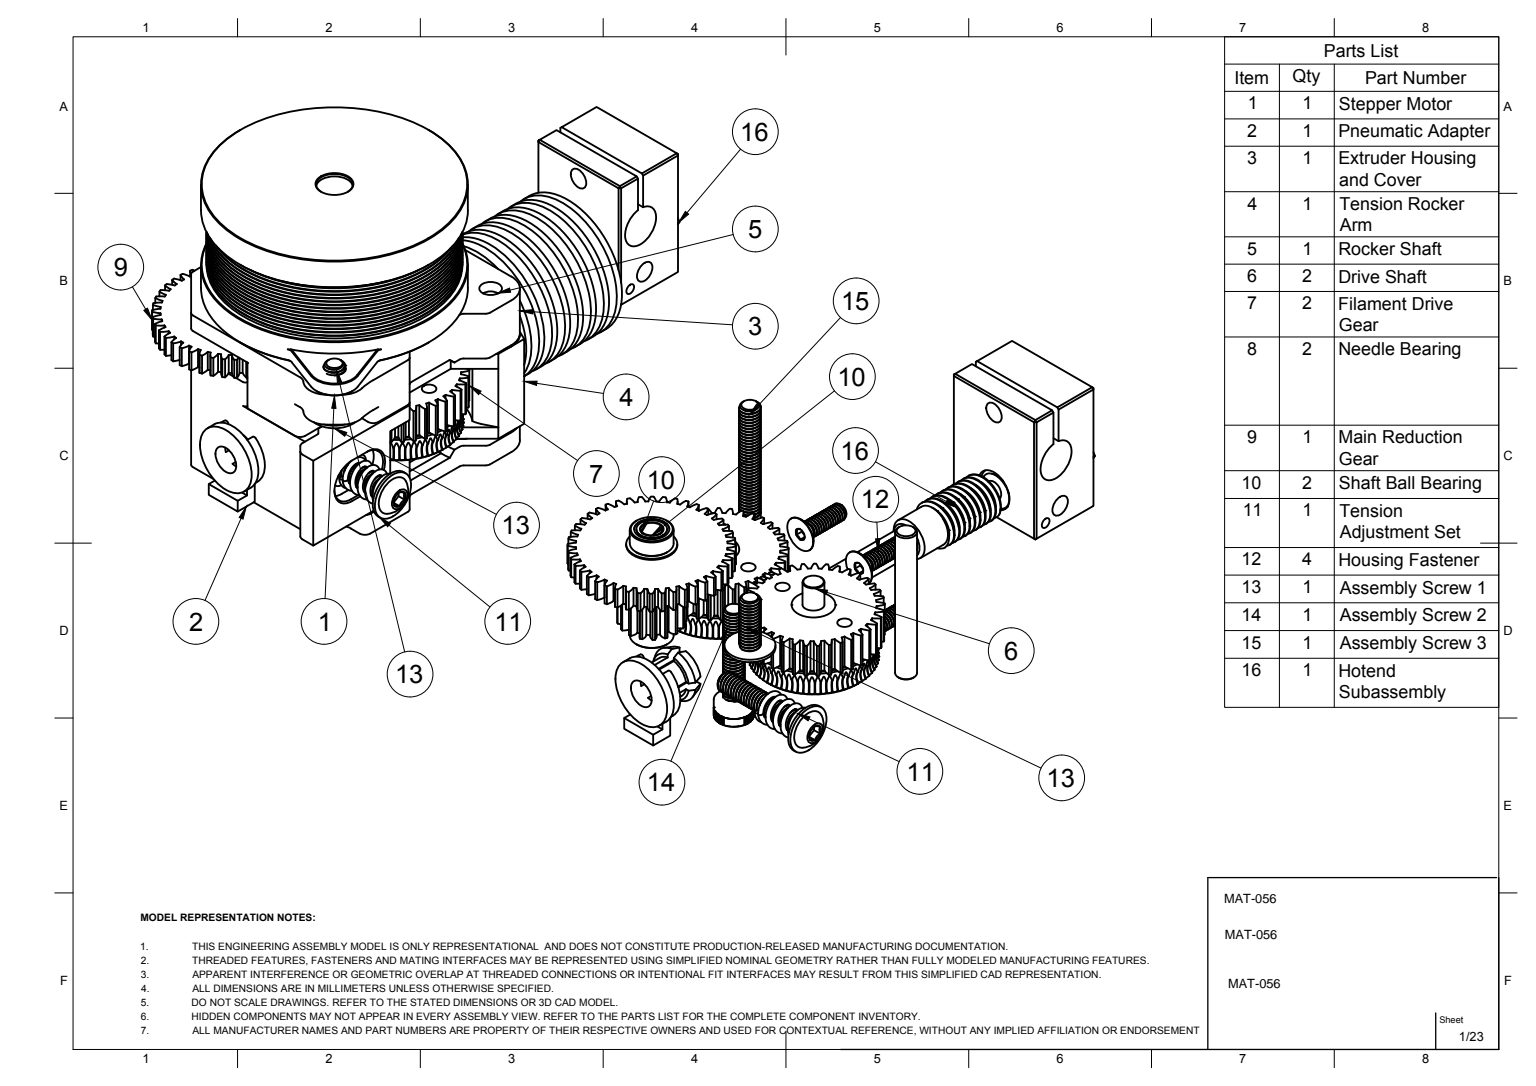
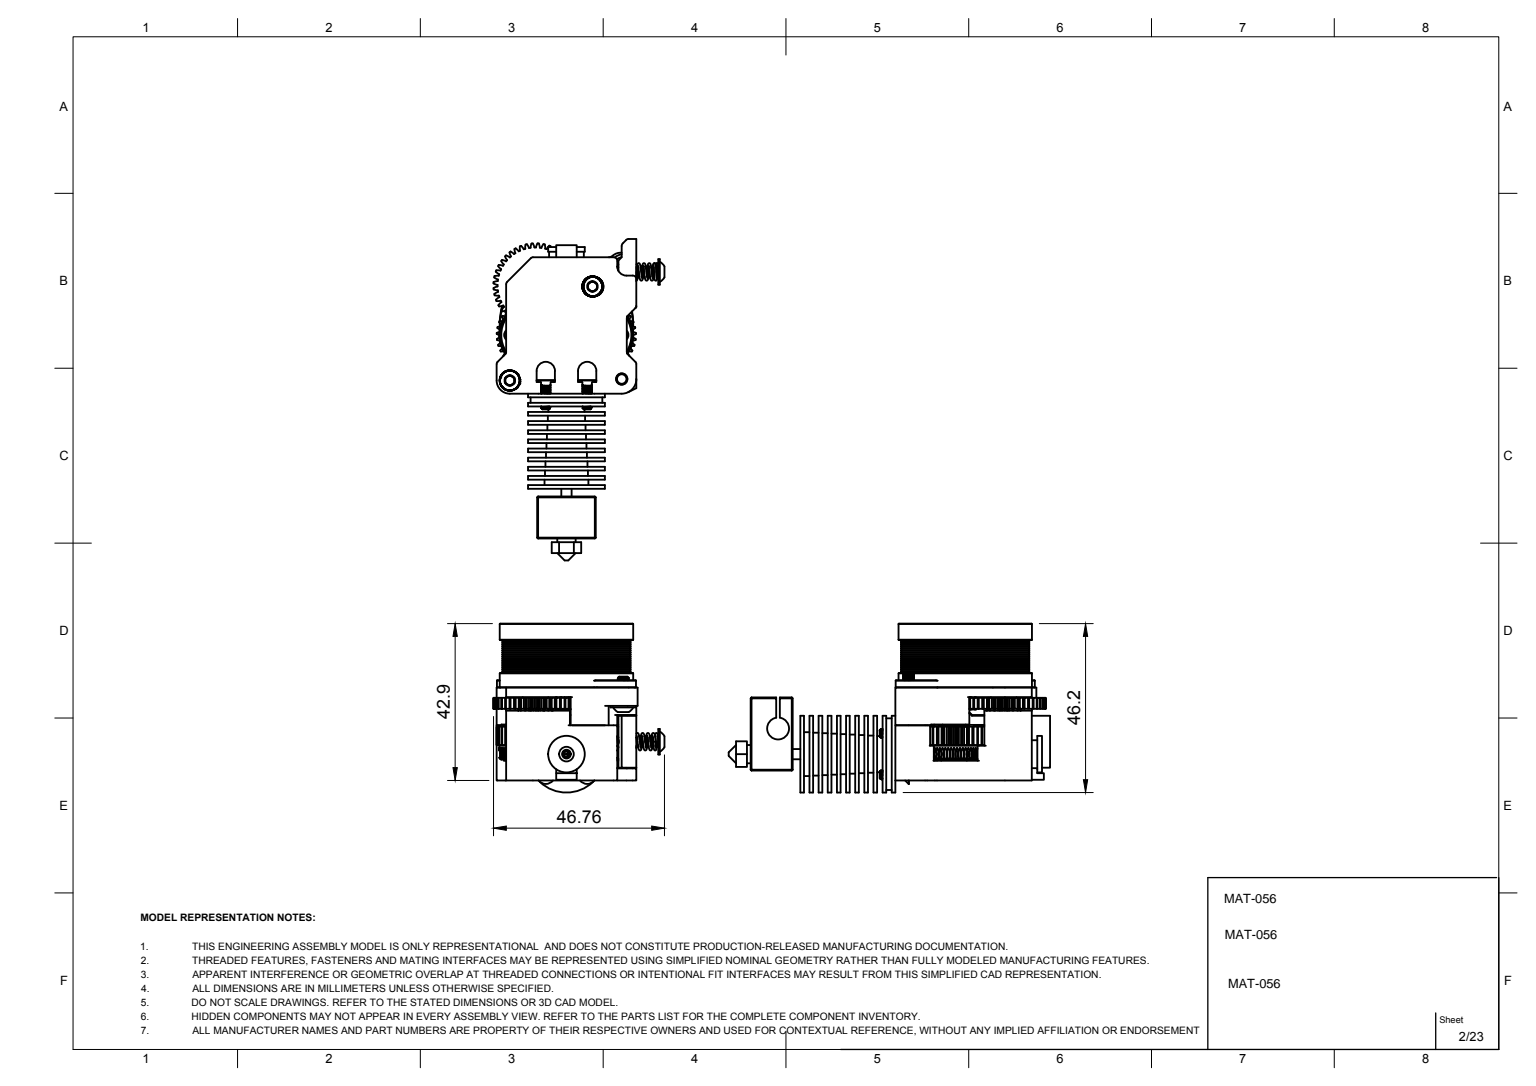
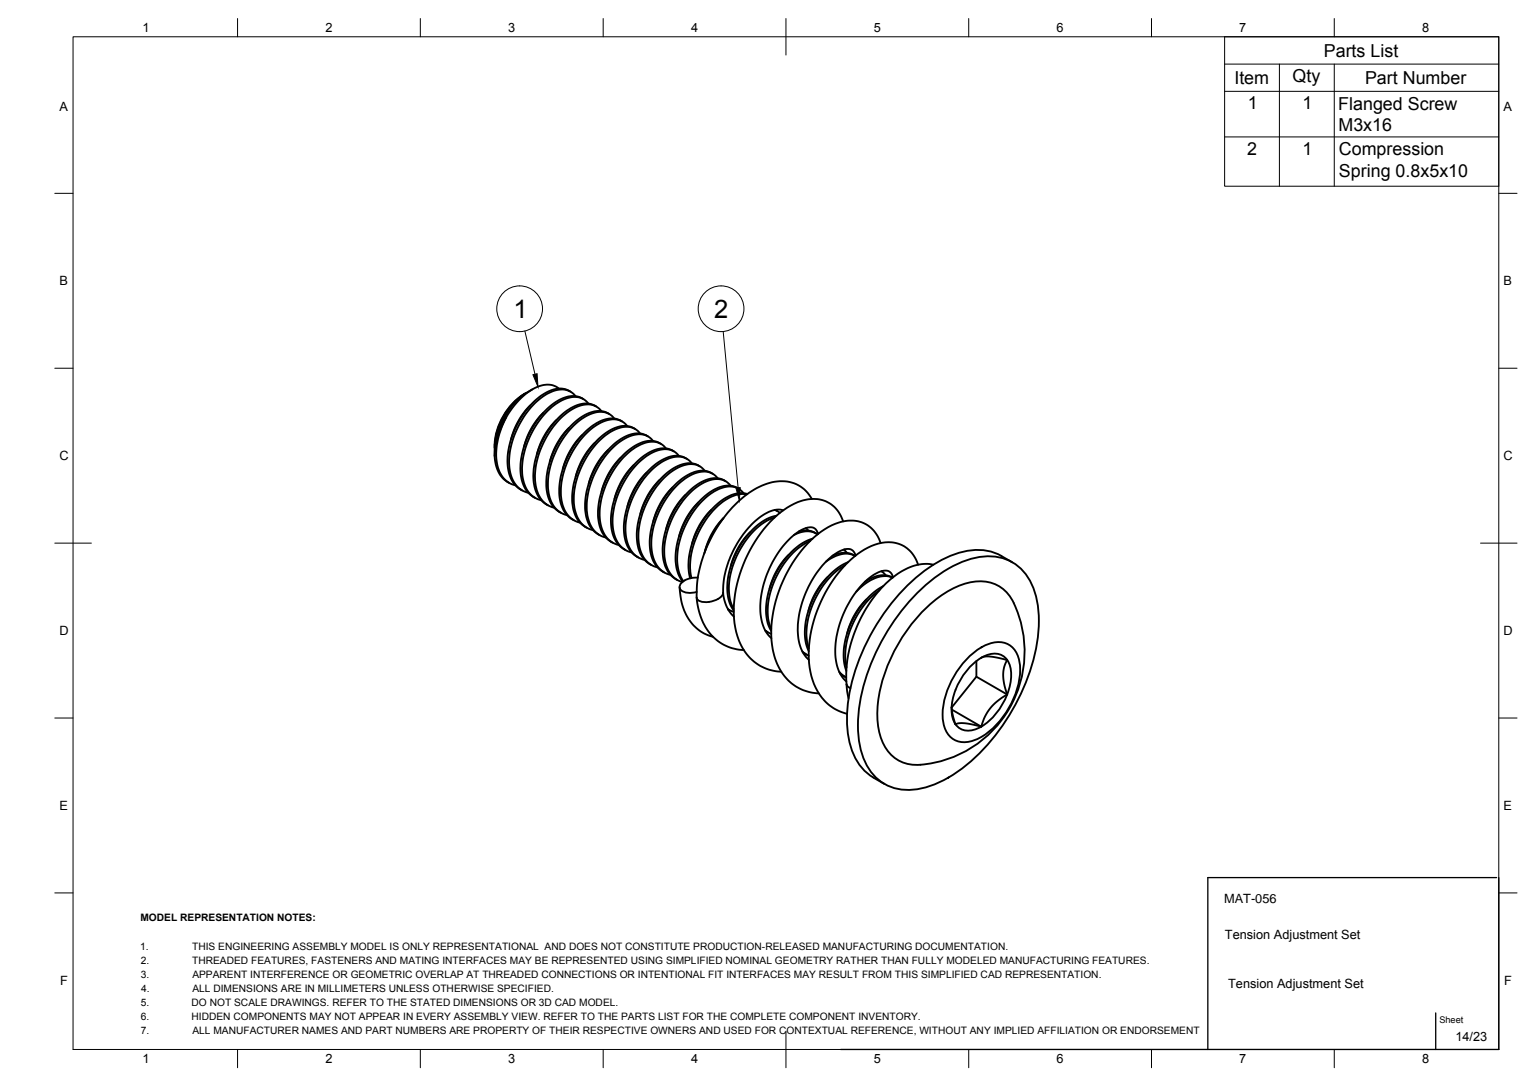
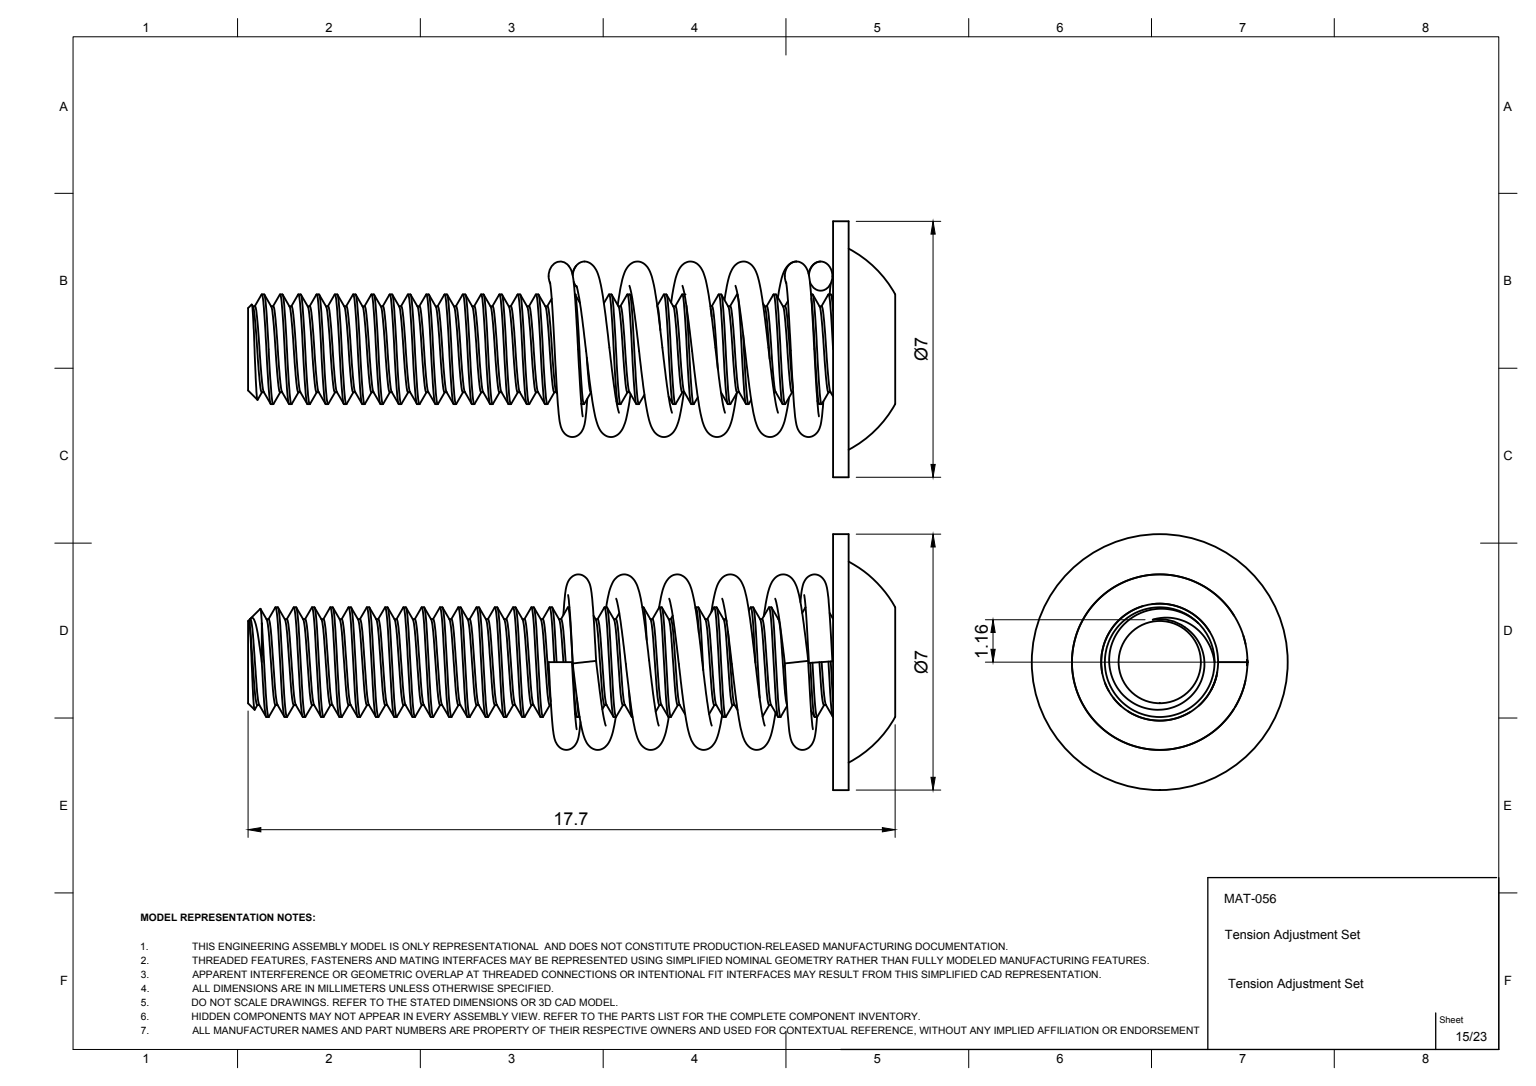
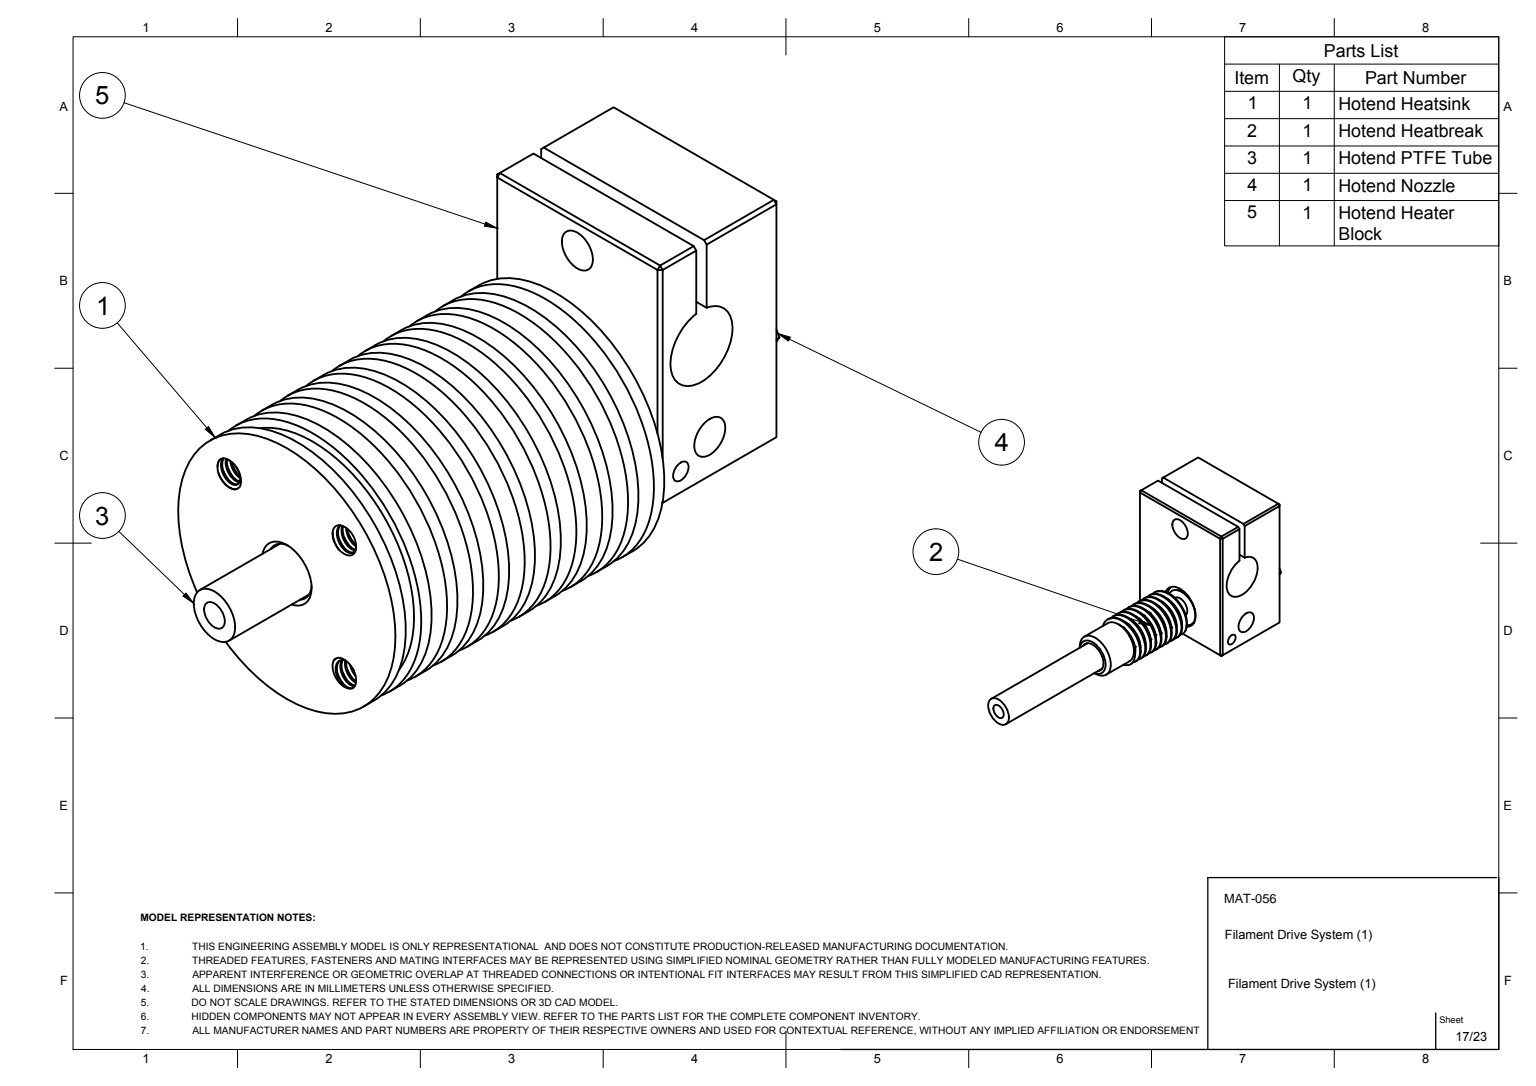
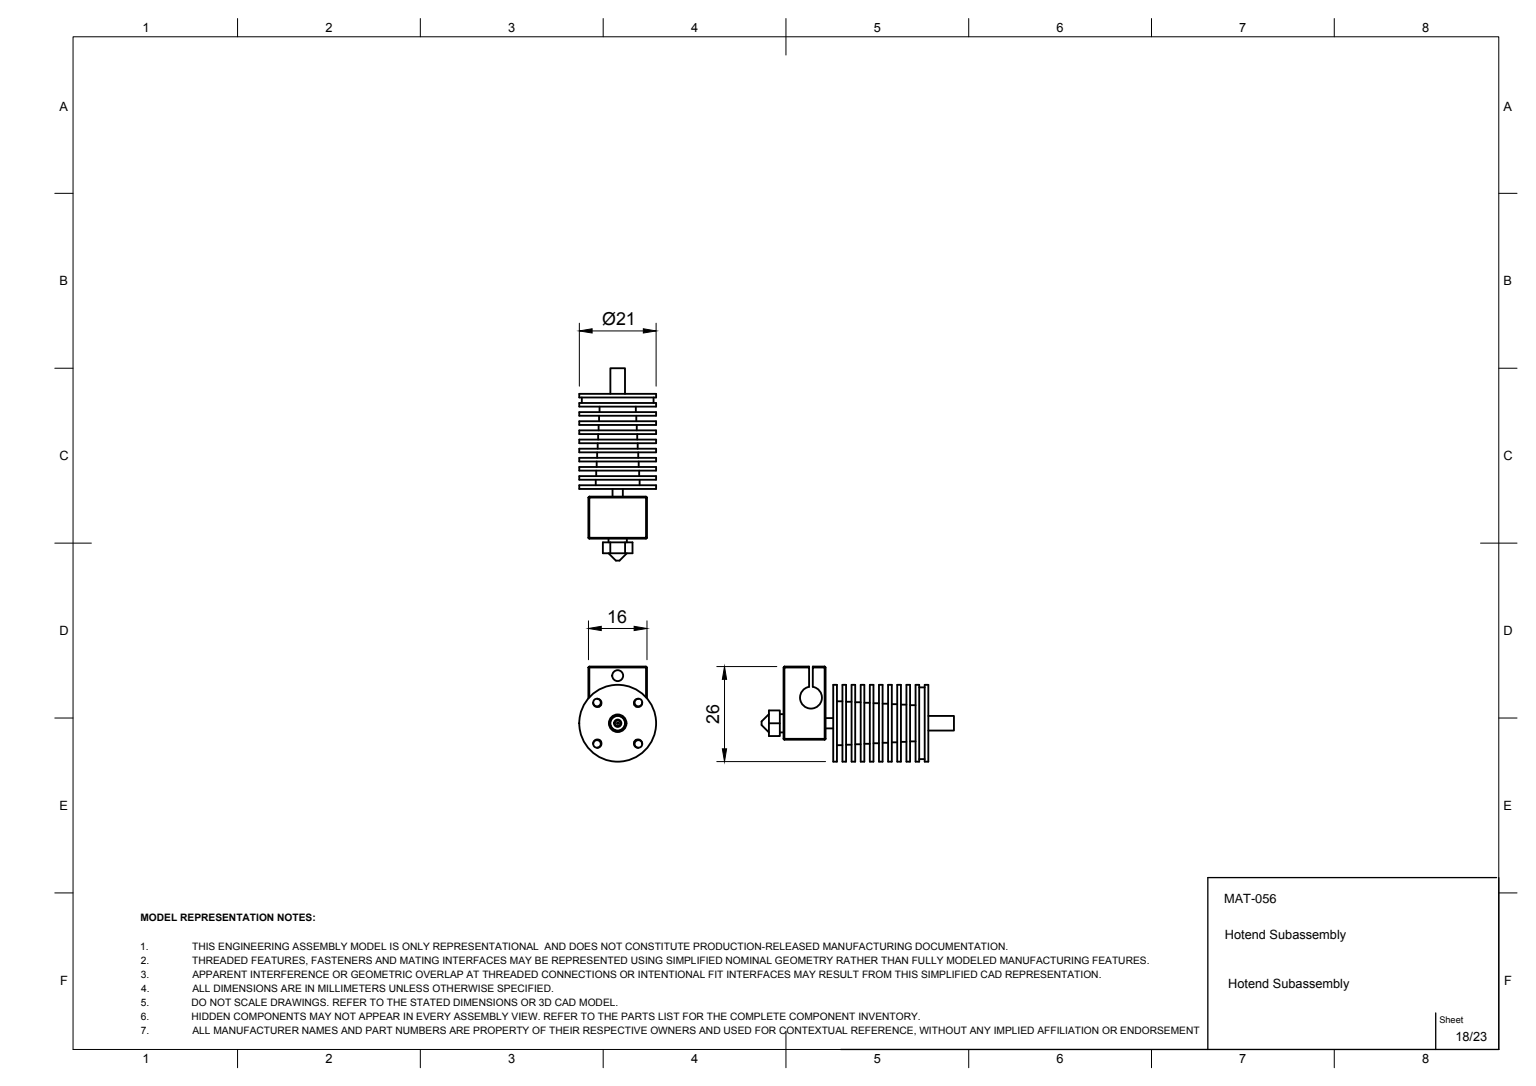
ISO-10303-21;
HEADER;
/* Generated by software containing ST-Developer
 * from STEP Tools, Inc. (www.steptools.com) 
 */

FILE_DESCRIPTION(
/* description */ (''),
/* implementation_level */ '2;1');

FILE_NAME(
/* name */ 'MAT-056',
/* time_stamp */ '2026-10-28T16:47:13+01:00',
/* author */ (''),
/* organization */ (''),
/* preprocessor_version */ 'ST-DEVELOPER v20.2',
/* originating_system */ 'Autodesk Translation Framework v15.17.0.0',
/* authorisation */ '');

FILE_SCHEMA (('AUTOMOTIVE_DESIGN { 1 0 10303 214 3 1 1 }'));
ENDSEC;

DATA;
#10=MECHANICAL_DESIGN_GEOMETRIC_PRESENTATION_REPRESENTATION('',(#4494,#4495,
#4496,#4497,#4498,#4499,#4500,#4501,#4502,#4503,#4504,#4505,#4506,#4507,
#4508,#4509,#4510,#4511,#4512,#4513,#4514,#4515,#4516,#4517,#4518,#4519,
#4520,#4521,#4522,#4523,#4524,#4525,#4526,#4527,#4528,#4529,#4530,#4531,
#4532,#4533,#4534,#4535,#4536,#4537,#4538,#4539,#4540,#4541,#4542,#4543,
#4544,#4545,#4546,#4547,#4548,#4549,#4550,#4551,#4552,#4553,#4554,#4555,
#4556,#4557,#4558,#4559,#4560,#4561,#4562,#4563,#4564,#4565,#4566,#4567,
#4568,#4569,#4570,#4571,#4572,#4573,#4574,#4575,#4576,#4577,#4578,#4579,
#4580,#4581,#4582,#4583,#4584,#4585,#4586,#4587,#4588,#4589,#4590,#4591,
#4592,#4593,#4594,#4595,#4596,#4597,#4598,#4599,#4600,#4601,#4602,#4603,
#4604,#4605,#4606,#4607,#4608,#4609,#4610,#4611,#4612,#4613),#459242);
#11=ITEM_DEFINED_TRANSFORMATION($,$,#99052,#99169);
#12=ITEM_DEFINED_TRANSFORMATION($,$,#99154,#99170);
#13=ITEM_DEFINED_TRANSFORMATION($,$,#105175,#105546);
#14=ITEM_DEFINED_TRANSFORMATION($,$,#105363,#105547);
#15=ITEM_DEFINED_TRANSFORMATION($,$,#105431,#105548);
#16=ITEM_DEFINED_TRANSFORMATION($,$,#105440,#105549);
#17=ITEM_DEFINED_TRANSFORMATION($,$,#105494,#105550);
#18=ITEM_DEFINED_TRANSFORMATION($,$,#94906,#105551);
#19=ITEM_DEFINED_TRANSFORMATION($,$,#95243,#105552);
#20=ITEM_DEFINED_TRANSFORMATION($,$,#95341,#105553);
#21=ITEM_DEFINED_TRANSFORMATION($,$,#97093,#105554);
#22=ITEM_DEFINED_TRANSFORMATION($,$,#97223,#105555);
#23=ITEM_DEFINED_TRANSFORMATION($,$,#97233,#105556);
#24=ITEM_DEFINED_TRANSFORMATION($,$,#97243,#105557);
#25=ITEM_DEFINED_TRANSFORMATION($,$,#97233,#105558);
#26=ITEM_DEFINED_TRANSFORMATION($,$,#98856,#105559);
#27=ITEM_DEFINED_TRANSFORMATION($,$,#97243,#105560);
#28=ITEM_DEFINED_TRANSFORMATION($,$,#98432,#105561);
#29=ITEM_DEFINED_TRANSFORMATION($,$,#99171,#105562);
#30=ITEM_DEFINED_TRANSFORMATION($,$,#98856,#105563);
#31=ITEM_DEFINED_TRANSFORMATION($,$,#99051,#105564);
#32=ITEM_DEFINED_TRANSFORMATION($,$,#99171,#105565);
#33=ITEM_DEFINED_TRANSFORMATION($,$,#99318,#105566);
#34=ITEM_DEFINED_TRANSFORMATION($,$,#99248,#105567);
#35=ITEM_DEFINED_TRANSFORMATION($,$,#99318,#105568);
#36=ITEM_DEFINED_TRANSFORMATION($,$,#99318,#105569);
#37=ITEM_DEFINED_TRANSFORMATION($,$,#99318,#105570);
#38=ITEM_DEFINED_TRANSFORMATION($,$,#99385,#105571);
#39=ITEM_DEFINED_TRANSFORMATION($,$,#102648,#105572);
#40=ITEM_DEFINED_TRANSFORMATION($,$,#105174,#105573);
#41=ITEM_DEFINED_TRANSFORMATION($,$,#94905,#105574);
#42=(
REPRESENTATION_RELATIONSHIP($,$,#459340,#459339)
REPRESENTATION_RELATIONSHIP_WITH_TRANSFORMATION(#11)
SHAPE_REPRESENTATION_RELATIONSHIP()
);
#43=(
REPRESENTATION_RELATIONSHIP($,$,#459341,#459339)
REPRESENTATION_RELATIONSHIP_WITH_TRANSFORMATION(#12)
SHAPE_REPRESENTATION_RELATIONSHIP()
);
#44=(
REPRESENTATION_RELATIONSHIP($,$,#459348,#459347)
REPRESENTATION_RELATIONSHIP_WITH_TRANSFORMATION(#13)
SHAPE_REPRESENTATION_RELATIONSHIP()
);
#45=(
REPRESENTATION_RELATIONSHIP($,$,#459349,#459347)
REPRESENTATION_RELATIONSHIP_WITH_TRANSFORMATION(#14)
SHAPE_REPRESENTATION_RELATIONSHIP()
);
#46=(
REPRESENTATION_RELATIONSHIP($,$,#459350,#459347)
REPRESENTATION_RELATIONSHIP_WITH_TRANSFORMATION(#15)
SHAPE_REPRESENTATION_RELATIONSHIP()
);
#47=(
REPRESENTATION_RELATIONSHIP($,$,#459351,#459347)
REPRESENTATION_RELATIONSHIP_WITH_TRANSFORMATION(#16)
SHAPE_REPRESENTATION_RELATIONSHIP()
);
#48=(
REPRESENTATION_RELATIONSHIP($,$,#459352,#459347)
REPRESENTATION_RELATIONSHIP_WITH_TRANSFORMATION(#17)
SHAPE_REPRESENTATION_RELATIONSHIP()
);
#49=(
REPRESENTATION_RELATIONSHIP($,$,#459330,#459329)
REPRESENTATION_RELATIONSHIP_WITH_TRANSFORMATION(#18)
SHAPE_REPRESENTATION_RELATIONSHIP()
);
#50=(
REPRESENTATION_RELATIONSHIP($,$,#459331,#459329)
REPRESENTATION_RELATIONSHIP_WITH_TRANSFORMATION(#19)
SHAPE_REPRESENTATION_RELATIONSHIP()
);
#51=(
REPRESENTATION_RELATIONSHIP($,$,#459332,#459329)
REPRESENTATION_RELATIONSHIP_WITH_TRANSFORMATION(#20)
SHAPE_REPRESENTATION_RELATIONSHIP()
);
#52=(
REPRESENTATION_RELATIONSHIP($,$,#459333,#459329)
REPRESENTATION_RELATIONSHIP_WITH_TRANSFORMATION(#21)
SHAPE_REPRESENTATION_RELATIONSHIP()
);
#53=(
REPRESENTATION_RELATIONSHIP($,$,#459334,#459329)
REPRESENTATION_RELATIONSHIP_WITH_TRANSFORMATION(#22)
SHAPE_REPRESENTATION_RELATIONSHIP()
);
#54=(
REPRESENTATION_RELATIONSHIP($,$,#459335,#459329)
REPRESENTATION_RELATIONSHIP_WITH_TRANSFORMATION(#23)
SHAPE_REPRESENTATION_RELATIONSHIP()
);
#55=(
REPRESENTATION_RELATIONSHIP($,$,#459336,#459329)
REPRESENTATION_RELATIONSHIP_WITH_TRANSFORMATION(#24)
SHAPE_REPRESENTATION_RELATIONSHIP()
);
#56=(
REPRESENTATION_RELATIONSHIP($,$,#459335,#459329)
REPRESENTATION_RELATIONSHIP_WITH_TRANSFORMATION(#25)
SHAPE_REPRESENTATION_RELATIONSHIP()
);
#57=(
REPRESENTATION_RELATIONSHIP($,$,#459338,#459329)
REPRESENTATION_RELATIONSHIP_WITH_TRANSFORMATION(#26)
SHAPE_REPRESENTATION_RELATIONSHIP()
);
#58=(
REPRESENTATION_RELATIONSHIP($,$,#459336,#459329)
REPRESENTATION_RELATIONSHIP_WITH_TRANSFORMATION(#27)
SHAPE_REPRESENTATION_RELATIONSHIP()
);
#59=(
REPRESENTATION_RELATIONSHIP($,$,#459337,#459329)
REPRESENTATION_RELATIONSHIP_WITH_TRANSFORMATION(#28)
SHAPE_REPRESENTATION_RELATIONSHIP()
);
#60=(
REPRESENTATION_RELATIONSHIP($,$,#459342,#459329)
REPRESENTATION_RELATIONSHIP_WITH_TRANSFORMATION(#29)
SHAPE_REPRESENTATION_RELATIONSHIP()
);
#61=(
REPRESENTATION_RELATIONSHIP($,$,#459338,#459329)
REPRESENTATION_RELATIONSHIP_WITH_TRANSFORMATION(#30)
SHAPE_REPRESENTATION_RELATIONSHIP()
);
#62=(
REPRESENTATION_RELATIONSHIP($,$,#459339,#459329)
REPRESENTATION_RELATIONSHIP_WITH_TRANSFORMATION(#31)
SHAPE_REPRESENTATION_RELATIONSHIP()
);
#63=(
REPRESENTATION_RELATIONSHIP($,$,#459342,#459329)
REPRESENTATION_RELATIONSHIP_WITH_TRANSFORMATION(#32)
SHAPE_REPRESENTATION_RELATIONSHIP()
);
#64=(
REPRESENTATION_RELATIONSHIP($,$,#459344,#459329)
REPRESENTATION_RELATIONSHIP_WITH_TRANSFORMATION(#33)
SHAPE_REPRESENTATION_RELATIONSHIP()
);
#65=(
REPRESENTATION_RELATIONSHIP($,$,#459343,#459329)
REPRESENTATION_RELATIONSHIP_WITH_TRANSFORMATION(#34)
SHAPE_REPRESENTATION_RELATIONSHIP()
);
#66=(
REPRESENTATION_RELATIONSHIP($,$,#459344,#459329)
REPRESENTATION_RELATIONSHIP_WITH_TRANSFORMATION(#35)
SHAPE_REPRESENTATION_RELATIONSHIP()
);
#67=(
REPRESENTATION_RELATIONSHIP($,$,#459344,#459329)
REPRESENTATION_RELATIONSHIP_WITH_TRANSFORMATION(#36)
SHAPE_REPRESENTATION_RELATIONSHIP()
);
#68=(
REPRESENTATION_RELATIONSHIP($,$,#459344,#459329)
REPRESENTATION_RELATIONSHIP_WITH_TRANSFORMATION(#37)
SHAPE_REPRESENTATION_RELATIONSHIP()
);
#69=(
REPRESENTATION_RELATIONSHIP($,$,#459345,#459329)
REPRESENTATION_RELATIONSHIP_WITH_TRANSFORMATION(#38)
SHAPE_REPRESENTATION_RELATIONSHIP()
);
#70=(
REPRESENTATION_RELATIONSHIP($,$,#459346,#459329)
REPRESENTATION_RELATIONSHIP_WITH_TRANSFORMATION(#39)
SHAPE_REPRESENTATION_RELATIONSHIP()
);
#71=(
REPRESENTATION_RELATIONSHIP($,$,#459347,#459329)
REPRESENTATION_RELATIONSHIP_WITH_TRANSFORMATION(#40)
SHAPE_REPRESENTATION_RELATIONSHIP()
);
#72=(
REPRESENTATION_RELATIONSHIP($,$,#459329,#459328)
REPRESENTATION_RELATIONSHIP_WITH_TRANSFORMATION(#41)
SHAPE_REPRESENTATION_RELATIONSHIP()
);
#73=CONTEXT_DEPENDENT_SHAPE_REPRESENTATION(#42,#459286);
#74=CONTEXT_DEPENDENT_SHAPE_REPRESENTATION(#43,#459287);
#75=CONTEXT_DEPENDENT_SHAPE_REPRESENTATION(#44,#459299);
#76=CONTEXT_DEPENDENT_SHAPE_REPRESENTATION(#45,#459300);
#77=CONTEXT_DEPENDENT_SHAPE_REPRESENTATION(#46,#459301);
#78=CONTEXT_DEPENDENT_SHAPE_REPRESENTATION(#47,#459302);
#79=CONTEXT_DEPENDENT_SHAPE_REPRESENTATION(#48,#459303);
#80=CONTEXT_DEPENDENT_SHAPE_REPRESENTATION(#49,#459304);
#81=CONTEXT_DEPENDENT_SHAPE_REPRESENTATION(#50,#459305);
#82=CONTEXT_DEPENDENT_SHAPE_REPRESENTATION(#51,#459306);
#83=CONTEXT_DEPENDENT_SHAPE_REPRESENTATION(#52,#459307);
#84=CONTEXT_DEPENDENT_SHAPE_REPRESENTATION(#53,#459308);
#85=CONTEXT_DEPENDENT_SHAPE_REPRESENTATION(#54,#459309);
#86=CONTEXT_DEPENDENT_SHAPE_REPRESENTATION(#55,#459310);
#87=CONTEXT_DEPENDENT_SHAPE_REPRESENTATION(#56,#459311);
#88=CONTEXT_DEPENDENT_SHAPE_REPRESENTATION(#57,#459312);
#89=CONTEXT_DEPENDENT_SHAPE_REPRESENTATION(#58,#459313);
#90=CONTEXT_DEPENDENT_SHAPE_REPRESENTATION(#59,#459314);
#91=CONTEXT_DEPENDENT_SHAPE_REPRESENTATION(#60,#459315);
#92=CONTEXT_DEPENDENT_SHAPE_REPRESENTATION(#61,#459316);
#93=CONTEXT_DEPENDENT_SHAPE_REPRESENTATION(#62,#459317);
#94=CONTEXT_DEPENDENT_SHAPE_REPRESENTATION(#63,#459318);
#95=CONTEXT_DEPENDENT_SHAPE_REPRESENTATION(#64,#459319);
#96=CONTEXT_DEPENDENT_SHAPE_REPRESENTATION(#65,#459320);
#97=CONTEXT_DEPENDENT_SHAPE_REPRESENTATION(#66,#459321);
#98=CONTEXT_DEPENDENT_SHAPE_REPRESENTATION(#67,#459322);
#99=CONTEXT_DEPENDENT_SHAPE_REPRESENTATION(#68,#459323);
#100=CONTEXT_DEPENDENT_SHAPE_REPRESENTATION(#69,#459324);
#101=CONTEXT_DEPENDENT_SHAPE_REPRESENTATION(#70,#459325);
#102=CONTEXT_DEPENDENT_SHAPE_REPRESENTATION(#71,#459326);
#103=CONTEXT_DEPENDENT_SHAPE_REPRESENTATION(#72,#459327);
#104=NEXT_ASSEMBLY_USAGE_OCCURRENCE('Flanged Screw M3x16:1',
'Flanged Screw M3x16:1','Flanged Screw M3x16:1',#459365,#459366,
'Flanged Screw M3x16:1');
#105=NEXT_ASSEMBLY_USAGE_OCCURRENCE('Compression Spring 0.8x5x10:1',
'Compression Spring 0.8x5x10:1','Compression Spring 0.8x5x10:1',#459365,
#459367,'Compression Spring 0.8x5x10:1');
#106=NEXT_ASSEMBLY_USAGE_OCCURRENCE('Hotend Heatsink:1',
'Hotend Heatsink:1','Hotend Heatsink:1',#459373,#459374,
'Hotend Heatsink:1');
#107=NEXT_ASSEMBLY_USAGE_OCCURRENCE('Hotend Heatbreak:1',
'Hotend Heatbreak:1','Hotend Heatbreak:1',#459373,#459375,
'Hotend Heatbreak:1');
#108=NEXT_ASSEMBLY_USAGE_OCCURRENCE('Hotend PTFE Tube:1',
'Hotend PTFE Tube:1','Hotend PTFE Tube:1',#459373,#459376,
'Hotend PTFE Tube:1');
#109=NEXT_ASSEMBLY_USAGE_OCCURRENCE('Hotend Nozzle:1','Hotend Nozzle:1',
'Hotend Nozzle:1',#459373,#459377,'Hotend Nozzle:1');
#110=NEXT_ASSEMBLY_USAGE_OCCURRENCE('Hotend Heater Block:1',
'Hotend Heater Block:1','Hotend Heater Block:1',#459373,#459378,
'Hotend Heater Block:1');
#111=NEXT_ASSEMBLY_USAGE_OCCURRENCE('Stepper Motor:1','Stepper Motor:1',
'Stepper Motor:1',#459355,#459356,'Stepper Motor:1');
#112=NEXT_ASSEMBLY_USAGE_OCCURRENCE('Pneumatic Adapter:1',
'Pneumatic Adapter:1','Pneumatic Adapter:1',#459355,#459357,
'Pneumatic Adapter:1');
#113=NEXT_ASSEMBLY_USAGE_OCCURRENCE('Extruder Housing and Cover:1',
'Extruder Housing and Cover:1','Extruder Housing and Cover:1',#459355,#459358,
'Extruder Housing and Cover:1');
#114=NEXT_ASSEMBLY_USAGE_OCCURRENCE('Tension Rocker Arm:1',
'Tension Rocker Arm:1','Tension Rocker Arm:1',#459355,#459359,
'Tension Rocker Arm:1');
#115=NEXT_ASSEMBLY_USAGE_OCCURRENCE('Rocker Shaft:1','Rocker Shaft:1',
'Rocker Shaft:1',#459355,#459360,'Rocker Shaft:1');
#116=NEXT_ASSEMBLY_USAGE_OCCURRENCE('Drive Shaft:1','Drive Shaft:1',
'Drive Shaft:1',#459355,#459361,'Drive Shaft:1');
#117=NEXT_ASSEMBLY_USAGE_OCCURRENCE('Filament Drive Gear:1',
'Filament Drive Gear:1','Filament Drive Gear:1',#459355,#459362,
'Filament Drive Gear:1');
#118=NEXT_ASSEMBLY_USAGE_OCCURRENCE('Drive Shaft:2','Drive Shaft:2',
'Drive Shaft:2',#459355,#459361,'Drive Shaft:2');
#119=NEXT_ASSEMBLY_USAGE_OCCURRENCE('Needle Bearing:1',
'Needle Bearing:1','Needle Bearing:1',#459355,#459364,
'Needle Bearing:1');
#120=NEXT_ASSEMBLY_USAGE_OCCURRENCE('Filament Drive Gear:2',
'Filament Drive Gear:2','Filament Drive Gear:2',#459355,#459362,
'Filament Drive Gear:2');
#121=NEXT_ASSEMBLY_USAGE_OCCURRENCE('Main Reduction Gear:1',
'Main Reduction Gear:1','Main Reduction Gear:1',#459355,#459363,
'Main Reduction Gear:1');
#122=NEXT_ASSEMBLY_USAGE_OCCURRENCE('Shaft Ball Bearing:1',
'Shaft Ball Bearing:1','Shaft Ball Bearing:1',#459355,#459368,
'Shaft Ball Bearing:1');
#123=NEXT_ASSEMBLY_USAGE_OCCURRENCE('Needle Bearing:2',
'Needle Bearing:2','Needle Bearing:2',#459355,#459364,
'Needle Bearing:2');
#124=NEXT_ASSEMBLY_USAGE_OCCURRENCE('Tension Adjustment Set:1',
'Tension Adjustment Set:1','Tension Adjustment Set:1',#459355,#459365,
'Tension Adjustment Set:1');
#125=NEXT_ASSEMBLY_USAGE_OCCURRENCE('Shaft Ball Bearing:2',
'Shaft Ball Bearing:2','Shaft Ball Bearing:2',#459355,#459368,
'Shaft Ball Bearing:2');
#126=NEXT_ASSEMBLY_USAGE_OCCURRENCE('Housing Fastener:1',
'Housing Fastener:1','Housing Fastener:1',#459355,#459370,
'Housing Fastener:1');
#127=NEXT_ASSEMBLY_USAGE_OCCURRENCE('Assembly Screw 1:1',
'Assembly Screw 1:1','Assembly Screw 1:1',#459355,#459369,
'Assembly Screw 1:1');
#128=NEXT_ASSEMBLY_USAGE_OCCURRENCE('Housing Fastener:2',
'Housing Fastener:2','Housing Fastener:2',#459355,#459370,
'Housing Fastener:2');
#129=NEXT_ASSEMBLY_USAGE_OCCURRENCE('Housing Fastener:3',
'Housing Fastener:3','Housing Fastener:3',#459355,#459370,
'Housing Fastener:3');
#130=NEXT_ASSEMBLY_USAGE_OCCURRENCE('Housing Fastener:4',
'Housing Fastener:4','Housing Fastener:4',#459355,#459370,
'Housing Fastener:4');
#131=NEXT_ASSEMBLY_USAGE_OCCURRENCE('Assembly Screw 2:1',
'Assembly Screw 2:1','Assembly Screw 2:1',#459355,#459371,
'Assembly Screw 2:1');
#132=NEXT_ASSEMBLY_USAGE_OCCURRENCE('Assembly Screw 3:1',
'Assembly Screw 3:1','Assembly Screw 3:1',#459355,#459372,
'Assembly Screw 3:1');
#133=NEXT_ASSEMBLY_USAGE_OCCURRENCE('Hotend Subassembly:1',
'Hotend Subassembly:1','Hotend Subassembly:1',#459355,#459373,
'Hotend Subassembly:1');
#134=NEXT_ASSEMBLY_USAGE_OCCURRENCE('Filament Drive System:1',
'Filament Drive System:1','Filament Drive System:1',#459354,#459355,
'Filament Drive System:1');
#135=SPHERICAL_SURFACE('',#96252,3.7);
#136=SPHERICAL_SURFACE('',#96289,0.4);
#137=SPHERICAL_SURFACE('',#96515,3.7);
#138=SPHERICAL_SURFACE('',#96673,2.5);
#139=SPHERICAL_SURFACE('',#96678,2.5);
#140=SPHERICAL_SURFACE('',#96891,0.4);
#141=SPHERICAL_SURFACE('',#96896,0.4);
#142=SPHERICAL_SURFACE('',#99121,3.10691712599126);
#143=SPHERICAL_SURFACE('',#99208,0.576463888168111);
#144=SPHERICAL_SURFACE('',#99210,0.576463888168111);
#145=SPHERICAL_SURFACE('',#99212,0.576463888168111);
#146=SPHERICAL_SURFACE('',#99214,0.576463888168111);
#147=SPHERICAL_SURFACE('',#99216,0.576463888168111);
#148=SPHERICAL_SURFACE('',#99218,0.576463888168111);
#149=SPHERICAL_SURFACE('',#99220,0.576463888168111);
#150=SPHERICAL_SURFACE('',#99222,0.576463888168111);
#151=SPHERICAL_SURFACE('',#99224,0.576463888168111);
#152=SPHERICAL_SURFACE('',#99226,0.576463888168111);
#153=SPHERICAL_SURFACE('',#99228,0.576463888168111);
#154=SPHERICAL_SURFACE('',#99230,0.576463888168111);
#155=SPHERICAL_SURFACE('',#99285,3.10691712599126);
#156=ELLIPSE('',#96160,1.23559647500717,0.4);
#157=ELLIPSE('',#96173,0.405496303869506,0.4);
#158=ELLIPSE('',#96175,0.680073525436772,0.4);
#159=ELLIPSE('',#96193,0.565685424949236,0.4);
#160=ELLIPSE('',#96250,11.2311262166053,9.2);
#161=ELLIPSE('',#96391,11.2311262166054,9.2);
#162=ELLIPSE('',#96412,0.565685424948761,0.4);
#163=ELLIPSE('',#96519,10.6232449530892,9.2);
#164=ELLIPSE('',#96520,11.2311262166053,9.2);
#165=ELLIPSE('',#96521,11.2311262166053,9.2);
#166=ELLIPSE('',#96562,11.2311262166054,9.2);
#167=ELLIPSE('',#96563,10.6232449530892,9.2);
#168=ELLIPSE('',#96876,12.4909175466738,7.94395207421036);
#169=ELLIPSE('',#97006,2.10877579943506,1.);
#170=ELLIPSE('',#97007,2.46373699895096,1.);
#171=ELLIPSE('',#97009,2.59999999999994,1.3);
#172=ELLIPSE('',#97010,0.230940107675852,0.2);
#173=ELLIPSE('',#97011,0.230940107675852,0.2);
#174=ELLIPSE('',#97015,2.26648083430746,1.3);
#175=ELLIPSE('',#97016,0.24415491775229,0.2);
#176=ELLIPSE('',#97017,0.24415491775229,0.2);
#177=ELLIPSE('',#97027,0.24415491775229,0.2);
#178=ELLIPSE('',#97030,0.24415491775229,0.2);
#179=ELLIPSE('',#97033,0.230940107675851,0.2);
#180=ELLIPSE('',#97035,0.230940107675851,0.2);
#181=ELLIPSE('',#97037,2.59999999999997,1.3);
#182=ELLIPSE('',#97038,2.46373699895092,1.);
#183=ELLIPSE('',#97040,2.10877579943508,1.);
#184=ELLIPSE('',#97042,2.26648083430744,1.3);
#185=ELLIPSE('',#97153,2.40416305603427,1.7);
#186=ELLIPSE('',#99155,0.40000000018352,0.321902553589955);
#187=ELLIPSE('',#99156,0.400000000332434,0.321319291807333);
#188=ELLIPSE('',#99157,0.40000000018352,0.321902553589955);
#189=ELLIPSE('',#99158,0.400000000010015,0.321902553729585);
#190=ELLIPSE('',#99159,0.400000000010015,0.321902553729585);
#191=ELLIPSE('',#99160,0.4,0.32);
#192=ELLIPSE('',#99161,0.4,0.32);
#193=ELLIPSE('',#99162,0.400000000010016,0.321902553729585);
#194=ELLIPSE('',#99163,0.400000000010016,0.321902553729585);
#195=ELLIPSE('',#99165,0.400000000183514,0.321902553589955);
#196=ELLIPSE('',#99166,0.400000000183514,0.321902553589955);
#197=ELLIPSE('',#99168,0.40000000033243,0.321319291807334);
#198=ELLIPSE('',#99479,0.027499979201819,0.0194466400235264);
#199=ELLIPSE('',#99481,0.0274999792018223,0.0194466400235272);
#200=ELLIPSE('',#99483,0.0274999792017924,0.0194466400235207);
#201=ELLIPSE('',#99485,0.0274999792018212,0.0194466400235271);
#202=ELLIPSE('',#99487,0.0274999792018093,0.0194466400235266);
#203=ELLIPSE('',#99489,0.0274999792018116,0.0194466400235246);
#204=ELLIPSE('',#99491,0.0274999792018137,0.0194466400235258);
#205=ELLIPSE('',#99493,0.0274999792018285,0.019446640023529);
#206=ELLIPSE('',#99495,0.0274999792018225,0.0194466400235274);
#207=ELLIPSE('',#99497,0.0274999792018218,0.0194466400235291);
#208=ELLIPSE('',#99499,0.0274999792018109,0.019446640023525);
#209=ELLIPSE('',#99501,0.0274999792018031,0.0194466400235235);
#210=ELLIPSE('',#99503,0.0274999792018403,0.0194466400235318);
#211=ELLIPSE('',#99505,0.0274999792018273,0.0194466400235287);
#212=ELLIPSE('',#99507,0.0274999792018071,0.0194466400235239);
#213=ELLIPSE('',#99509,0.0274999792018003,0.0194466400235229);
#214=ELLIPSE('',#99511,0.0274999792018132,0.0194466400235249);
#215=ELLIPSE('',#99513,0.0274999792018307,0.0194466400235292);
#216=ELLIPSE('',#99515,0.0274999792018211,0.0194466400235281);
#217=ELLIPSE('',#99517,0.027499979201803,0.0194466400235226);
#218=ELLIPSE('',#99519,0.027499979201819,0.019446640023527);
#219=ELLIPSE('',#99521,0.0274999792018149,0.0194466400235247);
#220=ELLIPSE('',#99523,0.0274999792018479,0.019446640023533);
#221=ELLIPSE('',#99525,0.0274999792018327,0.0194466400235312);
#222=ELLIPSE('',#99527,0.0274999792018231,0.0194466400235292);
#223=ELLIPSE('',#99529,0.0274999792018213,0.0194466400235274);
#224=ELLIPSE('',#99531,0.0274999792018071,0.0194466400235238);
#225=ELLIPSE('',#99533,0.0274999792018454,0.0194466400235312);
#226=ELLIPSE('',#99535,0.0274999792018473,0.0194466400235348);
#227=ELLIPSE('',#99537,0.0274999792017789,0.0194466400235172);
#228=ELLIPSE('',#99539,0.0274999792017695,0.0194466400235156);
#229=ELLIPSE('',#99541,0.0274999792018213,0.0194466400235258);
#230=ELLIPSE('',#99543,0.0274999792018424,0.0194466400235306);
#231=ELLIPSE('',#99545,0.0274999792018183,0.0194466400235275);
#232=ELLIPSE('',#99547,0.0274999792018239,0.0194466400235288);
#233=ELLIPSE('',#99549,0.02749997920184,0.0194466400235311);
#234=ELLIPSE('',#99551,0.0274999792018135,0.0194466400235251);
#235=ELLIPSE('',#99553,0.0274999792017894,0.019446640023519);
#236=ELLIPSE('',#99555,0.0274999792018526,0.0194466400235354);
#237=ELLIPSE('',#99557,0.0274999792017924,0.0194466400235216);
#238=ELLIPSE('',#99559,0.0274999792018348,0.0194466400235303);
#239=ELLIPSE('',#99561,0.0274999792018408,0.0194466400235337);
#240=ELLIPSE('',#99563,0.0274999792018198,0.0194466400235256);
#241=ELLIPSE('',#99565,0.0274999792018384,0.0194466400235318);
#242=ELLIPSE('',#99567,0.027499979201788,0.0194466400235206);
#243=ELLIPSE('',#99569,0.0274999792018338,0.0194466400235292);
#244=ELLIPSE('',#99571,0.027499979201835,0.0194466400235291);
#245=ELLIPSE('',#99573,0.0274999792018021,0.0194466400235238);
#246=ELLIPSE('',#99575,0.0274999792018534,0.0194466400235355);
#247=ELLIPSE('',#99580,0.0274999792018521,0.0194466400235337);
#248=ELLIPSE('',#99582,0.027499979201854,0.0194466400235346);
#249=ELLIPSE('',#99584,0.0274999792018411,0.0194466400235325);
#250=ELLIPSE('',#99586,0.0274999792017827,0.0194466400235186);
#251=ELLIPSE('',#99588,0.0274999792018246,0.0194466400235274);
#252=ELLIPSE('',#99590,0.0274999792018228,0.0194466400235272);
#253=ELLIPSE('',#99592,0.0274999792018508,0.0194466400235342);
#254=ELLIPSE('',#99594,0.027499979201825,0.019446640023528);
#255=ELLIPSE('',#99596,0.0274999792018088,0.0194466400235245);
#256=ELLIPSE('',#99598,0.0274999792018039,0.0194466400235234);
#257=ELLIPSE('',#99600,0.0274999792018231,0.0194466400235278);
#258=ELLIPSE('',#99602,0.0274999792018028,0.0194466400235229);
#259=ELLIPSE('',#99604,0.0274999792018038,0.019446640023523);
#260=ELLIPSE('',#99606,0.0274999792018027,0.0194466400235246);
#261=ELLIPSE('',#99608,0.0274999792018087,0.0194466400235226);
#262=ELLIPSE('',#99610,0.027499979201824,0.0194466400235279);
#263=ELLIPSE('',#99612,0.0274999792018275,0.0194466400235301);
#264=ELLIPSE('',#99614,0.0274999792018072,0.019446640023524);
#265=ELLIPSE('',#99616,0.0274999792018082,0.0194466400235244);
#266=ELLIPSE('',#99618,0.0274999792018318,0.0194466400235293);
#267=ELLIPSE('',#99620,0.0274999792017886,0.0194466400235195);
#268=ELLIPSE('',#99622,0.0274999792018619,0.0194466400235365);
#269=ELLIPSE('',#99624,0.0274999792018085,0.0194466400235243);
#270=ELLIPSE('',#99626,0.0274999792018058,0.0194466400235241);
#271=ELLIPSE('',#99628,0.0274999792018022,0.0194466400235246);
#272=ELLIPSE('',#99630,0.02749997920182,0.0194466400235268);
#273=ELLIPSE('',#99632,0.0274999792017819,0.0194466400235169);
#274=ELLIPSE('',#99634,0.0274999792018284,0.0194466400235286);
#275=ELLIPSE('',#99636,0.0274999792018055,0.0194466400235254);
#276=ELLIPSE('',#99638,0.0274999792018053,0.0194466400235236);
#277=ELLIPSE('',#99640,0.0274999792018291,0.0194466400235292);
#278=ELLIPSE('',#99642,0.0274999792018261,0.0194466400235284);
#279=ELLIPSE('',#99644,0.0274999792018197,0.0194466400235282);
#280=ELLIPSE('',#99646,0.0274999792018074,0.0194466400235247);
#281=ELLIPSE('',#99648,0.0274999792018118,0.0194466400235253);
#282=ELLIPSE('',#99650,0.0274999792018347,0.0194466400235298);
#283=ELLIPSE('',#99652,0.0274999792017871,0.0194466400235192);
#284=ELLIPSE('',#99654,0.0274999792018461,0.0194466400235328);
#285=ELLIPSE('',#99656,0.0274999792018429,0.0194466400235337);
#286=ELLIPSE('',#99658,0.0274999792018179,0.0194466400235262);
#287=ELLIPSE('',#99660,0.0274999792018226,0.0194466400235276);
#288=ELLIPSE('',#99662,0.0274999792018338,0.0194466400235298);
#289=ELLIPSE('',#99664,0.027499979201791,0.0194466400235187);
#290=ELLIPSE('',#99666,0.0274999792018158,0.0194466400235259);
#291=ELLIPSE('',#99668,0.0274999792018309,0.0194466400235295);
#292=ELLIPSE('',#99670,0.0274999792018025,0.0194466400235224);
#293=ELLIPSE('',#99672,0.0274999792018289,0.0194466400235288);
#294=ELLIPSE('',#99674,0.0274999792018066,0.0194466400235238);
#295=ELLIPSE('',#99676,0.027499979201837,0.0194466400235302);
#296=ELLIPSE('',#99682,0.0377939546271109,0.0250703601820978);
#297=ELLIPSE('',#99684,0.0378695219465235,0.0250983059764406);
#298=ELLIPSE('',#99686,0.0377939546270395,0.0250703601820702);
#299=ELLIPSE('',#99688,0.037869521946444,0.0250983059764107);
#300=ELLIPSE('',#99690,0.0377939546272685,0.0250703601821445);
#301=ELLIPSE('',#99692,0.0378695219466119,0.0250983059764672);
#302=ELLIPSE('',#99694,0.0377939546269576,0.0250703601820378);
#303=ELLIPSE('',#99696,0.0378695219464082,0.0250983059763933);
#304=ELLIPSE('',#99698,0.0377939546267997,0.0250703601819834);
#305=ELLIPSE('',#99700,0.0378695219464645,0.0250983059764194);
#306=ELLIPSE('',#99702,0.0377939546267974,0.0250703601819848);
#307=ELLIPSE('',#99704,0.0378695219466849,0.0250983059764935);
#308=ELLIPSE('',#99706,0.0377939546269491,0.0250703601820439);
#309=ELLIPSE('',#99708,0.0378695219464801,0.0250983059764239);
#310=ELLIPSE('',#99710,0.0377939546268274,0.0250703601820047);
#311=ELLIPSE('',#99712,0.0378695219465395,0.0250983059764457);
#312=ELLIPSE('',#99714,0.0377939546270607,0.0250703601820776);
#313=ELLIPSE('',#99716,0.0378695219463676,0.02509830597638);
#314=ELLIPSE('',#99718,0.0377939546270672,0.0250703601820751);
#315=ELLIPSE('',#99720,0.0378695219465767,0.0250983059764549);
#316=ELLIPSE('',#99722,0.0377939546270847,0.0250703601820898);
#317=ELLIPSE('',#99724,0.0378695219463306,0.0250983059763689);
#318=ELLIPSE('',#99726,0.0377939546271058,0.0250703601820951);
#319=ELLIPSE('',#99728,0.0378695219463806,0.0250983059763838);
#320=ELLIPSE('',#99730,0.0377939546273992,0.0250703601821958);
#321=ELLIPSE('',#99732,0.0378695219463341,0.0250983059763734);
#322=ELLIPSE('',#99734,0.0377939546267671,0.0250703601819788);
#323=ELLIPSE('',#99736,0.0378695219467491,0.0250983059765119);
#324=ELLIPSE('',#99738,0.037793954627011,0.0250703601820574);
#325=ELLIPSE('',#99740,0.0378695219464796,0.0250983059764208);
#326=ELLIPSE('',#99742,0.0377939546271938,0.0250703601821272);
#327=ELLIPSE('',#99744,0.0378695219464403,0.0250983059764047);
#328=ELLIPSE('',#99746,0.0377939546272078,0.0250703601821293);
#329=ELLIPSE('',#99748,0.0378695219462217,0.0250983059763317);
#330=ELLIPSE('',#99750,0.0377939546274431,0.0250703601822155);
#331=ELLIPSE('',#99752,0.0378695219465727,0.025098305976455);
#332=ELLIPSE('',#99754,0.0377939546272413,0.0250703601821465);
#333=ELLIPSE('',#99756,0.0378695219465893,0.0250983059764576);
#334=ELLIPSE('',#99758,0.0377939546268262,0.0250703601819944);
#335=ELLIPSE('',#99760,0.037869521946427,0.0250983059763988);
#336=ELLIPSE('',#99762,0.0377939546267704,0.0250703601819765);
#337=ELLIPSE('',#99764,0.0378695219464597,0.0250983059764122);
#338=ELLIPSE('',#99766,0.0377939546267808,0.0250703601819798);
#339=ELLIPSE('',#99768,0.0378695219460054,0.025098305976261);
#340=ELLIPSE('',#99770,0.0377939546271222,0.0250703601820998);
#341=ELLIPSE('',#99772,0.0378695219467645,0.0250983059765208);
#342=ELLIPSE('',#99774,0.0377939546272981,0.025070360182163);
#343=ELLIPSE('',#99776,0.0378695219464416,0.0250983059764082);
#344=ELLIPSE('',#99778,0.0377939546270981,0.0250703601820953);
#345=ELLIPSE('',#99780,0.0378695219463879,0.0250983059763866);
#346=ELLIPSE('',#99782,0.0377939546269133,0.0250703601820331);
#347=ELLIPSE('',#99784,0.03786952194643,0.0250983059764058);
#348=ELLIPSE('',#99786,0.037793954627311,0.0250703601821679);
#349=ELLIPSE('',#99788,0.0378695219464575,0.0250983059764103);
#350=ELLIPSE('',#99790,0.037793954626787,0.0250703601819827);
#351=ELLIPSE('',#99792,0.0378695219465744,0.0250983059764543);
#352=ELLIPSE('',#99794,0.037793954627,0.0250703601820628);
#353=ELLIPSE('',#99796,0.0378695219464972,0.0250983059764296);
#354=ELLIPSE('',#99798,0.0377939546271824,0.0250703601821208);
#355=ELLIPSE('',#99800,0.0378695219463181,0.0250983059763621);
#356=ELLIPSE('',#99802,0.0377939546270806,0.02507036018209);
#357=ELLIPSE('',#99804,0.0378695219464793,0.025098305976419);
#358=ELLIPSE('',#99806,0.0377939546271536,0.0250703601821112);
#359=ELLIPSE('',#99808,0.0378695219464171,0.0250983059764114);
#360=ELLIPSE('',#99810,0.0377939546268865,0.0250703601820144);
#361=ELLIPSE('',#99812,0.0378695219466686,0.0250983059764919);
#362=ELLIPSE('',#99814,0.0377939546269507,0.0250703601820383);
#363=ELLIPSE('',#99816,0.0378695219467058,0.0250983059764957);
#364=ELLIPSE('',#99818,0.0377939546272764,0.0250703601821624);
#365=ELLIPSE('',#99820,0.0378695219461522,0.0250983059763082);
#366=ELLIPSE('',#99822,0.0377939546272405,0.0250703601821427);
#367=ELLIPSE('',#99824,0.0378695219465727,0.0250983059764577);
#368=ELLIPSE('',#99826,0.0377939546272697,0.0250703601821556);
#369=ELLIPSE('',#99828,0.0378695219465898,0.0250983059764639);
#370=ELLIPSE('',#99830,0.0377939546271452,0.0250703601821021);
#371=ELLIPSE('',#99832,0.0378695219464919,0.0250983059764311);
#372=ELLIPSE('',#99834,0.0377939546270735,0.0250703601820848);
#373=ELLIPSE('',#99836,0.0378695219467591,0.0250983059765092);
#374=ELLIPSE('',#99838,0.0377939546272653,0.0250703601821518);
#375=ELLIPSE('',#99840,0.0378695219467233,0.0250983059764915);
#376=ELLIPSE('',#99842,0.0377939546271496,0.0250703601821116);
#377=ELLIPSE('',#99844,0.037869521946483,0.0250983059764293);
#378=ELLIPSE('',#99846,0.0377939546268239,0.0250703601819968);
#379=ELLIPSE('',#99848,0.0378695219468845,0.0250983059765543);
#380=ELLIPSE('',#99850,0.0377939546266337,0.0250703601819282);
#381=ELLIPSE('',#99852,0.0378695219461948,0.0250983059763309);
#382=ELLIPSE('',#99854,0.0377939546269812,0.025070360182053);
#383=ELLIPSE('',#99856,0.0378695219463886,0.0250983059763826);
#384=ELLIPSE('',#99858,0.037793954627197,0.025070360182132);
#385=ELLIPSE('',#99860,0.0378695219465481,0.0250983059764459);
#386=ELLIPSE('',#99862,0.0377939546267804,0.0250703601819784);
#387=ELLIPSE('',#99864,0.0378695219459524,0.0250983059762446);
#388=ELLIPSE('',#99866,0.0377939546270476,0.0250703601820695);
#389=ELLIPSE('',#99868,0.0378695219469002,0.0250983059765617);
#390=ELLIPSE('',#99870,0.0377939546271249,0.0250703601820983);
#391=ELLIPSE('',#99872,0.037869521946226,0.0250983059763336);
#392=ELLIPSE('',#99874,0.0377939546270712,0.0250703601820862);
#393=ELLIPSE('',#99876,0.0378695219466723,0.0250983059764892);
#394=ELLIPSE('',#99879,0.0377939546273518,0.0250703601821778);
#395=ELLIPSE('',#99881,0.037869521947147,0.0250983059766503);
#396=ELLIPSE('',#99883,0.0377939546273672,0.0250703601821858);
#397=ELLIPSE('',#99885,0.0378695219471249,0.0250983059766443);
#398=ELLIPSE('',#99887,0.0377939546272684,0.0250703601821527);
#399=ELLIPSE('',#99889,0.0378695219465376,0.0250983059764453);
#400=ELLIPSE('',#99891,0.0377939546267177,0.0250703601819543);
#401=ELLIPSE('',#99893,0.0378695219465633,0.0250983059764556);
#402=ELLIPSE('',#99895,0.0377939546267279,0.0250703601819634);
#403=ELLIPSE('',#99897,0.0378695219465408,0.0250983059764424);
#404=ELLIPSE('',#99899,0.0377939546271458,0.0250703601821111);
#405=ELLIPSE('',#99901,0.037869521946556,0.0250983059764535);
#406=ELLIPSE('',#99903,0.0377939546272391,0.0250703601821381);
#407=ELLIPSE('',#99905,0.0378695219461841,0.0250983059763208);
#408=ELLIPSE('',#99907,0.0377939546271602,0.0250703601821172);
#409=ELLIPSE('',#99909,0.0378695219469737,0.0250983059765869);
#410=ELLIPSE('',#99911,0.0377939546268286,0.025070360181992);
#411=ELLIPSE('',#99913,0.0378695219464023,0.0250983059763922);
#412=ELLIPSE('',#99915,0.0377939546271851,0.0250703601821223);
#413=ELLIPSE('',#99917,0.0378695219460789,0.0250983059762906);
#414=ELLIPSE('',#99919,0.037793954627282,0.0250703601821508);
#415=ELLIPSE('',#99921,0.0378695219465084,0.0250983059764242);
#416=ELLIPSE('',#99923,0.0377939546267815,0.0250703601819804);
#417=ELLIPSE('',#99925,0.0378695219463702,0.0250983059763883);
#418=ELLIPSE('',#99927,0.0377939546265622,0.025070360181903);
#419=ELLIPSE('',#99929,0.0378695219464024,0.0250983059764034);
#420=ELLIPSE('',#99931,0.0377939546270649,0.0250703601820832);
#421=ELLIPSE('',#99933,0.037869521946096,0.0250983059762913);
#422=ELLIPSE('',#99935,0.0377939546270451,0.0250703601820666);
#423=ELLIPSE('',#99937,0.0378695219465469,0.0250983059764424);
#424=ELLIPSE('',#99939,0.0377939546274933,0.025070360182228);
#425=ELLIPSE('',#99941,0.0378695219459719,0.0250983059762507);
#426=ELLIPSE('',#99943,0.037793954626721,0.0250703601819633);
#427=ELLIPSE('',#99945,0.0378695219467833,0.0250983059765231);
#428=ELLIPSE('',#99947,0.0377939546272019,0.0250703601821268);
#429=ELLIPSE('',#99949,0.0378695219465463,0.0250983059764481);
#430=ELLIPSE('',#99951,0.0377939546273632,0.0250703601821844);
#431=ELLIPSE('',#99953,0.0378695219468885,0.0250983059765562);
#432=ELLIPSE('',#99955,0.0377939546272644,0.0250703601821503);
#433=ELLIPSE('',#99957,0.0378695219465198,0.0250983059764359);
#434=ELLIPSE('',#99959,0.0377939546270628,0.025070360182078);
#435=ELLIPSE('',#99961,0.0378695219461977,0.02509830597633);
#436=ELLIPSE('',#99963,0.0377939546271482,0.0250703601821143);
#437=ELLIPSE('',#99965,0.0378695219465306,0.0250983059764382);
#438=ELLIPSE('',#99967,0.0377939546267965,0.0250703601819846);
#439=ELLIPSE('',#99969,0.0378695219466369,0.0250983059764776);
#440=ELLIPSE('',#99971,0.0377939546272131,0.0250703601821351);
#441=ELLIPSE('',#99973,0.0378695219464218,0.0250983059764017);
#442=ELLIPSE('',#99975,0.0377939546270981,0.0250703601820953);
#443=ELLIPSE('',#99977,0.0378695219460318,0.0250983059762701);
#444=ELLIPSE('',#99979,0.0377939546271911,0.0250703601821247);
#445=ELLIPSE('',#99981,0.0378695219466486,0.0250983059764816);
#446=ELLIPSE('',#99983,0.0377939546272545,0.0250703601821443);
#447=ELLIPSE('',#99985,0.0378695219464022,0.0250983059763928);
#448=ELLIPSE('',#99987,0.0377939546270471,0.0250703601820705);
#449=ELLIPSE('',#99989,0.0378695219464218,0.025098305976405);
#450=ELLIPSE('',#99991,0.037793954627098,0.0250703601820907);
#451=ELLIPSE('',#99993,0.03786952194662,0.0250983059764673);
#452=ELLIPSE('',#99995,0.0377939546268382,0.0250703601819987);
#453=ELLIPSE('',#99997,0.0378695219465927,0.0250983059764667);
#454=ELLIPSE('',#99999,0.0377939546271273,0.0250703601821041);
#455=ELLIPSE('',#100001,0.0378695219461789,0.0250983059763172);
#456=ELLIPSE('',#100003,0.0377939546268529,0.0250703601820112);
#457=ELLIPSE('',#100005,0.0378695219465492,0.0250983059764485);
#458=ELLIPSE('',#100007,0.0377939546268233,0.0250703601819974);
#459=ELLIPSE('',#100009,0.0378695219464527,0.0250983059764105);
#460=ELLIPSE('',#100011,0.0377939546267064,0.0250703601819536);
#461=ELLIPSE('',#100013,0.0378695219465347,0.0250983059764463);
#462=ELLIPSE('',#100015,0.0377939546271184,0.0250703601820973);
#463=ELLIPSE('',#100017,0.0378695219464462,0.0250983059764076);
#464=ELLIPSE('',#100019,0.0377939546269241,0.0250703601820279);
#465=ELLIPSE('',#100021,0.037869521946493,0.0250983059764276);
#466=ELLIPSE('',#100023,0.0377939546272981,0.025070360182169);
#467=ELLIPSE('',#100025,0.037869521946465,0.0250983059764108);
#468=ELLIPSE('',#100027,0.037793954627171,0.0250703601821197);
#469=ELLIPSE('',#100029,0.0378695219462166,0.0250983059763296);
#470=ELLIPSE('',#100031,0.0377939546272262,0.0250703601821393);
#471=ELLIPSE('',#100033,0.0378695219463891,0.0250983059763892);
#472=ELLIPSE('',#100035,0.0377939546270739,0.0250703601820887);
#473=ELLIPSE('',#100037,0.0378695219466546,0.0250983059764808);
#474=ELLIPSE('',#100039,0.0377939546270089,0.0250703601820585);
#475=ELLIPSE('',#100041,0.0378695219463441,0.0250983059763761);
#476=ELLIPSE('',#100043,0.0377939546270472,0.0250703601820732);
#477=ELLIPSE('',#100045,0.0378695219463518,0.0250983059763784);
#478=ELLIPSE('',#100047,0.0377939546271573,0.0250703601821169);
#479=ELLIPSE('',#100049,0.0378695219466952,0.0250983059764971);
#480=ELLIPSE('',#100051,0.0377939546271577,0.0250703601821112);
#481=ELLIPSE('',#100053,0.0378695219462776,0.0250983059763517);
#482=ELLIPSE('',#100055,0.0377939546271348,0.0250703601821107);
#483=ELLIPSE('',#100057,0.0378695219464613,0.0250983059764109);
#484=ELLIPSE('',#100059,0.0377939546271653,0.0250703601821089);
#485=ELLIPSE('',#100061,0.0378695219465757,0.0250983059764537);
#486=ELLIPSE('',#100063,0.0377939546272274,0.0250703601821409);
#487=ELLIPSE('',#100065,0.0378695219463364,0.0250983059763705);
#488=ELLIPSE('',#100067,0.0377939546269824,0.0250703601820482);
#489=ELLIPSE('',#100069,0.0378695219463565,0.0250983059763739);
#490=ELLIPSE('',#100071,0.0377939546272586,0.0250703601821497);
#491=ELLIPSE('',#100073,0.037869521946479,0.0250983059764217);
#492=ELLIPSE('',#100075,0.0594717522093815,0.0552292627679723);
#493=ELLIPSE('',#100076,0.0523574408941029,0.0489195958911169);
#494=ELLIPSE('',#100078,0.0523574408930336,0.048919595889694);
#495=ELLIPSE('',#100079,0.0594717522063949,0.0552292627663424);
#496=ELLIPSE('',#100081,0.059471752210527,0.0552292627685546);
#497=ELLIPSE('',#100082,0.0523574408933772,0.0489195958901572);
#498=ELLIPSE('',#100084,0.0594717522080122,0.0552292627672104);
#499=ELLIPSE('',#100085,0.0523574408945968,0.0489195958918944);
#500=ELLIPSE('',#100087,0.0594717522099653,0.0552292627682868);
#501=ELLIPSE('',#100088,0.0523574408935738,0.0489195958903706);
#502=ELLIPSE('',#100090,0.0594717522071289,0.0552292627667538);
#503=ELLIPSE('',#100091,0.0523574408941314,0.0489195958911761);
#504=ELLIPSE('',#100093,0.0594717522078325,0.0552292627671278);
#505=ELLIPSE('',#100094,0.0523574408930899,0.0489195958898256);
#506=ELLIPSE('',#100096,0.0594717522074437,0.0552292627669329);
#507=ELLIPSE('',#100097,0.0523574408948173,0.0489195958920454);
#508=ELLIPSE('',#100099,0.0594717522075256,0.0552292627669854);
#509=ELLIPSE('',#100100,0.0523574408932733,0.0489195958900324);
#510=ELLIPSE('',#100102,0.0594717522088852,0.0552292627677376);
#511=ELLIPSE('',#100103,0.0523574408934708,0.0489195958902787);
#512=ELLIPSE('',#100105,0.0594717522104183,0.0552292627685669);
#513=ELLIPSE('',#100106,0.0523574408933491,0.0489195958901329);
#514=ELLIPSE('',#100108,0.059471752206937,0.0552292627666515);
#515=ELLIPSE('',#100109,0.0523574408941294,0.0489195958912471);
#516=ELLIPSE('',#100111,0.0594717522082379,0.055229262767351);
#517=ELLIPSE('',#100112,0.052357440893126,0.0489195958898559);
#518=ELLIPSE('',#100114,0.0594717522082644,0.0552292627674078);
#519=ELLIPSE('',#100115,0.0523574408934445,0.0489195958902684);
#520=ELLIPSE('',#100117,0.0594717522068689,0.0552292627666162);
#521=ELLIPSE('',#100118,0.0523574408922878,0.0489195958887345);
#522=ELLIPSE('',#100120,0.0594717522080172,0.055229262767222);
#523=ELLIPSE('',#100121,0.0523574408943491,0.0489195958914509);
#524=ELLIPSE('',#100123,0.0594717522070147,0.055229262766697);
#525=ELLIPSE('',#100124,0.0523574408928524,0.0489195958894166);
#526=ELLIPSE('',#100126,0.059471752206359,0.0552292627663632);
#527=ELLIPSE('',#100127,0.0523574408936573,0.0489195958905023);
#528=ELLIPSE('',#100129,0.0594717522080242,0.0552292627672641);
#529=ELLIPSE('',#100130,0.0523574408925724,0.0489195958890778);
#530=ELLIPSE('',#100132,0.0594717522087728,0.0552292627676604);
#531=ELLIPSE('',#100133,0.0523574408942549,0.0489195958913365);
#532=ELLIPSE('',#100135,0.0594717522117556,0.0552292627692794);
#533=ELLIPSE('',#100136,0.0523574408925802,0.0489195958890979);
#534=ELLIPSE('',#100138,0.0594717522092905,0.055229262767912);
#535=ELLIPSE('',#100139,0.0523574408935547,0.0489195958904525);
#536=ELLIPSE('',#100141,0.0594717522079891,0.0552292627672496);
#537=ELLIPSE('',#100142,0.0523574408925326,0.0489195958890156);
#538=ELLIPSE('',#100144,0.059471752209349,0.05522926276795);
#539=ELLIPSE('',#100145,0.0523574408931156,0.048919595889817);
#540=ELLIPSE('',#100147,0.0594717522060788,0.0552292627661841);
#541=ELLIPSE('',#100148,0.0523574408937248,0.0489195958905856);
#542=ELLIPSE('',#100150,0.0594717522076025,0.0552292627670435);
#543=ELLIPSE('',#100151,0.0523574408931184,0.0489195958898577);
#544=ELLIPSE('',#100153,0.0594717522085552,0.0552292627675089);
#545=ELLIPSE('',#100154,0.0523574408942864,0.0489195958914513);
#546=ELLIPSE('',#100156,0.0594717522095339,0.0552292627680599);
#547=ELLIPSE('',#100157,0.0523574408933161,0.0489195958900139);
#548=ELLIPSE('',#100159,0.0594717522094596,0.0552292627679749);
#549=ELLIPSE('',#100160,0.0523574408929958,0.0489195958896259);
#550=ELLIPSE('',#100162,0.0594717522107856,0.0552292627686926);
#551=ELLIPSE('',#100163,0.052357440893669,0.0489195958905554);
#552=ELLIPSE('',#100165,0.059471752207577,0.0552292627670372);
#553=ELLIPSE('',#100166,0.0523574408935437,0.0489195958903441);
#554=ELLIPSE('',#100168,0.0594717522095802,0.0552292627680481);
#555=ELLIPSE('',#100169,0.0523574408924447,0.0489195958888946);
#556=ELLIPSE('',#100171,0.0594717522083012,0.0552292627673983);
#557=ELLIPSE('',#100172,0.052357440892708,0.0489195958892621);
#558=ELLIPSE('',#100174,0.0594717522076934,0.0552292627670944);
#559=ELLIPSE('',#100175,0.0523574408938724,0.0489195958907808);
#560=ELLIPSE('',#100177,0.0594717522081998,0.0552292627673637);
#561=ELLIPSE('',#100178,0.0523574408925381,0.0489195958889725);
#562=ELLIPSE('',#100180,0.0594717522060484,0.0552292627661945);
#563=ELLIPSE('',#100181,0.0523574408917811,0.0489195958880099);
#564=ELLIPSE('',#100183,0.0594717522096474,0.0552292627681111);
#565=ELLIPSE('',#100184,0.0523574408933097,0.0489195958901172);
#566=ELLIPSE('',#100186,0.0594717522073831,0.0552292627668932);
#567=ELLIPSE('',#100187,0.0523574408935224,0.0489195958904008);
#568=ELLIPSE('',#100189,0.0594717522078441,0.0552292627671437);
#569=ELLIPSE('',#100190,0.0523574408939627,0.0489195958908927);
#570=ELLIPSE('',#100192,0.0594717522112087,0.0552292627689124);
#571=ELLIPSE('',#100193,0.0523574408926999,0.0489195958892166);
#572=ELLIPSE('',#100195,0.0594717522077727,0.0552292627671321);
#573=ELLIPSE('',#100196,0.0523574408945673,0.0489195958917693);
#574=ELLIPSE('',#100198,0.0594717522067864,0.0552292627665967);
#575=ELLIPSE('',#100199,0.052357440893046,0.048919595889673);
#576=ELLIPSE('',#100201,0.0594717522070521,0.0552292627667294);
#577=ELLIPSE('',#100202,0.052357440893711,0.0489195958906244);
#578=ELLIPSE('',#100204,0.0594717522074139,0.055229262766935);
#579=ELLIPSE('',#100205,0.0523574408936527,0.0489195958906036);
#580=ELLIPSE('',#100207,0.0594717522106702,0.0552292627686464);
#581=ELLIPSE('',#100208,0.0523574408925687,0.0489195958890896);
#582=ELLIPSE('',#100210,0.0594717522061032,0.0552292627662244);
#583=ELLIPSE('',#100211,0.0523574408933305,0.0489195958901204);
#584=ELLIPSE('',#100213,0.0594717522078377,0.0552292627671592);
#585=ELLIPSE('',#100214,0.0523574408934019,0.0489195958902017);
#586=ELLIPSE('',#100216,0.0594717522095676,0.0552292627680807);
#587=ELLIPSE('',#100217,0.0523574408935074,0.048919595890387);
#588=ELLIPSE('',#100219,0.0594717522063091,0.0552292627662996);
#589=ELLIPSE('',#100220,0.0523574408934654,0.0489195958902804);
#590=ELLIPSE('',#100222,0.0594717522078024,0.055229262767126);
#591=ELLIPSE('',#100223,0.0523574408931717,0.048919595889865);
#592=ELLIPSE('',#100225,0.0594717522062108,0.0552292627662818);
#593=ELLIPSE('',#100226,0.0523574408944596,0.048919595891611);
#594=ELLIPSE('',#100228,0.0594717522059097,0.055229262766132);
#595=ELLIPSE('',#100229,0.0523574408929005,0.0489195958895422);
#596=ELLIPSE('',#100231,0.0594717522087653,0.0552292627676661);
#597=ELLIPSE('',#100232,0.052357440892832,0.0489195958893877);
#598=ELLIPSE('',#100234,0.0594717522108721,0.0552292627687884);
#599=ELLIPSE('',#100235,0.0523574408940629,0.0489195958911095);
#600=ELLIPSE('',#100237,0.0594717522082771,0.0552292627674181);
#601=ELLIPSE('',#100238,0.0523574408928738,0.0489195958895351);
#602=ELLIPSE('',#100240,0.0594717522078313,0.0552292627671469);
#603=ELLIPSE('',#100241,0.0523574408941011,0.0489195958911154);
#604=ELLIPSE('',#100243,0.0594717522081063,0.0552292627673198);
#605=ELLIPSE('',#100244,0.0523574408937338,0.0489195958906628);
#606=ELLIPSE('',#100246,0.0594717522056887,0.0552292627659561);
#607=ELLIPSE('',#100247,0.0523574408928622,0.0489195958894712);
#608=ELLIPSE('',#100249,0.0594717522088224,0.0552292627677157);
#609=ELLIPSE('',#100250,0.0523574408944811,0.0489195958916444);
#610=ELLIPSE('',#100252,0.0594717522089922,0.0552292627677814);
#611=ELLIPSE('',#100253,0.0523574408947637,0.0489195958920602);
#612=ELLIPSE('',#100255,0.0594717522120167,0.0552292627693562);
#613=ELLIPSE('',#100256,0.0523574408934261,0.0489195958901972);
#614=ELLIPSE('',#100258,0.0594717522125058,0.0552292627696656);
#615=ELLIPSE('',#100259,0.052357440893374,0.048919595890127);
#616=ELLIPSE('',#100261,0.0594717522094242,0.0552292627680217);
#617=ELLIPSE('',#100262,0.0523574408935378,0.0489195958903875);
#618=ELLIPSE('',#100264,0.0594717522087569,0.0552292627676444);
#619=ELLIPSE('',#100265,0.052357440892614,0.0489195958891282);
#620=ELLIPSE('',#100267,0.0594717522092211,0.0552292627678974);
#621=ELLIPSE('',#100268,0.0523574408936857,0.0489195958905767);
#622=ELLIPSE('',#100270,0.0523574408929943,0.0489195958897697);
#623=ELLIPSE('',#100271,0.0594717522085673,0.0552292627675639);
#624=ELLIPSE('',#100273,0.0523574408939794,0.0489195958909905);
#625=ELLIPSE('',#100274,0.0594717522101173,0.0552292627683671);
#626=ELLIPSE('',#100276,0.052357440892821,0.0489195958893363);
#627=ELLIPSE('',#100277,0.0594717522076746,0.0552292627670676);
#628=ELLIPSE('',#100279,0.0523574408943176,0.048919595891439);
#629=ELLIPSE('',#100280,0.0594717522097422,0.0552292627682068);
#630=ELLIPSE('',#100282,0.0523574408948324,0.0489195958921146);
#631=ELLIPSE('',#100283,0.0594717522092244,0.0552292627678736);
#632=ELLIPSE('',#100285,0.0523574408928958,0.0489195958894956);
#633=ELLIPSE('',#100286,0.059471752209436,0.0552292627679566);
#634=ELLIPSE('',#100288,0.0523574408927136,0.0489195958892958);
#635=ELLIPSE('',#100289,0.0594717522101865,0.0552292627683888);
#636=ELLIPSE('',#100291,0.0523574408933246,0.0489195958900545);
#637=ELLIPSE('',#100292,0.0594717522084889,0.0552292627675033);
#638=ELLIPSE('',#100294,0.0523574408929252,0.0489195958895466);
#639=ELLIPSE('',#100295,0.0594717522067242,0.0552292627665378);
#640=ELLIPSE('',#100297,0.0523574408935323,0.0489195958904197);
#641=ELLIPSE('',#100298,0.0594717522084362,0.0552292627674681);
#642=ELLIPSE('',#100300,0.0523574408934523,0.048919595890263);
#643=ELLIPSE('',#100301,0.0594717522090756,0.0552292627677804);
#644=ELLIPSE('',#100303,0.052357440893078,0.0489195958897325);
#645=ELLIPSE('',#100304,0.0594717522116622,0.055229262769157);
#646=ELLIPSE('',#100306,0.0523574408933239,0.0489195958901453);
#647=ELLIPSE('',#100307,0.0594717522098756,0.0552292627682184);
#648=ELLIPSE('',#100309,0.0523574408931826,0.0489195958898953);
#649=ELLIPSE('',#100310,0.05947175220972,0.0552292627681239);
#650=ELLIPSE('',#100312,0.0523574408929838,0.0489195958896346);
#651=ELLIPSE('',#100313,0.0594717522045155,0.0552292627653588);
#652=ELLIPSE('',#100315,0.0523574408926991,0.0489195958892291);
#653=ELLIPSE('',#100316,0.0594717522098512,0.0552292627682459);
#654=ELLIPSE('',#100318,0.0523574408937797,0.0489195958907056);
#655=ELLIPSE('',#100319,0.0594717522087746,0.0552292627676573);
#656=ELLIPSE('',#100321,0.0523574408945519,0.0489195958917232);
#657=ELLIPSE('',#100322,0.0594717522092935,0.0552292627679665);
#658=ELLIPSE('',#100324,0.0523574408931019,0.0489195958897895);
#659=ELLIPSE('',#100325,0.059471752208446,0.0552292627674902);
#660=ELLIPSE('',#100327,0.0523574408941714,0.0489195958912245);
#661=ELLIPSE('',#100328,0.0594717522091084,0.0552292627678568);
#662=ELLIPSE('',#100330,0.0523574408940044,0.0489195958909118);
#663=ELLIPSE('',#100331,0.0594717522068734,0.0552292627666293);
#664=ELLIPSE('',#100333,0.0523574408937834,0.0489195958907224);
#665=ELLIPSE('',#100334,0.0594717522098918,0.0552292627682498);
#666=ELLIPSE('',#100336,0.0523574408935842,0.0489195958904222);
#667=ELLIPSE('',#100337,0.0594717522076412,0.0552292627670567);
#668=ELLIPSE('',#100339,0.0523574408937256,0.0489195958906133);
#669=ELLIPSE('',#100340,0.0594717522070184,0.0552292627667054);
#670=ELLIPSE('',#100342,0.0523574408927693,0.0489195958892124);
#671=ELLIPSE('',#100343,0.0594717522081041,0.0552292627672715);
#672=ELLIPSE('',#100345,0.0523574408933158,0.0489195958900367);
#673=ELLIPSE('',#100346,0.0594717522063655,0.0552292627663595);
#674=ELLIPSE('',#100348,0.0523574408935146,0.0489195958902675);
#675=ELLIPSE('',#100349,0.0594717522087871,0.0552292627676304);
#676=ELLIPSE('',#100351,0.0523574408942678,0.0489195958913386);
#677=ELLIPSE('',#100352,0.0594717522065507,0.0552292627664879);
#678=ELLIPSE('',#100354,0.0523574408935429,0.0489195958904555);
#679=ELLIPSE('',#100355,0.0594717522103784,0.0552292627684482);
#680=ELLIPSE('',#100357,0.0523574408931172,0.0489195958897559);
#681=ELLIPSE('',#100358,0.0594717522069347,0.0552292627666673);
#682=ELLIPSE('',#100360,0.0523574408936834,0.0489195958906288);
#683=ELLIPSE('',#100361,0.0594717522080242,0.0552292627672641);
#684=ELLIPSE('',#100363,0.059471752207151,0.0552292627668208);
#685=ELLIPSE('',#100364,0.0523574408926382,0.0489195958891156);
#686=ELLIPSE('',#100368,0.0496327928416145,0.0434076000955403);
#687=ELLIPSE('',#100370,0.0425526869750752,0.039014288226265);
#688=ELLIPSE('',#100383,0.0594717522070795,0.0552292627667962);
#689=ELLIPSE('',#100384,0.0523574408936573,0.0489195958905023);
#690=ELLIPSE('',#100402,0.0192307675635318,0.0124961950671783);
#691=ELLIPSE('',#100406,0.0192307675634953,0.0124961950670989);
#692=ELLIPSE('',#100418,0.0425526869738727,0.0390142882252431);
#693=ELLIPSE('',#100420,0.0496327928421636,0.0434076000958099);
#694=ELLIPSE('',#100423,0.0192307675634341,0.0124961950670948);
#695=ELLIPSE('',#100424,0.0192307675633307,0.0124961950669426);
#696=ELLIPSE('',#100441,0.0425526869750512,0.0390142882262157);
#697=ELLIPSE('',#100443,0.0496327928428896,0.0434076000962082);
#698=ELLIPSE('',#100446,0.0192307675634649,0.0124961950671064);
#699=ELLIPSE('',#100447,0.0192307675632899,0.0124961950669237);
#700=ELLIPSE('',#100464,0.0425526869732722,0.0390142882247097);
#701=ELLIPSE('',#100466,0.0496327928411177,0.0434076000953248);
#702=ELLIPSE('',#100469,0.0192307675635973,0.0124961950671957);
#703=ELLIPSE('',#100470,0.0192307675633788,0.0124961950669941);
#704=ELLIPSE('',#100487,0.042552686974379,0.0390142882257283);
#705=ELLIPSE('',#100489,0.0496327928396385,0.0434076000945822);
#706=ELLIPSE('',#100492,0.0192307675633234,0.0124961950669785);
#707=ELLIPSE('',#100493,0.0192307675635267,0.0124961950671152);
#708=ELLIPSE('',#100510,0.0425526869749281,0.0390142882261518);
#709=ELLIPSE('',#100512,0.0496327928406238,0.0434076000950604);
#710=ELLIPSE('',#100515,0.0192307675632406,0.0124961950669363);
#711=ELLIPSE('',#100516,0.0192307675635317,0.0124961950671101);
#712=ELLIPSE('',#100533,0.0425526869741915,0.0390142882254985);
#713=ELLIPSE('',#100535,0.0496327928403701,0.0434076000948868);
#714=ELLIPSE('',#100538,0.0192307675638857,0.0124961950674675);
#715=ELLIPSE('',#100539,0.0192307675637902,0.0124961950673144);
#716=ELLIPSE('',#100556,0.0425526869735336,0.0390142882250337);
#717=ELLIPSE('',#100558,0.0496327928395447,0.0434076000945563);
#718=ELLIPSE('',#100561,0.0192307675636895,0.0124961950672939);
#719=ELLIPSE('',#100562,0.0192307675635296,0.0124961950671171);
#720=ELLIPSE('',#100579,0.0425526869736662,0.0390142882251435);
#721=ELLIPSE('',#100581,0.0496327928443886,0.0434076000968867);
#722=ELLIPSE('',#100584,0.0192307675636211,0.0124961950672701);
#723=ELLIPSE('',#100585,0.0192307675635263,0.0124961950670976);
#724=ELLIPSE('',#100602,0.042552686973854,0.0390142882252422);
#725=ELLIPSE('',#100604,0.049632792838296,0.0434076000939053);
#726=ELLIPSE('',#100607,0.0192307675635304,0.0124961950671889);
#727=ELLIPSE('',#100608,0.0192307675630496,0.0124961950667192);
#728=ELLIPSE('',#100625,0.0425526869739649,0.0390142882253226);
#729=ELLIPSE('',#100627,0.0496327928427627,0.0434076000960995);
#730=ELLIPSE('',#100630,0.0192307675628893,0.0124961950666526);
#731=ELLIPSE('',#100631,0.0192307675635299,0.0124961950671293);
#732=ELLIPSE('',#100648,0.0425526869747805,0.0390142882260044);
#733=ELLIPSE('',#100650,0.049632792841599,0.0434076000955309);
#734=ELLIPSE('',#100653,0.0192307675637578,0.0124961950673562);
#735=ELLIPSE('',#100654,0.0192307675639124,0.012496195067421);
#736=ELLIPSE('',#100671,0.0425526869743715,0.0390142882256719);
#737=ELLIPSE('',#100673,0.0496327928404835,0.043407600094977);
#738=ELLIPSE('',#100676,0.0192307675632384,0.012496195066941);
#739=ELLIPSE('',#100677,0.0192307675635312,0.0124961950671388);
#740=ELLIPSE('',#100694,0.0425526869740824,0.0390142882254308);
#741=ELLIPSE('',#100696,0.0496327928393061,0.0434076000944058);
#742=ELLIPSE('',#100699,0.019230767563583,0.0124961950672037);
#743=ELLIPSE('',#100700,0.0192307675632949,0.0124961950669026);
#744=ELLIPSE('',#100717,0.0425526869744841,0.0390142882257579);
#745=ELLIPSE('',#100719,0.0496327928399138,0.0434076000947192);
#746=ELLIPSE('',#100722,0.0192307675631686,0.0124961950668521);
#747=ELLIPSE('',#100723,0.0192307675635192,0.0124961950671158);
#748=ELLIPSE('',#100740,0.0425526869733499,0.0390142882248535);
#749=ELLIPSE('',#100742,0.0496327928401791,0.0434076000948666);
#750=ELLIPSE('',#100745,0.0192307675633233,0.0124961950669949);
#751=ELLIPSE('',#100746,0.0192307675638509,0.012496195067394);
#752=ELLIPSE('',#100763,0.0425526869753439,0.0390142882264477);
#753=ELLIPSE('',#100765,0.0496327928419698,0.0434076000956947);
#754=ELLIPSE('',#100768,0.0192307675639329,0.0124961950675036);
#755=ELLIPSE('',#100769,0.0192307675637545,0.0124961950673123);
#756=ELLIPSE('',#100786,0.0425526869744145,0.0390142882257717);
#757=ELLIPSE('',#100788,0.0496327928401159,0.0434076000948093);
#758=ELLIPSE('',#100791,0.0192307675636705,0.0124961950673185);
#759=ELLIPSE('',#100792,0.0192307675636708,0.0124961950672442);
#760=ELLIPSE('',#100809,0.0425526869732906,0.0390142882248623);
#761=ELLIPSE('',#100811,0.04963279284165,0.0434076000955818);
#762=ELLIPSE('',#100814,0.0192307675631284,0.012496195066834);
#763=ELLIPSE('',#100815,0.0192307675635161,0.012496195067104);
#764=ELLIPSE('',#100832,0.0425526869746155,0.0390142882259526);
#765=ELLIPSE('',#100834,0.0496327928399284,0.0434076000947457);
#766=ELLIPSE('',#100837,0.019230767563741,0.0124961950673528);
#767=ELLIPSE('',#100838,0.0192307675636219,0.0124961950671777);
#768=ELLIPSE('',#100855,0.0425526869749252,0.0390142882261626);
#769=ELLIPSE('',#100857,0.0496327928407413,0.0434076000951222);
#770=ELLIPSE('',#100860,0.0192307675635523,0.012496195067215);
#771=ELLIPSE('',#100861,0.0192307675633197,0.0124961950669376);
#772=ELLIPSE('',#100878,0.0425526869747909,0.0390142882260437);
#773=ELLIPSE('',#100880,0.0496327928410715,0.043407600095254);
#774=ELLIPSE('',#100883,0.0192307675635571,0.0124961950671645);
#775=ELLIPSE('',#100884,0.0192307675637541,0.0124961950673131);
#776=ELLIPSE('',#100901,0.0425526869737034,0.0390142882252059);
#777=ELLIPSE('',#100903,0.0496327928401919,0.0434076000948428);
#778=ELLIPSE('',#100906,0.0192307675631893,0.0124961950668821);
#779=ELLIPSE('',#100907,0.0192307675632753,0.0124961950669121);
#780=ELLIPSE('',#100924,0.0425526869745075,0.0390142882257448);
#781=ELLIPSE('',#100926,0.0496327928397759,0.0434076000946169);
#782=ELLIPSE('',#100929,0.0192307675634038,0.0124961950670969);
#783=ELLIPSE('',#100930,0.0192307675637935,0.0124961950673019);
#784=ELLIPSE('',#100947,0.0425526869742738,0.0390142882255607);
#785=ELLIPSE('',#100949,0.0496327928432332,0.0434076000963396);
#786=ELLIPSE('',#100952,0.0192307675634102,0.0124961950670913);
#787=ELLIPSE('',#100953,0.019230767563503,0.012496195067078);
#788=ELLIPSE('',#100970,0.0425526869742644,0.0390142882255844);
#789=ELLIPSE('',#100972,0.0496327928394013,0.043407600094468);
#790=ELLIPSE('',#100975,0.0192307675630013,0.0124961950667316);
#791=ELLIPSE('',#100976,0.0192307675636216,0.0124961950672165);
#792=ELLIPSE('',#100993,0.0425526869761727,0.0390142882271604);
#793=ELLIPSE('',#100995,0.0496327928412727,0.0434076000953756);
#794=ELLIPSE('',#100998,0.0192307675631514,0.0124961950668792);
#795=ELLIPSE('',#100999,0.019230767563722,0.0124961950672546);
#796=ELLIPSE('',#101016,0.0425526869747384,0.0390142882259681);
#797=ELLIPSE('',#101018,0.0496327928446237,0.0434076000970921);
#798=ELLIPSE('',#101021,0.0192307675632903,0.0124961950669737);
#799=ELLIPSE('',#101022,0.019230767563666,0.0124961950672293);
#800=ELLIPSE('',#101039,0.0425526869737097,0.0390142882251084);
#801=ELLIPSE('',#101041,0.0496327928425481,0.0434076000960501);
#802=ELLIPSE('',#101044,0.0192307675631588,0.0124961950668712);
#803=ELLIPSE('',#101045,0.0192307675640625,0.0124961950675836);
#804=ELLIPSE('',#101062,0.0425526869745639,0.0390142882258298);
#805=ELLIPSE('',#101064,0.0496327928409908,0.043407600095271);
#806=ELLIPSE('',#101067,0.0192307675634594,0.0124961950671047);
#807=ELLIPSE('',#101068,0.0192307675634831,0.0124961950671005);
#808=ELLIPSE('',#101085,0.0425526869762421,0.0390142882271955);
#809=ELLIPSE('',#101087,0.0496327928398201,0.0434076000947202);
#810=ELLIPSE('',#101090,0.0192307675634189,0.0124961950670756);
#811=ELLIPSE('',#101091,0.0192307675636712,0.0124961950672523);
#812=ELLIPSE('',#101108,0.0425526869751123,0.0390142882263016);
#813=ELLIPSE('',#101110,0.0496327928428975,0.0434076000961352);
#814=ELLIPSE('',#101113,0.0192307675638601,0.0124961950674287);
#815=ELLIPSE('',#101114,0.0192307675633655,0.0124961950669765);
#816=ELLIPSE('',#101131,0.042552686974957,0.039014288226131);
#817=ELLIPSE('',#101133,0.0496327928377014,0.0434076000936218);
#818=ELLIPSE('',#101136,0.0192307675633611,0.0124961950670825);
#819=ELLIPSE('',#101137,0.0192307675636668,0.0124961950672304);
#820=ELLIPSE('',#101154,0.0425526869741348,0.0390142882255173);
#821=ELLIPSE('',#101156,0.0496327928422112,0.0434076000958298);
#822=ELLIPSE('',#101159,0.0192307675636596,0.0124961950672704);
#823=ELLIPSE('',#101160,0.0192307675634132,0.0124961950670193);
#824=ELLIPSE('',#101177,0.0425526869757438,0.0390142882268549);
#825=ELLIPSE('',#101179,0.049632792839498,0.0434076000944692);
#826=ELLIPSE('',#101182,0.0192307675636907,0.0124961950673134);
#827=ELLIPSE('',#101183,0.0192307675632347,0.0124961950668581);
#828=ELLIPSE('',#101200,0.0425526869756515,0.0390142882267198);
#829=ELLIPSE('',#101202,0.0496327928408119,0.0434076000951749);
#830=ELLIPSE('',#101205,0.019230767563772,0.0124961950673667);
#831=ELLIPSE('',#101206,0.0192307675640002,0.0124961950674824);
#832=ELLIPSE('',#101223,0.0425526869742298,0.0390142882257123);
#833=ELLIPSE('',#101225,0.0496327928392884,0.0434076000944368);
#834=ELLIPSE('',#101228,0.0192307675638603,0.0124961950674543);
#835=ELLIPSE('',#101229,0.0192307675640063,0.0124961950675154);
#836=ELLIPSE('',#101246,0.0425526869754304,0.039014288226562);
#837=ELLIPSE('',#101248,0.0496327928399952,0.0434076000947494);
#838=ELLIPSE('',#101251,0.0192307675631104,0.0124961950668259);
#839=ELLIPSE('',#101252,0.0192307675637105,0.0124961950672723);
#840=ELLIPSE('',#101269,0.0425526869751533,0.0390142882263134);
#841=ELLIPSE('',#101271,0.0496327928434795,0.0434076000964837);
#842=ELLIPSE('',#101274,0.0192307675635219,0.012496195067161);
#843=ELLIPSE('',#101275,0.0192307675636582,0.0124961950672209);
#844=ELLIPSE('',#101292,0.0425526869738089,0.0390142882252893);
#845=ELLIPSE('',#101294,0.0496327928415335,0.0434076000954915);
#846=ELLIPSE('',#101297,0.0192307675636047,0.0124961950672229);
#847=ELLIPSE('',#101298,0.0192307675637509,0.0124961950672977);
#848=ELLIPSE('',#101315,0.0425526869748406,0.0390142882260696);
#849=ELLIPSE('',#101317,0.0496327928416895,0.0434076000955919);
#850=ELLIPSE('',#101320,0.0192307675636503,0.0124961950672501);
#851=ELLIPSE('',#101321,0.0192307675637744,0.0124961950673005);
#852=ELLIPSE('',#101338,0.0425526869748277,0.0390142882260173);
#853=ELLIPSE('',#101340,0.0496327928393208,0.0434076000944356);
#854=ELLIPSE('',#101343,0.019230767563307,0.0124961950669749);
#855=ELLIPSE('',#101344,0.0192307675635884,0.0124961950671878);
#856=ELLIPSE('',#101361,0.0425526869745431,0.0390142882258003);
#857=ELLIPSE('',#101363,0.049632792839495,0.0434076000945007);
#858=ELLIPSE('',#101366,0.0192307675636009,0.0124961950672421);
#859=ELLIPSE('',#101367,0.0192307675639625,0.0124961950674852);
#860=ELLIPSE('',#101384,0.0425526869740447,0.0390142882253699);
#861=ELLIPSE('',#101386,0.0496327928390667,0.043407600094334);
#862=ELLIPSE('',#101389,0.0192307675635503,0.012496195067186);
#863=ELLIPSE('',#101390,0.0192307675639065,0.0124961950674353);
#864=ELLIPSE('',#101407,0.042552686974613,0.0390142882258343);
#865=ELLIPSE('',#101409,0.0496327928417377,0.0434076000955981);
#866=ELLIPSE('',#101412,0.0192307675632349,0.0124961950669307);
#867=ELLIPSE('',#101413,0.0192307675636638,0.012496195067226);
#868=ELLIPSE('',#101430,0.0425526869746227,0.0390142882258163);
#869=ELLIPSE('',#101432,0.0496327928412397,0.043407600095381);
#870=ELLIPSE('',#101435,0.0192307675631595,0.0124961950668576);
#871=ELLIPSE('',#101436,0.019230767563481,0.012496195067064);
#872=ELLIPSE('',#101453,0.0425526869750388,0.0390142882262424);
#873=ELLIPSE('',#101455,0.0496327928405082,0.0434076000950075);
#874=ELLIPSE('',#101458,0.0192307675638917,0.0124961950674706);
#875=ELLIPSE('',#101459,0.0192307675638487,0.01249619506737);
#876=ELLIPSE('',#101476,0.0425526869741601,0.0390142882255349);
#877=ELLIPSE('',#101478,0.0496327928403301,0.0434076000948956);
#878=ELLIPSE('',#101481,0.0192307675637445,0.0124961950673484);
#879=ELLIPSE('',#101482,0.0192307675638341,0.0124961950673598);
#880=ELLIPSE('',#101499,0.0425526869743731,0.0390142882256932);
#881=ELLIPSE('',#101501,0.049632792839551,0.0434076000945117);
#882=ELLIPSE('',#101504,0.0192307675633938,0.0124961950670532);
#883=ELLIPSE('',#101505,0.0192307675634615,0.0124961950670706);
#884=ELLIPSE('',#101522,0.0425526869753327,0.0390142882265068);
#885=ELLIPSE('',#101524,0.0496327928392813,0.0434076000943744);
#886=ELLIPSE('',#101527,0.0192307675634685,0.0124961950671455);
#887=ELLIPSE('',#101528,0.0192307675636214,0.01249619506719);
#888=ELLIPSE('',#101545,0.0425526869753598,0.039014288226546);
#889=ELLIPSE('',#101547,0.0496327928418455,0.0434076000956737);
#890=ELLIPSE('',#101550,0.0192307675632718,0.0124961950669572);
#891=ELLIPSE('',#101551,0.0192307675635591,0.0124961950671161);
#892=ELLIPSE('',#101568,0.0425526869738626,0.0390142882253316);
#893=ELLIPSE('',#101570,0.0496327928412948,0.0434076000954059);
#894=ELLIPSE('',#101573,0.0192307675634556,0.0124961950670978);
#895=ELLIPSE('',#101574,0.0192307675636301,0.0124961950672015);
#896=ELLIPSE('',#101591,0.0425526869756818,0.0390142882267155);
#897=ELLIPSE('',#101593,0.0496327928431759,0.0434076000963139);
#898=ELLIPSE('',#101596,0.0192307675635293,0.0124961950671862);
#899=ELLIPSE('',#101597,0.0192307675636501,0.0124961950672362);
#900=ELLIPSE('',#101614,0.0425526869746175,0.0390142882259505);
#901=ELLIPSE('',#101616,0.049632792837045,0.0434076000933051);
#902=ELLIPSE('',#101619,0.0192307675633792,0.0124961950670546);
#903=ELLIPSE('',#101620,0.0192307675635501,0.0124961950671421);
#904=ELLIPSE('',#101637,0.0425526869752923,0.0390142882263946);
#905=ELLIPSE('',#101639,0.0496327928408134,0.0434076000951231);
#906=ELLIPSE('',#101642,0.0192307675636319,0.0124961950672612);
#907=ELLIPSE('',#101643,0.0192307675636181,0.0124961950671656);
#908=ELLIPSE('',#101660,0.0425526869742864,0.0390142882256438);
#909=ELLIPSE('',#101662,0.0496327928417663,0.0434076000956443);
#910=ELLIPSE('',#101665,0.0192307675637982,0.012496195067383);
#911=ELLIPSE('',#101666,0.0192307675638904,0.012496195067438);
#912=ELLIPSE('',#101683,0.0425526869752358,0.0390142882264552);
#913=ELLIPSE('',#101685,0.0496327928396165,0.0434076000945633);
#914=ELLIPSE('',#101688,0.019230767563197,0.0124961950669256);
#915=ELLIPSE('',#101689,0.0192307675639446,0.0124961950674674);
#916=ELLIPSE('',#101706,0.0425526869754807,0.0390142882265653);
#917=ELLIPSE('',#101708,0.0496327928408132,0.0434076000951034);
#918=ELLIPSE('',#101711,0.0192307675635509,0.0124961950671871);
#919=ELLIPSE('',#101712,0.0192307675641415,0.0124961950676206);
#920=ELLIPSE('',#101729,0.0425526869749276,0.0390142882262301);
#921=ELLIPSE('',#101731,0.0496327928440629,0.0434076000967274);
#922=ELLIPSE('',#101734,0.019230767563645,0.0124961950672504);
#923=ELLIPSE('',#101735,0.0192307675638628,0.0124961950674008);
#924=ELLIPSE('',#101752,0.0425526869745453,0.0390142882258204);
#925=ELLIPSE('',#101754,0.0496327928416776,0.0434076000955951);
#926=ELLIPSE('',#101757,0.0192307675636142,0.0124961950672563);
#927=ELLIPSE('',#101758,0.0192307675632203,0.0124961950668388);
#928=ELLIPSE('',#101775,0.0425526869749915,0.0390142882261663);
#929=ELLIPSE('',#101777,0.0496327928438602,0.0434076000966784);
#930=ELLIPSE('',#101780,0.0192307675633165,0.0124961950669919);
#931=ELLIPSE('',#101781,0.01923076756384,0.0124961950673881);
#932=ELLIPSE('',#101798,0.0425526869744079,0.0390142882256586);
#933=ELLIPSE('',#101800,0.0496327928408126,0.0434076000951567);
#934=ELLIPSE('',#101803,0.0192307675637739,0.0124961950674063);
#935=ELLIPSE('',#101804,0.0192307675637082,0.0124961950672627);
#936=ELLIPSE('',#101821,0.0425526869734033,0.0390142882248949);
#937=ELLIPSE('',#101823,0.0496327928401318,0.0434076000948125);
#938=ELLIPSE('',#101826,0.0192307675635592,0.0124961950672023);
#939=ELLIPSE('',#101827,0.0192307675639849,0.0124961950674855);
#940=ELLIPSE('',#101844,0.042552686975287,0.0390142882264506);
#941=ELLIPSE('',#101846,0.0496327928407087,0.043407600095097);
#942=ELLIPSE('',#101849,0.0192307675633303,0.0124961950670066);
#943=ELLIPSE('',#101850,0.0192307675633735,0.0124961950670145);
#944=ELLIPSE('',#101867,0.0425526869737294,0.0390142882251553);
#945=ELLIPSE('',#101869,0.0496327928412784,0.0434076000953894);
#946=ELLIPSE('',#101872,0.0192307675636036,0.0124961950672486);
#947=ELLIPSE('',#101873,0.0192307675637504,0.0124961950672888);
#948=ELLIPSE('',#101890,0.0425526869748891,0.039014288226071);
#949=ELLIPSE('',#101892,0.0496327928397892,0.0434076000946233);
#950=ELLIPSE('',#101895,0.0192307675635607,0.0124961950671772);
#951=ELLIPSE('',#101896,0.0192307675637951,0.0124961950673368);
#952=ELLIPSE('',#101913,0.0425526869755134,0.0390142882265691);
#953=ELLIPSE('',#101915,0.0496327928419113,0.0434076000957154);
#954=ELLIPSE('',#101918,0.0192307675634443,0.0124961950671131);
#955=ELLIPSE('',#101919,0.0192307675636348,0.0124961950672014);
#956=ELLIPSE('',#101936,0.042552686974117,0.0390142882255079);
#957=ELLIPSE('',#101938,0.0496327928414422,0.0434076000954564);
#958=ELLIPSE('',#101941,0.0192307675635264,0.0124961950671719);
#959=ELLIPSE('',#101942,0.0192307675631223,0.0124961950667821);
#960=ELLIPSE('',#101959,0.0425526869740302,0.0390142882253675);
#961=ELLIPSE('',#101961,0.049632792844195,0.0434076000968254);
#962=ELLIPSE('',#101964,0.0192307675632831,0.0124961950669592);
#963=ELLIPSE('',#101965,0.0192307675637101,0.0124961950672638);
#964=ELLIPSE('',#101982,0.0425526869744749,0.0390142882257445);
#965=ELLIPSE('',#101984,0.0496327928427934,0.0434076000960854);
#966=ELLIPSE('',#101987,0.0192307675634205,0.0124961950670957);
#967=ELLIPSE('',#101988,0.0192307675635492,0.012496195067125);
#968=ELLIPSE('',#102005,0.042552686973661,0.0390142882250711);
#969=ELLIPSE('',#102007,0.0496327928417467,0.0434076000956492);
#970=ELLIPSE('',#102010,0.0192307675638008,0.0124961950674073);
#971=ELLIPSE('',#102011,0.0192307675632246,0.0124961950668404);
#972=ELLIPSE('',#102028,0.0425526869754936,0.0390142882266065);
#973=ELLIPSE('',#102030,0.0496327928427154,0.0434076000961266);
#974=ELLIPSE('',#102033,0.0192307675637723,0.0124961950673811);
#975=ELLIPSE('',#102034,0.0192307675634061,0.0124961950670075);
#976=ELLIPSE('',#102051,0.0425526869745814,0.0390142882258619);
#977=ELLIPSE('',#102053,0.0496327928401041,0.0434076000948024);
#978=ELLIPSE('',#102056,0.0192307675635512,0.0124961950671918);
#979=ELLIPSE('',#102057,0.0192307675634758,0.0124961950670549);
#980=ELLIPSE('',#102074,0.0425526869738501,0.0390142882253079);
#981=ELLIPSE('',#102076,0.0496327928405524,0.0434076000950126);
#982=ELLIPSE('',#102079,0.0192307675632594,0.0124961950669426);
#983=ELLIPSE('',#102080,0.019230767563644,0.0124961950672196);
#984=ELLIPSE('',#102097,0.0425526869746686,0.0390142882259405);
#985=ELLIPSE('',#102099,0.0496327928412873,0.0434076000953856);
#986=ELLIPSE('',#102102,0.0192307675633519,0.0124961950670217);
#987=ELLIPSE('',#102103,0.0192307675635051,0.012496195067098);
#988=ELLIPSE('',#102120,0.0425526869738852,0.0390142882252857);
#989=ELLIPSE('',#102122,0.0496327928420414,0.0434076000957133);
#990=ELLIPSE('',#102125,0.0192307675637008,0.0124961950673219);
#991=ELLIPSE('',#102126,0.019230767563814,0.0124961950673542);
#992=ELLIPSE('',#102143,0.0425526869754299,0.0390142882265886);
#993=ELLIPSE('',#102145,0.0496327928386749,0.0434076000941317);
#994=ELLIPSE('',#102148,0.0192307675633133,0.0124961950669842);
#995=ELLIPSE('',#102149,0.0192307675636375,0.0124961950671983);
#996=ELLIPSE('',#102166,0.0425526869745743,0.0390142882257796);
#997=ELLIPSE('',#102168,0.0496327928421313,0.043407600095765);
#998=ELLIPSE('',#102171,0.0192307675631128,0.0124961950668294);
#999=ELLIPSE('',#102172,0.0192307675634278,0.0124961950670298);
#1000=ELLIPSE('',#102189,0.0425526869737158,0.0390142882251488);
#1001=ELLIPSE('',#102191,0.0496327928430415,0.0434076000962617);
#1002=ELLIPSE('',#102194,0.0192307675635778,0.0124961950672225);
#1003=ELLIPSE('',#102195,0.019230767563536,0.0124961950671344);
#1004=ELLIPSE('',#102212,0.0425526869745159,0.0390142882257335);
#1005=ELLIPSE('',#102214,0.0496327928416729,0.0434076000956114);
#1006=ELLIPSE('',#102217,0.0192307675629175,0.0124961950666397);
#1007=ELLIPSE('',#102218,0.0192307675639304,0.0124961950674491);
#1008=ELLIPSE('',#102235,0.0425526869749957,0.0390142882261683);
#1009=ELLIPSE('',#102237,0.0496327928395604,0.0434076000945359);
#1010=ELLIPSE('',#102240,0.0192307675634575,0.0124961950671176);
#1011=ELLIPSE('',#102241,0.0192307675637056,0.0124961950672668);
#1012=ELLIPSE('',#102258,0.0425526869750752,0.039014288226265);
#1013=ELLIPSE('',#102260,0.0496327928416145,0.0434076000955403);
#1014=ELLIPSE('',#102263,0.0192307675635318,0.0124961950671783);
#1015=ELLIPSE('',#102264,0.019230767563965,0.012496195067492);
#1016=ELLIPSE('',#102281,0.0425526869753011,0.0390142882264729);
#1017=ELLIPSE('',#102283,0.0496327928402229,0.0434076000948783);
#1018=ELLIPSE('',#102286,0.0192307675628003,0.0124961950665828);
#1019=ELLIPSE('',#102287,0.0192307675639499,0.0124961950674749);
#1020=ELLIPSE('',#102304,0.0425526869746192,0.0390142882259507);
#1021=ELLIPSE('',#102306,0.0496327928388132,0.0434076000941526);
#1022=ELLIPSE('',#102309,0.0192307675632284,0.0124961950669226);
#1023=ELLIPSE('',#102310,0.0192307675632992,0.0124961950669107);
#1024=ELLIPSE('',#102327,0.0425526869730377,0.0390142882245624);
#1025=ELLIPSE('',#102329,0.0496327928419789,0.0434076000957078);
#1026=ELLIPSE('',#102332,0.0192307675636472,0.012496195067296);
#1027=ELLIPSE('',#102333,0.0192307675638403,0.0124961950673552);
#1028=ELLIPSE('',#102350,0.0425526869748947,0.0390142882261328);
#1029=ELLIPSE('',#102352,0.0496327928390325,0.0434076000943003);
#1030=ELLIPSE('',#102355,0.0192307675634255,0.0124961950670811);
#1031=ELLIPSE('',#102356,0.0192307675635047,0.0124961950670899);
#1032=ELLIPSE('',#102373,0.0425526869747593,0.0390142882260281);
#1033=ELLIPSE('',#102375,0.0496327928439498,0.0434076000966843);
#1034=ELLIPSE('',#102378,0.0192307675631962,0.0124961950669167);
#1035=ELLIPSE('',#102379,0.0192307675637204,0.0124961950672605);
#1036=ELLIPSE('',#102396,0.0425526869755656,0.0390142882266576);
#1037=ELLIPSE('',#102398,0.0496327928402873,0.0434076000948886);
#1038=ELLIPSE('',#102401,0.0192307675633131,0.0124961950669589);
#1039=ELLIPSE('',#102402,0.0192307675637082,0.0124961950672744);
#1040=ELLIPSE('',#102419,0.0425526869745731,0.0390142882258727);
#1041=ELLIPSE('',#102421,0.0496327928400867,0.0434076000948188);
#1042=ELLIPSE('',#102424,0.0192307675635455,0.0124961950671794);
#1043=ELLIPSE('',#102425,0.0192307675635274,0.0124961950671071);
#1044=ELLIPSE('',#102442,0.0425526869749222,0.0390142882261123);
#1045=ELLIPSE('',#102444,0.0496327928431116,0.0434076000963298);
#1046=ELLIPSE('',#102447,0.0192307675635483,0.0124961950671917);
#1047=ELLIPSE('',#102448,0.0192307675640448,0.0124961950675534);
#1048=ELLIPSE('',#102465,0.0425526869742523,0.0390142882255338);
#1049=ELLIPSE('',#102467,0.0496327928418504,0.0434076000956289);
#1050=ELLIPSE('',#102470,0.0192307675635763,0.0124961950672184);
#1051=ELLIPSE('',#102471,0.0192307675639207,0.0124961950674505);
#1052=ELLIPSE('',#102488,0.0425526869744852,0.0390142882257258);
#1053=ELLIPSE('',#102490,0.0496327928436922,0.0434076000965822);
#1054=ELLIPSE('',#102493,0.0192307675635066,0.0124961950671226);
#1055=ELLIPSE('',#102494,0.0192307675639793,0.0124961950675183);
#1056=ELLIPSE('',#102511,0.0425526869738252,0.0390142882252166);
#1057=ELLIPSE('',#102513,0.0496327928419966,0.0434076000957468);
#1058=ELLIPSE('',#102516,0.0192307675630665,0.0124961950667913);
#1059=ELLIPSE('',#102517,0.0192307675639641,0.0124961950674707);
#1060=ELLIPSE('',#102534,0.0425526869765007,0.039014288227406);
#1061=ELLIPSE('',#102536,0.0496327928408136,0.0434076000951572);
#1062=ELLIPSE('',#102539,0.0192307675633216,0.012496195066993);
#1063=ELLIPSE('',#102540,0.0192307675635825,0.0124961950671522);
#1064=ELLIPSE('',#102557,0.0425526869734816,0.0390142882249933);
#1065=ELLIPSE('',#102559,0.0496327928387264,0.043407600094146);
#1066=ELLIPSE('',#102562,0.0192307675637256,0.012496195067343);
#1067=ELLIPSE('',#102563,0.0192307675635382,0.0124961950671278);
#1068=ELLIPSE('',#102580,0.0425526869735161,0.0390142882249432);
#1069=ELLIPSE('',#102582,0.0496327928400537,0.043407600094742);
#1070=ELLIPSE('',#102585,0.0192307675635381,0.0124961950671603);
#1071=ELLIPSE('',#102586,0.0192307675638612,0.0124961950674075);
#1072=ELLIPSE('',#102603,0.0425526869739921,0.0390142882253723);
#1073=ELLIPSE('',#102605,0.0496327928392701,0.0434076000943856);
#1074=ELLIPSE('',#102608,0.019230767563548,0.0124961950671943);
#1075=ELLIPSE('',#102609,0.0192307675638532,0.0124961950673877);
#1076=ELLIPSE('',#102626,0.0425526869752034,0.039014288226399);
#1077=ELLIPSE('',#102628,0.0496327928432613,0.0434076000963658);
#1078=ELLIPSE('',#102631,0.019230767563464,0.0124961950671191);
#1079=ELLIPSE('',#102632,0.0192307675637455,0.0124961950673029);
#1080=ELLIPSE('',#103301,0.0947748497909006,0.0898017844795411);
#1081=ELLIPSE('',#103302,0.0972540504460011,0.0908803722731057);
#1082=ELLIPSE('',#103304,0.0972540504441047,0.0908803722721906);
#1083=ELLIPSE('',#103305,0.094774849794112,0.089801784481129);
#1084=ELLIPSE('',#103307,0.0947748497926148,0.0898017844804075);
#1085=ELLIPSE('',#103308,0.0972540504400136,0.0908803722702226);
#1086=ELLIPSE('',#103310,0.094774849789673,0.0898017844789408);
#1087=ELLIPSE('',#103311,0.0972540504453024,0.0908803722727663);
#1088=ELLIPSE('',#103313,0.094774849786822,0.0898017844775384);
#1089=ELLIPSE('',#103314,0.0972540504422525,0.0908803722712843);
#1090=ELLIPSE('',#103316,0.0947748497908327,0.0898017844795387);
#1091=ELLIPSE('',#103317,0.0972540504468864,0.0908803722735133);
#1092=ELLIPSE('',#103319,0.0947748497890312,0.0898017844786284);
#1093=ELLIPSE('',#103320,0.0972540504424856,0.0908803722714283);
#1094=ELLIPSE('',#103322,0.0947748497876344,0.0898017844779163);
#1095=ELLIPSE('',#103323,0.0972540504418127,0.0908803722711085);
#1096=ELLIPSE('',#103325,0.0947748497848643,0.0898017844765636);
#1097=ELLIPSE('',#103326,0.0972540504452924,0.0908803722727769);
#1098=ELLIPSE('',#103328,0.0947748497895253,0.0898017844788167);
#1099=ELLIPSE('',#103329,0.0972540504473756,0.0908803722737362);
#1100=ELLIPSE('',#103331,0.0947748497843389,0.0898017844762829);
#1101=ELLIPSE('',#103332,0.0972540504474796,0.0908803722737873);
#1102=ELLIPSE('',#103334,0.0947748497882029,0.089801784478216);
#1103=ELLIPSE('',#103335,0.0972540504461555,0.0908803722731809);
#1104=ELLIPSE('',#103337,0.0947748497881544,0.0898017844781412);
#1105=ELLIPSE('',#103338,0.097254050445608,0.0908803722729431);
#1106=ELLIPSE('',#103340,0.0947748497883721,0.0898017844782773);
#1107=ELLIPSE('',#103341,0.0972540504426967,0.090880372271529);
#1108=ELLIPSE('',#103343,0.0947748497912198,0.0898017844796705);
#1109=ELLIPSE('',#103344,0.097254050442374,0.0908803722713863);
#1110=ELLIPSE('',#103346,0.0947748497899889,0.0898017844791001);
#1111=ELLIPSE('',#103347,0.09725405044176,0.0908803722710741);
#1112=ELLIPSE('',#103349,0.0947748497919646,0.0898017844800436);
#1113=ELLIPSE('',#103350,0.0972540504477304,0.0908803722739094);
#1114=ELLIPSE('',#103352,0.0947748497877307,0.0898017844779762);
#1115=ELLIPSE('',#103353,0.0972540504444203,0.0908803722723428);
#1116=ELLIPSE('',#103355,0.0947748497875329,0.0898017844778618);
#1117=ELLIPSE('',#103356,0.0972540504420591,0.0908803722711656);
#1118=ELLIPSE('',#103358,0.0947748497891401,0.0898017844787187);
#1119=ELLIPSE('',#103359,0.0972540504458414,0.0908803722730333);
#1120=ELLIPSE('',#103361,0.0947748497842726,0.0898017844762788);
#1121=ELLIPSE('',#103362,0.097254050446,0.0908803722731059);
#1122=ELLIPSE('',#103364,0.0947748497896824,0.0898017844789354);
#1123=ELLIPSE('',#103365,0.0972540504473757,0.0908803722737566);
#1124=ELLIPSE('',#103367,0.0947748497879396,0.0898017844780717);
#1125=ELLIPSE('',#103368,0.0972540504470089,0.0908803722736072);
#1126=ELLIPSE('',#103370,0.0947748497897777,0.0898017844789476);
#1127=ELLIPSE('',#103371,0.0972540504424488,0.0908803722714188);
#1128=ELLIPSE('',#103373,0.0947748497858688,0.089801784477053);
#1129=ELLIPSE('',#103374,0.0972540504452601,0.0908803722727454);
#1130=ELLIPSE('',#103376,0.0947748497860426,0.0898017844771369);
#1131=ELLIPSE('',#103377,0.0972540504427043,0.0908803722715334);
#1132=ELLIPSE('',#103379,0.0947748497911017,0.0898017844796039);
#1133=ELLIPSE('',#103380,0.0972540504471524,0.0908803722736316);
#1134=ELLIPSE('',#103382,0.0947748497922374,0.0898017844801959);
#1135=ELLIPSE('',#103383,0.0972540504445394,0.0908803722723832);
#1136=ELLIPSE('',#103385,0.0947748497900101,0.0898017844790907);
#1137=ELLIPSE('',#103386,0.0972540504431669,0.0908803722717343);
#1138=ELLIPSE('',#103388,0.0947748497928145,0.0898017844805255);
#1139=ELLIPSE('',#103389,0.0972540504431744,0.0908803722717194);
#1140=ELLIPSE('',#103391,0.0947748497892975,0.089801784478741);
#1141=ELLIPSE('',#103392,0.0972540504433099,0.0908803722717966);
#1142=ELLIPSE('',#103394,0.0947748497905813,0.0898017844793987);
#1143=ELLIPSE('',#103395,0.0972540504447271,0.0908803722724841);
#1144=ELLIPSE('',#103397,0.0947748497888503,0.089801784478531);
#1145=ELLIPSE('',#103398,0.0972540504397721,0.0908803722700921);
#1146=ELLIPSE('',#103400,0.0947748497870893,0.0898017844776473);
#1147=ELLIPSE('',#103401,0.097254050445599,0.0908803722729439);
#1148=ELLIPSE('',#103403,0.0947748497869435,0.0898017844776184);
#1149=ELLIPSE('',#103404,0.0972540504398893,0.0908803722701564);
#1150=ELLIPSE('',#103406,0.0947748497885468,0.0898017844783568);
#1151=ELLIPSE('',#103407,0.0972540504452832,0.0908803722727715);
#1152=ELLIPSE('',#103409,0.0947748497938607,0.0898017844810411);
#1153=ELLIPSE('',#103410,0.0972540504442418,0.0908803722722562);
#1154=ELLIPSE('',#103412,0.0947748497932972,0.0898017844807086);
#1155=ELLIPSE('',#103413,0.0972540504442487,0.0908803722722781);
#1156=ELLIPSE('',#103415,0.0947748497875134,0.0898017844778826);
#1157=ELLIPSE('',#103416,0.0972540504437859,0.0908803722720484);
#1158=ELLIPSE('',#103418,0.0947748497930879,0.0898017844806332);
#1159=ELLIPSE('',#103419,0.0972540504418411,0.0908803722711222);
#1160=ELLIPSE('',#103421,0.0947748497905372,0.0898017844793675);
#1161=ELLIPSE('',#103422,0.0972540504448954,0.0908803722725851);
#1162=ELLIPSE('',#103424,0.0947748497895737,0.0898017844788519);
#1163=ELLIPSE('',#103425,0.0972540504458755,0.0908803722730405);
#1164=ELLIPSE('',#103427,0.0947748497952288,0.0898017844816764);
#1165=ELLIPSE('',#103428,0.0972540504431929,0.0908803722717643);
#1166=ELLIPSE('',#103430,0.0947748497907875,0.0898017844794307);
#1167=ELLIPSE('',#103431,0.0972540504433047,0.090880372271786);
#1168=ELLIPSE('',#103433,0.0947748497925041,0.0898017844803797);
#1169=ELLIPSE('',#103434,0.097254050447641,0.0908803722738984);
#1170=ELLIPSE('',#103436,0.0947748497896336,0.0898017844789406);
#1171=ELLIPSE('',#103437,0.0972540504450963,0.0908803722726497);
#1172=ELLIPSE('',#103439,0.0947748497902753,0.0898017844792372);
#1173=ELLIPSE('',#103440,0.0972540504430836,0.0908803722717207);
#1174=ELLIPSE('',#103442,0.0947748497870242,0.0898017844776269);
#1175=ELLIPSE('',#103443,0.0972540504459792,0.090880372273105);
#1176=ELLIPSE('',#103445,0.0947748497890259,0.0898017844786251);
#1177=ELLIPSE('',#103446,0.0972540504488311,0.0908803722744611);
#1178=ELLIPSE('',#103448,0.0947748497922702,0.0898017844801884);
#1179=ELLIPSE('',#103449,0.0972540504411497,0.0908803722707469);
#1180=ELLIPSE('',#103451,0.0947748497905426,0.0898017844793613);
#1181=ELLIPSE('',#103452,0.0972540504401611,0.0908803722702625);
#1182=ELLIPSE('',#103454,0.0947748497905523,0.0898017844793281);
#1183=ELLIPSE('',#103455,0.0972540504497045,0.0908803722748831);
#1184=ELLIPSE('',#103457,0.094774849791047,0.089801784479608);
#1185=ELLIPSE('',#103458,0.0972540504464803,0.0908803722733509);
#1186=ELLIPSE('',#103460,0.0947748497888638,0.08980178447855);
#1187=ELLIPSE('',#103461,0.0972540504428653,0.0908803722716096);
#1188=ELLIPSE('',#103463,0.0947748497937681,0.0898017844809604);
#1189=ELLIPSE('',#103464,0.0972540504468058,0.090880372273465);
#1190=ELLIPSE('',#103466,0.0947748497887476,0.0898017844784555);
#1191=ELLIPSE('',#103467,0.0972540504424136,0.0908803722713366);
#1192=ELLIPSE('',#103469,0.0947748497937203,0.0898017844809448);
#1193=ELLIPSE('',#103470,0.097254050439549,0.0908803722699748);
#1194=ELLIPSE('',#103472,0.0947748497936973,0.089801784480952);
#1195=ELLIPSE('',#103473,0.097254050446727,0.0908803722734838);
#1196=ELLIPSE('',#103475,0.0947748497887032,0.0898017844784639);
#1197=ELLIPSE('',#103476,0.0972540504410564,0.090880372270709);
#1198=ELLIPSE('',#103478,0.0947748497904981,0.0898017844793291);
#1199=ELLIPSE('',#103479,0.0972540504464435,0.0908803722733254);
#1200=ELLIPSE('',#103481,0.0947748497869006,0.0898017844775519);
#1201=ELLIPSE('',#103482,0.0972540504383138,0.0908803722693876);
#1202=ELLIPSE('',#103484,0.0947748497936647,0.0898017844808587);
#1203=ELLIPSE('',#103485,0.0972540504444964,0.090880372272367);
#1204=ELLIPSE('',#103487,0.0947748497914323,0.0898017844798336);
#1205=ELLIPSE('',#103488,0.097254050440378,0.0908803722703976);
#1206=ELLIPSE('',#103490,0.0947748497888831,0.0898017844785387);
#1207=ELLIPSE('',#103491,0.0972540504428949,0.0908803722715775);
#1208=ELLIPSE('',#103493,0.0972540504453366,0.0908803722727811);
#1209=ELLIPSE('',#103494,0.0947748497894938,0.0898017844788294);
#1210=ELLIPSE('',#103496,0.097254050445453,0.0908803722728491);
#1211=ELLIPSE('',#103497,0.0947748497859855,0.0898017844771064);
#1212=ELLIPSE('',#103499,0.097254050440179,0.0908803722702838);
#1213=ELLIPSE('',#103500,0.0947748497888099,0.0898017844785166);
#1214=ELLIPSE('',#103502,0.0972540504444705,0.0908803722723385);
#1215=ELLIPSE('',#103503,0.09477484978895,0.0898017844785994);
#1216=ELLIPSE('',#103505,0.0972540504441078,0.0908803722721443);
#1217=ELLIPSE('',#103506,0.0947748497941903,0.0898017844811543);
#1218=ELLIPSE('',#103508,0.0972540504441623,0.0908803722721518);
#1219=ELLIPSE('',#103509,0.0947748497891558,0.0898017844787237);
#1220=ELLIPSE('',#103511,0.0972540504465191,0.090880372273371);
#1221=ELLIPSE('',#103512,0.0947748497877717,0.0898017844779554);
#1222=ELLIPSE('',#103514,0.0972540504455481,0.0908803722728434);
#1223=ELLIPSE('',#103515,0.0947748497885424,0.089801784478368);
#1224=ELLIPSE('',#103517,0.0972540504450305,0.0908803722726285);
#1225=ELLIPSE('',#103518,0.0947748497924166,0.0898017844803043);
#1226=ELLIPSE('',#103520,0.0972540504423171,0.0908803722713102);
#1227=ELLIPSE('',#103521,0.094774849789829,0.0898017844790031);
#1228=ELLIPSE('',#103523,0.0972540504450714,0.0908803722726709);
#1229=ELLIPSE('',#103524,0.0947748497893594,0.0898017844787876);
#1230=ELLIPSE('',#103526,0.0947748497916052,0.0898017844799109);
#1231=ELLIPSE('',#103527,0.0972540504466488,0.0908803722733968);
#1232=ELLIPSE('',#103529,0.0365824585612681,0.0343843127629441);
#1233=ELLIPSE('',#103530,0.0365824585612681,0.0343843127629441);
#1234=ELLIPSE('',#103532,0.0752932753395665,0.0683396339849831);
#1235=ELLIPSE('',#103534,0.068253186714463,0.0644989639553658);
#1236=ELLIPSE('',#103548,0.0947748497910113,0.0898017844796313);
#1237=ELLIPSE('',#103549,0.0972540504436445,0.0908803722719478);
#1238=ELLIPSE('',#103565,20.5655698940688,0.57588643813926);
#1239=ELLIPSE('',#103579,0.0682531867111947,0.0644989639532992);
#1240=ELLIPSE('',#103581,0.0752932753386038,0.0683396339845777);
#1241=ELLIPSE('',#103583,0.0365824585612599,0.0343843127629419);
#1242=ELLIPSE('',#103584,0.0365824585612599,0.0343843127629419);
#1243=ELLIPSE('',#103587,20.5663229393736,0.575899814551761);
#1244=ELLIPSE('',#103600,0.0682531867094754,0.064498963952367);
#1245=ELLIPSE('',#103602,0.0752932753433806,0.0683396339869066);
#1246=ELLIPSE('',#103604,0.0365824585612664,0.0343843127629435);
#1247=ELLIPSE('',#103605,0.0365824585612664,0.0343843127629435);
#1248=ELLIPSE('',#103608,20.5662371819658,0.575898279112179);
#1249=ELLIPSE('',#103621,0.0682531867098176,0.0644989639525022);
#1250=ELLIPSE('',#103623,0.0752932753414954,0.0683396339859597);
#1251=ELLIPSE('',#103625,0.0365824585612623,0.0343843127629425);
#1252=ELLIPSE('',#103626,0.0365824585612623,0.0343843127629425);
#1253=ELLIPSE('',#103629,20.5664729686215,0.575902484006716);
#1254=ELLIPSE('',#103642,0.0682531867102852,0.0644989639528799);
#1255=ELLIPSE('',#103644,0.0752932753421658,0.0683396339862994);
#1256=ELLIPSE('',#103646,0.0365824585612823,0.0343843127629472);
#1257=ELLIPSE('',#103647,0.0365824585612823,0.0343843127629472);
#1258=ELLIPSE('',#103650,20.5678571921608,0.575927076211219);
#1259=ELLIPSE('',#103663,0.0682531867113445,0.0644989639535526);
#1260=ELLIPSE('',#103665,0.075293275342646,0.0683396339865244);
#1261=ELLIPSE('',#103667,0.0365824585612725,0.0343843127629449);
#1262=ELLIPSE('',#103668,0.0365824585612725,0.0343843127629449);
#1263=ELLIPSE('',#103671,20.5672810058914,0.575916860252127);
#1264=ELLIPSE('',#103684,0.0682531867116232,0.0644989639537626);
#1265=ELLIPSE('',#103686,0.0752932753401903,0.0683396339853526);
#1266=ELLIPSE('',#103688,0.0365824585612739,0.0343843127629457);
#1267=ELLIPSE('',#103689,0.0365824585612739,0.0343843127629457);
#1268=ELLIPSE('',#103692,20.5658263631507,0.575890993606254);
#1269=ELLIPSE('',#103705,0.0682531867065395,0.0644989639503165);
#1270=ELLIPSE('',#103707,0.0752932753395809,0.0683396339850594);
#1271=ELLIPSE('',#103709,0.0365824585612871,0.0343843127629484);
#1272=ELLIPSE('',#103710,0.0365824585612871,0.0343843127629484);
#1273=ELLIPSE('',#103713,20.5645162727811,0.575867690121613);
#1274=ELLIPSE('',#103726,0.0682531867118177,0.0644989639537703);
#1275=ELLIPSE('',#103728,0.075293275340606,0.0683396339855119);
#1276=ELLIPSE('',#103730,0.0365824585612647,0.0343843127629428);
#1277=ELLIPSE('',#103731,0.0365824585612647,0.0343843127629428);
#1278=ELLIPSE('',#103734,20.5647351111823,0.575871593292131);
#1279=ELLIPSE('',#103747,0.0682531867054113,0.0644989639497118);
#1280=ELLIPSE('',#103749,0.0752932753420776,0.0683396339862422);
#1281=ELLIPSE('',#103751,0.0365824585612792,0.0343843127629464);
#1282=ELLIPSE('',#103752,0.0365824585612792,0.0343843127629464);
#1283=ELLIPSE('',#103755,20.5664678496986,0.575902371596359);
#1284=ELLIPSE('',#103768,0.0682531867081726,0.0644989639514463);
#1285=ELLIPSE('',#103770,0.0752932753410852,0.0683396339857466);
#1286=ELLIPSE('',#103772,0.0365824585612641,0.0343843127629426);
#1287=ELLIPSE('',#103773,0.0365824585612641,0.0343843127629426);
#1288=ELLIPSE('',#103776,20.5669390412555,0.575910766874766);
#1289=ELLIPSE('',#103789,0.068253186706991,0.0644989639507338);
#1290=ELLIPSE('',#103791,0.0752932753374719,0.0683396339840305);
#1291=ELLIPSE('',#103793,0.0365824585612722,0.0343843127629447);
#1292=ELLIPSE('',#103794,0.0365824585612722,0.0343843127629447);
#1293=ELLIPSE('',#103797,20.5672143657057,0.575915656399323);
#1294=ELLIPSE('',#103810,0.0682531867126107,0.0644989639543164);
#1295=ELLIPSE('',#103812,0.0752932753438051,0.0683396339870321);
#1296=ELLIPSE('',#103814,0.0365824585612707,0.0343843127629448);
#1297=ELLIPSE('',#103815,0.0365824585612707,0.0343843127629448);
#1298=ELLIPSE('',#103818,20.5666091795923,0.575904895820283);
#1299=ELLIPSE('',#103831,0.0682531867124643,0.0644989639541045);
#1300=ELLIPSE('',#103833,0.0752932753410141,0.0683396339857257);
#1301=ELLIPSE('',#103835,0.0365824585612672,0.0343843127629434);
#1302=ELLIPSE('',#103836,0.0365824585612672,0.0343843127629434);
#1303=ELLIPSE('',#103839,20.5655464083401,0.575886023270062);
#1304=ELLIPSE('',#103852,0.0682531867065658,0.0644989639504541);
#1305=ELLIPSE('',#103854,0.0752932753402659,0.0683396339853328);
#1306=ELLIPSE('',#103856,0.0365824585612715,0.0343843127629447);
#1307=ELLIPSE('',#103857,0.0365824585612715,0.0343843127629447);
#1308=ELLIPSE('',#103860,20.5646822681491,0.575870652388697);
#1309=ELLIPSE('',#103873,0.0682531867120338,0.0644989639538604);
#1310=ELLIPSE('',#103875,0.0752932753391909,0.0683396339848181);
#1311=ELLIPSE('',#103877,0.0365824585612667,0.0343843127629439);
#1312=ELLIPSE('',#103878,0.0365824585612667,0.0343843127629439);
#1313=ELLIPSE('',#103881,20.5655365027352,0.575885832702478);
#1314=ELLIPSE('',#103894,0.0682531867127566,0.0644989639543388);
#1315=ELLIPSE('',#103896,0.0752932753420776,0.0683396339862422);
#1316=ELLIPSE('',#103898,0.0365824585612694,0.0343843127629439);
#1317=ELLIPSE('',#103899,0.0365824585612694,0.0343843127629439);
#1318=ELLIPSE('',#103902,20.5688852559233,0.575945359262387);
#1319=ELLIPSE('',#103915,0.0682531867130963,0.064498963954561);
#1320=ELLIPSE('',#103917,0.0752932753382094,0.0683396339843537);
#1321=ELLIPSE('',#103919,0.0365824585612733,0.034384312762945);
#1322=ELLIPSE('',#103920,0.0365824585612733,0.034384312762945);
#1323=ELLIPSE('',#103923,20.5668625413724,0.575909393256759);
#1324=ELLIPSE('',#103936,0.0682531867084203,0.0644989639516756);
#1325=ELLIPSE('',#103938,0.0752932753436893,0.0683396339869951);
#1326=ELLIPSE('',#103940,0.0365824585612695,0.0343843127629441);
#1327=ELLIPSE('',#103941,0.0365824585612695,0.0343843127629441);
#1328=ELLIPSE('',#103944,20.5665715965953,0.575904239966151);
#1329=ELLIPSE('',#103957,0.068253186708846,0.064498963951929);
#1330=ELLIPSE('',#103959,0.0752932753363512,0.0683396339834891);
#1331=ELLIPSE('',#103961,0.0365824585612623,0.0343843127629426);
#1332=ELLIPSE('',#103962,0.0365824585612623,0.0343843127629426);
#1333=ELLIPSE('',#103965,20.5661257179486,0.575896290425635);
#1334=ELLIPSE('',#103978,0.0682531867104988,0.0644989639528177);
#1335=ELLIPSE('',#103980,0.0752932753396825,0.0683396339850846);
#1336=ELLIPSE('',#103982,0.0365824585612735,0.034384312762945);
#1337=ELLIPSE('',#103983,0.0365824585612735,0.034384312762945);
#1338=ELLIPSE('',#103986,20.5661929652102,0.575897501216388);
#1339=ELLIPSE('',#103999,0.0682531867089655,0.0644989639517745);
#1340=ELLIPSE('',#104001,0.0752932753431176,0.0683396339867453);
#1341=ELLIPSE('',#104003,0.0365824585612691,0.034384312762944);
#1342=ELLIPSE('',#104004,0.0365824585612691,0.034384312762944);
#1343=ELLIPSE('',#104007,20.5650746168456,0.5758776240409);
#1344=ELLIPSE('',#104020,0.0682531867060306,0.0644989639500308);
#1345=ELLIPSE('',#104022,0.0752932753402928,0.0683396339853569);
#1346=ELLIPSE('',#104024,0.036582458561283,0.0343843127629472);
#1347=ELLIPSE('',#104025,0.036582458561283,0.0343843127629472);
#1348=ELLIPSE('',#104028,20.5657406141823,0.575889449951057);
#1349=ELLIPSE('',#104041,0.0682531867074524,0.0644989639509632);
#1350=ELLIPSE('',#104043,0.0752932753386184,0.0683396339845661);
#1351=ELLIPSE('',#104045,0.0365824585612756,0.0343843127629454);
#1352=ELLIPSE('',#104046,0.0365824585612756,0.0343843127629454);
#1353=ELLIPSE('',#104049,20.5643894487282,0.575865453162332);
#1354=ELLIPSE('',#104062,0.0682531867044203,0.0644989639489921);
#1355=ELLIPSE('',#104064,0.0752932753451356,0.0683396339877038);
#1356=ELLIPSE('',#104066,0.0365824585612593,0.0343843127629417);
#1357=ELLIPSE('',#104067,0.0365824585612593,0.0343843127629417);
#1358=ELLIPSE('',#104070,20.5656209986185,0.575887328706856);
#1359=ELLIPSE('',#104083,0.068253186707082,0.0644989639507634);
#1360=ELLIPSE('',#104085,0.0752932753377725,0.0683396339841321);
#1361=ELLIPSE('',#104087,0.0365824585612572,0.0343843127629406);
#1362=ELLIPSE('',#104088,0.0365824585612572,0.0343843127629406);
#1363=ELLIPSE('',#104091,20.5648167949509,0.575873048464462);
#1364=ELLIPSE('',#104104,0.0682531867132729,0.0644989639547264);
#1365=ELLIPSE('',#104106,0.0752932753412577,0.0683396339859388);
#1366=ELLIPSE('',#104108,0.0365824585612782,0.0343843127629461);
#1367=ELLIPSE('',#104109,0.0365824585612782,0.0343843127629461);
#1368=ELLIPSE('',#104112,20.5673748138211,0.575918526296799);
#1369=ELLIPSE('',#104125,0.0682531867117419,0.0644989639536371);
#1370=ELLIPSE('',#104127,0.0752932753379916,0.0683396339842599);
#1371=ELLIPSE('',#104129,0.0365824585612557,0.0343843127629409);
#1372=ELLIPSE('',#104130,0.0365824585612557,0.0343843127629409);
#1373=ELLIPSE('',#104133,20.5657430869869,0.575889508004331);
#1374=ELLIPSE('',#104146,0.068253186712517,0.0644989639542092);
#1375=ELLIPSE('',#104148,0.0752932753416743,0.0683396339860329);
#1376=ELLIPSE('',#104150,0.0365824585612746,0.034384312762945);
#1377=ELLIPSE('',#104151,0.0365824585612746,0.034384312762945);
#1378=ELLIPSE('',#104154,20.5673584002177,0.575918223147289);
#1379=ELLIPSE('',#104167,0.068253186713621,0.0644989639549432);
#1380=ELLIPSE('',#104169,0.0752932753389554,0.0683396339847396);
#1381=ELLIPSE('',#104171,0.0365824585612687,0.0343843127629438);
#1382=ELLIPSE('',#104172,0.0365824585612687,0.0343843127629438);
#1383=ELLIPSE('',#104175,20.5667255038569,0.575906974270808);
#1384=ELLIPSE('',#104188,0.0682531867092921,0.0644989639522078);
#1385=ELLIPSE('',#104190,0.0752932753390765,0.0683396339847818);
#1386=ELLIPSE('',#104192,0.036582458561274,0.0343843127629452);
#1387=ELLIPSE('',#104193,0.036582458561274,0.0343843127629452);
#1388=ELLIPSE('',#104196,20.5667004386175,0.57590654076783);
#1389=ELLIPSE('',#104209,0.0682531867061263,0.0644989639501379);
#1390=ELLIPSE('',#104211,0.0752932753377836,0.0683396339842295);
#1391=ELLIPSE('',#104213,0.0365824585612689,0.034384312762944);
#1392=ELLIPSE('',#104214,0.0365824585612689,0.034384312762944);
#1393=ELLIPSE('',#104217,20.5669358575543,0.575910702097059);
#1394=ELLIPSE('',#104230,0.0682531867090717,0.0644989639519959);
#1395=ELLIPSE('',#104232,0.075293275340053,0.0683396339852434);
#1396=ELLIPSE('',#104234,0.0365824585612704,0.034384312762944);
#1397=ELLIPSE('',#104235,0.0365824585612704,0.034384312762944);
#1398=ELLIPSE('',#104238,20.5662681156164,0.575898853502041);
#1399=ELLIPSE('',#104251,0.0682531867097275,0.0644989639524759);
#1400=ELLIPSE('',#104253,0.0752932753429599,0.0683396339866412);
#1401=ELLIPSE('',#104255,0.0365824585612673,0.0343843127629433);
#1402=ELLIPSE('',#104256,0.0365824585612673,0.0343843127629433);
#1403=ELLIPSE('',#104259,20.5670037655622,0.57591192326816);
#1404=ELLIPSE('',#104272,0.0682531867142658,0.06449896395531);
#1405=ELLIPSE('',#104274,0.0752932753384642,0.0683396339845221);
#1406=ELLIPSE('',#104276,0.03658245856126,0.0343843127629417);
#1407=ELLIPSE('',#104277,0.03658245856126,0.0343843127629417);
#1408=ELLIPSE('',#104280,20.5649490683217,0.575875401255735);
#1409=ELLIPSE('',#104293,0.0682531867126994,0.0644989639543507);
#1410=ELLIPSE('',#104295,0.0752932753421147,0.0683396339862076);
#1411=ELLIPSE('',#104297,0.03658245856127,0.034384312762944);
#1412=ELLIPSE('',#104298,0.03658245856127,0.034384312762944);
#1413=ELLIPSE('',#104301,20.5657460307936,0.575889566336278);
#1414=ELLIPSE('',#104314,0.0682531867125926,0.064498963954206);
#1415=ELLIPSE('',#104316,0.0752932753386351,0.0683396339845576);
#1416=ELLIPSE('',#104318,0.0365824585612653,0.0343843127629431);
#1417=ELLIPSE('',#104319,0.0365824585612653,0.0343843127629431);
#1418=ELLIPSE('',#104322,20.566106933613,0.575895983526128);
#1419=ELLIPSE('',#104335,0.0682531867125118,0.0644989639541397);
#1420=ELLIPSE('',#104337,0.0752932753399427,0.0683396339852131);
#1421=ELLIPSE('',#104339,0.036582458561266,0.0343843127629433);
#1422=ELLIPSE('',#104340,0.036582458561266,0.0343843127629433);
#1423=ELLIPSE('',#104343,20.5662209241031,0.575898008612868);
#1424=ELLIPSE('',#104356,0.0682531867080255,0.0644989639513619);
#1425=ELLIPSE('',#104358,0.0752932753417252,0.0683396339860757);
#1426=ELLIPSE('',#104360,0.0365824585612643,0.0343843127629431);
#1427=ELLIPSE('',#104361,0.0365824585612643,0.0343843127629431);
#1428=ELLIPSE('',#104364,20.5668829564603,0.575909777573919);
#1429=ELLIPSE('',#104377,0.0682531867108673,0.0644989639530764);
#1430=ELLIPSE('',#104379,0.0752932753393979,0.0683396339849238);
#1431=ELLIPSE('',#104381,0.0365824585612754,0.0343843127629457);
#1432=ELLIPSE('',#104382,0.0365824585612754,0.0343843127629457);
#1433=ELLIPSE('',#104385,20.5656204522085,0.575887327180999);
#1434=ELLIPSE('',#104398,0.0682531867121636,0.064498963953902);
#1435=ELLIPSE('',#104400,0.0752932753435212,0.0683396339869279);
#1436=ELLIPSE('',#104402,0.0365824585612717,0.0343843127629449);
#1437=ELLIPSE('',#104403,0.0365824585612717,0.0343843127629449);
#1438=ELLIPSE('',#104406,20.5649985423749,0.575876281188508);
#1439=ELLIPSE('',#104419,0.0682531867100479,0.0644989639525862);
#1440=ELLIPSE('',#104421,0.0752932753365371,0.068339633983568);
#1441=ELLIPSE('',#104423,0.0365824585612617,0.0343843127629418);
#1442=ELLIPSE('',#104424,0.0365824585612617,0.0343843127629418);
#1443=ELLIPSE('',#104427,20.5660877699337,0.575895627154355);
#1444=ELLIPSE('',#104440,0.0682531867089013,0.0644989639519441);
#1445=ELLIPSE('',#104442,0.0752932753417667,0.0683396339860729);
#1446=ELLIPSE('',#104444,0.0365824585612718,0.0343843127629447);
#1447=ELLIPSE('',#104445,0.0365824585612718,0.0343843127629447);
#1448=ELLIPSE('',#104448,20.5667145066123,0.575906772537685);
#1449=ELLIPSE('',#104461,0.0682531867123641,0.0644989639540796);
#1450=ELLIPSE('',#104463,0.0752932753404132,0.0683396339854202);
#1451=ELLIPSE('',#104465,0.0365824585612721,0.0343843127629448);
#1452=ELLIPSE('',#104466,0.0365824585612721,0.0343843127629448);
#1453=ELLIPSE('',#104469,20.5655320840775,0.575885745020712);
#1454=ELLIPSE('',#104482,0.0682531867076054,0.0644989639510852);
#1455=ELLIPSE('',#104484,0.0752932753418868,0.0683396339861622);
#1456=ELLIPSE('',#104486,0.0365824585612703,0.0343843127629439);
#1457=ELLIPSE('',#104487,0.0365824585612703,0.0343843127629439);
#1458=ELLIPSE('',#104490,20.5656645738439,0.575888110796235);
#1459=ELLIPSE('',#104503,0.0682531867104776,0.0644989639529921);
#1460=ELLIPSE('',#104505,0.0752932753402919,0.0683396339853131);
#1461=ELLIPSE('',#104507,0.0365824585612638,0.0343843127629429);
#1462=ELLIPSE('',#104508,0.0365824585612638,0.0343843127629429);
#1463=ELLIPSE('',#104511,20.5649673526229,0.575875718878864);
#1464=ELLIPSE('',#104524,0.0682531867113191,0.064498963953423);
#1465=ELLIPSE('',#104526,0.0752932753419452,0.0683396339861261);
#1466=ELLIPSE('',#104528,0.036582458561263,0.0343843127629426);
#1467=ELLIPSE('',#104529,0.036582458561263,0.0343843127629426);
#1468=ELLIPSE('',#104532,20.5669984446418,0.575911817820984);
#1469=ELLIPSE('',#104545,0.0682531867132061,0.0644989639546646);
#1470=ELLIPSE('',#104547,0.0752932753409153,0.0683396339856607);
#1471=ELLIPSE('',#104549,0.0365824585612572,0.0343843127629414);
#1472=ELLIPSE('',#104550,0.0365824585612572,0.0343843127629414);
#1473=ELLIPSE('',#104553,20.5683868647745,0.575936493679187);
#1474=ELLIPSE('',#104566,0.0682531867051281,0.0644989639495226);
#1475=ELLIPSE('',#104568,0.0752932753371693,0.068339633983922);
#1476=ELLIPSE('',#104570,0.0365824585612551,0.0343843127629402);
#1477=ELLIPSE('',#104571,0.0365824585612551,0.0343843127629402);
#1478=ELLIPSE('',#104574,20.5642184742806,0.575862395393301);
#1479=ELLIPSE('',#104587,0.0682531867130814,0.0644989639545292);
#1480=ELLIPSE('',#104589,0.0752932753382603,0.0683396339843966);
#1481=ELLIPSE('',#104591,0.0365824585612835,0.0343843127629476);
#1482=ELLIPSE('',#104592,0.0365824585612835,0.0343843127629476);
#1483=ELLIPSE('',#104595,20.5674049560068,0.575919072631943);
#1484=ELLIPSE('',#104608,0.0682531867118938,0.0644989639538107);
#1485=ELLIPSE('',#104610,0.0752932753398767,0.0683396339852028);
#1486=ELLIPSE('',#104612,0.0365824585612653,0.0343843127629431);
#1487=ELLIPSE('',#104613,0.0365824585612653,0.0343843127629431);
#1488=ELLIPSE('',#104616,20.5655633575056,0.575886299567876);
#1489=ELLIPSE('',#104629,0.0682531867143369,0.0644989639553002);
#1490=ELLIPSE('',#104631,0.0752932753394289,0.0683396339849304);
#1491=ELLIPSE('',#104633,0.0365824585612765,0.0343843127629459);
#1492=ELLIPSE('',#104634,0.0365824585612765,0.0343843127629459);
#1493=ELLIPSE('',#104637,20.5653921601537,0.575883266585551);
#1494=ELLIPSE('',#104650,0.0682531867093569,0.0644989639522558);
#1495=ELLIPSE('',#104652,0.0752932753403644,0.0683396339854381);
#1496=ELLIPSE('',#104654,0.0365824585612568,0.0343843127629409);
#1497=ELLIPSE('',#104655,0.0365824585612568,0.0343843127629409);
#1498=ELLIPSE('',#104658,20.5661203042729,0.575896214636728);
#1499=ELLIPSE('',#104671,0.0682531867085627,0.0644989639517258);
#1500=ELLIPSE('',#104673,0.0752932753420239,0.0683396339862363);
#1501=ELLIPSE('',#104675,0.0365824585612604,0.0343843127629423);
#1502=ELLIPSE('',#104676,0.0365824585612604,0.0343843127629423);
#1503=ELLIPSE('',#104679,20.565803505481,0.575890582176382);
#1504=ELLIPSE('',#104692,0.0682531867095197,0.0644989639523459);
#1505=ELLIPSE('',#104694,0.0752932753387221,0.0683396339846143);
#1506=ELLIPSE('',#104696,0.0365824585612599,0.0343843127629417);
#1507=ELLIPSE('',#104697,0.0365824585612599,0.0343843127629417);
#1508=ELLIPSE('',#104700,20.5648309710559,0.575873292072556);
#1509=ELLIPSE('',#104713,0.0682531867074291,0.0644989639509719);
#1510=ELLIPSE('',#104715,0.0752932753429965,0.0683396339866554);
#1511=ELLIPSE('',#104717,0.0365824585612629,0.0343843127629425);
#1512=ELLIPSE('',#104718,0.0365824585612629,0.0343843127629425);
#1513=ELLIPSE('',#104721,20.5669825590435,0.57591154955311);
#1514=ELLIPSE('',#104734,0.0682531867130314,0.0644989639545135);
#1515=ELLIPSE('',#104736,0.0752932753441584,0.0683396339872419);
#1516=ELLIPSE('',#104738,0.0365824585612645,0.0343843127629429);
#1517=ELLIPSE('',#104739,0.0365824585612645,0.0343843127629429);
#1518=ELLIPSE('',#104742,20.5662483858826,0.575898493672706);
#1519=ELLIPSE('',#104755,0.0682531867098831,0.0644989639526421);
#1520=ELLIPSE('',#104757,0.0752932753409068,0.0683396339856623);
#1521=ELLIPSE('',#104759,0.0365824585612578,0.034384312762941);
#1522=ELLIPSE('',#104760,0.0365824585612578,0.034384312762941);
#1523=ELLIPSE('',#104763,20.5670224417481,0.575912258561078);
#1524=ELLIPSE('',#104776,0.0682531867061702,0.064498963950201);
#1525=ELLIPSE('',#104778,0.0752932753411104,0.068339633985768);
#1526=ELLIPSE('',#104780,0.0365824585612508,0.0343843127629396);
#1527=ELLIPSE('',#104781,0.0365824585612508,0.0343843127629396);
#1528=ELLIPSE('',#104784,20.5655347324022,0.575885805162513);
#1529=ELLIPSE('',#104797,0.0682531867118699,0.06449896395374);
#1530=ELLIPSE('',#104799,0.0752932753373313,0.068339633983908);
#1531=ELLIPSE('',#104801,0.0365824585612802,0.0343843127629466);
#1532=ELLIPSE('',#104802,0.0365824585612802,0.0343843127629466);
#1533=ELLIPSE('',#104805,20.5668284617458,0.575908795317053);
#1534=ELLIPSE('',#104818,0.0682531867127595,0.0644989639543824);
#1535=ELLIPSE('',#104820,0.0752932753396919,0.0683396339850703);
#1536=ELLIPSE('',#104822,0.0365824585612809,0.0343843127629465);
#1537=ELLIPSE('',#104823,0.0365824585612809,0.0343843127629465);
#1538=ELLIPSE('',#104826,20.5660203821645,0.575894443446422);
#1539=ELLIPSE('',#104839,0.0682531867122131,0.0644989639539199);
#1540=ELLIPSE('',#104841,0.0752932753438411,0.0683396339870888);
#1541=ELLIPSE('',#104843,0.0365824585612538,0.0343843127629404);
#1542=ELLIPSE('',#104844,0.0365824585612538,0.0343843127629404);
#1543=ELLIPSE('',#104847,20.56719128229,0.575915266446949);
#1544=ELLIPSE('',#104860,0.0682531867057307,0.0644989639499098);
#1545=ELLIPSE('',#104862,0.0752932753421604,0.0683396339862518);
#1546=ELLIPSE('',#104864,0.0365824585612703,0.0343843127629442);
#1547=ELLIPSE('',#104865,0.0365824585612703,0.0343843127629442);
#1548=ELLIPSE('',#104868,20.5659951690371,0.575893990843115);
#1549=ELLIPSE('',#104881,0.0682531867104656,0.0644989639528107);
#1550=ELLIPSE('',#104883,0.0752932753453524,0.0683396339878613);
#1551=ELLIPSE('',#104885,0.0365824585612831,0.0343843127629476);
#1552=ELLIPSE('',#104886,0.0365824585612831,0.0343843127629476);
#1553=ELLIPSE('',#104889,20.5657598820384,0.575889811600635);
#1554=ELLIPSE('',#104902,0.0682531867127301,0.0644989639542877);
#1555=ELLIPSE('',#104904,0.0752932753397943,0.0683396339851374);
#1556=ELLIPSE('',#104906,0.0365824585612655,0.0343843127629432);
#1557=ELLIPSE('',#104907,0.0365824585612655,0.0343843127629432);
#1558=ELLIPSE('',#104910,20.5670517301527,0.575912785764959);
#1559=ELLIPSE('',#104923,0.0682531867142145,0.0644989639552584);
#1560=ELLIPSE('',#104925,0.0752932753421681,0.0683396339862674);
#1561=ELLIPSE('',#104927,0.0365824585612741,0.0343843127629453);
#1562=ELLIPSE('',#104928,0.0365824585612741,0.0343843127629453);
#1563=ELLIPSE('',#104931,20.5676060497922,0.575922623380279);
#1564=ELLIPSE('',#104944,0.0682531867068906,0.0644989639506861);
#1565=ELLIPSE('',#104946,0.0752932753417022,0.0683396339860361);
#1566=ELLIPSE('',#104948,0.0365824585612606,0.0343843127629421);
#1567=ELLIPSE('',#104949,0.0365824585612606,0.0343843127629421);
#1568=ELLIPSE('',#104952,20.5663132227207,0.575899648889507);
#1569=ELLIPSE('',#104965,0.0682531867059857,0.064498963949947);
#1570=ELLIPSE('',#104967,0.0752932753409169,0.0683396339856948);
#1571=ELLIPSE('',#104969,0.0365824585612755,0.0343843127629457);
#1572=ELLIPSE('',#104970,0.0365824585612755,0.0343843127629457);
#1573=ELLIPSE('',#104973,20.5655942010141,0.575886853588054);
#1574=ELLIPSE('',#104986,0.0682531867157525,0.0644989639562768);
#1575=ELLIPSE('',#104988,0.0752932753414462,0.0683396339859915);
#1576=ELLIPSE('',#104990,0.0365824585612798,0.0343843127629466);
#1577=ELLIPSE('',#104991,0.0365824585612798,0.0343843127629466);
#1578=ELLIPSE('',#104994,20.5663123862977,0.575899628805844);
#1579=ELLIPSE('',#105007,0.068253186715127,0.064498963955807);
#1580=ELLIPSE('',#105009,0.0752932753417337,0.0683396339861055);
#1581=ELLIPSE('',#105011,0.0365824585612683,0.0343843127629441);
#1582=ELLIPSE('',#105012,0.0365824585612683,0.0343843127629441);
#1583=ELLIPSE('',#105015,20.5655922399963,0.575886817441797);
#1584=ELLIPSE('',#105028,0.0682531867100915,0.0644989639525808);
#1585=ELLIPSE('',#105030,0.0752932753384642,0.0683396339845221);
#1586=ELLIPSE('',#105032,0.0365824585612694,0.0343843127629441);
#1587=ELLIPSE('',#105033,0.0365824585612694,0.0343843127629441);
#1588=ELLIPSE('',#105036,20.5655714685528,0.575886444727038);
#1589=ELLIPSE('',#105049,0.0682531867063946,0.0644989639502737);
#1590=ELLIPSE('',#105051,0.0752932753406007,0.068339633985507);
#1591=ELLIPSE('',#105053,0.0365824585612642,0.034384312762943);
#1592=ELLIPSE('',#105054,0.0365824585612642,0.034384312762943);
#1593=ELLIPSE('',#105057,20.5655513367587,0.575886094758606);
#1594=ELLIPSE('',#105070,0.0682531867133225,0.064498963954612);
#1595=ELLIPSE('',#105072,0.0752932753383297,0.0683396339844693);
#1596=ELLIPSE('',#105074,0.0365824585612559,0.0343843127629409);
#1597=ELLIPSE('',#105075,0.0365824585612559,0.0343843127629409);
#1598=ELLIPSE('',#105078,20.5653884221969,0.575883206356478);
#1599=ELLIPSE('',#105091,0.0682531867116082,0.0644989639535029);
#1600=ELLIPSE('',#105093,0.0752932753428825,0.0683396339866211);
#1601=ELLIPSE('',#105095,0.0365824585612799,0.0343843127629468);
#1602=ELLIPSE('',#105096,0.0365824585612799,0.0343843127629468);
#1603=ELLIPSE('',#105099,20.5654095917158,0.575883579934909);
#1604=ELLIPSE('',#105112,0.0682531867092451,0.0644989639521952);
#1605=ELLIPSE('',#105114,0.0752932753342181,0.068339633982504);
#1606=ELLIPSE('',#105116,0.036582458561269,0.0343843127629441);
#1607=ELLIPSE('',#105117,0.036582458561269,0.0343843127629441);
#1608=ELLIPSE('',#105120,20.5668717945422,0.57590955878625);
#1609=ELLIPSE('',#105133,0.0682531867087737,0.0644989639517802);
#1610=ELLIPSE('',#105135,0.075293275340429,0.068339633985475);
#1611=ELLIPSE('',#105137,0.0365824585612684,0.0343843127629437);
#1612=ELLIPSE('',#105138,0.0365824585612684,0.0343843127629437);
#1613=ELLIPSE('',#105141,20.5665469813456,0.575903803880655);
#1614=ELLIPSE('',#105154,0.0682531867062315,0.0644989639502229);
#1615=ELLIPSE('',#105156,0.0752932753417253,0.0683396339860757);
#1616=ELLIPSE('',#105158,0.0365824585612617,0.0343843127629423);
#1617=ELLIPSE('',#105159,0.0365824585612617,0.0343843127629423);
#1618=ELLIPSE('',#105162,20.5651929436534,0.575879730590434);
#1619=ORIENTED_CLOSED_SHELL('',*,#94627,.F.);
#1620=BREP_WITH_VOIDS('Cover',#94628,(#1619));
#1621=TOROIDAL_SURFACE('',#95348,5.05,0.4);
#1622=TOROIDAL_SURFACE('',#95355,10.4999999997296,0.4);
#1623=TOROIDAL_SURFACE('',#95362,11.6,0.4);
#1624=TOROIDAL_SURFACE('',#95390,3.6,0.4);
#1625=TOROIDAL_SURFACE('',#95404,1.2,0.4);
#1626=TOROIDAL_SURFACE('',#95413,13.6,0.4);
#1627=TOROIDAL_SURFACE('',#95420,3.55,0.4);
#1628=TOROIDAL_SURFACE('',#95445,10.1000000149012,0.4);
#1629=TOROIDAL_SURFACE('',#95463,3.6,0.4);
#1630=TOROIDAL_SURFACE('',#95475,3.55,0.4);
#1631=TOROIDAL_SURFACE('',#95497,10.1000000149012,0.4);
#1632=TOROIDAL_SURFACE('',#95504,4.1,0.4);
#1633=TOROIDAL_SURFACE('',#95508,3.2,0.4);
#1634=TOROIDAL_SURFACE('',#95514,5.80000000000001,0.4);
#1635=TOROIDAL_SURFACE('',#95535,5.2,0.4);
#1636=TOROIDAL_SURFACE('',#95543,5.8,0.4);
#1637=TOROIDAL_SURFACE('',#95547,7.59496173936711,0.4);
#1638=TOROIDAL_SURFACE('',#95556,1.2,0.4);
#1639=TOROIDAL_SURFACE('',#95570,3.5,0.4);
#1640=TOROIDAL_SURFACE('',#95591,9.7949617393671,0.4);
#1641=TOROIDAL_SURFACE('',#95596,3.6,0.4);
#1642=TOROIDAL_SURFACE('',#95603,10.1,0.4);
#1643=TOROIDAL_SURFACE('',#95610,16.9949617393671,0.4);
#1644=TOROIDAL_SURFACE('',#95631,4.,0.4);
#1645=TOROIDAL_SURFACE('',#95639,23.3449617393671,0.4);
#1646=TOROIDAL_SURFACE('',#95643,0.8,0.4);
#1647=TOROIDAL_SURFACE('',#95647,8.2,0.4);
#1648=TOROIDAL_SURFACE('',#95669,19.3949617393671,0.4);
#1649=TOROIDAL_SURFACE('',#95676,10.1,0.4);
#1650=TOROIDAL_SURFACE('',#95699,5.05,0.4);
#1651=TOROIDAL_SURFACE('',#95707,13.,0.4);
#1652=TOROIDAL_SURFACE('',#95716,11.6,0.4);
#1653=TOROIDAL_SURFACE('',#95723,10.4999999997296,0.4);
#1654=TOROIDAL_SURFACE('',#95753,4.,0.4);
#1655=TOROIDAL_SURFACE('',#95760,13.6,0.4);
#1656=TOROIDAL_SURFACE('',#96072,5.05,0.4);
#1657=TOROIDAL_SURFACE('',#96090,11.,0.4);
#1658=TOROIDAL_SURFACE('',#96106,3.6,0.4);
#1659=TOROIDAL_SURFACE('',#96110,2.1,0.4);
#1660=TOROIDAL_SURFACE('',#96116,2.1,0.4);
#1661=TOROIDAL_SURFACE('',#96119,16.9949617393671,0.4);
#1662=TOROIDAL_SURFACE('',#96123,3.6,0.4);
#1663=TOROIDAL_SURFACE('',#96126,9.79496173936711,0.4);
#1664=TOROIDAL_SURFACE('',#96138,11.95,0.4);
#1665=TOROIDAL_SURFACE('',#96145,4.2,0.4);
#1666=TOROIDAL_SURFACE('',#96178,4.2,0.4);
#1667=TOROIDAL_SURFACE('',#96185,25.3449617393673,0.4);
#1668=TOROIDAL_SURFACE('',#96201,4.09750037145961,0.4);
#1669=TOROIDAL_SURFACE('',#96206,3.2,0.4);
#1670=TOROIDAL_SURFACE('',#96209,4.1,0.4);
#1671=TOROIDAL_SURFACE('',#96230,8.8,0.4);
#1672=TOROIDAL_SURFACE('',#96253,4.6,0.4);
#1673=TOROIDAL_SURFACE('',#96263,1.2,0.4);
#1674=TOROIDAL_SURFACE('',#96272,6.1,0.4);
#1675=TOROIDAL_SURFACE('',#96280,5.2,0.4);
#1676=TOROIDAL_SURFACE('',#96286,7.2949617393671,0.4);
#1677=TOROIDAL_SURFACE('',#96310,4.5,0.4);
#1678=TOROIDAL_SURFACE('',#96319,8.2,0.4);
#1679=TOROIDAL_SURFACE('',#96326,19.4949617393671,0.4);
#1680=TOROIDAL_SURFACE('',#96361,4.1,0.4);
#1681=TOROIDAL_SURFACE('',#96365,6.2,0.4);
#1682=TOROIDAL_SURFACE('',#96372,22.1949617393671,0.4);
#1683=TOROIDAL_SURFACE('',#96376,8.8,0.4);
#1684=TOROIDAL_SURFACE('',#96397,12.05,0.4);
#1685=TOROIDAL_SURFACE('',#96404,3.6,0.4);
#1686=TOROIDAL_SURFACE('',#96429,1.2,0.4);
#1687=TOROIDAL_SURFACE('',#96438,8.8,0.4);
#1688=TOROIDAL_SURFACE('',#96450,3.9,0.4);
#1689=TOROIDAL_SURFACE('',#96478,8.8,0.4);
#1690=TOROIDAL_SURFACE('',#96495,3.9,0.4);
#1691=TOROIDAL_SURFACE('',#96506,8.8,0.4);
#1692=TOROIDAL_SURFACE('',#96509,4.0975003714596,0.4);
#1693=TOROIDAL_SURFACE('',#96525,8.8,0.4);
#1694=TOROIDAL_SURFACE('',#96538,3.9,0.4);
#1695=TOROIDAL_SURFACE('',#96884,3.6,0.4);
#1696=TOROIDAL_SURFACE('',#96902,3.6,0.4);
#1697=TOROIDAL_SURFACE('',#96914,4.64877154610377,0.4);
#1698=TOROIDAL_SURFACE('',#97244,10.516666667,1.816666667);
#1699=TOROIDAL_SURFACE('',#97247,10.516666667,1.816666667);
#1700=TOROIDAL_SURFACE('',#97250,10.516666667,1.816666667);
#1701=TOROIDAL_SURFACE('',#97253,10.516666667,1.816666667);
#1702=TOROIDAL_SURFACE('',#97256,10.516666667,1.816666667);
#1703=TOROIDAL_SURFACE('',#97259,10.516666667,1.816666667);
#1704=TOROIDAL_SURFACE('',#97262,10.516666667,1.816666667);
#1705=TOROIDAL_SURFACE('',#97265,10.516666667,1.816666667);
#1706=TOROIDAL_SURFACE('',#97268,10.516666667,1.816666667);
#1707=TOROIDAL_SURFACE('',#97271,10.516666667,1.816666667);
#1708=TOROIDAL_SURFACE('',#97274,10.516666667,1.816666667);
#1709=TOROIDAL_SURFACE('',#97277,10.516666667,1.816666667);
#1710=TOROIDAL_SURFACE('',#97280,10.516666667,1.816666667);
#1711=TOROIDAL_SURFACE('',#97283,10.516666667,1.816666667);
#1712=TOROIDAL_SURFACE('',#97286,10.516666667,1.816666667);
#1713=TOROIDAL_SURFACE('',#97289,10.516666667,1.816666667);
#1714=TOROIDAL_SURFACE('',#97292,10.516666667,1.816666667);
#1715=TOROIDAL_SURFACE('',#97295,10.516666667,1.816666667);
#1716=TOROIDAL_SURFACE('',#97298,10.516666667,1.816666667);
#1717=TOROIDAL_SURFACE('',#97301,10.516666667,1.816666667);
#1718=TOROIDAL_SURFACE('',#97304,10.516666667,1.816666667);
#1719=TOROIDAL_SURFACE('',#97307,10.516666667,1.816666667);
#1720=TOROIDAL_SURFACE('',#97310,10.516666667,1.816666667);
#1721=TOROIDAL_SURFACE('',#97313,10.516666667,1.816666667);
#1722=TOROIDAL_SURFACE('',#97316,10.516666667,1.816666667);
#1723=TOROIDAL_SURFACE('',#97319,10.516666667,1.816666667);
#1724=TOROIDAL_SURFACE('',#97322,10.516666667,1.816666667);
#1725=TOROIDAL_SURFACE('',#97325,10.516666667,1.816666667);
#1726=TOROIDAL_SURFACE('',#97328,10.516666667,1.816666667);
#1727=TOROIDAL_SURFACE('',#97331,10.516666667,1.816666667);
#1728=TOROIDAL_SURFACE('',#97334,10.516666667,1.816666667);
#1729=TOROIDAL_SURFACE('',#97337,10.516666667,1.816666667);
#1730=TOROIDAL_SURFACE('',#97340,10.516666667,1.816666667);
#1731=TOROIDAL_SURFACE('',#97343,10.516666667,1.816666667);
#1732=TOROIDAL_SURFACE('',#97346,10.516666667,1.816666667);
#1733=TOROIDAL_SURFACE('',#97349,10.516666667,1.816666667);
#1734=TOROIDAL_SURFACE('',#97352,10.516666667,1.816666667);
#1735=TOROIDAL_SURFACE('',#97355,10.516666667,1.816666667);
#1736=TOROIDAL_SURFACE('',#97358,10.516666667,1.816666667);
#1737=TOROIDAL_SURFACE('',#97361,10.516666667,1.816666667);
#1738=TOROIDAL_SURFACE('',#97364,10.516666667,1.816666667);
#1739=TOROIDAL_SURFACE('',#97367,10.516666667,1.816666667);
#1740=TOROIDAL_SURFACE('',#97370,10.516666667,1.816666667);
#1741=TOROIDAL_SURFACE('',#97373,10.516666667,1.816666667);
#1742=TOROIDAL_SURFACE('',#97376,10.516666667,1.816666667);
#1743=TOROIDAL_SURFACE('',#97379,10.516666667,1.816666667);
#1744=TOROIDAL_SURFACE('',#97382,10.516666667,1.816666667);
#1745=TOROIDAL_SURFACE('',#97385,10.516666667,1.816666667);
#1746=TOROIDAL_SURFACE('',#97388,10.516666667,1.816666667);
#1747=TOROIDAL_SURFACE('',#97391,10.516666667,1.816666667);
#1748=TOROIDAL_SURFACE('',#97394,10.516666667,1.816666667);
#1749=TOROIDAL_SURFACE('',#97397,10.516666667,1.816666667);
#1750=TOROIDAL_SURFACE('',#97400,10.516666667,1.816666667);
#1751=TOROIDAL_SURFACE('',#97403,10.516666667,1.816666667);
#1752=TOROIDAL_SURFACE('',#97406,10.516666667,1.816666667);
#1753=TOROIDAL_SURFACE('',#97409,10.516666667,1.816666667);
#1754=TOROIDAL_SURFACE('',#97412,10.516666667,1.816666667);
#1755=TOROIDAL_SURFACE('',#97415,10.516666667,1.816666667);
#1756=TOROIDAL_SURFACE('',#97418,10.516666667,1.816666667);
#1757=TOROIDAL_SURFACE('',#97421,10.516666667,1.816666667);
#1758=TOROIDAL_SURFACE('',#97424,10.516666667,1.816666667);
#1759=TOROIDAL_SURFACE('',#97427,10.516666667,1.816666667);
#1760=TOROIDAL_SURFACE('',#97430,10.516666667,1.816666667);
#1761=TOROIDAL_SURFACE('',#97433,10.516666667,1.816666667);
#1762=TOROIDAL_SURFACE('',#97436,10.516666667,1.816666667);
#1763=TOROIDAL_SURFACE('',#97439,10.516666667,1.816666667);
#1764=TOROIDAL_SURFACE('',#97442,10.516666667,1.816666667);
#1765=TOROIDAL_SURFACE('',#97445,10.516666667,1.816666667);
#1766=TOROIDAL_SURFACE('',#97448,10.516666667,1.816666667);
#1767=TOROIDAL_SURFACE('',#97451,10.516666667,1.816666667);
#1768=TOROIDAL_SURFACE('',#97496,2.222884449,0.1);
#1769=TOROIDAL_SURFACE('',#97501,2.222884449,0.1);
#1770=TOROIDAL_SURFACE('',#97506,2.222884449,0.1);
#1771=TOROIDAL_SURFACE('',#97511,2.222884449,0.1);
#1772=TOROIDAL_SURFACE('',#97516,2.222884449,0.1);
#1773=TOROIDAL_SURFACE('',#97521,2.222884449,0.1);
#1774=TOROIDAL_SURFACE('',#97526,2.222884449,0.1);
#1775=TOROIDAL_SURFACE('',#97531,2.222884449,0.1);
#1776=TOROIDAL_SURFACE('',#97536,2.222884449,0.1);
#1777=TOROIDAL_SURFACE('',#97541,2.222884449,0.1);
#1778=TOROIDAL_SURFACE('',#97546,2.222884449,0.1);
#1779=TOROIDAL_SURFACE('',#97551,2.222884449,0.1);
#1780=TOROIDAL_SURFACE('',#97556,2.222884449,0.1);
#1781=TOROIDAL_SURFACE('',#97561,2.222884449,0.1);
#1782=TOROIDAL_SURFACE('',#97566,2.222884449,0.1);
#1783=TOROIDAL_SURFACE('',#97571,2.222884449,0.1);
#1784=TOROIDAL_SURFACE('',#97576,2.222884449,0.1);
#1785=TOROIDAL_SURFACE('',#97581,2.222884449,0.1);
#1786=TOROIDAL_SURFACE('',#97586,2.222884449,0.1);
#1787=TOROIDAL_SURFACE('',#97591,2.222884449,0.1);
#1788=TOROIDAL_SURFACE('',#97596,2.222884449,0.1);
#1789=TOROIDAL_SURFACE('',#97601,2.222884449,0.1);
#1790=TOROIDAL_SURFACE('',#97606,2.222884449,0.1);
#1791=TOROIDAL_SURFACE('',#97611,2.222884449,0.1);
#1792=TOROIDAL_SURFACE('',#97616,2.222884449,0.1);
#1793=TOROIDAL_SURFACE('',#97621,2.222884449,0.1);
#1794=TOROIDAL_SURFACE('',#97626,2.222884449,0.1);
#1795=TOROIDAL_SURFACE('',#97631,2.222884449,0.1);
#1796=TOROIDAL_SURFACE('',#97636,2.222884449,0.1);
#1797=TOROIDAL_SURFACE('',#97641,2.222884449,0.1);
#1798=TOROIDAL_SURFACE('',#97646,2.222884449,0.1);
#1799=TOROIDAL_SURFACE('',#97651,2.222884449,0.1);
#1800=TOROIDAL_SURFACE('',#97656,2.222884449,0.1);
#1801=TOROIDAL_SURFACE('',#97661,2.222884449,0.1);
#1802=TOROIDAL_SURFACE('',#97666,2.222884449,0.1);
#1803=TOROIDAL_SURFACE('',#97671,2.222884449,0.1);
#1804=TOROIDAL_SURFACE('',#97676,2.222884449,0.1);
#1805=TOROIDAL_SURFACE('',#97681,2.222884449,0.1);
#1806=TOROIDAL_SURFACE('',#97686,2.222884449,0.1);
#1807=TOROIDAL_SURFACE('',#97691,2.222884449,0.1);
#1808=TOROIDAL_SURFACE('',#97696,2.222884449,0.1);
#1809=TOROIDAL_SURFACE('',#97701,2.222884449,0.1);
#1810=TOROIDAL_SURFACE('',#97706,2.222884449,0.1);
#1811=TOROIDAL_SURFACE('',#97711,2.222884449,0.1);
#1812=TOROIDAL_SURFACE('',#97716,2.222884449,0.1);
#1813=TOROIDAL_SURFACE('',#97721,2.222884449,0.1);
#1814=TOROIDAL_SURFACE('',#97726,2.222884449,0.1);
#1815=TOROIDAL_SURFACE('',#97731,2.222884449,0.1);
#1816=TOROIDAL_SURFACE('',#97736,2.222884449,0.1);
#1817=TOROIDAL_SURFACE('',#97741,2.222884449,0.1);
#1818=TOROIDAL_SURFACE('',#97746,2.222884449,0.1);
#1819=TOROIDAL_SURFACE('',#97751,2.222884449,0.1);
#1820=TOROIDAL_SURFACE('',#97756,2.222884449,0.1);
#1821=TOROIDAL_SURFACE('',#97761,2.222884449,0.1);
#1822=TOROIDAL_SURFACE('',#97766,2.222884449,0.1);
#1823=TOROIDAL_SURFACE('',#97771,2.222884449,0.1);
#1824=TOROIDAL_SURFACE('',#97776,2.222884449,0.1);
#1825=TOROIDAL_SURFACE('',#97781,2.222884449,0.1);
#1826=TOROIDAL_SURFACE('',#97786,2.222884449,0.1);
#1827=TOROIDAL_SURFACE('',#97791,2.222884449,0.1);
#1828=TOROIDAL_SURFACE('',#97796,2.222884449,0.1);
#1829=TOROIDAL_SURFACE('',#97801,2.222884449,0.1);
#1830=TOROIDAL_SURFACE('',#97806,2.222884449,0.1);
#1831=TOROIDAL_SURFACE('',#97811,2.222884449,0.1);
#1832=TOROIDAL_SURFACE('',#97816,2.222884449,0.1);
#1833=TOROIDAL_SURFACE('',#97821,2.222884449,0.1);
#1834=TOROIDAL_SURFACE('',#97826,2.222884449,0.1);
#1835=TOROIDAL_SURFACE('',#97831,2.222884449,0.1);
#1836=TOROIDAL_SURFACE('',#97836,2.222884449,0.1);
#1837=TOROIDAL_SURFACE('',#97841,2.222884449,0.1);
#1838=TOROIDAL_SURFACE('',#97850,1.6,0.1);
#1839=TOROIDAL_SURFACE('',#97854,1.6,0.1);
#1840=TOROIDAL_SURFACE('',#97858,1.7,0.2);
#1841=TOROIDAL_SURFACE('',#97863,1.7,0.2);
#1842=TOROIDAL_SURFACE('',#97867,2.8,0.2);
#1843=TOROIDAL_SURFACE('',#97872,0.6,0.2);
#1844=TOROIDAL_SURFACE('',#97877,0.6,0.2);
#1845=TOROIDAL_SURFACE('',#97882,3.9,0.4);
#1846=TOROIDAL_SURFACE('',#97887,1.1,0.4);
#1847=TOROIDAL_SURFACE('',#97892,1.1,0.4);
#1848=TOROIDAL_SURFACE('',#98404,0.6,0.2);
#1849=TOROIDAL_SURFACE('',#98409,7.4,0.2);
#1850=TOROIDAL_SURFACE('',#98410,0.6,0.2);
#1851=TOROIDAL_SURFACE('',#98412,4.8,0.2);
#1852=TOROIDAL_SURFACE('',#98416,0.6,0.2);
#1853=TOROIDAL_SURFACE('',#98417,0.6,0.2);
#1854=TOROIDAL_SURFACE('',#98420,4.8,0.2);
#1855=TOROIDAL_SURFACE('',#98423,0.6,0.2);
#1856=TOROIDAL_SURFACE('',#98427,7.4,0.2);
#1857=TOROIDAL_SURFACE('',#98429,0.6,0.2);
#1858=TOROIDAL_SURFACE('',#98857,1.76666666666667,0.166666666666667);
#1859=TOROIDAL_SURFACE('',#98884,2.23333333333333,0.166666666666667);
#1860=TOROIDAL_SURFACE('',#98908,2.23333333333333,0.166666666666667);
#1861=TOROIDAL_SURFACE('',#98913,1.76666666666667,0.166666666666667);
#1862=TOROIDAL_SURFACE('',#99175,2.25,0.576463888168111);
#1863=TOROIDAL_SURFACE('',#99190,2.25,0.57646388816811);
#1864=TOROIDAL_SURFACE('',#99456,1.625,0.125);
#1865=TOROIDAL_SURFACE('',#99468,2.50721825406948,0.0550000000000003);
#1866=TOROIDAL_SURFACE('',#99474,2.695,0.0550000000000007);
#1867=TOROIDAL_SURFACE('',#99677,2.50721825406948,0.0549999999999999);
#1868=TOROIDAL_SURFACE('',#100074,2.695,0.0550000000000003);
#1869=TOROIDAL_SURFACE('',#100077,2.695,0.0550000000000003);
#1870=TOROIDAL_SURFACE('',#100080,2.695,0.0550000000000003);
#1871=TOROIDAL_SURFACE('',#100083,2.695,0.0550000000000003);
#1872=TOROIDAL_SURFACE('',#100086,2.695,0.0550000000000003);
#1873=TOROIDAL_SURFACE('',#100089,2.695,0.0550000000000003);
#1874=TOROIDAL_SURFACE('',#100092,2.695,0.0550000000000003);
#1875=TOROIDAL_SURFACE('',#100095,2.695,0.0550000000000003);
#1876=TOROIDAL_SURFACE('',#100098,2.695,0.0550000000000003);
#1877=TOROIDAL_SURFACE('',#100101,2.695,0.0550000000000003);
#1878=TOROIDAL_SURFACE('',#100104,2.695,0.0550000000000003);
#1879=TOROIDAL_SURFACE('',#100107,2.695,0.0550000000000003);
#1880=TOROIDAL_SURFACE('',#100110,2.695,0.0550000000000003);
#1881=TOROIDAL_SURFACE('',#100113,2.695,0.0550000000000003);
#1882=TOROIDAL_SURFACE('',#100116,2.695,0.0550000000000003);
#1883=TOROIDAL_SURFACE('',#100119,2.695,0.0550000000000003);
#1884=TOROIDAL_SURFACE('',#100122,2.695,0.0550000000000003);
#1885=TOROIDAL_SURFACE('',#100125,2.695,0.0550000000000003);
#1886=TOROIDAL_SURFACE('',#100128,2.695,0.0550000000000003);
#1887=TOROIDAL_SURFACE('',#100131,2.695,0.0550000000000003);
#1888=TOROIDAL_SURFACE('',#100134,2.695,0.0550000000000003);
#1889=TOROIDAL_SURFACE('',#100137,2.695,0.0550000000000003);
#1890=TOROIDAL_SURFACE('',#100140,2.695,0.0550000000000003);
#1891=TOROIDAL_SURFACE('',#100143,2.695,0.0550000000000003);
#1892=TOROIDAL_SURFACE('',#100146,2.695,0.0550000000000003);
#1893=TOROIDAL_SURFACE('',#100149,2.695,0.0550000000000003);
#1894=TOROIDAL_SURFACE('',#100152,2.695,0.0550000000000003);
#1895=TOROIDAL_SURFACE('',#100155,2.695,0.0550000000000003);
#1896=TOROIDAL_SURFACE('',#100158,2.695,0.0550000000000003);
#1897=TOROIDAL_SURFACE('',#100161,2.695,0.0550000000000003);
#1898=TOROIDAL_SURFACE('',#100164,2.695,0.0550000000000003);
#1899=TOROIDAL_SURFACE('',#100167,2.695,0.0550000000000003);
#1900=TOROIDAL_SURFACE('',#100170,2.695,0.0550000000000003);
#1901=TOROIDAL_SURFACE('',#100173,2.695,0.0550000000000003);
#1902=TOROIDAL_SURFACE('',#100176,2.695,0.0550000000000003);
#1903=TOROIDAL_SURFACE('',#100179,2.695,0.0550000000000003);
#1904=TOROIDAL_SURFACE('',#100182,2.695,0.0550000000000003);
#1905=TOROIDAL_SURFACE('',#100185,2.695,0.0550000000000003);
#1906=TOROIDAL_SURFACE('',#100188,2.695,0.0550000000000003);
#1907=TOROIDAL_SURFACE('',#100191,2.695,0.0550000000000003);
#1908=TOROIDAL_SURFACE('',#100194,2.695,0.0550000000000003);
#1909=TOROIDAL_SURFACE('',#100197,2.695,0.0550000000000003);
#1910=TOROIDAL_SURFACE('',#100200,2.695,0.0550000000000003);
#1911=TOROIDAL_SURFACE('',#100203,2.695,0.0550000000000003);
#1912=TOROIDAL_SURFACE('',#100206,2.695,0.0550000000000003);
#1913=TOROIDAL_SURFACE('',#100209,2.695,0.0550000000000003);
#1914=TOROIDAL_SURFACE('',#100212,2.695,0.0550000000000003);
#1915=TOROIDAL_SURFACE('',#100215,2.695,0.0550000000000003);
#1916=TOROIDAL_SURFACE('',#100218,2.695,0.0550000000000003);
#1917=TOROIDAL_SURFACE('',#100221,2.695,0.0550000000000003);
#1918=TOROIDAL_SURFACE('',#100224,2.695,0.0550000000000003);
#1919=TOROIDAL_SURFACE('',#100227,2.695,0.0550000000000003);
#1920=TOROIDAL_SURFACE('',#100230,2.695,0.0550000000000003);
#1921=TOROIDAL_SURFACE('',#100233,2.695,0.0550000000000003);
#1922=TOROIDAL_SURFACE('',#100236,2.695,0.0550000000000003);
#1923=TOROIDAL_SURFACE('',#100239,2.695,0.0550000000000003);
#1924=TOROIDAL_SURFACE('',#100242,2.695,0.0550000000000003);
#1925=TOROIDAL_SURFACE('',#100245,2.695,0.0550000000000003);
#1926=TOROIDAL_SURFACE('',#100248,2.695,0.0550000000000003);
#1927=TOROIDAL_SURFACE('',#100251,2.695,0.0550000000000003);
#1928=TOROIDAL_SURFACE('',#100254,2.695,0.0550000000000003);
#1929=TOROIDAL_SURFACE('',#100257,2.695,0.0550000000000003);
#1930=TOROIDAL_SURFACE('',#100260,2.695,0.0550000000000003);
#1931=TOROIDAL_SURFACE('',#100263,2.695,0.0550000000000003);
#1932=TOROIDAL_SURFACE('',#100266,2.695,0.0550000000000003);
#1933=TOROIDAL_SURFACE('',#100269,2.695,0.0550000000000003);
#1934=TOROIDAL_SURFACE('',#100272,2.695,0.0550000000000003);
#1935=TOROIDAL_SURFACE('',#100275,2.695,0.0550000000000003);
#1936=TOROIDAL_SURFACE('',#100278,2.695,0.0550000000000003);
#1937=TOROIDAL_SURFACE('',#100281,2.695,0.0550000000000003);
#1938=TOROIDAL_SURFACE('',#100284,2.695,0.0550000000000003);
#1939=TOROIDAL_SURFACE('',#100287,2.695,0.0550000000000003);
#1940=TOROIDAL_SURFACE('',#100290,2.695,0.0550000000000003);
#1941=TOROIDAL_SURFACE('',#100293,2.695,0.0550000000000003);
#1942=TOROIDAL_SURFACE('',#100296,2.695,0.0550000000000003);
#1943=TOROIDAL_SURFACE('',#100299,2.695,0.0550000000000003);
#1944=TOROIDAL_SURFACE('',#100302,2.695,0.0550000000000003);
#1945=TOROIDAL_SURFACE('',#100305,2.695,0.0550000000000003);
#1946=TOROIDAL_SURFACE('',#100308,2.695,0.0550000000000003);
#1947=TOROIDAL_SURFACE('',#100311,2.695,0.0550000000000003);
#1948=TOROIDAL_SURFACE('',#100314,2.695,0.0550000000000003);
#1949=TOROIDAL_SURFACE('',#100317,2.695,0.0550000000000003);
#1950=TOROIDAL_SURFACE('',#100320,2.695,0.0550000000000003);
#1951=TOROIDAL_SURFACE('',#100323,2.695,0.0550000000000003);
#1952=TOROIDAL_SURFACE('',#100326,2.695,0.0550000000000003);
#1953=TOROIDAL_SURFACE('',#100329,2.695,0.0550000000000003);
#1954=TOROIDAL_SURFACE('',#100332,2.695,0.0550000000000003);
#1955=TOROIDAL_SURFACE('',#100335,2.695,0.0550000000000003);
#1956=TOROIDAL_SURFACE('',#100338,2.695,0.0550000000000003);
#1957=TOROIDAL_SURFACE('',#100341,2.695,0.0550000000000003);
#1958=TOROIDAL_SURFACE('',#100344,2.695,0.0550000000000003);
#1959=TOROIDAL_SURFACE('',#100347,2.695,0.0550000000000003);
#1960=TOROIDAL_SURFACE('',#100350,2.695,0.0550000000000003);
#1961=TOROIDAL_SURFACE('',#100353,2.695,0.0550000000000003);
#1962=TOROIDAL_SURFACE('',#100356,2.695,0.0550000000000003);
#1963=TOROIDAL_SURFACE('',#100359,2.695,0.0550000000000003);
#1964=TOROIDAL_SURFACE('',#100362,2.695,0.0550000000000003);
#1965=TOROIDAL_SURFACE('',#100382,2.695,0.0550000000000003);
#1966=TOROIDAL_SURFACE('',#100409,2.7375,0.0125);
#1967=TOROIDAL_SURFACE('',#100425,2.7375,0.0125);
#1968=TOROIDAL_SURFACE('',#100448,2.7375,0.0125);
#1969=TOROIDAL_SURFACE('',#100471,2.7375,0.0125);
#1970=TOROIDAL_SURFACE('',#100494,2.7375,0.0125);
#1971=TOROIDAL_SURFACE('',#100517,2.7375,0.0125);
#1972=TOROIDAL_SURFACE('',#100540,2.7375,0.0125);
#1973=TOROIDAL_SURFACE('',#100563,2.7375,0.0125);
#1974=TOROIDAL_SURFACE('',#100586,2.7375,0.0125);
#1975=TOROIDAL_SURFACE('',#100609,2.7375,0.0125);
#1976=TOROIDAL_SURFACE('',#100632,2.7375,0.0125);
#1977=TOROIDAL_SURFACE('',#100655,2.7375,0.0125);
#1978=TOROIDAL_SURFACE('',#100678,2.7375,0.0125);
#1979=TOROIDAL_SURFACE('',#100701,2.7375,0.0125);
#1980=TOROIDAL_SURFACE('',#100724,2.7375,0.0125);
#1981=TOROIDAL_SURFACE('',#100747,2.7375,0.0125);
#1982=TOROIDAL_SURFACE('',#100770,2.7375,0.0125);
#1983=TOROIDAL_SURFACE('',#100793,2.7375,0.0125);
#1984=TOROIDAL_SURFACE('',#100816,2.7375,0.0125);
#1985=TOROIDAL_SURFACE('',#100839,2.7375,0.0125);
#1986=TOROIDAL_SURFACE('',#100862,2.7375,0.0125);
#1987=TOROIDAL_SURFACE('',#100885,2.7375,0.0125);
#1988=TOROIDAL_SURFACE('',#100908,2.7375,0.0125);
#1989=TOROIDAL_SURFACE('',#100931,2.7375,0.0125);
#1990=TOROIDAL_SURFACE('',#100954,2.7375,0.0125);
#1991=TOROIDAL_SURFACE('',#100977,2.7375,0.0125);
#1992=TOROIDAL_SURFACE('',#101000,2.7375,0.0125);
#1993=TOROIDAL_SURFACE('',#101023,2.7375,0.0125);
#1994=TOROIDAL_SURFACE('',#101046,2.7375,0.0125);
#1995=TOROIDAL_SURFACE('',#101069,2.7375,0.0125);
#1996=TOROIDAL_SURFACE('',#101092,2.7375,0.0125);
#1997=TOROIDAL_SURFACE('',#101115,2.7375,0.0125);
#1998=TOROIDAL_SURFACE('',#101138,2.7375,0.0125);
#1999=TOROIDAL_SURFACE('',#101161,2.7375,0.0125);
#2000=TOROIDAL_SURFACE('',#101184,2.7375,0.0125);
#2001=TOROIDAL_SURFACE('',#101207,2.7375,0.0125);
#2002=TOROIDAL_SURFACE('',#101230,2.7375,0.0125);
#2003=TOROIDAL_SURFACE('',#101253,2.7375,0.0125);
#2004=TOROIDAL_SURFACE('',#101276,2.7375,0.0125);
#2005=TOROIDAL_SURFACE('',#101299,2.7375,0.0125);
#2006=TOROIDAL_SURFACE('',#101322,2.7375,0.0125);
#2007=TOROIDAL_SURFACE('',#101345,2.7375,0.0125);
#2008=TOROIDAL_SURFACE('',#101368,2.7375,0.0125);
#2009=TOROIDAL_SURFACE('',#101391,2.7375,0.0125);
#2010=TOROIDAL_SURFACE('',#101414,2.7375,0.0125);
#2011=TOROIDAL_SURFACE('',#101437,2.7375,0.0125);
#2012=TOROIDAL_SURFACE('',#101460,2.7375,0.0125);
#2013=TOROIDAL_SURFACE('',#101483,2.7375,0.0125);
#2014=TOROIDAL_SURFACE('',#101506,2.7375,0.0125);
#2015=TOROIDAL_SURFACE('',#101529,2.7375,0.0125);
#2016=TOROIDAL_SURFACE('',#101552,2.7375,0.0125);
#2017=TOROIDAL_SURFACE('',#101575,2.7375,0.0125);
#2018=TOROIDAL_SURFACE('',#101598,2.7375,0.0125);
#2019=TOROIDAL_SURFACE('',#101621,2.7375,0.0125);
#2020=TOROIDAL_SURFACE('',#101644,2.7375,0.0125);
#2021=TOROIDAL_SURFACE('',#101667,2.7375,0.0125);
#2022=TOROIDAL_SURFACE('',#101690,2.7375,0.0125);
#2023=TOROIDAL_SURFACE('',#101713,2.7375,0.0125);
#2024=TOROIDAL_SURFACE('',#101736,2.7375,0.0125);
#2025=TOROIDAL_SURFACE('',#101759,2.7375,0.0125);
#2026=TOROIDAL_SURFACE('',#101782,2.7375,0.0125);
#2027=TOROIDAL_SURFACE('',#101805,2.7375,0.0125);
#2028=TOROIDAL_SURFACE('',#101828,2.7375,0.0125);
#2029=TOROIDAL_SURFACE('',#101851,2.7375,0.0125);
#2030=TOROIDAL_SURFACE('',#101874,2.7375,0.0125);
#2031=TOROIDAL_SURFACE('',#101897,2.7375,0.0125);
#2032=TOROIDAL_SURFACE('',#101920,2.7375,0.0125);
#2033=TOROIDAL_SURFACE('',#101943,2.7375,0.0125);
#2034=TOROIDAL_SURFACE('',#101966,2.7375,0.0125);
#2035=TOROIDAL_SURFACE('',#101989,2.7375,0.0125);
#2036=TOROIDAL_SURFACE('',#102012,2.7375,0.0125);
#2037=TOROIDAL_SURFACE('',#102035,2.7375,0.0125);
#2038=TOROIDAL_SURFACE('',#102058,2.7375,0.0125);
#2039=TOROIDAL_SURFACE('',#102081,2.7375,0.0125);
#2040=TOROIDAL_SURFACE('',#102104,2.7375,0.0125);
#2041=TOROIDAL_SURFACE('',#102127,2.7375,0.0125);
#2042=TOROIDAL_SURFACE('',#102150,2.7375,0.0125);
#2043=TOROIDAL_SURFACE('',#102173,2.7375,0.0125);
#2044=TOROIDAL_SURFACE('',#102196,2.7375,0.0125);
#2045=TOROIDAL_SURFACE('',#102219,2.7375,0.0125);
#2046=TOROIDAL_SURFACE('',#102242,2.7375,0.0125);
#2047=TOROIDAL_SURFACE('',#102265,2.7375,0.0125);
#2048=TOROIDAL_SURFACE('',#102288,2.7375,0.0125);
#2049=TOROIDAL_SURFACE('',#102311,2.7375,0.0125);
#2050=TOROIDAL_SURFACE('',#102334,2.7375,0.0125);
#2051=TOROIDAL_SURFACE('',#102357,2.7375,0.0125);
#2052=TOROIDAL_SURFACE('',#102380,2.7375,0.0125);
#2053=TOROIDAL_SURFACE('',#102403,2.7375,0.0125);
#2054=TOROIDAL_SURFACE('',#102426,2.7375,0.0125);
#2055=TOROIDAL_SURFACE('',#102449,2.7375,0.0125);
#2056=TOROIDAL_SURFACE('',#102472,2.7375,0.0125);
#2057=TOROIDAL_SURFACE('',#102495,2.7375,0.0125);
#2058=TOROIDAL_SURFACE('',#102518,2.7375,0.0125);
#2059=TOROIDAL_SURFACE('',#102541,2.7375,0.0125);
#2060=TOROIDAL_SURFACE('',#102564,2.7375,0.0125);
#2061=TOROIDAL_SURFACE('',#102587,2.7375,0.0125);
#2062=TOROIDAL_SURFACE('',#102610,2.7375,0.0125);
#2063=TOROIDAL_SURFACE('',#102633,2.7375,0.0125);
#2064=TOROIDAL_SURFACE('',#102728,2.728,0.022);
#2065=TOROIDAL_SURFACE('',#102733,2.728,0.022);
#2066=TOROIDAL_SURFACE('',#102738,2.728,0.022);
#2067=TOROIDAL_SURFACE('',#102743,2.728,0.022);
#2068=TOROIDAL_SURFACE('',#102748,2.728,0.022);
#2069=TOROIDAL_SURFACE('',#102753,2.728,0.022);
#2070=TOROIDAL_SURFACE('',#102758,2.728,0.022);
#2071=TOROIDAL_SURFACE('',#102763,2.728,0.022);
#2072=TOROIDAL_SURFACE('',#102768,2.728,0.022);
#2073=TOROIDAL_SURFACE('',#102773,2.728,0.022);
#2074=TOROIDAL_SURFACE('',#102778,2.728,0.022);
#2075=TOROIDAL_SURFACE('',#102783,2.728,0.022);
#2076=TOROIDAL_SURFACE('',#102788,2.728,0.022);
#2077=TOROIDAL_SURFACE('',#102793,2.728,0.022);
#2078=TOROIDAL_SURFACE('',#102798,2.728,0.022);
#2079=TOROIDAL_SURFACE('',#102803,2.728,0.022);
#2080=TOROIDAL_SURFACE('',#102808,2.728,0.022);
#2081=TOROIDAL_SURFACE('',#102813,2.728,0.022);
#2082=TOROIDAL_SURFACE('',#102818,2.728,0.022);
#2083=TOROIDAL_SURFACE('',#102823,2.728,0.022);
#2084=TOROIDAL_SURFACE('',#102828,2.728,0.022);
#2085=TOROIDAL_SURFACE('',#102833,2.728,0.022);
#2086=TOROIDAL_SURFACE('',#102838,2.728,0.022);
#2087=TOROIDAL_SURFACE('',#102843,2.728,0.022);
#2088=TOROIDAL_SURFACE('',#102848,2.728,0.022);
#2089=TOROIDAL_SURFACE('',#102853,2.728,0.022);
#2090=TOROIDAL_SURFACE('',#102858,2.728,0.022);
#2091=TOROIDAL_SURFACE('',#102863,2.728,0.022);
#2092=TOROIDAL_SURFACE('',#102868,2.728,0.022);
#2093=TOROIDAL_SURFACE('',#102873,2.728,0.022);
#2094=TOROIDAL_SURFACE('',#102878,2.728,0.022);
#2095=TOROIDAL_SURFACE('',#102883,2.728,0.022);
#2096=TOROIDAL_SURFACE('',#102888,2.728,0.022);
#2097=TOROIDAL_SURFACE('',#102893,2.728,0.022);
#2098=TOROIDAL_SURFACE('',#102898,2.728,0.022);
#2099=TOROIDAL_SURFACE('',#102903,2.728,0.022);
#2100=TOROIDAL_SURFACE('',#102908,2.728,0.022);
#2101=TOROIDAL_SURFACE('',#102913,2.728,0.022);
#2102=TOROIDAL_SURFACE('',#102918,2.728,0.022);
#2103=TOROIDAL_SURFACE('',#102923,2.728,0.022);
#2104=TOROIDAL_SURFACE('',#102928,2.728,0.022);
#2105=TOROIDAL_SURFACE('',#102933,2.728,0.022);
#2106=TOROIDAL_SURFACE('',#102938,2.728,0.022);
#2107=TOROIDAL_SURFACE('',#102943,2.728,0.022);
#2108=TOROIDAL_SURFACE('',#102948,2.728,0.022);
#2109=TOROIDAL_SURFACE('',#102953,2.728,0.022);
#2110=TOROIDAL_SURFACE('',#102958,2.728,0.022);
#2111=TOROIDAL_SURFACE('',#102963,2.728,0.022);
#2112=TOROIDAL_SURFACE('',#102968,2.728,0.022);
#2113=TOROIDAL_SURFACE('',#102973,2.728,0.022);
#2114=TOROIDAL_SURFACE('',#102978,2.728,0.022);
#2115=TOROIDAL_SURFACE('',#102983,2.728,0.022);
#2116=TOROIDAL_SURFACE('',#102988,2.728,0.022);
#2117=TOROIDAL_SURFACE('',#102993,2.728,0.022);
#2118=TOROIDAL_SURFACE('',#102998,2.728,0.022);
#2119=TOROIDAL_SURFACE('',#103003,2.728,0.022);
#2120=TOROIDAL_SURFACE('',#103008,2.728,0.022);
#2121=TOROIDAL_SURFACE('',#103013,2.728,0.022);
#2122=TOROIDAL_SURFACE('',#103018,2.728,0.022);
#2123=TOROIDAL_SURFACE('',#103023,2.728,0.022);
#2124=TOROIDAL_SURFACE('',#103028,2.728,0.022);
#2125=TOROIDAL_SURFACE('',#103033,2.728,0.022);
#2126=TOROIDAL_SURFACE('',#103038,2.728,0.022);
#2127=TOROIDAL_SURFACE('',#103043,2.728,0.022);
#2128=TOROIDAL_SURFACE('',#103048,2.728,0.022);
#2129=TOROIDAL_SURFACE('',#103053,2.728,0.022);
#2130=TOROIDAL_SURFACE('',#103058,2.728,0.022);
#2131=TOROIDAL_SURFACE('',#103063,2.728,0.022);
#2132=TOROIDAL_SURFACE('',#103068,2.728,0.022);
#2133=TOROIDAL_SURFACE('',#103073,2.728,0.022);
#2134=TOROIDAL_SURFACE('',#103078,2.728,0.022);
#2135=TOROIDAL_SURFACE('',#103083,2.728,0.022);
#2136=TOROIDAL_SURFACE('',#103088,2.728,0.022);
#2137=TOROIDAL_SURFACE('',#103093,2.728,0.022);
#2138=TOROIDAL_SURFACE('',#103098,2.728,0.022);
#2139=TOROIDAL_SURFACE('',#103103,2.728,0.022);
#2140=TOROIDAL_SURFACE('',#103108,2.728,0.022);
#2141=TOROIDAL_SURFACE('',#103129,2.49354920651122,0.0879999999999989);
#2142=TOROIDAL_SURFACE('',#103135,2.662,0.088000000000018);
#2143=TOROIDAL_SURFACE('',#103219,2.49354920651117,0.0879999999999994);
#2144=TOROIDAL_SURFACE('',#103300,2.662,0.0879999999999984);
#2145=TOROIDAL_SURFACE('',#103303,2.662,0.0879999999999984);
#2146=TOROIDAL_SURFACE('',#103306,2.662,0.0879999999999984);
#2147=TOROIDAL_SURFACE('',#103309,2.662,0.0879999999999984);
#2148=TOROIDAL_SURFACE('',#103312,2.662,0.0879999999999984);
#2149=TOROIDAL_SURFACE('',#103315,2.662,0.0879999999999984);
#2150=TOROIDAL_SURFACE('',#103318,2.662,0.0879999999999984);
#2151=TOROIDAL_SURFACE('',#103321,2.662,0.0879999999999984);
#2152=TOROIDAL_SURFACE('',#103324,2.662,0.0879999999999984);
#2153=TOROIDAL_SURFACE('',#103327,2.662,0.0879999999999984);
#2154=TOROIDAL_SURFACE('',#103330,2.662,0.0879999999999984);
#2155=TOROIDAL_SURFACE('',#103333,2.662,0.0879999999999984);
#2156=TOROIDAL_SURFACE('',#103336,2.662,0.0879999999999984);
#2157=TOROIDAL_SURFACE('',#103339,2.662,0.0879999999999984);
#2158=TOROIDAL_SURFACE('',#103342,2.662,0.0879999999999984);
#2159=TOROIDAL_SURFACE('',#103345,2.662,0.0879999999999984);
#2160=TOROIDAL_SURFACE('',#103348,2.662,0.0879999999999984);
#2161=TOROIDAL_SURFACE('',#103351,2.662,0.0879999999999984);
#2162=TOROIDAL_SURFACE('',#103354,2.662,0.0879999999999984);
#2163=TOROIDAL_SURFACE('',#103357,2.662,0.0879999999999984);
#2164=TOROIDAL_SURFACE('',#103360,2.662,0.0879999999999984);
#2165=TOROIDAL_SURFACE('',#103363,2.662,0.0879999999999984);
#2166=TOROIDAL_SURFACE('',#103366,2.662,0.0879999999999984);
#2167=TOROIDAL_SURFACE('',#103369,2.662,0.0879999999999984);
#2168=TOROIDAL_SURFACE('',#103372,2.662,0.0879999999999984);
#2169=TOROIDAL_SURFACE('',#103375,2.662,0.0879999999999984);
#2170=TOROIDAL_SURFACE('',#103378,2.662,0.0879999999999984);
#2171=TOROIDAL_SURFACE('',#103381,2.662,0.0879999999999984);
#2172=TOROIDAL_SURFACE('',#103384,2.662,0.0879999999999984);
#2173=TOROIDAL_SURFACE('',#103387,2.662,0.0879999999999984);
#2174=TOROIDAL_SURFACE('',#103390,2.662,0.0879999999999984);
#2175=TOROIDAL_SURFACE('',#103393,2.662,0.0879999999999984);
#2176=TOROIDAL_SURFACE('',#103396,2.662,0.0879999999999984);
#2177=TOROIDAL_SURFACE('',#103399,2.662,0.0879999999999984);
#2178=TOROIDAL_SURFACE('',#103402,2.662,0.0879999999999984);
#2179=TOROIDAL_SURFACE('',#103405,2.662,0.0879999999999984);
#2180=TOROIDAL_SURFACE('',#103408,2.662,0.0879999999999984);
#2181=TOROIDAL_SURFACE('',#103411,2.662,0.0879999999999984);
#2182=TOROIDAL_SURFACE('',#103414,2.662,0.0879999999999984);
#2183=TOROIDAL_SURFACE('',#103417,2.662,0.0879999999999984);
#2184=TOROIDAL_SURFACE('',#103420,2.662,0.0879999999999984);
#2185=TOROIDAL_SURFACE('',#103423,2.662,0.0879999999999984);
#2186=TOROIDAL_SURFACE('',#103426,2.662,0.0879999999999984);
#2187=TOROIDAL_SURFACE('',#103429,2.662,0.0879999999999984);
#2188=TOROIDAL_SURFACE('',#103432,2.662,0.0879999999999984);
#2189=TOROIDAL_SURFACE('',#103435,2.662,0.0879999999999984);
#2190=TOROIDAL_SURFACE('',#103438,2.662,0.0879999999999984);
#2191=TOROIDAL_SURFACE('',#103441,2.662,0.0879999999999984);
#2192=TOROIDAL_SURFACE('',#103444,2.662,0.0879999999999984);
#2193=TOROIDAL_SURFACE('',#103447,2.662,0.0879999999999984);
#2194=TOROIDAL_SURFACE('',#103450,2.662,0.0879999999999984);
#2195=TOROIDAL_SURFACE('',#103453,2.662,0.0879999999999984);
#2196=TOROIDAL_SURFACE('',#103456,2.662,0.0879999999999984);
#2197=TOROIDAL_SURFACE('',#103459,2.662,0.0879999999999984);
#2198=TOROIDAL_SURFACE('',#103462,2.662,0.0879999999999984);
#2199=TOROIDAL_SURFACE('',#103465,2.662,0.0879999999999984);
#2200=TOROIDAL_SURFACE('',#103468,2.662,0.0879999999999984);
#2201=TOROIDAL_SURFACE('',#103471,2.662,0.0879999999999984);
#2202=TOROIDAL_SURFACE('',#103474,2.662,0.0879999999999984);
#2203=TOROIDAL_SURFACE('',#103477,2.662,0.0879999999999984);
#2204=TOROIDAL_SURFACE('',#103480,2.662,0.0879999999999984);
#2205=TOROIDAL_SURFACE('',#103483,2.662,0.0879999999999984);
#2206=TOROIDAL_SURFACE('',#103486,2.662,0.0879999999999984);
#2207=TOROIDAL_SURFACE('',#103489,2.662,0.0879999999999984);
#2208=TOROIDAL_SURFACE('',#103492,2.662,0.0879999999999984);
#2209=TOROIDAL_SURFACE('',#103495,2.662,0.0879999999999984);
#2210=TOROIDAL_SURFACE('',#103498,2.662,0.0879999999999984);
#2211=TOROIDAL_SURFACE('',#103501,2.662,0.0879999999999984);
#2212=TOROIDAL_SURFACE('',#103504,2.662,0.0879999999999984);
#2213=TOROIDAL_SURFACE('',#103507,2.662,0.0879999999999984);
#2214=TOROIDAL_SURFACE('',#103510,2.662,0.0879999999999984);
#2215=TOROIDAL_SURFACE('',#103513,2.662,0.0879999999999984);
#2216=TOROIDAL_SURFACE('',#103516,2.662,0.0879999999999984);
#2217=TOROIDAL_SURFACE('',#103519,2.662,0.0879999999999984);
#2218=TOROIDAL_SURFACE('',#103522,2.662,0.0879999999999984);
#2219=TOROIDAL_SURFACE('',#103525,2.662,0.0879999999999984);
#2220=TOROIDAL_SURFACE('',#103547,2.662,0.0879999999999984);
#2221=(
BOUNDED_SURFACE()
B_SPLINE_SURFACE(2,2,((#138725,#138726,#138727,#138728,#138729),(#138730,
#138731,#138732,#138733,#138734),(#138735,#138736,#138737,#138738,#138739)),
 .UNSPECIFIED.,.F.,.F.,.F.)
B_SPLINE_SURFACE_WITH_KNOTS((3,3),(3,2,3),(-1.08356648062379E-15,1.5707963267949),
(-0.78539816339629,0.381098988689,1.54759614077429),.UNSPECIFIED.)
GEOMETRIC_REPRESENTATION_ITEM()
RATIONAL_B_SPLINE_SURFACE(((1.,0.834677941920344,1.,0.834677941920344,1.),
(0.707106781186542,0.590206432838701,0.707106781186542,0.590206432838701,
0.707106781186542),(1.,0.834677941920344,1.,0.834677941920344,1.)))
REPRESENTATION_ITEM('')
SURFACE()
);
#2222=(
BOUNDED_SURFACE()
B_SPLINE_SURFACE(2,2,((#138751,#138752,#138753,#138754,#138755),(#138756,
#138757,#138758,#138759,#138760),(#138761,#138762,#138763,#138764,#138765)),
 .UNSPECIFIED.,.F.,.F.,.F.)
B_SPLINE_SURFACE_WITH_KNOTS((3,3),(3,2,3),(-2.56377862909096E-16,1.5707963267949),
(0.206471222704293,1.13583112104019,2.06519101937609),.UNSPECIFIED.)
GEOMETRIC_REPRESENTATION_ITEM()
RATIONAL_B_SPLINE_SURFACE(((1.,0.89396503791678,1.,0.89396503791678,1.),
(0.707106781186548,0.632128740454645,0.707106781186548,0.632128740454645,
0.707106781186548),(1.,0.89396503791678,1.,0.89396503791678,1.)))
REPRESENTATION_ITEM('')
SURFACE()
);
#2223=(
BOUNDED_SURFACE()
B_SPLINE_SURFACE(2,2,((#138777,#138778,#138779,#138780,#138781),(#138782,
#138783,#138784,#138785,#138786),(#138787,#138788,#138789,#138790,#138791)),
 .UNSPECIFIED.,.F.,.F.,.F.)
B_SPLINE_SURFACE_WITH_KNOTS((3,3),(3,2,3),(-4.13193059734374E-15,1.5707963267949),
(-0.913769759667264,1.11022302462516E-16,0.913769759667264),
 .UNSPECIFIED.)
GEOMETRIC_REPRESENTATION_ITEM()
RATIONAL_B_SPLINE_SURFACE(((1.,0.89743109935827,1.,0.89743109935827,1.),
(0.707106781186553,0.634579616003937,0.707106781186553,0.634579616003937,
0.707106781186553),(1.,0.89743109935827,1.,0.89743109935827,1.)))
REPRESENTATION_ITEM('')
SURFACE()
);
#2224=(
BOUNDED_SURFACE()
B_SPLINE_SURFACE(2,2,((#138803,#138804,#138805),(#138806,#138807,#138808),
(#138809,#138810,#138811)),.UNSPECIFIED.,.F.,.F.,.F.)
B_SPLINE_SURFACE_WITH_KNOTS((3,3),(3,3),(-3.94009957434615E-16,1.5707963267949),
(-2.61567274150278,-1.57079632679301),.UNSPECIFIED.)
GEOMETRIC_REPRESENTATION_ITEM()
RATIONAL_B_SPLINE_SURFACE(((1.,0.866605104543064,1.),(0.707106781186545,
0.612782346033276,0.707106781186545),(1.,0.866605104543064,1.)))
REPRESENTATION_ITEM('')
SURFACE()
);
#2225=(
BOUNDED_SURFACE()
B_SPLINE_SURFACE(2,2,((#138823,#138824,#138825),(#138826,#138827,#138828),
(#138829,#138830,#138831)),.UNSPECIFIED.,.F.,.F.,.F.)
B_SPLINE_SURFACE_WITH_KNOTS((3,3),(3,3),(-1.43399263023479E-17,1.5707963267949),
(-1.57079632679302,-0.785398163396283),.UNSPECIFIED.)
GEOMETRIC_REPRESENTATION_ITEM()
RATIONAL_B_SPLINE_SURFACE(((1.,0.923879532511424,1.),(0.707106781186537,
0.653281482438276,0.707106781186537),(1.,0.923879532511424,1.)))
REPRESENTATION_ITEM('')
SURFACE()
);
#2226=(
BOUNDED_SURFACE()
B_SPLINE_SURFACE(2,2,((#138884,#138885,#138886),(#138887,#138888,#138889),
(#138890,#138891,#138892)),.UNSPECIFIED.,.F.,.F.,.F.)
B_SPLINE_SURFACE_WITH_KNOTS((3,3),(3,3),(-2.92306873924357E-15,1.5707963267949),
(-0.624753868765047,0.624753868765048),.UNSPECIFIED.)
GEOMETRIC_REPRESENTATION_ITEM()
RATIONAL_B_SPLINE_SURFACE(((1.,0.81110710565381,1.),(0.707106781186553,
0.573539334676407,0.707106781186553),(1.,0.81110710565381,1.)))
REPRESENTATION_ITEM('')
SURFACE()
);
#2227=(
BOUNDED_SURFACE()
B_SPLINE_SURFACE(2,2,((#138904,#138905,#138906,#138907,#138908),(#138909,
#138910,#138911,#138912,#138913),(#138914,#138915,#138916,#138917,#138918)),
 .UNSPECIFIED.,.F.,.F.,.F.)
B_SPLINE_SURFACE_WITH_KNOTS((3,3),(3,2,3),(-4.23634106201263E-16,1.5707963267949),
(-0.93774449040515,0.,0.93774449040515),.UNSPECIFIED.)
GEOMETRIC_REPRESENTATION_ITEM()
RATIONAL_B_SPLINE_SURFACE(((1.,0.892078465806108,1.,0.892078465806108,1.),
(0.707106781186543,0.630794732521986,0.707106781186543,0.630794732521986,
0.707106781186543),(1.,0.892078465806108,1.,0.892078465806108,1.)))
REPRESENTATION_ITEM('')
SURFACE()
);
#2228=(
BOUNDED_SURFACE()
B_SPLINE_SURFACE(2,2,((#138930,#138931,#138932),(#138933,#138934,#138935),
(#138936,#138937,#138938)),.UNSPECIFIED.,.F.,.F.,.F.)
B_SPLINE_SURFACE_WITH_KNOTS((3,3),(3,3),(-1.38777878078474E-15,1.5707963267949),
(-1.57079632680232,-0.78539816339745),.UNSPECIFIED.)
GEOMETRIC_REPRESENTATION_ITEM()
RATIONAL_B_SPLINE_SURFACE(((1.,0.923879532509866,1.),(0.707106781186554,
0.653281482437189,0.707106781186554),(1.,0.923879532509866,1.)))
REPRESENTATION_ITEM('')
SURFACE()
);
#2229=(
BOUNDED_SURFACE()
B_SPLINE_SURFACE(2,2,((#138962,#138963,#138964,#138965,#138966),(#138967,
#138968,#138969,#138970,#138971),(#138972,#138973,#138974,#138975,#138976)),
 .UNSPECIFIED.,.F.,.F.,.F.)
B_SPLINE_SURFACE_WITH_KNOTS((3,3),(3,2,3),(-3.22429839320269E-16,1.57079632679491),
(-1.57079632679301,-0.578762685695985,0.413270955399318),.UNSPECIFIED.)
GEOMETRIC_REPRESENTATION_ITEM()
RATIONAL_B_SPLINE_SURFACE(((1.,0.87948523306508,1.,0.87948523306508,1.),
(0.707106781186541,0.621889972253744,0.707106781186541,0.621889972253744,
0.707106781186541),(1.,0.87948523306508,1.,0.87948523306508,1.)))
REPRESENTATION_ITEM('')
SURFACE()
);
#2230=(
BOUNDED_SURFACE()
B_SPLINE_SURFACE(2,2,((#138988,#138989,#138990),(#138991,#138992,#138993),
(#138994,#138995,#138996)),.UNSPECIFIED.,.F.,.F.,.F.)
B_SPLINE_SURFACE_WITH_KNOTS((3,3),(3,3),(-4.80258936466661E-17,1.5707963267949),
(0.338566037798194,1.71521306218255),.UNSPECIFIED.)
GEOMETRIC_REPRESENTATION_ITEM()
RATIONAL_B_SPLINE_SURFACE(((1.,0.772312077486283,1.),(0.707106781186543,
0.546107107182817,0.707106781186543),(1.,0.772312077486283,1.)))
REPRESENTATION_ITEM('')
SURFACE()
);
#2231=(
BOUNDED_SURFACE()
B_SPLINE_SURFACE(2,2,((#139010,#139011,#139012),(#139013,#139014,#139015),
(#139016,#139017,#139018)),.UNSPECIFIED.,.F.,.F.,.F.)
B_SPLINE_SURFACE_WITH_KNOTS((3,3),(3,3),(-2.97223913180379E-15,1.5707963267949),
(0.821121559764502,2.02961305550291),.UNSPECIFIED.)
GEOMETRIC_REPRESENTATION_ITEM()
RATIONAL_B_SPLINE_SURFACE(((1.,0.82293085364046,1.),(0.707106781186547,
0.581899987056804,0.707106781186547),(1.,0.82293085364046,1.)))
REPRESENTATION_ITEM('')
SURFACE()
);
#2232=(
BOUNDED_SURFACE()
B_SPLINE_SURFACE(2,2,((#139080,#139081,#139082),(#139083,#139084,#139085),
(#139086,#139087,#139088)),.UNSPECIFIED.,.F.,.F.,.F.)
B_SPLINE_SURFACE_WITH_KNOTS((3,3),(3,3),(1.36100253158678E-19,1.57079632679491),
(0.135935745545801,1.57038769941725),.UNSPECIFIED.)
GEOMETRIC_REPRESENTATION_ITEM()
RATIONAL_B_SPLINE_SURFACE(((1.,0.753631982435871,1.),(0.707106781186546,
0.532898285299465,0.707106781186546),(1.,0.753631982435871,1.)))
REPRESENTATION_ITEM('')
SURFACE()
);
#2233=(
BOUNDED_SURFACE()
B_SPLINE_SURFACE(2,2,((#139100,#139101,#139102,#139103,#139104),(#139105,
#139106,#139107,#139108,#139109),(#139110,#139111,#139112,#139113,#139114)),
 .UNSPECIFIED.,.F.,.F.,.F.)
B_SPLINE_SURFACE_WITH_KNOTS((3,3),(3,2,3),(-3.39617731412459E-16,1.570796326795),
(1.57038769941725,2.35599017650376,3.14159265359003),.UNSPECIFIED.)
GEOMETRIC_REPRESENTATION_ITEM()
RATIONAL_B_SPLINE_SURFACE(((1.,0.92384043395866,1.,0.92384043395866,1.),
(0.707106781186508,0.653253835586454,0.707106781186508,0.653253835586454,
0.707106781186508),(1.,0.92384043395866,1.,0.92384043395866,1.)))
REPRESENTATION_ITEM('')
SURFACE()
);
#2234=(
BOUNDED_SURFACE()
B_SPLINE_SURFACE(2,2,((#139126,#139127,#139128,#139129,#139130),(#139131,
#139132,#139133,#139134,#139135),(#139136,#139137,#139138,#139139,#139140)),
 .UNSPECIFIED.,.F.,.F.,.F.)
B_SPLINE_SURFACE_WITH_KNOTS((3,3),(3,2,3),(-3.35182484084685E-16,1.5707963267949),
(-3.14159265359013,-2.16753947400706,-1.19348629442367),.UNSPECIFIED.)
GEOMETRIC_REPRESENTATION_ITEM()
RATIONAL_B_SPLINE_SURFACE(((1.,0.883728319944576,1.,0.883728319944576,1.),
(0.707106781186538,0.624890287759396,0.707106781186538,0.624890287759396,
0.707106781186538),(1.,0.883728319944576,1.,0.883728319944576,1.)))
REPRESENTATION_ITEM('')
SURFACE()
);
#2235=(
BOUNDED_SURFACE()
B_SPLINE_SURFACE(2,2,((#139152,#139153,#139154),(#139155,#139156,#139157),
(#139158,#139159,#139160)),.UNSPECIFIED.,.F.,.F.,.F.)
B_SPLINE_SURFACE_WITH_KNOTS((3,3),(3,3),(-2.40560064119055E-16,1.5707963267949),
(-2.36148733561698,-1.11197959808688),.UNSPECIFIED.)
GEOMETRIC_REPRESENTATION_ITEM()
RATIONAL_B_SPLINE_SURFACE(((1.,0.81110710565381,1.),(0.707106781186542,
0.573539334676398,0.707106781186542),(1.,0.81110710565381,1.)))
REPRESENTATION_ITEM('')
SURFACE()
);
#2236=(
BOUNDED_SURFACE()
B_SPLINE_SURFACE(2,2,((#139172,#139173,#139174),(#139175,#139176,#139177),
(#139178,#139179,#139180)),.UNSPECIFIED.,.F.,.F.,.F.)
B_SPLINE_SURFACE_WITH_KNOTS((3,3),(3,3),(-3.67871583187674E-16,1.5707963267949),
(-1.11197959808689,0.13308724141338),.UNSPECIFIED.)
GEOMETRIC_REPRESENTATION_ITEM()
RATIONAL_B_SPLINE_SURFACE(((1.,0.812403840463596,1.),(0.707106781186548,
0.574456264653803,0.707106781186548),(1.,0.812403840463596,1.)))
REPRESENTATION_ITEM('')
SURFACE()
);
#2237=(
BOUNDED_SURFACE()
B_SPLINE_SURFACE(2,2,((#139189,#139190,#139191),(#139192,#139193,#139194),
(#139195,#139196,#139197)),.UNSPECIFIED.,.F.,.F.,.F.)
B_SPLINE_SURFACE_WITH_KNOTS((3,3),(3,3),(-3.62332867476797E-16,1.5707963267949),
(-0.379047751698848,0.883627629924469),.UNSPECIFIED.)
GEOMETRIC_REPRESENTATION_ITEM()
RATIONAL_B_SPLINE_SURFACE(((1.,0.8072386920689,1.),(0.707106781186543,0.570803953198074,
0.707106781186543),(1.,0.8072386920689,1.)))
REPRESENTATION_ITEM('')
SURFACE()
);
#2238=(
BOUNDED_SURFACE()
B_SPLINE_SURFACE(2,2,((#139234,#139235,#139236),(#139237,#139238,#139239),
(#139240,#139241,#139242)),.UNSPECIFIED.,.F.,.F.,.F.)
B_SPLINE_SURFACE_WITH_KNOTS((3,3),(3,3),(-2.78610200478756E-15,1.5707963267949),
(-1.57120495417254,-0.136753000301094),.UNSPECIFIED.)
GEOMETRIC_REPRESENTATION_ITEM()
RATIONAL_B_SPLINE_SURFACE(((1.,0.753631982435872,1.),(0.707106781186546,
0.532898285299465,0.707106781186546),(1.,0.753631982435872,1.)))
REPRESENTATION_ITEM('')
SURFACE()
);
#2239=(
BOUNDED_SURFACE()
B_SPLINE_SURFACE(2,2,((#139254,#139255,#139256),(#139257,#139258,#139259),
(#139260,#139261,#139262)),.UNSPECIFIED.,.F.,.F.,.F.)
B_SPLINE_SURFACE_WITH_KNOTS((3,3),(3,3),(2.55184415889316E-16,1.5707963267949),
(-0.59217173005856,0.724821492103155),.UNSPECIFIED.)
GEOMETRIC_REPRESENTATION_ITEM()
RATIONAL_B_SPLINE_SURFACE(((1.,0.790913091470082,1.),(0.707106781186549,
0.559260010307712,0.707106781186549),(1.,0.790913091470082,1.)))
REPRESENTATION_ITEM('')
SURFACE()
);
#2240=(
BOUNDED_SURFACE()
B_SPLINE_SURFACE(2,2,((#139292,#139293,#139294,#139295,#139296),(#139297,
#139298,#139299,#139300,#139301),(#139302,#139303,#139304,#139305,#139306)),
 .UNSPECIFIED.,.F.,.F.,.F.)
B_SPLINE_SURFACE_WITH_KNOTS((3,3),(3,2,3),(-3.35271616303555E-16,1.57079632679502),
(1.26610367277728,2.20384816318377,3.14159265359003),.UNSPECIFIED.)
GEOMETRIC_REPRESENTATION_ITEM()
RATIONAL_B_SPLINE_SURFACE(((1.,0.892078465805831,1.,0.892078465805831,1.),
(0.707106781186508,0.630794732521759,0.707106781186508,0.630794732521759,
0.707106781186508),(1.,0.892078465805831,1.,0.892078465805831,1.)))
REPRESENTATION_ITEM('')
SURFACE()
);
#2241=(
BOUNDED_SURFACE()
B_SPLINE_SURFACE(2,2,((#139318,#139319,#139320),(#139321,#139322,#139323),
(#139324,#139325,#139326)),.UNSPECIFIED.,.F.,.F.,.F.)
B_SPLINE_SURFACE_WITH_KNOTS((3,3),(3,3),(-3.10863177296109E-15,1.5707963267949),
(-3.14159265359013,-1.57120495417254),.UNSPECIFIED.)
GEOMETRIC_REPRESENTATION_ITEM()
RATIONAL_B_SPLINE_SURFACE(((1.,0.707251238021515,1.),(0.707106781186534,
0.500102146407585,0.707106781186534),(1.,0.707251238021515,1.)))
REPRESENTATION_ITEM('')
SURFACE()
);
#2242=(
BOUNDED_SURFACE()
B_SPLINE_SURFACE(2,2,((#139373,#139374,#139375,#139376,#139377),(#139378,
#139379,#139380,#139381,#139382),(#139383,#139384,#139385,#139386,#139387)),
 .UNSPECIFIED.,.F.,.F.,.F.)
B_SPLINE_SURFACE_WITH_KNOTS((3,3),(3,2,3),(-3.79723113300163E-16,1.5707963267949),
(-2.21649908067713,-1.20577137048503,-0.195043660292926),.UNSPECIFIED.)
GEOMETRIC_REPRESENTATION_ITEM()
RATIONAL_B_SPLINE_SURFACE(((1.,0.874998380695011,1.,0.874998380695011,1.),
(0.707106781186542,0.618717288516686,0.707106781186542,0.618717288516686,
0.707106781186542),(1.,0.874998380695011,1.,0.874998380695011,1.)))
REPRESENTATION_ITEM('')
SURFACE()
);
#2243=(
BOUNDED_SURFACE()
B_SPLINE_SURFACE(2,2,((#139405,#139406,#139407,#139408,#139409),(#139410,
#139411,#139412,#139413,#139414),(#139415,#139416,#139417,#139418,#139419)),
 .UNSPECIFIED.,.F.,.F.,.F.)
B_SPLINE_SURFACE_WITH_KNOTS((3,3),(3,2,3),(-2.33769771306233E-15,1.5707963267949),
(-0.139437550001727,0.715679388398409,1.57079632679678),.UNSPECIFIED.)
GEOMETRIC_REPRESENTATION_ITEM()
RATIONAL_B_SPLINE_SURFACE(((1.,0.909980842363504,1.,0.909980842363504,1.),
(0.707106781186545,0.643453624385078,0.707106781186545,0.643453624385078,
0.707106781186545),(1.,0.909980842363504,1.,0.909980842363504,1.)))
REPRESENTATION_ITEM('')
SURFACE()
);
#2244=(
BOUNDED_SURFACE()
B_SPLINE_SURFACE(2,2,((#139443,#139444,#139445),(#139446,#139447,#139448),
(#139449,#139450,#139451)),.UNSPECIFIED.,.F.,.F.,.F.)
B_SPLINE_SURFACE_WITH_KNOTS((3,3),(3,3),(1.38777878078144E-17,1.5707963267949),
(0.785398163397444,1.5707963267949),.UNSPECIFIED.)
GEOMETRIC_REPRESENTATION_ITEM()
RATIONAL_B_SPLINE_SURFACE(((1.,0.923879532511286,1.),(0.707106781186537,
0.653281482438178,0.707106781186537),(1.,0.923879532511286,1.)))
REPRESENTATION_ITEM('')
SURFACE()
);
#2245=(
BOUNDED_SURFACE()
B_SPLINE_SURFACE(2,2,((#139463,#139464,#139465,#139466,#139467),(#139468,
#139469,#139470,#139471,#139472),(#139473,#139474,#139475,#139476,#139477)),
 .UNSPECIFIED.,.F.,.F.,.F.)
B_SPLINE_SURFACE_WITH_KNOTS((3,3),(3,2,3),(-2.76514922070703E-15,1.5707963267949),
(-1.03943004137575,0.,1.03943004137575),.UNSPECIFIED.)
GEOMETRIC_REPRESENTATION_ITEM()
RATIONAL_B_SPLINE_SURFACE(((1.,0.867960744996435,1.,0.867960744996435,1.),
(0.707106781186546,0.613740928590705,0.707106781186546,0.613740928590705,
0.707106781186546),(1.,0.867960744996435,1.,0.867960744996435,1.)))
REPRESENTATION_ITEM('')
SURFACE()
);
#2246=(
BOUNDED_SURFACE()
B_SPLINE_SURFACE(2,2,((#139489,#139490,#139491,#139492,#139493),(#139494,
#139495,#139496,#139497,#139498),(#139499,#139500,#139501,#139502,#139503)),
 .UNSPECIFIED.,.F.,.F.,.F.)
B_SPLINE_SURFACE_WITH_KNOTS((3,3),(3,2,3),(-4.15746516061636E-16,1.5707963267949),
(-1.31482537730283,-2.22044604925031E-16,1.31482537730283),
 .UNSPECIFIED.)
GEOMETRIC_REPRESENTATION_ITEM()
RATIONAL_B_SPLINE_SURFACE(((1.,0.791575909743,1.,0.791575909743,1.),(0.707106781186554,
0.559728693603191,0.707106781186554,0.559728693603191,0.707106781186554),
(1.,0.791575909743,1.,0.791575909743,1.)))
REPRESENTATION_ITEM('')
SURFACE()
);
#2247=(
BOUNDED_SURFACE()
B_SPLINE_SURFACE(2,2,((#139558,#139559,#139560,#139561,#139562),(#139563,
#139564,#139565,#139566,#139567),(#139568,#139569,#139570,#139571,#139572)),
 .UNSPECIFIED.,.F.,.F.,.F.)
B_SPLINE_SURFACE_WITH_KNOTS((3,3),(3,2,3),(-2.46171489419642E-16,1.5707963267949),
(-2.81803077212777,-1.86696066691245,-0.915890561697128),.UNSPECIFIED.)
GEOMETRIC_REPRESENTATION_ITEM()
RATIONAL_B_SPLINE_SURFACE(((1.,0.889047894212165,1.,0.889047894212165,1.),
(0.707106781186546,0.628651794797041,0.707106781186546,0.628651794797041,
0.707106781186546),(1.,0.889047894212165,1.,0.889047894212165,1.)))
REPRESENTATION_ITEM('')
SURFACE()
);
#2248=(
BOUNDED_SURFACE()
B_SPLINE_SURFACE(2,2,((#139584,#139585,#139586),(#139587,#139588,#139589),
(#139590,#139591,#139592)),.UNSPECIFIED.,.F.,.F.,.F.)
B_SPLINE_SURFACE_WITH_KNOTS((3,3),(3,3),(-4.20649046086306E-17,1.5707963267949),
(-1.66612611099672,-0.292748166464849),.UNSPECIFIED.)
GEOMETRIC_REPRESENTATION_ITEM()
RATIONAL_B_SPLINE_SURFACE(((1.,0.773349375865919,1.),(0.707106781186547,
0.546840587901175,0.707106781186547),(1.,0.773349375865919,1.)))
REPRESENTATION_ITEM('')
SURFACE()
);
#2249=(
BOUNDED_SURFACE()
B_SPLINE_SURFACE(2,2,((#139604,#139605,#139606,#139607,#139608),(#139609,
#139610,#139611,#139612,#139613),(#139614,#139615,#139616,#139617,#139618)),
 .UNSPECIFIED.,.F.,.F.,.F.)
B_SPLINE_SURFACE_WITH_KNOTS((3,3),(3,2,3),(-2.33310191252187E-15,1.5707963267949),
(-0.0602957815162571,0.75525027264115,1.57079632679678),.UNSPECIFIED.)
GEOMETRIC_REPRESENTATION_ITEM()
RATIONAL_B_SPLINE_SURFACE(((1.,0.918006240075228,1.,0.918006240075228,1.),
(0.707106781186546,0.649128437528759,0.707106781186546,0.649128437528759,
0.707106781186546),(1.,0.918006240075228,1.,0.918006240075228,1.)))
REPRESENTATION_ITEM('')
SURFACE()
);
#2250=(
BOUNDED_SURFACE()
B_SPLINE_SURFACE(2,2,((#139630,#139631,#139632),(#139633,#139634,#139635),
(#139636,#139637,#139638)),.UNSPECIFIED.,.F.,.F.,.F.)
B_SPLINE_SURFACE_WITH_KNOTS((3,3),(3,3),(-4.40596164996656E-16,1.5707963267949),
(1.57079632679678,3.04334701619792),.UNSPECIFIED.)
GEOMETRIC_REPRESENTATION_ITEM()
RATIONAL_B_SPLINE_SURFACE(((1.,0.740974920563651,1.),(0.707106781186542,
0.523948391019717,0.707106781186542),(1.,0.740974920563651,1.)))
REPRESENTATION_ITEM('')
SURFACE()
);
#2251=(
BOUNDED_SURFACE()
B_SPLINE_SURFACE(2,2,((#139673,#139674,#139675),(#139676,#139677,#139678),
(#139679,#139680,#139681)),.UNSPECIFIED.,.F.,.F.,.F.)
B_SPLINE_SURFACE_WITH_KNOTS((3,3),(3,3),(-3.19704967403774E-16,1.5707963267949),
(-0.873151522554683,-0.203094574416464),.UNSPECIFIED.)
GEOMETRIC_REPRESENTATION_ITEM()
RATIONAL_B_SPLINE_SURFACE(((1.,0.944400947853729,1.),(0.707106781186549,
0.667792314386376,0.707106781186549),(1.,0.944400947853729,1.)))
REPRESENTATION_ITEM('')
SURFACE()
);
#2252=(
BOUNDED_SURFACE()
B_SPLINE_SURFACE(2,2,((#139705,#139706,#139707),(#139708,#139709,#139710),
(#139711,#139712,#139713)),.UNSPECIFIED.,.F.,.F.,.F.)
B_SPLINE_SURFACE_WITH_KNOTS((3,3),(3,3),(-5.55723799297029E-15,1.5707963267949),
(-1.5533380622009,-0.0271380096021075),.UNSPECIFIED.)
GEOMETRIC_REPRESENTATION_ITEM()
RATIONAL_B_SPLINE_SURFACE(((1.,0.722696856670203,1.),(0.707106781186542,
0.511023848093699,0.707106781186542),(1.,0.722696856670203,1.)))
REPRESENTATION_ITEM('')
SURFACE()
);
#2253=(
BOUNDED_SURFACE()
B_SPLINE_SURFACE(2,2,((#139725,#139726,#139727,#139728,#139729),(#139730,
#139731,#139732,#139733,#139734),(#139735,#139736,#139737,#139738,#139739)),
 .UNSPECIFIED.,.F.,.F.,.F.)
B_SPLINE_SURFACE_WITH_KNOTS((3,3),(3,2,3),(1.04083408558608E-17,1.5707963267949),
(-0.027138009602113,0.771829158596392,1.5707963267949),.UNSPECIFIED.)
GEOMETRIC_REPRESENTATION_ITEM()
RATIONAL_B_SPLINE_SURFACE(((1.,0.921261973001208,1.,0.921261973001208,1.),
(0.707106781186546,0.651430588358451,0.707106781186546,0.651430588358451,
0.707106781186546),(1.,0.921261973001208,1.,0.921261973001208,1.)))
REPRESENTATION_ITEM('')
SURFACE()
);
#2254=(
BOUNDED_SURFACE()
B_SPLINE_SURFACE(2,2,((#139751,#139752,#139753),(#139754,#139755,#139756),
(#139757,#139758,#139759)),.UNSPECIFIED.,.F.,.F.,.F.)
B_SPLINE_SURFACE_WITH_KNOTS((3,3),(3,3),(-3.04212300157278E-16,1.5707963267949),
(1.5707963267949,2.35619449019235),.UNSPECIFIED.)
GEOMETRIC_REPRESENTATION_ITEM()
RATIONAL_B_SPLINE_SURFACE(((1.,0.923879532511286,1.),(0.707106781186548,
0.653281482438189,0.707106781186548),(1.,0.923879532511286,1.)))
REPRESENTATION_ITEM('')
SURFACE()
);
#2255=(
BOUNDED_SURFACE()
B_SPLINE_SURFACE(2,2,((#139771,#139772,#139773),(#139774,#139775,#139776),
(#139777,#139778,#139779)),.UNSPECIFIED.,.F.,.F.,.F.)
B_SPLINE_SURFACE_WITH_KNOTS((3,3),(3,3),(-4.44307714369147E-16,1.5707963267949),
(-0.411322268457341,0.411322268457339),.UNSPECIFIED.)
GEOMETRIC_REPRESENTATION_ITEM()
RATIONAL_B_SPLINE_SURFACE(((1.,0.9165929526849,1.),(0.707106781186543,0.648129092431289,
0.707106781186543),(1.,0.9165929526849,1.)))
REPRESENTATION_ITEM('')
SURFACE()
);
#2256=(
BOUNDED_SURFACE()
B_SPLINE_SURFACE(2,2,((#139791,#139792,#139793),(#139794,#139795,#139796),
(#139797,#139798,#139799)),.UNSPECIFIED.,.F.,.F.,.F.)
B_SPLINE_SURFACE_WITH_KNOTS((3,3),(3,3),(-3.09236869201824E-15,1.57079632679491),
(-0.743192726042517,0.743192726042517),.UNSPECIFIED.)
GEOMETRIC_REPRESENTATION_ITEM()
RATIONAL_B_SPLINE_SURFACE(((1.,0.736311982025157,1.),(0.707106781186541,
0.520651195558891,0.707106781186541),(1.,0.736311982025157,1.)))
REPRESENTATION_ITEM('')
SURFACE()
);
#2257=(
BOUNDED_SURFACE()
B_SPLINE_SURFACE(2,2,((#139811,#139812,#139813,#139814,#139815),(#139816,
#139817,#139818,#139819,#139820),(#139821,#139822,#139823,#139824,#139825)),
 .UNSPECIFIED.,.F.,.F.,.F.)
B_SPLINE_SURFACE_WITH_KNOTS((3,3),(3,2,3),(-3.88201214029742E-16,1.5707963267949),
(-2.21206449869477,-1.24517592036125,-0.278287342027729),.UNSPECIFIED.)
GEOMETRIC_REPRESENTATION_ITEM()
RATIONAL_B_SPLINE_SURFACE(((1.,0.885399163650358,1.,0.885399163650358,1.),
(0.70710678118654,0.626071752674059,0.70710678118654,0.626071752674059,
0.70710678118654),(1.,0.885399163650358,1.,0.885399163650358,1.)))
REPRESENTATION_ITEM('')
SURFACE()
);
#2258=(
BOUNDED_SURFACE()
B_SPLINE_SURFACE(2,2,((#139876,#139877,#139878,#139879,#139880),(#139881,
#139882,#139883,#139884,#139885),(#139886,#139887,#139888,#139889,#139890)),
 .UNSPECIFIED.,.F.,.F.,.F.)
B_SPLINE_SURFACE_WITH_KNOTS((3,3),(3,2,3),(-3.2009740160607E-15,1.5707963267949),
(-2.81763962832209,-1.47992684575006,-0.142214063178028),.UNSPECIFIED.)
GEOMETRIC_REPRESENTATION_ITEM()
RATIONAL_B_SPLINE_SURFACE(((1.,0.784531318155132,1.,0.784531318155132,1.),
(0.707106781186547,0.554747415120714,0.707106781186547,0.554747415120714,
0.707106781186547),(1.,0.784531318155132,1.,0.784531318155132,1.)))
REPRESENTATION_ITEM('')
SURFACE()
);
#2259=(
BOUNDED_SURFACE()
B_SPLINE_SURFACE(2,2,((#139908,#139909,#139910),(#139911,#139912,#139913),
(#139914,#139915,#139916)),.UNSPECIFIED.,.F.,.F.,.F.)
B_SPLINE_SURFACE_WITH_KNOTS((3,3),(3,3),(-9.43679832250494E-16,1.5707963267949),
(-4.54149544011533E-19,1.07849707504375),.UNSPECIFIED.)
GEOMETRIC_REPRESENTATION_ITEM()
RATIONAL_B_SPLINE_SURFACE(((1.,0.858094793061586,1.),(0.707106781186537,
0.606764647074706,0.707106781186537),(1.,0.858094793061586,1.)))
REPRESENTATION_ITEM('')
SURFACE()
);
#2260=(
BOUNDED_SURFACE()
B_SPLINE_SURFACE(2,2,((#139928,#139929,#139930,#139931,#139932),(#139933,
#139934,#139935,#139936,#139937),(#139938,#139939,#139940,#139941,#139942)),
 .UNSPECIFIED.,.F.,.F.,.F.)
B_SPLINE_SURFACE_WITH_KNOTS((3,3),(3,2,3),(-1.37198715633005E-15,1.5707963267949),
(-0.913769759667265,0.,0.913769759667266),.UNSPECIFIED.)
GEOMETRIC_REPRESENTATION_ITEM()
RATIONAL_B_SPLINE_SURFACE(((1.,0.89743109935827,1.,0.89743109935827,1.),
(0.707106781186543,0.634579616003927,0.707106781186543,0.634579616003927,
0.707106781186543),(1.,0.89743109935827,1.,0.89743109935827,1.)))
REPRESENTATION_ITEM('')
SURFACE()
);
#2261=(
BOUNDED_SURFACE()
B_SPLINE_SURFACE(2,2,((#139954,#139955,#139956,#139957,#139958),(#139959,
#139960,#139961,#139962,#139963),(#139964,#139965,#139966,#139967,#139968)),
 .UNSPECIFIED.,.F.,.F.,.F.)
B_SPLINE_SURFACE_WITH_KNOTS((3,3),(3,2,3),(-5.97388390143348E-15,1.5707963267949),
(-0.929359898335899,0.,0.929359898335898),.UNSPECIFIED.)
GEOMETRIC_REPRESENTATION_ITEM()
RATIONAL_B_SPLINE_SURFACE(((1.,0.89396503791678,1.,0.89396503791678,1.),
(0.707106781186544,0.632128740454641,0.707106781186544,0.632128740454641,
0.707106781186544),(1.,0.89396503791678,1.,0.89396503791678,1.)))
REPRESENTATION_ITEM('')
SURFACE()
);
#2262=(
BOUNDED_SURFACE()
B_SPLINE_SURFACE(2,2,((#140011,#140012,#140013),(#140014,#140015,#140016),
(#140017,#140018,#140019)),.UNSPECIFIED.,.F.,.F.,.F.)
B_SPLINE_SURFACE_WITH_KNOTS((3,3),(3,3),(-2.44248335016468E-15,1.5707963267949),
(-1.38777878078145E-17,1.5707963267949),.UNSPECIFIED.)
GEOMETRIC_REPRESENTATION_ITEM()
RATIONAL_B_SPLINE_SURFACE(((1.,0.707106781186547,1.),(0.707106781186554,
0.500000000000004,0.707106781186554),(1.,0.707106781186547,1.)))
REPRESENTATION_ITEM('')
SURFACE()
);
#2263=(
BOUNDED_SURFACE()
B_SPLINE_SURFACE(2,2,((#140031,#140032,#140033,#140034,#140035),(#140036,
#140037,#140038,#140039,#140040),(#140041,#140042,#140043,#140044,#140045)),
 .UNSPECIFIED.,.F.,.F.,.F.)
B_SPLINE_SURFACE_WITH_KNOTS((3,3),(3,2,3),(-2.87162691077515E-16,1.5707963267949),
(-1.06707356455707,0.,1.06707356455707),.UNSPECIFIED.)
GEOMETRIC_REPRESENTATION_ITEM()
RATIONAL_B_SPLINE_SURFACE(((1.,0.86101371653255,1.,0.86101371653255,1.),
(0.707106781186543,0.608828637654794,0.707106781186543,0.608828637654794,
0.707106781186543),(1.,0.86101371653255,1.,0.86101371653255,1.)))
REPRESENTATION_ITEM('')
SURFACE()
);
#2264=(
BOUNDED_SURFACE()
B_SPLINE_SURFACE(2,2,((#140057,#140058,#140059,#140060,#140061),(#140062,
#140063,#140064,#140065,#140066),(#140067,#140068,#140069,#140070,#140071)),
 .UNSPECIFIED.,.F.,.F.,.F.)
B_SPLINE_SURFACE_WITH_KNOTS((3,3),(3,2,3),(-3.12052122059803E-16,1.5707963267949),
(-0.937275919666155,0.,0.937275919666154),.UNSPECIFIED.)
GEOMETRIC_REPRESENTATION_ITEM()
RATIONAL_B_SPLINE_SURFACE(((1.,0.892184310318489,1.,0.892184310318489,1.),
(0.707106781186544,0.630869575894443,0.707106781186544,0.630869575894443,
0.707106781186544),(1.,0.892184310318489,1.,0.892184310318489,1.)))
REPRESENTATION_ITEM('')
SURFACE()
);
#2265=(
BOUNDED_SURFACE()
B_SPLINE_SURFACE(2,2,((#140083,#140084,#140085,#140086,#140087),(#140088,
#140089,#140090,#140091,#140092),(#140093,#140094,#140095,#140096,#140097)),
 .UNSPECIFIED.,.F.,.F.,.F.)
B_SPLINE_SURFACE_WITH_KNOTS((3,3),(3,2,3),(-2.44248335016467E-15,1.5707963267949),
(-1.94884750401252,-0.974423752006261,1.12987552192351E-32),
 .UNSPECIFIED.)
GEOMETRIC_REPRESENTATION_ITEM()
RATIONAL_B_SPLINE_SURFACE(((1.,0.883641590777673,1.,0.883641590777673,1.),
(0.707106781186542,0.624828960977356,0.707106781186542,0.624828960977356,
0.707106781186542),(1.,0.883641590777673,1.,0.883641590777673,1.)))
REPRESENTATION_ITEM('')
SURFACE()
);
#2266=(
BOUNDED_SURFACE()
B_SPLINE_SURFACE(2,2,((#141085,#141086,#141087,#141088,#141089),(#141090,
#141091,#141092,#141093,#141094),(#141095,#141096,#141097,#141098,#141099)),
 .UNSPECIFIED.,.F.,.F.,.F.)
B_SPLINE_SURFACE_WITH_KNOTS((3,3),(3,2,3),(-4.40321821990384E-16,1.5707963267949),
(-1.1664971520853,0.,1.16649715208529),.UNSPECIFIED.)
GEOMETRIC_REPRESENTATION_ITEM()
RATIONAL_B_SPLINE_SURFACE(((1.,0.834677941920342,1.,0.834677941920342,1.),
(0.707106781186555,0.590206432838712,0.707106781186555,0.590206432838712,
0.707106781186555),(1.,0.834677941920342,1.,0.834677941920342,1.)))
REPRESENTATION_ITEM('')
SURFACE()
);
#2267=(
BOUNDED_SURFACE()
B_SPLINE_SURFACE(2,2,((#141108,#141109,#141110),(#141111,#141112,#141113),
(#141114,#141115,#141116)),.UNSPECIFIED.,.F.,.F.,.F.)
B_SPLINE_SURFACE_WITH_KNOTS((3,3),(3,3),(-3.04212300157654E-16,1.5707963267949),
(-2.35619449019351,-1.57079632679678),.UNSPECIFIED.)
GEOMETRIC_REPRESENTATION_ITEM()
RATIONAL_B_SPLINE_SURFACE(((1.,0.923879532511424,1.),(0.707106781186556,
0.653281482438293,0.707106781186556),(1.,0.923879532511424,1.)))
REPRESENTATION_ITEM('')
SURFACE()
);
#2268=(
BOUNDED_SURFACE()
B_SPLINE_SURFACE(2,2,((#141128,#141129,#141130,#141131,#141132),(#141133,
#141134,#141135,#141136,#141137),(#141138,#141139,#141140,#141141,#141142)),
 .UNSPECIFIED.,.F.,.F.,.F.)
B_SPLINE_SURFACE_WITH_KNOTS((3,3),(3,2,3),(1.38777878069775E-17,1.5707963267949),
(-1.57079632679678,-0.570510447746883,0.429775431304741),.UNSPECIFIED.)
GEOMETRIC_REPRESENTATION_ITEM()
RATIONAL_B_SPLINE_SURFACE(((1.,0.877514024066407,1.,0.877514024066407,1.),
(0.70710678118655,0.620496117003654,0.70710678118655,0.620496117003654,
0.70710678118655),(1.,0.877514024066407,1.,0.877514024066407,1.)))
REPRESENTATION_ITEM('')
SURFACE()
);
#2269=(
BOUNDED_SURFACE()
B_SPLINE_SURFACE(2,2,((#141154,#141155,#141156,#141157,#141158),(#141159,
#141160,#141161,#141162,#141163),(#141164,#141165,#141166,#141167,#141168)),
 .UNSPECIFIED.,.F.,.F.,.F.)
B_SPLINE_SURFACE_WITH_KNOTS((3,3),(3,2,3),(-2.04068455613418E-16,1.5707963267949),
(0.317238733765724,1.23836023442364,2.15948173508156),.UNSPECIFIED.)
GEOMETRIC_REPRESENTATION_ITEM()
RATIONAL_B_SPLINE_SURFACE(((1.,0.895803412613763,1.,0.895803412613763,1.),
(0.707106781186556,0.63342866766925,0.707106781186556,0.63342866766925,
0.707106781186556),(1.,0.895803412613763,1.,0.895803412613763,1.)))
REPRESENTATION_ITEM('')
SURFACE()
);
#2270=(
BOUNDED_SURFACE()
B_SPLINE_SURFACE(2,2,((#141344,#141345,#141346,#141347,#141348),(#141349,
#141350,#141351,#141352,#141353),(#141354,#141355,#141356,#141357,#141358)),
 .UNSPECIFIED.,.F.,.F.,.F.)
B_SPLINE_SURFACE_WITH_KNOTS((3,3),(3,2,3),(-2.00928091613498E-16,1.5707963267949),
(0.492169594955417,1.33946582626418,2.18676205757294),.UNSPECIFIED.)
GEOMETRIC_REPRESENTATION_ITEM()
RATIONAL_B_SPLINE_SURFACE(((1.,0.911595310291363,1.,0.911595310291363,1.),
(0.707106781186556,0.644595225604885,0.707106781186556,0.644595225604885,
0.707106781186556),(1.,0.911595310291363,1.,0.911595310291363,1.)))
REPRESENTATION_ITEM('')
SURFACE()
);
#2271=(
BOUNDED_SURFACE()
B_SPLINE_SURFACE(2,2,((#141547,#141548,#141549),(#141550,#141551,#141552),
(#141553,#141554,#141555)),.UNSPECIFIED.,.F.,.F.,.F.)
B_SPLINE_SURFACE_WITH_KNOTS((3,3),(3,3),(-3.40404913931651E-16,1.5707963267949),
(1.57079632679491,3.14159265358979),.UNSPECIFIED.)
GEOMETRIC_REPRESENTATION_ITEM()
RATIONAL_B_SPLINE_SURFACE(((1.,0.707106781186554,1.),(0.707106781186545,
0.500000000000003,0.707106781186545),(1.,0.707106781186554,1.)))
REPRESENTATION_ITEM('')
SURFACE()
);
#2272=(
BOUNDED_SURFACE()
B_SPLINE_SURFACE(2,2,((#141662,#141663,#141664,#141665,#141666),(#141667,
#141668,#141669,#141670,#141671),(#141672,#141673,#141674,#141675,#141676)),
 .UNSPECIFIED.,.F.,.F.,.F.)
B_SPLINE_SURFACE_WITH_KNOTS((3,3),(3,2,3),(9.65265731632566E-18,1.5707963267949),
(-1.57306506263583,-0.715832961083556,0.141399140468717),.UNSPECIFIED.)
GEOMETRIC_REPRESENTATION_ITEM()
RATIONAL_B_SPLINE_SURFACE(((1.,0.909541807036257,1.,0.909541807036257,1.),
(0.707106781186556,0.643143179528011,0.707106781186556,0.643143179528011,
0.707106781186556),(1.,0.909541807036257,1.,0.909541807036257,1.)))
REPRESENTATION_ITEM('')
SURFACE()
);
#2273=(
BOUNDED_SURFACE()
B_SPLINE_SURFACE(2,2,((#141688,#141689,#141690),(#141691,#141692,#141693),
(#141694,#141695,#141696)),.UNSPECIFIED.,.F.,.F.,.F.)
B_SPLINE_SURFACE_WITH_KNOTS((3,3),(3,3),(-1.07735048008271E-14,1.57079632679491),
(0.133494798627492,1.57079632679493),.UNSPECIFIED.)
GEOMETRIC_REPRESENTATION_ITEM()
RATIONAL_B_SPLINE_SURFACE(((1.,0.752694710045445,1.),(0.707106781186546,
0.532235533636375,0.707106781186546),(1.,0.752694710045445,1.)))
REPRESENTATION_ITEM('')
SURFACE()
);
#2274=(
BOUNDED_SURFACE()
B_SPLINE_SURFACE(2,2,((#141811,#141812,#141813),(#141814,#141815,#141816),
(#141817,#141818,#141819)),.UNSPECIFIED.,.F.,.F.,.F.)
B_SPLINE_SURFACE_WITH_KNOTS((3,3),(3,3),(-7.12649760132934E-17,1.20783157419784),
(0.404259769435194,1.75111622640166),.UNSPECIFIED.)
GEOMETRIC_REPRESENTATION_ITEM()
RATIONAL_B_SPLINE_SURFACE(((1.,0.781688182176695,1.),(0.823118273259482,
0.643421826740624,0.823118273259482),(1.,0.781688182176695,1.)))
REPRESENTATION_ITEM('')
SURFACE()
);
#2275=(
BOUNDED_SURFACE()
B_SPLINE_SURFACE(2,2,((#141851,#141852,#141853),(#141854,#141855,#141856),
(#141857,#141858,#141859)),.UNSPECIFIED.,.F.,.F.,.F.)
B_SPLINE_SURFACE_WITH_KNOTS((3,3),(3,3),(-3.40404913931651E-16,1.5707963267949),
(1.5707963267949,3.14159265358979),.UNSPECIFIED.)
GEOMETRIC_REPRESENTATION_ITEM()
RATIONAL_B_SPLINE_SURFACE(((1.,0.707106781186548,1.),(0.707106781186553,
0.500000000000004,0.707106781186553),(1.,0.707106781186548,1.)))
REPRESENTATION_ITEM('')
SURFACE()
);
#2276=(
BOUNDED_SURFACE()
B_SPLINE_SURFACE(2,2,((#141867,#141868,#141869),(#141870,#141871,#141872),
(#141873,#141874,#141875)),.UNSPECIFIED.,.F.,.F.,.F.)
B_SPLINE_SURFACE_WITH_KNOTS((3,3),(3,3),(-3.38850230422209E-16,1.5707963267949),
(-3.14159265358979,-1.5707963267949),.UNSPECIFIED.)
GEOMETRIC_REPRESENTATION_ITEM()
RATIONAL_B_SPLINE_SURFACE(((1.,0.707106781186548,1.),(0.707106781186553,
0.500000000000004,0.707106781186553),(1.,0.707106781186548,1.)))
REPRESENTATION_ITEM('')
SURFACE()
);
#2277=(
BOUNDED_SURFACE()
B_SPLINE_SURFACE(2,2,((#141883,#141884,#141885),(#141886,#141887,#141888),
(#141889,#141890,#141891)),.UNSPECIFIED.,.F.,.F.,.F.)
B_SPLINE_SURFACE_WITH_KNOTS((3,3),(3,3),(1.04083408558608E-17,1.5707963267949),
(-1.5707963267949,-1.21122148599942),.UNSPECIFIED.)
GEOMETRIC_REPRESENTATION_ITEM()
RATIONAL_B_SPLINE_SURFACE(((1.,0.983881728593355,1.),(0.707106781186553,
0.69570944217391,0.707106781186553),(1.,0.983881728593355,1.)))
REPRESENTATION_ITEM('')
SURFACE()
);
#2278=(
BOUNDED_SURFACE()
B_SPLINE_SURFACE(2,2,((#142040,#142041,#142042,#142043,#142044),(#142045,
#142046,#142047,#142048,#142049),(#142050,#142051,#142052,#142053,#142054)),
 .UNSPECIFIED.,.F.,.F.,.F.)
B_SPLINE_SURFACE_WITH_KNOTS((3,3),(3,2,3),(-3.26817438467699E-16,1.5707963267949),
(-0.0112409050907196,1.17247679255081,2.35619449019235),.UNSPECIFIED.)
GEOMETRIC_REPRESENTATION_ITEM()
RATIONAL_B_SPLINE_SURFACE(((1.,0.829905053082259,1.,0.829905053082259,1.),
(0.70710678118655,0.586831490775449,0.70710678118655,0.586831490775449,
0.70710678118655),(1.,0.829905053082259,1.,0.829905053082259,1.)))
REPRESENTATION_ITEM('')
SURFACE()
);
#2279=(
BOUNDED_SURFACE()
B_SPLINE_SURFACE(2,2,((#142078,#142079,#142080,#142081,#142082),(#142083,
#142084,#142085,#142086,#142087),(#142088,#142089,#142090,#142091,#142092)),
 .UNSPECIFIED.,.F.,.F.,.F.)
B_SPLINE_SURFACE_WITH_KNOTS((3,3),(3,2,3),(-4.37390637964367E-16,1.5707963267949),
(-0.858171546837339,1.11022302462516E-16,0.85817154683734),
 .UNSPECIFIED.)
GEOMETRIC_REPRESENTATION_ITEM()
RATIONAL_B_SPLINE_SURFACE(((1.,0.909346484128941,1.,0.909346484128941,1.),
(0.70710678118655,0.643005065375722,0.70710678118655,0.643005065375722,
0.70710678118655),(1.,0.909346484128941,1.,0.909346484128941,1.)))
REPRESENTATION_ITEM('')
SURFACE()
);
#2280=(
BOUNDED_SURFACE()
B_SPLINE_SURFACE(2,2,((#142107,#142108,#142109,#142110,#142111),(#142112,
#142113,#142114,#142115,#142116),(#142117,#142118,#142119,#142120,#142121)),
 .UNSPECIFIED.,.F.,.F.,.F.)
B_SPLINE_SURFACE_WITH_KNOTS((3,3),(3,2,3),(-3.23084773091812E-16,1.5707963267949),
(-2.9253611858372,-1.9555154025201,-0.98566961920299),.UNSPECIFIED.)
GEOMETRIC_REPRESENTATION_ITEM()
RATIONAL_B_SPLINE_SURFACE(((1.,0.884710895031854,1.,0.884710895031854,1.),
(0.707106781186556,0.625585073266651,0.707106781186556,0.625585073266651,
0.707106781186556),(1.,0.884710895031854,1.,0.884710895031854,1.)))
REPRESENTATION_ITEM('')
SURFACE()
);
#2281=(
BOUNDED_SURFACE()
B_SPLINE_SURFACE(2,2,((#142179,#142180,#142181),(#142182,#142183,#142184),
(#142185,#142186,#142187)),.UNSPECIFIED.,.F.,.F.,.F.)
B_SPLINE_SURFACE_WITH_KNOTS((3,3),(3,3),(-3.40404913931651E-16,1.5707963267949),
(1.5707963267949,3.14159265358979),.UNSPECIFIED.)
GEOMETRIC_REPRESENTATION_ITEM()
RATIONAL_B_SPLINE_SURFACE(((1.,0.707106781186548,1.),(0.70710678118655,
0.500000000000002,0.70710678118655),(1.,0.707106781186548,1.)))
REPRESENTATION_ITEM('')
SURFACE()
);
#2282=(
BOUNDED_SURFACE()
B_SPLINE_SURFACE(2,2,((#142205,#142206,#142207,#142208,#142209),(#142210,
#142211,#142212,#142213,#142214),(#142215,#142216,#142217,#142218,#142219)),
 .UNSPECIFIED.,.F.,.F.,.F.)
B_SPLINE_SURFACE_WITH_KNOTS((3,3),(3,2,3),(-3.38916221447103E-16,1.5707963267949),
(-0.993480418549077,0.,0.993480418549077),.UNSPECIFIED.)
GEOMETRIC_REPRESENTATION_ITEM()
RATIONAL_B_SPLINE_SURFACE(((1.,0.879140723351448,1.,0.879140723351448,1.),
(0.707106781186546,0.621646367099054,0.707106781186546,0.621646367099054,
0.707106781186546),(1.,0.879140723351448,1.,0.879140723351448,1.)))
REPRESENTATION_ITEM('')
SURFACE()
);
#2283=(
BOUNDED_SURFACE()
B_SPLINE_SURFACE(2,2,((#142237,#142238,#142239,#142240,#142241),(#142242,
#142243,#142244,#142245,#142246),(#142247,#142248,#142249,#142250,#142251)),
 .UNSPECIFIED.,.F.,.F.,.F.)
B_SPLINE_SURFACE_WITH_KNOTS((3,3),(3,2,3),(-1.80387197830009E-16,1.5707963267949),
(-2.1740397470008,-1.03404943345041,0.105940880099987),.UNSPECIFIED.)
GEOMETRIC_REPRESENTATION_ITEM()
RATIONAL_B_SPLINE_SURFACE(((1.,0.841903588711717,1.,0.841903588711717,1.),
(0.707106781186553,0.59531573668335,0.707106781186553,0.59531573668335,
0.707106781186553),(1.,0.841903588711717,1.,0.841903588711717,1.)))
REPRESENTATION_ITEM('')
SURFACE()
);
#2284=(
BOUNDED_SURFACE()
B_SPLINE_SURFACE(2,2,((#142263,#142264,#142265),(#142266,#142267,#142268),
(#142269,#142270,#142271)),.UNSPECIFIED.,.F.,.F.,.F.)
B_SPLINE_SURFACE_WITH_KNOTS((3,3),(3,3),(3.04212300157275E-16,1.5707963267949),
(-0.0419015857269754,0.785398163397452),.UNSPECIFIED.)
GEOMETRIC_REPRESENTATION_ITEM()
RATIONAL_B_SPLINE_SURFACE(((1.,0.915659843255931,1.),(0.707106781186539,
0.647469284426472,0.707106781186539),(1.,0.915659843255931,1.)))
REPRESENTATION_ITEM('')
SURFACE()
);
#2285=(
BOUNDED_SURFACE()
B_SPLINE_SURFACE(2,2,((#142283,#142284,#142285),(#142286,#142287,#142288),
(#142289,#142290,#142291)),.UNSPECIFIED.,.F.,.F.,.F.)
B_SPLINE_SURFACE_WITH_KNOTS((3,3),(3,3),(-1.43399263032023E-17,1.5707963267949),
(0.78539816339745,1.5707963267949),.UNSPECIFIED.)
GEOMETRIC_REPRESENTATION_ITEM()
RATIONAL_B_SPLINE_SURFACE(((1.,0.923879532511287,1.),(0.707106781186552,
0.653281482438192,0.707106781186552),(1.,0.923879532511287,1.)))
REPRESENTATION_ITEM('')
SURFACE()
);
#2286=(
BOUNDED_SURFACE()
B_SPLINE_SURFACE(2,2,((#142330,#142331,#142332),(#142333,#142334,#142335),
(#142336,#142337,#142338)),.UNSPECIFIED.,.F.,.F.,.F.)
B_SPLINE_SURFACE_WITH_KNOTS((3,3),(3,3),(1.04083408558608E-17,1.5707963267949),
(-1.5707963267949,2.95409308984431E-16),.UNSPECIFIED.)
GEOMETRIC_REPRESENTATION_ITEM()
RATIONAL_B_SPLINE_SURFACE(((1.,0.707106781186547,1.),(0.707106781186553,
0.500000000000004,0.707106781186553),(1.,0.707106781186547,1.)))
REPRESENTATION_ITEM('')
SURFACE()
);
#2287=(
BOUNDED_SURFACE()
B_SPLINE_SURFACE(2,2,((#142350,#142351,#142352),(#142353,#142354,#142355),
(#142356,#142357,#142358)),.UNSPECIFIED.,.F.,.F.,.F.)
B_SPLINE_SURFACE_WITH_KNOTS((3,3),(3,3),(-1.0408340855861E-17,1.5707963267949),
(-2.76167977375508E-15,1.5707963267949),.UNSPECIFIED.)
GEOMETRIC_REPRESENTATION_ITEM()
RATIONAL_B_SPLINE_SURFACE(((1.,0.707106781186546,1.),(0.707106781186553,
0.500000000000003,0.707106781186553),(1.,0.707106781186546,1.)))
REPRESENTATION_ITEM('')
SURFACE()
);
#2288=(
BOUNDED_SURFACE()
B_SPLINE_SURFACE(2,2,((#142382,#142383,#142384,#142385,#142386),(#142387,
#142388,#142389,#142390,#142391),(#142392,#142393,#142394,#142395,#142396)),
 .UNSPECIFIED.,.F.,.F.,.F.)
B_SPLINE_SURFACE_WITH_KNOTS((3,3),(3,2,3),(-3.33132048898093E-16,1.5707963267949),
(-1.09723005759692,0.,1.09723005759692),.UNSPECIFIED.)
GEOMETRIC_REPRESENTATION_ITEM()
RATIONAL_B_SPLINE_SURFACE(((1.,0.85324761095477,1.,0.85324761095477,1.),
(0.707106781186558,0.603337171737348,0.707106781186558,0.603337171737348,
0.707106781186558),(1.,0.85324761095477,1.,0.85324761095477,1.)))
REPRESENTATION_ITEM('')
SURFACE()
);
#2289=(
BOUNDED_SURFACE()
B_SPLINE_SURFACE(2,2,((#142414,#142415,#142416),(#142417,#142418,#142419),
(#142420,#142421,#142422)),.UNSPECIFIED.,.F.,.F.,.F.)
B_SPLINE_SURFACE_WITH_KNOTS((3,3),(3,3),(-1.07755746139668E-16,1.5707963267949),
(-1.93037116759037,-1.5707963267949),.UNSPECIFIED.)
GEOMETRIC_REPRESENTATION_ITEM()
RATIONAL_B_SPLINE_SURFACE(((1.,0.983881728593356,1.),(0.707106781186554,
0.695709442173911,0.707106781186554),(1.,0.983881728593356,1.)))
REPRESENTATION_ITEM('')
SURFACE()
);
#2290=(
BOUNDED_SURFACE()
B_SPLINE_SURFACE(2,2,((#142555,#142556,#142557,#142558,#142559),(#142560,
#142561,#142562,#142563,#142564),(#142565,#142566,#142567,#142568,#142569)),
 .UNSPECIFIED.,.F.,.F.,.F.)
B_SPLINE_SURFACE_WITH_KNOTS((3,3),(3,2,3),(-3.36658337620736E-16,1.5707963267949),
(-0.939955765746386,-1.11022302462516E-16,0.939955765746385),
 .UNSPECIFIED.)
GEOMETRIC_REPRESENTATION_ITEM()
RATIONAL_B_SPLINE_SURFACE(((1.,0.891578304520668,1.,0.891578304520668,1.),
(0.707106781186548,0.63044106508537,0.707106781186548,0.63044106508537,
0.707106781186548),(1.,0.891578304520668,1.,0.891578304520668,1.)))
REPRESENTATION_ITEM('')
SURFACE()
);
#2291=(
BOUNDED_SURFACE()
B_SPLINE_SURFACE(2,2,((#142581,#142582,#142583,#142584,#142585),(#142586,
#142587,#142588,#142589,#142590),(#142591,#142592,#142593,#142594,#142595)),
 .UNSPECIFIED.,.F.,.F.,.F.)
B_SPLINE_SURFACE_WITH_KNOTS((3,3),(3,2,3),(-1.55728298388104E-16,1.5707963267949),
(-1.94810635916574,-0.974053179581248,1.68810521070105E-12),
 .UNSPECIFIED.)
GEOMETRIC_REPRESENTATION_ITEM()
RATIONAL_B_SPLINE_SURFACE(((1.,0.883728319944464,1.,0.883728319944464,1.),
(0.707106781186545,0.624890287759324,0.707106781186545,0.624890287759324,
0.707106781186545),(1.,0.883728319944464,1.,0.883728319944464,1.)))
REPRESENTATION_ITEM('')
SURFACE()
);
#2292=(
BOUNDED_SURFACE()
B_SPLINE_SURFACE(2,2,((#142747,#142748,#142749,#142750,#142751),(#142752,
#142753,#142754,#142755,#142756),(#142757,#142758,#142759,#142760,#142761)),
 .UNSPECIFIED.,.F.,.F.,.F.)
B_SPLINE_SURFACE_WITH_KNOTS((3,3),(3,2,3),(-2.28159225117958E-16,1.5707963267949),
(-2.35619449019236,-1.53123643686414,-0.706278383535922),.UNSPECIFIED.)
GEOMETRIC_REPRESENTATION_ITEM()
RATIONAL_B_SPLINE_SURFACE(((1.,0.916129842560975,1.,0.916129842560975,1.),
(0.707106781186559,0.64780162412224,0.707106781186559,0.64780162412224,
0.707106781186559),(1.,0.916129842560975,1.,0.916129842560975,1.)))
REPRESENTATION_ITEM('')
SURFACE()
);
#2293=(
BOUNDED_SURFACE()
B_SPLINE_SURFACE(2,2,((#142773,#142774,#142775,#142776,#142777),(#142778,
#142779,#142780,#142781,#142782),(#142783,#142784,#142785,#142786,#142787)),
 .UNSPECIFIED.,.F.,.F.,.F.)
B_SPLINE_SURFACE_WITH_KNOTS((3,3),(3,2,3),(1.54818837825044E-16,1.5707963267949),
(-0.663590463352779,0.191803543921911,1.0471975511966),.UNSPECIFIED.)
GEOMETRIC_REPRESENTATION_ITEM()
RATIONAL_B_SPLINE_SURFACE(((1.,0.909923390286242,1.,0.909923390286242,1.),
(0.70710678118655,0.643412999631658,0.70710678118655,0.643412999631658,
0.70710678118655),(1.,0.909923390286242,1.,0.909923390286242,1.)))
REPRESENTATION_ITEM('')
SURFACE()
);
#2294=(
BOUNDED_SURFACE()
B_SPLINE_SURFACE(2,2,((#142799,#142800,#142801),(#142802,#142803,#142804),
(#142805,#142806,#142807)),.UNSPECIFIED.,.F.,.F.,.F.)
B_SPLINE_SURFACE_WITH_KNOTS((3,3),(3,3),(-2.38131079176154E-16,1.5707963267949),
(1.0471975511966,2.32096244656348),.UNSPECIFIED.)
GEOMETRIC_REPRESENTATION_ITEM()
RATIONAL_B_SPLINE_SURFACE(((1.,0.803953645065829,1.),(0.707106781186556,
0.568481074185697,0.707106781186556),(1.,0.803953645065829,1.)))
REPRESENTATION_ITEM('')
SURFACE()
);
#2295=(
BOUNDED_SURFACE()
B_SPLINE_SURFACE(2,2,((#142821,#142822,#142823),(#142824,#142825,#142826),
(#142827,#142828,#142829)),.UNSPECIFIED.,.F.,.F.,.F.)
B_SPLINE_SURFACE_WITH_KNOTS((3,3),(3,3),(-1.75550993291529E-16,1.5707963267949),
(0.820630207026316,2.0943951023932),.UNSPECIFIED.)
GEOMETRIC_REPRESENTATION_ITEM()
RATIONAL_B_SPLINE_SURFACE(((1.,0.803953645065829,1.),(0.707106781186554,
0.568481074185696,0.707106781186554),(1.,0.803953645065829,1.)))
REPRESENTATION_ITEM('')
SURFACE()
);
#2296=(
BOUNDED_SURFACE()
B_SPLINE_SURFACE(2,2,((#142841,#142842,#142843,#142844,#142845),(#142846,
#142847,#142848,#142849,#142850),(#142851,#142852,#142853,#142854,#142855)),
 .UNSPECIFIED.,.F.,.F.,.F.)
B_SPLINE_SURFACE_WITH_KNOTS((3,3),(3,2,3),(-4.26771686360733E-16,1.5707963267949),
(-1.30899693899481,0.,1.30899693899481),.UNSPECIFIED.)
GEOMETRIC_REPRESENTATION_ITEM()
RATIONAL_B_SPLINE_SURFACE(((1.,0.793353340291521,1.,0.793353340291521,1.),
(0.707106781186554,0.560985526797139,0.707106781186554,0.560985526797139,
0.707106781186554),(1.,0.793353340291521,1.,0.793353340291521,1.)))
REPRESENTATION_ITEM('')
SURFACE()
);
#2297=(
BOUNDED_SURFACE()
B_SPLINE_SURFACE(2,2,((#142926,#142927,#142928),(#142929,#142930,#142931),
(#142932,#142933,#142934)),.UNSPECIFIED.,.F.,.F.,.F.)
B_SPLINE_SURFACE_WITH_KNOTS((3,3),(3,3),(-1.04083408558608E-17,1.5707963267949),
(1.24587053304372,1.5707963267949),.UNSPECIFIED.)
GEOMETRIC_REPRESENTATION_ITEM()
RATIONAL_B_SPLINE_SURFACE(((1.,0.986831905268789,1.),(0.707106781186553,
0.697795532106808,0.707106781186553),(1.,0.986831905268789,1.)))
REPRESENTATION_ITEM('')
SURFACE()
);
#2298=(
BOUNDED_SURFACE()
B_SPLINE_SURFACE(2,2,((#142946,#142947,#142948),(#142949,#142950,#142951),
(#142952,#142953,#142954)),.UNSPECIFIED.,.F.,.F.,.F.)
B_SPLINE_SURFACE_WITH_KNOTS((3,3),(3,3),(-3.40404913931651E-16,1.5707963267949),
(1.5707963267949,3.14159265358979),.UNSPECIFIED.)
GEOMETRIC_REPRESENTATION_ITEM()
RATIONAL_B_SPLINE_SURFACE(((1.,0.707106781186548,1.),(0.707106781186553,
0.500000000000004,0.707106781186553),(1.,0.707106781186548,1.)))
REPRESENTATION_ITEM('')
SURFACE()
);
#2299=(
BOUNDED_SURFACE()
B_SPLINE_SURFACE(2,2,((#142966,#142967,#142968),(#142969,#142970,#142971),
(#142972,#142973,#142974)),.UNSPECIFIED.,.F.,.F.,.F.)
B_SPLINE_SURFACE_WITH_KNOTS((3,3),(3,3),(-3.33074211398212E-16,1.5707963267949),
(-3.14159265358979,-1.86782775822291),.UNSPECIFIED.)
GEOMETRIC_REPRESENTATION_ITEM()
RATIONAL_B_SPLINE_SURFACE(((1.,0.80395364506583,1.),(0.707106781186555,
0.568481074185697,0.707106781186555),(1.,0.80395364506583,1.)))
REPRESENTATION_ITEM('')
SURFACE()
);
#2300=(
BOUNDED_SURFACE()
B_SPLINE_SURFACE(2,2,((#142983,#142984,#142985),(#142986,#142987,#142988),
(#142989,#142990,#142991)),.UNSPECIFIED.,.F.,.F.,.F.)
B_SPLINE_SURFACE_WITH_KNOTS((3,3),(3,3),(-3.32755772175793E-16,1.5707963267949),
(-0.636882447683443,0.636882447683442),.UNSPECIFIED.)
GEOMETRIC_REPRESENTATION_ITEM()
RATIONAL_B_SPLINE_SURFACE(((1.,0.803953645065828,1.),(0.707106781186554,
0.568481074185695,0.707106781186554),(1.,0.803953645065828,1.)))
REPRESENTATION_ITEM('')
SURFACE()
);
#2301=(
BOUNDED_SURFACE()
B_SPLINE_SURFACE(2,2,((#143003,#143004,#143005,#143006,#143007),(#143008,
#143009,#143010,#143011,#143012),(#143013,#143014,#143015,#143016,#143017)),
 .UNSPECIFIED.,.F.,.F.,.F.)
B_SPLINE_SURFACE_WITH_KNOTS((3,3),(3,2,3),(-1.64312426003188E-16,1.5707963267949),
(-2.0943951023932,-1.23900109511851,-0.383607087843824),.UNSPECIFIED.)
GEOMETRIC_REPRESENTATION_ITEM()
RATIONAL_B_SPLINE_SURFACE(((1.,0.909923390286242,1.,0.909923390286242,1.),
(0.707106781186545,0.643412999631653,0.707106781186545,0.643412999631653,
0.707106781186545),(1.,0.909923390286242,1.,0.909923390286242,1.)))
REPRESENTATION_ITEM('')
SURFACE()
);
#2302=(
BOUNDED_SURFACE()
B_SPLINE_SURFACE(2,2,((#143187,#143188,#143189,#143190,#143191),(#143192,
#143193,#143194,#143195,#143196),(#143197,#143198,#143199,#143200,#143201)),
 .UNSPECIFIED.,.F.,.F.,.F.)
B_SPLINE_SURFACE_WITH_KNOTS((3,3),(3,2,3),(-3.04971088561005E-16,1.5707963267949),
(-2.75798556574597,-1.90259155847128,-1.0471975511966),.UNSPECIFIED.)
GEOMETRIC_REPRESENTATION_ITEM()
RATIONAL_B_SPLINE_SURFACE(((1.,0.909923390286243,1.,0.909923390286243,1.),
(0.707106781186553,0.643412999631661,0.707106781186553,0.643412999631661,
0.707106781186553),(1.,0.909923390286243,1.,0.909923390286243,1.)))
REPRESENTATION_ITEM('')
SURFACE()
);
#2303=(
BOUNDED_SURFACE()
B_SPLINE_SURFACE(2,2,((#143213,#143214,#143215),(#143216,#143217,#143218),
(#143219,#143220,#143221)),.UNSPECIFIED.,.F.,.F.,.F.)
B_SPLINE_SURFACE_WITH_KNOTS((3,3),(3,3),(1.72872884261539E-16,1.5707963267949),
(-1.0471975511966,0.226567344170284),.UNSPECIFIED.)
GEOMETRIC_REPRESENTATION_ITEM()
RATIONAL_B_SPLINE_SURFACE(((1.,0.803953645065828,1.),(0.707106781186554,
0.568481074185695,0.707106781186554),(1.,0.803953645065828,1.)))
REPRESENTATION_ITEM('')
SURFACE()
);
#2304=(
BOUNDED_SURFACE()
B_SPLINE_SURFACE(2,2,((#143230,#143231,#143232),(#143233,#143234,#143235),
(#143236,#143237,#143238)),.UNSPECIFIED.,.F.,.F.,.F.)
B_SPLINE_SURFACE_WITH_KNOTS((3,3),(3,3),(1.0220704756512E-16,1.5707963267949),
(-1.27376489536688,1.38777878078145E-17),.UNSPECIFIED.)
GEOMETRIC_REPRESENTATION_ITEM()
RATIONAL_B_SPLINE_SURFACE(((1.,0.80395364506583,1.),(0.707106781186553,
0.568481074185696,0.707106781186553),(1.,0.80395364506583,1.)))
REPRESENTATION_ITEM('')
SURFACE()
);
#2305=(
BOUNDED_SURFACE()
B_SPLINE_SURFACE(2,2,((#143250,#143251,#143252),(#143253,#143254,#143255),
(#143256,#143257,#143258)),.UNSPECIFIED.,.F.,.F.,.F.)
B_SPLINE_SURFACE_WITH_KNOTS((3,3),(3,3),(-1.04083408558608E-17,1.5707963267949),
(-6.80011602582909E-16,1.5707963267949),.UNSPECIFIED.)
GEOMETRIC_REPRESENTATION_ITEM()
RATIONAL_B_SPLINE_SURFACE(((1.,0.707106781186547,1.),(0.707106781186555,
0.500000000000005,0.707106781186555),(1.,0.707106781186547,1.)))
REPRESENTATION_ITEM('')
SURFACE()
);
#2306=(
BOUNDED_SURFACE()
B_SPLINE_SURFACE(2,2,((#143270,#143271,#143272),(#143273,#143274,#143275),
(#143276,#143277,#143278)),.UNSPECIFIED.,.F.,.F.,.F.)
B_SPLINE_SURFACE_WITH_KNOTS((3,3),(3,3),(-1.16510060523539E-16,1.5707963267949),
(1.5707963267949,1.89572212054608),.UNSPECIFIED.)
GEOMETRIC_REPRESENTATION_ITEM()
RATIONAL_B_SPLINE_SURFACE(((1.,0.986831905268789,1.),(0.707106781186554,
0.697795532106808,0.707106781186554),(1.,0.986831905268789,1.)))
REPRESENTATION_ITEM('')
SURFACE()
);
#2307=(
BOUNDED_SURFACE()
B_SPLINE_SURFACE(1,2,((#362051,#362052,#362053,#362054,#362055,#362056,
#362057,#362058,#362059,#362060,#362061,#362062,#362063,#362064,#362065,
#362066,#362067,#362068,#362069,#362070,#362071,#362072,#362073,#362074,
#362075,#362076,#362077,#362078,#362079,#362080,#362081,#362082,#362083,
#362084,#362085,#362086,#362087,#362088,#362089,#362090,#362091,#362092,
#362093,#362094,#362095,#362096,#362097,#362098,#362099,#362100,#362101,
#362102,#362103,#362104,#362105,#362106,#362107,#362108,#362109,#362110,
#362111,#362112,#362113,#362114,#362115,#362116,#362117,#362118,#362119,
#362120,#362121,#362122,#362123,#362124,#362125,#362126,#362127,#362128,
#362129,#362130,#362131,#362132,#362133,#362134,#362135,#362136,#362137,
#362138,#362139,#362140,#362141,#362142,#362143,#362144,#362145,#362146,
#362147,#362148,#362149,#362150,#362151,#362152,#362153,#362154,#362155,
#362156,#362157,#362158,#362159,#362160,#362161,#362162,#362163,#362164,
#362165,#362166,#362167,#362168,#362169,#362170,#362171,#362172,#362173,
#362174,#362175,#362176,#362177,#362178,#362179,#362180,#362181,#362182,
#362183,#362184,#362185,#362186,#362187,#362188,#362189,#362190,#362191,
#362192,#362193,#362194,#362195,#362196,#362197,#362198,#362199,#362200,
#362201,#362202,#362203,#362204,#362205,#362206,#362207,#362208,#362209,
#362210,#362211,#362212,#362213,#362214,#362215,#362216,#362217,#362218,
#362219,#362220,#362221,#362222,#362223,#362224,#362225,#362226,#362227,
#362228,#362229,#362230,#362231,#362232,#362233,#362234,#362235,#362236,
#362237,#362238,#362239,#362240,#362241,#362242,#362243,#362244,#362245,
#362246,#362247,#362248,#362249,#362250,#362251,#362252,#362253,#362254,
#362255,#362256,#362257,#362258,#362259,#362260,#362261,#362262,#362263,
#362264,#362265,#362266,#362267,#362268,#362269,#362270,#362271,#362272,
#362273,#362274,#362275,#362276,#362277,#362278,#362279,#362280,#362281,
#362282,#362283,#362284,#362285,#362286,#362287,#362288,#362289,#362290,
#362291,#362292,#362293,#362294,#362295,#362296,#362297,#362298,#362299,
#362300,#362301,#362302,#362303,#362304,#362305,#362306,#362307,#362308,
#362309,#362310,#362311,#362312,#362313,#362314,#362315,#362316,#362317,
#362318,#362319,#362320,#362321,#362322,#362323,#362324,#362325,#362326,
#362327,#362328,#362329,#362330,#362331,#362332,#362333,#362334,#362335,
#362336,#362337,#362338,#362339,#362340,#362341,#362342,#362343,#362344,
#362345,#362346,#362347,#362348,#362349,#362350,#362351,#362352,#362353,
#362354,#362355,#362356,#362357,#362358,#362359,#362360,#362361,#362362,
#362363,#362364,#362365,#362366,#362367,#362368,#362369,#362370,#362371,
#362372,#362373,#362374,#362375,#362376,#362377,#362378,#362379,#362380,
#362381,#362382,#362383,#362384,#362385,#362386,#362387,#362388,#362389,
#362390,#362391,#362392,#362393,#362394,#362395,#362396,#362397,#362398,
#362399,#362400,#362401,#362402,#362403,#362404,#362405,#362406,#362407,
#362408,#362409,#362410,#362411,#362412,#362413,#362414,#362415,#362416,
#362417,#362418,#362419,#362420,#362421,#362422,#362423,#362424,#362425,
#362426,#362427,#362428,#362429,#362430,#362431,#362432,#362433,#362434,
#362435,#362436,#362437,#362438,#362439,#362440,#362441,#362442,#362443,
#362444,#362445,#362446,#362447),(#362448,#362449,#362450,#362451,#362452,
#362453,#362454,#362455,#362456,#362457,#362458,#362459,#362460,#362461,
#362462,#362463,#362464,#362465,#362466,#362467,#362468,#362469,#362470,
#362471,#362472,#362473,#362474,#362475,#362476,#362477,#362478,#362479,
#362480,#362481,#362482,#362483,#362484,#362485,#362486,#362487,#362488,
#362489,#362490,#362491,#362492,#362493,#362494,#362495,#362496,#362497,
#362498,#362499,#362500,#362501,#362502,#362503,#362504,#362505,#362506,
#362507,#362508,#362509,#362510,#362511,#362512,#362513,#362514,#362515,
#362516,#362517,#362518,#362519,#362520,#362521,#362522,#362523,#362524,
#362525,#362526,#362527,#362528,#362529,#362530,#362531,#362532,#362533,
#362534,#362535,#362536,#362537,#362538,#362539,#362540,#362541,#362542,
#362543,#362544,#362545,#362546,#362547,#362548,#362549,#362550,#362551,
#362552,#362553,#362554,#362555,#362556,#362557,#362558,#362559,#362560,
#362561,#362562,#362563,#362564,#362565,#362566,#362567,#362568,#362569,
#362570,#362571,#362572,#362573,#362574,#362575,#362576,#362577,#362578,
#362579,#362580,#362581,#362582,#362583,#362584,#362585,#362586,#362587,
#362588,#362589,#362590,#362591,#362592,#362593,#362594,#362595,#362596,
#362597,#362598,#362599,#362600,#362601,#362602,#362603,#362604,#362605,
#362606,#362607,#362608,#362609,#362610,#362611,#362612,#362613,#362614,
#362615,#362616,#362617,#362618,#362619,#362620,#362621,#362622,#362623,
#362624,#362625,#362626,#362627,#362628,#362629,#362630,#362631,#362632,
#362633,#362634,#362635,#362636,#362637,#362638,#362639,#362640,#362641,
#362642,#362643,#362644,#362645,#362646,#362647,#362648,#362649,#362650,
#362651,#362652,#362653,#362654,#362655,#362656,#362657,#362658,#362659,
#362660,#362661,#362662,#362663,#362664,#362665,#362666,#362667,#362668,
#362669,#362670,#362671,#362672,#362673,#362674,#362675,#362676,#362677,
#362678,#362679,#362680,#362681,#362682,#362683,#362684,#362685,#362686,
#362687,#362688,#362689,#362690,#362691,#362692,#362693,#362694,#362695,
#362696,#362697,#362698,#362699,#362700,#362701,#362702,#362703,#362704,
#362705,#362706,#362707,#362708,#362709,#362710,#362711,#362712,#362713,
#362714,#362715,#362716,#362717,#362718,#362719,#362720,#362721,#362722,
#362723,#362724,#362725,#362726,#362727,#362728,#362729,#362730,#362731,
#362732,#362733,#362734,#362735,#362736,#362737,#362738,#362739,#362740,
#362741,#362742,#362743,#362744,#362745,#362746,#362747,#362748,#362749,
#362750,#362751,#362752,#362753,#362754,#362755,#362756,#362757,#362758,
#362759,#362760,#362761,#362762,#362763,#362764,#362765,#362766,#362767,
#362768,#362769,#362770,#362771,#362772,#362773,#362774,#362775,#362776,
#362777,#362778,#362779,#362780,#362781,#362782,#362783,#362784,#362785,
#362786,#362787,#362788,#362789,#362790,#362791,#362792,#362793,#362794,
#362795,#362796,#362797,#362798,#362799,#362800,#362801,#362802,#362803,
#362804,#362805,#362806,#362807,#362808,#362809,#362810,#362811,#362812,
#362813,#362814,#362815,#362816,#362817,#362818,#362819,#362820,#362821,
#362822,#362823,#362824,#362825,#362826,#362827,#362828,#362829,#362830,
#362831,#362832,#362833,#362834,#362835,#362836,#362837,#362838,#362839,
#362840,#362841,#362842,#362843,#362844)),.UNSPECIFIED.,.F.,.F.,.F.)
B_SPLINE_SURFACE_WITH_KNOTS((2,2),(3,2,2,2,2,2,2,2,2,2,2,2,2,2,2,2,2,2,
2,2,2,2,2,2,2,2,2,2,2,2,2,2,2,2,2,2,2,2,2,2,2,2,2,2,2,2,2,2,2,2,2,2,2,2,
2,2,2,2,2,2,2,2,2,2,2,2,2,2,2,2,2,2,2,2,2,2,2,2,2,2,2,2,2,2,2,2,2,2,2,2,
2,2,2,2,2,2,2,2,2,2,2,2,2,2,2,2,2,2,2,2,2,2,2,2,2,2,2,2,2,2,2,2,2,2,2,2,
2,2,2,2,2,2,2,2,2,2,2,2,2,2,2,2,2,2,2,2,2,2,2,2,2,2,2,2,2,2,2,2,2,2,2,2,
2,2,2,2,2,2,2,2,2,2,2,2,2,2,2,2,2,2,2,2,2,2,2,2,2,2,2,2,2,2,2,2,2,2,2,2,
3),(0.,1.),(0.,0.00505050505050505,0.0101010101010101,0.0151515151515152,
0.0202020202020202,0.0252525252525253,0.0303030303030303,0.0353535353535354,
0.0404040404040404,0.0454545454545455,0.0505050505050505,0.0555555555555556,
0.0606060606060606,0.0656565656565657,0.0707070707070707,0.0757575757575758,
0.0808080808080808,0.0858585858585859,0.0909090909090909,0.095959595959596,
0.101010101010101,0.106060606060606,0.111111111111111,0.116161616161616,
0.121212121212121,0.126262626262626,0.131313131313131,0.136363636363636,
0.141414141414141,0.146464646464646,0.151515151515152,0.156565656565657,
0.161616161616162,0.166666666666667,0.171717171717172,0.176767676767677,
0.181818181818182,0.186868686868687,0.191919191919192,0.196969696969697,
0.202020202020202,0.207070707070707,0.212121212121212,0.217171717171717,
0.222222222222222,0.227272727272727,0.232323232323232,0.237373737373737,
0.242424242424242,0.247474747474747,0.252525252525253,0.257575757575758,
0.262626262626263,0.267676767676768,0.272727272727273,0.277777777777778,
0.282828282828283,0.287878787878788,0.292929292929293,0.297979797979798,
0.303030303030303,0.308080808080808,0.313131313131313,0.318181818181818,
0.323232323232323,0.328282828282828,0.333333333333333,0.338383838383838,
0.343434343434343,0.348484848484849,0.353535353535354,0.358585858585859,
0.363636363636364,0.368686868686869,0.373737373737374,0.378787878787879,
0.383838383838384,0.388888888888889,0.393939393939394,0.398989898989899,
0.404040404040404,0.409090909090909,0.414141414141414,0.419191919191919,
0.424242424242424,0.429292929292929,0.434343434343434,0.439393939393939,
0.444444444444444,0.44949494949495,0.454545454545455,0.45959595959596,0.464646464646465,
0.46969696969697,0.474747474747475,0.47979797979798,0.484848484848485,0.48989898989899,
0.494949494949495,0.5,0.505050505050505,0.51010101010101,0.515151515151515,
0.52020202020202,0.525252525252525,0.53030303030303,0.535353535353535,0.54040404040404,
0.545454545454545,0.55050505050505,0.555555555555556,0.560606060606061,
0.565656565656566,0.570707070707071,0.575757575757576,0.580808080808081,
0.585858585858586,0.590909090909091,0.595959595959596,0.601010101010101,
0.606060606060606,0.611111111111111,0.616161616161616,0.621212121212121,
0.626262626262626,0.631313131313131,0.636363636363636,0.641414141414141,
0.646464646464647,0.651515151515151,0.656565656565657,0.661616161616162,
0.666666666666667,0.671717171717172,0.676767676767677,0.681818181818182,
0.686868686868687,0.691919191919192,0.696969696969697,0.702020202020202,
0.707070707070707,0.712121212121212,0.717171717171717,0.722222222222222,
0.727272727272727,0.732323232323232,0.737373737373737,0.742424242424242,
0.747474747474748,0.752525252525252,0.757575757575758,0.762626262626263,
0.767676767676768,0.772727272727273,0.777777777777778,0.782828282828283,
0.787878787878788,0.792929292929293,0.797979797979798,0.803030303030303,
0.808080808080808,0.813131313131313,0.818181818181818,0.823232323232323,
0.828282828282828,0.833333333333333,0.838383838383838,0.843434343434343,
0.848484848484849,0.853535353535353,0.858585858585859,0.863636363636364,
0.868686868686869,0.873737373737374,0.878787878787879,0.883838383838384,
0.888888888888889,0.893939393939394,0.898989898989899,0.904040404040404,
0.909090909090909,0.914141414141414,0.919191919191919,0.924242424242424,
0.929292929292929,0.934343434343434,0.939393939393939,0.944444444444444,
0.94949494949495,0.954545454545455,0.95959595959596,0.964646464646465,0.96969696969697,
0.974747474747475,0.97979797979798,0.984848484848485,0.98989898989899,0.994949494949495,
1.),.UNSPECIFIED.)
GEOMETRIC_REPRESENTATION_ITEM()
RATIONAL_B_SPLINE_SURFACE(((1.,0.866025403784439,1.,0.866025403784439,1.,
0.866025403784439,1.,0.866025403784439,1.,0.866025403784439,1.,0.866025403784439,
1.,0.866025403784439,1.,0.866025403784439,1.,0.866025403784439,1.,0.866025403784439,
1.,0.866025403784439,1.,0.866025403784439,1.,0.866025403784439,1.,0.866025403784439,
1.,0.866025403784439,1.,0.866025403784439,1.,0.866025403784439,1.,0.866025403784439,
1.,0.866025403784439,1.,0.866025403784439,1.,0.866025403784439,1.,0.866025403784439,
1.,0.866025403784439,1.,0.866025403784439,1.,0.866025403784439,1.,0.866025403784439,
1.,0.866025403784439,1.,0.866025403784439,1.,0.866025403784439,1.,0.866025403784439,
1.,0.866025403784439,1.,0.866025403784439,1.,0.866025403784439,1.,0.866025403784439,
1.,0.866025403784439,1.,0.866025403784439,1.,0.866025403784439,1.,0.866025403784439,
1.,0.866025403784439,1.,0.866025403784439,1.,0.866025403784439,1.,0.866025403784439,
1.,0.866025403784439,1.,0.866025403784439,1.,0.866025403784439,1.,0.866025403784439,
1.,0.866025403784439,1.,0.866025403784439,1.,0.866025403784439,1.,0.866025403784439,
1.,0.866025403784439,1.,0.866025403784439,1.,0.866025403784439,1.,0.866025403784439,
1.,0.866025403784439,1.,0.866025403784439,1.,0.866025403784439,1.,0.866025403784439,
1.,0.866025403784439,1.,0.866025403784439,1.,0.866025403784439,1.,0.866025403784439,
1.,0.866025403784439,1.,0.866025403784439,1.,0.866025403784439,1.,0.866025403784439,
1.,0.866025403784439,1.,0.866025403784439,1.,0.866025403784439,1.,0.866025403784439,
1.,0.866025403784439,1.,0.866025403784439,1.,0.866025403784439,1.,0.866025403784439,
1.,0.866025403784439,1.,0.866025403784439,1.,0.866025403784439,1.,0.866025403784439,
1.,0.866025403784439,1.,0.866025403784439,1.,0.866025403784439,1.,0.866025403784439,
1.,0.866025403784439,1.,0.866025403784439,1.,0.866025403784439,1.,0.866025403784439,
1.,0.866025403784439,1.,0.866025403784439,1.,0.866025403784439,1.,0.866025403784439,
1.,0.866025403784439,1.,0.866025403784439,1.,0.866025403784439,1.,0.866025403784439,
1.,0.866025403784439,1.,0.866025403784439,1.,0.866025403784439,1.,0.866025403784439,
1.,0.866025403784439,1.,0.866025403784439,1.,0.866025403784439,1.,0.866025403784439,
1.,0.866025403784439,1.,0.866025403784439,1.,0.866025403784439,1.,0.866025403784439,
1.,0.866025403784439,1.,0.866025403784439,1.,0.866025403784439,1.,0.866025403784439,
1.,0.866025403784439,1.,0.866025403784439,1.,0.866025403784439,1.,0.866025403784439,
1.,0.866025403784439,1.,0.866025403784439,1.,0.866025403784439,1.,0.866025403784439,
1.,0.866025403784439,1.,0.866025403784439,1.,0.866025403784439,1.,0.866025403784439,
1.,0.866025403784439,1.,0.866025403784439,1.,0.866025403784439,1.,0.866025403784439,
1.,0.866025403784439,1.,0.866025403784439,1.,0.866025403784439,1.,0.866025403784439,
1.,0.866025403784439,1.,0.866025403784439,1.,0.866025403784439,1.,0.866025403784439,
1.,0.866025403784439,1.,0.866025403784439,1.,0.866025403784439,1.,0.866025403784439,
1.,0.866025403784439,1.,0.866025403784439,1.,0.866025403784439,1.,0.866025403784439,
1.,0.866025403784439,1.,0.866025403784439,1.,0.866025403784439,1.,0.866025403784439,
1.,0.866025403784439,1.,0.866025403784439,1.,0.866025403784439,1.,0.866025403784439,
1.,0.866025403784439,1.,0.866025403784439,1.,0.866025403784439,1.,0.866025403784439,
1.,0.866025403784439,1.,0.866025403784439,1.,0.866025403784439,1.,0.866025403784439,
1.,0.866025403784439,1.,0.866025403784439,1.,0.866025403784439,1.,0.866025403784439,
1.,0.866025403784439,1.,0.866025403784439,1.,0.866025403784439,1.,0.866025403784439,
1.,0.866025403784439,1.,0.866025403784439,1.,0.866025403784439,1.,0.866025403784439,
1.,0.866025403784439,1.,0.866025403784439,1.,0.866025403784439,1.,0.866025403784439,
1.,0.866025403784439,1.,0.866025403784439,1.,0.866025403784439,1.,0.866025403784439,
1.,0.866025403784439,1.,0.866025403784439,1.,0.866025403784439,1.,0.866025403784439,
1.,0.866025403784439,1.,0.866025403784439,1.,0.866025403784439,1.,0.866025403784439,
1.,0.866025403784439,1.,0.866025403784439,1.,0.866025403784439,1.,0.866025403784439,
1.,0.866025403784439,1.,0.866025403784439,1.,0.866025403784439,1.,0.866025403784439,
1.,0.866025403784439,1.,0.866025403784439,1.,0.866025403784439,1.,0.866025403784439,
1.),(1.,0.866025403784439,1.,0.866025403784439,1.,0.866025403784439,1.,
0.866025403784439,1.,0.866025403784439,1.,0.866025403784439,1.,0.866025403784439,
1.,0.866025403784439,1.,0.866025403784439,1.,0.866025403784439,1.,0.866025403784439,
1.,0.866025403784439,1.,0.866025403784439,1.,0.866025403784439,1.,0.866025403784439,
1.,0.866025403784439,1.,0.866025403784439,1.,0.866025403784439,1.,0.866025403784439,
1.,0.866025403784439,1.,0.866025403784439,1.,0.866025403784439,1.,0.866025403784439,
1.,0.866025403784439,1.,0.866025403784439,1.,0.866025403784439,1.,0.866025403784439,
1.,0.866025403784439,1.,0.866025403784439,1.,0.866025403784439,1.,0.866025403784439,
1.,0.866025403784439,1.,0.866025403784439,1.,0.866025403784439,1.,0.866025403784439,
1.,0.866025403784439,1.,0.866025403784439,1.,0.866025403784439,1.,0.866025403784439,
1.,0.866025403784439,1.,0.866025403784439,1.,0.866025403784439,1.,0.866025403784439,
1.,0.866025403784439,1.,0.866025403784439,1.,0.866025403784439,1.,0.866025403784439,
1.,0.866025403784439,1.,0.866025403784439,1.,0.866025403784439,1.,0.866025403784439,
1.,0.866025403784439,1.,0.866025403784439,1.,0.866025403784439,1.,0.866025403784439,
1.,0.866025403784439,1.,0.866025403784439,1.,0.866025403784439,1.,0.866025403784439,
1.,0.866025403784439,1.,0.866025403784439,1.,0.866025403784439,1.,0.866025403784439,
1.,0.866025403784439,1.,0.866025403784439,1.,0.866025403784439,1.,0.866025403784439,
1.,0.866025403784439,1.,0.866025403784439,1.,0.866025403784439,1.,0.866025403784439,
1.,0.866025403784439,1.,0.866025403784439,1.,0.866025403784439,1.,0.866025403784439,
1.,0.866025403784439,1.,0.866025403784439,1.,0.866025403784439,1.,0.866025403784439,
1.,0.866025403784439,1.,0.866025403784439,1.,0.866025403784439,1.,0.866025403784439,
1.,0.866025403784439,1.,0.866025403784439,1.,0.866025403784439,1.,0.866025403784439,
1.,0.866025403784439,1.,0.866025403784439,1.,0.866025403784439,1.,0.866025403784439,
1.,0.866025403784439,1.,0.866025403784439,1.,0.866025403784439,1.,0.866025403784439,
1.,0.866025403784439,1.,0.866025403784439,1.,0.866025403784439,1.,0.866025403784439,
1.,0.866025403784439,1.,0.866025403784439,1.,0.866025403784439,1.,0.866025403784439,
1.,0.866025403784439,1.,0.866025403784439,1.,0.866025403784439,1.,0.866025403784439,
1.,0.866025403784439,1.,0.866025403784439,1.,0.866025403784439,1.,0.866025403784439,
1.,0.866025403784439,1.,0.866025403784439,1.,0.866025403784439,1.,0.866025403784439,
1.,0.866025403784439,1.,0.866025403784439,1.,0.866025403784439,1.,0.866025403784439,
1.,0.866025403784439,1.,0.866025403784439,1.,0.866025403784439,1.,0.866025403784439,
1.,0.866025403784439,1.,0.866025403784439,1.,0.866025403784439,1.,0.866025403784439,
1.,0.866025403784439,1.,0.866025403784439,1.,0.866025403784439,1.,0.866025403784439,
1.,0.866025403784439,1.,0.866025403784439,1.,0.866025403784439,1.,0.866025403784439,
1.,0.866025403784439,1.,0.866025403784439,1.,0.866025403784439,1.,0.866025403784439,
1.,0.866025403784439,1.,0.866025403784439,1.,0.866025403784439,1.,0.866025403784439,
1.,0.866025403784439,1.,0.866025403784439,1.,0.866025403784439,1.,0.866025403784439,
1.,0.866025403784439,1.,0.866025403784439,1.,0.866025403784439,1.,0.866025403784439,
1.,0.866025403784439,1.,0.866025403784439,1.,0.866025403784439,1.,0.866025403784439,
1.,0.866025403784439,1.,0.866025403784439,1.,0.866025403784439,1.,0.866025403784439,
1.,0.866025403784439,1.,0.866025403784439,1.,0.866025403784439,1.,0.866025403784439,
1.,0.866025403784439,1.,0.866025403784439,1.,0.866025403784439,1.,0.866025403784439,
1.,0.866025403784439,1.,0.866025403784439,1.,0.866025403784439,1.,0.866025403784439,
1.,0.866025403784439,1.,0.866025403784439,1.,0.866025403784439,1.,0.866025403784439,
1.,0.866025403784439,1.,0.866025403784439,1.,0.866025403784439,1.,0.866025403784439,
1.,0.866025403784439,1.,0.866025403784439,1.,0.866025403784439,1.,0.866025403784439,
1.,0.866025403784439,1.,0.866025403784439,1.,0.866025403784439,1.,0.866025403784439,
1.,0.866025403784439,1.,0.866025403784439,1.,0.866025403784439,1.,0.866025403784439,
1.,0.866025403784439,1.,0.866025403784439,1.,0.866025403784439,1.,0.866025403784439,
1.,0.866025403784439,1.,0.866025403784439,1.,0.866025403784439,1.)))
REPRESENTATION_ITEM('')
SURFACE()
);
#2308=(
BOUNDED_SURFACE()
B_SPLINE_SURFACE(1,2,((#362849,#362850,#362851,#362852,#362853,#362854,
#362855,#362856,#362857,#362858,#362859,#362860,#362861,#362862,#362863,
#362864,#362865,#362866,#362867,#362868,#362869,#362870,#362871,#362872,
#362873,#362874,#362875,#362876,#362877,#362878,#362879,#362880,#362881,
#362882,#362883,#362884,#362885,#362886,#362887,#362888,#362889,#362890,
#362891,#362892,#362893,#362894,#362895,#362896,#362897,#362898,#362899,
#362900,#362901,#362902,#362903,#362904,#362905,#362906,#362907,#362908,
#362909,#362910,#362911,#362912,#362913,#362914,#362915,#362916,#362917,
#362918,#362919,#362920,#362921,#362922,#362923,#362924,#362925,#362926,
#362927,#362928,#362929,#362930,#362931,#362932,#362933,#362934,#362935,
#362936,#362937,#362938,#362939,#362940,#362941,#362942,#362943,#362944,
#362945,#362946,#362947,#362948,#362949,#362950,#362951,#362952,#362953,
#362954,#362955,#362956,#362957,#362958,#362959,#362960,#362961,#362962,
#362963,#362964,#362965,#362966,#362967,#362968,#362969,#362970,#362971,
#362972,#362973,#362974,#362975,#362976,#362977,#362978,#362979,#362980,
#362981,#362982,#362983,#362984,#362985,#362986,#362987,#362988,#362989,
#362990,#362991,#362992,#362993,#362994,#362995,#362996,#362997,#362998,
#362999,#363000,#363001,#363002,#363003,#363004,#363005,#363006,#363007,
#363008,#363009,#363010,#363011,#363012,#363013,#363014,#363015,#363016,
#363017,#363018,#363019,#363020,#363021,#363022,#363023,#363024,#363025,
#363026,#363027,#363028,#363029,#363030,#363031,#363032,#363033,#363034,
#363035,#363036,#363037,#363038,#363039,#363040,#363041,#363042,#363043,
#363044,#363045,#363046,#363047,#363048,#363049,#363050,#363051,#363052,
#363053,#363054,#363055,#363056,#363057,#363058,#363059,#363060,#363061,
#363062,#363063,#363064,#363065,#363066,#363067,#363068,#363069,#363070,
#363071,#363072,#363073,#363074,#363075,#363076,#363077,#363078,#363079,
#363080,#363081,#363082,#363083,#363084,#363085,#363086,#363087,#363088,
#363089,#363090,#363091,#363092,#363093,#363094,#363095,#363096,#363097,
#363098,#363099,#363100,#363101,#363102,#363103,#363104,#363105,#363106,
#363107,#363108,#363109,#363110,#363111,#363112,#363113,#363114,#363115,
#363116,#363117,#363118,#363119,#363120,#363121,#363122,#363123,#363124,
#363125,#363126,#363127,#363128,#363129,#363130,#363131,#363132,#363133,
#363134,#363135,#363136,#363137,#363138,#363139,#363140,#363141,#363142,
#363143,#363144,#363145,#363146,#363147,#363148,#363149,#363150,#363151,
#363152,#363153,#363154,#363155,#363156,#363157,#363158,#363159,#363160,
#363161,#363162,#363163,#363164,#363165,#363166,#363167,#363168,#363169,
#363170,#363171,#363172,#363173,#363174,#363175,#363176,#363177,#363178,
#363179,#363180,#363181,#363182,#363183,#363184,#363185,#363186,#363187,
#363188,#363189,#363190,#363191,#363192,#363193,#363194,#363195,#363196,
#363197,#363198,#363199,#363200,#363201,#363202,#363203,#363204,#363205,
#363206,#363207,#363208,#363209,#363210,#363211,#363212,#363213,#363214,
#363215,#363216,#363217,#363218,#363219,#363220,#363221,#363222,#363223,
#363224,#363225,#363226,#363227,#363228,#363229,#363230,#363231,#363232,
#363233,#363234,#363235,#363236,#363237,#363238,#363239,#363240,#363241,
#363242,#363243,#363244,#363245),(#363246,#363247,#363248,#363249,#363250,
#363251,#363252,#363253,#363254,#363255,#363256,#363257,#363258,#363259,
#363260,#363261,#363262,#363263,#363264,#363265,#363266,#363267,#363268,
#363269,#363270,#363271,#363272,#363273,#363274,#363275,#363276,#363277,
#363278,#363279,#363280,#363281,#363282,#363283,#363284,#363285,#363286,
#363287,#363288,#363289,#363290,#363291,#363292,#363293,#363294,#363295,
#363296,#363297,#363298,#363299,#363300,#363301,#363302,#363303,#363304,
#363305,#363306,#363307,#363308,#363309,#363310,#363311,#363312,#363313,
#363314,#363315,#363316,#363317,#363318,#363319,#363320,#363321,#363322,
#363323,#363324,#363325,#363326,#363327,#363328,#363329,#363330,#363331,
#363332,#363333,#363334,#363335,#363336,#363337,#363338,#363339,#363340,
#363341,#363342,#363343,#363344,#363345,#363346,#363347,#363348,#363349,
#363350,#363351,#363352,#363353,#363354,#363355,#363356,#363357,#363358,
#363359,#363360,#363361,#363362,#363363,#363364,#363365,#363366,#363367,
#363368,#363369,#363370,#363371,#363372,#363373,#363374,#363375,#363376,
#363377,#363378,#363379,#363380,#363381,#363382,#363383,#363384,#363385,
#363386,#363387,#363388,#363389,#363390,#363391,#363392,#363393,#363394,
#363395,#363396,#363397,#363398,#363399,#363400,#363401,#363402,#363403,
#363404,#363405,#363406,#363407,#363408,#363409,#363410,#363411,#363412,
#363413,#363414,#363415,#363416,#363417,#363418,#363419,#363420,#363421,
#363422,#363423,#363424,#363425,#363426,#363427,#363428,#363429,#363430,
#363431,#363432,#363433,#363434,#363435,#363436,#363437,#363438,#363439,
#363440,#363441,#363442,#363443,#363444,#363445,#363446,#363447,#363448,
#363449,#363450,#363451,#363452,#363453,#363454,#363455,#363456,#363457,
#363458,#363459,#363460,#363461,#363462,#363463,#363464,#363465,#363466,
#363467,#363468,#363469,#363470,#363471,#363472,#363473,#363474,#363475,
#363476,#363477,#363478,#363479,#363480,#363481,#363482,#363483,#363484,
#363485,#363486,#363487,#363488,#363489,#363490,#363491,#363492,#363493,
#363494,#363495,#363496,#363497,#363498,#363499,#363500,#363501,#363502,
#363503,#363504,#363505,#363506,#363507,#363508,#363509,#363510,#363511,
#363512,#363513,#363514,#363515,#363516,#363517,#363518,#363519,#363520,
#363521,#363522,#363523,#363524,#363525,#363526,#363527,#363528,#363529,
#363530,#363531,#363532,#363533,#363534,#363535,#363536,#363537,#363538,
#363539,#363540,#363541,#363542,#363543,#363544,#363545,#363546,#363547,
#363548,#363549,#363550,#363551,#363552,#363553,#363554,#363555,#363556,
#363557,#363558,#363559,#363560,#363561,#363562,#363563,#363564,#363565,
#363566,#363567,#363568,#363569,#363570,#363571,#363572,#363573,#363574,
#363575,#363576,#363577,#363578,#363579,#363580,#363581,#363582,#363583,
#363584,#363585,#363586,#363587,#363588,#363589,#363590,#363591,#363592,
#363593,#363594,#363595,#363596,#363597,#363598,#363599,#363600,#363601,
#363602,#363603,#363604,#363605,#363606,#363607,#363608,#363609,#363610,
#363611,#363612,#363613,#363614,#363615,#363616,#363617,#363618,#363619,
#363620,#363621,#363622,#363623,#363624,#363625,#363626,#363627,#363628,
#363629,#363630,#363631,#363632,#363633,#363634,#363635,#363636,#363637,
#363638,#363639,#363640,#363641,#363642)),.UNSPECIFIED.,.F.,.F.,.F.)
B_SPLINE_SURFACE_WITH_KNOTS((2,2),(3,2,2,2,2,2,2,2,2,2,2,2,2,2,2,2,2,2,
2,2,2,2,2,2,2,2,2,2,2,2,2,2,2,2,2,2,2,2,2,2,2,2,2,2,2,2,2,2,2,2,2,2,2,2,
2,2,2,2,2,2,2,2,2,2,2,2,2,2,2,2,2,2,2,2,2,2,2,2,2,2,2,2,2,2,2,2,2,2,2,2,
2,2,2,2,2,2,2,2,2,2,2,2,2,2,2,2,2,2,2,2,2,2,2,2,2,2,2,2,2,2,2,2,2,2,2,2,
2,2,2,2,2,2,2,2,2,2,2,2,2,2,2,2,2,2,2,2,2,2,2,2,2,2,2,2,2,2,2,2,2,2,2,2,
2,2,2,2,2,2,2,2,2,2,2,2,2,2,2,2,2,2,2,2,2,2,2,2,2,2,2,2,2,2,2,2,2,2,2,2,
3),(-1.21782920567261E-5,1.),(0.,0.00505050505050505,0.0101010101010101,
0.0151515151515152,0.0202020202020202,0.0252525252525253,0.0303030303030303,
0.0353535353535354,0.0404040404040404,0.0454545454545455,0.0505050505050505,
0.0555555555555556,0.0606060606060606,0.0656565656565657,0.0707070707070707,
0.0757575757575758,0.0808080808080808,0.0858585858585859,0.0909090909090909,
0.095959595959596,0.101010101010101,0.106060606060606,0.111111111111111,
0.116161616161616,0.121212121212121,0.126262626262626,0.131313131313131,
0.136363636363636,0.141414141414141,0.146464646464646,0.151515151515152,
0.156565656565657,0.161616161616162,0.166666666666667,0.171717171717172,
0.176767676767677,0.181818181818182,0.186868686868687,0.191919191919192,
0.196969696969697,0.202020202020202,0.207070707070707,0.212121212121212,
0.217171717171717,0.222222222222222,0.227272727272727,0.232323232323232,
0.237373737373737,0.242424242424242,0.247474747474747,0.252525252525253,
0.257575757575758,0.262626262626263,0.267676767676768,0.272727272727273,
0.277777777777778,0.282828282828283,0.287878787878788,0.292929292929293,
0.297979797979798,0.303030303030303,0.308080808080808,0.313131313131313,
0.318181818181818,0.323232323232323,0.328282828282828,0.333333333333333,
0.338383838383838,0.343434343434343,0.348484848484849,0.353535353535354,
0.358585858585859,0.363636363636364,0.368686868686869,0.373737373737374,
0.378787878787879,0.383838383838384,0.388888888888889,0.393939393939394,
0.398989898989899,0.404040404040404,0.409090909090909,0.414141414141414,
0.419191919191919,0.424242424242424,0.429292929292929,0.434343434343434,
0.439393939393939,0.444444444444444,0.44949494949495,0.454545454545455,
0.45959595959596,0.464646464646465,0.46969696969697,0.474747474747475,0.47979797979798,
0.484848484848485,0.48989898989899,0.494949494949495,0.5,0.505050505050505,
0.51010101010101,0.515151515151515,0.52020202020202,0.525252525252525,0.53030303030303,
0.535353535353535,0.54040404040404,0.545454545454545,0.55050505050505,0.555555555555556,
0.560606060606061,0.565656565656566,0.570707070707071,0.575757575757576,
0.580808080808081,0.585858585858586,0.590909090909091,0.595959595959596,
0.601010101010101,0.606060606060606,0.611111111111111,0.616161616161616,
0.621212121212121,0.626262626262626,0.631313131313131,0.636363636363636,
0.641414141414141,0.646464646464647,0.651515151515151,0.656565656565657,
0.661616161616162,0.666666666666667,0.671717171717172,0.676767676767677,
0.681818181818182,0.686868686868687,0.691919191919192,0.696969696969697,
0.702020202020202,0.707070707070707,0.712121212121212,0.717171717171717,
0.722222222222222,0.727272727272727,0.732323232323232,0.737373737373737,
0.742424242424242,0.747474747474748,0.752525252525252,0.757575757575758,
0.762626262626263,0.767676767676768,0.772727272727273,0.777777777777778,
0.782828282828283,0.787878787878788,0.792929292929293,0.797979797979798,
0.803030303030303,0.808080808080808,0.813131313131313,0.818181818181818,
0.823232323232323,0.828282828282828,0.833333333333333,0.838383838383838,
0.843434343434343,0.848484848484849,0.853535353535353,0.858585858585859,
0.863636363636364,0.868686868686869,0.873737373737374,0.878787878787879,
0.883838383838384,0.888888888888889,0.893939393939394,0.898989898989899,
0.904040404040404,0.909090909090909,0.914141414141414,0.919191919191919,
0.924242424242424,0.929292929292929,0.934343434343434,0.939393939393939,
0.944444444444444,0.94949494949495,0.954545454545455,0.95959595959596,0.964646464646465,
0.96969696969697,0.974747474747475,0.97979797979798,0.984848484848485,0.98989898989899,
0.994949494949495,1.),.UNSPECIFIED.)
GEOMETRIC_REPRESENTATION_ITEM()
RATIONAL_B_SPLINE_SURFACE(((1.,0.866025403784439,1.,0.866025403784439,1.,
0.866025403784439,1.,0.866025403784439,1.,0.866025403784439,1.,0.866025403784439,
1.,0.866025403784439,1.,0.866025403784439,1.,0.866025403784439,1.,0.866025403784439,
1.,0.866025403784439,1.,0.866025403784439,1.,0.866025403784439,1.,0.866025403784439,
1.,0.866025403784439,1.,0.866025403784439,1.,0.866025403784439,1.,0.866025403784439,
1.,0.866025403784439,1.,0.866025403784439,1.,0.866025403784439,1.,0.866025403784439,
1.,0.866025403784439,1.,0.866025403784439,1.,0.866025403784439,1.,0.866025403784439,
1.,0.866025403784439,1.,0.866025403784439,1.,0.866025403784439,1.,0.866025403784439,
1.,0.866025403784439,1.,0.866025403784439,1.,0.866025403784439,1.,0.866025403784439,
1.,0.866025403784439,1.,0.866025403784439,1.,0.866025403784439,1.,0.866025403784439,
1.,0.866025403784439,1.,0.866025403784439,1.,0.866025403784439,1.,0.866025403784439,
1.,0.866025403784439,1.,0.866025403784439,1.,0.866025403784439,1.,0.866025403784439,
1.,0.866025403784439,1.,0.866025403784439,1.,0.866025403784439,1.,0.866025403784439,
1.,0.866025403784439,1.,0.866025403784439,1.,0.866025403784439,1.,0.866025403784439,
1.,0.866025403784439,1.,0.866025403784439,1.,0.866025403784439,1.,0.866025403784439,
1.,0.866025403784439,1.,0.866025403784439,1.,0.866025403784439,1.,0.866025403784439,
1.,0.866025403784439,1.,0.866025403784439,1.,0.866025403784439,1.,0.866025403784439,
1.,0.866025403784439,1.,0.866025403784439,1.,0.866025403784439,1.,0.866025403784439,
1.,0.866025403784439,1.,0.866025403784439,1.,0.866025403784439,1.,0.866025403784439,
1.,0.866025403784439,1.,0.866025403784439,1.,0.866025403784439,1.,0.866025403784439,
1.,0.866025403784439,1.,0.866025403784439,1.,0.866025403784439,1.,0.866025403784439,
1.,0.866025403784439,1.,0.866025403784439,1.,0.866025403784439,1.,0.866025403784439,
1.,0.866025403784439,1.,0.866025403784439,1.,0.866025403784439,1.,0.866025403784439,
1.,0.866025403784439,1.,0.866025403784439,1.,0.866025403784439,1.,0.866025403784439,
1.,0.866025403784439,1.,0.866025403784439,1.,0.866025403784439,1.,0.866025403784439,
1.,0.866025403784439,1.,0.866025403784439,1.,0.866025403784439,1.,0.866025403784439,
1.,0.866025403784439,1.,0.866025403784439,1.,0.866025403784439,1.,0.866025403784439,
1.,0.866025403784439,1.,0.866025403784439,1.,0.866025403784439,1.,0.866025403784439,
1.,0.866025403784439,1.,0.866025403784439,1.,0.866025403784439,1.,0.866025403784439,
1.,0.866025403784439,1.,0.866025403784439,1.,0.866025403784439,1.,0.866025403784439,
1.,0.866025403784439,1.,0.866025403784439,1.,0.866025403784439,1.,0.866025403784439,
1.,0.866025403784439,1.,0.866025403784439,1.,0.866025403784439,1.,0.866025403784439,
1.,0.866025403784439,1.,0.866025403784439,1.,0.866025403784439,1.,0.866025403784439,
1.,0.866025403784439,1.,0.866025403784439,1.,0.866025403784439,1.,0.866025403784439,
1.,0.866025403784439,1.,0.866025403784439,1.,0.866025403784439,1.,0.866025403784439,
1.,0.866025403784439,1.,0.866025403784439,1.,0.866025403784439,1.,0.866025403784439,
1.,0.866025403784439,1.,0.866025403784439,1.,0.866025403784439,1.,0.866025403784439,
1.,0.866025403784439,1.,0.866025403784439,1.,0.866025403784439,1.,0.866025403784439,
1.,0.866025403784439,1.,0.866025403784439,1.,0.866025403784439,1.,0.866025403784439,
1.,0.866025403784439,1.,0.866025403784439,1.,0.866025403784439,1.,0.866025403784439,
1.,0.866025403784439,1.,0.866025403784439,1.,0.866025403784439,1.,0.866025403784439,
1.,0.866025403784439,1.,0.866025403784439,1.,0.866025403784439,1.,0.866025403784439,
1.,0.866025403784439,1.,0.866025403784439,1.,0.866025403784439,1.,0.866025403784439,
1.,0.866025403784439,1.,0.866025403784439,1.,0.866025403784439,1.,0.866025403784439,
1.,0.866025403784439,1.,0.866025403784439,1.,0.866025403784439,1.,0.866025403784439,
1.,0.866025403784439,1.,0.866025403784439,1.,0.866025403784439,1.,0.866025403784439,
1.,0.866025403784439,1.,0.866025403784439,1.,0.866025403784439,1.,0.866025403784439,
1.,0.866025403784439,1.,0.866025403784439,1.,0.866025403784439,1.,0.866025403784439,
1.,0.866025403784439,1.,0.866025403784439,1.,0.866025403784439,1.,0.866025403784439,
1.,0.866025403784439,1.,0.866025403784439,1.,0.866025403784439,1.,0.866025403784439,
1.),(1.,0.866025403784439,1.,0.866025403784439,1.,0.866025403784439,1.,
0.866025403784439,1.,0.866025403784439,1.,0.866025403784439,1.,0.866025403784439,
1.,0.866025403784439,1.,0.866025403784439,1.,0.866025403784439,1.,0.866025403784439,
1.,0.866025403784439,1.,0.866025403784439,1.,0.866025403784439,1.,0.866025403784439,
1.,0.866025403784439,1.,0.866025403784439,1.,0.866025403784439,1.,0.866025403784439,
1.,0.866025403784439,1.,0.866025403784439,1.,0.866025403784439,1.,0.866025403784439,
1.,0.866025403784439,1.,0.866025403784439,1.,0.866025403784439,1.,0.866025403784439,
1.,0.866025403784439,1.,0.866025403784439,1.,0.866025403784439,1.,0.866025403784439,
1.,0.866025403784439,1.,0.866025403784439,1.,0.866025403784439,1.,0.866025403784439,
1.,0.866025403784439,1.,0.866025403784439,1.,0.866025403784439,1.,0.866025403784439,
1.,0.866025403784439,1.,0.866025403784439,1.,0.866025403784439,1.,0.866025403784439,
1.,0.866025403784439,1.,0.866025403784439,1.,0.866025403784439,1.,0.866025403784439,
1.,0.866025403784439,1.,0.866025403784439,1.,0.866025403784439,1.,0.866025403784439,
1.,0.866025403784439,1.,0.866025403784439,1.,0.866025403784439,1.,0.866025403784439,
1.,0.866025403784439,1.,0.866025403784439,1.,0.866025403784439,1.,0.866025403784439,
1.,0.866025403784439,1.,0.866025403784439,1.,0.866025403784439,1.,0.866025403784439,
1.,0.866025403784439,1.,0.866025403784439,1.,0.866025403784439,1.,0.866025403784439,
1.,0.866025403784439,1.,0.866025403784439,1.,0.866025403784439,1.,0.866025403784439,
1.,0.866025403784439,1.,0.866025403784439,1.,0.866025403784439,1.,0.866025403784439,
1.,0.866025403784439,1.,0.866025403784439,1.,0.866025403784439,1.,0.866025403784439,
1.,0.866025403784439,1.,0.866025403784439,1.,0.866025403784439,1.,0.866025403784439,
1.,0.866025403784439,1.,0.866025403784439,1.,0.866025403784439,1.,0.866025403784439,
1.,0.866025403784439,1.,0.866025403784439,1.,0.866025403784439,1.,0.866025403784439,
1.,0.866025403784439,1.,0.866025403784439,1.,0.866025403784439,1.,0.866025403784439,
1.,0.866025403784439,1.,0.866025403784439,1.,0.866025403784439,1.,0.866025403784439,
1.,0.866025403784439,1.,0.866025403784439,1.,0.866025403784439,1.,0.866025403784439,
1.,0.866025403784439,1.,0.866025403784439,1.,0.866025403784439,1.,0.866025403784439,
1.,0.866025403784439,1.,0.866025403784439,1.,0.866025403784439,1.,0.866025403784439,
1.,0.866025403784439,1.,0.866025403784439,1.,0.866025403784439,1.,0.866025403784439,
1.,0.866025403784439,1.,0.866025403784439,1.,0.866025403784439,1.,0.866025403784439,
1.,0.866025403784439,1.,0.866025403784439,1.,0.866025403784439,1.,0.866025403784439,
1.,0.866025403784439,1.,0.866025403784439,1.,0.866025403784439,1.,0.866025403784439,
1.,0.866025403784439,1.,0.866025403784439,1.,0.866025403784439,1.,0.866025403784439,
1.,0.866025403784439,1.,0.866025403784439,1.,0.866025403784439,1.,0.866025403784439,
1.,0.866025403784439,1.,0.866025403784439,1.,0.866025403784439,1.,0.866025403784439,
1.,0.866025403784439,1.,0.866025403784439,1.,0.866025403784439,1.,0.866025403784439,
1.,0.866025403784439,1.,0.866025403784439,1.,0.866025403784439,1.,0.866025403784439,
1.,0.866025403784439,1.,0.866025403784439,1.,0.866025403784439,1.,0.866025403784439,
1.,0.866025403784439,1.,0.866025403784439,1.,0.866025403784439,1.,0.866025403784439,
1.,0.866025403784439,1.,0.866025403784439,1.,0.866025403784439,1.,0.866025403784439,
1.,0.866025403784439,1.,0.866025403784439,1.,0.866025403784439,1.,0.866025403784439,
1.,0.866025403784439,1.,0.866025403784439,1.,0.866025403784439,1.,0.866025403784439,
1.,0.866025403784439,1.,0.866025403784439,1.,0.866025403784439,1.,0.866025403784439,
1.,0.866025403784439,1.,0.866025403784439,1.,0.866025403784439,1.,0.866025403784439,
1.,0.866025403784439,1.,0.866025403784439,1.,0.866025403784439,1.,0.866025403784439,
1.,0.866025403784439,1.,0.866025403784439,1.,0.866025403784439,1.,0.866025403784439,
1.,0.866025403784439,1.,0.866025403784439,1.,0.866025403784439,1.,0.866025403784439,
1.,0.866025403784439,1.,0.866025403784439,1.,0.866025403784439,1.,0.866025403784439,
1.,0.866025403784439,1.,0.866025403784439,1.,0.866025403784439,1.,0.866025403784439,
1.,0.866025403784439,1.,0.866025403784439,1.,0.866025403784439,1.)))
REPRESENTATION_ITEM('')
SURFACE()
);
#2309=(
BOUNDED_SURFACE()
B_SPLINE_SURFACE(3,3,((#363644,#363645,#363646,#363647,#363648,#363649,
#363650,#363651,#363652,#363653,#363654,#363655,#363656,#363657,#363658,
#363659,#363660,#363661,#363662,#363663,#363664,#363665,#363666,#363667,
#363668,#363669,#363670,#363671,#363672),(#363673,#363674,#363675,#363676,
#363677,#363678,#363679,#363680,#363681,#363682,#363683,#363684,#363685,
#363686,#363687,#363688,#363689,#363690,#363691,#363692,#363693,#363694,
#363695,#363696,#363697,#363698,#363699,#363700,#363701),(#363702,#363703,
#363704,#363705,#363706,#363707,#363708,#363709,#363710,#363711,#363712,
#363713,#363714,#363715,#363716,#363717,#363718,#363719,#363720,#363721,
#363722,#363723,#363724,#363725,#363726,#363727,#363728,#363729,#363730),
(#363731,#363732,#363733,#363734,#363735,#363736,#363737,#363738,#363739,
#363740,#363741,#363742,#363743,#363744,#363745,#363746,#363747,#363748,
#363749,#363750,#363751,#363752,#363753,#363754,#363755,#363756,#363757,
#363758,#363759),(#363760,#363761,#363762,#363763,#363764,#363765,#363766,
#363767,#363768,#363769,#363770,#363771,#363772,#363773,#363774,#363775,
#363776,#363777,#363778,#363779,#363780,#363781,#363782,#363783,#363784,
#363785,#363786,#363787,#363788),(#363789,#363790,#363791,#363792,#363793,
#363794,#363795,#363796,#363797,#363798,#363799,#363800,#363801,#363802,
#363803,#363804,#363805,#363806,#363807,#363808,#363809,#363810,#363811,
#363812,#363813,#363814,#363815,#363816,#363817),(#363818,#363819,#363820,
#363821,#363822,#363823,#363824,#363825,#363826,#363827,#363828,#363829,
#363830,#363831,#363832,#363833,#363834,#363835,#363836,#363837,#363838,
#363839,#363840,#363841,#363842,#363843,#363844,#363845,#363846)),
 .UNSPECIFIED.,.T.,.F.,.F.)
B_SPLINE_SURFACE_WITH_KNOTS((4,3,4),(4,1,1,1,1,1,1,1,1,1,1,1,1,1,1,1,1,
1,1,1,1,1,1,1,1,1,4),(0.,0.5,1.),(0.,0.0310703336761616,0.0624385278003938,
0.0937144048499659,0.124978469089869,0.166663774179581,0.208294236860357,
0.249966520356582,0.291641529650434,0.3332733240007,0.374947073344913,0.416620808022619,
0.458253030541402,0.499926784452264,0.54160045129851,0.583232674441905,
0.624906496125386,0.666580158626562,0.708211959489969,0.749887054558503,
0.791559255246094,0.833189756589646,0.87487513422873,0.906139159779086,
0.937415106668169,0.968783217665703,1.),.UNSPECIFIED.)
GEOMETRIC_REPRESENTATION_ITEM()
RATIONAL_B_SPLINE_SURFACE(((1.,1.,1.,1.,1.,1.,1.,1.,1.,1.,1.,1.,1.,1.,1.,
1.,1.,1.,1.,1.,1.,1.,1.,1.,1.,1.,1.,1.,1.),(0.333333333333333,0.333333333333333,
0.333333333333334,0.333333333333333,0.333333333333333,0.333333333333333,
0.333333333333333,0.333333333333333,0.333333333333333,0.333333333333333,
0.333333333333333,0.333333333333333,0.333333333333334,0.333333333333333,
0.333333333333333,0.333333333333333,0.333333333333333,0.333333333333333,
0.333333333333333,0.333333333333333,0.333333333333333,0.333333333333333,
0.333333333333333,0.333333333333333,0.333333333333333,0.333333333333333,
0.333333333333333,0.333333333333333,0.333333333333333),(0.333333333333333,
0.333333333333333,0.333333333333334,0.333333333333333,0.333333333333333,
0.333333333333333,0.333333333333333,0.333333333333333,0.333333333333333,
0.333333333333333,0.333333333333333,0.333333333333333,0.333333333333334,
0.333333333333333,0.333333333333333,0.333333333333333,0.333333333333333,
0.333333333333333,0.333333333333333,0.333333333333333,0.333333333333333,
0.333333333333333,0.333333333333333,0.333333333333333,0.333333333333333,
0.333333333333333,0.333333333333333,0.333333333333333,0.333333333333333),
(1.,1.,1.,1.,1.,1.,1.,1.,1.,1.,1.,1.,1.,1.,1.,1.,1.,1.,1.,1.,1.,1.,1.,1.,
1.,1.,1.,1.,1.),(0.333333333333333,0.333333333333333,0.333333333333334,
0.333333333333333,0.333333333333333,0.333333333333333,0.333333333333333,
0.333333333333333,0.333333333333333,0.333333333333333,0.333333333333333,
0.333333333333333,0.333333333333334,0.333333333333333,0.333333333333333,
0.333333333333333,0.333333333333333,0.333333333333333,0.333333333333333,
0.333333333333333,0.333333333333333,0.333333333333333,0.333333333333333,
0.333333333333333,0.333333333333333,0.333333333333333,0.333333333333333,
0.333333333333333,0.333333333333333),(0.333333333333333,0.333333333333333,
0.333333333333334,0.333333333333333,0.333333333333333,0.333333333333333,
0.333333333333333,0.333333333333333,0.333333333333333,0.333333333333333,
0.333333333333333,0.333333333333333,0.333333333333334,0.333333333333333,
0.333333333333333,0.333333333333333,0.333333333333333,0.333333333333333,
0.333333333333333,0.333333333333333,0.333333333333333,0.333333333333333,
0.333333333333333,0.333333333333333,0.333333333333333,0.333333333333333,
0.333333333333333,0.333333333333333,0.333333333333333),(1.,1.,1.,1.,1.,
1.,1.,1.,1.,1.,1.,1.,1.,1.,1.,1.,1.,1.,1.,1.,1.,1.,1.,1.,1.,1.,1.,1.,1.)))
REPRESENTATION_ITEM('')
SURFACE()
);
#2310=(
BOUNDED_SURFACE()
B_SPLINE_SURFACE(3,3,((#363913,#363914,#363915,#363916,#363917,#363918,
#363919,#363920,#363921,#363922,#363923,#363924,#363925,#363926,#363927,
#363928,#363929,#363930,#363931,#363932,#363933,#363934,#363935,#363936,
#363937,#363938,#363939,#363940,#363941,#363942,#363943,#363944,#363945,
#363946,#363947,#363948,#363949,#363950,#363951,#363952,#363953,#363954,
#363955,#363956,#363957,#363958,#363959,#363960,#363961,#363962,#363963,
#363964,#363965,#363966,#363967,#363968,#363969,#363970,#363971,#363972,
#363973,#363974,#363975,#363976,#363977,#363978,#363979,#363980,#363981,
#363982,#363983,#363984,#363985,#363986,#363987,#363988,#363989,#363990,
#363991,#363992,#363993,#363994,#363995,#363996,#363997,#363998,#363999,
#364000,#364001,#364002,#364003,#364004,#364005,#364006,#364007,#364008,
#364009,#364010,#364011),(#364012,#364013,#364014,#364015,#364016,#364017,
#364018,#364019,#364020,#364021,#364022,#364023,#364024,#364025,#364026,
#364027,#364028,#364029,#364030,#364031,#364032,#364033,#364034,#364035,
#364036,#364037,#364038,#364039,#364040,#364041,#364042,#364043,#364044,
#364045,#364046,#364047,#364048,#364049,#364050,#364051,#364052,#364053,
#364054,#364055,#364056,#364057,#364058,#364059,#364060,#364061,#364062,
#364063,#364064,#364065,#364066,#364067,#364068,#364069,#364070,#364071,
#364072,#364073,#364074,#364075,#364076,#364077,#364078,#364079,#364080,
#364081,#364082,#364083,#364084,#364085,#364086,#364087,#364088,#364089,
#364090,#364091,#364092,#364093,#364094,#364095,#364096,#364097,#364098,
#364099,#364100,#364101,#364102,#364103,#364104,#364105,#364106,#364107,
#364108,#364109,#364110),(#364111,#364112,#364113,#364114,#364115,#364116,
#364117,#364118,#364119,#364120,#364121,#364122,#364123,#364124,#364125,
#364126,#364127,#364128,#364129,#364130,#364131,#364132,#364133,#364134,
#364135,#364136,#364137,#364138,#364139,#364140,#364141,#364142,#364143,
#364144,#364145,#364146,#364147,#364148,#364149,#364150,#364151,#364152,
#364153,#364154,#364155,#364156,#364157,#364158,#364159,#364160,#364161,
#364162,#364163,#364164,#364165,#364166,#364167,#364168,#364169,#364170,
#364171,#364172,#364173,#364174,#364175,#364176,#364177,#364178,#364179,
#364180,#364181,#364182,#364183,#364184,#364185,#364186,#364187,#364188,
#364189,#364190,#364191,#364192,#364193,#364194,#364195,#364196,#364197,
#364198,#364199,#364200,#364201,#364202,#364203,#364204,#364205,#364206,
#364207,#364208,#364209),(#364210,#364211,#364212,#364213,#364214,#364215,
#364216,#364217,#364218,#364219,#364220,#364221,#364222,#364223,#364224,
#364225,#364226,#364227,#364228,#364229,#364230,#364231,#364232,#364233,
#364234,#364235,#364236,#364237,#364238,#364239,#364240,#364241,#364242,
#364243,#364244,#364245,#364246,#364247,#364248,#364249,#364250,#364251,
#364252,#364253,#364254,#364255,#364256,#364257,#364258,#364259,#364260,
#364261,#364262,#364263,#364264,#364265,#364266,#364267,#364268,#364269,
#364270,#364271,#364272,#364273,#364274,#364275,#364276,#364277,#364278,
#364279,#364280,#364281,#364282,#364283,#364284,#364285,#364286,#364287,
#364288,#364289,#364290,#364291,#364292,#364293,#364294,#364295,#364296,
#364297,#364298,#364299,#364300,#364301,#364302,#364303,#364304,#364305,
#364306,#364307,#364308),(#364309,#364310,#364311,#364312,#364313,#364314,
#364315,#364316,#364317,#364318,#364319,#364320,#364321,#364322,#364323,
#364324,#364325,#364326,#364327,#364328,#364329,#364330,#364331,#364332,
#364333,#364334,#364335,#364336,#364337,#364338,#364339,#364340,#364341,
#364342,#364343,#364344,#364345,#364346,#364347,#364348,#364349,#364350,
#364351,#364352,#364353,#364354,#364355,#364356,#364357,#364358,#364359,
#364360,#364361,#364362,#364363,#364364,#364365,#364366,#364367,#364368,
#364369,#364370,#364371,#364372,#364373,#364374,#364375,#364376,#364377,
#364378,#364379,#364380,#364381,#364382,#364383,#364384,#364385,#364386,
#364387,#364388,#364389,#364390,#364391,#364392,#364393,#364394,#364395,
#364396,#364397,#364398,#364399,#364400,#364401,#364402,#364403,#364404,
#364405,#364406,#364407),(#364408,#364409,#364410,#364411,#364412,#364413,
#364414,#364415,#364416,#364417,#364418,#364419,#364420,#364421,#364422,
#364423,#364424,#364425,#364426,#364427,#364428,#364429,#364430,#364431,
#364432,#364433,#364434,#364435,#364436,#364437,#364438,#364439,#364440,
#364441,#364442,#364443,#364444,#364445,#364446,#364447,#364448,#364449,
#364450,#364451,#364452,#364453,#364454,#364455,#364456,#364457,#364458,
#364459,#364460,#364461,#364462,#364463,#364464,#364465,#364466,#364467,
#364468,#364469,#364470,#364471,#364472,#364473,#364474,#364475,#364476,
#364477,#364478,#364479,#364480,#364481,#364482,#364483,#364484,#364485,
#364486,#364487,#364488,#364489,#364490,#364491,#364492,#364493,#364494,
#364495,#364496,#364497,#364498,#364499,#364500,#364501,#364502,#364503,
#364504,#364505,#364506),(#364507,#364508,#364509,#364510,#364511,#364512,
#364513,#364514,#364515,#364516,#364517,#364518,#364519,#364520,#364521,
#364522,#364523,#364524,#364525,#364526,#364527,#364528,#364529,#364530,
#364531,#364532,#364533,#364534,#364535,#364536,#364537,#364538,#364539,
#364540,#364541,#364542,#364543,#364544,#364545,#364546,#364547,#364548,
#364549,#364550,#364551,#364552,#364553,#364554,#364555,#364556,#364557,
#364558,#364559,#364560,#364561,#364562,#364563,#364564,#364565,#364566,
#364567,#364568,#364569,#364570,#364571,#364572,#364573,#364574,#364575,
#364576,#364577,#364578,#364579,#364580,#364581,#364582,#364583,#364584,
#364585,#364586,#364587,#364588,#364589,#364590,#364591,#364592,#364593,
#364594,#364595,#364596,#364597,#364598,#364599,#364600,#364601,#364602,
#364603,#364604,#364605)),.UNSPECIFIED.,.T.,.F.,.F.)
B_SPLINE_SURFACE_WITH_KNOTS((4,3,4),(4,1,1,1,1,1,1,1,1,1,1,1,1,1,1,1,1,
1,1,1,1,1,1,1,1,1,1,1,1,1,1,1,1,1,1,1,1,1,1,1,1,1,1,1,1,1,1,1,1,1,1,1,1,
1,1,1,1,1,1,1,1,1,1,1,1,1,1,1,1,1,1,1,1,1,1,1,1,1,1,1,1,1,1,1,1,1,1,1,1,
1,1,1,1,1,1,1,4),(0.,0.5,1.),(0.,0.0104467457848562,0.0208697051534179,
0.0312830741812588,0.0417059245369557,0.0521151844214314,0.0625350854994869,
0.072955523619078,0.0833651614361216,0.093785355257659,0.104205506224069,
0.114615259182489,0.125035444608255,0.135455580151817,0.145865343296126,
0.156285526040368,0.166705661591602,0.177115425208493,0.187535607700786,
0.197955743339009,0.208365506953668,0.218785689432554,0.229205825080053,
0.239615588692213,0.250035771170918,0.260455906818944,0.270865670430874,
0.281285852909622,0.291705988557657,0.302115752169577,0.312535934648329,
0.322956070296362,0.333365833908282,0.343786016387035,0.354206152035067,
0.364615915646988,0.375036098125741,0.385456233773773,0.395865997385694,
0.406286179864446,0.416706315512479,0.427116079124399,0.437536261603152,
0.447956397251184,0.458366160863105,0.468786343341857,0.47920647898989,
0.48961624260181,0.500036425080563,0.510456560728595,0.520866324340516,
0.531286506819269,0.541706642467301,0.552116406079222,0.562536588557974,
0.572956724206007,0.583366487817927,0.59378667029668,0.604206805944712,
0.614616569556633,0.625036752035385,0.635456887683418,0.645866651295338,
0.656286833774091,0.666706969422123,0.677116733034044,0.687536915512797,
0.697957051160829,0.708366814772749,0.718786997251504,0.729207132899531,
0.739616896511461,0.750037078990207,0.760457214638192,0.770866978250353,
0.781287160728572,0.791707296376735,0.802117059991444,0.812537242460403,
0.822957378121908,0.833367141740239,0.843787324122365,0.85420746003523,
0.864617223206175,0.875037405580635,0.885457544175532,0.895867297492078,
0.906287495257385,0.916707642366043,0.927117283641006,0.937537767903979,
0.947957624414904,0.958366904818021,0.968789794286159,0.979203137018726,
0.989626134310512,1.),.UNSPECIFIED.)
GEOMETRIC_REPRESENTATION_ITEM()
RATIONAL_B_SPLINE_SURFACE(((1.,1.,1.,1.,1.,1.,1.,1.,1.,1.,1.,1.,1.,1.,1.,
1.,1.,1.,1.,1.,1.,1.,1.,1.,1.,1.,1.,1.,1.,1.,1.,1.,1.,1.,1.,1.,1.,1.,1.,
1.,1.,1.,1.,1.,1.,1.,1.,1.,1.,1.,1.,1.,1.,1.,1.,1.,1.,1.,1.,1.,1.,1.,1.,
1.,1.,1.,1.,1.,1.,1.,1.,1.,1.,1.,1.,1.,1.,1.,1.,1.,1.,1.,1.,1.,1.,1.,1.,
1.,1.,1.,1.,1.,1.,1.,1.,1.,1.,1.,1.),(0.333333333333333,0.333333333333333,
0.333333333333333,0.333333333333333,0.333333333333333,0.333333333333333,
0.333333333333333,0.333333333333333,0.333333333333333,0.333333333333333,
0.333333333333333,0.333333333333333,0.333333333333333,0.333333333333333,
0.333333333333333,0.333333333333333,0.333333333333333,0.333333333333333,
0.333333333333333,0.333333333333333,0.333333333333333,0.333333333333333,
0.333333333333333,0.333333333333333,0.333333333333333,0.333333333333333,
0.333333333333333,0.333333333333333,0.333333333333333,0.333333333333333,
0.333333333333333,0.333333333333333,0.333333333333333,0.333333333333333,
0.333333333333333,0.333333333333333,0.333333333333333,0.333333333333333,
0.333333333333333,0.333333333333333,0.333333333333333,0.333333333333333,
0.333333333333333,0.333333333333333,0.333333333333333,0.333333333333333,
0.333333333333333,0.333333333333333,0.333333333333333,0.333333333333333,
0.333333333333333,0.333333333333333,0.333333333333333,0.333333333333333,
0.333333333333333,0.333333333333333,0.333333333333333,0.333333333333333,
0.333333333333333,0.333333333333333,0.333333333333333,0.333333333333333,
0.333333333333333,0.333333333333333,0.333333333333333,0.333333333333333,
0.333333333333333,0.333333333333333,0.333333333333333,0.333333333333333,
0.333333333333333,0.333333333333333,0.333333333333333,0.333333333333333,
0.333333333333333,0.333333333333333,0.333333333333333,0.333333333333333,
0.333333333333333,0.333333333333333,0.333333333333333,0.333333333333333,
0.333333333333333,0.333333333333333,0.333333333333333,0.333333333333333,
0.333333333333333,0.333333333333333,0.333333333333333,0.333333333333333,
0.333333333333333,0.333333333333333,0.333333333333333,0.333333333333333,
0.333333333333333,0.333333333333333,0.333333333333333,0.333333333333333,
0.333333333333333),(0.333333333333333,0.333333333333333,0.333333333333333,
0.333333333333333,0.333333333333333,0.333333333333333,0.333333333333333,
0.333333333333333,0.333333333333333,0.333333333333333,0.333333333333333,
0.333333333333333,0.333333333333333,0.333333333333333,0.333333333333333,
0.333333333333333,0.333333333333333,0.333333333333333,0.333333333333333,
0.333333333333333,0.333333333333333,0.333333333333333,0.333333333333333,
0.333333333333333,0.333333333333333,0.333333333333333,0.333333333333333,
0.333333333333333,0.333333333333333,0.333333333333333,0.333333333333333,
0.333333333333333,0.333333333333333,0.333333333333333,0.333333333333333,
0.333333333333333,0.333333333333333,0.333333333333333,0.333333333333333,
0.333333333333333,0.333333333333333,0.333333333333333,0.333333333333333,
0.333333333333333,0.333333333333333,0.333333333333333,0.333333333333333,
0.333333333333333,0.333333333333333,0.333333333333333,0.333333333333333,
0.333333333333333,0.333333333333333,0.333333333333333,0.333333333333333,
0.333333333333333,0.333333333333333,0.333333333333333,0.333333333333333,
0.333333333333333,0.333333333333333,0.333333333333333,0.333333333333333,
0.333333333333333,0.333333333333333,0.333333333333333,0.333333333333333,
0.333333333333333,0.333333333333333,0.333333333333333,0.333333333333333,
0.333333333333333,0.333333333333333,0.333333333333333,0.333333333333333,
0.333333333333333,0.333333333333333,0.333333333333333,0.333333333333333,
0.333333333333333,0.333333333333333,0.333333333333333,0.333333333333333,
0.333333333333333,0.333333333333333,0.333333333333333,0.333333333333333,
0.333333333333333,0.333333333333333,0.333333333333333,0.333333333333333,
0.333333333333333,0.333333333333333,0.333333333333333,0.333333333333333,
0.333333333333333,0.333333333333333,0.333333333333333,0.333333333333333),
(1.,1.,1.,1.,1.,1.,1.,1.,1.,1.,1.,1.,1.,1.,1.,1.,1.,1.,1.,1.,1.,1.,1.,1.,
1.,1.,1.,1.,1.,1.,1.,1.,1.,1.,1.,1.,1.,1.,1.,1.,1.,1.,1.,1.,1.,1.,1.,1.,
1.,1.,1.,1.,1.,1.,1.,1.,1.,1.,1.,1.,1.,1.,1.,1.,1.,1.,1.,1.,1.,1.,1.,1.,
1.,1.,1.,1.,1.,1.,1.,1.,1.,1.,1.,1.,1.,1.,1.,1.,1.,1.,1.,1.,1.,1.,1.,1.,
1.,1.,1.),(0.333333333333333,0.333333333333333,0.333333333333333,0.333333333333333,
0.333333333333333,0.333333333333333,0.333333333333333,0.333333333333333,
0.333333333333333,0.333333333333333,0.333333333333333,0.333333333333333,
0.333333333333333,0.333333333333333,0.333333333333333,0.333333333333333,
0.333333333333333,0.333333333333333,0.333333333333333,0.333333333333333,
0.333333333333333,0.333333333333333,0.333333333333333,0.333333333333333,
0.333333333333333,0.333333333333333,0.333333333333333,0.333333333333333,
0.333333333333333,0.333333333333333,0.333333333333333,0.333333333333333,
0.333333333333333,0.333333333333333,0.333333333333333,0.333333333333333,
0.333333333333333,0.333333333333333,0.333333333333333,0.333333333333333,
0.333333333333333,0.333333333333333,0.333333333333333,0.333333333333333,
0.333333333333333,0.333333333333333,0.333333333333333,0.333333333333333,
0.333333333333333,0.333333333333333,0.333333333333333,0.333333333333333,
0.333333333333333,0.333333333333333,0.333333333333333,0.333333333333333,
0.333333333333333,0.333333333333333,0.333333333333333,0.333333333333333,
0.333333333333333,0.333333333333333,0.333333333333333,0.333333333333333,
0.333333333333333,0.333333333333333,0.333333333333333,0.333333333333333,
0.333333333333333,0.333333333333333,0.333333333333333,0.333333333333333,
0.333333333333333,0.333333333333333,0.333333333333333,0.333333333333333,
0.333333333333333,0.333333333333333,0.333333333333333,0.333333333333333,
0.333333333333333,0.333333333333333,0.333333333333333,0.333333333333333,
0.333333333333333,0.333333333333333,0.333333333333333,0.333333333333333,
0.333333333333333,0.333333333333333,0.333333333333333,0.333333333333333,
0.333333333333333,0.333333333333333,0.333333333333333,0.333333333333333,
0.333333333333333,0.333333333333333,0.333333333333333),(0.333333333333333,
0.333333333333333,0.333333333333333,0.333333333333333,0.333333333333333,
0.333333333333333,0.333333333333333,0.333333333333333,0.333333333333333,
0.333333333333333,0.333333333333333,0.333333333333333,0.333333333333333,
0.333333333333333,0.333333333333333,0.333333333333333,0.333333333333333,
0.333333333333333,0.333333333333333,0.333333333333333,0.333333333333333,
0.333333333333333,0.333333333333333,0.333333333333333,0.333333333333333,
0.333333333333333,0.333333333333333,0.333333333333333,0.333333333333333,
0.333333333333333,0.333333333333333,0.333333333333333,0.333333333333333,
0.333333333333333,0.333333333333333,0.333333333333333,0.333333333333333,
0.333333333333333,0.333333333333333,0.333333333333333,0.333333333333333,
0.333333333333333,0.333333333333333,0.333333333333333,0.333333333333333,
0.333333333333333,0.333333333333333,0.333333333333333,0.333333333333333,
0.333333333333333,0.333333333333333,0.333333333333333,0.333333333333333,
0.333333333333333,0.333333333333333,0.333333333333333,0.333333333333333,
0.333333333333333,0.333333333333333,0.333333333333333,0.333333333333333,
0.333333333333333,0.333333333333333,0.333333333333333,0.333333333333333,
0.333333333333333,0.333333333333333,0.333333333333333,0.333333333333333,
0.333333333333333,0.333333333333333,0.333333333333333,0.333333333333333,
0.333333333333333,0.333333333333333,0.333333333333333,0.333333333333333,
0.333333333333333,0.333333333333333,0.333333333333333,0.333333333333333,
0.333333333333333,0.333333333333333,0.333333333333333,0.333333333333333,
0.333333333333333,0.333333333333333,0.333333333333333,0.333333333333333,
0.333333333333333,0.333333333333333,0.333333333333333,0.333333333333333,
0.333333333333333,0.333333333333333,0.333333333333333,0.333333333333333,
0.333333333333333,0.333333333333333),(1.,1.,1.,1.,1.,1.,1.,1.,1.,1.,1.,
1.,1.,1.,1.,1.,1.,1.,1.,1.,1.,1.,1.,1.,1.,1.,1.,1.,1.,1.,1.,1.,1.,1.,1.,
1.,1.,1.,1.,1.,1.,1.,1.,1.,1.,1.,1.,1.,1.,1.,1.,1.,1.,1.,1.,1.,1.,1.,1.,
1.,1.,1.,1.,1.,1.,1.,1.,1.,1.,1.,1.,1.,1.,1.,1.,1.,1.,1.,1.,1.,1.,1.,1.,
1.,1.,1.,1.,1.,1.,1.,1.,1.,1.,1.,1.,1.,1.,1.,1.)))
REPRESENTATION_ITEM('')
SURFACE()
);
#2311=(
BOUNDED_SURFACE()
B_SPLINE_SURFACE(3,3,((#364809,#364810,#364811,#364812,#364813,#364814,
#364815,#364816,#364817,#364818,#364819,#364820,#364821,#364822,#364823,
#364824,#364825,#364826,#364827,#364828,#364829,#364830,#364831,#364832,
#364833,#364834,#364835,#364836,#364837),(#364838,#364839,#364840,#364841,
#364842,#364843,#364844,#364845,#364846,#364847,#364848,#364849,#364850,
#364851,#364852,#364853,#364854,#364855,#364856,#364857,#364858,#364859,
#364860,#364861,#364862,#364863,#364864,#364865,#364866),(#364867,#364868,
#364869,#364870,#364871,#364872,#364873,#364874,#364875,#364876,#364877,
#364878,#364879,#364880,#364881,#364882,#364883,#364884,#364885,#364886,
#364887,#364888,#364889,#364890,#364891,#364892,#364893,#364894,#364895),
(#364896,#364897,#364898,#364899,#364900,#364901,#364902,#364903,#364904,
#364905,#364906,#364907,#364908,#364909,#364910,#364911,#364912,#364913,
#364914,#364915,#364916,#364917,#364918,#364919,#364920,#364921,#364922,
#364923,#364924),(#364925,#364926,#364927,#364928,#364929,#364930,#364931,
#364932,#364933,#364934,#364935,#364936,#364937,#364938,#364939,#364940,
#364941,#364942,#364943,#364944,#364945,#364946,#364947,#364948,#364949,
#364950,#364951,#364952,#364953),(#364954,#364955,#364956,#364957,#364958,
#364959,#364960,#364961,#364962,#364963,#364964,#364965,#364966,#364967,
#364968,#364969,#364970,#364971,#364972,#364973,#364974,#364975,#364976,
#364977,#364978,#364979,#364980,#364981,#364982),(#364983,#364984,#364985,
#364986,#364987,#364988,#364989,#364990,#364991,#364992,#364993,#364994,
#364995,#364996,#364997,#364998,#364999,#365000,#365001,#365002,#365003,
#365004,#365005,#365006,#365007,#365008,#365009,#365010,#365011)),
 .UNSPECIFIED.,.T.,.F.,.F.)
B_SPLINE_SURFACE_WITH_KNOTS((4,3,4),(4,1,1,1,1,1,1,1,1,1,1,1,1,1,1,1,1,
1,1,1,1,1,1,1,1,1,4),(0.,0.5,1.),(0.,0.0311997468912562,0.0625509890871527,
0.0938098447846757,0.1250568872711,0.166719530856106,0.208327420639085,
0.249977065870109,0.291629399375196,0.333238604634684,0.374889730322128,
0.41654078485731,0.458150415717,0.499801548056339,0.541452534012182,0.583062165488229,
0.624713366295055,0.666364346005318,0.707973557473876,0.749626035232519,
0.791275541260273,0.832883464833855,0.874546235186119,0.905793212129613,
0.937052173453026,0.968403278656631,1.),.UNSPECIFIED.)
GEOMETRIC_REPRESENTATION_ITEM()
RATIONAL_B_SPLINE_SURFACE(((1.,1.,1.,1.,1.,1.,1.,1.,1.,1.,1.,1.,1.,1.,1.,
1.,1.,1.,1.,1.,1.,1.,1.,1.,1.,1.,1.,1.,1.),(0.333333333333333,0.333333333333333,
0.333333333333333,0.333333333333333,0.333333333333333,0.333333333333333,
0.333333333333334,0.333333333333333,0.333333333333333,0.333333333333333,
0.333333333333333,0.333333333333333,0.333333333333333,0.333333333333334,
0.333333333333333,0.333333333333333,0.333333333333333,0.333333333333333,
0.333333333333333,0.333333333333333,0.333333333333333,0.333333333333333,
0.333333333333333,0.333333333333333,0.333333333333334,0.333333333333333,
0.333333333333333,0.333333333333333,0.333333333333333),(0.333333333333333,
0.333333333333333,0.333333333333333,0.333333333333333,0.333333333333333,
0.333333333333333,0.333333333333334,0.333333333333333,0.333333333333333,
0.333333333333333,0.333333333333333,0.333333333333333,0.333333333333333,
0.333333333333334,0.333333333333333,0.333333333333333,0.333333333333333,
0.333333333333333,0.333333333333333,0.333333333333333,0.333333333333333,
0.333333333333333,0.333333333333333,0.333333333333333,0.333333333333334,
0.333333333333333,0.333333333333333,0.333333333333333,0.333333333333333),
(1.,1.,1.,1.,1.,1.,1.,1.,1.,1.,1.,1.,1.,1.,1.,1.,1.,1.,1.,1.,1.,1.,1.,1.,
1.,1.,1.,1.,1.),(0.333333333333333,0.333333333333333,0.333333333333333,
0.333333333333333,0.333333333333333,0.333333333333333,0.333333333333334,
0.333333333333333,0.333333333333333,0.333333333333333,0.333333333333333,
0.333333333333333,0.333333333333333,0.333333333333334,0.333333333333333,
0.333333333333333,0.333333333333333,0.333333333333333,0.333333333333333,
0.333333333333333,0.333333333333333,0.333333333333333,0.333333333333333,
0.333333333333333,0.333333333333334,0.333333333333333,0.333333333333333,
0.333333333333333,0.333333333333333),(0.333333333333333,0.333333333333333,
0.333333333333333,0.333333333333333,0.333333333333333,0.333333333333333,
0.333333333333334,0.333333333333333,0.333333333333333,0.333333333333333,
0.333333333333333,0.333333333333333,0.333333333333333,0.333333333333334,
0.333333333333333,0.333333333333333,0.333333333333333,0.333333333333333,
0.333333333333333,0.333333333333333,0.333333333333333,0.333333333333333,
0.333333333333333,0.333333333333333,0.333333333333334,0.333333333333333,
0.333333333333333,0.333333333333333,0.333333333333333),(1.,1.,1.,1.,1.,
1.,1.,1.,1.,1.,1.,1.,1.,1.,1.,1.,1.,1.,1.,1.,1.,1.,1.,1.,1.,1.,1.,1.,1.)))
REPRESENTATION_ITEM('')
SURFACE()
);
#2312=(
BOUNDED_SURFACE()
B_SPLINE_SURFACE(3,3,((#365073,#365074,#365075,#365076,#365077,#365078,
#365079,#365080,#365081,#365082,#365083,#365084,#365085,#365086,#365087,
#365088,#365089,#365090,#365091,#365092,#365093,#365094,#365095,#365096,
#365097,#365098,#365099,#365100,#365101),(#365102,#365103,#365104,#365105,
#365106,#365107,#365108,#365109,#365110,#365111,#365112,#365113,#365114,
#365115,#365116,#365117,#365118,#365119,#365120,#365121,#365122,#365123,
#365124,#365125,#365126,#365127,#365128,#365129,#365130),(#365131,#365132,
#365133,#365134,#365135,#365136,#365137,#365138,#365139,#365140,#365141,
#365142,#365143,#365144,#365145,#365146,#365147,#365148,#365149,#365150,
#365151,#365152,#365153,#365154,#365155,#365156,#365157,#365158,#365159),
(#365160,#365161,#365162,#365163,#365164,#365165,#365166,#365167,#365168,
#365169,#365170,#365171,#365172,#365173,#365174,#365175,#365176,#365177,
#365178,#365179,#365180,#365181,#365182,#365183,#365184,#365185,#365186,
#365187,#365188),(#365189,#365190,#365191,#365192,#365193,#365194,#365195,
#365196,#365197,#365198,#365199,#365200,#365201,#365202,#365203,#365204,
#365205,#365206,#365207,#365208,#365209,#365210,#365211,#365212,#365213,
#365214,#365215,#365216,#365217),(#365218,#365219,#365220,#365221,#365222,
#365223,#365224,#365225,#365226,#365227,#365228,#365229,#365230,#365231,
#365232,#365233,#365234,#365235,#365236,#365237,#365238,#365239,#365240,
#365241,#365242,#365243,#365244,#365245,#365246),(#365247,#365248,#365249,
#365250,#365251,#365252,#365253,#365254,#365255,#365256,#365257,#365258,
#365259,#365260,#365261,#365262,#365263,#365264,#365265,#365266,#365267,
#365268,#365269,#365270,#365271,#365272,#365273,#365274,#365275)),
 .UNSPECIFIED.,.T.,.F.,.F.)
B_SPLINE_SURFACE_WITH_KNOTS((4,3,4),(4,1,1,1,1,1,1,1,1,1,1,1,1,1,1,1,1,
1,1,1,1,1,1,1,1,1,4),(0.,0.5,1.),(0.,0.0311997468912562,0.0625509890871527,
0.0938098447846757,0.1250568872711,0.166719530856106,0.208327420639085,
0.249977065870109,0.291629399375196,0.333238604634684,0.374889730322128,
0.41654078485731,0.458150415717,0.499801548056339,0.541452534012182,0.583062165488229,
0.624713366295055,0.666364346005318,0.707973557473876,0.749626035232519,
0.791275541260273,0.832883464833855,0.874546235186119,0.905793212129613,
0.937052173453026,0.968403278656631,1.),.UNSPECIFIED.)
GEOMETRIC_REPRESENTATION_ITEM()
RATIONAL_B_SPLINE_SURFACE(((1.,1.,1.,1.,1.,1.,1.,1.,1.,1.,1.,1.,1.,1.,1.,
1.,1.,1.,1.,1.,1.,1.,1.,1.,1.,1.,1.,1.,1.),(0.333333333333333,0.333333333333333,
0.333333333333333,0.333333333333333,0.333333333333333,0.333333333333333,
0.333333333333334,0.333333333333333,0.333333333333333,0.333333333333333,
0.333333333333333,0.333333333333333,0.333333333333333,0.333333333333334,
0.333333333333333,0.333333333333333,0.333333333333333,0.333333333333333,
0.333333333333333,0.333333333333333,0.333333333333333,0.333333333333333,
0.333333333333333,0.333333333333333,0.333333333333334,0.333333333333333,
0.333333333333333,0.333333333333333,0.333333333333333),(0.333333333333333,
0.333333333333333,0.333333333333333,0.333333333333333,0.333333333333333,
0.333333333333333,0.333333333333334,0.333333333333333,0.333333333333333,
0.333333333333333,0.333333333333333,0.333333333333333,0.333333333333333,
0.333333333333334,0.333333333333333,0.333333333333333,0.333333333333333,
0.333333333333333,0.333333333333333,0.333333333333333,0.333333333333333,
0.333333333333333,0.333333333333333,0.333333333333333,0.333333333333334,
0.333333333333333,0.333333333333333,0.333333333333333,0.333333333333333),
(1.,1.,1.,1.,1.,1.,1.,1.,1.,1.,1.,1.,1.,1.,1.,1.,1.,1.,1.,1.,1.,1.,1.,1.,
1.,1.,1.,1.,1.),(0.333333333333333,0.333333333333333,0.333333333333333,
0.333333333333333,0.333333333333333,0.333333333333333,0.333333333333334,
0.333333333333333,0.333333333333333,0.333333333333333,0.333333333333333,
0.333333333333333,0.333333333333333,0.333333333333334,0.333333333333333,
0.333333333333333,0.333333333333333,0.333333333333333,0.333333333333333,
0.333333333333333,0.333333333333333,0.333333333333333,0.333333333333333,
0.333333333333333,0.333333333333334,0.333333333333333,0.333333333333333,
0.333333333333333,0.333333333333333),(0.333333333333333,0.333333333333333,
0.333333333333333,0.333333333333333,0.333333333333333,0.333333333333333,
0.333333333333334,0.333333333333333,0.333333333333333,0.333333333333333,
0.333333333333333,0.333333333333333,0.333333333333333,0.333333333333334,
0.333333333333333,0.333333333333333,0.333333333333333,0.333333333333333,
0.333333333333333,0.333333333333333,0.333333333333333,0.333333333333333,
0.333333333333333,0.333333333333333,0.333333333333334,0.333333333333333,
0.333333333333333,0.333333333333333,0.333333333333333),(1.,1.,1.,1.,1.,
1.,1.,1.,1.,1.,1.,1.,1.,1.,1.,1.,1.,1.,1.,1.,1.,1.,1.,1.,1.,1.,1.,1.,1.)))
REPRESENTATION_ITEM('')
SURFACE()
);
#2313=(
BOUNDED_SURFACE()
B_SPLINE_SURFACE(3,3,((#365281,#365282,#365283,#365284,#365285,#365286,
#365287,#365288,#365289,#365290,#365291,#365292,#365293,#365294,#365295,
#365296,#365297,#365298,#365299,#365300,#365301,#365302,#365303,#365304,
#365305,#365306,#365307,#365308,#365309,#365310,#365311,#365312,#365313,
#365314,#365315,#365316,#365317,#365318,#365319,#365320,#365321,#365322,
#365323,#365324,#365325,#365326,#365327,#365328,#365329,#365330,#365331,
#365332,#365333,#365334,#365335,#365336,#365337,#365338,#365339,#365340,
#365341,#365342,#365343,#365344,#365345,#365346,#365347,#365348,#365349,
#365350,#365351,#365352,#365353,#365354,#365355,#365356,#365357,#365358,
#365359,#365360,#365361,#365362,#365363,#365364,#365365,#365366,#365367,
#365368,#365369,#365370,#365371,#365372,#365373,#365374,#365375,#365376,
#365377,#365378,#365379),(#365380,#365381,#365382,#365383,#365384,#365385,
#365386,#365387,#365388,#365389,#365390,#365391,#365392,#365393,#365394,
#365395,#365396,#365397,#365398,#365399,#365400,#365401,#365402,#365403,
#365404,#365405,#365406,#365407,#365408,#365409,#365410,#365411,#365412,
#365413,#365414,#365415,#365416,#365417,#365418,#365419,#365420,#365421,
#365422,#365423,#365424,#365425,#365426,#365427,#365428,#365429,#365430,
#365431,#365432,#365433,#365434,#365435,#365436,#365437,#365438,#365439,
#365440,#365441,#365442,#365443,#365444,#365445,#365446,#365447,#365448,
#365449,#365450,#365451,#365452,#365453,#365454,#365455,#365456,#365457,
#365458,#365459,#365460,#365461,#365462,#365463,#365464,#365465,#365466,
#365467,#365468,#365469,#365470,#365471,#365472,#365473,#365474,#365475,
#365476,#365477,#365478),(#365479,#365480,#365481,#365482,#365483,#365484,
#365485,#365486,#365487,#365488,#365489,#365490,#365491,#365492,#365493,
#365494,#365495,#365496,#365497,#365498,#365499,#365500,#365501,#365502,
#365503,#365504,#365505,#365506,#365507,#365508,#365509,#365510,#365511,
#365512,#365513,#365514,#365515,#365516,#365517,#365518,#365519,#365520,
#365521,#365522,#365523,#365524,#365525,#365526,#365527,#365528,#365529,
#365530,#365531,#365532,#365533,#365534,#365535,#365536,#365537,#365538,
#365539,#365540,#365541,#365542,#365543,#365544,#365545,#365546,#365547,
#365548,#365549,#365550,#365551,#365552,#365553,#365554,#365555,#365556,
#365557,#365558,#365559,#365560,#365561,#365562,#365563,#365564,#365565,
#365566,#365567,#365568,#365569,#365570,#365571,#365572,#365573,#365574,
#365575,#365576,#365577),(#365578,#365579,#365580,#365581,#365582,#365583,
#365584,#365585,#365586,#365587,#365588,#365589,#365590,#365591,#365592,
#365593,#365594,#365595,#365596,#365597,#365598,#365599,#365600,#365601,
#365602,#365603,#365604,#365605,#365606,#365607,#365608,#365609,#365610,
#365611,#365612,#365613,#365614,#365615,#365616,#365617,#365618,#365619,
#365620,#365621,#365622,#365623,#365624,#365625,#365626,#365627,#365628,
#365629,#365630,#365631,#365632,#365633,#365634,#365635,#365636,#365637,
#365638,#365639,#365640,#365641,#365642,#365643,#365644,#365645,#365646,
#365647,#365648,#365649,#365650,#365651,#365652,#365653,#365654,#365655,
#365656,#365657,#365658,#365659,#365660,#365661,#365662,#365663,#365664,
#365665,#365666,#365667,#365668,#365669,#365670,#365671,#365672,#365673,
#365674,#365675,#365676),(#365677,#365678,#365679,#365680,#365681,#365682,
#365683,#365684,#365685,#365686,#365687,#365688,#365689,#365690,#365691,
#365692,#365693,#365694,#365695,#365696,#365697,#365698,#365699,#365700,
#365701,#365702,#365703,#365704,#365705,#365706,#365707,#365708,#365709,
#365710,#365711,#365712,#365713,#365714,#365715,#365716,#365717,#365718,
#365719,#365720,#365721,#365722,#365723,#365724,#365725,#365726,#365727,
#365728,#365729,#365730,#365731,#365732,#365733,#365734,#365735,#365736,
#365737,#365738,#365739,#365740,#365741,#365742,#365743,#365744,#365745,
#365746,#365747,#365748,#365749,#365750,#365751,#365752,#365753,#365754,
#365755,#365756,#365757,#365758,#365759,#365760,#365761,#365762,#365763,
#365764,#365765,#365766,#365767,#365768,#365769,#365770,#365771,#365772,
#365773,#365774,#365775),(#365776,#365777,#365778,#365779,#365780,#365781,
#365782,#365783,#365784,#365785,#365786,#365787,#365788,#365789,#365790,
#365791,#365792,#365793,#365794,#365795,#365796,#365797,#365798,#365799,
#365800,#365801,#365802,#365803,#365804,#365805,#365806,#365807,#365808,
#365809,#365810,#365811,#365812,#365813,#365814,#365815,#365816,#365817,
#365818,#365819,#365820,#365821,#365822,#365823,#365824,#365825,#365826,
#365827,#365828,#365829,#365830,#365831,#365832,#365833,#365834,#365835,
#365836,#365837,#365838,#365839,#365840,#365841,#365842,#365843,#365844,
#365845,#365846,#365847,#365848,#365849,#365850,#365851,#365852,#365853,
#365854,#365855,#365856,#365857,#365858,#365859,#365860,#365861,#365862,
#365863,#365864,#365865,#365866,#365867,#365868,#365869,#365870,#365871,
#365872,#365873,#365874),(#365875,#365876,#365877,#365878,#365879,#365880,
#365881,#365882,#365883,#365884,#365885,#365886,#365887,#365888,#365889,
#365890,#365891,#365892,#365893,#365894,#365895,#365896,#365897,#365898,
#365899,#365900,#365901,#365902,#365903,#365904,#365905,#365906,#365907,
#365908,#365909,#365910,#365911,#365912,#365913,#365914,#365915,#365916,
#365917,#365918,#365919,#365920,#365921,#365922,#365923,#365924,#365925,
#365926,#365927,#365928,#365929,#365930,#365931,#365932,#365933,#365934,
#365935,#365936,#365937,#365938,#365939,#365940,#365941,#365942,#365943,
#365944,#365945,#365946,#365947,#365948,#365949,#365950,#365951,#365952,
#365953,#365954,#365955,#365956,#365957,#365958,#365959,#365960,#365961,
#365962,#365963,#365964,#365965,#365966,#365967,#365968,#365969,#365970,
#365971,#365972,#365973)),.UNSPECIFIED.,.T.,.F.,.F.)
B_SPLINE_SURFACE_WITH_KNOTS((4,3,4),(4,1,1,1,1,1,1,1,1,1,1,1,1,1,1,1,1,
1,1,1,1,1,1,1,1,1,1,1,1,1,1,1,1,1,1,1,1,1,1,1,1,1,1,1,1,1,1,1,1,1,1,1,1,
1,1,1,1,1,1,1,1,1,1,1,1,1,1,1,1,1,1,1,1,1,1,1,1,1,1,1,1,1,1,1,1,1,1,1,1,
1,1,1,1,1,1,1,4),(0.,0.5,1.),(0.,0.0104467457848562,0.0208697051534179,
0.0312830741812588,0.0417059245369557,0.0521151844214314,0.0625350854994869,
0.072955523619078,0.0833651614361216,0.093785355257659,0.104205506224069,
0.114615259182489,0.125035444608255,0.135455580151817,0.145865343296126,
0.156285526040368,0.166705661591602,0.177115425208493,0.187535607700786,
0.197955743339009,0.208365506953668,0.218785689432554,0.229205825080053,
0.239615588692213,0.250035771170918,0.260455906818944,0.270865670430874,
0.281285852909622,0.291705988557657,0.302115752169577,0.312535934648329,
0.322956070296362,0.333365833908282,0.343786016387035,0.354206152035067,
0.364615915646988,0.375036098125741,0.385456233773773,0.395865997385694,
0.406286179864446,0.416706315512479,0.427116079124399,0.437536261603152,
0.447956397251184,0.458366160863105,0.468786343341857,0.47920647898989,
0.48961624260181,0.500036425080563,0.510456560728595,0.520866324340516,
0.531286506819269,0.541706642467301,0.552116406079222,0.562536588557974,
0.572956724206007,0.583366487817927,0.59378667029668,0.604206805944712,
0.614616569556633,0.625036752035385,0.635456887683418,0.645866651295338,
0.656286833774091,0.666706969422123,0.677116733034044,0.687536915512797,
0.697957051160829,0.708366814772749,0.718786997251504,0.729207132899531,
0.739616896511461,0.750037078990207,0.760457214638192,0.770866978250353,
0.781287160728572,0.791707296376735,0.802117059991444,0.812537242460403,
0.822957378121908,0.833367141740239,0.843787324122365,0.85420746003523,
0.864617223206175,0.875037405580635,0.885457544175532,0.895867297492078,
0.906287495257385,0.916707642366043,0.927117283641006,0.937537767903979,
0.947957624414904,0.958366904818021,0.968789794286159,0.979203137018726,
0.989626134310512,1.),.UNSPECIFIED.)
GEOMETRIC_REPRESENTATION_ITEM()
RATIONAL_B_SPLINE_SURFACE(((1.,1.,1.,1.,1.,1.,1.,1.,1.,1.,1.,1.,1.,1.,1.,
1.,1.,1.,1.,1.,1.,1.,1.,1.,1.,1.,1.,1.,1.,1.,1.,1.,1.,1.,1.,1.,1.,1.,1.,
1.,1.,1.,1.,1.,1.,1.,1.,1.,1.,1.,1.,1.,1.,1.,1.,1.,1.,1.,1.,1.,1.,1.,1.,
1.,1.,1.,1.,1.,1.,1.,1.,1.,1.,1.,1.,1.,1.,1.,1.,1.,1.,1.,1.,1.,1.,1.,1.,
1.,1.,1.,1.,1.,1.,1.,1.,1.,1.,1.,1.),(0.333333333333333,0.333333333333333,
0.333333333333333,0.333333333333333,0.333333333333333,0.333333333333333,
0.333333333333333,0.333333333333333,0.333333333333333,0.333333333333333,
0.333333333333333,0.333333333333333,0.333333333333333,0.333333333333333,
0.333333333333333,0.333333333333333,0.333333333333333,0.333333333333333,
0.333333333333333,0.333333333333333,0.333333333333333,0.333333333333333,
0.333333333333333,0.333333333333333,0.333333333333333,0.333333333333333,
0.333333333333333,0.333333333333333,0.333333333333333,0.333333333333333,
0.333333333333333,0.333333333333333,0.333333333333333,0.333333333333333,
0.333333333333333,0.333333333333333,0.333333333333333,0.333333333333333,
0.333333333333333,0.333333333333333,0.333333333333333,0.333333333333333,
0.333333333333333,0.333333333333333,0.333333333333333,0.333333333333333,
0.333333333333333,0.333333333333333,0.333333333333333,0.333333333333333,
0.333333333333333,0.333333333333333,0.333333333333333,0.333333333333333,
0.333333333333333,0.333333333333333,0.333333333333333,0.333333333333333,
0.333333333333333,0.333333333333333,0.333333333333333,0.333333333333333,
0.333333333333333,0.333333333333333,0.333333333333333,0.333333333333333,
0.333333333333333,0.333333333333333,0.333333333333333,0.333333333333333,
0.333333333333333,0.333333333333333,0.333333333333333,0.333333333333333,
0.333333333333333,0.333333333333333,0.333333333333333,0.333333333333333,
0.333333333333333,0.333333333333333,0.333333333333333,0.333333333333333,
0.333333333333333,0.333333333333333,0.333333333333333,0.333333333333333,
0.333333333333333,0.333333333333333,0.333333333333333,0.333333333333333,
0.333333333333333,0.333333333333333,0.333333333333333,0.333333333333333,
0.333333333333333,0.333333333333333,0.333333333333333,0.333333333333333,
0.333333333333333),(0.333333333333333,0.333333333333333,0.333333333333333,
0.333333333333333,0.333333333333333,0.333333333333333,0.333333333333333,
0.333333333333333,0.333333333333333,0.333333333333333,0.333333333333333,
0.333333333333333,0.333333333333333,0.333333333333333,0.333333333333333,
0.333333333333333,0.333333333333333,0.333333333333333,0.333333333333333,
0.333333333333333,0.333333333333333,0.333333333333333,0.333333333333333,
0.333333333333333,0.333333333333333,0.333333333333333,0.333333333333333,
0.333333333333333,0.333333333333333,0.333333333333333,0.333333333333333,
0.333333333333333,0.333333333333333,0.333333333333333,0.333333333333333,
0.333333333333333,0.333333333333333,0.333333333333333,0.333333333333333,
0.333333333333333,0.333333333333333,0.333333333333333,0.333333333333333,
0.333333333333333,0.333333333333333,0.333333333333333,0.333333333333333,
0.333333333333333,0.333333333333333,0.333333333333333,0.333333333333333,
0.333333333333333,0.333333333333333,0.333333333333333,0.333333333333333,
0.333333333333333,0.333333333333333,0.333333333333333,0.333333333333333,
0.333333333333333,0.333333333333333,0.333333333333333,0.333333333333333,
0.333333333333333,0.333333333333333,0.333333333333333,0.333333333333333,
0.333333333333333,0.333333333333333,0.333333333333333,0.333333333333333,
0.333333333333333,0.333333333333333,0.333333333333333,0.333333333333333,
0.333333333333333,0.333333333333333,0.333333333333333,0.333333333333333,
0.333333333333333,0.333333333333333,0.333333333333333,0.333333333333333,
0.333333333333333,0.333333333333333,0.333333333333333,0.333333333333333,
0.333333333333333,0.333333333333333,0.333333333333333,0.333333333333333,
0.333333333333333,0.333333333333333,0.333333333333333,0.333333333333333,
0.333333333333333,0.333333333333333,0.333333333333333,0.333333333333333),
(1.,1.,1.,1.,1.,1.,1.,1.,1.,1.,1.,1.,1.,1.,1.,1.,1.,1.,1.,1.,1.,1.,1.,1.,
1.,1.,1.,1.,1.,1.,1.,1.,1.,1.,1.,1.,1.,1.,1.,1.,1.,1.,1.,1.,1.,1.,1.,1.,
1.,1.,1.,1.,1.,1.,1.,1.,1.,1.,1.,1.,1.,1.,1.,1.,1.,1.,1.,1.,1.,1.,1.,1.,
1.,1.,1.,1.,1.,1.,1.,1.,1.,1.,1.,1.,1.,1.,1.,1.,1.,1.,1.,1.,1.,1.,1.,1.,
1.,1.,1.),(0.333333333333333,0.333333333333333,0.333333333333333,0.333333333333333,
0.333333333333333,0.333333333333333,0.333333333333333,0.333333333333333,
0.333333333333333,0.333333333333333,0.333333333333333,0.333333333333333,
0.333333333333333,0.333333333333333,0.333333333333333,0.333333333333333,
0.333333333333333,0.333333333333333,0.333333333333333,0.333333333333333,
0.333333333333333,0.333333333333333,0.333333333333333,0.333333333333333,
0.333333333333333,0.333333333333333,0.333333333333333,0.333333333333333,
0.333333333333333,0.333333333333333,0.333333333333333,0.333333333333333,
0.333333333333333,0.333333333333333,0.333333333333333,0.333333333333333,
0.333333333333333,0.333333333333333,0.333333333333333,0.333333333333333,
0.333333333333333,0.333333333333333,0.333333333333333,0.333333333333333,
0.333333333333333,0.333333333333333,0.333333333333333,0.333333333333333,
0.333333333333333,0.333333333333333,0.333333333333333,0.333333333333333,
0.333333333333333,0.333333333333333,0.333333333333333,0.333333333333333,
0.333333333333333,0.333333333333333,0.333333333333333,0.333333333333333,
0.333333333333333,0.333333333333333,0.333333333333333,0.333333333333333,
0.333333333333333,0.333333333333333,0.333333333333333,0.333333333333333,
0.333333333333333,0.333333333333333,0.333333333333333,0.333333333333333,
0.333333333333333,0.333333333333333,0.333333333333333,0.333333333333333,
0.333333333333333,0.333333333333333,0.333333333333333,0.333333333333333,
0.333333333333333,0.333333333333333,0.333333333333333,0.333333333333333,
0.333333333333333,0.333333333333333,0.333333333333333,0.333333333333333,
0.333333333333333,0.333333333333333,0.333333333333333,0.333333333333333,
0.333333333333333,0.333333333333333,0.333333333333333,0.333333333333333,
0.333333333333333,0.333333333333333,0.333333333333333),(0.333333333333333,
0.333333333333333,0.333333333333333,0.333333333333333,0.333333333333333,
0.333333333333333,0.333333333333333,0.333333333333333,0.333333333333333,
0.333333333333333,0.333333333333333,0.333333333333333,0.333333333333333,
0.333333333333333,0.333333333333333,0.333333333333333,0.333333333333333,
0.333333333333333,0.333333333333333,0.333333333333333,0.333333333333333,
0.333333333333333,0.333333333333333,0.333333333333333,0.333333333333333,
0.333333333333333,0.333333333333333,0.333333333333333,0.333333333333333,
0.333333333333333,0.333333333333333,0.333333333333333,0.333333333333333,
0.333333333333333,0.333333333333333,0.333333333333333,0.333333333333333,
0.333333333333333,0.333333333333333,0.333333333333333,0.333333333333333,
0.333333333333333,0.333333333333333,0.333333333333333,0.333333333333333,
0.333333333333333,0.333333333333333,0.333333333333333,0.333333333333333,
0.333333333333333,0.333333333333333,0.333333333333333,0.333333333333333,
0.333333333333333,0.333333333333333,0.333333333333333,0.333333333333333,
0.333333333333333,0.333333333333333,0.333333333333333,0.333333333333333,
0.333333333333333,0.333333333333333,0.333333333333333,0.333333333333333,
0.333333333333333,0.333333333333333,0.333333333333333,0.333333333333333,
0.333333333333333,0.333333333333333,0.333333333333333,0.333333333333333,
0.333333333333333,0.333333333333333,0.333333333333333,0.333333333333333,
0.333333333333333,0.333333333333333,0.333333333333333,0.333333333333333,
0.333333333333333,0.333333333333333,0.333333333333333,0.333333333333333,
0.333333333333333,0.333333333333333,0.333333333333333,0.333333333333333,
0.333333333333333,0.333333333333333,0.333333333333333,0.333333333333333,
0.333333333333333,0.333333333333333,0.333333333333333,0.333333333333333,
0.333333333333333,0.333333333333333),(1.,1.,1.,1.,1.,1.,1.,1.,1.,1.,1.,
1.,1.,1.,1.,1.,1.,1.,1.,1.,1.,1.,1.,1.,1.,1.,1.,1.,1.,1.,1.,1.,1.,1.,1.,
1.,1.,1.,1.,1.,1.,1.,1.,1.,1.,1.,1.,1.,1.,1.,1.,1.,1.,1.,1.,1.,1.,1.,1.,
1.,1.,1.,1.,1.,1.,1.,1.,1.,1.,1.,1.,1.,1.,1.,1.,1.,1.,1.,1.,1.,1.,1.,1.,
1.,1.,1.,1.,1.,1.,1.,1.,1.,1.,1.,1.,1.,1.,1.,1.)))
REPRESENTATION_ITEM('')
SURFACE()
);
#2314=(
BOUNDED_SURFACE()
B_SPLINE_SURFACE(3,3,((#365979,#365980,#365981,#365982,#365983,#365984,
#365985,#365986,#365987,#365988,#365989,#365990,#365991,#365992,#365993,
#365994,#365995,#365996,#365997,#365998,#365999,#366000,#366001,#366002,
#366003,#366004,#366005,#366006,#366007),(#366008,#366009,#366010,#366011,
#366012,#366013,#366014,#366015,#366016,#366017,#366018,#366019,#366020,
#366021,#366022,#366023,#366024,#366025,#366026,#366027,#366028,#366029,
#366030,#366031,#366032,#366033,#366034,#366035,#366036),(#366037,#366038,
#366039,#366040,#366041,#366042,#366043,#366044,#366045,#366046,#366047,
#366048,#366049,#366050,#366051,#366052,#366053,#366054,#366055,#366056,
#366057,#366058,#366059,#366060,#366061,#366062,#366063,#366064,#366065),
(#366066,#366067,#366068,#366069,#366070,#366071,#366072,#366073,#366074,
#366075,#366076,#366077,#366078,#366079,#366080,#366081,#366082,#366083,
#366084,#366085,#366086,#366087,#366088,#366089,#366090,#366091,#366092,
#366093,#366094),(#366095,#366096,#366097,#366098,#366099,#366100,#366101,
#366102,#366103,#366104,#366105,#366106,#366107,#366108,#366109,#366110,
#366111,#366112,#366113,#366114,#366115,#366116,#366117,#366118,#366119,
#366120,#366121,#366122,#366123),(#366124,#366125,#366126,#366127,#366128,
#366129,#366130,#366131,#366132,#366133,#366134,#366135,#366136,#366137,
#366138,#366139,#366140,#366141,#366142,#366143,#366144,#366145,#366146,
#366147,#366148,#366149,#366150,#366151,#366152),(#366153,#366154,#366155,
#366156,#366157,#366158,#366159,#366160,#366161,#366162,#366163,#366164,
#366165,#366166,#366167,#366168,#366169,#366170,#366171,#366172,#366173,
#366174,#366175,#366176,#366177,#366178,#366179,#366180,#366181)),
 .UNSPECIFIED.,.T.,.F.,.F.)
B_SPLINE_SURFACE_WITH_KNOTS((4,3,4),(4,1,1,1,1,1,1,1,1,1,1,1,1,1,1,1,1,
1,1,1,1,1,1,1,1,1,4),(0.,0.5,1.),(0.,0.0310703336761616,0.0624385278003938,
0.0937144048499659,0.124978469089869,0.166663774179581,0.208294236860357,
0.249966520356582,0.291641529650434,0.3332733240007,0.374947073344913,0.416620808022619,
0.458253030541402,0.499926784452264,0.54160045129851,0.583232674441905,
0.624906496125386,0.666580158626562,0.708211959489969,0.749887054558503,
0.791559255246094,0.833189756589646,0.87487513422873,0.906139159779086,
0.937415106668169,0.968783217665703,1.),.UNSPECIFIED.)
GEOMETRIC_REPRESENTATION_ITEM()
RATIONAL_B_SPLINE_SURFACE(((1.,1.,1.,1.,1.,1.,1.,1.,1.,1.,1.,1.,1.,1.,1.,
1.,1.,1.,1.,1.,1.,1.,1.,1.,1.,1.,1.,1.,1.),(0.333333333333333,0.333333333333333,
0.333333333333334,0.333333333333333,0.333333333333333,0.333333333333333,
0.333333333333333,0.333333333333333,0.333333333333333,0.333333333333333,
0.333333333333333,0.333333333333333,0.333333333333334,0.333333333333333,
0.333333333333333,0.333333333333333,0.333333333333333,0.333333333333333,
0.333333333333333,0.333333333333333,0.333333333333333,0.333333333333333,
0.333333333333333,0.333333333333333,0.333333333333333,0.333333333333333,
0.333333333333333,0.333333333333333,0.333333333333333),(0.333333333333333,
0.333333333333333,0.333333333333334,0.333333333333333,0.333333333333333,
0.333333333333333,0.333333333333333,0.333333333333333,0.333333333333333,
0.333333333333333,0.333333333333333,0.333333333333333,0.333333333333334,
0.333333333333333,0.333333333333333,0.333333333333333,0.333333333333333,
0.333333333333333,0.333333333333333,0.333333333333333,0.333333333333333,
0.333333333333333,0.333333333333333,0.333333333333333,0.333333333333333,
0.333333333333333,0.333333333333333,0.333333333333333,0.333333333333333),
(1.,1.,1.,1.,1.,1.,1.,1.,1.,1.,1.,1.,1.,1.,1.,1.,1.,1.,1.,1.,1.,1.,1.,1.,
1.,1.,1.,1.,1.),(0.333333333333333,0.333333333333333,0.333333333333334,
0.333333333333333,0.333333333333333,0.333333333333333,0.333333333333333,
0.333333333333333,0.333333333333333,0.333333333333333,0.333333333333333,
0.333333333333333,0.333333333333334,0.333333333333333,0.333333333333333,
0.333333333333333,0.333333333333333,0.333333333333333,0.333333333333333,
0.333333333333333,0.333333333333333,0.333333333333333,0.333333333333333,
0.333333333333333,0.333333333333333,0.333333333333333,0.333333333333333,
0.333333333333333,0.333333333333333),(0.333333333333333,0.333333333333333,
0.333333333333334,0.333333333333333,0.333333333333333,0.333333333333333,
0.333333333333333,0.333333333333333,0.333333333333333,0.333333333333333,
0.333333333333333,0.333333333333333,0.333333333333334,0.333333333333333,
0.333333333333333,0.333333333333333,0.333333333333333,0.333333333333333,
0.333333333333333,0.333333333333333,0.333333333333333,0.333333333333333,
0.333333333333333,0.333333333333333,0.333333333333333,0.333333333333333,
0.333333333333333,0.333333333333333,0.333333333333333),(1.,1.,1.,1.,1.,
1.,1.,1.,1.,1.,1.,1.,1.,1.,1.,1.,1.,1.,1.,1.,1.,1.,1.,1.,1.,1.,1.,1.,1.)))
REPRESENTATION_ITEM('')
SURFACE()
);
#2315=(
BOUNDED_SURFACE()
B_SPLINE_SURFACE(1,2,((#368140,#368141,#368142,#368143,#368144,#368145,
#368146,#368147,#368148,#368149,#368150,#368151,#368152,#368153,#368154,
#368155,#368156,#368157,#368158,#368159,#368160,#368161,#368162,#368163,
#368164,#368165,#368166,#368167,#368168,#368169,#368170,#368171,#368172,
#368173,#368174,#368175,#368176,#368177,#368178,#368179,#368180,#368181,
#368182,#368183,#368184,#368185,#368186,#368187,#368188,#368189,#368190,
#368191,#368192,#368193,#368194,#368195,#368196,#368197,#368198,#368199,
#368200,#368201,#368202,#368203,#368204,#368205,#368206,#368207,#368208,
#368209,#368210,#368211,#368212,#368213,#368214,#368215,#368216,#368217,
#368218,#368219,#368220,#368221,#368222,#368223,#368224,#368225,#368226,
#368227,#368228,#368229,#368230,#368231,#368232,#368233,#368234,#368235,
#368236,#368237,#368238,#368239,#368240,#368241,#368242,#368243,#368244,
#368245,#368246,#368247,#368248,#368249,#368250,#368251,#368252,#368253,
#368254,#368255,#368256,#368257,#368258,#368259,#368260,#368261,#368262,
#368263,#368264,#368265,#368266,#368267,#368268,#368269,#368270,#368271,
#368272,#368273,#368274,#368275,#368276,#368277,#368278,#368279,#368280,
#368281,#368282,#368283,#368284,#368285,#368286,#368287,#368288,#368289,
#368290,#368291,#368292,#368293,#368294,#368295,#368296,#368297,#368298,
#368299,#368300,#368301,#368302,#368303,#368304,#368305,#368306,#368307,
#368308,#368309,#368310,#368311,#368312,#368313,#368314,#368315,#368316,
#368317,#368318,#368319,#368320,#368321,#368322,#368323,#368324,#368325,
#368326,#368327,#368328,#368329,#368330,#368331,#368332,#368333,#368334,
#368335,#368336,#368337,#368338,#368339,#368340,#368341,#368342,#368343,
#368344),(#368345,#368346,#368347,#368348,#368349,#368350,#368351,#368352,
#368353,#368354,#368355,#368356,#368357,#368358,#368359,#368360,#368361,
#368362,#368363,#368364,#368365,#368366,#368367,#368368,#368369,#368370,
#368371,#368372,#368373,#368374,#368375,#368376,#368377,#368378,#368379,
#368380,#368381,#368382,#368383,#368384,#368385,#368386,#368387,#368388,
#368389,#368390,#368391,#368392,#368393,#368394,#368395,#368396,#368397,
#368398,#368399,#368400,#368401,#368402,#368403,#368404,#368405,#368406,
#368407,#368408,#368409,#368410,#368411,#368412,#368413,#368414,#368415,
#368416,#368417,#368418,#368419,#368420,#368421,#368422,#368423,#368424,
#368425,#368426,#368427,#368428,#368429,#368430,#368431,#368432,#368433,
#368434,#368435,#368436,#368437,#368438,#368439,#368440,#368441,#368442,
#368443,#368444,#368445,#368446,#368447,#368448,#368449,#368450,#368451,
#368452,#368453,#368454,#368455,#368456,#368457,#368458,#368459,#368460,
#368461,#368462,#368463,#368464,#368465,#368466,#368467,#368468,#368469,
#368470,#368471,#368472,#368473,#368474,#368475,#368476,#368477,#368478,
#368479,#368480,#368481,#368482,#368483,#368484,#368485,#368486,#368487,
#368488,#368489,#368490,#368491,#368492,#368493,#368494,#368495,#368496,
#368497,#368498,#368499,#368500,#368501,#368502,#368503,#368504,#368505,
#368506,#368507,#368508,#368509,#368510,#368511,#368512,#368513,#368514,
#368515,#368516,#368517,#368518,#368519,#368520,#368521,#368522,#368523,
#368524,#368525,#368526,#368527,#368528,#368529,#368530,#368531,#368532,
#368533,#368534,#368535,#368536,#368537,#368538,#368539,#368540,#368541,
#368542,#368543,#368544,#368545,#368546,#368547,#368548,#368549)),
 .UNSPECIFIED.,.F.,.F.,.F.)
B_SPLINE_SURFACE_WITH_KNOTS((2,2),(3,2,2,2,2,2,2,2,2,2,2,2,2,2,2,2,2,2,
2,2,2,2,2,2,2,2,2,2,2,2,2,2,2,2,2,2,2,2,2,2,2,2,2,2,2,2,2,2,2,2,2,2,2,2,
2,2,2,2,2,2,2,2,2,2,2,2,2,2,2,2,2,2,2,2,2,2,2,2,2,2,2,2,2,2,2,2,2,2,2,2,
2,2,2,2,2,2,2,2,2,2,2,2,3),(0.,1.),(0.,0.00980392156862745,0.0196078431372549,
0.0294117647058824,0.0392156862745098,0.0490196078431373,0.0588235294117647,
0.0686274509803922,0.0784313725490196,0.0882352941176471,0.0980392156862745,
0.107843137254902,0.117647058823529,0.127450980392157,0.137254901960784,
0.147058823529412,0.156862745098039,0.166666666666667,0.176470588235294,
0.186274509803922,0.196078431372549,0.205882352941176,0.215686274509804,
0.225490196078431,0.235294117647059,0.245098039215686,0.254901960784314,
0.264705882352941,0.274509803921569,0.284313725490196,0.294117647058824,
0.303921568627451,0.313725490196078,0.323529411764706,0.333333333333333,
0.343137254901961,0.352941176470588,0.362745098039216,0.372549019607843,
0.382352941176471,0.392156862745098,0.401960784313726,0.411764705882353,
0.42156862745098,0.431372549019608,0.441176470588235,0.450980392156863,
0.46078431372549,0.470588235294118,0.480392156862745,0.490196078431373,
0.5,0.509803921568627,0.519607843137255,0.529411764705882,0.53921568627451,
0.549019607843137,0.558823529411765,0.568627450980392,0.57843137254902,
0.588235294117647,0.598039215686274,0.607843137254902,0.617647058823529,
0.627450980392157,0.637254901960784,0.647058823529412,0.656862745098039,
0.666666666666667,0.676470588235294,0.686274509803922,0.696078431372549,
0.705882352941177,0.715686274509804,0.725490196078431,0.735294117647059,
0.745098039215686,0.754901960784314,0.764705882352941,0.774509803921569,
0.784313725490196,0.794117647058823,0.803921568627451,0.813725490196078,
0.823529411764706,0.833333333333333,0.843137254901961,0.852941176470588,
0.862745098039216,0.872549019607843,0.882352941176471,0.892156862745098,
0.901960784313726,0.911764705882353,0.92156862745098,0.931372549019608,
0.941176470588235,0.950980392156863,0.96078431372549,0.970588235294118,
0.980392156862745,0.990196078431373,1.),.UNSPECIFIED.)
GEOMETRIC_REPRESENTATION_ITEM()
RATIONAL_B_SPLINE_SURFACE(((1.,0.866025403784439,1.,0.866025403784439,1.,
0.866025403784439,1.,0.866025403784439,1.,0.866025403784439,1.,0.866025403784439,
1.,0.866025403784439,1.,0.866025403784439,1.,0.866025403784439,1.,0.866025403784439,
1.,0.866025403784439,1.,0.866025403784439,1.,0.866025403784439,1.,0.866025403784439,
1.,0.866025403784439,1.,0.866025403784439,1.,0.866025403784439,1.,0.866025403784439,
1.,0.866025403784439,1.,0.866025403784439,1.,0.866025403784439,1.,0.866025403784439,
1.,0.866025403784439,1.,0.866025403784439,1.,0.866025403784439,1.,0.866025403784439,
1.,0.866025403784439,1.,0.866025403784439,1.,0.866025403784439,1.,0.866025403784439,
1.,0.866025403784439,1.,0.866025403784439,1.,0.866025403784439,1.,0.866025403784439,
1.,0.866025403784439,1.,0.866025403784439,1.,0.866025403784439,1.,0.866025403784439,
1.,0.866025403784439,1.,0.866025403784439,1.,0.866025403784439,1.,0.866025403784439,
1.,0.866025403784439,1.,0.866025403784439,1.,0.866025403784439,1.,0.866025403784439,
1.,0.866025403784439,1.,0.866025403784439,1.,0.866025403784439,1.,0.866025403784439,
1.,0.866025403784439,1.,0.866025403784439,1.,0.866025403784439,1.,0.866025403784439,
1.,0.866025403784439,1.,0.866025403784439,1.,0.866025403784439,1.,0.866025403784439,
1.,0.866025403784439,1.,0.866025403784439,1.,0.866025403784439,1.,0.866025403784439,
1.,0.866025403784439,1.,0.866025403784439,1.,0.866025403784439,1.,0.866025403784439,
1.,0.866025403784439,1.,0.866025403784439,1.,0.866025403784439,1.,0.866025403784439,
1.,0.866025403784439,1.,0.866025403784439,1.,0.866025403784439,1.,0.866025403784439,
1.,0.866025403784439,1.,0.866025403784439,1.,0.866025403784439,1.,0.866025403784439,
1.,0.866025403784439,1.,0.866025403784439,1.,0.866025403784439,1.,0.866025403784439,
1.,0.866025403784439,1.,0.866025403784439,1.,0.866025403784439,1.,0.866025403784439,
1.,0.866025403784439,1.,0.866025403784439,1.,0.866025403784439,1.,0.866025403784439,
1.,0.866025403784439,1.,0.866025403784439,1.,0.866025403784439,1.,0.866025403784439,
1.,0.866025403784439,1.,0.866025403784439,1.,0.866025403784439,1.,0.866025403784439,
1.,0.866025403784439,1.,0.866025403784439,1.,0.866025403784439,1.,0.866025403784439,
1.),(1.,0.866025403784439,1.,0.866025403784439,1.,0.866025403784439,1.,
0.866025403784439,1.,0.866025403784439,1.,0.866025403784439,1.,0.866025403784439,
1.,0.866025403784439,1.,0.866025403784439,1.,0.866025403784439,1.,0.866025403784439,
1.,0.866025403784439,1.,0.866025403784439,1.,0.866025403784439,1.,0.866025403784439,
1.,0.866025403784439,1.,0.866025403784439,1.,0.866025403784439,1.,0.866025403784439,
1.,0.866025403784439,1.,0.866025403784439,1.,0.866025403784439,1.,0.866025403784439,
1.,0.866025403784439,1.,0.866025403784439,1.,0.866025403784439,1.,0.866025403784439,
1.,0.866025403784439,1.,0.866025403784439,1.,0.866025403784439,1.,0.866025403784439,
1.,0.866025403784439,1.,0.866025403784439,1.,0.866025403784439,1.,0.866025403784439,
1.,0.866025403784439,1.,0.866025403784439,1.,0.866025403784439,1.,0.866025403784439,
1.,0.866025403784439,1.,0.866025403784439,1.,0.866025403784439,1.,0.866025403784439,
1.,0.866025403784439,1.,0.866025403784439,1.,0.866025403784439,1.,0.866025403784439,
1.,0.866025403784439,1.,0.866025403784439,1.,0.866025403784439,1.,0.866025403784439,
1.,0.866025403784439,1.,0.866025403784439,1.,0.866025403784439,1.,0.866025403784439,
1.,0.866025403784439,1.,0.866025403784439,1.,0.866025403784439,1.,0.866025403784439,
1.,0.866025403784439,1.,0.866025403784439,1.,0.866025403784439,1.,0.866025403784439,
1.,0.866025403784439,1.,0.866025403784439,1.,0.866025403784439,1.,0.866025403784439,
1.,0.866025403784439,1.,0.866025403784439,1.,0.866025403784439,1.,0.866025403784439,
1.,0.866025403784439,1.,0.866025403784439,1.,0.866025403784439,1.,0.866025403784439,
1.,0.866025403784439,1.,0.866025403784439,1.,0.866025403784439,1.,0.866025403784439,
1.,0.866025403784439,1.,0.866025403784439,1.,0.866025403784439,1.,0.866025403784439,
1.,0.866025403784439,1.,0.866025403784439,1.,0.866025403784439,1.,0.866025403784439,
1.,0.866025403784439,1.,0.866025403784439,1.,0.866025403784439,1.,0.866025403784439,
1.,0.866025403784439,1.,0.866025403784439,1.,0.866025403784439,1.,0.866025403784439,
1.,0.866025403784439,1.,0.866025403784439,1.,0.866025403784439,1.,0.866025403784439,
1.,0.866025403784439,1.,0.866025403784439,1.,0.866025403784439,1.)))
REPRESENTATION_ITEM('')
SURFACE()
);
#2316=(
BOUNDED_SURFACE()
B_SPLINE_SURFACE(1,2,((#368577,#368578,#368579,#368580,#368581,#368582,
#368583,#368584,#368585,#368586,#368587,#368588,#368589,#368590,#368591,
#368592,#368593,#368594,#368595,#368596,#368597,#368598,#368599,#368600,
#368601,#368602,#368603,#368604,#368605,#368606,#368607,#368608,#368609,
#368610,#368611,#368612,#368613,#368614,#368615,#368616,#368617,#368618,
#368619,#368620,#368621,#368622,#368623,#368624,#368625,#368626,#368627,
#368628,#368629,#368630,#368631,#368632,#368633,#368634,#368635,#368636,
#368637,#368638,#368639,#368640,#368641,#368642,#368643,#368644,#368645,
#368646,#368647,#368648,#368649,#368650,#368651,#368652,#368653,#368654,
#368655,#368656,#368657,#368658,#368659,#368660,#368661,#368662,#368663,
#368664,#368665,#368666,#368667,#368668,#368669,#368670,#368671,#368672,
#368673,#368674,#368675,#368676,#368677,#368678,#368679,#368680,#368681,
#368682,#368683,#368684,#368685,#368686,#368687,#368688,#368689,#368690,
#368691,#368692,#368693,#368694,#368695,#368696,#368697,#368698,#368699,
#368700,#368701,#368702,#368703,#368704,#368705,#368706,#368707,#368708,
#368709,#368710,#368711,#368712,#368713,#368714,#368715,#368716,#368717,
#368718,#368719,#368720,#368721,#368722,#368723,#368724,#368725,#368726,
#368727,#368728,#368729,#368730,#368731,#368732,#368733,#368734,#368735,
#368736,#368737,#368738,#368739,#368740,#368741,#368742,#368743,#368744,
#368745,#368746,#368747,#368748,#368749,#368750,#368751,#368752,#368753,
#368754,#368755,#368756,#368757,#368758,#368759,#368760,#368761,#368762,
#368763,#368764,#368765,#368766,#368767,#368768,#368769,#368770,#368771,
#368772,#368773,#368774,#368775,#368776,#368777,#368778,#368779,#368780,
#368781),(#368782,#368783,#368784,#368785,#368786,#368787,#368788,#368789,
#368790,#368791,#368792,#368793,#368794,#368795,#368796,#368797,#368798,
#368799,#368800,#368801,#368802,#368803,#368804,#368805,#368806,#368807,
#368808,#368809,#368810,#368811,#368812,#368813,#368814,#368815,#368816,
#368817,#368818,#368819,#368820,#368821,#368822,#368823,#368824,#368825,
#368826,#368827,#368828,#368829,#368830,#368831,#368832,#368833,#368834,
#368835,#368836,#368837,#368838,#368839,#368840,#368841,#368842,#368843,
#368844,#368845,#368846,#368847,#368848,#368849,#368850,#368851,#368852,
#368853,#368854,#368855,#368856,#368857,#368858,#368859,#368860,#368861,
#368862,#368863,#368864,#368865,#368866,#368867,#368868,#368869,#368870,
#368871,#368872,#368873,#368874,#368875,#368876,#368877,#368878,#368879,
#368880,#368881,#368882,#368883,#368884,#368885,#368886,#368887,#368888,
#368889,#368890,#368891,#368892,#368893,#368894,#368895,#368896,#368897,
#368898,#368899,#368900,#368901,#368902,#368903,#368904,#368905,#368906,
#368907,#368908,#368909,#368910,#368911,#368912,#368913,#368914,#368915,
#368916,#368917,#368918,#368919,#368920,#368921,#368922,#368923,#368924,
#368925,#368926,#368927,#368928,#368929,#368930,#368931,#368932,#368933,
#368934,#368935,#368936,#368937,#368938,#368939,#368940,#368941,#368942,
#368943,#368944,#368945,#368946,#368947,#368948,#368949,#368950,#368951,
#368952,#368953,#368954,#368955,#368956,#368957,#368958,#368959,#368960,
#368961,#368962,#368963,#368964,#368965,#368966,#368967,#368968,#368969,
#368970,#368971,#368972,#368973,#368974,#368975,#368976,#368977,#368978,
#368979,#368980,#368981,#368982,#368983,#368984,#368985,#368986)),
 .UNSPECIFIED.,.F.,.F.,.F.)
B_SPLINE_SURFACE_WITH_KNOTS((2,2),(3,2,2,2,2,2,2,2,2,2,2,2,2,2,2,2,2,2,
2,2,2,2,2,2,2,2,2,2,2,2,2,2,2,2,2,2,2,2,2,2,2,2,2,2,2,2,2,2,2,2,2,2,2,2,
2,2,2,2,2,2,2,2,2,2,2,2,2,2,2,2,2,2,2,2,2,2,2,2,2,2,2,2,2,2,2,2,2,2,2,2,
2,2,2,2,2,2,2,2,2,2,2,2,3),(-2.36351427691722E-5,1.),(0.,0.00980392156862745,
0.0196078431372549,0.0294117647058824,0.0392156862745098,0.0490196078431373,
0.0588235294117647,0.0686274509803922,0.0784313725490196,0.0882352941176471,
0.0980392156862745,0.107843137254902,0.117647058823529,0.127450980392157,
0.137254901960784,0.147058823529412,0.156862745098039,0.166666666666667,
0.176470588235294,0.186274509803922,0.196078431372549,0.205882352941176,
0.215686274509804,0.225490196078431,0.235294117647059,0.245098039215686,
0.254901960784314,0.264705882352941,0.274509803921569,0.284313725490196,
0.294117647058824,0.303921568627451,0.313725490196078,0.323529411764706,
0.333333333333333,0.343137254901961,0.352941176470588,0.362745098039216,
0.372549019607843,0.382352941176471,0.392156862745098,0.401960784313726,
0.411764705882353,0.42156862745098,0.431372549019608,0.441176470588235,
0.450980392156863,0.46078431372549,0.470588235294118,0.480392156862745,
0.490196078431373,0.5,0.509803921568627,0.519607843137255,0.529411764705882,
0.53921568627451,0.549019607843137,0.558823529411765,0.568627450980392,
0.57843137254902,0.588235294117647,0.598039215686274,0.607843137254902,
0.617647058823529,0.627450980392157,0.637254901960784,0.647058823529412,
0.656862745098039,0.666666666666667,0.676470588235294,0.686274509803922,
0.696078431372549,0.705882352941177,0.715686274509804,0.725490196078431,
0.735294117647059,0.745098039215686,0.754901960784314,0.764705882352941,
0.774509803921569,0.784313725490196,0.794117647058823,0.803921568627451,
0.813725490196078,0.823529411764706,0.833333333333333,0.843137254901961,
0.852941176470588,0.862745098039216,0.872549019607843,0.882352941176471,
0.892156862745098,0.901960784313726,0.911764705882353,0.92156862745098,
0.931372549019608,0.941176470588235,0.950980392156863,0.96078431372549,
0.970588235294118,0.980392156862745,0.990196078431373,1.),.UNSPECIFIED.)
GEOMETRIC_REPRESENTATION_ITEM()
RATIONAL_B_SPLINE_SURFACE(((1.,0.866025403784439,1.,0.866025403784439,1.,
0.866025403784439,1.,0.866025403784439,1.,0.866025403784439,1.,0.866025403784439,
1.,0.866025403784439,1.,0.866025403784439,1.,0.866025403784439,1.,0.866025403784439,
1.,0.866025403784439,1.,0.866025403784439,1.,0.866025403784439,1.,0.866025403784439,
1.,0.866025403784439,1.,0.866025403784439,1.,0.866025403784439,1.,0.866025403784439,
1.,0.866025403784439,1.,0.866025403784439,1.,0.866025403784439,1.,0.866025403784439,
1.,0.866025403784439,1.,0.866025403784439,1.,0.866025403784439,1.,0.866025403784439,
1.,0.866025403784439,1.,0.866025403784439,1.,0.866025403784439,1.,0.866025403784439,
1.,0.866025403784439,1.,0.866025403784439,1.,0.866025403784439,1.,0.866025403784439,
1.,0.866025403784439,1.,0.866025403784439,1.,0.866025403784439,1.,0.866025403784439,
1.,0.866025403784439,1.,0.866025403784439,1.,0.866025403784439,1.,0.866025403784439,
1.,0.866025403784439,1.,0.866025403784439,1.,0.866025403784439,1.,0.866025403784439,
1.,0.866025403784439,1.,0.866025403784439,1.,0.866025403784439,1.,0.866025403784439,
1.,0.866025403784439,1.,0.866025403784439,1.,0.866025403784439,1.,0.866025403784439,
1.,0.866025403784439,1.,0.866025403784439,1.,0.866025403784439,1.,0.866025403784439,
1.,0.866025403784439,1.,0.866025403784439,1.,0.866025403784439,1.,0.866025403784439,
1.,0.866025403784439,1.,0.866025403784439,1.,0.866025403784439,1.,0.866025403784439,
1.,0.866025403784439,1.,0.866025403784439,1.,0.866025403784439,1.,0.866025403784439,
1.,0.866025403784439,1.,0.866025403784439,1.,0.866025403784439,1.,0.866025403784439,
1.,0.866025403784439,1.,0.866025403784439,1.,0.866025403784439,1.,0.866025403784439,
1.,0.866025403784439,1.,0.866025403784439,1.,0.866025403784439,1.,0.866025403784439,
1.,0.866025403784439,1.,0.866025403784439,1.,0.866025403784439,1.,0.866025403784439,
1.,0.866025403784439,1.,0.866025403784439,1.,0.866025403784439,1.,0.866025403784439,
1.,0.866025403784439,1.,0.866025403784439,1.,0.866025403784439,1.,0.866025403784439,
1.,0.866025403784439,1.,0.866025403784439,1.,0.866025403784439,1.,0.866025403784439,
1.,0.866025403784439,1.,0.866025403784439,1.,0.866025403784439,1.,0.866025403784439,
1.),(1.,0.866025403784439,1.,0.866025403784439,1.,0.866025403784439,1.,
0.866025403784439,1.,0.866025403784439,1.,0.866025403784439,1.,0.866025403784439,
1.,0.866025403784439,1.,0.866025403784439,1.,0.866025403784439,1.,0.866025403784439,
1.,0.866025403784439,1.,0.866025403784439,1.,0.866025403784439,1.,0.866025403784439,
1.,0.866025403784439,1.,0.866025403784439,1.,0.866025403784439,1.,0.866025403784439,
1.,0.866025403784439,1.,0.866025403784439,1.,0.866025403784439,1.,0.866025403784439,
1.,0.866025403784439,1.,0.866025403784439,1.,0.866025403784439,1.,0.866025403784439,
1.,0.866025403784439,1.,0.866025403784439,1.,0.866025403784439,1.,0.866025403784439,
1.,0.866025403784439,1.,0.866025403784439,1.,0.866025403784439,1.,0.866025403784439,
1.,0.866025403784439,1.,0.866025403784439,1.,0.866025403784439,1.,0.866025403784439,
1.,0.866025403784439,1.,0.866025403784439,1.,0.866025403784439,1.,0.866025403784439,
1.,0.866025403784439,1.,0.866025403784439,1.,0.866025403784439,1.,0.866025403784439,
1.,0.866025403784439,1.,0.866025403784439,1.,0.866025403784439,1.,0.866025403784439,
1.,0.866025403784439,1.,0.866025403784439,1.,0.866025403784439,1.,0.866025403784439,
1.,0.866025403784439,1.,0.866025403784439,1.,0.866025403784439,1.,0.866025403784439,
1.,0.866025403784439,1.,0.866025403784439,1.,0.866025403784439,1.,0.866025403784439,
1.,0.866025403784439,1.,0.866025403784439,1.,0.866025403784439,1.,0.866025403784439,
1.,0.866025403784439,1.,0.866025403784439,1.,0.866025403784439,1.,0.866025403784439,
1.,0.866025403784439,1.,0.866025403784439,1.,0.866025403784439,1.,0.866025403784439,
1.,0.866025403784439,1.,0.866025403784439,1.,0.866025403784439,1.,0.866025403784439,
1.,0.866025403784439,1.,0.866025403784439,1.,0.866025403784439,1.,0.866025403784439,
1.,0.866025403784439,1.,0.866025403784439,1.,0.866025403784439,1.,0.866025403784439,
1.,0.866025403784439,1.,0.866025403784439,1.,0.866025403784439,1.,0.866025403784439,
1.,0.866025403784439,1.,0.866025403784439,1.,0.866025403784439,1.,0.866025403784439,
1.,0.866025403784439,1.,0.866025403784439,1.,0.866025403784439,1.,0.866025403784439,
1.,0.866025403784439,1.,0.866025403784439,1.,0.866025403784439,1.)))
REPRESENTATION_ITEM('')
SURFACE()
);
#2317=(
BOUNDED_SURFACE()
B_SPLINE_SURFACE(1,2,((#370739,#370740,#370741,#370742,#370743,#370744,
#370745,#370746,#370747,#370748,#370749,#370750,#370751,#370752,#370753,
#370754,#370755,#370756,#370757,#370758,#370759,#370760,#370761,#370762,
#370763,#370764,#370765,#370766,#370767,#370768,#370769,#370770,#370771,
#370772,#370773,#370774,#370775,#370776,#370777,#370778,#370779,#370780,
#370781,#370782,#370783,#370784,#370785,#370786,#370787,#370788,#370789,
#370790,#370791,#370792,#370793,#370794,#370795,#370796,#370797,#370798,
#370799,#370800,#370801,#370802,#370803,#370804,#370805,#370806,#370807,
#370808,#370809,#370810,#370811,#370812,#370813,#370814,#370815,#370816,
#370817,#370818,#370819,#370820,#370821,#370822,#370823,#370824,#370825,
#370826,#370827,#370828,#370829,#370830,#370831,#370832,#370833,#370834,
#370835,#370836,#370837,#370838,#370839,#370840,#370841,#370842,#370843,
#370844,#370845,#370846,#370847,#370848,#370849,#370850,#370851,#370852,
#370853,#370854,#370855,#370856,#370857,#370858,#370859,#370860,#370861,
#370862,#370863,#370864,#370865,#370866,#370867,#370868,#370869,#370870,
#370871,#370872,#370873,#370874,#370875,#370876,#370877,#370878,#370879,
#370880,#370881,#370882,#370883,#370884,#370885,#370886,#370887,#370888,
#370889,#370890,#370891,#370892,#370893,#370894,#370895,#370896,#370897,
#370898,#370899,#370900,#370901,#370902,#370903,#370904,#370905,#370906,
#370907,#370908,#370909,#370910,#370911,#370912,#370913,#370914,#370915,
#370916,#370917,#370918,#370919,#370920,#370921,#370922,#370923,#370924,
#370925,#370926,#370927,#370928,#370929,#370930,#370931,#370932,#370933,
#370934,#370935,#370936,#370937,#370938,#370939,#370940,#370941,#370942,
#370943,#370944,#370945,#370946,#370947,#370948,#370949,#370950,#370951,
#370952,#370953,#370954,#370955),(#370956,#370957,#370958,#370959,#370960,
#370961,#370962,#370963,#370964,#370965,#370966,#370967,#370968,#370969,
#370970,#370971,#370972,#370973,#370974,#370975,#370976,#370977,#370978,
#370979,#370980,#370981,#370982,#370983,#370984,#370985,#370986,#370987,
#370988,#370989,#370990,#370991,#370992,#370993,#370994,#370995,#370996,
#370997,#370998,#370999,#371000,#371001,#371002,#371003,#371004,#371005,
#371006,#371007,#371008,#371009,#371010,#371011,#371012,#371013,#371014,
#371015,#371016,#371017,#371018,#371019,#371020,#371021,#371022,#371023,
#371024,#371025,#371026,#371027,#371028,#371029,#371030,#371031,#371032,
#371033,#371034,#371035,#371036,#371037,#371038,#371039,#371040,#371041,
#371042,#371043,#371044,#371045,#371046,#371047,#371048,#371049,#371050,
#371051,#371052,#371053,#371054,#371055,#371056,#371057,#371058,#371059,
#371060,#371061,#371062,#371063,#371064,#371065,#371066,#371067,#371068,
#371069,#371070,#371071,#371072,#371073,#371074,#371075,#371076,#371077,
#371078,#371079,#371080,#371081,#371082,#371083,#371084,#371085,#371086,
#371087,#371088,#371089,#371090,#371091,#371092,#371093,#371094,#371095,
#371096,#371097,#371098,#371099,#371100,#371101,#371102,#371103,#371104,
#371105,#371106,#371107,#371108,#371109,#371110,#371111,#371112,#371113,
#371114,#371115,#371116,#371117,#371118,#371119,#371120,#371121,#371122,
#371123,#371124,#371125,#371126,#371127,#371128,#371129,#371130,#371131,
#371132,#371133,#371134,#371135,#371136,#371137,#371138,#371139,#371140,
#371141,#371142,#371143,#371144,#371145,#371146,#371147,#371148,#371149,
#371150,#371151,#371152,#371153,#371154,#371155,#371156,#371157,#371158,
#371159,#371160,#371161,#371162,#371163,#371164,#371165,#371166,#371167,
#371168,#371169,#371170,#371171,#371172)),.UNSPECIFIED.,.F.,.F.,.F.)
B_SPLINE_SURFACE_WITH_KNOTS((2,2),(3,2,2,2,2,2,2,2,2,2,2,2,2,2,2,2,2,2,
2,2,2,2,2,2,2,2,2,2,2,2,2,2,2,2,2,2,2,2,2,2,2,2,2,2,2,2,2,2,2,2,2,2,2,2,
2,2,2,2,2,2,2,2,2,2,2,2,2,2,2,2,2,2,2,2,2,2,2,2,2,2,2,2,2,2,2,2,2,2,2,2,
2,2,2,2,2,2,2,2,2,2,2,2,2,2,2,2,2,2,3),(-1.08044907090275E-5,1.),(0.,0.00925925925925926,
0.0185185185185185,0.0277777777777778,0.037037037037037,0.0462962962962963,
0.0555555555555556,0.0648148148148148,0.0740740740740741,0.0833333333333333,
0.0925925925925926,0.101851851851852,0.111111111111111,0.12037037037037,
0.12962962962963,0.138888888888889,0.148148148148148,0.157407407407407,
0.166666666666667,0.175925925925926,0.185185185185185,0.194444444444444,
0.203703703703704,0.212962962962963,0.222222222222222,0.231481481481481,
0.240740740740741,0.25,0.259259259259259,0.268518518518519,0.277777777777778,
0.287037037037037,0.296296296296296,0.305555555555556,0.314814814814815,
0.324074074074074,0.333333333333333,0.342592592592593,0.351851851851852,
0.361111111111111,0.37037037037037,0.37962962962963,0.388888888888889,0.398148148148148,
0.407407407407407,0.416666666666667,0.425925925925926,0.435185185185185,
0.444444444444444,0.453703703703704,0.462962962962963,0.472222222222222,
0.481481481481481,0.490740740740741,0.5,0.509259259259259,0.518518518518518,
0.527777777777778,0.537037037037037,0.546296296296296,0.555555555555556,
0.564814814814815,0.574074074074074,0.583333333333333,0.592592592592593,
0.601851851851852,0.611111111111111,0.62037037037037,0.62962962962963,0.638888888888889,
0.648148148148148,0.657407407407407,0.666666666666667,0.675925925925926,
0.685185185185185,0.694444444444444,0.703703703703704,0.712962962962963,
0.722222222222222,0.731481481481482,0.740740740740741,0.75,0.759259259259259,
0.768518518518518,0.777777777777778,0.787037037037037,0.796296296296296,
0.805555555555556,0.814814814814815,0.824074074074074,0.833333333333333,
0.842592592592593,0.851851851851852,0.861111111111111,0.87037037037037,
0.87962962962963,0.888888888888889,0.898148148148148,0.907407407407407,
0.916666666666667,0.925925925925926,0.935185185185185,0.944444444444444,
0.953703703703704,0.962962962962963,0.972222222222222,0.981481481481482,
0.987622467374972,0.997498692048721),.UNSPECIFIED.)
GEOMETRIC_REPRESENTATION_ITEM()
RATIONAL_B_SPLINE_SURFACE(((1.,0.866025403784439,1.,0.866025403784439,1.,
0.866025403784439,1.,0.866025403784439,1.,0.866025403784439,1.,0.866025403784439,
1.,0.866025403784439,1.,0.866025403784439,1.,0.866025403784439,1.,0.866025403784439,
1.,0.866025403784439,1.,0.866025403784439,1.,0.866025403784439,1.,0.866025403784439,
1.,0.866025403784439,1.,0.866025403784439,1.,0.866025403784439,1.,0.866025403784439,
1.,0.866025403784439,1.,0.866025403784439,1.,0.866025403784439,1.,0.866025403784439,
1.,0.866025403784439,1.,0.866025403784439,1.,0.866025403784439,1.,0.866025403784439,
1.,0.866025403784439,1.,0.866025403784439,1.,0.866025403784439,1.,0.866025403784439,
1.,0.866025403784439,1.,0.866025403784439,1.,0.866025403784439,1.,0.866025403784439,
1.,0.866025403784439,1.,0.866025403784439,1.,0.866025403784439,1.,0.866025403784439,
1.,0.866025403784439,1.,0.866025403784439,1.,0.866025403784439,1.,0.866025403784439,
1.,0.866025403784439,1.,0.866025403784439,1.,0.866025403784439,1.,0.866025403784439,
1.,0.866025403784439,1.,0.866025403784439,1.,0.866025403784439,1.,0.866025403784439,
1.,0.866025403784439,1.,0.866025403784439,1.,0.866025403784439,1.,0.866025403784439,
1.,0.866025403784439,1.,0.866025403784439,1.,0.866025403784439,1.,0.866025403784439,
1.,0.866025403784439,1.,0.866025403784439,1.,0.866025403784439,1.,0.866025403784439,
1.,0.866025403784439,1.,0.866025403784439,1.,0.866025403784439,1.,0.866025403784439,
1.,0.866025403784439,1.,0.866025403784439,1.,0.866025403784439,1.,0.866025403784439,
1.,0.866025403784439,1.,0.866025403784439,1.,0.866025403784439,1.,0.866025403784439,
1.,0.866025403784439,1.,0.866025403784439,1.,0.866025403784439,1.,0.866025403784439,
1.,0.866025403784439,1.,0.866025403784439,1.,0.866025403784439,1.,0.866025403784439,
1.,0.866025403784439,1.,0.866025403784439,1.,0.866025403784439,1.,0.866025403784439,
1.,0.866025403784439,1.,0.866025403784439,1.,0.866025403784439,1.,0.866025403784439,
1.,0.866025403784439,1.,0.866025403784439,1.,0.866025403784439,1.,0.866025403784439,
1.,0.866025403784439,1.,0.866025403784439,1.,0.866025403784439,1.,0.866025403784439,
1.,0.866025403784439,1.,0.866025403784439,1.,0.866025403784439,1.,0.866025403784439,
1.,0.866025403784439,1.,0.866025403784439,1.,0.866025403784439,1.,0.866025403784439,
1.,0.911144500611853,0.940151640776859,0.940151640776859,0.940151640776859),
(1.,0.866025403784439,1.,0.866025403784439,1.,0.866025403784439,1.,0.866025403784439,
1.,0.866025403784439,1.,0.866025403784439,1.,0.866025403784439,1.,0.866025403784439,
1.,0.866025403784439,1.,0.866025403784439,1.,0.866025403784439,1.,0.866025403784439,
1.,0.866025403784439,1.,0.866025403784439,1.,0.866025403784439,1.,0.866025403784439,
1.,0.866025403784439,1.,0.866025403784439,1.,0.866025403784439,1.,0.866025403784439,
1.,0.866025403784439,1.,0.866025403784439,1.,0.866025403784439,1.,0.866025403784439,
1.,0.866025403784439,1.,0.866025403784439,1.,0.866025403784439,1.,0.866025403784439,
1.,0.866025403784439,1.,0.866025403784439,1.,0.866025403784439,1.,0.866025403784439,
1.,0.866025403784439,1.,0.866025403784439,1.,0.866025403784439,1.,0.866025403784439,
1.,0.866025403784439,1.,0.866025403784439,1.,0.866025403784439,1.,0.866025403784439,
1.,0.866025403784439,1.,0.866025403784439,1.,0.866025403784439,1.,0.866025403784439,
1.,0.866025403784439,1.,0.866025403784439,1.,0.866025403784439,1.,0.866025403784439,
1.,0.866025403784439,1.,0.866025403784439,1.,0.866025403784439,1.,0.866025403784439,
1.,0.866025403784439,1.,0.866025403784439,1.,0.866025403784439,1.,0.866025403784439,
1.,0.866025403784439,1.,0.866025403784439,1.,0.866025403784439,1.,0.866025403784439,
1.,0.866025403784439,1.,0.866025403784439,1.,0.866025403784439,1.,0.866025403784439,
1.,0.866025403784439,1.,0.866025403784439,1.,0.866025403784439,1.,0.866025403784439,
1.,0.866025403784439,1.,0.866025403784439,1.,0.866025403784439,1.,0.866025403784439,
1.,0.866025403784439,1.,0.866025403784439,1.,0.866025403784439,1.,0.866025403784439,
1.,0.866025403784439,1.,0.866025403784439,1.,0.866025403784439,1.,0.866025403784439,
1.,0.866025403784439,1.,0.866025403784439,1.,0.866025403784439,1.,0.866025403784439,
1.,0.866025403784439,1.,0.866025403784439,1.,0.866025403784439,1.,0.866025403784439,
1.,0.866025403784439,1.,0.866025403784439,1.,0.866025403784439,1.,0.866025403784439,
1.,0.866025403784439,1.,0.866025403784439,1.,0.866025403784439,1.,0.866025403784439,
1.,0.866025403784439,1.,0.866025403784439,1.,0.866025403784439,1.,0.866025403784439,
1.,0.866025403784439,1.,0.866025403784439,1.,0.866025403784439,1.,0.866025403784439,
1.,0.866025403784439,1.,0.866025403784439,1.,0.911144500611853,0.940151640776859,
0.940151640776859,0.940151640776859)))
REPRESENTATION_ITEM('')
SURFACE()
);
#2318=(
BOUNDED_SURFACE()
B_SPLINE_SURFACE(1,2,((#371177,#371178,#371179,#371180,#371181,#371182,
#371183,#371184,#371185,#371186,#371187,#371188,#371189,#371190,#371191,
#371192,#371193,#371194,#371195,#371196,#371197,#371198,#371199,#371200,
#371201,#371202,#371203,#371204,#371205,#371206,#371207,#371208,#371209,
#371210,#371211,#371212,#371213,#371214,#371215,#371216,#371217,#371218,
#371219,#371220,#371221,#371222,#371223,#371224,#371225,#371226,#371227,
#371228,#371229,#371230,#371231,#371232,#371233,#371234,#371235,#371236,
#371237,#371238,#371239,#371240,#371241,#371242,#371243,#371244,#371245,
#371246,#371247,#371248,#371249,#371250,#371251,#371252,#371253,#371254,
#371255,#371256,#371257,#371258,#371259,#371260,#371261,#371262,#371263,
#371264,#371265,#371266,#371267,#371268,#371269,#371270,#371271,#371272,
#371273,#371274,#371275,#371276,#371277,#371278,#371279,#371280,#371281,
#371282,#371283,#371284,#371285,#371286,#371287,#371288,#371289,#371290,
#371291,#371292,#371293,#371294,#371295,#371296,#371297,#371298,#371299,
#371300,#371301,#371302,#371303,#371304,#371305,#371306,#371307,#371308,
#371309,#371310,#371311,#371312,#371313,#371314,#371315,#371316,#371317,
#371318,#371319,#371320,#371321,#371322,#371323,#371324,#371325,#371326,
#371327,#371328,#371329,#371330,#371331,#371332,#371333,#371334,#371335,
#371336,#371337,#371338,#371339,#371340,#371341,#371342,#371343,#371344,
#371345,#371346,#371347,#371348,#371349,#371350,#371351,#371352,#371353,
#371354,#371355,#371356,#371357,#371358,#371359,#371360,#371361,#371362,
#371363,#371364,#371365,#371366,#371367,#371368,#371369,#371370,#371371,
#371372,#371373,#371374,#371375,#371376,#371377,#371378,#371379,#371380,
#371381,#371382,#371383,#371384,#371385,#371386,#371387,#371388,#371389,
#371390,#371391),(#371392,#371393,#371394,#371395,#371396,#371397,#371398,
#371399,#371400,#371401,#371402,#371403,#371404,#371405,#371406,#371407,
#371408,#371409,#371410,#371411,#371412,#371413,#371414,#371415,#371416,
#371417,#371418,#371419,#371420,#371421,#371422,#371423,#371424,#371425,
#371426,#371427,#371428,#371429,#371430,#371431,#371432,#371433,#371434,
#371435,#371436,#371437,#371438,#371439,#371440,#371441,#371442,#371443,
#371444,#371445,#371446,#371447,#371448,#371449,#371450,#371451,#371452,
#371453,#371454,#371455,#371456,#371457,#371458,#371459,#371460,#371461,
#371462,#371463,#371464,#371465,#371466,#371467,#371468,#371469,#371470,
#371471,#371472,#371473,#371474,#371475,#371476,#371477,#371478,#371479,
#371480,#371481,#371482,#371483,#371484,#371485,#371486,#371487,#371488,
#371489,#371490,#371491,#371492,#371493,#371494,#371495,#371496,#371497,
#371498,#371499,#371500,#371501,#371502,#371503,#371504,#371505,#371506,
#371507,#371508,#371509,#371510,#371511,#371512,#371513,#371514,#371515,
#371516,#371517,#371518,#371519,#371520,#371521,#371522,#371523,#371524,
#371525,#371526,#371527,#371528,#371529,#371530,#371531,#371532,#371533,
#371534,#371535,#371536,#371537,#371538,#371539,#371540,#371541,#371542,
#371543,#371544,#371545,#371546,#371547,#371548,#371549,#371550,#371551,
#371552,#371553,#371554,#371555,#371556,#371557,#371558,#371559,#371560,
#371561,#371562,#371563,#371564,#371565,#371566,#371567,#371568,#371569,
#371570,#371571,#371572,#371573,#371574,#371575,#371576,#371577,#371578,
#371579,#371580,#371581,#371582,#371583,#371584,#371585,#371586,#371587,
#371588,#371589,#371590,#371591,#371592,#371593,#371594,#371595,#371596,
#371597,#371598,#371599,#371600,#371601,#371602,#371603,#371604,#371605,
#371606)),.UNSPECIFIED.,.F.,.F.,.F.)
B_SPLINE_SURFACE_WITH_KNOTS((2,2),(3,2,2,2,2,2,2,2,2,2,2,2,2,2,2,2,2,2,
2,2,2,2,2,2,2,2,2,2,2,2,2,2,2,2,2,2,2,2,2,2,2,2,2,2,2,2,2,2,2,2,2,2,2,2,
2,2,2,2,2,2,2,2,2,2,2,2,2,2,2,2,2,2,2,2,2,2,2,2,2,2,2,2,2,2,2,2,2,2,2,2,
2,2,2,2,2,2,2,2,2,2,2,2,2,2,2,2,2,3),(0.,1.),(0.,0.00925925925925926,0.0185185185185185,
0.0277777777777778,0.037037037037037,0.0462962962962963,0.0555555555555556,
0.0648148148148148,0.0740740740740741,0.0833333333333333,0.0925925925925926,
0.101851851851852,0.111111111111111,0.12037037037037,0.12962962962963,0.138888888888889,
0.148148148148148,0.157407407407407,0.166666666666667,0.175925925925926,
0.185185185185185,0.194444444444444,0.203703703703704,0.212962962962963,
0.222222222222222,0.231481481481481,0.240740740740741,0.25,0.259259259259259,
0.268518518518519,0.277777777777778,0.287037037037037,0.296296296296296,
0.305555555555556,0.314814814814815,0.324074074074074,0.333333333333333,
0.342592592592593,0.351851851851852,0.361111111111111,0.37037037037037,
0.37962962962963,0.388888888888889,0.398148148148148,0.407407407407407,
0.416666666666667,0.425925925925926,0.435185185185185,0.444444444444444,
0.453703703703704,0.462962962962963,0.472222222222222,0.481481481481481,
0.490740740740741,0.5,0.509259259259259,0.518518518518518,0.527777777777778,
0.537037037037037,0.546296296296296,0.555555555555556,0.564814814814815,
0.574074074074074,0.583333333333333,0.592592592592593,0.601851851851852,
0.611111111111111,0.62037037037037,0.62962962962963,0.638888888888889,0.648148148148148,
0.657407407407407,0.666666666666667,0.675925925925926,0.685185185185185,
0.694444444444444,0.703703703703704,0.712962962962963,0.722222222222222,
0.731481481481482,0.740740740740741,0.75,0.759259259259259,0.768518518518518,
0.777777777777778,0.787037037037037,0.796296296296296,0.805555555555556,
0.814814814814815,0.824074074074074,0.833333333333333,0.842592592592593,
0.851851851851852,0.861111111111111,0.87037037037037,0.87962962962963,0.888888888888889,
0.898148148148148,0.907407407407407,0.916666666666667,0.925925925925926,
0.935185185185185,0.944444444444444,0.953703703703704,0.962962962962963,
0.972222222222222,0.981481481481482,0.987622586258463),.UNSPECIFIED.)
GEOMETRIC_REPRESENTATION_ITEM()
RATIONAL_B_SPLINE_SURFACE(((1.,0.866025403784439,1.,0.866025403784439,1.,
0.866025403784439,1.,0.866025403784439,1.,0.866025403784439,1.,0.866025403784439,
1.,0.866025403784439,1.,0.866025403784439,1.,0.866025403784439,1.,0.866025403784439,
1.,0.866025403784439,1.,0.866025403784439,1.,0.866025403784439,1.,0.866025403784439,
1.,0.866025403784439,1.,0.866025403784439,1.,0.866025403784439,1.,0.866025403784439,
1.,0.866025403784439,1.,0.866025403784439,1.,0.866025403784439,1.,0.866025403784439,
1.,0.866025403784439,1.,0.866025403784439,1.,0.866025403784439,1.,0.866025403784439,
1.,0.866025403784439,1.,0.866025403784439,1.,0.866025403784439,1.,0.866025403784439,
1.,0.866025403784439,1.,0.866025403784439,1.,0.866025403784439,1.,0.866025403784439,
1.,0.866025403784439,1.,0.866025403784439,1.,0.866025403784439,1.,0.866025403784439,
1.,0.866025403784439,1.,0.866025403784439,1.,0.866025403784439,1.,0.866025403784439,
1.,0.866025403784439,1.,0.866025403784439,1.,0.866025403784439,1.,0.866025403784439,
1.,0.866025403784439,1.,0.866025403784439,1.,0.866025403784439,1.,0.866025403784439,
1.,0.866025403784439,1.,0.866025403784439,1.,0.866025403784439,1.,0.866025403784439,
1.,0.866025403784439,1.,0.866025403784439,1.,0.866025403784439,1.,0.866025403784439,
1.,0.866025403784439,1.,0.866025403784439,1.,0.866025403784439,1.,0.866025403784439,
1.,0.866025403784439,1.,0.866025403784439,1.,0.866025403784439,1.,0.866025403784439,
1.,0.866025403784439,1.,0.866025403784439,1.,0.866025403784439,1.,0.866025403784439,
1.,0.866025403784439,1.,0.866025403784439,1.,0.866025403784439,1.,0.866025403784439,
1.,0.866025403784439,1.,0.866025403784439,1.,0.866025403784439,1.,0.866025403784439,
1.,0.866025403784439,1.,0.866025403784439,1.,0.866025403784439,1.,0.866025403784439,
1.,0.866025403784439,1.,0.866025403784439,1.,0.866025403784439,1.,0.866025403784439,
1.,0.866025403784439,1.,0.866025403784439,1.,0.866025403784439,1.,0.866025403784439,
1.,0.866025403784439,1.,0.866025403784439,1.,0.866025403784439,1.,0.866025403784439,
1.,0.866025403784439,1.,0.866025403784439,1.,0.866025403784439,1.,0.866025403784439,
1.,0.866025403784439,1.,0.866025403784439,1.,0.866025403784439,1.,0.866025403784439,
1.,0.866025403784439,1.,0.866025403784439,1.,0.866025403784439,1.,0.866025403784439,
1.,0.911142780456138,0.940152763920857),(1.,0.866025403784439,1.,0.866025403784439,
1.,0.866025403784439,1.,0.866025403784439,1.,0.866025403784439,1.,0.866025403784439,
1.,0.866025403784439,1.,0.866025403784439,1.,0.866025403784439,1.,0.866025403784439,
1.,0.866025403784439,1.,0.866025403784439,1.,0.866025403784439,1.,0.866025403784439,
1.,0.866025403784439,1.,0.866025403784439,1.,0.866025403784439,1.,0.866025403784439,
1.,0.866025403784439,1.,0.866025403784439,1.,0.866025403784439,1.,0.866025403784439,
1.,0.866025403784439,1.,0.866025403784439,1.,0.866025403784439,1.,0.866025403784439,
1.,0.866025403784439,1.,0.866025403784439,1.,0.866025403784439,1.,0.866025403784439,
1.,0.866025403784439,1.,0.866025403784439,1.,0.866025403784439,1.,0.866025403784439,
1.,0.866025403784439,1.,0.866025403784439,1.,0.866025403784439,1.,0.866025403784439,
1.,0.866025403784439,1.,0.866025403784439,1.,0.866025403784439,1.,0.866025403784439,
1.,0.866025403784439,1.,0.866025403784439,1.,0.866025403784439,1.,0.866025403784439,
1.,0.866025403784439,1.,0.866025403784439,1.,0.866025403784439,1.,0.866025403784439,
1.,0.866025403784439,1.,0.866025403784439,1.,0.866025403784439,1.,0.866025403784439,
1.,0.866025403784439,1.,0.866025403784439,1.,0.866025403784439,1.,0.866025403784439,
1.,0.866025403784439,1.,0.866025403784439,1.,0.866025403784439,1.,0.866025403784439,
1.,0.866025403784439,1.,0.866025403784439,1.,0.866025403784439,1.,0.866025403784439,
1.,0.866025403784439,1.,0.866025403784439,1.,0.866025403784439,1.,0.866025403784439,
1.,0.866025403784439,1.,0.866025403784439,1.,0.866025403784439,1.,0.866025403784439,
1.,0.866025403784439,1.,0.866025403784439,1.,0.866025403784439,1.,0.866025403784439,
1.,0.866025403784439,1.,0.866025403784439,1.,0.866025403784439,1.,0.866025403784439,
1.,0.866025403784439,1.,0.866025403784439,1.,0.866025403784439,1.,0.866025403784439,
1.,0.866025403784439,1.,0.866025403784439,1.,0.866025403784439,1.,0.866025403784439,
1.,0.866025403784439,1.,0.866025403784439,1.,0.866025403784439,1.,0.866025403784439,
1.,0.866025403784439,1.,0.866025403784439,1.,0.866025403784439,1.,0.866025403784439,
1.,0.866025403784439,1.,0.866025403784439,1.,0.866025403784439,1.,0.866025403784439,
1.,0.866025403784439,1.,0.866025403784439,1.,0.866025403784439,1.,0.866025403784439,
1.,0.911142780456138,0.940152763920857)))
REPRESENTATION_ITEM('')
SURFACE()
);
#2319=(
BOUNDED_SURFACE()
B_SPLINE_SURFACE(1,2,((#378429,#378430,#378431,#378432,#378433,#378434,
#378435,#378436,#378437,#378438,#378439,#378440,#378441,#378442,#378443,
#378444,#378445,#378446,#378447,#378448,#378449,#378450,#378451,#378452,
#378453,#378454,#378455,#378456,#378457,#378458,#378459,#378460,#378461,
#378462,#378463,#378464,#378465,#378466,#378467,#378468,#378469,#378470,
#378471,#378472,#378473,#378474,#378475,#378476,#378477,#378478,#378479,
#378480,#378481,#378482,#378483,#378484,#378485,#378486,#378487,#378488,
#378489,#378490,#378491,#378492,#378493,#378494,#378495,#378496,#378497,
#378498,#378499,#378500,#378501,#378502,#378503,#378504,#378505,#378506,
#378507,#378508,#378509,#378510,#378511,#378512,#378513,#378514,#378515,
#378516,#378517,#378518,#378519,#378520,#378521,#378522,#378523,#378524,
#378525,#378526,#378527,#378528,#378529,#378530,#378531,#378532,#378533,
#378534,#378535,#378536,#378537,#378538,#378539,#378540,#378541,#378542,
#378543,#378544,#378545,#378546,#378547,#378548,#378549,#378550,#378551,
#378552,#378553,#378554,#378555,#378556,#378557,#378558,#378559,#378560,
#378561,#378562,#378563,#378564,#378565,#378566,#378567,#378568,#378569,
#378570,#378571,#378572,#378573,#378574,#378575,#378576,#378577,#378578,
#378579,#378580,#378581,#378582,#378583,#378584,#378585,#378586,#378587,
#378588,#378589,#378590,#378591,#378592,#378593,#378594,#378595,#378596,
#378597,#378598,#378599,#378600,#378601,#378602,#378603,#378604,#378605,
#378606,#378607,#378608,#378609,#378610,#378611,#378612,#378613,#378614,
#378615,#378616,#378617,#378618,#378619,#378620,#378621,#378622,#378623,
#378624,#378625,#378626,#378627,#378628,#378629,#378630,#378631,#378632,
#378633,#378634,#378635,#378636,#378637,#378638,#378639,#378640,#378641,
#378642,#378643,#378644,#378645,#378646,#378647,#378648,#378649,#378650,
#378651,#378652,#378653,#378654,#378655,#378656,#378657,#378658,#378659,
#378660,#378661,#378662,#378663,#378664,#378665,#378666,#378667,#378668,
#378669,#378670,#378671,#378672,#378673,#378674,#378675,#378676,#378677,
#378678,#378679,#378680,#378681,#378682,#378683,#378684,#378685,#378686,
#378687,#378688,#378689,#378690,#378691,#378692,#378693,#378694,#378695,
#378696,#378697,#378698,#378699,#378700,#378701,#378702,#378703,#378704,
#378705,#378706,#378707,#378708,#378709,#378710,#378711,#378712,#378713,
#378714,#378715,#378716,#378717,#378718,#378719,#378720,#378721,#378722,
#378723,#378724,#378725,#378726,#378727,#378728,#378729,#378730,#378731,
#378732,#378733,#378734,#378735,#378736,#378737,#378738,#378739,#378740,
#378741,#378742,#378743,#378744,#378745,#378746,#378747,#378748,#378749,
#378750,#378751,#378752,#378753,#378754,#378755,#378756,#378757,#378758,
#378759,#378760,#378761,#378762,#378763,#378764,#378765,#378766,#378767,
#378768,#378769,#378770,#378771,#378772,#378773,#378774,#378775,#378776,
#378777,#378778,#378779,#378780,#378781,#378782,#378783,#378784,#378785,
#378786,#378787,#378788,#378789,#378790,#378791,#378792,#378793,#378794,
#378795,#378796,#378797,#378798,#378799,#378800,#378801),(#378802,#378803,
#378804,#378805,#378806,#378807,#378808,#378809,#378810,#378811,#378812,
#378813,#378814,#378815,#378816,#378817,#378818,#378819,#378820,#378821,
#378822,#378823,#378824,#378825,#378826,#378827,#378828,#378829,#378830,
#378831,#378832,#378833,#378834,#378835,#378836,#378837,#378838,#378839,
#378840,#378841,#378842,#378843,#378844,#378845,#378846,#378847,#378848,
#378849,#378850,#378851,#378852,#378853,#378854,#378855,#378856,#378857,
#378858,#378859,#378860,#378861,#378862,#378863,#378864,#378865,#378866,
#378867,#378868,#378869,#378870,#378871,#378872,#378873,#378874,#378875,
#378876,#378877,#378878,#378879,#378880,#378881,#378882,#378883,#378884,
#378885,#378886,#378887,#378888,#378889,#378890,#378891,#378892,#378893,
#378894,#378895,#378896,#378897,#378898,#378899,#378900,#378901,#378902,
#378903,#378904,#378905,#378906,#378907,#378908,#378909,#378910,#378911,
#378912,#378913,#378914,#378915,#378916,#378917,#378918,#378919,#378920,
#378921,#378922,#378923,#378924,#378925,#378926,#378927,#378928,#378929,
#378930,#378931,#378932,#378933,#378934,#378935,#378936,#378937,#378938,
#378939,#378940,#378941,#378942,#378943,#378944,#378945,#378946,#378947,
#378948,#378949,#378950,#378951,#378952,#378953,#378954,#378955,#378956,
#378957,#378958,#378959,#378960,#378961,#378962,#378963,#378964,#378965,
#378966,#378967,#378968,#378969,#378970,#378971,#378972,#378973,#378974,
#378975,#378976,#378977,#378978,#378979,#378980,#378981,#378982,#378983,
#378984,#378985,#378986,#378987,#378988,#378989,#378990,#378991,#378992,
#378993,#378994,#378995,#378996,#378997,#378998,#378999,#379000,#379001,
#379002,#379003,#379004,#379005,#379006,#379007,#379008,#379009,#379010,
#379011,#379012,#379013,#379014,#379015,#379016,#379017,#379018,#379019,
#379020,#379021,#379022,#379023,#379024,#379025,#379026,#379027,#379028,
#379029,#379030,#379031,#379032,#379033,#379034,#379035,#379036,#379037,
#379038,#379039,#379040,#379041,#379042,#379043,#379044,#379045,#379046,
#379047,#379048,#379049,#379050,#379051,#379052,#379053,#379054,#379055,
#379056,#379057,#379058,#379059,#379060,#379061,#379062,#379063,#379064,
#379065,#379066,#379067,#379068,#379069,#379070,#379071,#379072,#379073,
#379074,#379075,#379076,#379077,#379078,#379079,#379080,#379081,#379082,
#379083,#379084,#379085,#379086,#379087,#379088,#379089,#379090,#379091,
#379092,#379093,#379094,#379095,#379096,#379097,#379098,#379099,#379100,
#379101,#379102,#379103,#379104,#379105,#379106,#379107,#379108,#379109,
#379110,#379111,#379112,#379113,#379114,#379115,#379116,#379117,#379118,
#379119,#379120,#379121,#379122,#379123,#379124,#379125,#379126,#379127,
#379128,#379129,#379130,#379131,#379132,#379133,#379134,#379135,#379136,
#379137,#379138,#379139,#379140,#379141,#379142,#379143,#379144,#379145,
#379146,#379147,#379148,#379149,#379150,#379151,#379152,#379153,#379154,
#379155,#379156,#379157,#379158,#379159,#379160,#379161,#379162,#379163,
#379164,#379165,#379166,#379167,#379168,#379169,#379170,#379171,#379172,
#379173,#379174)),.UNSPECIFIED.,.F.,.F.,.F.)
B_SPLINE_SURFACE_WITH_KNOTS((2,2),(3,2,2,2,2,2,2,2,2,2,2,2,2,2,2,2,2,2,
2,2,2,2,2,2,2,2,2,2,2,2,2,2,2,2,2,2,2,2,2,2,2,2,2,2,2,2,2,2,2,2,2,2,2,2,
2,2,2,2,2,2,2,2,2,2,2,2,2,2,2,2,2,2,2,2,2,2,2,2,2,2,2,2,2,2,2,2,2,2,2,2,
2,2,2,2,2,2,2,2,2,2,2,2,2,2,2,2,2,2,2,2,2,2,2,2,2,2,2,2,2,2,2,2,2,2,2,2,
2,2,2,2,2,2,2,2,2,2,2,2,2,2,2,2,2,2,2,2,2,2,2,2,2,2,2,2,2,2,2,2,2,2,2,2,
2,2,2,2,2,2,2,2,2,2,2,2,2,2,2,2,2,2,2,2,2,2,2,2,3),(0.,1.),(0.,0.00537634408602151,
0.010752688172043,0.0161290322580645,0.021505376344086,0.0268817204301075,
0.032258064516129,0.0376344086021505,0.043010752688172,0.0483870967741935,
0.0537634408602151,0.0591397849462366,0.0645161290322581,0.0698924731182796,
0.0752688172043011,0.0806451612903226,0.0860215053763441,0.0913978494623656,
0.0967741935483871,0.102150537634409,0.10752688172043,0.112903225806452,
0.118279569892473,0.123655913978495,0.129032258064516,0.134408602150538,
0.139784946236559,0.145161290322581,0.150537634408602,0.155913978494624,
0.161290322580645,0.166666666666667,0.172043010752688,0.17741935483871,
0.182795698924731,0.188172043010753,0.193548387096774,0.198924731182796,
0.204301075268817,0.209677419354839,0.21505376344086,0.220430107526882,
0.225806451612903,0.231182795698925,0.236559139784946,0.241935483870968,
0.247311827956989,0.252688172043011,0.258064516129032,0.263440860215054,
0.268817204301075,0.274193548387097,0.279569892473118,0.28494623655914,
0.290322580645161,0.295698924731183,0.301075268817204,0.306451612903226,
0.311827956989247,0.317204301075269,0.32258064516129,0.327956989247312,
0.333333333333333,0.338709677419355,0.344086021505376,0.349462365591398,
0.354838709677419,0.360215053763441,0.365591397849462,0.370967741935484,
0.376344086021505,0.381720430107527,0.387096774193548,0.39247311827957,
0.397849462365591,0.403225806451613,0.408602150537634,0.413978494623656,
0.419354838709677,0.424731182795699,0.43010752688172,0.435483870967742,
0.440860215053763,0.446236559139785,0.451612903225806,0.456989247311828,
0.462365591397849,0.467741935483871,0.473118279569892,0.478494623655914,
0.483870967741935,0.489247311827957,0.494623655913978,0.5,0.505376344086022,
0.510752688172043,0.516129032258065,0.521505376344086,0.526881720430108,
0.532258064516129,0.537634408602151,0.543010752688172,0.548387096774194,
0.553763440860215,0.559139784946237,0.564516129032258,0.56989247311828,
0.575268817204301,0.580645161290323,0.586021505376344,0.591397849462366,
0.596774193548387,0.602150537634409,0.60752688172043,0.612903225806452,
0.618279569892473,0.623655913978495,0.629032258064516,0.634408602150538,
0.639784946236559,0.645161290322581,0.650537634408602,0.655913978494624,
0.661290322580645,0.666666666666667,0.672043010752688,0.67741935483871,
0.682795698924731,0.688172043010753,0.693548387096774,0.698924731182796,
0.704301075268817,0.709677419354839,0.71505376344086,0.720430107526882,
0.725806451612903,0.731182795698925,0.736559139784946,0.741935483870968,
0.747311827956989,0.752688172043011,0.758064516129032,0.763440860215054,
0.768817204301075,0.774193548387097,0.779569892473118,0.78494623655914,
0.790322580645161,0.795698924731183,0.801075268817204,0.806451612903226,
0.811827956989247,0.817204301075269,0.82258064516129,0.827956989247312,
0.833333333333333,0.838709677419355,0.844086021505376,0.849462365591398,
0.854838709677419,0.860215053763441,0.865591397849462,0.870967741935484,
0.876344086021505,0.881720430107527,0.887096774193548,0.89247311827957,
0.897849462365591,0.903225806451613,0.908602150537634,0.913978494623656,
0.919354838709677,0.924731182795699,0.93010752688172,0.935483870967742,
0.940860215053763,0.946236559139785,0.951612903225806,0.956989247311828,
0.962365591397849,0.967741935483871,0.973118279569892,0.978494623655914,
0.983870967741935,0.989247311827957,0.994623655913978,1.),.UNSPECIFIED.)
GEOMETRIC_REPRESENTATION_ITEM()
RATIONAL_B_SPLINE_SURFACE(((1.,0.866025403784439,1.,0.866025403784439,1.,
0.866025403784439,1.,0.866025403784439,1.,0.866025403784439,1.,0.866025403784439,
1.,0.866025403784439,1.,0.866025403784439,1.,0.866025403784439,1.,0.866025403784439,
1.,0.866025403784439,1.,0.866025403784439,1.,0.866025403784439,1.,0.866025403784439,
1.,0.866025403784439,1.,0.866025403784439,1.,0.866025403784439,1.,0.866025403784439,
1.,0.866025403784439,1.,0.866025403784439,1.,0.866025403784439,1.,0.866025403784439,
1.,0.866025403784439,1.,0.866025403784439,1.,0.866025403784439,1.,0.866025403784439,
1.,0.866025403784439,1.,0.866025403784439,1.,0.866025403784439,1.,0.866025403784439,
1.,0.866025403784439,1.,0.866025403784439,1.,0.866025403784439,1.,0.866025403784439,
1.,0.866025403784439,1.,0.866025403784439,1.,0.866025403784439,1.,0.866025403784439,
1.,0.866025403784439,1.,0.866025403784439,1.,0.866025403784439,1.,0.866025403784439,
1.,0.866025403784439,1.,0.866025403784439,1.,0.866025403784439,1.,0.866025403784439,
1.,0.866025403784439,1.,0.866025403784439,1.,0.866025403784439,1.,0.866025403784439,
1.,0.866025403784439,1.,0.866025403784439,1.,0.866025403784439,1.,0.866025403784439,
1.,0.866025403784439,1.,0.866025403784439,1.,0.866025403784439,1.,0.866025403784439,
1.,0.866025403784439,1.,0.866025403784439,1.,0.866025403784439,1.,0.866025403784439,
1.,0.866025403784439,1.,0.866025403784439,1.,0.866025403784439,1.,0.866025403784439,
1.,0.866025403784439,1.,0.866025403784439,1.,0.866025403784439,1.,0.866025403784439,
1.,0.866025403784439,1.,0.866025403784439,1.,0.866025403784439,1.,0.866025403784439,
1.,0.866025403784439,1.,0.866025403784439,1.,0.866025403784439,1.,0.866025403784439,
1.,0.866025403784439,1.,0.866025403784439,1.,0.866025403784439,1.,0.866025403784439,
1.,0.866025403784439,1.,0.866025403784439,1.,0.866025403784439,1.,0.866025403784439,
1.,0.866025403784439,1.,0.866025403784439,1.,0.866025403784439,1.,0.866025403784439,
1.,0.866025403784439,1.,0.866025403784439,1.,0.866025403784439,1.,0.866025403784439,
1.,0.866025403784439,1.,0.866025403784439,1.,0.866025403784439,1.,0.866025403784439,
1.,0.866025403784439,1.,0.866025403784439,1.,0.866025403784439,1.,0.866025403784439,
1.,0.866025403784439,1.,0.866025403784439,1.,0.866025403784439,1.,0.866025403784439,
1.,0.866025403784439,1.,0.866025403784439,1.,0.866025403784439,1.,0.866025403784439,
1.,0.866025403784439,1.,0.866025403784439,1.,0.866025403784439,1.,0.866025403784439,
1.,0.866025403784439,1.,0.866025403784439,1.,0.866025403784439,1.,0.866025403784439,
1.,0.866025403784439,1.,0.866025403784439,1.,0.866025403784439,1.,0.866025403784439,
1.,0.866025403784439,1.,0.866025403784439,1.,0.866025403784439,1.,0.866025403784439,
1.,0.866025403784439,1.,0.866025403784439,1.,0.866025403784439,1.,0.866025403784439,
1.,0.866025403784439,1.,0.866025403784439,1.,0.866025403784439,1.,0.866025403784439,
1.,0.866025403784439,1.,0.866025403784439,1.,0.866025403784439,1.,0.866025403784439,
1.,0.866025403784439,1.,0.866025403784439,1.,0.866025403784439,1.,0.866025403784439,
1.,0.866025403784439,1.,0.866025403784439,1.,0.866025403784439,1.,0.866025403784439,
1.,0.866025403784439,1.,0.866025403784439,1.,0.866025403784439,1.,0.866025403784439,
1.,0.866025403784439,1.,0.866025403784439,1.,0.866025403784439,1.,0.866025403784439,
1.,0.866025403784439,1.,0.866025403784439,1.,0.866025403784439,1.,0.866025403784439,
1.,0.866025403784439,1.,0.866025403784439,1.,0.866025403784439,1.,0.866025403784439,
1.,0.866025403784439,1.,0.866025403784439,1.,0.866025403784439,1.,0.866025403784439,
1.,0.866025403784439,1.,0.866025403784439,1.,0.866025403784439,1.,0.866025403784439,
1.,0.866025403784439,1.,0.866025403784439,1.,0.866025403784439,1.,0.866025403784439,
1.,0.866025403784439,1.,0.866025403784439,1.,0.866025403784439,1.,0.866025403784439,
1.,0.866025403784439,1.,0.866025403784439,1.,0.866025403784439,1.,0.866025403784439,
1.,0.866025403784439,1.,0.866025403784439,1.,0.866025403784439,1.,0.866025403784439,
1.),(1.,0.866025403784439,1.,0.866025403784439,1.,0.866025403784439,1.,
0.866025403784439,1.,0.866025403784439,1.,0.866025403784439,1.,0.866025403784439,
1.,0.866025403784439,1.,0.866025403784439,1.,0.866025403784439,1.,0.866025403784439,
1.,0.866025403784439,1.,0.866025403784439,1.,0.866025403784439,1.,0.866025403784439,
1.,0.866025403784439,1.,0.866025403784439,1.,0.866025403784439,1.,0.866025403784439,
1.,0.866025403784439,1.,0.866025403784439,1.,0.866025403784439,1.,0.866025403784439,
1.,0.866025403784439,1.,0.866025403784439,1.,0.866025403784439,1.,0.866025403784439,
1.,0.866025403784439,1.,0.866025403784439,1.,0.866025403784439,1.,0.866025403784439,
1.,0.866025403784439,1.,0.866025403784439,1.,0.866025403784439,1.,0.866025403784439,
1.,0.866025403784439,1.,0.866025403784439,1.,0.866025403784439,1.,0.866025403784439,
1.,0.866025403784439,1.,0.866025403784439,1.,0.866025403784439,1.,0.866025403784439,
1.,0.866025403784439,1.,0.866025403784439,1.,0.866025403784439,1.,0.866025403784439,
1.,0.866025403784439,1.,0.866025403784439,1.,0.866025403784439,1.,0.866025403784439,
1.,0.866025403784439,1.,0.866025403784439,1.,0.866025403784439,1.,0.866025403784439,
1.,0.866025403784439,1.,0.866025403784439,1.,0.866025403784439,1.,0.866025403784439,
1.,0.866025403784439,1.,0.866025403784439,1.,0.866025403784439,1.,0.866025403784439,
1.,0.866025403784439,1.,0.866025403784439,1.,0.866025403784439,1.,0.866025403784439,
1.,0.866025403784439,1.,0.866025403784439,1.,0.866025403784439,1.,0.866025403784439,
1.,0.866025403784439,1.,0.866025403784439,1.,0.866025403784439,1.,0.866025403784439,
1.,0.866025403784439,1.,0.866025403784439,1.,0.866025403784439,1.,0.866025403784439,
1.,0.866025403784439,1.,0.866025403784439,1.,0.866025403784439,1.,0.866025403784439,
1.,0.866025403784439,1.,0.866025403784439,1.,0.866025403784439,1.,0.866025403784439,
1.,0.866025403784439,1.,0.866025403784439,1.,0.866025403784439,1.,0.866025403784439,
1.,0.866025403784439,1.,0.866025403784439,1.,0.866025403784439,1.,0.866025403784439,
1.,0.866025403784439,1.,0.866025403784439,1.,0.866025403784439,1.,0.866025403784439,
1.,0.866025403784439,1.,0.866025403784439,1.,0.866025403784439,1.,0.866025403784439,
1.,0.866025403784439,1.,0.866025403784439,1.,0.866025403784439,1.,0.866025403784439,
1.,0.866025403784439,1.,0.866025403784439,1.,0.866025403784439,1.,0.866025403784439,
1.,0.866025403784439,1.,0.866025403784439,1.,0.866025403784439,1.,0.866025403784439,
1.,0.866025403784439,1.,0.866025403784439,1.,0.866025403784439,1.,0.866025403784439,
1.,0.866025403784439,1.,0.866025403784439,1.,0.866025403784439,1.,0.866025403784439,
1.,0.866025403784439,1.,0.866025403784439,1.,0.866025403784439,1.,0.866025403784439,
1.,0.866025403784439,1.,0.866025403784439,1.,0.866025403784439,1.,0.866025403784439,
1.,0.866025403784439,1.,0.866025403784439,1.,0.866025403784439,1.,0.866025403784439,
1.,0.866025403784439,1.,0.866025403784439,1.,0.866025403784439,1.,0.866025403784439,
1.,0.866025403784439,1.,0.866025403784439,1.,0.866025403784439,1.,0.866025403784439,
1.,0.866025403784439,1.,0.866025403784439,1.,0.866025403784439,1.,0.866025403784439,
1.,0.866025403784439,1.,0.866025403784439,1.,0.866025403784439,1.,0.866025403784439,
1.,0.866025403784439,1.,0.866025403784439,1.,0.866025403784439,1.,0.866025403784439,
1.,0.866025403784439,1.,0.866025403784439,1.,0.866025403784439,1.,0.866025403784439,
1.,0.866025403784439,1.,0.866025403784439,1.,0.866025403784439,1.,0.866025403784439,
1.,0.866025403784439,1.,0.866025403784439,1.,0.866025403784439,1.,0.866025403784439,
1.,0.866025403784439,1.,0.866025403784439,1.,0.866025403784439,1.,0.866025403784439,
1.,0.866025403784439,1.,0.866025403784439,1.,0.866025403784439,1.,0.866025403784439,
1.,0.866025403784439,1.,0.866025403784439,1.,0.866025403784439,1.,0.866025403784439,
1.,0.866025403784439,1.,0.866025403784439,1.,0.866025403784439,1.,0.866025403784439,
1.,0.866025403784439,1.,0.866025403784439,1.,0.866025403784439,1.)))
REPRESENTATION_ITEM('')
SURFACE()
);
#2320=(
BOUNDED_SURFACE()
B_SPLINE_SURFACE(1,2,((#379175,#379176,#379177,#379178,#379179,#379180,
#379181,#379182,#379183,#379184,#379185,#379186,#379187,#379188,#379189,
#379190,#379191,#379192,#379193,#379194,#379195,#379196,#379197,#379198,
#379199,#379200,#379201,#379202,#379203,#379204,#379205,#379206,#379207,
#379208,#379209,#379210,#379211,#379212,#379213,#379214,#379215,#379216,
#379217,#379218,#379219,#379220,#379221,#379222,#379223,#379224,#379225,
#379226,#379227,#379228,#379229,#379230,#379231,#379232,#379233,#379234,
#379235,#379236,#379237,#379238,#379239,#379240,#379241,#379242,#379243,
#379244,#379245,#379246,#379247,#379248,#379249,#379250,#379251,#379252,
#379253,#379254,#379255,#379256,#379257,#379258,#379259,#379260,#379261,
#379262,#379263,#379264,#379265,#379266,#379267,#379268,#379269,#379270,
#379271,#379272,#379273,#379274,#379275,#379276,#379277,#379278,#379279,
#379280,#379281,#379282,#379283,#379284,#379285,#379286,#379287,#379288,
#379289,#379290,#379291,#379292,#379293,#379294,#379295,#379296,#379297,
#379298,#379299,#379300,#379301,#379302,#379303,#379304,#379305,#379306,
#379307,#379308,#379309,#379310,#379311,#379312,#379313,#379314,#379315,
#379316,#379317,#379318,#379319,#379320,#379321,#379322,#379323,#379324,
#379325,#379326,#379327,#379328,#379329,#379330,#379331,#379332,#379333,
#379334,#379335,#379336,#379337,#379338,#379339,#379340,#379341,#379342,
#379343,#379344,#379345,#379346,#379347,#379348,#379349,#379350,#379351,
#379352,#379353,#379354,#379355,#379356,#379357,#379358,#379359,#379360,
#379361,#379362,#379363,#379364,#379365,#379366,#379367,#379368,#379369,
#379370,#379371,#379372,#379373,#379374,#379375,#379376,#379377,#379378,
#379379,#379380,#379381,#379382,#379383,#379384,#379385,#379386,#379387,
#379388,#379389,#379390,#379391,#379392,#379393,#379394,#379395,#379396,
#379397,#379398,#379399,#379400,#379401,#379402,#379403,#379404,#379405,
#379406,#379407,#379408,#379409,#379410,#379411,#379412,#379413,#379414,
#379415,#379416,#379417,#379418,#379419,#379420,#379421,#379422,#379423,
#379424,#379425,#379426,#379427,#379428,#379429,#379430,#379431,#379432,
#379433,#379434,#379435,#379436,#379437,#379438,#379439,#379440,#379441,
#379442,#379443,#379444,#379445,#379446,#379447,#379448,#379449,#379450,
#379451,#379452,#379453,#379454,#379455,#379456,#379457,#379458,#379459,
#379460,#379461,#379462,#379463,#379464,#379465,#379466,#379467,#379468,
#379469,#379470,#379471,#379472,#379473,#379474,#379475,#379476,#379477,
#379478,#379479,#379480,#379481,#379482,#379483,#379484,#379485,#379486,
#379487,#379488,#379489,#379490,#379491,#379492,#379493,#379494,#379495,
#379496,#379497,#379498,#379499,#379500,#379501,#379502,#379503,#379504,
#379505,#379506,#379507,#379508,#379509,#379510,#379511,#379512,#379513,
#379514,#379515,#379516,#379517,#379518,#379519,#379520,#379521,#379522,
#379523,#379524,#379525,#379526,#379527,#379528,#379529,#379530,#379531,
#379532,#379533,#379534,#379535,#379536,#379537,#379538,#379539,#379540,
#379541,#379542,#379543,#379544,#379545,#379546,#379547),(#379548,#379549,
#379550,#379551,#379552,#379553,#379554,#379555,#379556,#379557,#379558,
#379559,#379560,#379561,#379562,#379563,#379564,#379565,#379566,#379567,
#379568,#379569,#379570,#379571,#379572,#379573,#379574,#379575,#379576,
#379577,#379578,#379579,#379580,#379581,#379582,#379583,#379584,#379585,
#379586,#379587,#379588,#379589,#379590,#379591,#379592,#379593,#379594,
#379595,#379596,#379597,#379598,#379599,#379600,#379601,#379602,#379603,
#379604,#379605,#379606,#379607,#379608,#379609,#379610,#379611,#379612,
#379613,#379614,#379615,#379616,#379617,#379618,#379619,#379620,#379621,
#379622,#379623,#379624,#379625,#379626,#379627,#379628,#379629,#379630,
#379631,#379632,#379633,#379634,#379635,#379636,#379637,#379638,#379639,
#379640,#379641,#379642,#379643,#379644,#379645,#379646,#379647,#379648,
#379649,#379650,#379651,#379652,#379653,#379654,#379655,#379656,#379657,
#379658,#379659,#379660,#379661,#379662,#379663,#379664,#379665,#379666,
#379667,#379668,#379669,#379670,#379671,#379672,#379673,#379674,#379675,
#379676,#379677,#379678,#379679,#379680,#379681,#379682,#379683,#379684,
#379685,#379686,#379687,#379688,#379689,#379690,#379691,#379692,#379693,
#379694,#379695,#379696,#379697,#379698,#379699,#379700,#379701,#379702,
#379703,#379704,#379705,#379706,#379707,#379708,#379709,#379710,#379711,
#379712,#379713,#379714,#379715,#379716,#379717,#379718,#379719,#379720,
#379721,#379722,#379723,#379724,#379725,#379726,#379727,#379728,#379729,
#379730,#379731,#379732,#379733,#379734,#379735,#379736,#379737,#379738,
#379739,#379740,#379741,#379742,#379743,#379744,#379745,#379746,#379747,
#379748,#379749,#379750,#379751,#379752,#379753,#379754,#379755,#379756,
#379757,#379758,#379759,#379760,#379761,#379762,#379763,#379764,#379765,
#379766,#379767,#379768,#379769,#379770,#379771,#379772,#379773,#379774,
#379775,#379776,#379777,#379778,#379779,#379780,#379781,#379782,#379783,
#379784,#379785,#379786,#379787,#379788,#379789,#379790,#379791,#379792,
#379793,#379794,#379795,#379796,#379797,#379798,#379799,#379800,#379801,
#379802,#379803,#379804,#379805,#379806,#379807,#379808,#379809,#379810,
#379811,#379812,#379813,#379814,#379815,#379816,#379817,#379818,#379819,
#379820,#379821,#379822,#379823,#379824,#379825,#379826,#379827,#379828,
#379829,#379830,#379831,#379832,#379833,#379834,#379835,#379836,#379837,
#379838,#379839,#379840,#379841,#379842,#379843,#379844,#379845,#379846,
#379847,#379848,#379849,#379850,#379851,#379852,#379853,#379854,#379855,
#379856,#379857,#379858,#379859,#379860,#379861,#379862,#379863,#379864,
#379865,#379866,#379867,#379868,#379869,#379870,#379871,#379872,#379873,
#379874,#379875,#379876,#379877,#379878,#379879,#379880,#379881,#379882,
#379883,#379884,#379885,#379886,#379887,#379888,#379889,#379890,#379891,
#379892,#379893,#379894,#379895,#379896,#379897,#379898,#379899,#379900,
#379901,#379902,#379903,#379904,#379905,#379906,#379907,#379908,#379909,
#379910,#379911,#379912,#379913,#379914,#379915,#379916,#379917,#379918,
#379919,#379920)),.UNSPECIFIED.,.F.,.F.,.F.)
B_SPLINE_SURFACE_WITH_KNOTS((2,2),(3,2,2,2,2,2,2,2,2,2,2,2,2,2,2,2,2,2,
2,2,2,2,2,2,2,2,2,2,2,2,2,2,2,2,2,2,2,2,2,2,2,2,2,2,2,2,2,2,2,2,2,2,2,2,
2,2,2,2,2,2,2,2,2,2,2,2,2,2,2,2,2,2,2,2,2,2,2,2,2,2,2,2,2,2,2,2,2,2,2,2,
2,2,2,2,2,2,2,2,2,2,2,2,2,2,2,2,2,2,2,2,2,2,2,2,2,2,2,2,2,2,2,2,2,2,2,2,
2,2,2,2,2,2,2,2,2,2,2,2,2,2,2,2,2,2,2,2,2,2,2,2,2,2,2,2,2,2,2,2,2,2,2,2,
2,2,2,2,2,2,2,2,2,2,2,2,2,2,2,2,2,2,2,2,2,2,2,2,3),(0.,1.00002458575229),
(0.,0.00537634408602151,0.010752688172043,0.0161290322580645,0.021505376344086,
0.0268817204301075,0.032258064516129,0.0376344086021505,0.043010752688172,
0.0483870967741935,0.0537634408602151,0.0591397849462366,0.0645161290322581,
0.0698924731182796,0.0752688172043011,0.0806451612903226,0.0860215053763441,
0.0913978494623656,0.0967741935483871,0.102150537634409,0.10752688172043,
0.112903225806452,0.118279569892473,0.123655913978495,0.129032258064516,
0.134408602150538,0.139784946236559,0.145161290322581,0.150537634408602,
0.155913978494624,0.161290322580645,0.166666666666667,0.172043010752688,
0.17741935483871,0.182795698924731,0.188172043010753,0.193548387096774,
0.198924731182796,0.204301075268817,0.209677419354839,0.21505376344086,
0.220430107526882,0.225806451612903,0.231182795698925,0.236559139784946,
0.241935483870968,0.247311827956989,0.252688172043011,0.258064516129032,
0.263440860215054,0.268817204301075,0.274193548387097,0.279569892473118,
0.28494623655914,0.290322580645161,0.295698924731183,0.301075268817204,
0.306451612903226,0.311827956989247,0.317204301075269,0.32258064516129,
0.327956989247312,0.333333333333333,0.338709677419355,0.344086021505376,
0.349462365591398,0.354838709677419,0.360215053763441,0.365591397849462,
0.370967741935484,0.376344086021505,0.381720430107527,0.387096774193548,
0.39247311827957,0.397849462365591,0.403225806451613,0.408602150537634,
0.413978494623656,0.419354838709677,0.424731182795699,0.43010752688172,
0.435483870967742,0.440860215053763,0.446236559139785,0.451612903225806,
0.456989247311828,0.462365591397849,0.467741935483871,0.473118279569892,
0.478494623655914,0.483870967741935,0.489247311827957,0.494623655913978,
0.5,0.505376344086022,0.510752688172043,0.516129032258065,0.521505376344086,
0.526881720430108,0.532258064516129,0.537634408602151,0.543010752688172,
0.548387096774194,0.553763440860215,0.559139784946237,0.564516129032258,
0.56989247311828,0.575268817204301,0.580645161290323,0.586021505376344,
0.591397849462366,0.596774193548387,0.602150537634409,0.60752688172043,
0.612903225806452,0.618279569892473,0.623655913978495,0.629032258064516,
0.634408602150538,0.639784946236559,0.645161290322581,0.650537634408602,
0.655913978494624,0.661290322580645,0.666666666666667,0.672043010752688,
0.67741935483871,0.682795698924731,0.688172043010753,0.693548387096774,
0.698924731182796,0.704301075268817,0.709677419354839,0.71505376344086,
0.720430107526882,0.725806451612903,0.731182795698925,0.736559139784946,
0.741935483870968,0.747311827956989,0.752688172043011,0.758064516129032,
0.763440860215054,0.768817204301075,0.774193548387097,0.779569892473118,
0.78494623655914,0.790322580645161,0.795698924731183,0.801075268817204,
0.806451612903226,0.811827956989247,0.817204301075269,0.82258064516129,
0.827956989247312,0.833333333333333,0.838709677419355,0.844086021505376,
0.849462365591398,0.854838709677419,0.860215053763441,0.865591397849462,
0.870967741935484,0.876344086021505,0.881720430107527,0.887096774193548,
0.89247311827957,0.897849462365591,0.903225806451613,0.908602150537634,
0.913978494623656,0.919354838709677,0.924731182795699,0.93010752688172,
0.935483870967742,0.940860215053763,0.946236559139785,0.951612903225806,
0.956989247311828,0.962365591397849,0.967741935483871,0.973118279569892,
0.978494623655914,0.983870967741935,0.989247311827957,0.994623655913978,
1.),.UNSPECIFIED.)
GEOMETRIC_REPRESENTATION_ITEM()
RATIONAL_B_SPLINE_SURFACE(((1.,0.866025403784439,1.,0.866025403784439,1.,
0.866025403784439,1.,0.866025403784439,1.,0.866025403784439,1.,0.866025403784439,
1.,0.866025403784439,1.,0.866025403784439,1.,0.866025403784439,1.,0.866025403784439,
1.,0.866025403784439,1.,0.866025403784439,1.,0.866025403784439,1.,0.866025403784439,
1.,0.866025403784439,1.,0.866025403784439,1.,0.866025403784439,1.,0.866025403784439,
1.,0.866025403784439,1.,0.866025403784439,1.,0.866025403784439,1.,0.866025403784439,
1.,0.866025403784439,1.,0.866025403784439,1.,0.866025403784439,1.,0.866025403784439,
1.,0.866025403784439,1.,0.866025403784439,1.,0.866025403784439,1.,0.866025403784439,
1.,0.866025403784439,1.,0.866025403784439,1.,0.866025403784439,1.,0.866025403784439,
1.,0.866025403784439,1.,0.866025403784439,1.,0.866025403784439,1.,0.866025403784439,
1.,0.866025403784439,1.,0.866025403784439,1.,0.866025403784439,1.,0.866025403784439,
1.,0.866025403784439,1.,0.866025403784439,1.,0.866025403784439,1.,0.866025403784439,
1.,0.866025403784439,1.,0.866025403784439,1.,0.866025403784439,1.,0.866025403784439,
1.,0.866025403784439,1.,0.866025403784439,1.,0.866025403784439,1.,0.866025403784439,
1.,0.866025403784439,1.,0.866025403784439,1.,0.866025403784439,1.,0.866025403784439,
1.,0.866025403784439,1.,0.866025403784439,1.,0.866025403784439,1.,0.866025403784439,
1.,0.866025403784439,1.,0.866025403784439,1.,0.866025403784439,1.,0.866025403784439,
1.,0.866025403784439,1.,0.866025403784439,1.,0.866025403784439,1.,0.866025403784439,
1.,0.866025403784439,1.,0.866025403784439,1.,0.866025403784439,1.,0.866025403784439,
1.,0.866025403784439,1.,0.866025403784439,1.,0.866025403784439,1.,0.866025403784439,
1.,0.866025403784439,1.,0.866025403784439,1.,0.866025403784439,1.,0.866025403784439,
1.,0.866025403784439,1.,0.866025403784439,1.,0.866025403784439,1.,0.866025403784439,
1.,0.866025403784439,1.,0.866025403784439,1.,0.866025403784439,1.,0.866025403784439,
1.,0.866025403784439,1.,0.866025403784439,1.,0.866025403784439,1.,0.866025403784439,
1.,0.866025403784439,1.,0.866025403784439,1.,0.866025403784439,1.,0.866025403784439,
1.,0.866025403784439,1.,0.866025403784439,1.,0.866025403784439,1.,0.866025403784439,
1.,0.866025403784439,1.,0.866025403784439,1.,0.866025403784439,1.,0.866025403784439,
1.,0.866025403784439,1.,0.866025403784439,1.,0.866025403784439,1.,0.866025403784439,
1.,0.866025403784439,1.,0.866025403784439,1.,0.866025403784439,1.,0.866025403784439,
1.,0.866025403784439,1.,0.866025403784439,1.,0.866025403784439,1.,0.866025403784439,
1.,0.866025403784439,1.,0.866025403784439,1.,0.866025403784439,1.,0.866025403784439,
1.,0.866025403784439,1.,0.866025403784439,1.,0.866025403784439,1.,0.866025403784439,
1.,0.866025403784439,1.,0.866025403784439,1.,0.866025403784439,1.,0.866025403784439,
1.,0.866025403784439,1.,0.866025403784439,1.,0.866025403784439,1.,0.866025403784439,
1.,0.866025403784439,1.,0.866025403784439,1.,0.866025403784439,1.,0.866025403784439,
1.,0.866025403784439,1.,0.866025403784439,1.,0.866025403784439,1.,0.866025403784439,
1.,0.866025403784439,1.,0.866025403784439,1.,0.866025403784439,1.,0.866025403784439,
1.,0.866025403784439,1.,0.866025403784439,1.,0.866025403784439,1.,0.866025403784439,
1.,0.866025403784439,1.,0.866025403784439,1.,0.866025403784439,1.,0.866025403784439,
1.,0.866025403784439,1.,0.866025403784439,1.,0.866025403784439,1.,0.866025403784439,
1.,0.866025403784439,1.,0.866025403784439,1.,0.866025403784439,1.,0.866025403784439,
1.,0.866025403784439,1.,0.866025403784439,1.,0.866025403784439,1.,0.866025403784439,
1.,0.866025403784439,1.,0.866025403784439,1.,0.866025403784439,1.,0.866025403784439,
1.,0.866025403784439,1.,0.866025403784439,1.,0.866025403784439,1.,0.866025403784439,
1.,0.866025403784439,1.,0.866025403784439,1.,0.866025403784439,1.,0.866025403784439,
1.,0.866025403784439,1.,0.866025403784439,1.,0.866025403784439,1.,0.866025403784439,
1.,0.866025403784439,1.,0.866025403784439,1.,0.866025403784439,1.,0.866025403784439,
1.),(1.,0.866025403784439,1.,0.866025403784439,1.,0.866025403784439,1.,
0.866025403784439,1.,0.866025403784439,1.,0.866025403784439,1.,0.866025403784439,
1.,0.866025403784439,1.,0.866025403784439,1.,0.866025403784439,1.,0.866025403784439,
1.,0.866025403784439,1.,0.866025403784439,1.,0.866025403784439,1.,0.866025403784439,
1.,0.866025403784439,1.,0.866025403784439,1.,0.866025403784439,1.,0.866025403784439,
1.,0.866025403784439,1.,0.866025403784439,1.,0.866025403784439,1.,0.866025403784439,
1.,0.866025403784439,1.,0.866025403784439,1.,0.866025403784439,1.,0.866025403784439,
1.,0.866025403784439,1.,0.866025403784439,1.,0.866025403784439,1.,0.866025403784439,
1.,0.866025403784439,1.,0.866025403784439,1.,0.866025403784439,1.,0.866025403784439,
1.,0.866025403784439,1.,0.866025403784439,1.,0.866025403784439,1.,0.866025403784439,
1.,0.866025403784439,1.,0.866025403784439,1.,0.866025403784439,1.,0.866025403784439,
1.,0.866025403784439,1.,0.866025403784439,1.,0.866025403784439,1.,0.866025403784439,
1.,0.866025403784439,1.,0.866025403784439,1.,0.866025403784439,1.,0.866025403784439,
1.,0.866025403784439,1.,0.866025403784439,1.,0.866025403784439,1.,0.866025403784439,
1.,0.866025403784439,1.,0.866025403784439,1.,0.866025403784439,1.,0.866025403784439,
1.,0.866025403784439,1.,0.866025403784439,1.,0.866025403784439,1.,0.866025403784439,
1.,0.866025403784439,1.,0.866025403784439,1.,0.866025403784439,1.,0.866025403784439,
1.,0.866025403784439,1.,0.866025403784439,1.,0.866025403784439,1.,0.866025403784439,
1.,0.866025403784439,1.,0.866025403784439,1.,0.866025403784439,1.,0.866025403784439,
1.,0.866025403784439,1.,0.866025403784439,1.,0.866025403784439,1.,0.866025403784439,
1.,0.866025403784439,1.,0.866025403784439,1.,0.866025403784439,1.,0.866025403784439,
1.,0.866025403784439,1.,0.866025403784439,1.,0.866025403784439,1.,0.866025403784439,
1.,0.866025403784439,1.,0.866025403784439,1.,0.866025403784439,1.,0.866025403784439,
1.,0.866025403784439,1.,0.866025403784439,1.,0.866025403784439,1.,0.866025403784439,
1.,0.866025403784439,1.,0.866025403784439,1.,0.866025403784439,1.,0.866025403784439,
1.,0.866025403784439,1.,0.866025403784439,1.,0.866025403784439,1.,0.866025403784439,
1.,0.866025403784439,1.,0.866025403784439,1.,0.866025403784439,1.,0.866025403784439,
1.,0.866025403784439,1.,0.866025403784439,1.,0.866025403784439,1.,0.866025403784439,
1.,0.866025403784439,1.,0.866025403784439,1.,0.866025403784439,1.,0.866025403784439,
1.,0.866025403784439,1.,0.866025403784439,1.,0.866025403784439,1.,0.866025403784439,
1.,0.866025403784439,1.,0.866025403784439,1.,0.866025403784439,1.,0.866025403784439,
1.,0.866025403784439,1.,0.866025403784439,1.,0.866025403784439,1.,0.866025403784439,
1.,0.866025403784439,1.,0.866025403784439,1.,0.866025403784439,1.,0.866025403784439,
1.,0.866025403784439,1.,0.866025403784439,1.,0.866025403784439,1.,0.866025403784439,
1.,0.866025403784439,1.,0.866025403784439,1.,0.866025403784439,1.,0.866025403784439,
1.,0.866025403784439,1.,0.866025403784439,1.,0.866025403784439,1.,0.866025403784439,
1.,0.866025403784439,1.,0.866025403784439,1.,0.866025403784439,1.,0.866025403784439,
1.,0.866025403784439,1.,0.866025403784439,1.,0.866025403784439,1.,0.866025403784439,
1.,0.866025403784439,1.,0.866025403784439,1.,0.866025403784439,1.,0.866025403784439,
1.,0.866025403784439,1.,0.866025403784439,1.,0.866025403784439,1.,0.866025403784439,
1.,0.866025403784439,1.,0.866025403784439,1.,0.866025403784439,1.,0.866025403784439,
1.,0.866025403784439,1.,0.866025403784439,1.,0.866025403784439,1.,0.866025403784439,
1.,0.866025403784439,1.,0.866025403784439,1.,0.866025403784439,1.,0.866025403784439,
1.,0.866025403784439,1.,0.866025403784439,1.,0.866025403784439,1.,0.866025403784439,
1.,0.866025403784439,1.,0.866025403784439,1.,0.866025403784439,1.,0.866025403784439,
1.,0.866025403784439,1.,0.866025403784439,1.,0.866025403784439,1.,0.866025403784439,
1.,0.866025403784439,1.,0.866025403784439,1.,0.866025403784439,1.)))
REPRESENTATION_ITEM('')
SURFACE()
);
#2321=(
BOUNDED_SURFACE()
B_SPLINE_SURFACE(3,2,((#379934,#379935,#379936),(#379937,#379938,#379939),
(#379940,#379941,#379942),(#379943,#379944,#379945)),.UNSPECIFIED.,.F.,
 .F.,.F.)
B_SPLINE_SURFACE_WITH_KNOTS((4,4),(3,3),(0.00135801595889393,0.00148409170619832),
(0.,1.),.UNSPECIFIED.)
GEOMETRIC_REPRESENTATION_ITEM()
RATIONAL_B_SPLINE_SURFACE(((1.,0.818301933966443,1.),(1.,0.817226613172337,
1.),(1.,0.816179643373948,1.),(1.,0.815159387863655,1.)))
REPRESENTATION_ITEM('')
SURFACE()
);
#2322=(
BOUNDED_SURFACE()
B_SPLINE_SURFACE(3,2,((#379981,#379982,#379983),(#379984,#379985,#379986),
(#379987,#379988,#379989),(#379990,#379991,#379992)),.UNSPECIFIED.,.F.,
 .F.,.F.)
B_SPLINE_SURFACE_WITH_KNOTS((4,4),(3,3),(-1.54744435122076E-6,1.54744435122076E-5),
(-0.0151698983610561,1.),.UNSPECIFIED.)
GEOMETRIC_REPRESENTATION_ITEM()
RATIONAL_B_SPLINE_SURFACE(((1.02018382472812,0.334740937357287,1.),(1.00401234488797,
0.867753072813418,1.),(1.00033622856778,0.988917903080862,1.),(1.,1.,1.)))
REPRESENTATION_ITEM('')
SURFACE()
);
#2323=(
BOUNDED_SURFACE()
B_SPLINE_SURFACE(3,2,((#379994,#379995,#379996),(#379997,#379998,#379999),
(#380000,#380001,#380002),(#380003,#380004,#380005)),.UNSPECIFIED.,.F.,
 .F.,.F.)
B_SPLINE_SURFACE_WITH_KNOTS((4,4),(3,3),(1.55009486301137E-5,4.92065510474431E-5),
(-8.13759512746712E-5,1.),.UNSPECIFIED.)
GEOMETRIC_REPRESENTATION_ITEM()
RATIONAL_B_SPLINE_SURFACE(((1.0000237291233,0.85420063959972,1.),(1.0000142358599,
0.912530301180549,1.),(1.00000710550469,0.956341495377441,1.),(1.00001238975905,
0.923873338137039,1.)))
REPRESENTATION_ITEM('')
SURFACE()
);
#2324=(
BOUNDED_SURFACE()
B_SPLINE_SURFACE(3,2,((#380007,#380008,#380009),(#380010,#380011,#380012),
(#380013,#380014,#380015),(#380016,#380017,#380018)),.UNSPECIFIED.,.F.,
 .F.,.F.)
B_SPLINE_SURFACE_WITH_KNOTS((4,4),(3,3),(-3.39934179457821E-6,3.73927597403565E-5),
(-0.00186004067418894,1.00069373317436),.UNSPECIFIED.)
GEOMETRIC_REPRESENTATION_ITEM()
RATIONAL_B_SPLINE_SURFACE(((1.00072100136055,0.806051963875345,1.0002685964269),
(1.00060048440154,0.838470803558665,1.00022369994495),(1.00053106448795,
0.857144632272366,1.00019783877218),(1.00054515072852,0.853355459539107,
1.00020308635436)))
REPRESENTATION_ITEM('')
SURFACE()
);
#2325=(
BOUNDED_SURFACE()
B_SPLINE_SURFACE(3,2,((#380020,#380021,#380022),(#380023,#380024,#380025),
(#380026,#380027,#380028),(#380029,#380030,#380031)),.UNSPECIFIED.,.F.,
 .F.,.F.)
B_SPLINE_SURFACE_WITH_KNOTS((4,4),(3,3),(0.00137194782501028,0.00149814269699235),
(0.,1.),.UNSPECIFIED.)
GEOMETRIC_REPRESENTATION_ITEM()
RATIONAL_B_SPLINE_SURFACE(((1.,0.815158509402307,1.),(1.,0.816179044148172,
1.),(1.,0.817226308119919,1.),(1.,0.818301939488809,1.)))
REPRESENTATION_ITEM('')
SURFACE()
);
#2326=(
BOUNDED_SURFACE()
B_SPLINE_SURFACE(3,2,((#380068,#380069,#380070),(#380071,#380072,#380073),
(#380074,#380075,#380076),(#380077,#380078,#380079)),.UNSPECIFIED.,.F.,
 .F.,.F.)
B_SPLINE_SURFACE_WITH_KNOTS((4,4),(3,3),(0.,9.54361881492174E-5),(0.,1.),
 .UNSPECIFIED.)
GEOMETRIC_REPRESENTATION_ITEM()
RATIONAL_B_SPLINE_SURFACE(((1.,0.816715621142057,1.),(1.,0.815907587407932,
1.),(1.,0.81511595934521,1.),(1.,0.814339887349193,1.)))
REPRESENTATION_ITEM('')
SURFACE()
);
#2327=(
BOUNDED_SURFACE()
B_SPLINE_SURFACE(3,2,((#380081,#380082,#380083),(#380084,#380085,#380086),
(#380087,#380088,#380089),(#380090,#380091,#380092)),.UNSPECIFIED.,.F.,
 .F.,.F.)
B_SPLINE_SURFACE_WITH_KNOTS((4,4),(3,3),(2.02993869230509E-5,5.39756952686906E-5),
(-0.000116281069492499,1.),.UNSPECIFIED.)
GEOMETRIC_REPRESENTATION_ITEM()
RATIONAL_B_SPLINE_SURFACE(((1.00001770479723,0.923870681143041,1.),(1.00001014104055,
0.956394275543438,1.),(1.00002037300271,0.912397594905722,1.),(1.00003390859456,
0.85419555086991,1.)))
REPRESENTATION_ITEM('')
SURFACE()
);
#2328=(
BOUNDED_SURFACE()
B_SPLINE_SURFACE(3,2,((#380094,#380095,#380096),(#380097,#380098,#380099),
(#380100,#380101,#380102),(#380103,#380104,#380105)),.UNSPECIFIED.,.F.,
 .F.,.F.)
B_SPLINE_SURFACE_WITH_KNOTS((4,4),(3,3),(0.,4.68197758448209E-5),(0.,1.),
 .UNSPECIFIED.)
GEOMETRIC_REPRESENTATION_ITEM()
RATIONAL_B_SPLINE_SURFACE(((1.,0.816715621142057,1.),(1.,0.953638980025206,
1.),(1.,0.954506925408047,1.),(1.,0.816715621142055,1.)))
REPRESENTATION_ITEM('')
SURFACE()
);
#2329=(
BOUNDED_SURFACE()
B_SPLINE_SURFACE(3,2,((#380109,#380110,#380111),(#380112,#380113,#380114),
(#380115,#380116,#380117),(#380118,#380119,#380120)),.UNSPECIFIED.,.F.,
 .F.,.F.)
B_SPLINE_SURFACE_WITH_KNOTS((4,4),(3,3),(0.,9.54361881492177E-5),(0.,1.),
 .UNSPECIFIED.)
GEOMETRIC_REPRESENTATION_ITEM()
RATIONAL_B_SPLINE_SURFACE(((1.,0.814339887349193,1.),(1.,0.815115959345207,
1.),(1.,0.815907587407933,1.),(1.,0.816715621142057,1.)))
REPRESENTATION_ITEM('')
SURFACE()
);
#2330=(
BOUNDED_SURFACE()
B_SPLINE_SURFACE(3,2,((#380122,#380123,#380124),(#380125,#380126,#380127),
(#380128,#380129,#380130),(#380131,#380132,#380133)),.UNSPECIFIED.,.F.,
 .F.,.F.)
B_SPLINE_SURFACE_WITH_KNOTS((4,4),(3,3),(-3.39528393502487E-6,3.73481232852736E-5),
(-0.0016501803328463,1.),.UNSPECIFIED.)
GEOMETRIC_REPRESENTATION_ITEM()
RATIONAL_B_SPLINE_SURFACE(((1.00048354385553,0.853487571660461,1.),(1.00047110510908,
0.857256476851525,1.),(1.00053193201093,0.83882609665593,1.),(1.00063970687709,
0.806170615310181,1.)))
REPRESENTATION_ITEM('')
SURFACE()
);
#2331=(
BOUNDED_SURFACE()
B_SPLINE_SURFACE(3,2,((#380225,#380226,#380227),(#380228,#380229,#380230),
(#380231,#380232,#380233),(#380234,#380235,#380236)),.UNSPECIFIED.,.F.,
 .F.,.F.)
B_SPLINE_SURFACE_WITH_KNOTS((4,4),(3,3),(0.00135801595889393,0.00148409170619832),
(0.,1.),.UNSPECIFIED.)
GEOMETRIC_REPRESENTATION_ITEM()
RATIONAL_B_SPLINE_SURFACE(((1.,0.818301933966445,1.),(1.,0.817226613172352,
1.),(1.,0.816179643373942,1.),(1.,0.815159387863666,1.)))
REPRESENTATION_ITEM('')
SURFACE()
);
#2332=(
BOUNDED_SURFACE()
B_SPLINE_SURFACE(3,2,((#380275,#380276,#380277),(#380278,#380279,#380280),
(#380281,#380282,#380283),(#380284,#380285,#380286)),.UNSPECIFIED.,.F.,
 .F.,.F.)
B_SPLINE_SURFACE_WITH_KNOTS((4,4),(3,3),(-1.54744435122067E-6,1.54744435122073E-5),
(-0.015169898363932,1.),.UNSPECIFIED.)
GEOMETRIC_REPRESENTATION_ITEM()
RATIONAL_B_SPLINE_SURFACE(((1.02018382473201,0.334740937355304,1.),(1.00401234488873,
0.867753072813129,1.),(1.00033622856785,0.988917903080821,1.),(1.,1.,1.)))
REPRESENTATION_ITEM('')
SURFACE()
);
#2333=(
BOUNDED_SURFACE()
B_SPLINE_SURFACE(3,2,((#380288,#380289,#380290),(#380291,#380292,#380293),
(#380294,#380295,#380296),(#380297,#380298,#380299)),.UNSPECIFIED.,.F.,
 .F.,.F.)
B_SPLINE_SURFACE_WITH_KNOTS((4,4),(3,3),(0.00137194782501028,0.00149814269699235),
(0.,1.),.UNSPECIFIED.)
GEOMETRIC_REPRESENTATION_ITEM()
RATIONAL_B_SPLINE_SURFACE(((1.,0.815158509402316,1.),(1.,0.816179044148162,
1.),(1.,0.817226308119924,1.),(1.,0.818301939488816,1.)))
REPRESENTATION_ITEM('')
SURFACE()
);
#2334=(
BOUNDED_SURFACE()
B_SPLINE_SURFACE(3,2,((#380343,#380344,#380345),(#380346,#380347,#380348),
(#380349,#380350,#380351),(#380352,#380353,#380354)),.UNSPECIFIED.,.F.,
 .F.,.F.)
B_SPLINE_SURFACE_WITH_KNOTS((4,4),(3,3),(1.55009486301137E-5,4.92065510474432E-5),
(-8.13759515860464E-5,1.),.UNSPECIFIED.)
GEOMETRIC_REPRESENTATION_ITEM()
RATIONAL_B_SPLINE_SURFACE(((1.00002372912339,0.854200639599671,1.),(1.00001423585995,
0.91253030118053,1.),(1.00000710550472,0.956341495377424,1.),(1.0000123897591,
0.923873338137017,1.)))
REPRESENTATION_ITEM('')
SURFACE()
);
#2335=(
BOUNDED_SURFACE()
B_SPLINE_SURFACE(3,2,((#380358,#380359,#380360),(#380361,#380362,#380363),
(#380364,#380365,#380366),(#380367,#380368,#380369)),.UNSPECIFIED.,.F.,
 .F.,.F.)
B_SPLINE_SURFACE_WITH_KNOTS((4,4),(3,3),(-3.3993417945781E-6,3.73927597403567E-5),
(-0.00186004067406598,1.00069373317433),.UNSPECIFIED.)
GEOMETRIC_REPRESENTATION_ITEM()
RATIONAL_B_SPLINE_SURFACE(((1.0007210013605,0.806051963875402,1.00026859642688),
(1.0006004844015,0.838470803558646,1.00022369994494),(1.00053106448791,
0.85714463227243,1.00019783877218),(1.00054515072849,0.853355459539126,
1.00020308635435)))
REPRESENTATION_ITEM('')
SURFACE()
);
#2336=(
BOUNDED_SURFACE()
B_SPLINE_SURFACE(3,2,((#380371,#380372,#380373),(#380374,#380375,#380376),
(#380377,#380378,#380379),(#380380,#380381,#380382)),.UNSPECIFIED.,.F.,
 .F.,.F.)
B_SPLINE_SURFACE_WITH_KNOTS((4,4),(3,3),(1.62630325872826E-19,9.54361881492175E-5),
(0.,1.),.UNSPECIFIED.)
GEOMETRIC_REPRESENTATION_ITEM()
RATIONAL_B_SPLINE_SURFACE(((1.,0.816715621142059,1.),(1.,0.815907587407935,
1.),(1.,0.815115959345216,1.),(1.,0.814339887349207,1.)))
REPRESENTATION_ITEM('')
SURFACE()
);
#2337=(
BOUNDED_SURFACE()
B_SPLINE_SURFACE(3,2,((#380384,#380385,#380386),(#380387,#380388,#380389),
(#380390,#380391,#380392),(#380393,#380394,#380395)),.UNSPECIFIED.,.F.,
 .F.,.F.)
B_SPLINE_SURFACE_WITH_KNOTS((4,4),(3,3),(9.48676900924816E-20,4.68197758448212E-5),
(0.,1.),.UNSPECIFIED.)
GEOMETRIC_REPRESENTATION_ITEM()
RATIONAL_B_SPLINE_SURFACE(((1.,0.81671562114204,1.),(1.,0.953638980025222,
1.),(1.,0.954506925408046,1.),(1.,0.816715621142051,1.)))
REPRESENTATION_ITEM('')
SURFACE()
);
#2338=(
BOUNDED_SURFACE()
B_SPLINE_SURFACE(3,2,((#380397,#380398,#380399),(#380400,#380401,#380402),
(#380403,#380404,#380405),(#380406,#380407,#380408)),.UNSPECIFIED.,.F.,
 .F.,.F.)
B_SPLINE_SURFACE_WITH_KNOTS((4,4),(3,3),(5.42101086242752E-20,9.54361881492177E-5),
(0.,1.),.UNSPECIFIED.)
GEOMETRIC_REPRESENTATION_ITEM()
RATIONAL_B_SPLINE_SURFACE(((1.,0.814339887349192,1.),(1.,0.815115959345195,
1.),(1.,0.815907587407961,1.),(1.,0.81671562114204,1.)))
REPRESENTATION_ITEM('')
SURFACE()
);
#2339=(
BOUNDED_SURFACE()
B_SPLINE_SURFACE(3,2,((#380410,#380411,#380412),(#380413,#380414,#380415),
(#380416,#380417,#380418),(#380419,#380420,#380421)),.UNSPECIFIED.,.F.,
 .F.,.F.)
B_SPLINE_SURFACE_WITH_KNOTS((4,4),(3,3),(-3.39528393502487E-6,3.73481232852731E-5),
(-0.00165018033312054,1.),.UNSPECIFIED.)
GEOMETRIC_REPRESENTATION_ITEM()
RATIONAL_B_SPLINE_SURFACE(((1.00048354385561,0.853487571660432,1.),(1.00047110510916,
0.857256476851472,1.),(1.00053193201102,0.838826096655894,1.),(1.00063970687719,
0.806170615310123,1.)))
REPRESENTATION_ITEM('')
SURFACE()
);
#2340=(
BOUNDED_SURFACE()
B_SPLINE_SURFACE(3,2,((#380425,#380426,#380427),(#380428,#380429,#380430),
(#380431,#380432,#380433),(#380434,#380435,#380436)),.UNSPECIFIED.,.F.,
 .F.,.F.)
B_SPLINE_SURFACE_WITH_KNOTS((4,4),(3,3),(2.02993869230509E-5,5.39756952686907E-5),
(-0.000116281069872552,1.),.UNSPECIFIED.)
GEOMETRIC_REPRESENTATION_ITEM()
RATIONAL_B_SPLINE_SURFACE(((1.00001770479729,0.923870681143009,1.),(1.00001014104058,
0.956394275543428,1.),(1.00002037300278,0.912397594905674,1.),(1.00003390859467,
0.85419555086986,1.)))
REPRESENTATION_ITEM('')
SURFACE()
);
#2341=(
BOUNDED_SURFACE()
B_SPLINE_SURFACE(3,2,((#380529,#380530,#380531),(#380532,#380533,#380534),
(#380535,#380536,#380537),(#380538,#380539,#380540)),.UNSPECIFIED.,.F.,
 .F.,.F.)
B_SPLINE_SURFACE_WITH_KNOTS((4,4),(3,3),(0.00135801595889393,0.00148409170619832),
(0.,1.),.UNSPECIFIED.)
GEOMETRIC_REPRESENTATION_ITEM()
RATIONAL_B_SPLINE_SURFACE(((1.,0.818301933966445,1.),(1.,0.817226613172355,
1.),(1.,0.81617964337394,1.),(1.,0.815159387863663,1.)))
REPRESENTATION_ITEM('')
SURFACE()
);
#2342=(
BOUNDED_SURFACE()
B_SPLINE_SURFACE(3,2,((#380579,#380580,#380581),(#380582,#380583,#380584),
(#380585,#380586,#380587),(#380588,#380589,#380590)),.UNSPECIFIED.,.F.,
 .F.,.F.)
B_SPLINE_SURFACE_WITH_KNOTS((4,4),(3,3),(-1.54744435122007E-6,1.54744435122084E-5),
(-0.0151698983689038,1.),.UNSPECIFIED.)
GEOMETRIC_REPRESENTATION_ITEM()
RATIONAL_B_SPLINE_SURFACE(((1.02018382473872,0.334740937352125,1.),(1.00401234489007,
0.86775307281241,1.),(1.00033622856796,0.988917903080806,1.),(1.,1.,1.)))
REPRESENTATION_ITEM('')
SURFACE()
);
#2343=(
BOUNDED_SURFACE()
B_SPLINE_SURFACE(3,2,((#380592,#380593,#380594),(#380595,#380596,#380597),
(#380598,#380599,#380600),(#380601,#380602,#380603)),.UNSPECIFIED.,.F.,
 .F.,.F.)
B_SPLINE_SURFACE_WITH_KNOTS((4,4),(3,3),(0.00137194782501028,0.00149814269699235),
(0.,1.),.UNSPECIFIED.)
GEOMETRIC_REPRESENTATION_ITEM()
RATIONAL_B_SPLINE_SURFACE(((1.,0.815158509402318,1.),(1.,0.816179044148178,
1.),(1.,0.817226308119925,1.),(1.,0.818301939488807,1.)))
REPRESENTATION_ITEM('')
SURFACE()
);
#2344=(
BOUNDED_SURFACE()
B_SPLINE_SURFACE(3,2,((#380647,#380648,#380649),(#380650,#380651,#380652),
(#380653,#380654,#380655),(#380656,#380657,#380658)),.UNSPECIFIED.,.F.,
 .F.,.F.)
B_SPLINE_SURFACE_WITH_KNOTS((4,4),(3,3),(1.55009486301137E-5,4.92065510474435E-5),
(-8.13759514786794E-5,1.),.UNSPECIFIED.)
GEOMETRIC_REPRESENTATION_ITEM()
RATIONAL_B_SPLINE_SURFACE(((1.00002372912336,0.854200639599684,1.),(1.00001423585993,
0.912530301180555,1.),(1.00000710550471,0.956341495377423,1.),(1.00001238975908,
0.923873338137021,1.)))
REPRESENTATION_ITEM('')
SURFACE()
);
#2345=(
BOUNDED_SURFACE()
B_SPLINE_SURFACE(3,2,((#380662,#380663,#380664),(#380665,#380666,#380667),
(#380668,#380669,#380670),(#380671,#380672,#380673)),.UNSPECIFIED.,.F.,
 .F.,.F.)
B_SPLINE_SURFACE_WITH_KNOTS((4,4),(3,3),(-3.39934179457836E-6,3.73927597403564E-5),
(-0.00186004067423522,1.00069373317444),.UNSPECIFIED.)
GEOMETRIC_REPRESENTATION_ITEM()
RATIONAL_B_SPLINE_SURFACE(((1.00072100136056,0.806051963875341,1.00026859642693),
(1.00060048440156,0.838470803558606,1.00022369994497),(1.00053106448796,
0.85714463227239,1.00019783877221),(1.00054515072854,0.853355459539081,
1.00020308635438)))
REPRESENTATION_ITEM('')
SURFACE()
);
#2346=(
BOUNDED_SURFACE()
B_SPLINE_SURFACE(3,2,((#380675,#380676,#380677),(#380678,#380679,#380680),
(#380681,#380682,#380683),(#380684,#380685,#380686)),.UNSPECIFIED.,.F.,
 .F.,.F.)
B_SPLINE_SURFACE_WITH_KNOTS((4,4),(3,3),(2.71050543121376E-19,9.54361881492173E-5),
(0.,1.),.UNSPECIFIED.)
GEOMETRIC_REPRESENTATION_ITEM()
RATIONAL_B_SPLINE_SURFACE(((1.,0.816715621142052,1.),(1.,0.815907587407943,
1.),(1.,0.815115959345205,1.),(1.,0.814339887349196,1.)))
REPRESENTATION_ITEM('')
SURFACE()
);
#2347=(
BOUNDED_SURFACE()
B_SPLINE_SURFACE(3,2,((#380688,#380689,#380690),(#380691,#380692,#380693),
(#380694,#380695,#380696),(#380697,#380698,#380699)),.UNSPECIFIED.,.F.,
 .F.,.F.)
B_SPLINE_SURFACE_WITH_KNOTS((4,4),(3,3),(4.74338450462408E-20,4.6819775844821E-5),
(0.,1.),.UNSPECIFIED.)
GEOMETRIC_REPRESENTATION_ITEM()
RATIONAL_B_SPLINE_SURFACE(((1.,0.816715621142047,1.),(1.,0.953638980025206,
1.),(1.,0.954506925408053,1.),(1.,0.816715621142052,1.)))
REPRESENTATION_ITEM('')
SURFACE()
);
#2348=(
BOUNDED_SURFACE()
B_SPLINE_SURFACE(3,2,((#380701,#380702,#380703),(#380704,#380705,#380706),
(#380707,#380708,#380709),(#380710,#380711,#380712)),.UNSPECIFIED.,.F.,
 .F.,.F.)
B_SPLINE_SURFACE_WITH_KNOTS((4,4),(3,3),(-1.62630325872826E-19,9.54361881492177E-5),
(0.,1.),.UNSPECIFIED.)
GEOMETRIC_REPRESENTATION_ITEM()
RATIONAL_B_SPLINE_SURFACE(((1.,0.814339887349194,1.),(1.,0.815115959345216,
1.),(1.,0.815907587407934,1.),(1.,0.816715621142047,1.)))
REPRESENTATION_ITEM('')
SURFACE()
);
#2349=(
BOUNDED_SURFACE()
B_SPLINE_SURFACE(3,2,((#380714,#380715,#380716),(#380717,#380718,#380719),
(#380720,#380721,#380722),(#380723,#380724,#380725)),.UNSPECIFIED.,.F.,
 .F.,.F.)
B_SPLINE_SURFACE_WITH_KNOTS((4,4),(3,3),(-3.39528393502481E-6,3.73481232852726E-5),
(-0.00165018033327409,1.),.UNSPECIFIED.)
GEOMETRIC_REPRESENTATION_ITEM()
RATIONAL_B_SPLINE_SURFACE(((1.00048354385565,0.853487571660394,1.),(1.0004711051092,
0.857256476851478,1.),(1.00053193201107,0.838826096655851,1.),(1.00063970687725,
0.806170615310114,1.)))
REPRESENTATION_ITEM('')
SURFACE()
);
#2350=(
BOUNDED_SURFACE()
B_SPLINE_SURFACE(3,2,((#380729,#380730,#380731),(#380732,#380733,#380734),
(#380735,#380736,#380737),(#380738,#380739,#380740)),.UNSPECIFIED.,.F.,
 .F.,.F.)
B_SPLINE_SURFACE_WITH_KNOTS((4,4),(3,3),(2.0299386923051E-5,5.39756952687117E-5),
(-0.000116281068889452,1.),.UNSPECIFIED.)
GEOMETRIC_REPRESENTATION_ITEM()
RATIONAL_B_SPLINE_SURFACE(((1.00001770479714,0.923870681143094,1.),(1.0000101410405,
0.95639427554349,1.),(1.0000203730026,0.912397594905705,1.),(1.00003390859439,
0.85419555086989,1.)))
REPRESENTATION_ITEM('')
SURFACE()
);
#2351=(
BOUNDED_SURFACE()
B_SPLINE_SURFACE(3,2,((#380833,#380834,#380835),(#380836,#380837,#380838),
(#380839,#380840,#380841),(#380842,#380843,#380844)),.UNSPECIFIED.,.F.,
 .F.,.F.)
B_SPLINE_SURFACE_WITH_KNOTS((4,4),(3,3),(0.00135801595889393,0.00148409170619832),
(0.,1.),.UNSPECIFIED.)
GEOMETRIC_REPRESENTATION_ITEM()
RATIONAL_B_SPLINE_SURFACE(((1.,0.818301933966442,1.),(1.,0.817226613172345,
1.),(1.,0.81617964337394,1.),(1.,0.815159387863652,1.)))
REPRESENTATION_ITEM('')
SURFACE()
);
#2352=(
BOUNDED_SURFACE()
B_SPLINE_SURFACE(3,2,((#380883,#380884,#380885),(#380886,#380887,#380888),
(#380889,#380890,#380891),(#380892,#380893,#380894)),.UNSPECIFIED.,.F.,
 .F.,.F.)
B_SPLINE_SURFACE_WITH_KNOTS((4,4),(3,3),(-1.54744435122067E-6,1.54744435122072E-5),
(-0.0151698983630455,1.0151698983594),.UNSPECIFIED.)
GEOMETRIC_REPRESENTATION_ITEM()
RATIONAL_B_SPLINE_SURFACE(((1.02018382473081,0.324498219413325,1.02018382472589),
(1.00401234488849,0.865716921710696,1.00401234488751),(1.00033622856783,
0.98874727662963,1.00033622856775),(1.,1.,1.)))
REPRESENTATION_ITEM('')
SURFACE()
);
#2353=(
BOUNDED_SURFACE()
B_SPLINE_SURFACE(3,2,((#380896,#380897,#380898),(#380899,#380900,#380901),
(#380902,#380903,#380904),(#380905,#380906,#380907)),.UNSPECIFIED.,.F.,
 .F.,.F.)
B_SPLINE_SURFACE_WITH_KNOTS((4,4),(3,3),(0.00137194782501028,0.00149814269699235),
(0.,1.),.UNSPECIFIED.)
GEOMETRIC_REPRESENTATION_ITEM()
RATIONAL_B_SPLINE_SURFACE(((1.,0.815158509402329,1.),(1.,0.816179044148147,
1.),(1.,0.817226308119943,1.),(1.,0.818301939488811,1.)))
REPRESENTATION_ITEM('')
SURFACE()
);
#2354=(
BOUNDED_SURFACE()
B_SPLINE_SURFACE(3,2,((#380951,#380952,#380953),(#380954,#380955,#380956),
(#380957,#380958,#380959),(#380960,#380961,#380962)),.UNSPECIFIED.,.F.,
 .F.,.F.)
B_SPLINE_SURFACE_WITH_KNOTS((4,4),(3,3),(1.55009486301137E-5,4.9206551047443E-5),
(-8.13759513938222E-5,1.),.UNSPECIFIED.)
GEOMETRIC_REPRESENTATION_ITEM()
RATIONAL_B_SPLINE_SURFACE(((1.00002372912333,0.854200639599693,1.),(1.00001423585992,
0.912530301180551,1.),(1.0000071055047,0.956341495377431,1.),(1.00001238975907,
0.923873338137031,1.)))
REPRESENTATION_ITEM('')
SURFACE()
);
#2355=(
BOUNDED_SURFACE()
B_SPLINE_SURFACE(3,2,((#380966,#380967,#380968),(#380969,#380970,#380971),
(#380972,#380973,#380974),(#380975,#380976,#380977)),.UNSPECIFIED.,.F.,
 .F.,.F.)
B_SPLINE_SURFACE_WITH_KNOTS((4,4),(3,3),(-3.39934179457771E-6,3.73927597403564E-5),
(-0.00186004067387202,1.00069373317419),.UNSPECIFIED.)
GEOMETRIC_REPRESENTATION_ITEM()
RATIONAL_B_SPLINE_SURFACE(((1.00072100136042,0.806051963875442,1.00026859642683),
(1.00060048440144,0.838470803558734,1.00022369994489),(1.00053106448786,
0.857144632272446,1.00019783877213),(1.00054515072843,0.853355459539176,
1.00020308635431)))
REPRESENTATION_ITEM('')
SURFACE()
);
#2356=(
BOUNDED_SURFACE()
B_SPLINE_SURFACE(3,2,((#380979,#380980,#380981),(#380982,#380983,#380984),
(#380985,#380986,#380987),(#380988,#380989,#380990)),.UNSPECIFIED.,.F.,
 .F.,.F.)
B_SPLINE_SURFACE_WITH_KNOTS((4,4),(3,3),(-5.42101086242752E-20,9.54361881492173E-5),
(0.,1.),.UNSPECIFIED.)
GEOMETRIC_REPRESENTATION_ITEM()
RATIONAL_B_SPLINE_SURFACE(((1.,0.816715621142041,1.),(1.,0.815907587407945,
1.),(1.,0.815115959345203,1.),(1.,0.814339887349193,1.)))
REPRESENTATION_ITEM('')
SURFACE()
);
#2357=(
BOUNDED_SURFACE()
B_SPLINE_SURFACE(3,2,((#380992,#380993,#380994),(#380995,#380996,#380997),
(#380998,#380999,#381000),(#381001,#381002,#381003)),.UNSPECIFIED.,.F.,
 .F.,.F.)
B_SPLINE_SURFACE_WITH_KNOTS((4,4),(3,3),(-6.94567016748526E-20,4.68197758448209E-5),
(0.,1.),.UNSPECIFIED.)
GEOMETRIC_REPRESENTATION_ITEM()
RATIONAL_B_SPLINE_SURFACE(((1.,0.816715621142046,1.),(1.,0.953638980025212,
1.),(1.,0.954506925408061,1.),(1.,0.816715621142055,1.)))
REPRESENTATION_ITEM('')
SURFACE()
);
#2358=(
BOUNDED_SURFACE()
B_SPLINE_SURFACE(3,2,((#381005,#381006,#381007),(#381008,#381009,#381010),
(#381011,#381012,#381013),(#381014,#381015,#381016)),.UNSPECIFIED.,.F.,
 .F.,.F.)
B_SPLINE_SURFACE_WITH_KNOTS((4,4),(3,3),(0.,9.54361881492177E-5),(0.,1.),
 .UNSPECIFIED.)
GEOMETRIC_REPRESENTATION_ITEM()
RATIONAL_B_SPLINE_SURFACE(((1.,0.814339887349197,1.),(1.,0.815115959345203,
1.),(1.,0.815907587407944,1.),(1.,0.816715621142052,1.)))
REPRESENTATION_ITEM('')
SURFACE()
);
#2359=(
BOUNDED_SURFACE()
B_SPLINE_SURFACE(3,2,((#381018,#381019,#381020),(#381021,#381022,#381023),
(#381024,#381025,#381026),(#381027,#381028,#381029)),.UNSPECIFIED.,.F.,
 .F.,.F.)
B_SPLINE_SURFACE_WITH_KNOTS((4,4),(3,3),(-3.39528393502478E-6,3.73481232852734E-5),
(-0.00165018033339765,1.),.UNSPECIFIED.)
GEOMETRIC_REPRESENTATION_ITEM()
RATIONAL_B_SPLINE_SURFACE(((1.00048354385569,0.853487571660387,1.),(1.00047110510924,
0.857256476851426,1.),(1.00053193201111,0.838826096655854,1.),(1.0006397068773,
0.806170615310073,1.)))
REPRESENTATION_ITEM('')
SURFACE()
);
#2360=(
BOUNDED_SURFACE()
B_SPLINE_SURFACE(3,2,((#381033,#381034,#381035),(#381036,#381037,#381038),
(#381039,#381040,#381041),(#381042,#381043,#381044)),.UNSPECIFIED.,.F.,
 .F.,.F.)
B_SPLINE_SURFACE_WITH_KNOTS((4,4),(3,3),(2.02993869230509E-5,5.39756952687123E-5),
(-0.000116281069965564,1.),.UNSPECIFIED.)
GEOMETRIC_REPRESENTATION_ITEM()
RATIONAL_B_SPLINE_SURFACE(((1.0000177047973,0.923870681143007,1.),(1.00001014104059,
0.956394275543447,1.),(1.00002037300279,0.912397594905618,1.),(1.0000339085947,
0.854195550869732,1.)))
REPRESENTATION_ITEM('')
SURFACE()
);
#2361=(
BOUNDED_SURFACE()
B_SPLINE_SURFACE(3,2,((#381137,#381138,#381139),(#381140,#381141,#381142),
(#381143,#381144,#381145),(#381146,#381147,#381148)),.UNSPECIFIED.,.F.,
 .F.,.F.)
B_SPLINE_SURFACE_WITH_KNOTS((4,4),(3,3),(0.00135801595889393,0.00148409170619832),
(0.,1.),.UNSPECIFIED.)
GEOMETRIC_REPRESENTATION_ITEM()
RATIONAL_B_SPLINE_SURFACE(((1.,0.818301933966441,1.),(1.,0.81722661317235,
1.),(1.,0.816179643373941,1.),(1.,0.815159387863647,1.)))
REPRESENTATION_ITEM('')
SURFACE()
);
#2362=(
BOUNDED_SURFACE()
B_SPLINE_SURFACE(3,2,((#381187,#381188,#381189),(#381190,#381191,#381192),
(#381193,#381194,#381195),(#381196,#381197,#381198)),.UNSPECIFIED.,.F.,
 .F.,.F.)
B_SPLINE_SURFACE_WITH_KNOTS((4,4),(3,3),(-1.5474443512207E-6,1.54744435122068E-5),
(-0.0151698983641212,1.01516989835814),.UNSPECIFIED.)
GEOMETRIC_REPRESENTATION_ITEM()
RATIONAL_B_SPLINE_SURFACE(((1.02018382473226,0.324498219413555,1.02018382472418),
(1.00401234488878,0.865716921710647,1.00401234488718),(1.00033622856785,
0.988747276629687,1.00033622856772),(1.,1.,1.)))
REPRESENTATION_ITEM('')
SURFACE()
);
#2363=(
BOUNDED_SURFACE()
B_SPLINE_SURFACE(3,2,((#381200,#381201,#381202),(#381203,#381204,#381205),
(#381206,#381207,#381208),(#381209,#381210,#381211)),.UNSPECIFIED.,.F.,
 .F.,.F.)
B_SPLINE_SURFACE_WITH_KNOTS((4,4),(3,3),(0.00137194782501028,0.00149814269699235),
(0.,1.),.UNSPECIFIED.)
GEOMETRIC_REPRESENTATION_ITEM()
RATIONAL_B_SPLINE_SURFACE(((1.,0.815158509402315,1.),(1.,0.816179044148158,
1.),(1.,0.817226308119926,1.),(1.,0.818301939488807,1.)))
REPRESENTATION_ITEM('')
SURFACE()
);
#2364=(
BOUNDED_SURFACE()
B_SPLINE_SURFACE(3,2,((#381255,#381256,#381257),(#381258,#381259,#381260),
(#381261,#381262,#381263),(#381264,#381265,#381266)),.UNSPECIFIED.,.F.,
 .F.,.F.)
B_SPLINE_SURFACE_WITH_KNOTS((4,4),(3,3),(1.55009486301137E-5,4.9206551047443E-5),
(-8.13759514042935E-5,1.),.UNSPECIFIED.)
GEOMETRIC_REPRESENTATION_ITEM()
RATIONAL_B_SPLINE_SURFACE(((1.00002372912333,0.854200639599698,1.),(1.00001423585992,
0.912530301180538,1.),(1.0000071055047,0.956341495377442,1.),(1.00001238975907,
0.923873338137026,1.)))
REPRESENTATION_ITEM('')
SURFACE()
);
#2365=(
BOUNDED_SURFACE()
B_SPLINE_SURFACE(3,2,((#381270,#381271,#381272),(#381273,#381274,#381275),
(#381276,#381277,#381278),(#381279,#381280,#381281)),.UNSPECIFIED.,.F.,
 .F.,.F.)
B_SPLINE_SURFACE_WITH_KNOTS((4,4),(3,3),(-3.39934179457819E-6,3.73927597403567E-5),
(-0.00186004067378984,1.00069373317421),.UNSPECIFIED.)
GEOMETRIC_REPRESENTATION_ITEM()
RATIONAL_B_SPLINE_SURFACE(((1.00072100136039,0.80605196387545,1.00026859642684),
(1.00060048440141,0.838470803558752,1.0002236999449),(1.00053106448783,
0.85714463227244,1.00019783877214),(1.00054515072841,0.853355459539185,
1.00020308635432)))
REPRESENTATION_ITEM('')
SURFACE()
);
#2366=(
BOUNDED_SURFACE()
B_SPLINE_SURFACE(3,2,((#381283,#381284,#381285),(#381286,#381287,#381288),
(#381289,#381290,#381291),(#381292,#381293,#381294)),.UNSPECIFIED.,.F.,
 .F.,.F.)
B_SPLINE_SURFACE_WITH_KNOTS((4,4),(3,3),(-5.42101086242752E-20,9.54361881492172E-5),
(0.,1.),.UNSPECIFIED.)
GEOMETRIC_REPRESENTATION_ITEM()
RATIONAL_B_SPLINE_SURFACE(((1.,0.816715621142048,1.),(1.,0.815907587407955,
1.),(1.,0.815115959345183,1.),(1.,0.814339887349201,1.)))
REPRESENTATION_ITEM('')
SURFACE()
);
#2367=(
BOUNDED_SURFACE()
B_SPLINE_SURFACE(3,2,((#381296,#381297,#381298),(#381299,#381300,#381301),
(#381302,#381303,#381304),(#381305,#381306,#381307)),.UNSPECIFIED.,.F.,
 .F.,.F.)
B_SPLINE_SURFACE_WITH_KNOTS((4,4),(3,3),(2.87991202066462E-20,4.6819775844821E-5),
(0.,1.),.UNSPECIFIED.)
GEOMETRIC_REPRESENTATION_ITEM()
RATIONAL_B_SPLINE_SURFACE(((1.,0.816715621142047,1.),(1.,0.953638980025212,
1.),(1.,0.954506925408053,1.),(1.,0.816715621142048,1.)))
REPRESENTATION_ITEM('')
SURFACE()
);
#2368=(
BOUNDED_SURFACE()
B_SPLINE_SURFACE(3,2,((#381309,#381310,#381311),(#381312,#381313,#381314),
(#381315,#381316,#381317),(#381318,#381319,#381320)),.UNSPECIFIED.,.F.,
 .F.,.F.)
B_SPLINE_SURFACE_WITH_KNOTS((4,4),(3,3),(-1.62630325872826E-19,9.54361881492175E-5),
(0.,1.),.UNSPECIFIED.)
GEOMETRIC_REPRESENTATION_ITEM()
RATIONAL_B_SPLINE_SURFACE(((1.,0.814339887349191,1.),(1.,0.815115959345201,
1.),(1.,0.81590758740795,1.),(1.,0.816715621142048,1.)))
REPRESENTATION_ITEM('')
SURFACE()
);
#2369=(
BOUNDED_SURFACE()
B_SPLINE_SURFACE(3,2,((#381322,#381323,#381324),(#381325,#381326,#381327),
(#381328,#381329,#381330),(#381331,#381332,#381333)),.UNSPECIFIED.,.F.,
 .F.,.F.)
B_SPLINE_SURFACE_WITH_KNOTS((4,4),(3,3),(-3.39528393502376E-6,3.73481232852727E-5),
(-0.00165018033296025,1.),.UNSPECIFIED.)
GEOMETRIC_REPRESENTATION_ITEM()
RATIONAL_B_SPLINE_SURFACE(((1.00048354385556,0.853487571660445,1.),(1.00047110510911,
0.857256476851498,1.),(1.00053193201097,0.838826096655924,1.),(1.00063970687713,
0.806170615310152,1.)))
REPRESENTATION_ITEM('')
SURFACE()
);
#2370=(
BOUNDED_SURFACE()
B_SPLINE_SURFACE(3,2,((#381337,#381338,#381339),(#381340,#381341,#381342),
(#381343,#381344,#381345),(#381346,#381347,#381348)),.UNSPECIFIED.,.F.,
 .F.,.F.)
B_SPLINE_SURFACE_WITH_KNOTS((4,4),(3,3),(2.0299386923051E-5,5.39756952686909E-5),
(-0.000116281070037132,1.),.UNSPECIFIED.)
GEOMETRIC_REPRESENTATION_ITEM()
RATIONAL_B_SPLINE_SURFACE(((1.00001770479732,0.923870681143002,1.),(1.0000101410406,
0.956394275543398,1.),(1.0000203730028,0.91239759490568,1.),(1.00003390859472,
0.854195550869837,1.)))
REPRESENTATION_ITEM('')
SURFACE()
);
#2371=(
BOUNDED_SURFACE()
B_SPLINE_SURFACE(3,2,((#381441,#381442,#381443),(#381444,#381445,#381446),
(#381447,#381448,#381449),(#381450,#381451,#381452)),.UNSPECIFIED.,.F.,
 .F.,.F.)
B_SPLINE_SURFACE_WITH_KNOTS((4,4),(3,3),(0.00135801595889393,0.00148409170619832),
(0.,1.),.UNSPECIFIED.)
GEOMETRIC_REPRESENTATION_ITEM()
RATIONAL_B_SPLINE_SURFACE(((1.,0.818301933966442,1.),(1.,0.817226613172349,
1.),(1.,0.816179643373945,1.),(1.,0.815159387863655,1.)))
REPRESENTATION_ITEM('')
SURFACE()
);
#2372=(
BOUNDED_SURFACE()
B_SPLINE_SURFACE(3,2,((#381491,#381492,#381493),(#381494,#381495,#381496),
(#381497,#381498,#381499),(#381500,#381501,#381502)),.UNSPECIFIED.,.F.,
 .F.,.F.)
B_SPLINE_SURFACE_WITH_KNOTS((4,4),(3,3),(-1.54744435122081E-6,1.54744435122079E-5),
(-0.0151698983621951,1.),.UNSPECIFIED.)
GEOMETRIC_REPRESENTATION_ITEM()
RATIONAL_B_SPLINE_SURFACE(((1.02018382472966,0.334740937356506,1.),(1.00401234488827,
0.867753072813274,1.),(1.00033622856781,0.988917903080871,1.),(1.,1.,1.)))
REPRESENTATION_ITEM('')
SURFACE()
);
#2373=(
BOUNDED_SURFACE()
B_SPLINE_SURFACE(3,2,((#381504,#381505,#381506),(#381507,#381508,#381509),
(#381510,#381511,#381512),(#381513,#381514,#381515)),.UNSPECIFIED.,.F.,
 .F.,.F.)
B_SPLINE_SURFACE_WITH_KNOTS((4,4),(3,3),(0.00137194782501028,0.00149814269699235),
(0.,1.),.UNSPECIFIED.)
GEOMETRIC_REPRESENTATION_ITEM()
RATIONAL_B_SPLINE_SURFACE(((1.,0.815158509402317,1.),(1.,0.81617904414816,
1.),(1.,0.817226308119932,1.),(1.,0.818301939488811,1.)))
REPRESENTATION_ITEM('')
SURFACE()
);
#2374=(
BOUNDED_SURFACE()
B_SPLINE_SURFACE(3,2,((#381559,#381560,#381561),(#381562,#381563,#381564),
(#381565,#381566,#381567),(#381568,#381569,#381570)),.UNSPECIFIED.,.F.,
 .F.,.F.)
B_SPLINE_SURFACE_WITH_KNOTS((4,4),(3,3),(1.55009486301137E-5,4.92065510474435E-5),
(-8.13759516055901E-5,1.),.UNSPECIFIED.)
GEOMETRIC_REPRESENTATION_ITEM()
RATIONAL_B_SPLINE_SURFACE(((1.00002372912339,0.854200639599675,1.),(1.00001423585996,
0.91253030118052,1.),(1.00000710550472,0.956341495377425,1.),(1.0000123897591,
0.923873338137014,1.)))
REPRESENTATION_ITEM('')
SURFACE()
);
#2375=(
BOUNDED_SURFACE()
B_SPLINE_SURFACE(3,2,((#381574,#381575,#381576),(#381577,#381578,#381579),
(#381580,#381581,#381582),(#381583,#381584,#381585)),.UNSPECIFIED.,.F.,
 .F.,.F.)
B_SPLINE_SURFACE_WITH_KNOTS((4,4),(3,3),(-3.39934179457775E-6,3.73927597403566E-5),
(-0.00186004067423228,1.00069373317438),.UNSPECIFIED.)
GEOMETRIC_REPRESENTATION_ITEM()
RATIONAL_B_SPLINE_SURFACE(((1.00072100136056,0.806051963875337,1.0002685964269),
(1.00060048440155,0.838470803558647,1.00022369994495),(1.00053106448796,
0.857144632272365,1.00019783877219),(1.00054515072854,0.853355459539096,
1.00020308635436)))
REPRESENTATION_ITEM('')
SURFACE()
);
#2376=(
BOUNDED_SURFACE()
B_SPLINE_SURFACE(3,2,((#381587,#381588,#381589),(#381590,#381591,#381592),
(#381593,#381594,#381595),(#381596,#381597,#381598)),.UNSPECIFIED.,.F.,
 .F.,.F.)
B_SPLINE_SURFACE_WITH_KNOTS((4,4),(3,3),(-3.79470760369927E-19,9.54361881492172E-5),
(0.,1.),.UNSPECIFIED.)
GEOMETRIC_REPRESENTATION_ITEM()
RATIONAL_B_SPLINE_SURFACE(((1.,0.81671562114205,1.),(1.,0.815907587407947,
1.),(1.,0.815115959345205,1.),(1.,0.814339887349194,1.)))
REPRESENTATION_ITEM('')
SURFACE()
);
#2377=(
BOUNDED_SURFACE()
B_SPLINE_SURFACE(3,2,((#381600,#381601,#381602),(#381603,#381604,#381605),
(#381606,#381607,#381608),(#381609,#381610,#381611)),.UNSPECIFIED.,.F.,
 .F.,.F.)
B_SPLINE_SURFACE_WITH_KNOTS((4,4),(3,3),(-1.27054942088145E-19,4.68197758448207E-5),
(0.,1.),.UNSPECIFIED.)
GEOMETRIC_REPRESENTATION_ITEM()
RATIONAL_B_SPLINE_SURFACE(((1.,0.816715621142049,1.),(1.,0.953638980025204,
1.),(1.,0.954506925408054,1.),(1.,0.816715621142057,1.)))
REPRESENTATION_ITEM('')
SURFACE()
);
#2378=(
BOUNDED_SURFACE()
B_SPLINE_SURFACE(3,2,((#381613,#381614,#381615),(#381616,#381617,#381618),
(#381619,#381620,#381621),(#381622,#381623,#381624)),.UNSPECIFIED.,.F.,
 .F.,.F.)
B_SPLINE_SURFACE_WITH_KNOTS((4,4),(3,3),(-1.0842021724855E-19,9.54361881492175E-5),
(0.,1.),.UNSPECIFIED.)
GEOMETRIC_REPRESENTATION_ITEM()
RATIONAL_B_SPLINE_SURFACE(((1.,0.814339887349193,1.),(1.,0.81511595934522,
1.),(1.,0.815907587407938,1.),(1.,0.81671562114205,1.)))
REPRESENTATION_ITEM('')
SURFACE()
);
#2379=(
BOUNDED_SURFACE()
B_SPLINE_SURFACE(3,2,((#381626,#381627,#381628),(#381629,#381630,#381631),
(#381632,#381633,#381634),(#381635,#381636,#381637)),.UNSPECIFIED.,.F.,
 .F.,.F.)
B_SPLINE_SURFACE_WITH_KNOTS((4,4),(3,3),(-3.39528393502485E-6,3.73481232852735E-5),
(-0.00165018033289677,1.),.UNSPECIFIED.)
GEOMETRIC_REPRESENTATION_ITEM()
RATIONAL_B_SPLINE_SURFACE(((1.00048354385554,0.853487571660458,1.),(1.0004711051091,
0.857256476851515,1.),(1.00053193201095,0.838826096655935,1.),(1.00063970687711,
0.806170615310171,1.)))
REPRESENTATION_ITEM('')
SURFACE()
);
#2380=(
BOUNDED_SURFACE()
B_SPLINE_SURFACE(3,2,((#381641,#381642,#381643),(#381644,#381645,#381646),
(#381647,#381648,#381649),(#381650,#381651,#381652)),.UNSPECIFIED.,.F.,
 .F.,.F.)
B_SPLINE_SURFACE_WITH_KNOTS((4,4),(3,3),(2.02993869230508E-5,5.39756952686903E-5),
(-0.000116281069679975,1.),.UNSPECIFIED.)
GEOMETRIC_REPRESENTATION_ITEM()
RATIONAL_B_SPLINE_SURFACE(((1.00001770479726,0.923870681143028,1.),(1.00001014104057,
0.956394275543431,1.),(1.00002037300274,0.912397594905693,1.),(1.00003390859462,
0.854195550869887,1.)))
REPRESENTATION_ITEM('')
SURFACE()
);
#2381=(
BOUNDED_SURFACE()
B_SPLINE_SURFACE(3,2,((#381745,#381746,#381747),(#381748,#381749,#381750),
(#381751,#381752,#381753),(#381754,#381755,#381756)),.UNSPECIFIED.,.F.,
 .F.,.F.)
B_SPLINE_SURFACE_WITH_KNOTS((4,4),(3,3),(0.00135801595889393,0.00148409170619832),
(0.,1.),.UNSPECIFIED.)
GEOMETRIC_REPRESENTATION_ITEM()
RATIONAL_B_SPLINE_SURFACE(((1.,0.818301933966442,1.),(1.,0.817226613172351,
1.),(1.,0.816179643373944,1.),(1.,0.815159387863653,1.)))
REPRESENTATION_ITEM('')
SURFACE()
);
#2382=(
BOUNDED_SURFACE()
B_SPLINE_SURFACE(3,2,((#381795,#381796,#381797),(#381798,#381799,#381800),
(#381801,#381802,#381803),(#381804,#381805,#381806)),.UNSPECIFIED.,.F.,
 .F.,.F.)
B_SPLINE_SURFACE_WITH_KNOTS((4,4),(3,3),(-1.54744435122086E-6,1.54744435122087E-5),
(-0.0151698983707459,1.01516989835136),.UNSPECIFIED.)
GEOMETRIC_REPRESENTATION_ITEM()
RATIONAL_B_SPLINE_SURFACE(((1.02018382474121,0.324498219413668,1.02018382471503),
(1.00401234489057,0.865716921710515,1.00401234488536),(1.000336228568,0.988747276629717,
1.00033622856756),(1.,1.,1.)))
REPRESENTATION_ITEM('')
SURFACE()
);
#2383=(
BOUNDED_SURFACE()
B_SPLINE_SURFACE(3,2,((#381808,#381809,#381810),(#381811,#381812,#381813),
(#381814,#381815,#381816),(#381817,#381818,#381819)),.UNSPECIFIED.,.F.,
 .F.,.F.)
B_SPLINE_SURFACE_WITH_KNOTS((4,4),(3,3),(0.00137194782501028,0.00149814269699235),
(0.,1.),.UNSPECIFIED.)
GEOMETRIC_REPRESENTATION_ITEM()
RATIONAL_B_SPLINE_SURFACE(((1.,0.815158509402316,1.),(1.,0.816179044148168,
1.),(1.,0.817226308119923,1.),(1.,0.81830193948881,1.)))
REPRESENTATION_ITEM('')
SURFACE()
);
#2384=(
BOUNDED_SURFACE()
B_SPLINE_SURFACE(3,2,((#381863,#381864,#381865),(#381866,#381867,#381868),
(#381869,#381870,#381871),(#381872,#381873,#381874)),.UNSPECIFIED.,.F.,
 .F.,.F.)
B_SPLINE_SURFACE_WITH_KNOTS((4,4),(3,3),(1.55009486301137E-5,4.92065510474433E-5),
(-8.13759517471266E-5,1.),.UNSPECIFIED.)
GEOMETRIC_REPRESENTATION_ITEM()
RATIONAL_B_SPLINE_SURFACE(((1.00002372912343,0.854200639599643,1.),(1.00001423585998,
0.912530301180509,1.),(1.00000710550473,0.956341495377418,1.),(1.00001238975912,
0.923873338136999,1.)))
REPRESENTATION_ITEM('')
SURFACE()
);
#2385=(
BOUNDED_SURFACE()
B_SPLINE_SURFACE(3,2,((#381878,#381879,#381880),(#381881,#381882,#381883),
(#381884,#381885,#381886),(#381887,#381888,#381889)),.UNSPECIFIED.,.F.,
 .F.,.F.)
B_SPLINE_SURFACE_WITH_KNOTS((4,4),(3,3),(-3.39934179457816E-6,3.73927597403566E-5),
(-0.00186004067451563,1.00069373317446),.UNSPECIFIED.)
GEOMETRIC_REPRESENTATION_ITEM()
RATIONAL_B_SPLINE_SURFACE(((1.00072100136067,0.806051963875284,1.00026859642693),
(1.00060048440165,0.838470803558566,1.00022369994498),(1.00053106448804,
0.857144632272327,1.00019783877221),(1.00054515072862,0.853355459539038,
1.00020308635439)))
REPRESENTATION_ITEM('')
SURFACE()
);
#2386=(
BOUNDED_SURFACE()
B_SPLINE_SURFACE(3,2,((#381891,#381892,#381893),(#381894,#381895,#381896),
(#381897,#381898,#381899),(#381900,#381901,#381902)),.UNSPECIFIED.,.F.,
 .F.,.F.)
B_SPLINE_SURFACE_WITH_KNOTS((4,4),(3,3),(2.16840434497101E-19,9.54361881492174E-5),
(0.,1.),.UNSPECIFIED.)
GEOMETRIC_REPRESENTATION_ITEM()
RATIONAL_B_SPLINE_SURFACE(((1.,0.816715621142049,1.),(1.,0.815907587407941,
1.),(1.,0.8151159593452,1.),(1.,0.814339887349195,1.)))
REPRESENTATION_ITEM('')
SURFACE()
);
#2387=(
BOUNDED_SURFACE()
B_SPLINE_SURFACE(3,2,((#381904,#381905,#381906),(#381907,#381908,#381909),
(#381910,#381911,#381912),(#381913,#381914,#381915)),.UNSPECIFIED.,.F.,
 .F.,.F.)
B_SPLINE_SURFACE_WITH_KNOTS((4,4),(3,3),(2.71050543121376E-20,4.68197758448213E-5),
(0.,1.),.UNSPECIFIED.)
GEOMETRIC_REPRESENTATION_ITEM()
RATIONAL_B_SPLINE_SURFACE(((1.,0.816715621142051,1.),(1.,0.953638980025212,
1.),(1.,0.954506925408045,1.),(1.,0.816715621142055,1.)))
REPRESENTATION_ITEM('')
SURFACE()
);
#2388=(
BOUNDED_SURFACE()
B_SPLINE_SURFACE(3,2,((#381917,#381918,#381919),(#381920,#381921,#381922),
(#381923,#381924,#381925),(#381926,#381927,#381928)),.UNSPECIFIED.,.F.,
 .F.,.F.)
B_SPLINE_SURFACE_WITH_KNOTS((4,4),(3,3),(0.,9.54361881492176E-5),(0.,1.),
 .UNSPECIFIED.)
GEOMETRIC_REPRESENTATION_ITEM()
RATIONAL_B_SPLINE_SURFACE(((1.,0.814339887349193,1.),(1.,0.815115959345204,
1.),(1.,0.815907587407941,1.),(1.,0.816715621142051,1.)))
REPRESENTATION_ITEM('')
SURFACE()
);
#2389=(
BOUNDED_SURFACE()
B_SPLINE_SURFACE(3,2,((#381930,#381931,#381932),(#381933,#381934,#381935),
(#381936,#381937,#381938),(#381939,#381940,#381941)),.UNSPECIFIED.,.F.,
 .F.,.F.)
B_SPLINE_SURFACE_WITH_KNOTS((4,4),(3,3),(-3.39528393502491E-6,3.73481232852736E-5),
(-0.0016501803332037,1.),.UNSPECIFIED.)
GEOMETRIC_REPRESENTATION_ITEM()
RATIONAL_B_SPLINE_SURFACE(((1.00048354385563,0.853487571660408,1.),(1.00047110510918,
0.857256476851472,1.),(1.00053193201105,0.83882609665589,1.),(1.00063970687722,
0.806170615310104,1.)))
REPRESENTATION_ITEM('')
SURFACE()
);
#2390=(
BOUNDED_SURFACE()
B_SPLINE_SURFACE(3,2,((#381945,#381946,#381947),(#381948,#381949,#381950),
(#381951,#381952,#381953),(#381954,#381955,#381956)),.UNSPECIFIED.,.F.,
 .F.,.F.)
B_SPLINE_SURFACE_WITH_KNOTS((4,4),(3,3),(2.02993869230507E-5,5.397569526869E-5),
(-0.00011628106952024,1.),.UNSPECIFIED.)
GEOMETRIC_REPRESENTATION_ITEM()
RATIONAL_B_SPLINE_SURFACE(((1.00001770479724,0.923870681143042,1.),(1.00001014104055,
0.956394275543437,1.),(1.00002037300271,0.912397594905713,1.),(1.00003390859457,
0.854195550869909,1.)))
REPRESENTATION_ITEM('')
SURFACE()
);
#2391=(
BOUNDED_SURFACE()
B_SPLINE_SURFACE(3,2,((#382049,#382050,#382051),(#382052,#382053,#382054),
(#382055,#382056,#382057),(#382058,#382059,#382060)),.UNSPECIFIED.,.F.,
 .F.,.F.)
B_SPLINE_SURFACE_WITH_KNOTS((4,4),(3,3),(0.00135801595889393,0.00148409170619832),
(0.,1.),.UNSPECIFIED.)
GEOMETRIC_REPRESENTATION_ITEM()
RATIONAL_B_SPLINE_SURFACE(((1.,0.818301933966448,1.),(1.,0.81722661317234,
1.),(1.,0.816179643373967,1.),(1.,0.815159387863657,1.)))
REPRESENTATION_ITEM('')
SURFACE()
);
#2392=(
BOUNDED_SURFACE()
B_SPLINE_SURFACE(3,2,((#382099,#382100,#382101),(#382102,#382103,#382104),
(#382105,#382106,#382107),(#382108,#382109,#382110)),.UNSPECIFIED.,.F.,
 .F.,.F.)
B_SPLINE_SURFACE_WITH_KNOTS((4,4),(3,3),(-1.54744435121997E-6,1.54744435122078E-5),
(-0.0151698983613011,1.01516989836171),.UNSPECIFIED.)
GEOMETRIC_REPRESENTATION_ITEM()
RATIONAL_B_SPLINE_SURFACE(((1.02018382472845,0.324498219413089,1.020183824729),
(1.00401234488803,0.865716921710524,1.00401234488814),(1.00033622856779,
0.988747276629642,1.0003362285678),(1.,1.,1.)))
REPRESENTATION_ITEM('')
SURFACE()
);
#2393=(
BOUNDED_SURFACE()
B_SPLINE_SURFACE(3,2,((#382112,#382113,#382114),(#382115,#382116,#382117),
(#382118,#382119,#382120),(#382121,#382122,#382123)),.UNSPECIFIED.,.F.,
 .F.,.F.)
B_SPLINE_SURFACE_WITH_KNOTS((4,4),(3,3),(0.00137194782501028,0.00149814269699235),
(0.,1.),.UNSPECIFIED.)
GEOMETRIC_REPRESENTATION_ITEM()
RATIONAL_B_SPLINE_SURFACE(((1.,0.815158509402318,1.),(1.,0.816179044148161,
1.),(1.,0.817226308119937,1.),(1.,0.818301939488799,1.)))
REPRESENTATION_ITEM('')
SURFACE()
);
#2394=(
BOUNDED_SURFACE()
B_SPLINE_SURFACE(3,2,((#382167,#382168,#382169),(#382170,#382171,#382172),
(#382173,#382174,#382175),(#382176,#382177,#382178)),.UNSPECIFIED.,.F.,
 .F.,.F.)
B_SPLINE_SURFACE_WITH_KNOTS((4,4),(3,3),(1.55009486301137E-5,4.92065510474436E-5),
(-8.13759516876729E-5,1.),.UNSPECIFIED.)
GEOMETRIC_REPRESENTATION_ITEM()
RATIONAL_B_SPLINE_SURFACE(((1.00002372912342,0.854200639599655,1.),(1.00001423585997,
0.912530301180514,1.),(1.00000710550473,0.95634149537743,1.),(1.00001238975912,
0.923873338137006,1.)))
REPRESENTATION_ITEM('')
SURFACE()
);
#2395=(
BOUNDED_SURFACE()
B_SPLINE_SURFACE(3,2,((#382182,#382183,#382184),(#382185,#382186,#382187),
(#382188,#382189,#382190),(#382191,#382192,#382193)),.UNSPECIFIED.,.F.,
 .F.,.F.)
B_SPLINE_SURFACE_WITH_KNOTS((4,4),(3,3),(-3.39934179457829E-6,3.73927597403564E-5),
(-0.00186004067411874,1.00069373317431),.UNSPECIFIED.)
GEOMETRIC_REPRESENTATION_ITEM()
RATIONAL_B_SPLINE_SURFACE(((1.00072100136052,0.806051963875365,1.00026859642688),
(1.00060048440152,0.838470803558694,1.00022369994493),(1.00053106448793,
0.857144632272389,1.00019783877217),(1.0005451507285,0.85335545953913,1.00020308635434)))
REPRESENTATION_ITEM('')
SURFACE()
);
#2396=(
BOUNDED_SURFACE()
B_SPLINE_SURFACE(3,2,((#382195,#382196,#382197),(#382198,#382199,#382200),
(#382201,#382202,#382203),(#382204,#382205,#382206)),.UNSPECIFIED.,.F.,
 .F.,.F.)
B_SPLINE_SURFACE_WITH_KNOTS((4,4),(3,3),(-1.0842021724855E-19,9.54361881492172E-5),
(0.,1.),.UNSPECIFIED.)
GEOMETRIC_REPRESENTATION_ITEM()
RATIONAL_B_SPLINE_SURFACE(((1.,0.816715621142054,1.),(1.,0.815907587407943,
1.),(1.,0.815115959345211,1.),(1.,0.814339887349197,1.)))
REPRESENTATION_ITEM('')
SURFACE()
);
#2397=(
BOUNDED_SURFACE()
B_SPLINE_SURFACE(3,2,((#382208,#382209,#382210),(#382211,#382212,#382213),
(#382214,#382215,#382216),(#382217,#382218,#382219)),.UNSPECIFIED.,.F.,
 .F.,.F.)
B_SPLINE_SURFACE_WITH_KNOTS((4,4),(3,3),(1.54159996400283E-19,4.68197758448204E-5),
(0.,1.),.UNSPECIFIED.)
GEOMETRIC_REPRESENTATION_ITEM()
RATIONAL_B_SPLINE_SURFACE(((1.,0.816715621142047,1.),(1.,0.953638980025207,
1.),(1.,0.954506925408052,1.),(1.,0.816715621142061,1.)))
REPRESENTATION_ITEM('')
SURFACE()
);
#2398=(
BOUNDED_SURFACE()
B_SPLINE_SURFACE(3,2,((#382221,#382222,#382223),(#382224,#382225,#382226),
(#382227,#382228,#382229),(#382230,#382231,#382232)),.UNSPECIFIED.,.F.,
 .F.,.F.)
B_SPLINE_SURFACE_WITH_KNOTS((4,4),(3,3),(2.16840434497101E-19,9.54361881492178E-5),
(0.,1.),.UNSPECIFIED.)
GEOMETRIC_REPRESENTATION_ITEM()
RATIONAL_B_SPLINE_SURFACE(((1.,0.814339887349196,1.),(1.,0.81511595934521,
1.),(1.,0.815907587407939,1.),(1.,0.816715621142047,1.)))
REPRESENTATION_ITEM('')
SURFACE()
);
#2399=(
BOUNDED_SURFACE()
B_SPLINE_SURFACE(3,2,((#382234,#382235,#382236),(#382237,#382238,#382239),
(#382240,#382241,#382242),(#382243,#382244,#382245)),.UNSPECIFIED.,.F.,
 .F.,.F.)
B_SPLINE_SURFACE_WITH_KNOTS((4,4),(3,3),(-3.39528393502487E-6,3.73481232852735E-5),
(-0.00165018033261962,1.),.UNSPECIFIED.)
GEOMETRIC_REPRESENTATION_ITEM()
RATIONAL_B_SPLINE_SURFACE(((1.00048354385546,0.853487571660497,1.),(1.00047110510902,
0.857256476851547,1.),(1.00053193201086,0.838826096655987,1.),(1.000639706877,
0.806170615310215,1.)))
REPRESENTATION_ITEM('')
SURFACE()
);
#2400=(
BOUNDED_SURFACE()
B_SPLINE_SURFACE(3,2,((#382249,#382250,#382251),(#382252,#382253,#382254),
(#382255,#382256,#382257),(#382258,#382259,#382260)),.UNSPECIFIED.,.F.,
 .F.,.F.)
B_SPLINE_SURFACE_WITH_KNOTS((4,4),(3,3),(2.02993869230507E-5,5.397569526869E-5),
(-0.000116281069878473,1.),.UNSPECIFIED.)
GEOMETRIC_REPRESENTATION_ITEM()
RATIONAL_B_SPLINE_SURFACE(((1.00001770479729,0.923870681143011,1.),(1.00001014104059,
0.956394275543423,1.),(1.00002037300278,0.912397594905672,1.),(1.00003390859468,
0.854195550869864,1.)))
REPRESENTATION_ITEM('')
SURFACE()
);
#2401=(
BOUNDED_SURFACE()
B_SPLINE_SURFACE(3,2,((#382353,#382354,#382355),(#382356,#382357,#382358),
(#382359,#382360,#382361),(#382362,#382363,#382364)),.UNSPECIFIED.,.F.,
 .F.,.F.)
B_SPLINE_SURFACE_WITH_KNOTS((4,4),(3,3),(0.00135801595889393,0.00148409170619832),
(0.,1.),.UNSPECIFIED.)
GEOMETRIC_REPRESENTATION_ITEM()
RATIONAL_B_SPLINE_SURFACE(((1.,0.818301933966445,1.),(1.,0.817226613172353,
1.),(1.,0.816179643373947,1.),(1.,0.815159387863659,1.)))
REPRESENTATION_ITEM('')
SURFACE()
);
#2402=(
BOUNDED_SURFACE()
B_SPLINE_SURFACE(3,2,((#382403,#382404,#382405),(#382406,#382407,#382408),
(#382409,#382410,#382411),(#382412,#382413,#382414)),.UNSPECIFIED.,.F.,
 .F.,.F.)
B_SPLINE_SURFACE_WITH_KNOTS((4,4),(3,3),(5.0821976835258E-20,1.54744435122074E-5),
(0.,1.),.UNSPECIFIED.)
GEOMETRIC_REPRESENTATION_ITEM()
RATIONAL_B_SPLINE_SURFACE(((1.,0.478041569704972,1.),(1.,0.890533857552081,
1.),(1.,0.990075913815901,1.),(1.,1.,1.)))
REPRESENTATION_ITEM('')
SURFACE()
);
#2403=(
BOUNDED_SURFACE()
B_SPLINE_SURFACE(3,2,((#382416,#382417,#382418),(#382419,#382420,#382421),
(#382422,#382423,#382424),(#382425,#382426,#382427)),.UNSPECIFIED.,.F.,
 .F.,.F.)
B_SPLINE_SURFACE_WITH_KNOTS((4,4),(3,3),(0.00137194782501028,0.00149814269699235),
(0.,1.),.UNSPECIFIED.)
GEOMETRIC_REPRESENTATION_ITEM()
RATIONAL_B_SPLINE_SURFACE(((1.,0.815158509402316,1.),(1.,0.81617904414817,
1.),(1.,0.817226308119927,1.),(1.,0.818301939488812,1.)))
REPRESENTATION_ITEM('')
SURFACE()
);
#2404=(
BOUNDED_SURFACE()
B_SPLINE_SURFACE(3,2,((#382471,#382472,#382473),(#382474,#382475,#382476),
(#382477,#382478,#382479),(#382480,#382481,#382482)),.UNSPECIFIED.,.F.,
 .F.,.F.)
B_SPLINE_SURFACE_WITH_KNOTS((4,4),(3,3),(1.55009486301137E-5,4.92065510474426E-5),
(-8.13759511169527E-5,1.),.UNSPECIFIED.)
GEOMETRIC_REPRESENTATION_ITEM()
RATIONAL_B_SPLINE_SURFACE(((1.00002372912325,0.854200639599739,1.),(1.00001423585987,
0.912530301180574,1.),(1.00000710550468,0.956341495377443,1.),(1.00001238975903,
0.92387333813705,1.)))
REPRESENTATION_ITEM('')
SURFACE()
);
#2405=(
BOUNDED_SURFACE()
B_SPLINE_SURFACE(3,2,((#382486,#382487,#382488),(#382489,#382490,#382491),
(#382492,#382493,#382494),(#382495,#382496,#382497)),.UNSPECIFIED.,.F.,
 .F.,.F.)
B_SPLINE_SURFACE_WITH_KNOTS((4,4),(3,3),(-3.39934179457774E-6,3.73927597403568E-5),
(-0.00186004067399766,1.00069373317424),.UNSPECIFIED.)
GEOMETRIC_REPRESENTATION_ITEM()
RATIONAL_B_SPLINE_SURFACE(((1.00072100136047,0.806051963875431,1.00026859642685),
(1.00060048440148,0.838470803558688,1.00022369994491),(1.00053106448789,
0.857144632272437,1.00019783877215),(1.00054515072847,0.853355459539152,
1.00020308635432)))
REPRESENTATION_ITEM('')
SURFACE()
);
#2406=(
BOUNDED_SURFACE()
B_SPLINE_SURFACE(3,2,((#382499,#382500,#382501),(#382502,#382503,#382504),
(#382505,#382506,#382507),(#382508,#382509,#382510)),.UNSPECIFIED.,.F.,
 .F.,.F.)
B_SPLINE_SURFACE_WITH_KNOTS((4,4),(3,3),(-2.71050543121376E-19,9.54361881492173E-5),
(0.,1.),.UNSPECIFIED.)
GEOMETRIC_REPRESENTATION_ITEM()
RATIONAL_B_SPLINE_SURFACE(((1.,0.81671562114205,1.),(1.,0.815907587407946,
1.),(1.,0.815115959345205,1.),(1.,0.814339887349197,1.)))
REPRESENTATION_ITEM('')
SURFACE()
);
#2407=(
BOUNDED_SURFACE()
B_SPLINE_SURFACE(3,2,((#382512,#382513,#382514),(#382515,#382516,#382517),
(#382518,#382519,#382520),(#382521,#382522,#382523)),.UNSPECIFIED.,.F.,
 .F.,.F.)
B_SPLINE_SURFACE_WITH_KNOTS((4,4),(3,3),(1.06726151354042E-19,4.68197758448204E-5),
(0.,1.),.UNSPECIFIED.)
GEOMETRIC_REPRESENTATION_ITEM()
RATIONAL_B_SPLINE_SURFACE(((1.,0.816715621142051,1.),(1.,0.9536389800252,
1.),(1.,0.954506925408061,1.),(1.,0.81671562114205,1.)))
REPRESENTATION_ITEM('')
SURFACE()
);
#2408=(
BOUNDED_SURFACE()
B_SPLINE_SURFACE(3,2,((#382525,#382526,#382527),(#382528,#382529,#382530),
(#382531,#382532,#382533),(#382534,#382535,#382536)),.UNSPECIFIED.,.F.,
 .F.,.F.)
B_SPLINE_SURFACE_WITH_KNOTS((4,4),(3,3),(5.42101086242752E-20,9.54361881492178E-5),
(0.,1.),.UNSPECIFIED.)
GEOMETRIC_REPRESENTATION_ITEM()
RATIONAL_B_SPLINE_SURFACE(((1.,0.814339887349194,1.),(1.,0.81511595934521,
1.),(1.,0.81590758740794,1.),(1.,0.816715621142051,1.)))
REPRESENTATION_ITEM('')
SURFACE()
);
#2409=(
BOUNDED_SURFACE()
B_SPLINE_SURFACE(3,2,((#382538,#382539,#382540),(#382541,#382542,#382543),
(#382544,#382545,#382546),(#382547,#382548,#382549)),.UNSPECIFIED.,.F.,
 .F.,.F.)
B_SPLINE_SURFACE_WITH_KNOTS((4,4),(3,3),(-3.3952839350248E-6,3.73481232852729E-5),
(-0.00165018033267285,1.),.UNSPECIFIED.)
GEOMETRIC_REPRESENTATION_ITEM()
RATIONAL_B_SPLINE_SURFACE(((1.00048354385548,0.853487571660492,1.),(1.00047110510903,
0.857256476851548,1.),(1.00053193201088,0.838826096655974,1.),(1.00063970687702,
0.80617061531021,1.)))
REPRESENTATION_ITEM('')
SURFACE()
);
#2410=(
BOUNDED_SURFACE()
B_SPLINE_SURFACE(3,2,((#382553,#382554,#382555),(#382556,#382557,#382558),
(#382559,#382560,#382561),(#382562,#382563,#382564)),.UNSPECIFIED.,.F.,
 .F.,.F.)
B_SPLINE_SURFACE_WITH_KNOTS((4,4),(3,3),(2.02993869230509E-5,5.39756952686904E-5),
(-0.000116281069613679,1.),.UNSPECIFIED.)
GEOMETRIC_REPRESENTATION_ITEM()
RATIONAL_B_SPLINE_SURFACE(((1.00001770479725,0.923870681143035,1.),(1.00001014104056,
0.956394275543439,1.),(1.00002037300273,0.91239759490569,1.),(1.0000339085946,
0.854195550869901,1.)))
REPRESENTATION_ITEM('')
SURFACE()
);
#2411=(
BOUNDED_SURFACE()
B_SPLINE_SURFACE(3,2,((#382657,#382658,#382659),(#382660,#382661,#382662),
(#382663,#382664,#382665),(#382666,#382667,#382668)),.UNSPECIFIED.,.F.,
 .F.,.F.)
B_SPLINE_SURFACE_WITH_KNOTS((4,4),(3,3),(0.00135801595889393,0.00148409170619832),
(0.,1.),.UNSPECIFIED.)
GEOMETRIC_REPRESENTATION_ITEM()
RATIONAL_B_SPLINE_SURFACE(((1.,0.818301933966442,1.),(1.,0.81722661317236,
1.),(1.,0.816179643373935,1.),(1.,0.815159387863652,1.)))
REPRESENTATION_ITEM('')
SURFACE()
);
#2412=(
BOUNDED_SURFACE()
B_SPLINE_SURFACE(3,2,((#382707,#382708,#382709),(#382710,#382711,#382712),
(#382713,#382714,#382715),(#382716,#382717,#382718)),.UNSPECIFIED.,.F.,
 .F.,.F.)
B_SPLINE_SURFACE_WITH_KNOTS((4,4),(3,3),(-1.54744435122025E-6,1.54744435122093E-5),
(-0.0151698983649992,1.),.UNSPECIFIED.)
GEOMETRIC_REPRESENTATION_ITEM()
RATIONAL_B_SPLINE_SURFACE(((1.02018382473345,0.334740937354653,1.),(1.00401234488902,
0.867753072812965,1.),(1.00033622856787,0.988917903080835,1.),(1.,1.,1.)))
REPRESENTATION_ITEM('')
SURFACE()
);
#2413=(
BOUNDED_SURFACE()
B_SPLINE_SURFACE(3,2,((#382720,#382721,#382722),(#382723,#382724,#382725),
(#382726,#382727,#382728),(#382729,#382730,#382731)),.UNSPECIFIED.,.F.,
 .F.,.F.)
B_SPLINE_SURFACE_WITH_KNOTS((4,4),(3,3),(0.00137194782501028,0.00149814269699235),
(0.,1.),.UNSPECIFIED.)
GEOMETRIC_REPRESENTATION_ITEM()
RATIONAL_B_SPLINE_SURFACE(((1.,0.815158509402317,1.),(1.,0.816179044148177,
1.),(1.,0.817226308119917,1.),(1.,0.81830193948881,1.)))
REPRESENTATION_ITEM('')
SURFACE()
);
#2414=(
BOUNDED_SURFACE()
B_SPLINE_SURFACE(3,2,((#382775,#382776,#382777),(#382778,#382779,#382780),
(#382781,#382782,#382783),(#382784,#382785,#382786)),.UNSPECIFIED.,.F.,
 .F.,.F.)
B_SPLINE_SURFACE_WITH_KNOTS((4,4),(3,3),(1.55009486301137E-5,4.92065510474434E-5),
(-8.13759515751784E-5,1.),.UNSPECIFIED.)
GEOMETRIC_REPRESENTATION_ITEM()
RATIONAL_B_SPLINE_SURFACE(((1.00002372912338,0.854200639599668,1.),(1.00001423585995,
0.912530301180522,1.),(1.00000710550472,0.95634149537743,1.),(1.0000123897591,
0.923873338137017,1.)))
REPRESENTATION_ITEM('')
SURFACE()
);
#2415=(
BOUNDED_SURFACE()
B_SPLINE_SURFACE(3,2,((#382790,#382791,#382792),(#382793,#382794,#382795),
(#382796,#382797,#382798),(#382799,#382800,#382801)),.UNSPECIFIED.,.F.,
 .F.,.F.)
B_SPLINE_SURFACE_WITH_KNOTS((4,4),(3,3),(-3.39934179457739E-6,3.73927597403563E-5),
(-0.00186004067473832,1.00069373317447),.UNSPECIFIED.)
GEOMETRIC_REPRESENTATION_ITEM()
RATIONAL_B_SPLINE_SURFACE(((1.00072100136076,0.806051963875238,1.00026859642694),
(1.00060048440172,0.838470803558532,1.00022369994498),(1.0005310644881,
0.857144632272293,1.00019783877222),(1.00054515072868,0.853355459539006,
1.00020308635439)))
REPRESENTATION_ITEM('')
SURFACE()
);
#2416=(
BOUNDED_SURFACE()
B_SPLINE_SURFACE(3,2,((#382803,#382804,#382805),(#382806,#382807,#382808),
(#382809,#382810,#382811),(#382812,#382813,#382814)),.UNSPECIFIED.,.F.,
 .F.,.F.)
B_SPLINE_SURFACE_WITH_KNOTS((4,4),(3,3),(-2.16840434497101E-19,9.54361881492172E-5),
(0.,1.),.UNSPECIFIED.)
GEOMETRIC_REPRESENTATION_ITEM()
RATIONAL_B_SPLINE_SURFACE(((1.,0.816715621142048,1.),(1.,0.815907587407942,
1.),(1.,0.81511595934521,1.),(1.,0.814339887349192,1.)))
REPRESENTATION_ITEM('')
SURFACE()
);
#2417=(
BOUNDED_SURFACE()
B_SPLINE_SURFACE(3,2,((#382816,#382817,#382818),(#382819,#382820,#382821),
(#382822,#382823,#382824),(#382825,#382826,#382827)),.UNSPECIFIED.,.F.,
 .F.,.F.)
B_SPLINE_SURFACE_WITH_KNOTS((4,4),(3,3),(4.40457132572236E-20,4.68197758448206E-5),
(0.,1.),.UNSPECIFIED.)
GEOMETRIC_REPRESENTATION_ITEM()
RATIONAL_B_SPLINE_SURFACE(((1.,0.816715621142052,1.),(1.,0.953638980025205,
1.),(1.,0.954506925408055,1.),(1.,0.816715621142055,1.)))
REPRESENTATION_ITEM('')
SURFACE()
);
#2418=(
BOUNDED_SURFACE()
B_SPLINE_SURFACE(3,2,((#382829,#382830,#382831),(#382832,#382833,#382834),
(#382835,#382836,#382837),(#382838,#382839,#382840)),.UNSPECIFIED.,.F.,
 .F.,.F.)
B_SPLINE_SURFACE_WITH_KNOTS((4,4),(3,3),(0.,9.54361881492178E-5),(0.,1.),
 .UNSPECIFIED.)
GEOMETRIC_REPRESENTATION_ITEM()
RATIONAL_B_SPLINE_SURFACE(((1.,0.8143398873492,1.),(1.,0.815115959345208,
1.),(1.,0.815907587407944,1.),(1.,0.816715621142052,1.)))
REPRESENTATION_ITEM('')
SURFACE()
);
#2419=(
BOUNDED_SURFACE()
B_SPLINE_SURFACE(3,2,((#382842,#382843,#382844),(#382845,#382846,#382847),
(#382848,#382849,#382850),(#382851,#382852,#382853)),.UNSPECIFIED.,.F.,
 .F.,.F.)
B_SPLINE_SURFACE_WITH_KNOTS((4,4),(3,3),(-3.3952839350249E-6,3.73481232852737E-5),
(-0.00165018033328263,1.),.UNSPECIFIED.)
GEOMETRIC_REPRESENTATION_ITEM()
RATIONAL_B_SPLINE_SURFACE(((1.00048354385566,0.853487571660404,1.),(1.00047110510921,
0.857256476851462,1.),(1.00053193201107,0.838826096655865,1.),(1.00063970687725,
0.806170615310108,0.999999999999999)))
REPRESENTATION_ITEM('')
SURFACE()
);
#2420=(
BOUNDED_SURFACE()
B_SPLINE_SURFACE(3,2,((#382857,#382858,#382859),(#382860,#382861,#382862),
(#382863,#382864,#382865),(#382866,#382867,#382868)),.UNSPECIFIED.,.F.,
 .F.,.F.)
B_SPLINE_SURFACE_WITH_KNOTS((4,4),(3,3),(2.02993869230504E-5,5.39756952686903E-5),
(-0.000116281069376645,1.),.UNSPECIFIED.)
GEOMETRIC_REPRESENTATION_ITEM()
RATIONAL_B_SPLINE_SURFACE(((1.00001770479722,0.923870681143052,1.),(1.00001014104054,
0.956394275543437,1.),(1.00002037300269,0.912397594905733,1.),(1.00003390859453,
0.854195550869932,1.)))
REPRESENTATION_ITEM('')
SURFACE()
);
#2421=(
BOUNDED_SURFACE()
B_SPLINE_SURFACE(3,2,((#382961,#382962,#382963),(#382964,#382965,#382966),
(#382967,#382968,#382969),(#382970,#382971,#382972)),.UNSPECIFIED.,.F.,
 .F.,.F.)
B_SPLINE_SURFACE_WITH_KNOTS((4,4),(3,3),(0.00135801595889393,0.00148409170619832),
(0.,1.),.UNSPECIFIED.)
GEOMETRIC_REPRESENTATION_ITEM()
RATIONAL_B_SPLINE_SURFACE(((1.,0.818301933966446,1.),(1.,0.817226613172346,
1.),(1.,0.816179643373951,1.),(1.,0.815159387863661,1.)))
REPRESENTATION_ITEM('')
SURFACE()
);
#2422=(
BOUNDED_SURFACE()
B_SPLINE_SURFACE(3,2,((#383011,#383012,#383013),(#383014,#383015,#383016),
(#383017,#383018,#383019),(#383020,#383021,#383022)),.UNSPECIFIED.,.F.,
 .F.,.F.)
B_SPLINE_SURFACE_WITH_KNOTS((4,4),(3,3),(-1.54744435122008E-6,1.54744435122076E-5),
(-0.0151698983742707,1.01516989834804),.UNSPECIFIED.)
GEOMETRIC_REPRESENTATION_ITEM()
RATIONAL_B_SPLINE_SURFACE(((1.02018382474597,0.32449821941359,1.02018382471054),
(1.00401234489151,0.865716921710459,1.00401234488447),(1.00033622856808,
0.988747276629742,1.00033622856749),(1.,1.,1.)))
REPRESENTATION_ITEM('')
SURFACE()
);
#2423=(
BOUNDED_SURFACE()
B_SPLINE_SURFACE(3,2,((#383024,#383025,#383026),(#383027,#383028,#383029),
(#383030,#383031,#383032),(#383033,#383034,#383035)),.UNSPECIFIED.,.F.,
 .F.,.F.)
B_SPLINE_SURFACE_WITH_KNOTS((4,4),(3,3),(0.00137194782501028,0.00149814269699235),
(0.,1.),.UNSPECIFIED.)
GEOMETRIC_REPRESENTATION_ITEM()
RATIONAL_B_SPLINE_SURFACE(((1.,0.81515850940232,1.),(1.,0.816179044148172,
1.),(1.,0.817226308119918,1.),(1.,0.818301939488811,1.)))
REPRESENTATION_ITEM('')
SURFACE()
);
#2424=(
BOUNDED_SURFACE()
B_SPLINE_SURFACE(3,2,((#383079,#383080,#383081),(#383082,#383083,#383084),
(#383085,#383086,#383087),(#383088,#383089,#383090)),.UNSPECIFIED.,.F.,
 .F.,.F.)
B_SPLINE_SURFACE_WITH_KNOTS((4,4),(3,3),(1.55009486301137E-5,4.92065510474435E-5),
(-8.13759513091309E-5,1.),.UNSPECIFIED.)
GEOMETRIC_REPRESENTATION_ITEM()
RATIONAL_B_SPLINE_SURFACE(((1.00002372912331,0.854200639599711,1.),(1.0000142358599,
0.912530301180553,1.),(1.00000710550469,0.956341495377436,1.),(1.00001238975906,
0.923873338137037,1.)))
REPRESENTATION_ITEM('')
SURFACE()
);
#2425=(
BOUNDED_SURFACE()
B_SPLINE_SURFACE(3,2,((#383094,#383095,#383096),(#383097,#383098,#383099),
(#383100,#383101,#383102),(#383103,#383104,#383105)),.UNSPECIFIED.,.F.,
 .F.,.F.)
B_SPLINE_SURFACE_WITH_KNOTS((4,4),(3,3),(-3.39934179457783E-6,3.73927597403565E-5),
(-0.00186004067468424,1.00069373317467),.UNSPECIFIED.)
GEOMETRIC_REPRESENTATION_ITEM()
RATIONAL_B_SPLINE_SURFACE(((1.00072100136074,0.806051963875206,1.00026859642702),
(1.0006004844017,0.838470803558528,1.00022369994505),(1.00053106448809,
0.857144632272264,1.00019783877227),(1.00054515072867,0.853355459538992,
1.00020308635445)))
REPRESENTATION_ITEM('')
SURFACE()
);
#2426=(
BOUNDED_SURFACE()
B_SPLINE_SURFACE(3,2,((#383107,#383108,#383109),(#383110,#383111,#383112),
(#383113,#383114,#383115),(#383116,#383117,#383118)),.UNSPECIFIED.,.F.,
 .F.,.F.)
B_SPLINE_SURFACE_WITH_KNOTS((4,4),(3,3),(4.33680868994202E-19,9.54361881492176E-5),
(0.,1.),.UNSPECIFIED.)
GEOMETRIC_REPRESENTATION_ITEM()
RATIONAL_B_SPLINE_SURFACE(((1.,0.81671562114205,1.),(1.,0.815907587407954,
1.),(1.,0.815115959345207,1.),(1.,0.814339887349196,1.)))
REPRESENTATION_ITEM('')
SURFACE()
);
#2427=(
BOUNDED_SURFACE()
B_SPLINE_SURFACE(3,2,((#383120,#383121,#383122),(#383123,#383124,#383125),
(#383126,#383127,#383128),(#383129,#383130,#383131)),.UNSPECIFIED.,.F.,
 .F.,.F.)
B_SPLINE_SURFACE_WITH_KNOTS((4,4),(3,3),(1.03338019565025E-19,4.68197758448208E-5),
(0.,1.),.UNSPECIFIED.)
GEOMETRIC_REPRESENTATION_ITEM()
RATIONAL_B_SPLINE_SURFACE(((1.,0.816715621142044,1.),(1.,0.953638980025212,
1.),(1.,0.954506925408053,1.),(1.,0.81671562114205,1.)))
REPRESENTATION_ITEM('')
SURFACE()
);
#2428=(
BOUNDED_SURFACE()
B_SPLINE_SURFACE(3,2,((#383133,#383134,#383135),(#383136,#383137,#383138),
(#383139,#383140,#383141),(#383142,#383143,#383144)),.UNSPECIFIED.,.F.,
 .F.,.F.)
B_SPLINE_SURFACE_WITH_KNOTS((4,4),(3,3),(1.62630325872826E-19,9.54361881492179E-5),
(0.,1.),.UNSPECIFIED.)
GEOMETRIC_REPRESENTATION_ITEM()
RATIONAL_B_SPLINE_SURFACE(((1.,0.81433988734919,1.),(1.,0.815115959345206,
1.),(1.,0.815907587407942,1.),(1.,0.816715621142044,1.)))
REPRESENTATION_ITEM('')
SURFACE()
);
#2429=(
BOUNDED_SURFACE()
B_SPLINE_SURFACE(3,2,((#383146,#383147,#383148),(#383149,#383150,#383151),
(#383152,#383153,#383154),(#383155,#383156,#383157)),.UNSPECIFIED.,.F.,
 .F.,.F.)
B_SPLINE_SURFACE_WITH_KNOTS((4,4),(3,3),(-3.39528393502381E-6,3.73481232852734E-5),
(-0.0016501803331559,1.),.UNSPECIFIED.)
GEOMETRIC_REPRESENTATION_ITEM()
RATIONAL_B_SPLINE_SURFACE(((1.00048354385562,0.853487571660411,1.),(1.00047110510917,
0.857256476851486,1.),(1.00053193201103,0.838826096655886,1.),(1.00063970687721,
0.806170615310118,1.)))
REPRESENTATION_ITEM('')
SURFACE()
);
#2430=(
BOUNDED_SURFACE()
B_SPLINE_SURFACE(3,2,((#383161,#383162,#383163),(#383164,#383165,#383166),
(#383167,#383168,#383169),(#383170,#383171,#383172)),.UNSPECIFIED.,.F.,
 .F.,.F.)
B_SPLINE_SURFACE_WITH_KNOTS((4,4),(3,3),(2.02993869230506E-5,5.39756952686892E-5),
(-0.000116281070440117,1.),.UNSPECIFIED.)
GEOMETRIC_REPRESENTATION_ITEM()
RATIONAL_B_SPLINE_SURFACE(((1.00001770479738,0.923870681142973,1.),(1.00001014104063,
0.956394275543383,1.),(1.00002037300287,0.912397594905633,1.),(1.00003390859484,
0.854195550869773,1.)))
REPRESENTATION_ITEM('')
SURFACE()
);
#2431=(
BOUNDED_SURFACE()
B_SPLINE_SURFACE(3,2,((#383265,#383266,#383267),(#383268,#383269,#383270),
(#383271,#383272,#383273),(#383274,#383275,#383276)),.UNSPECIFIED.,.F.,
 .F.,.F.)
B_SPLINE_SURFACE_WITH_KNOTS((4,4),(3,3),(0.00135801595889393,0.00148409170619832),
(0.,1.),.UNSPECIFIED.)
GEOMETRIC_REPRESENTATION_ITEM()
RATIONAL_B_SPLINE_SURFACE(((1.,0.818301933966448,1.),(1.,0.817226613172323,
1.),(1.,0.816179643373976,1.),(1.,0.815159387863649,1.)))
REPRESENTATION_ITEM('')
SURFACE()
);
#2432=(
BOUNDED_SURFACE()
B_SPLINE_SURFACE(3,2,((#383315,#383316,#383317),(#383318,#383319,#383320),
(#383321,#383322,#383323),(#383324,#383325,#383326)),.UNSPECIFIED.,.F.,
 .F.,.F.)
B_SPLINE_SURFACE_WITH_KNOTS((4,4),(3,3),(-1.54744435122076E-6,1.54744435122075E-5),
(-0.0151698983599064,1.01516989836254),.UNSPECIFIED.)
GEOMETRIC_REPRESENTATION_ITEM()
RATIONAL_B_SPLINE_SURFACE(((1.02018382472657,0.324498219413438,1.02018382473013),
(1.00401234488766,0.865716921710524,1.00401234488836),(1.00033622856776,
0.988747276629706,1.00033622856781),(1.,1.,1.)))
REPRESENTATION_ITEM('')
SURFACE()
);
#2433=(
BOUNDED_SURFACE()
B_SPLINE_SURFACE(3,2,((#383328,#383329,#383330),(#383331,#383332,#383333),
(#383334,#383335,#383336),(#383337,#383338,#383339)),.UNSPECIFIED.,.F.,
 .F.,.F.)
B_SPLINE_SURFACE_WITH_KNOTS((4,4),(3,3),(0.00137194782501028,0.00149814269699235),
(0.,1.),.UNSPECIFIED.)
GEOMETRIC_REPRESENTATION_ITEM()
RATIONAL_B_SPLINE_SURFACE(((1.,0.815158509402314,1.),(1.,0.816179044148168,
1.),(1.,0.817226308119925,1.),(1.,0.818301939488811,1.)))
REPRESENTATION_ITEM('')
SURFACE()
);
#2434=(
BOUNDED_SURFACE()
B_SPLINE_SURFACE(3,2,((#383383,#383384,#383385),(#383386,#383387,#383388),
(#383389,#383390,#383391),(#383392,#383393,#383394)),.UNSPECIFIED.,.F.,
 .F.,.F.)
B_SPLINE_SURFACE_WITH_KNOTS((4,4),(3,3),(1.55009486301138E-5,4.92065510474435E-5),
(-8.1375951280074E-5,1.),.UNSPECIFIED.)
GEOMETRIC_REPRESENTATION_ITEM()
RATIONAL_B_SPLINE_SURFACE(((1.0000237291233,0.854200639599717,1.),(1.0000142358599,
0.912530301180554,1.),(1.00000710550469,0.956341495377434,1.),(1.00001238975905,
0.923873338137037,1.)))
REPRESENTATION_ITEM('')
SURFACE()
);
#2435=(
BOUNDED_SURFACE()
B_SPLINE_SURFACE(3,2,((#383398,#383399,#383400),(#383401,#383402,#383403),
(#383404,#383405,#383406),(#383407,#383408,#383409)),.UNSPECIFIED.,.F.,
 .F.,.F.)
B_SPLINE_SURFACE_WITH_KNOTS((4,4),(3,3),(-3.39934179457824E-6,3.73927597403564E-5),
(-0.00186004067418031,1.00069373317447),.UNSPECIFIED.)
GEOMETRIC_REPRESENTATION_ITEM()
RATIONAL_B_SPLINE_SURFACE(((1.00072100136054,0.80605196387533,1.00026859642694),
(1.00060048440154,0.838470803558632,1.00022369994498),(1.00053106448795,
0.85714463227236,1.00019783877221),(1.00054515072852,0.853355459539088,
1.00020308635439)))
REPRESENTATION_ITEM('')
SURFACE()
);
#2436=(
BOUNDED_SURFACE()
B_SPLINE_SURFACE(3,2,((#383411,#383412,#383413),(#383414,#383415,#383416),
(#383417,#383418,#383419),(#383420,#383421,#383422)),.UNSPECIFIED.,.F.,
 .F.,.F.)
B_SPLINE_SURFACE_WITH_KNOTS((4,4),(3,3),(-5.42101086242752E-20,9.54361881492176E-5),
(0.,1.),.UNSPECIFIED.)
GEOMETRIC_REPRESENTATION_ITEM()
RATIONAL_B_SPLINE_SURFACE(((1.,0.816715621142047,1.),(1.,0.815907587407942,
1.),(1.,0.815115959345202,1.),(1.,0.814339887349191,1.)))
REPRESENTATION_ITEM('')
SURFACE()
);
#2437=(
BOUNDED_SURFACE()
B_SPLINE_SURFACE(3,2,((#383424,#383425,#383426),(#383427,#383428,#383429),
(#383430,#383431,#383432),(#383433,#383434,#383435)),.UNSPECIFIED.,.F.,
 .F.,.F.)
B_SPLINE_SURFACE_WITH_KNOTS((4,4),(3,3),(-8.13151629364128E-20,4.6819775844821E-5),
(0.,1.),.UNSPECIFIED.)
GEOMETRIC_REPRESENTATION_ITEM()
RATIONAL_B_SPLINE_SURFACE(((1.,0.816715621142044,1.),(1.,0.953638980025209,
1.),(1.,0.954506925408053,1.),(1.,0.816715621142054,1.)))
REPRESENTATION_ITEM('')
SURFACE()
);
#2438=(
BOUNDED_SURFACE()
B_SPLINE_SURFACE(3,2,((#383437,#383438,#383439),(#383440,#383441,#383442),
(#383443,#383444,#383445),(#383446,#383447,#383448)),.UNSPECIFIED.,.F.,
 .F.,.F.)
B_SPLINE_SURFACE_WITH_KNOTS((4,4),(3,3),(0.,9.54361881492175E-5),(0.,1.),
 .UNSPECIFIED.)
GEOMETRIC_REPRESENTATION_ITEM()
RATIONAL_B_SPLINE_SURFACE(((1.,0.814339887349196,1.),(1.,0.815115959345203,
1.),(1.,0.815907587407943,1.),(1.,0.816715621142047,1.)))
REPRESENTATION_ITEM('')
SURFACE()
);
#2439=(
BOUNDED_SURFACE()
B_SPLINE_SURFACE(3,2,((#383450,#383451,#383452),(#383453,#383454,#383455),
(#383456,#383457,#383458),(#383459,#383460,#383461)),.UNSPECIFIED.,.F.,
 .F.,.F.)
B_SPLINE_SURFACE_WITH_KNOTS((4,4),(3,3),(-3.39528393502484E-6,3.73481232852734E-5),
(-0.0016501803333211,1.),.UNSPECIFIED.)
GEOMETRIC_REPRESENTATION_ITEM()
RATIONAL_B_SPLINE_SURFACE(((1.00048354385567,0.853487571660387,1.),(1.00047110510922,
0.85725647685146,1.),(1.00053193201109,0.838826096655864,1.),(1.00063970687727,
0.806170615310083,1.)))
REPRESENTATION_ITEM('')
SURFACE()
);
#2440=(
BOUNDED_SURFACE()
B_SPLINE_SURFACE(3,2,((#383465,#383466,#383467),(#383468,#383469,#383470),
(#383471,#383472,#383473),(#383474,#383475,#383476)),.UNSPECIFIED.,.F.,
 .F.,.F.)
B_SPLINE_SURFACE_WITH_KNOTS((4,4),(3,3),(2.02993869230507E-5,5.397569526869E-5),
(-0.000116281069781334,1.),.UNSPECIFIED.)
GEOMETRIC_REPRESENTATION_ITEM()
RATIONAL_B_SPLINE_SURFACE(((1.00001770479728,0.923870681143021,1.),(1.00001014104058,
0.956394275543415,1.),(1.00002037300276,0.912397594905702,1.),(1.00003390859465,
0.85419555086987,1.)))
REPRESENTATION_ITEM('')
SURFACE()
);
#2441=(
BOUNDED_SURFACE()
B_SPLINE_SURFACE(3,2,((#383569,#383570,#383571),(#383572,#383573,#383574),
(#383575,#383576,#383577),(#383578,#383579,#383580)),.UNSPECIFIED.,.F.,
 .F.,.F.)
B_SPLINE_SURFACE_WITH_KNOTS((4,4),(3,3),(0.00135801595889393,0.00148409170619832),
(0.,1.),.UNSPECIFIED.)
GEOMETRIC_REPRESENTATION_ITEM()
RATIONAL_B_SPLINE_SURFACE(((1.,0.818301933966444,1.),(1.,0.817226613172353,
1.),(1.,0.816179643373948,1.),(1.,0.815159387863653,1.)))
REPRESENTATION_ITEM('')
SURFACE()
);
#2442=(
BOUNDED_SURFACE()
B_SPLINE_SURFACE(3,2,((#383619,#383620,#383621),(#383622,#383623,#383624),
(#383625,#383626,#383627),(#383628,#383629,#383630)),.UNSPECIFIED.,.F.,
 .F.,.F.)
B_SPLINE_SURFACE_WITH_KNOTS((4,4),(3,3),(3.19754937588498E-20,1.54744435122089E-5),
(0.,1.),.UNSPECIFIED.)
GEOMETRIC_REPRESENTATION_ITEM()
RATIONAL_B_SPLINE_SURFACE(((1.,0.478041569704873,1.),(1.,0.890533857552073,
1.),(1.,0.990075913815892,1.),(1.,1.,1.)))
REPRESENTATION_ITEM('')
SURFACE()
);
#2443=(
BOUNDED_SURFACE()
B_SPLINE_SURFACE(3,2,((#383632,#383633,#383634),(#383635,#383636,#383637),
(#383638,#383639,#383640),(#383641,#383642,#383643)),.UNSPECIFIED.,.F.,
 .F.,.F.)
B_SPLINE_SURFACE_WITH_KNOTS((4,4),(3,3),(0.00137194782501028,0.00149814269699235),
(0.,1.),.UNSPECIFIED.)
GEOMETRIC_REPRESENTATION_ITEM()
RATIONAL_B_SPLINE_SURFACE(((1.,0.815158509402317,1.),(1.,0.816179044148181,
1.),(1.,0.817226308119919,1.),(1.,0.818301939488807,1.)))
REPRESENTATION_ITEM('')
SURFACE()
);
#2444=(
BOUNDED_SURFACE()
B_SPLINE_SURFACE(3,2,((#383687,#383688,#383689),(#383690,#383691,#383692),
(#383693,#383694,#383695),(#383696,#383697,#383698)),.UNSPECIFIED.,.F.,
 .F.,.F.)
B_SPLINE_SURFACE_WITH_KNOTS((4,4),(3,3),(1.55009486301138E-5,4.92065510474436E-5),
(-8.13759515716345E-5,1.),.UNSPECIFIED.)
GEOMETRIC_REPRESENTATION_ITEM()
RATIONAL_B_SPLINE_SURFACE(((1.00002372912338,0.854200639599673,1.),(1.00001423585995,
0.912530301180534,1.),(1.00000710550472,0.956341495377423,1.),(1.0000123897591,
0.923873338137018,1.)))
REPRESENTATION_ITEM('')
SURFACE()
);
#2445=(
BOUNDED_SURFACE()
B_SPLINE_SURFACE(3,2,((#383702,#383703,#383704),(#383705,#383706,#383707),
(#383708,#383709,#383710),(#383711,#383712,#383713)),.UNSPECIFIED.,.F.,
 .F.,.F.)
B_SPLINE_SURFACE_WITH_KNOTS((4,4),(3,3),(-3.39934179457829E-6,3.73927597403563E-5),
(-0.00186004067487366,1.00069373317464),.UNSPECIFIED.)
GEOMETRIC_REPRESENTATION_ITEM()
RATIONAL_B_SPLINE_SURFACE(((1.00072100136081,0.806051963875175,1.000268596427),
(1.00060048440176,0.838470803558498,1.00022369994504),(1.00053106448814,
0.857144632272234,1.00019783877226),(1.00054515072872,0.853355459538972,
1.00020308635444)))
REPRESENTATION_ITEM('')
SURFACE()
);
#2446=(
BOUNDED_SURFACE()
B_SPLINE_SURFACE(3,2,((#383715,#383716,#383717),(#383718,#383719,#383720),
(#383721,#383722,#383723),(#383724,#383725,#383726)),.UNSPECIFIED.,.F.,
 .F.,.F.)
B_SPLINE_SURFACE_WITH_KNOTS((4,4),(3,3),(-5.42101086242752E-20,9.54361881492173E-5),
(0.,1.),.UNSPECIFIED.)
GEOMETRIC_REPRESENTATION_ITEM()
RATIONAL_B_SPLINE_SURFACE(((1.,0.816715621142058,1.),(1.,0.815907587407942,
1.),(1.,0.815115959345203,1.),(1.,0.814339887349202,1.)))
REPRESENTATION_ITEM('')
SURFACE()
);
#2447=(
BOUNDED_SURFACE()
B_SPLINE_SURFACE(3,2,((#383728,#383729,#383730),(#383731,#383732,#383733),
(#383734,#383735,#383736),(#383737,#383738,#383739)),.UNSPECIFIED.,.F.,
 .F.,.F.)
B_SPLINE_SURFACE_WITH_KNOTS((4,4),(3,3),(1.91429446079472E-19,4.68197758448213E-5),
(0.,1.),.UNSPECIFIED.)
GEOMETRIC_REPRESENTATION_ITEM()
RATIONAL_B_SPLINE_SURFACE(((1.,0.816715621142044,1.),(1.,0.953638980025207,
1.),(1.,0.954506925408054,1.),(1.,0.816715621142053,1.)))
REPRESENTATION_ITEM('')
SURFACE()
);
#2448=(
BOUNDED_SURFACE()
B_SPLINE_SURFACE(3,2,((#383741,#383742,#383743),(#383744,#383745,#383746),
(#383747,#383748,#383749),(#383750,#383751,#383752)),.UNSPECIFIED.,.F.,
 .F.,.F.)
B_SPLINE_SURFACE_WITH_KNOTS((4,4),(3,3),(-2.16840434497101E-19,9.54361881492177E-5),
(0.,1.),.UNSPECIFIED.)
GEOMETRIC_REPRESENTATION_ITEM()
RATIONAL_B_SPLINE_SURFACE(((1.,0.814339887349197,1.),(1.,0.815115959345205,
1.),(1.,0.815907587407944,1.),(1.,0.816715621142047,1.)))
REPRESENTATION_ITEM('')
SURFACE()
);
#2449=(
BOUNDED_SURFACE()
B_SPLINE_SURFACE(3,2,((#383754,#383755,#383756),(#383757,#383758,#383759),
(#383760,#383761,#383762),(#383763,#383764,#383765)),.UNSPECIFIED.,.F.,
 .F.,.F.)
B_SPLINE_SURFACE_WITH_KNOTS((4,4),(3,3),(-3.39528393502379E-6,3.73481232852736E-5),
(-0.00165018033327137,1.),.UNSPECIFIED.)
GEOMETRIC_REPRESENTATION_ITEM()
RATIONAL_B_SPLINE_SURFACE(((1.00048354385565,0.85348757166041,1.),(1.0004711051092,
0.857256476851454,1.),(1.00053193201107,0.83882609665588,1.),(1.00063970687725,
0.806170615310096,1.)))
REPRESENTATION_ITEM('')
SURFACE()
);
#2450=(
BOUNDED_SURFACE()
B_SPLINE_SURFACE(3,2,((#383769,#383770,#383771),(#383772,#383773,#383774),
(#383775,#383776,#383777),(#383778,#383779,#383780)),.UNSPECIFIED.,.F.,
 .F.,.F.)
B_SPLINE_SURFACE_WITH_KNOTS((4,4),(3,3),(2.02993869230508E-5,5.39756952686894E-5),
(-0.000116281069403863,1.),.UNSPECIFIED.)
GEOMETRIC_REPRESENTATION_ITEM()
RATIONAL_B_SPLINE_SURFACE(((1.00001770479722,0.923870681143049,1.),(1.00001014104054,
0.956394275543439,1.),(1.00002037300269,0.912397594905726,1.),(1.00003390859454,
0.854195550869924,1.)))
REPRESENTATION_ITEM('')
SURFACE()
);
#2451=(
BOUNDED_SURFACE()
B_SPLINE_SURFACE(3,2,((#383873,#383874,#383875),(#383876,#383877,#383878),
(#383879,#383880,#383881),(#383882,#383883,#383884)),.UNSPECIFIED.,.F.,
 .F.,.F.)
B_SPLINE_SURFACE_WITH_KNOTS((4,4),(3,3),(0.00135801595889393,0.00148409170619832),
(0.,1.),.UNSPECIFIED.)
GEOMETRIC_REPRESENTATION_ITEM()
RATIONAL_B_SPLINE_SURFACE(((1.,0.818301933966444,1.),(1.,0.817226613172333,
1.),(1.,0.816179643373965,1.),(1.,0.815159387863653,1.)))
REPRESENTATION_ITEM('')
SURFACE()
);
#2452=(
BOUNDED_SURFACE()
B_SPLINE_SURFACE(3,2,((#383923,#383924,#383925),(#383926,#383927,#383928),
(#383929,#383930,#383931),(#383932,#383933,#383934)),.UNSPECIFIED.,.F.,
 .F.,.F.)
B_SPLINE_SURFACE_WITH_KNOTS((4,4),(3,3),(-1.5474443512208E-6,1.54744435122078E-5),
(-0.0151698983643226,1.01516989835825),.UNSPECIFIED.)
GEOMETRIC_REPRESENTATION_ITEM()
RATIONAL_B_SPLINE_SURFACE(((1.02018382473254,0.324498219413273,1.02018382472433),
(1.00401234488884,0.865716921710659,1.00401234488721),(1.00033622856786,
0.988747276629648,1.00033622856772),(1.,1.,1.)))
REPRESENTATION_ITEM('')
SURFACE()
);
#2453=(
BOUNDED_SURFACE()
B_SPLINE_SURFACE(3,2,((#383936,#383937,#383938),(#383939,#383940,#383941),
(#383942,#383943,#383944),(#383945,#383946,#383947)),.UNSPECIFIED.,.F.,
 .F.,.F.)
B_SPLINE_SURFACE_WITH_KNOTS((4,4),(3,3),(0.00137194782501028,0.00149814269699235),
(0.,1.),.UNSPECIFIED.)
GEOMETRIC_REPRESENTATION_ITEM()
RATIONAL_B_SPLINE_SURFACE(((1.,0.815158509402318,1.),(1.,0.816179044148162,
1.),(1.,0.81722630811993,1.),(1.,0.818301939488811,1.)))
REPRESENTATION_ITEM('')
SURFACE()
);
#2454=(
BOUNDED_SURFACE()
B_SPLINE_SURFACE(3,2,((#383991,#383992,#383993),(#383994,#383995,#383996),
(#383997,#383998,#383999),(#384000,#384001,#384002)),.UNSPECIFIED.,.F.,
 .F.,.F.)
B_SPLINE_SURFACE_WITH_KNOTS((4,4),(3,3),(1.55009486301137E-5,4.9206551047443E-5),
(-8.13759512068241E-5,1.),.UNSPECIFIED.)
GEOMETRIC_REPRESENTATION_ITEM()
RATIONAL_B_SPLINE_SURFACE(((1.00002372912328,0.854200639599729,1.),(1.00001423585989,
0.912530301180557,1.),(1.00000710550468,0.956341495377445,1.),(1.00001238975904,
0.923873338137045,1.)))
REPRESENTATION_ITEM('')
SURFACE()
);
#2455=(
BOUNDED_SURFACE()
B_SPLINE_SURFACE(3,2,((#384006,#384007,#384008),(#384009,#384010,#384011),
(#384012,#384013,#384014),(#384015,#384016,#384017)),.UNSPECIFIED.,.F.,
 .F.,.F.)
B_SPLINE_SURFACE_WITH_KNOTS((4,4),(3,3),(-3.39934179457836E-6,3.73927597403565E-5),
(-0.00186004067393548,1.0006937331742),.UNSPECIFIED.)
GEOMETRIC_REPRESENTATION_ITEM()
RATIONAL_B_SPLINE_SURFACE(((1.00072100136045,0.80605196387545,1.00026859642683),
(1.00060048440146,0.838470803558697,1.00022369994489),(1.00053106448788,
0.857144632272436,1.00019783877214),(1.00054515072845,0.853355459539174,
1.00020308635431)))
REPRESENTATION_ITEM('')
SURFACE()
);
#2456=(
BOUNDED_SURFACE()
B_SPLINE_SURFACE(3,2,((#384019,#384020,#384021),(#384022,#384023,#384024),
(#384025,#384026,#384027),(#384028,#384029,#384030)),.UNSPECIFIED.,.F.,
 .F.,.F.)
B_SPLINE_SURFACE_WITH_KNOTS((4,4),(3,3),(-5.42101086242752E-20,9.54361881492175E-5),
(0.,1.),.UNSPECIFIED.)
GEOMETRIC_REPRESENTATION_ITEM()
RATIONAL_B_SPLINE_SURFACE(((1.,0.81671562114205,1.),(1.,0.815907587407945,
1.),(1.,0.815115959345207,1.),(1.,0.814339887349188,1.)))
REPRESENTATION_ITEM('')
SURFACE()
);
#2457=(
BOUNDED_SURFACE()
B_SPLINE_SURFACE(3,2,((#384032,#384033,#384034),(#384035,#384036,#384037),
(#384038,#384039,#384040),(#384041,#384042,#384043)),.UNSPECIFIED.,.F.,
 .F.,.F.)
B_SPLINE_SURFACE_WITH_KNOTS((4,4),(3,3),(5.25160427297666E-20,4.68197758448206E-5),
(0.,1.),.UNSPECIFIED.)
GEOMETRIC_REPRESENTATION_ITEM()
RATIONAL_B_SPLINE_SURFACE(((1.,0.816715621142045,1.),(1.,0.953638980025207,
1.),(1.,0.954506925408054,1.),(1.,0.816715621142054,1.)))
REPRESENTATION_ITEM('')
SURFACE()
);
#2458=(
BOUNDED_SURFACE()
B_SPLINE_SURFACE(3,2,((#384045,#384046,#384047),(#384048,#384049,#384050),
(#384051,#384052,#384053),(#384054,#384055,#384056)),.UNSPECIFIED.,.F.,
 .F.,.F.)
B_SPLINE_SURFACE_WITH_KNOTS((4,4),(3,3),(5.42101086242752E-20,9.54361881492178E-5),
(0.,1.),.UNSPECIFIED.)
GEOMETRIC_REPRESENTATION_ITEM()
RATIONAL_B_SPLINE_SURFACE(((1.,0.814339887349191,1.),(1.,0.815115959345209,
1.),(1.,0.815907587407936,1.),(1.,0.816715621142049,1.)))
REPRESENTATION_ITEM('')
SURFACE()
);
#2459=(
BOUNDED_SURFACE()
B_SPLINE_SURFACE(3,2,((#384058,#384059,#384060),(#384061,#384062,#384063),
(#384064,#384065,#384066),(#384067,#384068,#384069)),.UNSPECIFIED.,.F.,
 .F.,.F.)
B_SPLINE_SURFACE_WITH_KNOTS((4,4),(3,3),(-3.39528393502487E-6,3.73481232852724E-5),
(-0.00165018033260751,1.),.UNSPECIFIED.)
GEOMETRIC_REPRESENTATION_ITEM()
RATIONAL_B_SPLINE_SURFACE(((1.00048354385546,0.853487571660499,1.),(1.00047110510901,
0.857256476851543,1.),(1.00053193201086,0.838826096655999,1.),(1.00063970687699,
0.806170615310219,0.999999999999999)))
REPRESENTATION_ITEM('')
SURFACE()
);
#2460=(
BOUNDED_SURFACE()
B_SPLINE_SURFACE(3,2,((#384073,#384074,#384075),(#384076,#384077,#384078),
(#384079,#384080,#384081),(#384082,#384083,#384084)),.UNSPECIFIED.,.F.,
 .F.,.F.)
B_SPLINE_SURFACE_WITH_KNOTS((4,4),(3,3),(2.02993869230509E-5,5.39756952686904E-5),
(-0.000116281069838297,1.),.UNSPECIFIED.)
GEOMETRIC_REPRESENTATION_ITEM()
RATIONAL_B_SPLINE_SURFACE(((1.00001770479729,0.923870681143015,1.),(1.00001014104058,
0.956394275543424,1.),(1.00002037300277,0.912397594905687,1.),(1.00003390859466,
0.854195550869865,1.)))
REPRESENTATION_ITEM('')
SURFACE()
);
#2461=(
BOUNDED_SURFACE()
B_SPLINE_SURFACE(3,2,((#384177,#384178,#384179),(#384180,#384181,#384182),
(#384183,#384184,#384185),(#384186,#384187,#384188)),.UNSPECIFIED.,.F.,
 .F.,.F.)
B_SPLINE_SURFACE_WITH_KNOTS((4,4),(3,3),(0.00135801595889393,0.00148409170619832),
(0.,1.),.UNSPECIFIED.)
GEOMETRIC_REPRESENTATION_ITEM()
RATIONAL_B_SPLINE_SURFACE(((1.,0.818301933966448,1.),(1.,0.817226613172348,
1.),(1.,0.81617964337395,1.),(1.,0.815159387863654,1.)))
REPRESENTATION_ITEM('')
SURFACE()
);
#2462=(
BOUNDED_SURFACE()
B_SPLINE_SURFACE(3,2,((#384227,#384228,#384229),(#384230,#384231,#384232),
(#384233,#384234,#384235),(#384236,#384237,#384238)),.UNSPECIFIED.,.F.,
 .F.,.F.)
B_SPLINE_SURFACE_WITH_KNOTS((4,4),(3,3),(-1.5474443512208E-6,1.5474443512208E-5),
(-0.0151698983683404,1.01516989835403),.UNSPECIFIED.)
GEOMETRIC_REPRESENTATION_ITEM()
RATIONAL_B_SPLINE_SURFACE(((1.02018382473796,0.324498219413477,1.02018382471863),
(1.00401234488992,0.865716921710568,1.00401234488608),(1.00033622856795,
0.988747276629655,1.00033622856762),(1.,1.,1.)))
REPRESENTATION_ITEM('')
SURFACE()
);
#2463=(
BOUNDED_SURFACE()
B_SPLINE_SURFACE(3,2,((#384240,#384241,#384242),(#384243,#384244,#384245),
(#384246,#384247,#384248),(#384249,#384250,#384251)),.UNSPECIFIED.,.F.,
 .F.,.F.)
B_SPLINE_SURFACE_WITH_KNOTS((4,4),(3,3),(0.00137194782501028,0.00149814269699235),
(0.,1.),.UNSPECIFIED.)
GEOMETRIC_REPRESENTATION_ITEM()
RATIONAL_B_SPLINE_SURFACE(((1.,0.815158509402319,1.),(1.,0.816179044148174,
1.),(1.,0.817226308119916,1.),(1.,0.818301939488812,1.)))
REPRESENTATION_ITEM('')
SURFACE()
);
#2464=(
BOUNDED_SURFACE()
B_SPLINE_SURFACE(3,2,((#384295,#384296,#384297),(#384298,#384299,#384300),
(#384301,#384302,#384303),(#384304,#384305,#384306)),.UNSPECIFIED.,.F.,
 .F.,.F.)
B_SPLINE_SURFACE_WITH_KNOTS((4,4),(3,3),(1.55009486301138E-5,4.9206551047444E-5),
(-8.13759517028193E-5,1.),.UNSPECIFIED.)
GEOMETRIC_REPRESENTATION_ITEM()
RATIONAL_B_SPLINE_SURFACE(((1.00002372912342,0.854200639599655,1.),(1.00001423585997,
0.912530301180528,1.),(1.00000710550473,0.956341495377415,1.),(1.00001238975912,
0.923873338137004,1.)))
REPRESENTATION_ITEM('')
SURFACE()
);
#2465=(
BOUNDED_SURFACE()
B_SPLINE_SURFACE(3,2,((#384310,#384311,#384312),(#384313,#384314,#384315),
(#384316,#384317,#384318),(#384319,#384320,#384321)),.UNSPECIFIED.,.F.,
 .F.,.F.)
B_SPLINE_SURFACE_WITH_KNOTS((4,4),(3,3),(-3.39934179457804E-6,3.73927597403566E-5),
(-0.00186004067478799,1.00069373317431),.UNSPECIFIED.)
GEOMETRIC_REPRESENTATION_ITEM()
RATIONAL_B_SPLINE_SURFACE(((1.00072100136078,0.806051963875266,1.00026859642688),
(1.00060048440173,0.838470803558537,1.00022369994493),(1.00053106448812,
0.857144632272323,1.00019783877217),(1.0005451507287,0.85335545953902,1.00020308635434)))
REPRESENTATION_ITEM('')
SURFACE()
);
#2466=(
BOUNDED_SURFACE()
B_SPLINE_SURFACE(3,2,((#384323,#384324,#384325),(#384326,#384327,#384328),
(#384329,#384330,#384331),(#384332,#384333,#384334)),.UNSPECIFIED.,.F.,
 .F.,.F.)
B_SPLINE_SURFACE_WITH_KNOTS((4,4),(3,3),(0.,9.54361881492173E-5),(0.,1.),
 .UNSPECIFIED.)
GEOMETRIC_REPRESENTATION_ITEM()
RATIONAL_B_SPLINE_SURFACE(((1.,0.816715621142051,1.),(1.,0.815907587407942,
1.),(1.,0.815115959345209,1.),(1.,0.814339887349193,1.)))
REPRESENTATION_ITEM('')
SURFACE()
);
#2467=(
BOUNDED_SURFACE()
B_SPLINE_SURFACE(3,2,((#384336,#384337,#384338),(#384339,#384340,#384341),
(#384342,#384343,#384344),(#384345,#384346,#384347)),.UNSPECIFIED.,.F.,
 .F.,.F.)
B_SPLINE_SURFACE_WITH_KNOTS((4,4),(3,3),(1.01643953670516E-20,4.68197758448216E-5),
(0.,1.),.UNSPECIFIED.)
GEOMETRIC_REPRESENTATION_ITEM()
RATIONAL_B_SPLINE_SURFACE(((1.,0.816715621142039,1.),(1.,0.95363898002521,
1.),(1.,0.954506925408058,1.),(1.,0.816715621142055,1.)))
REPRESENTATION_ITEM('')
SURFACE()
);
#2468=(
BOUNDED_SURFACE()
B_SPLINE_SURFACE(3,2,((#384349,#384350,#384351),(#384352,#384353,#384354),
(#384355,#384356,#384357),(#384358,#384359,#384360)),.UNSPECIFIED.,.F.,
 .F.,.F.)
B_SPLINE_SURFACE_WITH_KNOTS((4,4),(3,3),(0.,9.54361881492177E-5),(0.,1.),
 .UNSPECIFIED.)
GEOMETRIC_REPRESENTATION_ITEM()
RATIONAL_B_SPLINE_SURFACE(((1.,0.814339887349194,1.),(1.,0.815115959345197,
1.),(1.,0.815907587407955,1.),(1.,0.816715621142046,1.)))
REPRESENTATION_ITEM('')
SURFACE()
);
#2469=(
BOUNDED_SURFACE()
B_SPLINE_SURFACE(3,2,((#384362,#384363,#384364),(#384365,#384366,#384367),
(#384368,#384369,#384370),(#384371,#384372,#384373)),.UNSPECIFIED.,.F.,
 .F.,.F.)
B_SPLINE_SURFACE_WITH_KNOTS((4,4),(3,3),(-3.39528393502377E-6,3.73481232852734E-5),
(-0.00165018033340471,1.),.UNSPECIFIED.)
GEOMETRIC_REPRESENTATION_ITEM()
RATIONAL_B_SPLINE_SURFACE(((1.00048354385569,0.853487571660383,1.),(1.00047110510924,
0.857256476851451,1.),(1.00053193201111,0.838826096655851,1.),(1.0006397068773,
0.806170615310069,1.)))
REPRESENTATION_ITEM('')
SURFACE()
);
#2470=(
BOUNDED_SURFACE()
B_SPLINE_SURFACE(3,2,((#384377,#384378,#384379),(#384380,#384381,#384382),
(#384383,#384384,#384385),(#384386,#384387,#384388)),.UNSPECIFIED.,.F.,
 .F.,.F.)
B_SPLINE_SURFACE_WITH_KNOTS((4,4),(3,3),(2.02993869230508E-5,5.397569526869E-5),
(-0.000116281070011194,1.),.UNSPECIFIED.)
GEOMETRIC_REPRESENTATION_ITEM()
RATIONAL_B_SPLINE_SURFACE(((1.00001770479731,0.923870681143,1.),(1.0000101410406,
0.956394275543404,1.),(1.0000203730028,0.912397594905675,1.),(1.00003390859471,
0.854195550869839,1.)))
REPRESENTATION_ITEM('')
SURFACE()
);
#2471=(
BOUNDED_SURFACE()
B_SPLINE_SURFACE(3,2,((#384481,#384482,#384483),(#384484,#384485,#384486),
(#384487,#384488,#384489),(#384490,#384491,#384492)),.UNSPECIFIED.,.F.,
 .F.,.F.)
B_SPLINE_SURFACE_WITH_KNOTS((4,4),(3,3),(0.00135801595889393,0.00148409170619832),
(0.,1.),.UNSPECIFIED.)
GEOMETRIC_REPRESENTATION_ITEM()
RATIONAL_B_SPLINE_SURFACE(((1.,0.818301933966444,1.),(1.,0.81722661317233,
1.),(1.,0.816179643373973,1.),(1.,0.815159387863652,1.)))
REPRESENTATION_ITEM('')
SURFACE()
);
#2472=(
BOUNDED_SURFACE()
B_SPLINE_SURFACE(3,2,((#384531,#384532,#384533),(#384534,#384535,#384536),
(#384537,#384538,#384539),(#384540,#384541,#384542)),.UNSPECIFIED.,.F.,
 .F.,.F.)
B_SPLINE_SURFACE_WITH_KNOTS((4,4),(3,3),(-1.54744435122086E-6,1.54744435122084E-5),
(-0.0151698983566559,1.01516989836567),.UNSPECIFIED.)
GEOMETRIC_REPRESENTATION_ITEM()
RATIONAL_B_SPLINE_SURFACE(((1.02018382472218,0.324498219413471,1.02018382473435),
(1.00401234488678,0.865716921710634,1.0040123448892),(1.00033622856768,
0.988747276629699,1.00033622856788),(1.,1.,1.)))
REPRESENTATION_ITEM('')
SURFACE()
);
#2473=(
BOUNDED_SURFACE()
B_SPLINE_SURFACE(3,2,((#384544,#384545,#384546),(#384547,#384548,#384549),
(#384550,#384551,#384552),(#384553,#384554,#384555)),.UNSPECIFIED.,.F.,
 .F.,.F.)
B_SPLINE_SURFACE_WITH_KNOTS((4,4),(3,3),(0.00137194782501028,0.00149814269699235),
(0.,1.),.UNSPECIFIED.)
GEOMETRIC_REPRESENTATION_ITEM()
RATIONAL_B_SPLINE_SURFACE(((1.,0.815158509402317,1.),(1.,0.816179044148182,
1.),(1.,0.817226308119902,1.),(1.,0.81830193948882,1.)))
REPRESENTATION_ITEM('')
SURFACE()
);
#2474=(
BOUNDED_SURFACE()
B_SPLINE_SURFACE(3,2,((#384599,#384600,#384601),(#384602,#384603,#384604),
(#384605,#384606,#384607),(#384608,#384609,#384610)),.UNSPECIFIED.,.F.,
 .F.,.F.)
B_SPLINE_SURFACE_WITH_KNOTS((4,4),(3,3),(1.55009486301137E-5,4.92065510474432E-5),
(-8.13759511476216E-5,1.),.UNSPECIFIED.)
GEOMETRIC_REPRESENTATION_ITEM()
RATIONAL_B_SPLINE_SURFACE(((1.00002372912326,0.854200639599733,1.),(1.00001423585988,
0.912530301180572,1.),(1.00000710550468,0.956341495377445,1.),(1.00001238975903,
0.923873338137047,1.)))
REPRESENTATION_ITEM('')
SURFACE()
);
#2475=(
BOUNDED_SURFACE()
B_SPLINE_SURFACE(3,2,((#384614,#384615,#384616),(#384617,#384618,#384619),
(#384620,#384621,#384622),(#384623,#384624,#384625)),.UNSPECIFIED.,.F.,
 .F.,.F.)
B_SPLINE_SURFACE_WITH_KNOTS((4,4),(3,3),(-3.39934179457803E-6,3.73927597403565E-5),
(-0.00186004067432212,1.00069373317451),.UNSPECIFIED.)
GEOMETRIC_REPRESENTATION_ITEM()
RATIONAL_B_SPLINE_SURFACE(((1.0007210013606,0.806051963875291,1.00026859642695),
(1.00060048440158,0.838470803558606,1.00022369994499),(1.00053106448799,
0.857144632272342,1.00019783877223),(1.00054515072856,0.853355459539061,
1.0002030863544)))
REPRESENTATION_ITEM('')
SURFACE()
);
#2476=(
BOUNDED_SURFACE()
B_SPLINE_SURFACE(3,2,((#384627,#384628,#384629),(#384630,#384631,#384632),
(#384633,#384634,#384635),(#384636,#384637,#384638)),.UNSPECIFIED.,.F.,
 .F.,.F.)
B_SPLINE_SURFACE_WITH_KNOTS((4,4),(3,3),(-2.16840434497101E-19,9.54361881492172E-5),
(0.,1.),.UNSPECIFIED.)
GEOMETRIC_REPRESENTATION_ITEM()
RATIONAL_B_SPLINE_SURFACE(((1.,0.816715621142053,1.),(1.,0.815907587407932,
1.),(1.,0.815115959345205,1.),(1.,0.814339887349196,1.)))
REPRESENTATION_ITEM('')
SURFACE()
);
#2477=(
BOUNDED_SURFACE()
B_SPLINE_SURFACE(3,2,((#384640,#384641,#384642),(#384643,#384644,#384645),
(#384646,#384647,#384648),(#384649,#384650,#384651)),.UNSPECIFIED.,.F.,
 .F.,.F.)
B_SPLINE_SURFACE_WITH_KNOTS((4,4),(3,3),(2.21922632180627E-19,4.68197758448208E-5),
(0.,1.),.UNSPECIFIED.)
GEOMETRIC_REPRESENTATION_ITEM()
RATIONAL_B_SPLINE_SURFACE(((1.,0.81671562114205,1.),(1.,0.9536389800252,
1.),(1.,0.954506925408054,1.),(1.,0.816715621142053,1.)))
REPRESENTATION_ITEM('')
SURFACE()
);
#2478=(
BOUNDED_SURFACE()
B_SPLINE_SURFACE(3,2,((#384653,#384654,#384655),(#384656,#384657,#384658),
(#384659,#384660,#384661),(#384662,#384663,#384664)),.UNSPECIFIED.,.F.,
 .F.,.F.)
B_SPLINE_SURFACE_WITH_KNOTS((4,4),(3,3),(-3.79470760369927E-19,9.54361881492173E-5),
(0.,1.),.UNSPECIFIED.)
GEOMETRIC_REPRESENTATION_ITEM()
RATIONAL_B_SPLINE_SURFACE(((1.,0.814339887349193,1.),(1.,0.81511595934522,
1.),(1.,0.815907587407937,1.),(1.,0.81671562114205,1.)))
REPRESENTATION_ITEM('')
SURFACE()
);
#2479=(
BOUNDED_SURFACE()
B_SPLINE_SURFACE(3,2,((#384666,#384667,#384668),(#384669,#384670,#384671),
(#384672,#384673,#384674),(#384675,#384676,#384677)),.UNSPECIFIED.,.F.,
 .F.,.F.)
B_SPLINE_SURFACE_WITH_KNOTS((4,4),(3,3),(-3.39528393502489E-6,3.73481232852735E-5),
(-0.00165018033256893,1.),.UNSPECIFIED.)
GEOMETRIC_REPRESENTATION_ITEM()
RATIONAL_B_SPLINE_SURFACE(((1.00048354385545,0.853487571660496,1.),(1.000471105109,
0.857256476851579,1.),(1.00053193201084,0.838826096655986,1.),(1.00063970687698,
0.806170615310235,1.)))
REPRESENTATION_ITEM('')
SURFACE()
);
#2480=(
BOUNDED_SURFACE()
B_SPLINE_SURFACE(3,2,((#384681,#384682,#384683),(#384684,#384685,#384686),
(#384687,#384688,#384689),(#384690,#384691,#384692)),.UNSPECIFIED.,.F.,
 .F.,.F.)
B_SPLINE_SURFACE_WITH_KNOTS((4,4),(3,3),(2.0299386923051E-5,5.39756952687128E-5),
(-0.000116281069528885,1.),.UNSPECIFIED.)
GEOMETRIC_REPRESENTATION_ITEM()
RATIONAL_B_SPLINE_SURFACE(((1.00001770479724,0.923870681143037,1.),(1.00001014104055,
0.956394275543469,1.),(1.00002037300272,0.912397594905643,1.),(1.00003390859457,
0.854195550869799,1.)))
REPRESENTATION_ITEM('')
SURFACE()
);
#2481=(
BOUNDED_SURFACE()
B_SPLINE_SURFACE(3,2,((#384785,#384786,#384787),(#384788,#384789,#384790),
(#384791,#384792,#384793),(#384794,#384795,#384796)),.UNSPECIFIED.,.F.,
 .F.,.F.)
B_SPLINE_SURFACE_WITH_KNOTS((4,4),(3,3),(0.00135801595889393,0.00148409170619832),
(0.,1.),.UNSPECIFIED.)
GEOMETRIC_REPRESENTATION_ITEM()
RATIONAL_B_SPLINE_SURFACE(((1.,0.818301933966446,1.),(1.,0.817226613172343,
1.),(1.,0.816179643373963,1.),(1.,0.815159387863655,1.)))
REPRESENTATION_ITEM('')
SURFACE()
);
#2482=(
BOUNDED_SURFACE()
B_SPLINE_SURFACE(3,2,((#384835,#384836,#384837),(#384838,#384839,#384840),
(#384841,#384842,#384843),(#384844,#384845,#384846)),.UNSPECIFIED.,.F.,
 .F.,.F.)
B_SPLINE_SURFACE_WITH_KNOTS((4,4),(3,3),(3.15519772852227E-20,1.54744435122079E-5),
(0.,1.),.UNSPECIFIED.)
GEOMETRIC_REPRESENTATION_ITEM()
RATIONAL_B_SPLINE_SURFACE(((1.,0.478041569704962,1.),(1.,0.890533857552089,
1.),(1.,0.990075913815913,1.),(1.,1.,1.)))
REPRESENTATION_ITEM('')
SURFACE()
);
#2483=(
BOUNDED_SURFACE()
B_SPLINE_SURFACE(3,2,((#384848,#384849,#384850),(#384851,#384852,#384853),
(#384854,#384855,#384856),(#384857,#384858,#384859)),.UNSPECIFIED.,.F.,
 .F.,.F.)
B_SPLINE_SURFACE_WITH_KNOTS((4,4),(3,3),(0.00137194782501028,0.00149814269699235),
(0.,1.),.UNSPECIFIED.)
GEOMETRIC_REPRESENTATION_ITEM()
RATIONAL_B_SPLINE_SURFACE(((1.,0.815158509402321,1.),(1.,0.816179044148162,
1.),(1.,0.817226308119932,1.),(1.,0.818301939488813,1.)))
REPRESENTATION_ITEM('')
SURFACE()
);
#2484=(
BOUNDED_SURFACE()
B_SPLINE_SURFACE(3,2,((#384903,#384904,#384905),(#384906,#384907,#384908),
(#384909,#384910,#384911),(#384912,#384913,#384914)),.UNSPECIFIED.,.F.,
 .F.,.F.)
B_SPLINE_SURFACE_WITH_KNOTS((4,4),(3,3),(1.55009486301137E-5,4.92065510474437E-5),
(-8.13759516774955E-5,1.),.UNSPECIFIED.)
GEOMETRIC_REPRESENTATION_ITEM()
RATIONAL_B_SPLINE_SURFACE(((1.00002372912341,0.854200639599657,1.),(1.00001423585997,
0.912530301180526,1.),(1.00000710550473,0.956341495377421,1.),(1.00001238975911,
0.923873338137008,1.)))
REPRESENTATION_ITEM('')
SURFACE()
);
#2485=(
BOUNDED_SURFACE()
B_SPLINE_SURFACE(3,2,((#384918,#384919,#384920),(#384921,#384922,#384923),
(#384924,#384925,#384926),(#384927,#384928,#384929)),.UNSPECIFIED.,.F.,
 .F.,.F.)
B_SPLINE_SURFACE_WITH_KNOTS((4,4),(3,3),(-3.39934179457824E-6,3.73927597403566E-5),
(-0.00186004067402246,1.00069373317468),.UNSPECIFIED.)
GEOMETRIC_REPRESENTATION_ITEM()
RATIONAL_B_SPLINE_SURFACE(((1.00072100136048,0.806051963875315,1.00026859642702),
(1.00060048440149,0.838470803558637,1.00022369994505),(1.0005310644879,
0.857144632272356,1.00019783877227),(1.00054515072847,0.853355459539086,
1.00020308635445)))
REPRESENTATION_ITEM('')
SURFACE()
);
#2486=(
BOUNDED_SURFACE()
B_SPLINE_SURFACE(3,2,((#384931,#384932,#384933),(#384934,#384935,#384936),
(#384937,#384938,#384939),(#384940,#384941,#384942)),.UNSPECIFIED.,.F.,
 .F.,.F.)
B_SPLINE_SURFACE_WITH_KNOTS((4,4),(3,3),(1.62630325872826E-19,9.54361881492175E-5),
(0.,1.),.UNSPECIFIED.)
GEOMETRIC_REPRESENTATION_ITEM()
RATIONAL_B_SPLINE_SURFACE(((1.,0.816715621142049,1.),(1.,0.815907587407945,
1.),(1.,0.815115959345202,1.),(1.,0.814339887349198,1.)))
REPRESENTATION_ITEM('')
SURFACE()
);
#2487=(
BOUNDED_SURFACE()
B_SPLINE_SURFACE(3,2,((#384944,#384945,#384946),(#384947,#384948,#384949),
(#384950,#384951,#384952),(#384953,#384954,#384955)),.UNSPECIFIED.,.F.,
 .F.,.F.)
B_SPLINE_SURFACE_WITH_KNOTS((4,4),(3,3),(5.59041745187838E-20,4.68197758448204E-5),
(0.,1.),.UNSPECIFIED.)
GEOMETRIC_REPRESENTATION_ITEM()
RATIONAL_B_SPLINE_SURFACE(((1.,0.81671562114205,1.),(1.,0.953638980025201,
1.),(1.,0.954506925408057,1.),(1.,0.816715621142055,1.)))
REPRESENTATION_ITEM('')
SURFACE()
);
#2488=(
BOUNDED_SURFACE()
B_SPLINE_SURFACE(3,2,((#384957,#384958,#384959),(#384960,#384961,#384962),
(#384963,#384964,#384965),(#384966,#384967,#384968)),.UNSPECIFIED.,.F.,
 .F.,.F.)
B_SPLINE_SURFACE_WITH_KNOTS((4,4),(3,3),(-5.42101086242752E-20,9.54361881492176E-5),
(0.,1.),.UNSPECIFIED.)
GEOMETRIC_REPRESENTATION_ITEM()
RATIONAL_B_SPLINE_SURFACE(((1.,0.814339887349194,1.),(1.,0.815115959345203,
1.),(1.,0.815907587407944,1.),(1.,0.81671562114205,1.)))
REPRESENTATION_ITEM('')
SURFACE()
);
#2489=(
BOUNDED_SURFACE()
B_SPLINE_SURFACE(3,2,((#384970,#384971,#384972),(#384973,#384974,#384975),
(#384976,#384977,#384978),(#384979,#384980,#384981)),.UNSPECIFIED.,.F.,
 .F.,.F.)
B_SPLINE_SURFACE_WITH_KNOTS((4,4),(3,3),(-3.3952839350249E-6,3.73481232852735E-5),
(-0.00165018033317863,1.),.UNSPECIFIED.)
GEOMETRIC_REPRESENTATION_ITEM()
RATIONAL_B_SPLINE_SURFACE(((1.00048354385562,0.853487571660423,1.),(1.00047110510918,
0.857256476851474,1.),(1.00053193201104,0.838826096655891,1.),(1.00063970687721,
0.806170615310117,1.)))
REPRESENTATION_ITEM('')
SURFACE()
);
#2490=(
BOUNDED_SURFACE()
B_SPLINE_SURFACE(3,2,((#384985,#384986,#384987),(#384988,#384989,#384990),
(#384991,#384992,#384993),(#384994,#384995,#384996)),.UNSPECIFIED.,.F.,
 .F.,.F.)
B_SPLINE_SURFACE_WITH_KNOTS((4,4),(3,3),(2.0299386923051E-5,5.39756952687133E-5),
(-0.000116281070167084,1.),.UNSPECIFIED.)
GEOMETRIC_REPRESENTATION_ITEM()
RATIONAL_B_SPLINE_SURFACE(((1.00001770479734,0.923870681142993,1.),(1.00001014104061,
0.95639427554343,1.),(1.00002037300283,0.912397594905591,1.),(1.00003390859476,
0.854195550869707,1.)))
REPRESENTATION_ITEM('')
SURFACE()
);
#2491=(
BOUNDED_SURFACE()
B_SPLINE_SURFACE(3,2,((#385089,#385090,#385091),(#385092,#385093,#385094),
(#385095,#385096,#385097),(#385098,#385099,#385100)),.UNSPECIFIED.,.F.,
 .F.,.F.)
B_SPLINE_SURFACE_WITH_KNOTS((4,4),(3,3),(0.00135801595889393,0.00148409170619832),
(0.,1.),.UNSPECIFIED.)
GEOMETRIC_REPRESENTATION_ITEM()
RATIONAL_B_SPLINE_SURFACE(((1.,0.818301933966444,1.),(1.,0.817226613172343,
1.),(1.,0.816179643373956,1.),(1.,0.815159387863651,1.)))
REPRESENTATION_ITEM('')
SURFACE()
);
#2492=(
BOUNDED_SURFACE()
B_SPLINE_SURFACE(3,2,((#385139,#385140,#385141),(#385142,#385143,#385144),
(#385145,#385146,#385147),(#385148,#385149,#385150)),.UNSPECIFIED.,.F.,
 .F.,.F.)
B_SPLINE_SURFACE_WITH_KNOTS((4,4),(3,3),(-1.54744435122067E-6,1.5474443512207E-5),
(-0.0151698983643363,1.01516989835806),.UNSPECIFIED.)
GEOMETRIC_REPRESENTATION_ITEM()
RATIONAL_B_SPLINE_SURFACE(((1.02018382473255,0.324498219413463,1.02018382472407),
(1.00401234488884,0.865716921710598,1.00401234488716),(1.00033622856786,
0.988747276629678,1.00033622856771),(1.,1.,1.)))
REPRESENTATION_ITEM('')
SURFACE()
);
#2493=(
BOUNDED_SURFACE()
B_SPLINE_SURFACE(3,2,((#385152,#385153,#385154),(#385155,#385156,#385157),
(#385158,#385159,#385160),(#385161,#385162,#385163)),.UNSPECIFIED.,.F.,
 .F.,.F.)
B_SPLINE_SURFACE_WITH_KNOTS((4,4),(3,3),(0.00137194782501028,0.00149814269699235),
(0.,1.),.UNSPECIFIED.)
GEOMETRIC_REPRESENTATION_ITEM()
RATIONAL_B_SPLINE_SURFACE(((1.,0.815158509402313,1.),(1.,0.816179044148164,
1.),(1.,0.81722630811993,1.),(1.,0.818301939488796,1.)))
REPRESENTATION_ITEM('')
SURFACE()
);
#2494=(
BOUNDED_SURFACE()
B_SPLINE_SURFACE(3,2,((#385207,#385208,#385209),(#385210,#385211,#385212),
(#385213,#385214,#385215),(#385216,#385217,#385218)),.UNSPECIFIED.,.F.,
 .F.,.F.)
B_SPLINE_SURFACE_WITH_KNOTS((4,4),(3,3),(1.55009486301137E-5,4.92065510474435E-5),
(-8.13759514913963E-5,1.),.UNSPECIFIED.)
GEOMETRIC_REPRESENTATION_ITEM()
RATIONAL_B_SPLINE_SURFACE(((1.00002372912336,0.85420063959969,1.),(1.00001423585994,
0.91253030118053,1.),(1.00000710550471,0.95634149537743,1.),(1.00001238975909,
0.923873338137023,1.)))
REPRESENTATION_ITEM('')
SURFACE()
);
#2495=(
BOUNDED_SURFACE()
B_SPLINE_SURFACE(3,2,((#385222,#385223,#385224),(#385225,#385226,#385227),
(#385228,#385229,#385230),(#385231,#385232,#385233)),.UNSPECIFIED.,.F.,
 .F.,.F.)
B_SPLINE_SURFACE_WITH_KNOTS((4,4),(3,3),(-3.39934179457805E-6,3.73927597403566E-5),
(-0.00186004067409043,1.00069373317417),.UNSPECIFIED.)
GEOMETRIC_REPRESENTATION_ITEM()
RATIONAL_B_SPLINE_SURFACE(((1.00072100136051,0.806051963875405,1.00026859642682),
(1.00060048440151,0.838470803558699,1.00022369994488),(1.00053106448792,
0.857144632272416,1.00019783877213),(1.00054515072849,0.85335545953915,
1.0002030863543)))
REPRESENTATION_ITEM('')
SURFACE()
);
#2496=(
BOUNDED_SURFACE()
B_SPLINE_SURFACE(3,2,((#385235,#385236,#385237),(#385238,#385239,#385240),
(#385241,#385242,#385243),(#385244,#385245,#385246)),.UNSPECIFIED.,.F.,
 .F.,.F.)
B_SPLINE_SURFACE_WITH_KNOTS((4,4),(3,3),(0.,9.54361881492173E-5),(0.,1.),
 .UNSPECIFIED.)
GEOMETRIC_REPRESENTATION_ITEM()
RATIONAL_B_SPLINE_SURFACE(((1.,0.816715621142048,1.),(1.,0.81590758740794,
1.),(1.,0.815115959345199,1.),(1.,0.814339887349196,1.)))
REPRESENTATION_ITEM('')
SURFACE()
);
#2497=(
BOUNDED_SURFACE()
B_SPLINE_SURFACE(3,2,((#385248,#385249,#385250),(#385251,#385252,#385253),
(#385254,#385255,#385256),(#385257,#385258,#385259)),.UNSPECIFIED.,.F.,
 .F.,.F.)
B_SPLINE_SURFACE_WITH_KNOTS((4,4),(3,3),(1.47383732822248E-19,4.68197758448205E-5),
(0.,1.),.UNSPECIFIED.)
GEOMETRIC_REPRESENTATION_ITEM()
RATIONAL_B_SPLINE_SURFACE(((1.,0.816715621142046,1.),(1.,0.953638980025211,
1.),(1.,0.954506925408045,1.),(1.,0.81671562114205,1.)))
REPRESENTATION_ITEM('')
SURFACE()
);
#2498=(
BOUNDED_SURFACE()
B_SPLINE_SURFACE(3,2,((#385261,#385262,#385263),(#385264,#385265,#385266),
(#385267,#385268,#385269),(#385270,#385271,#385272)),.UNSPECIFIED.,.F.,
 .F.,.F.)
B_SPLINE_SURFACE_WITH_KNOTS((4,4),(3,3),(-1.0842021724855E-19,9.5436188149218E-5),
(0.,1.),.UNSPECIFIED.)
GEOMETRIC_REPRESENTATION_ITEM()
RATIONAL_B_SPLINE_SURFACE(((1.,0.814339887349195,1.),(1.,0.815115959345212,
1.),(1.,0.815907587407936,1.),(1.,0.816715621142046,1.)))
REPRESENTATION_ITEM('')
SURFACE()
);
#2499=(
BOUNDED_SURFACE()
B_SPLINE_SURFACE(3,2,((#385274,#385275,#385276),(#385277,#385278,#385279),
(#385280,#385281,#385282),(#385283,#385284,#385285)),.UNSPECIFIED.,.F.,
 .F.,.F.)
B_SPLINE_SURFACE_WITH_KNOTS((4,4),(3,3),(-3.39528393502485E-6,3.73481232852731E-5),
(-0.00165018033290614,1.),.UNSPECIFIED.)
GEOMETRIC_REPRESENTATION_ITEM()
RATIONAL_B_SPLINE_SURFACE(((1.00048354385554,0.853487571660454,1.),(1.0004711051091,
0.857256476851504,1.),(1.00053193201095,0.838826096655941,1.),(1.00063970687711,
0.806170615310158,1.)))
REPRESENTATION_ITEM('')
SURFACE()
);
#2500=(
BOUNDED_SURFACE()
B_SPLINE_SURFACE(3,2,((#385289,#385290,#385291),(#385292,#385293,#385294),
(#385295,#385296,#385297),(#385298,#385299,#385300)),.UNSPECIFIED.,.F.,
 .F.,.F.)
B_SPLINE_SURFACE_WITH_KNOTS((4,4),(3,3),(2.02993869230509E-5,5.39756952686903E-5),
(-0.000116281069964736,1.),.UNSPECIFIED.)
GEOMETRIC_REPRESENTATION_ITEM()
RATIONAL_B_SPLINE_SURFACE(((1.0000177047973,0.923870681143004,1.),(1.00001014104059,
0.956394275543417,1.),(1.00002037300279,0.912397594905668,1.),(1.0000339085947,
0.854195550869854,1.)))
REPRESENTATION_ITEM('')
SURFACE()
);
#2501=(
BOUNDED_SURFACE()
B_SPLINE_SURFACE(3,2,((#385393,#385394,#385395),(#385396,#385397,#385398),
(#385399,#385400,#385401),(#385402,#385403,#385404)),.UNSPECIFIED.,.F.,
 .F.,.F.)
B_SPLINE_SURFACE_WITH_KNOTS((4,4),(3,3),(0.00135801595889393,0.00148409170619832),
(0.,1.),.UNSPECIFIED.)
GEOMETRIC_REPRESENTATION_ITEM()
RATIONAL_B_SPLINE_SURFACE(((1.,0.818301933966441,1.),(1.,0.817226613172338,
1.),(1.,0.816179643373964,1.),(1.,0.815159387863657,1.)))
REPRESENTATION_ITEM('')
SURFACE()
);
#2502=(
BOUNDED_SURFACE()
B_SPLINE_SURFACE(3,2,((#385443,#385444,#385445),(#385446,#385447,#385448),
(#385449,#385450,#385451),(#385452,#385453,#385454)),.UNSPECIFIED.,.F.,
 .F.,.F.)
B_SPLINE_SURFACE_WITH_KNOTS((4,4),(3,3),(-1.54744435122076E-6,1.54744435122078E-5),
(-0.0151698983634891,1.),.UNSPECIFIED.)
GEOMETRIC_REPRESENTATION_ITEM()
RATIONAL_B_SPLINE_SURFACE(((1.02018382473141,0.334740937355592,1.),(1.00401234488861,
0.86775307281324,1.),(1.00033622856784,0.988917903080779,1.),(1.,1.,1.)))
REPRESENTATION_ITEM('')
SURFACE()
);
#2503=(
BOUNDED_SURFACE()
B_SPLINE_SURFACE(3,2,((#385456,#385457,#385458),(#385459,#385460,#385461),
(#385462,#385463,#385464),(#385465,#385466,#385467)),.UNSPECIFIED.,.F.,
 .F.,.F.)
B_SPLINE_SURFACE_WITH_KNOTS((4,4),(3,3),(0.00137194782501028,0.00149814269699235),
(0.,1.),.UNSPECIFIED.)
GEOMETRIC_REPRESENTATION_ITEM()
RATIONAL_B_SPLINE_SURFACE(((1.,0.815158509402317,1.),(1.,0.816179044148157,
1.),(1.,0.817226308119947,1.),(1.,0.818301939488798,1.)))
REPRESENTATION_ITEM('')
SURFACE()
);
#2504=(
BOUNDED_SURFACE()
B_SPLINE_SURFACE(3,2,((#385511,#385512,#385513),(#385514,#385515,#385516),
(#385517,#385518,#385519),(#385520,#385521,#385522)),.UNSPECIFIED.,.F.,
 .F.,.F.)
B_SPLINE_SURFACE_WITH_KNOTS((4,4),(3,3),(1.55009486301138E-5,4.92065510474432E-5),
(-8.13759517454961E-5,1.),.UNSPECIFIED.)
GEOMETRIC_REPRESENTATION_ITEM()
RATIONAL_B_SPLINE_SURFACE(((1.00002372912343,0.854200639599646,1.),(1.00001423585998,
0.912530301180508,1.),(1.00000710550473,0.956341495377424,1.),(1.00001238975912,
0.923873338137003,1.)))
REPRESENTATION_ITEM('')
SURFACE()
);
#2505=(
BOUNDED_SURFACE()
B_SPLINE_SURFACE(3,2,((#385526,#385527,#385528),(#385529,#385530,#385531),
(#385532,#385533,#385534),(#385535,#385536,#385537)),.UNSPECIFIED.,.F.,
 .F.,.F.)
B_SPLINE_SURFACE_WITH_KNOTS((4,4),(3,3),(-3.39934179457826E-6,3.73927597403565E-5),
(-0.00186004067384692,1.00069373317454),.UNSPECIFIED.)
GEOMETRIC_REPRESENTATION_ITEM()
RATIONAL_B_SPLINE_SURFACE(((1.00072100136041,0.806051963875379,1.00026859642697),
(1.00060048440143,0.838470803558679,1.00022369994501),(1.00053106448785,
0.857144632272401,1.00019783877224),(1.00054515072842,0.853355459539132,
1.00020308635441)))
REPRESENTATION_ITEM('')
SURFACE()
);
#2506=(
BOUNDED_SURFACE()
B_SPLINE_SURFACE(3,2,((#385539,#385540,#385541),(#385542,#385543,#385544),
(#385545,#385546,#385547),(#385548,#385549,#385550)),.UNSPECIFIED.,.F.,
 .F.,.F.)
B_SPLINE_SURFACE_WITH_KNOTS((4,4),(3,3),(0.,9.54361881492173E-5),(0.,1.),
 .UNSPECIFIED.)
GEOMETRIC_REPRESENTATION_ITEM()
RATIONAL_B_SPLINE_SURFACE(((1.,0.816715621142047,1.),(1.,0.815907587407945,
1.),(1.,0.815115959345206,1.),(1.,0.814339887349193,1.)))
REPRESENTATION_ITEM('')
SURFACE()
);
#2507=(
BOUNDED_SURFACE()
B_SPLINE_SURFACE(3,2,((#385552,#385553,#385554),(#385555,#385556,#385557),
(#385558,#385559,#385560),(#385561,#385562,#385563)),.UNSPECIFIED.,.F.,
 .F.,.F.)
B_SPLINE_SURFACE_WITH_KNOTS((4,4),(3,3),(1.16890546721093E-19,4.68197758448207E-5),
(0.,1.),.UNSPECIFIED.)
GEOMETRIC_REPRESENTATION_ITEM()
RATIONAL_B_SPLINE_SURFACE(((1.,0.816715621142051,1.),(1.,0.953638980025205,
1.),(1.,0.954506925408056,1.),(1.,0.81671562114205,1.)))
REPRESENTATION_ITEM('')
SURFACE()
);
#2508=(
BOUNDED_SURFACE()
B_SPLINE_SURFACE(3,2,((#385565,#385566,#385567),(#385568,#385569,#385570),
(#385571,#385572,#385573),(#385574,#385575,#385576)),.UNSPECIFIED.,.F.,
 .F.,.F.)
B_SPLINE_SURFACE_WITH_KNOTS((4,4),(3,3),(-1.62630325872826E-19,9.54361881492177E-5),
(0.,1.),.UNSPECIFIED.)
GEOMETRIC_REPRESENTATION_ITEM()
RATIONAL_B_SPLINE_SURFACE(((1.,0.814339887349195,1.),(1.,0.815115959345206,
1.),(1.,0.81590758740794,1.),(1.,0.816715621142051,1.)))
REPRESENTATION_ITEM('')
SURFACE()
);
#2509=(
BOUNDED_SURFACE()
B_SPLINE_SURFACE(3,2,((#385578,#385579,#385580),(#385581,#385582,#385583),
(#385584,#385585,#385586),(#385587,#385588,#385589)),.UNSPECIFIED.,.F.,
 .F.,.F.)
B_SPLINE_SURFACE_WITH_KNOTS((4,4),(3,3),(-3.39528393502489E-6,3.7348123285274E-5),
(-0.00165018033282777,1.),.UNSPECIFIED.)
GEOMETRIC_REPRESENTATION_ITEM()
RATIONAL_B_SPLINE_SURFACE(((1.00048354385552,0.853487571660468,1.),(1.00047110510908,
0.857256476851526,1.),(1.00053193201093,0.838826096655947,1.),(1.00063970687708,
0.806170615310178,0.999999999999999)))
REPRESENTATION_ITEM('')
SURFACE()
);
#2510=(
BOUNDED_SURFACE()
B_SPLINE_SURFACE(3,2,((#385593,#385594,#385595),(#385596,#385597,#385598),
(#385599,#385600,#385601),(#385602,#385603,#385604)),.UNSPECIFIED.,.F.,
 .F.,.F.)
B_SPLINE_SURFACE_WITH_KNOTS((4,4),(3,3),(2.0299386923051E-5,5.3975695268712E-5),
(-0.000116281069906644,1.),.UNSPECIFIED.)
GEOMETRIC_REPRESENTATION_ITEM()
RATIONAL_B_SPLINE_SURFACE(((1.0000177047973,0.923870681143011,1.),(1.00001014104059,
0.956394275543454,1.),(1.00002037300278,0.912397594905597,1.),(1.00003390859468,
0.854195550869745,1.)))
REPRESENTATION_ITEM('')
SURFACE()
);
#2511=(
BOUNDED_SURFACE()
B_SPLINE_SURFACE(3,2,((#385697,#385698,#385699),(#385700,#385701,#385702),
(#385703,#385704,#385705),(#385706,#385707,#385708)),.UNSPECIFIED.,.F.,
 .F.,.F.)
B_SPLINE_SURFACE_WITH_KNOTS((4,4),(3,3),(0.00135801595889393,0.00148409170619832),
(0.,1.),.UNSPECIFIED.)
GEOMETRIC_REPRESENTATION_ITEM()
RATIONAL_B_SPLINE_SURFACE(((1.,0.818301933966441,1.),(1.,0.817226613172349,
1.),(1.,0.816179643373946,1.),(1.,0.815159387863657,1.)))
REPRESENTATION_ITEM('')
SURFACE()
);
#2512=(
BOUNDED_SURFACE()
B_SPLINE_SURFACE(3,2,((#385747,#385748,#385749),(#385750,#385751,#385752),
(#385753,#385754,#385755),(#385756,#385757,#385758)),.UNSPECIFIED.,.F.,
 .F.,.F.)
B_SPLINE_SURFACE_WITH_KNOTS((4,4),(3,3),(-1.54744435122074E-6,1.54744435122074E-5),
(-0.0151698983623385,1.01516989836002),.UNSPECIFIED.)
GEOMETRIC_REPRESENTATION_ITEM()
RATIONAL_B_SPLINE_SURFACE(((1.02018382472986,0.324498219413466,1.02018382472673),
(1.00401234488831,0.865716921710605,1.00401234488769),(1.00033622856781,
0.98874727662968,1.00033622856776),(1.,1.,1.)))
REPRESENTATION_ITEM('')
SURFACE()
);
#2513=(
BOUNDED_SURFACE()
B_SPLINE_SURFACE(3,2,((#385760,#385761,#385762),(#385763,#385764,#385765),
(#385766,#385767,#385768),(#385769,#385770,#385771)),.UNSPECIFIED.,.F.,
 .F.,.F.)
B_SPLINE_SURFACE_WITH_KNOTS((4,4),(3,3),(0.00137194782501028,0.00149814269699235),
(0.,1.),.UNSPECIFIED.)
GEOMETRIC_REPRESENTATION_ITEM()
RATIONAL_B_SPLINE_SURFACE(((1.,0.815158509402318,1.),(1.,0.816179044148164,
1.),(1.,0.817226308119924,1.),(1.,0.818301939488807,1.)))
REPRESENTATION_ITEM('')
SURFACE()
);
#2514=(
BOUNDED_SURFACE()
B_SPLINE_SURFACE(3,2,((#385815,#385816,#385817),(#385818,#385819,#385820),
(#385821,#385822,#385823),(#385824,#385825,#385826)),.UNSPECIFIED.,.F.,
 .F.,.F.)
B_SPLINE_SURFACE_WITH_KNOTS((4,4),(3,3),(1.55009486301137E-5,4.92065510474427E-5),
(-8.13759513362642E-5,1.),.UNSPECIFIED.)
GEOMETRIC_REPRESENTATION_ITEM()
RATIONAL_B_SPLINE_SURFACE(((1.00002372912331,0.854200639599707,1.),(1.00001423585991,
0.912530301180549,1.),(1.0000071055047,0.956341495377444,1.),(1.00001238975906,
0.923873338137031,1.)))
REPRESENTATION_ITEM('')
SURFACE()
);
#2515=(
BOUNDED_SURFACE()
B_SPLINE_SURFACE(3,2,((#385830,#385831,#385832),(#385833,#385834,#385835),
(#385836,#385837,#385838),(#385839,#385840,#385841)),.UNSPECIFIED.,.F.,
 .F.,.F.)
B_SPLINE_SURFACE_WITH_KNOTS((4,4),(3,3),(-3.39934179457806E-6,3.73927597403565E-5),
(-0.00186004067400375,1.00069373317447),.UNSPECIFIED.)
GEOMETRIC_REPRESENTATION_ITEM()
RATIONAL_B_SPLINE_SURFACE(((1.00072100136047,0.806051963875356,1.00026859642694),
(1.00060048440148,0.838470803558668,1.00022369994498),(1.00053106448789,
0.857144632272387,1.00019783877222),(1.00054515072847,0.85335545953912,
1.00020308635439)))
REPRESENTATION_ITEM('')
SURFACE()
);
#2516=(
BOUNDED_SURFACE()
B_SPLINE_SURFACE(3,2,((#385843,#385844,#385845),(#385846,#385847,#385848),
(#385849,#385850,#385851),(#385852,#385853,#385854)),.UNSPECIFIED.,.F.,
 .F.,.F.)
B_SPLINE_SURFACE_WITH_KNOTS((4,4),(3,3),(5.42101086242752E-20,9.54361881492175E-5),
(0.,1.),.UNSPECIFIED.)
GEOMETRIC_REPRESENTATION_ITEM()
RATIONAL_B_SPLINE_SURFACE(((1.,0.81671562114205,1.),(1.,0.815907587407938,
1.),(1.,0.815115959345202,1.),(1.,0.814339887349195,1.)))
REPRESENTATION_ITEM('')
SURFACE()
);
#2517=(
BOUNDED_SURFACE()
B_SPLINE_SURFACE(3,2,((#385856,#385857,#385858),(#385859,#385860,#385861),
(#385862,#385863,#385864),(#385865,#385866,#385867)),.UNSPECIFIED.,.F.,
 .F.,.F.)
B_SPLINE_SURFACE_WITH_KNOTS((4,4),(3,3),(1.18584612615602E-19,4.68197758448209E-5),
(0.,1.),.UNSPECIFIED.)
GEOMETRIC_REPRESENTATION_ITEM()
RATIONAL_B_SPLINE_SURFACE(((1.,0.816715621142049,1.),(1.,0.953638980025195,
1.),(1.,0.954506925408062,1.),(1.,0.816715621142057,1.)))
REPRESENTATION_ITEM('')
SURFACE()
);
#2518=(
BOUNDED_SURFACE()
B_SPLINE_SURFACE(3,2,((#385869,#385870,#385871),(#385872,#385873,#385874),
(#385875,#385876,#385877),(#385878,#385879,#385880)),.UNSPECIFIED.,.F.,
 .F.,.F.)
B_SPLINE_SURFACE_WITH_KNOTS((4,4),(3,3),(-1.62630325872826E-19,9.54361881492177E-5),
(0.,1.),.UNSPECIFIED.)
GEOMETRIC_REPRESENTATION_ITEM()
RATIONAL_B_SPLINE_SURFACE(((1.,0.81433988734919,1.),(1.,0.815115959345207,
1.),(1.,0.815907587407944,1.),(1.,0.816715621142049,1.)))
REPRESENTATION_ITEM('')
SURFACE()
);
#2519=(
BOUNDED_SURFACE()
B_SPLINE_SURFACE(3,2,((#385882,#385883,#385884),(#385885,#385886,#385887),
(#385888,#385889,#385890),(#385891,#385892,#385893)),.UNSPECIFIED.,.F.,
 .F.,.F.)
B_SPLINE_SURFACE_WITH_KNOTS((4,4),(3,3),(-3.39528393502492E-6,3.73481232852737E-5),
(-0.00165018033286106,1.),.UNSPECIFIED.)
GEOMETRIC_REPRESENTATION_ITEM()
RATIONAL_B_SPLINE_SURFACE(((1.00048354385553,0.853487571660456,1.),(1.00047110510909,
0.857256476851521,1.),(1.00053193201094,0.838826096655938,1.),(1.00063970687709,
0.806170615310175,1.)))
REPRESENTATION_ITEM('')
SURFACE()
);
#2520=(
BOUNDED_SURFACE()
B_SPLINE_SURFACE(3,2,((#385897,#385898,#385899),(#385900,#385901,#385902),
(#385903,#385904,#385905),(#385906,#385907,#385908)),.UNSPECIFIED.,.F.,
 .F.,.F.)
B_SPLINE_SURFACE_WITH_KNOTS((4,4),(3,3),(2.02993869230507E-5,5.39756952687127E-5),
(-0.000116281069855912,1.),.UNSPECIFIED.)
GEOMETRIC_REPRESENTATION_ITEM()
RATIONAL_B_SPLINE_SURFACE(((1.00001770479729,0.923870681143013,1.),(1.00001014104058,
0.956394275543447,1.),(1.00002037300277,0.912397594905622,1.),(1.00003390859467,
0.854195550869747,1.)))
REPRESENTATION_ITEM('')
SURFACE()
);
#2521=(
BOUNDED_SURFACE()
B_SPLINE_SURFACE(3,2,((#386001,#386002,#386003),(#386004,#386005,#386006),
(#386007,#386008,#386009),(#386010,#386011,#386012)),.UNSPECIFIED.,.F.,
 .F.,.F.)
B_SPLINE_SURFACE_WITH_KNOTS((4,4),(3,3),(0.00135801595889393,0.00148409170619832),
(0.,1.),.UNSPECIFIED.)
GEOMETRIC_REPRESENTATION_ITEM()
RATIONAL_B_SPLINE_SURFACE(((1.,0.818301933966445,1.),(1.,0.817226613172353,
1.),(1.,0.816179643373944,1.),(1.,0.815159387863655,1.)))
REPRESENTATION_ITEM('')
SURFACE()
);
#2522=(
BOUNDED_SURFACE()
B_SPLINE_SURFACE(3,2,((#386051,#386052,#386053),(#386054,#386055,#386056),
(#386057,#386058,#386059),(#386060,#386061,#386062)),.UNSPECIFIED.,.F.,
 .F.,.F.)
B_SPLINE_SURFACE_WITH_KNOTS((4,4),(3,3),(-1.54744435122071E-6,1.54744435122078E-5),
(-0.0151698983634562,1.),.UNSPECIFIED.)
GEOMETRIC_REPRESENTATION_ITEM()
RATIONAL_B_SPLINE_SURFACE(((1.02018382473136,0.334740937355685,1.),(1.00401234488861,
0.867753072813108,1.),(1.00033622856783,0.988917903080856,1.),(1.,1.,1.)))
REPRESENTATION_ITEM('')
SURFACE()
);
#2523=(
BOUNDED_SURFACE()
B_SPLINE_SURFACE(3,2,((#386064,#386065,#386066),(#386067,#386068,#386069),
(#386070,#386071,#386072),(#386073,#386074,#386075)),.UNSPECIFIED.,.F.,
 .F.,.F.)
B_SPLINE_SURFACE_WITH_KNOTS((4,4),(3,3),(0.00137194782501028,0.00149814269699235),
(0.,1.),.UNSPECIFIED.)
GEOMETRIC_REPRESENTATION_ITEM()
RATIONAL_B_SPLINE_SURFACE(((1.,0.815158509402317,1.),(1.,0.816179044148167,
1.),(1.,0.817226308119926,1.),(1.,0.818301939488808,1.)))
REPRESENTATION_ITEM('')
SURFACE()
);
#2524=(
BOUNDED_SURFACE()
B_SPLINE_SURFACE(3,2,((#386119,#386120,#386121),(#386122,#386123,#386124),
(#386125,#386126,#386127),(#386128,#386129,#386130)),.UNSPECIFIED.,.F.,
 .F.,.F.)
B_SPLINE_SURFACE_WITH_KNOTS((4,4),(3,3),(1.55009486301137E-5,4.92065510474429E-5),
(-8.13759514961233E-5,1.),.UNSPECIFIED.)
GEOMETRIC_REPRESENTATION_ITEM()
RATIONAL_B_SPLINE_SURFACE(((1.00002372912336,0.854200639599683,1.),(1.00001423585994,
0.912530301180529,1.),(1.00000710550471,0.956341495377432,1.),(1.00001238975909,
0.923873338137021,1.)))
REPRESENTATION_ITEM('')
SURFACE()
);
#2525=(
BOUNDED_SURFACE()
B_SPLINE_SURFACE(3,2,((#386134,#386135,#386136),(#386137,#386138,#386139),
(#386140,#386141,#386142),(#386143,#386144,#386145)),.UNSPECIFIED.,.F.,
 .F.,.F.)
B_SPLINE_SURFACE_WITH_KNOTS((4,4),(3,3),(-3.39934179457838E-6,3.73927597403565E-5),
(-0.00186004067399421,1.00069373317385),.UNSPECIFIED.)
GEOMETRIC_REPRESENTATION_ITEM()
RATIONAL_B_SPLINE_SURFACE(((1.00072100136047,0.806051963875509,1.0002685964267),
(1.00060048440148,0.838470803558736,1.00022369994478),(1.00053106448789,
0.857144632272504,1.00019783877204),(1.00054515072847,0.853355459539207,
1.00020308635421)))
REPRESENTATION_ITEM('')
SURFACE()
);
#2526=(
BOUNDED_SURFACE()
B_SPLINE_SURFACE(3,2,((#386147,#386148,#386149),(#386150,#386151,#386152),
(#386153,#386154,#386155),(#386156,#386157,#386158)),.UNSPECIFIED.,.F.,
 .F.,.F.)
B_SPLINE_SURFACE_WITH_KNOTS((4,4),(3,3),(0.,9.54361881492174E-5),(0.,1.),
 .UNSPECIFIED.)
GEOMETRIC_REPRESENTATION_ITEM()
RATIONAL_B_SPLINE_SURFACE(((1.,0.816715621142053,1.),(1.,0.81590758740794,
1.),(1.,0.815115959345204,1.),(1.,0.814339887349195,1.)))
REPRESENTATION_ITEM('')
SURFACE()
);
#2527=(
BOUNDED_SURFACE()
B_SPLINE_SURFACE(3,2,((#386160,#386161,#386162),(#386163,#386164,#386165),
(#386166,#386167,#386168),(#386169,#386170,#386171)),.UNSPECIFIED.,.F.,
 .F.,.F.)
B_SPLINE_SURFACE_WITH_KNOTS((4,4),(3,3),(-1.76182853028894E-19,4.68197758448203E-5),
(0.,1.),.UNSPECIFIED.)
GEOMETRIC_REPRESENTATION_ITEM()
RATIONAL_B_SPLINE_SURFACE(((1.,0.816715621142051,1.),(1.,0.953638980025202,
1.),(1.,0.954506925408056,1.),(1.,0.816715621142056,1.)))
REPRESENTATION_ITEM('')
SURFACE()
);
#2528=(
BOUNDED_SURFACE()
B_SPLINE_SURFACE(3,2,((#386173,#386174,#386175),(#386176,#386177,#386178),
(#386179,#386180,#386181),(#386182,#386183,#386184)),.UNSPECIFIED.,.F.,
 .F.,.F.)
B_SPLINE_SURFACE_WITH_KNOTS((4,4),(3,3),(-2.71050543121376E-19,9.54361881492173E-5),
(0.,1.),.UNSPECIFIED.)
GEOMETRIC_REPRESENTATION_ITEM()
RATIONAL_B_SPLINE_SURFACE(((1.,0.814339887349194,1.),(1.,0.815115959345203,
1.),(1.,0.815907587407945,1.),(1.,0.816715621142049,1.)))
REPRESENTATION_ITEM('')
SURFACE()
);
#2529=(
BOUNDED_SURFACE()
B_SPLINE_SURFACE(3,2,((#386186,#386187,#386188),(#386189,#386190,#386191),
(#386192,#386193,#386194),(#386195,#386196,#386197)),.UNSPECIFIED.,.F.,
 .F.,.F.)
B_SPLINE_SURFACE_WITH_KNOTS((4,4),(3,3),(-3.39528393502482E-6,3.73481232852729E-5),
(-0.00165018033288066,1.),.UNSPECIFIED.)
GEOMETRIC_REPRESENTATION_ITEM()
RATIONAL_B_SPLINE_SURFACE(((1.00048354385554,0.853487571660457,1.),(1.00047110510909,
0.85725647685152,1.),(1.00053193201094,0.838826096655938,1.),(1.0006397068771,
0.80617061531017,1.)))
REPRESENTATION_ITEM('')
SURFACE()
);
#2530=(
BOUNDED_SURFACE()
B_SPLINE_SURFACE(3,2,((#386201,#386202,#386203),(#386204,#386205,#386206),
(#386207,#386208,#386209),(#386210,#386211,#386212)),.UNSPECIFIED.,.F.,
 .F.,.F.)
B_SPLINE_SURFACE_WITH_KNOTS((4,4),(3,3),(2.02993869230509E-5,5.39756952687121E-5),
(-0.000116281069688478,1.),.UNSPECIFIED.)
GEOMETRIC_REPRESENTATION_ITEM()
RATIONAL_B_SPLINE_SURFACE(((1.00001770479726,0.923870681143028,1.),(1.00001014104057,
0.956394275543453,1.),(1.00002037300274,0.912397594905643,1.),(1.00003390859462,
0.854195550869773,1.)))
REPRESENTATION_ITEM('')
SURFACE()
);
#2531=(
BOUNDED_SURFACE()
B_SPLINE_SURFACE(3,2,((#386305,#386306,#386307),(#386308,#386309,#386310),
(#386311,#386312,#386313),(#386314,#386315,#386316)),.UNSPECIFIED.,.F.,
 .F.,.F.)
B_SPLINE_SURFACE_WITH_KNOTS((4,4),(3,3),(0.00135801595889393,0.00148409170619832),
(0.,1.),.UNSPECIFIED.)
GEOMETRIC_REPRESENTATION_ITEM()
RATIONAL_B_SPLINE_SURFACE(((1.,0.818301933966445,1.),(1.,0.817226613172355,
1.),(1.,0.816179643373943,1.),(1.,0.815159387863657,1.)))
REPRESENTATION_ITEM('')
SURFACE()
);
#2532=(
BOUNDED_SURFACE()
B_SPLINE_SURFACE(3,2,((#386355,#386356,#386357),(#386358,#386359,#386360),
(#386361,#386362,#386363),(#386364,#386365,#386366)),.UNSPECIFIED.,.F.,
 .F.,.F.)
B_SPLINE_SURFACE_WITH_KNOTS((4,4),(3,3),(-1.54744435122083E-6,1.54744435122081E-5),
(-0.0151698983585689,1.01516989836374),.UNSPECIFIED.)
GEOMETRIC_REPRESENTATION_ITEM()
RATIONAL_B_SPLINE_SURFACE(((1.02018382472476,0.324498219413556,1.02018382473175),
(1.0040123448873,0.865716921710493,1.00401234488869),(1.00033622856772,
0.988747276629742,1.00033622856784),(1.,1.,1.)))
REPRESENTATION_ITEM('')
SURFACE()
);
#2533=(
BOUNDED_SURFACE()
B_SPLINE_SURFACE(3,2,((#386368,#386369,#386370),(#386371,#386372,#386373),
(#386374,#386375,#386376),(#386377,#386378,#386379)),.UNSPECIFIED.,.F.,
 .F.,.F.)
B_SPLINE_SURFACE_WITH_KNOTS((4,4),(3,3),(0.00137194782501028,0.00149814269699235),
(0.,1.),.UNSPECIFIED.)
GEOMETRIC_REPRESENTATION_ITEM()
RATIONAL_B_SPLINE_SURFACE(((1.,0.815158509402318,1.),(1.,0.816179044148175,
1.),(1.,0.817226308119926,1.),(1.,0.818301939488811,1.)))
REPRESENTATION_ITEM('')
SURFACE()
);
#2534=(
BOUNDED_SURFACE()
B_SPLINE_SURFACE(3,2,((#386423,#386424,#386425),(#386426,#386427,#386428),
(#386429,#386430,#386431),(#386432,#386433,#386434)),.UNSPECIFIED.,.F.,
 .F.,.F.)
B_SPLINE_SURFACE_WITH_KNOTS((4,4),(3,3),(1.55009486301138E-5,4.92065510474436E-5),
(-8.13759515694668E-5,1.),.UNSPECIFIED.)
GEOMETRIC_REPRESENTATION_ITEM()
RATIONAL_B_SPLINE_SURFACE(((1.00002372912338,0.854200639599671,1.),(1.00001423585995,
0.912530301180525,1.),(1.00000710550472,0.956341495377431,1.),(1.0000123897591,
0.923873338137017,1.)))
REPRESENTATION_ITEM('')
SURFACE()
);
#2535=(
BOUNDED_SURFACE()
B_SPLINE_SURFACE(3,2,((#386438,#386439,#386440),(#386441,#386442,#386443),
(#386444,#386445,#386446),(#386447,#386448,#386449)),.UNSPECIFIED.,.F.,
 .F.,.F.)
B_SPLINE_SURFACE_WITH_KNOTS((4,4),(3,3),(-3.39934179457811E-6,3.73927597403567E-5),
(-0.0018600406746428,1.00069373317446),.UNSPECIFIED.)
GEOMETRIC_REPRESENTATION_ITEM()
RATIONAL_B_SPLINE_SURFACE(((1.00072100136072,0.806051963875256,1.00026859642693),
(1.00060048440169,0.838470803558557,1.00022369994498),(1.00053106448808,
0.857144632272301,1.00019783877221),(1.00054515072866,0.853355459539024,
1.00020308635439)))
REPRESENTATION_ITEM('')
SURFACE()
);
#2536=(
BOUNDED_SURFACE()
B_SPLINE_SURFACE(3,2,((#386451,#386452,#386453),(#386454,#386455,#386456),
(#386457,#386458,#386459),(#386460,#386461,#386462)),.UNSPECIFIED.,.F.,
 .F.,.F.)
B_SPLINE_SURFACE_WITH_KNOTS((4,4),(3,3),(2.71050543121376E-19,9.54361881492177E-5),
(0.,1.),.UNSPECIFIED.)
GEOMETRIC_REPRESENTATION_ITEM()
RATIONAL_B_SPLINE_SURFACE(((1.,0.816715621142051,1.),(1.,0.815907587407941,
1.),(1.,0.815115959345211,1.),(1.,0.814339887349194,1.)))
REPRESENTATION_ITEM('')
SURFACE()
);
#2537=(
BOUNDED_SURFACE()
B_SPLINE_SURFACE(3,2,((#386464,#386465,#386466),(#386467,#386468,#386469),
(#386470,#386471,#386472),(#386473,#386474,#386475)),.UNSPECIFIED.,.F.,
 .F.,.F.)
B_SPLINE_SURFACE_WITH_KNOTS((4,4),(3,3),(-4.91279109407494E-20,4.68197758448206E-5),
(0.,1.),.UNSPECIFIED.)
GEOMETRIC_REPRESENTATION_ITEM()
RATIONAL_B_SPLINE_SURFACE(((1.,0.81671562114205,1.),(1.,0.953638980025202,
1.),(1.,0.954506925408066,1.),(1.,0.816715621142053,1.)))
REPRESENTATION_ITEM('')
SURFACE()
);
#2538=(
BOUNDED_SURFACE()
B_SPLINE_SURFACE(3,2,((#386477,#386478,#386479),(#386480,#386481,#386482),
(#386483,#386484,#386485),(#386486,#386487,#386488)),.UNSPECIFIED.,.F.,
 .F.,.F.)
B_SPLINE_SURFACE_WITH_KNOTS((4,4),(3,3),(0.,9.54361881492175E-5),(0.,1.),
 .UNSPECIFIED.)
GEOMETRIC_REPRESENTATION_ITEM()
RATIONAL_B_SPLINE_SURFACE(((1.,0.814339887349197,1.),(1.,0.815115959345201,
1.),(1.,0.815907587407948,1.),(1.,0.81671562114205,1.)))
REPRESENTATION_ITEM('')
SURFACE()
);
#2539=(
BOUNDED_SURFACE()
B_SPLINE_SURFACE(3,2,((#386490,#386491,#386492),(#386493,#386494,#386495),
(#386496,#386497,#386498),(#386499,#386500,#386501)),.UNSPECIFIED.,.F.,
 .F.,.F.)
B_SPLINE_SURFACE_WITH_KNOTS((4,4),(3,3),(-3.39528393502379E-6,3.73481232852733E-5),
(-0.00165018033281,1.),.UNSPECIFIED.)
GEOMETRIC_REPRESENTATION_ITEM()
RATIONAL_B_SPLINE_SURFACE(((1.00048354385552,0.853487571660465,1.),(1.00047110510907,
0.857256476851538,1.),(1.00053193201092,0.838826096655939,1.),(1.00063970687707,
0.806170615310189,0.999999999999999)))
REPRESENTATION_ITEM('')
SURFACE()
);
#2540=(
BOUNDED_SURFACE()
B_SPLINE_SURFACE(3,2,((#386505,#386506,#386507),(#386508,#386509,#386510),
(#386511,#386512,#386513),(#386514,#386515,#386516)),.UNSPECIFIED.,.F.,
 .F.,.F.)
B_SPLINE_SURFACE_WITH_KNOTS((4,4),(3,3),(2.02993869230507E-5,5.3975695268713E-5),
(-0.000116281070062206,1.),.UNSPECIFIED.)
GEOMETRIC_REPRESENTATION_ITEM()
RATIONAL_B_SPLINE_SURFACE(((1.00001770479732,0.923870681143,1.),(1.0000101410406,
0.956394275543443,1.),(1.00002037300281,0.912397594905605,1.),(1.00003390859473,
0.854195550869708,1.)))
REPRESENTATION_ITEM('')
SURFACE()
);
#2541=(
BOUNDED_SURFACE()
B_SPLINE_SURFACE(3,2,((#386609,#386610,#386611),(#386612,#386613,#386614),
(#386615,#386616,#386617),(#386618,#386619,#386620)),.UNSPECIFIED.,.F.,
 .F.,.F.)
B_SPLINE_SURFACE_WITH_KNOTS((4,4),(3,3),(0.00135801595889393,0.00148409170619832),
(0.,1.),.UNSPECIFIED.)
GEOMETRIC_REPRESENTATION_ITEM()
RATIONAL_B_SPLINE_SURFACE(((1.,0.818301933966441,1.),(1.,0.817226613172342,
1.),(1.,0.816179643373956,1.),(1.,0.815159387863641,1.)))
REPRESENTATION_ITEM('')
SURFACE()
);
#2542=(
BOUNDED_SURFACE()
B_SPLINE_SURFACE(3,2,((#386659,#386660,#386661),(#386662,#386663,#386664),
(#386665,#386666,#386667),(#386668,#386669,#386670)),.UNSPECIFIED.,.F.,
 .F.,.F.)
B_SPLINE_SURFACE_WITH_KNOTS((4,4),(3,3),(-1.54744435122073E-6,1.54744435122074E-5),
(-0.0151698983629041,1.01516989835958),.UNSPECIFIED.)
GEOMETRIC_REPRESENTATION_ITEM()
RATIONAL_B_SPLINE_SURFACE(((1.02018382473062,0.324498219413462,1.02018382472613),
(1.00401234488846,0.865716921710508,1.00401234488757),(1.00033622856782,
0.988747276629692,1.00033622856775),(1.,1.,1.)))
REPRESENTATION_ITEM('')
SURFACE()
);
#2543=(
BOUNDED_SURFACE()
B_SPLINE_SURFACE(3,2,((#386672,#386673,#386674),(#386675,#386676,#386677),
(#386678,#386679,#386680),(#386681,#386682,#386683)),.UNSPECIFIED.,.F.,
 .F.,.F.)
B_SPLINE_SURFACE_WITH_KNOTS((4,4),(3,3),(0.00137194782501028,0.00149814269699235),
(0.,1.),.UNSPECIFIED.)
GEOMETRIC_REPRESENTATION_ITEM()
RATIONAL_B_SPLINE_SURFACE(((1.,0.815158509402317,1.),(1.,0.816179044148162,
1.),(1.,0.817226308119928,1.),(1.,0.818301939488809,1.)))
REPRESENTATION_ITEM('')
SURFACE()
);
#2544=(
BOUNDED_SURFACE()
B_SPLINE_SURFACE(3,2,((#386727,#386728,#386729),(#386730,#386731,#386732),
(#386733,#386734,#386735),(#386736,#386737,#386738)),.UNSPECIFIED.,.F.,
 .F.,.F.)
B_SPLINE_SURFACE_WITH_KNOTS((4,4),(3,3),(1.55009486301137E-5,4.92065510474433E-5),
(-8.13759518888895E-5,1.),.UNSPECIFIED.)
GEOMETRIC_REPRESENTATION_ITEM()
RATIONAL_B_SPLINE_SURFACE(((1.00002372912348,0.854200639599625,1.),(1.00001423586001,
0.912530301180506,1.),(1.00000710550474,0.956341495377407,1.),(1.00001238975915,
0.923873338136996,1.)))
REPRESENTATION_ITEM('')
SURFACE()
);
#2545=(
BOUNDED_SURFACE()
B_SPLINE_SURFACE(3,2,((#386742,#386743,#386744),(#386745,#386746,#386747),
(#386748,#386749,#386750),(#386751,#386752,#386753)),.UNSPECIFIED.,.F.,
 .F.,.F.)
B_SPLINE_SURFACE_WITH_KNOTS((4,4),(3,3),(-3.39934179457743E-6,3.73927597403565E-5),
(-0.0018600406739329,1.00069373317448),.UNSPECIFIED.)
GEOMETRIC_REPRESENTATION_ITEM()
RATIONAL_B_SPLINE_SURFACE(((1.00072100136045,0.806051963875354,1.00026859642694),
(1.00060048440146,0.838470803558705,1.00022369994498),(1.00053106448787,
0.857144632272372,1.00019783877222),(1.00054515072845,0.853355459539128,
1.00020308635439)))
REPRESENTATION_ITEM('')
SURFACE()
);
#2546=(
BOUNDED_SURFACE()
B_SPLINE_SURFACE(3,2,((#386755,#386756,#386757),(#386758,#386759,#386760),
(#386761,#386762,#386763),(#386764,#386765,#386766)),.UNSPECIFIED.,.F.,
 .F.,.F.)
B_SPLINE_SURFACE_WITH_KNOTS((4,4),(3,3),(0.,9.54361881492174E-5),(0.,1.),
 .UNSPECIFIED.)
GEOMETRIC_REPRESENTATION_ITEM()
RATIONAL_B_SPLINE_SURFACE(((1.,0.816715621142047,1.),(1.,0.815907587407938,
1.),(1.,0.815115959345211,1.),(1.,0.81433988734918,1.)))
REPRESENTATION_ITEM('')
SURFACE()
);
#2547=(
BOUNDED_SURFACE()
B_SPLINE_SURFACE(3,2,((#386768,#386769,#386770),(#386771,#386772,#386773),
(#386774,#386775,#386776),(#386777,#386778,#386779)),.UNSPECIFIED.,.F.,
 .F.,.F.)
B_SPLINE_SURFACE_WITH_KNOTS((4,4),(3,3),(5.59041745187838E-20,4.68197758448209E-5),
(0.,1.),.UNSPECIFIED.)
GEOMETRIC_REPRESENTATION_ITEM()
RATIONAL_B_SPLINE_SURFACE(((1.,0.81671562114205,1.),(1.,0.953638980025216,
1.),(1.,0.954506925408045,1.),(1.,0.816715621142053,1.)))
REPRESENTATION_ITEM('')
SURFACE()
);
#2548=(
BOUNDED_SURFACE()
B_SPLINE_SURFACE(3,2,((#386781,#386782,#386783),(#386784,#386785,#386786),
(#386787,#386788,#386789),(#386790,#386791,#386792)),.UNSPECIFIED.,.F.,
 .F.,.F.)
B_SPLINE_SURFACE_WITH_KNOTS((4,4),(3,3),(-2.16840434497101E-19,9.54361881492178E-5),
(0.,1.),.UNSPECIFIED.)
GEOMETRIC_REPRESENTATION_ITEM()
RATIONAL_B_SPLINE_SURFACE(((1.,0.814339887349194,1.),(1.,0.815115959345191,
1.),(1.,0.815907587407956,1.),(1.,0.81671562114205,1.)))
REPRESENTATION_ITEM('')
SURFACE()
);
#2549=(
BOUNDED_SURFACE()
B_SPLINE_SURFACE(3,2,((#386794,#386795,#386796),(#386797,#386798,#386799),
(#386800,#386801,#386802),(#386803,#386804,#386805)),.UNSPECIFIED.,.F.,
 .F.,.F.)
B_SPLINE_SURFACE_WITH_KNOTS((4,4),(3,3),(-3.39528393502388E-6,3.73481232852735E-5),
(-0.00165018033239079,1.),.UNSPECIFIED.)
GEOMETRIC_REPRESENTATION_ITEM()
RATIONAL_B_SPLINE_SURFACE(((1.00048354385539,0.853487571660534,1.),(1.00047110510895,
0.857256476851569,1.),(1.00053193201079,0.838826096656041,1.),(1.00063970687691,
0.806170615310252,1.)))
REPRESENTATION_ITEM('')
SURFACE()
);
#2550=(
BOUNDED_SURFACE()
B_SPLINE_SURFACE(3,2,((#386809,#386810,#386811),(#386812,#386813,#386814),
(#386815,#386816,#386817),(#386818,#386819,#386820)),.UNSPECIFIED.,.F.,
 .F.,.F.)
B_SPLINE_SURFACE_WITH_KNOTS((4,4),(3,3),(2.02993869230509E-5,5.39756952687124E-5),
(-0.000116281070051072,1.),.UNSPECIFIED.)
GEOMETRIC_REPRESENTATION_ITEM()
RATIONAL_B_SPLINE_SURFACE(((1.00001770479732,0.923870681143,1.),(1.0000101410406,
0.956394275543444,1.),(1.00002037300281,0.912397594905592,1.),(1.00003390859473,
0.854195550869727,1.)))
REPRESENTATION_ITEM('')
SURFACE()
);
#2551=(
BOUNDED_SURFACE()
B_SPLINE_SURFACE(3,2,((#386913,#386914,#386915),(#386916,#386917,#386918),
(#386919,#386920,#386921),(#386922,#386923,#386924)),.UNSPECIFIED.,.F.,
 .F.,.F.)
B_SPLINE_SURFACE_WITH_KNOTS((4,4),(3,3),(0.00135801595889393,0.00148409170619832),
(0.,1.),.UNSPECIFIED.)
GEOMETRIC_REPRESENTATION_ITEM()
RATIONAL_B_SPLINE_SURFACE(((1.,0.818301933966444,1.),(1.,0.817226613172349,
1.),(1.,0.816179643373945,1.),(1.,0.815159387863654,1.)))
REPRESENTATION_ITEM('')
SURFACE()
);
#2552=(
BOUNDED_SURFACE()
B_SPLINE_SURFACE(3,2,((#386963,#386964,#386965),(#386966,#386967,#386968),
(#386969,#386970,#386971),(#386972,#386973,#386974)),.UNSPECIFIED.,.F.,
 .F.,.F.)
B_SPLINE_SURFACE_WITH_KNOTS((4,4),(3,3),(-1.54744435121951E-6,1.5474443512209E-5),
(-0.0151698983658987,1.),.UNSPECIFIED.)
GEOMETRIC_REPRESENTATION_ITEM()
RATIONAL_B_SPLINE_SURFACE(((1.02018382473466,0.334740937354148,1.),(1.00401234488927,
0.867753072812766,1.),(1.00033622856789,0.988917903080833,1.),(1.,1.,1.)))
REPRESENTATION_ITEM('')
SURFACE()
);
#2553=(
BOUNDED_SURFACE()
B_SPLINE_SURFACE(3,2,((#386976,#386977,#386978),(#386979,#386980,#386981),
(#386982,#386983,#386984),(#386985,#386986,#386987)),.UNSPECIFIED.,.F.,
 .F.,.F.)
B_SPLINE_SURFACE_WITH_KNOTS((4,4),(3,3),(0.00137194782501028,0.00149814269699235),
(0.,1.),.UNSPECIFIED.)
GEOMETRIC_REPRESENTATION_ITEM()
RATIONAL_B_SPLINE_SURFACE(((1.,0.815158509402322,1.),(1.,0.816179044148155,
1.),(1.,0.817226308119924,1.),(1.,0.818301939488806,1.)))
REPRESENTATION_ITEM('')
SURFACE()
);
#2554=(
BOUNDED_SURFACE()
B_SPLINE_SURFACE(3,2,((#387031,#387032,#387033),(#387034,#387035,#387036),
(#387037,#387038,#387039),(#387040,#387041,#387042)),.UNSPECIFIED.,.F.,
 .F.,.F.)
B_SPLINE_SURFACE_WITH_KNOTS((4,4),(3,3),(1.55009486301137E-5,4.92065510474438E-5),
(-8.13759515736558E-5,1.),.UNSPECIFIED.)
GEOMETRIC_REPRESENTATION_ITEM()
RATIONAL_B_SPLINE_SURFACE(((1.00002372912338,0.854200639599664,1.),(1.00001423585995,
0.912530301180544,1.),(1.00000710550472,0.956341495377414,1.),(1.0000123897591,
0.923873338137018,1.)))
REPRESENTATION_ITEM('')
SURFACE()
);
#2555=(
BOUNDED_SURFACE()
B_SPLINE_SURFACE(3,2,((#387046,#387047,#387048),(#387049,#387050,#387051),
(#387052,#387053,#387054),(#387055,#387056,#387057)),.UNSPECIFIED.,.F.,
 .F.,.F.)
B_SPLINE_SURFACE_WITH_KNOTS((4,4),(3,3),(-3.39934179457825E-6,3.73927597403565E-5),
(-0.00186004067397268,1.00069373317423),.UNSPECIFIED.)
GEOMETRIC_REPRESENTATION_ITEM()
RATIONAL_B_SPLINE_SURFACE(((1.00072100136046,0.806051963875417,1.00026859642684),
(1.00060048440147,0.838470803558705,1.0002236999449),(1.00053106448789,
0.857144632272435,1.00019783877215),(1.00054515072846,0.853355459539152,
1.00020308635432)))
REPRESENTATION_ITEM('')
SURFACE()
);
#2556=(
BOUNDED_SURFACE()
B_SPLINE_SURFACE(3,2,((#387059,#387060,#387061),(#387062,#387063,#387064),
(#387065,#387066,#387067),(#387068,#387069,#387070)),.UNSPECIFIED.,.F.,
 .F.,.F.)
B_SPLINE_SURFACE_WITH_KNOTS((4,4),(3,3),(0.,9.54361881492175E-5),(0.,1.),
 .UNSPECIFIED.)
GEOMETRIC_REPRESENTATION_ITEM()
RATIONAL_B_SPLINE_SURFACE(((1.,0.81671562114206,1.),(1.,0.81590758740792,
1.),(1.,0.815115959345222,1.),(1.,0.814339887349192,1.)))
REPRESENTATION_ITEM('')
SURFACE()
);
#2557=(
BOUNDED_SURFACE()
B_SPLINE_SURFACE(3,2,((#387072,#387073,#387074),(#387075,#387076,#387077),
(#387078,#387079,#387080),(#387081,#387082,#387083)),.UNSPECIFIED.,.F.,
 .F.,.F.)
B_SPLINE_SURFACE_WITH_KNOTS((4,4),(3,3),(1.64324391767334E-19,4.68197758448208E-5),
(0.,1.),.UNSPECIFIED.)
GEOMETRIC_REPRESENTATION_ITEM()
RATIONAL_B_SPLINE_SURFACE(((1.,0.816715621142038,1.),(1.,0.953638980025226,
1.),(1.,0.954506925408039,1.),(1.,0.816715621142058,1.)))
REPRESENTATION_ITEM('')
SURFACE()
);
#2558=(
BOUNDED_SURFACE()
B_SPLINE_SURFACE(3,2,((#387085,#387086,#387087),(#387088,#387089,#387090),
(#387091,#387092,#387093),(#387094,#387095,#387096)),.UNSPECIFIED.,.F.,
 .F.,.F.)
B_SPLINE_SURFACE_WITH_KNOTS((4,4),(3,3),(1.62630325872826E-19,9.5436188149218E-5),
(0.,1.),.UNSPECIFIED.)
GEOMETRIC_REPRESENTATION_ITEM()
RATIONAL_B_SPLINE_SURFACE(((1.,0.814339887349191,1.),(1.,0.815115959345203,
1.),(1.,0.815907587407944,1.),(1.,0.816715621142039,1.)))
REPRESENTATION_ITEM('')
SURFACE()
);
#2559=(
BOUNDED_SURFACE()
B_SPLINE_SURFACE(3,2,((#387098,#387099,#387100),(#387101,#387102,#387103),
(#387104,#387105,#387106),(#387107,#387108,#387109)),.UNSPECIFIED.,.F.,
 .F.,.F.)
B_SPLINE_SURFACE_WITH_KNOTS((4,4),(3,3),(-3.39528393502273E-6,3.73481232852735E-5),
(-0.00165018033329502,1.),.UNSPECIFIED.)
GEOMETRIC_REPRESENTATION_ITEM()
RATIONAL_B_SPLINE_SURFACE(((1.00048354385566,0.853487571660388,0.999999999999999),
(1.00047110510921,0.857256476851473,1.),(1.00053193201108,0.838826096655837,
1.),(1.00063970687726,0.80617061531011,1.)))
REPRESENTATION_ITEM('')
SURFACE()
);
#2560=(
BOUNDED_SURFACE()
B_SPLINE_SURFACE(3,2,((#387113,#387114,#387115),(#387116,#387117,#387118),
(#387119,#387120,#387121),(#387122,#387123,#387124)),.UNSPECIFIED.,.F.,
 .F.,.F.)
B_SPLINE_SURFACE_WITH_KNOTS((4,4),(3,3),(2.02993869230509E-5,5.39756952687125E-5),
(-0.000116281069404188,1.),.UNSPECIFIED.)
GEOMETRIC_REPRESENTATION_ITEM()
RATIONAL_B_SPLINE_SURFACE(((1.00001770479722,0.923870681143052,1.),(1.00001014104054,
0.95639427554346,1.),(1.00002037300269,0.912397594905661,1.),(1.00003390859454,
0.854195550869813,1.)))
REPRESENTATION_ITEM('')
SURFACE()
);
#2561=(
BOUNDED_SURFACE()
B_SPLINE_SURFACE(3,2,((#387217,#387218,#387219),(#387220,#387221,#387222),
(#387223,#387224,#387225),(#387226,#387227,#387228)),.UNSPECIFIED.,.F.,
 .F.,.F.)
B_SPLINE_SURFACE_WITH_KNOTS((4,4),(3,3),(0.00135801595889393,0.00148409170619832),
(0.,1.),.UNSPECIFIED.)
GEOMETRIC_REPRESENTATION_ITEM()
RATIONAL_B_SPLINE_SURFACE(((1.,0.818301933966441,1.),(1.,0.817226613172353,
1.),(1.,0.816179643373937,1.),(1.,0.815159387863654,1.)))
REPRESENTATION_ITEM('')
SURFACE()
);
#2562=(
BOUNDED_SURFACE()
B_SPLINE_SURFACE(3,2,((#387267,#387268,#387269),(#387270,#387271,#387272),
(#387273,#387274,#387275),(#387276,#387277,#387278)),.UNSPECIFIED.,.F.,
 .F.,.F.)
B_SPLINE_SURFACE_WITH_KNOTS((4,4),(3,3),(-1.54744435122068E-6,1.54744435122067E-5),
(-0.0151698983720345,1.),.UNSPECIFIED.)
GEOMETRIC_REPRESENTATION_ITEM()
RATIONAL_B_SPLINE_SURFACE(((1.02018382474295,0.334740937350091,1.),(1.00401234489091,
0.867753072811983,1.),(1.00033622856803,0.988917903080762,1.),(1.,1.,1.)))
REPRESENTATION_ITEM('')
SURFACE()
);
#2563=(
BOUNDED_SURFACE()
B_SPLINE_SURFACE(3,2,((#387280,#387281,#387282),(#387283,#387284,#387285),
(#387286,#387287,#387288),(#387289,#387290,#387291)),.UNSPECIFIED.,.F.,
 .F.,.F.)
B_SPLINE_SURFACE_WITH_KNOTS((4,4),(3,3),(0.00137194782501028,0.00149814269699235),
(0.,1.),.UNSPECIFIED.)
GEOMETRIC_REPRESENTATION_ITEM()
RATIONAL_B_SPLINE_SURFACE(((1.,0.815158509402319,1.),(1.,0.816179044148152,
1.),(1.,0.817226308119945,1.),(1.,0.818301939488801,1.)))
REPRESENTATION_ITEM('')
SURFACE()
);
#2564=(
BOUNDED_SURFACE()
B_SPLINE_SURFACE(3,2,((#387335,#387336,#387337),(#387338,#387339,#387340),
(#387341,#387342,#387343),(#387344,#387345,#387346)),.UNSPECIFIED.,.F.,
 .F.,.F.)
B_SPLINE_SURFACE_WITH_KNOTS((4,4),(3,3),(1.55009486301137E-5,4.92065510474429E-5),
(-8.13759515085778E-5,1.),.UNSPECIFIED.)
GEOMETRIC_REPRESENTATION_ITEM()
RATIONAL_B_SPLINE_SURFACE(((1.00002372912336,0.854200639599683,1.),(1.00001423585994,
0.912530301180521,1.),(1.00000710550471,0.956341495377441,1.),(1.00001238975909,
0.923873338137018,1.)))
REPRESENTATION_ITEM('')
SURFACE()
);
#2565=(
BOUNDED_SURFACE()
B_SPLINE_SURFACE(3,2,((#387350,#387351,#387352),(#387353,#387354,#387355),
(#387356,#387357,#387358),(#387359,#387360,#387361)),.UNSPECIFIED.,.F.,
 .F.,.F.)
B_SPLINE_SURFACE_WITH_KNOTS((4,4),(3,3),(-3.39934179457791E-6,3.73927597403567E-5),
(-0.00186004067370867,1.00069373317445),.UNSPECIFIED.)
GEOMETRIC_REPRESENTATION_ITEM()
RATIONAL_B_SPLINE_SURFACE(((1.00072100136036,0.806051963875422,1.00026859642693),
(1.00060048440138,0.838470803558717,1.00022369994497),(1.00053106448781,
0.857144632272427,1.00019783877221),(1.00054515072838,0.853355459539162,
1.00020308635438)))
REPRESENTATION_ITEM('')
SURFACE()
);
#2566=(
BOUNDED_SURFACE()
B_SPLINE_SURFACE(3,2,((#387363,#387364,#387365),(#387366,#387367,#387368),
(#387369,#387370,#387371),(#387372,#387373,#387374)),.UNSPECIFIED.,.F.,
 .F.,.F.)
B_SPLINE_SURFACE_WITH_KNOTS((4,4),(3,3),(-2.71050543121376E-19,9.54361881492173E-5),
(0.,1.),.UNSPECIFIED.)
GEOMETRIC_REPRESENTATION_ITEM()
RATIONAL_B_SPLINE_SURFACE(((1.,0.816715621142049,1.),(1.,0.815907587407939,
1.),(1.,0.815115959345212,1.),(1.,0.814339887349184,1.)))
REPRESENTATION_ITEM('')
SURFACE()
);
#2567=(
BOUNDED_SURFACE()
B_SPLINE_SURFACE(3,2,((#387376,#387377,#387378),(#387379,#387380,#387381),
(#387382,#387383,#387384),(#387385,#387386,#387387)),.UNSPECIFIED.,.F.,
 .F.,.F.)
B_SPLINE_SURFACE_WITH_KNOTS((4,4),(3,3),(-2.71050543121376E-20,4.68197758448208E-5),
(0.,1.),.UNSPECIFIED.)
GEOMETRIC_REPRESENTATION_ITEM()
RATIONAL_B_SPLINE_SURFACE(((1.,0.816715621142045,1.),(1.,0.953638980025206,
1.),(1.,0.954506925408058,1.),(1.,0.816715621142055,1.)))
REPRESENTATION_ITEM('')
SURFACE()
);
#2568=(
BOUNDED_SURFACE()
B_SPLINE_SURFACE(3,2,((#387389,#387390,#387391),(#387392,#387393,#387394),
(#387395,#387396,#387397),(#387398,#387399,#387400)),.UNSPECIFIED.,.F.,
 .F.,.F.)
B_SPLINE_SURFACE_WITH_KNOTS((4,4),(3,3),(-2.16840434497101E-19,9.54361881492175E-5),
(0.,1.),.UNSPECIFIED.)
GEOMETRIC_REPRESENTATION_ITEM()
RATIONAL_B_SPLINE_SURFACE(((1.,0.814339887349195,1.),(1.,0.815115959345194,
1.),(1.,0.815907587407954,1.),(1.,0.816715621142052,1.)))
REPRESENTATION_ITEM('')
SURFACE()
);
#2569=(
BOUNDED_SURFACE()
B_SPLINE_SURFACE(3,2,((#387402,#387403,#387404),(#387405,#387406,#387407),
(#387408,#387409,#387410),(#387411,#387412,#387413)),.UNSPECIFIED.,.F.,
 .F.,.F.)
B_SPLINE_SURFACE_WITH_KNOTS((4,4),(3,3),(-3.39528393502381E-6,3.73481232852725E-5),
(-0.00165018033340393,1.),.UNSPECIFIED.)
GEOMETRIC_REPRESENTATION_ITEM()
RATIONAL_B_SPLINE_SURFACE(((1.00048354385569,0.85348757166039,1.),(1.00047110510924,
0.857256476851414,1.),(1.00053193201111,0.83882609665589,1.),(1.0006397068773,
0.806170615310054,1.)))
REPRESENTATION_ITEM('')
SURFACE()
);
#2570=(
BOUNDED_SURFACE()
B_SPLINE_SURFACE(3,2,((#387417,#387418,#387419),(#387420,#387421,#387422),
(#387423,#387424,#387425),(#387426,#387427,#387428)),.UNSPECIFIED.,.F.,
 .F.,.F.)
B_SPLINE_SURFACE_WITH_KNOTS((4,4),(3,3),(2.02993869230509E-5,5.39756952687122E-5),
(-0.000116281069851099,1.),.UNSPECIFIED.)
GEOMETRIC_REPRESENTATION_ITEM()
RATIONAL_B_SPLINE_SURFACE(((1.00001770479729,0.923870681143016,1.),(1.00001014104058,
0.956394275543448,1.),(1.00002037300277,0.912397594905624,1.),(1.00003390859467,
0.854195550869753,1.)))
REPRESENTATION_ITEM('')
SURFACE()
);
#2571=(
BOUNDED_SURFACE()
B_SPLINE_SURFACE(3,2,((#387521,#387522,#387523),(#387524,#387525,#387526),
(#387527,#387528,#387529),(#387530,#387531,#387532)),.UNSPECIFIED.,.F.,
 .F.,.F.)
B_SPLINE_SURFACE_WITH_KNOTS((4,4),(3,3),(0.00135801595889393,0.00148409170619832),
(0.,1.),.UNSPECIFIED.)
GEOMETRIC_REPRESENTATION_ITEM()
RATIONAL_B_SPLINE_SURFACE(((1.,0.818301933966442,1.),(1.,0.817226613172339,
1.),(1.,0.816179643373948,1.),(1.,0.815159387863652,1.)))
REPRESENTATION_ITEM('')
SURFACE()
);
#2572=(
BOUNDED_SURFACE()
B_SPLINE_SURFACE(3,2,((#387571,#387572,#387573),(#387574,#387575,#387576),
(#387577,#387578,#387579),(#387580,#387581,#387582)),.UNSPECIFIED.,.F.,
 .F.,.F.)
B_SPLINE_SURFACE_WITH_KNOTS((4,4),(3,3),(-1.54744435122023E-6,1.54744435122092E-5),
(-0.0151698983759789,1.),.UNSPECIFIED.)
GEOMETRIC_REPRESENTATION_ITEM()
RATIONAL_B_SPLINE_SURFACE(((1.02018382474828,0.334740937347494,1.),(1.00401234489197,
0.867753072811548,1.),(1.00033622856812,0.988917903080688,1.),(1.,1.,1.)))
REPRESENTATION_ITEM('')
SURFACE()
);
#2573=(
BOUNDED_SURFACE()
B_SPLINE_SURFACE(3,2,((#387584,#387585,#387586),(#387587,#387588,#387589),
(#387590,#387591,#387592),(#387593,#387594,#387595)),.UNSPECIFIED.,.F.,
 .F.,.F.)
B_SPLINE_SURFACE_WITH_KNOTS((4,4),(3,3),(0.00137194782501028,0.00149814269699235),
(0.,1.),.UNSPECIFIED.)
GEOMETRIC_REPRESENTATION_ITEM()
RATIONAL_B_SPLINE_SURFACE(((1.,0.81515850940232,1.),(1.,0.816179044148172,
1.),(1.,0.817226308119932,1.),(1.,0.818301939488812,1.)))
REPRESENTATION_ITEM('')
SURFACE()
);
#2574=(
BOUNDED_SURFACE()
B_SPLINE_SURFACE(3,2,((#387639,#387640,#387641),(#387642,#387643,#387644),
(#387645,#387646,#387647),(#387648,#387649,#387650)),.UNSPECIFIED.,.F.,
 .F.,.F.)
B_SPLINE_SURFACE_WITH_KNOTS((4,4),(3,3),(1.55009486301137E-5,4.92065510474435E-5),
(-8.13759514590226E-5,1.),.UNSPECIFIED.)
GEOMETRIC_REPRESENTATION_ITEM()
RATIONAL_B_SPLINE_SURFACE(((1.00002372912335,0.854200639599691,1.),(1.00001423585993,
0.912530301180533,1.),(1.00000710550471,0.956341495377436,1.),(1.00001238975908,
0.923873338137026,1.)))
REPRESENTATION_ITEM('')
SURFACE()
);
#2575=(
BOUNDED_SURFACE()
B_SPLINE_SURFACE(3,2,((#387654,#387655,#387656),(#387657,#387658,#387659),
(#387660,#387661,#387662),(#387663,#387664,#387665)),.UNSPECIFIED.,.F.,
 .F.,.F.)
B_SPLINE_SURFACE_WITH_KNOTS((4,4),(3,3),(-3.39934179457859E-6,3.73927597403564E-5),
(-0.0018600406738678,1.00069373317437),.UNSPECIFIED.)
GEOMETRIC_REPRESENTATION_ITEM()
RATIONAL_B_SPLINE_SURFACE(((1.00072100136042,0.80605196387541,1.0002685964269),
(1.00060048440144,0.838470803558693,1.00022369994495),(1.00053106448786,
0.857144632272428,1.00019783877219),(1.00054515072843,0.853355459539146,
1.00020308635436)))
REPRESENTATION_ITEM('')
SURFACE()
);
#2576=(
BOUNDED_SURFACE()
B_SPLINE_SURFACE(3,2,((#387667,#387668,#387669),(#387670,#387671,#387672),
(#387673,#387674,#387675),(#387676,#387677,#387678)),.UNSPECIFIED.,.F.,
 .F.,.F.)
B_SPLINE_SURFACE_WITH_KNOTS((4,4),(3,3),(3.25260651745651E-19,9.54361881492174E-5),
(0.,1.),.UNSPECIFIED.)
GEOMETRIC_REPRESENTATION_ITEM()
RATIONAL_B_SPLINE_SURFACE(((1.,0.816715621142049,1.),(1.,0.815907587407951,
1.),(1.,0.815115959345193,1.),(1.,0.814339887349191,1.)))
REPRESENTATION_ITEM('')
SURFACE()
);
#2577=(
BOUNDED_SURFACE()
B_SPLINE_SURFACE(3,2,((#387680,#387681,#387682),(#387683,#387684,#387685),
(#387686,#387687,#387688),(#387689,#387690,#387691)),.UNSPECIFIED.,.F.,
 .F.,.F.)
B_SPLINE_SURFACE_WITH_KNOTS((4,4),(3,3),(2.84603070277445E-19,4.68197758448212E-5),
(0.,1.),.UNSPECIFIED.)
GEOMETRIC_REPRESENTATION_ITEM()
RATIONAL_B_SPLINE_SURFACE(((1.,0.816715621142052,1.),(1.,0.953638980025206,
1.),(1.,0.954506925408059,1.),(1.,0.816715621142047,1.)))
REPRESENTATION_ITEM('')
SURFACE()
);
#2578=(
BOUNDED_SURFACE()
B_SPLINE_SURFACE(3,2,((#387693,#387694,#387695),(#387696,#387697,#387698),
(#387699,#387700,#387701),(#387702,#387703,#387704)),.UNSPECIFIED.,.F.,
 .F.,.F.)
B_SPLINE_SURFACE_WITH_KNOTS((4,4),(3,3),(5.42101086242752E-20,9.54361881492178E-5),
(0.,1.),.UNSPECIFIED.)
GEOMETRIC_REPRESENTATION_ITEM()
RATIONAL_B_SPLINE_SURFACE(((1.,0.814339887349196,1.),(1.,0.815115959345201,
1.),(1.,0.81590758740795,1.),(1.,0.816715621142052,1.)))
REPRESENTATION_ITEM('')
SURFACE()
);
#2579=(
BOUNDED_SURFACE()
B_SPLINE_SURFACE(3,2,((#387706,#387707,#387708),(#387709,#387710,#387711),
(#387712,#387713,#387714),(#387715,#387716,#387717)),.UNSPECIFIED.,.F.,
 .F.,.F.)
B_SPLINE_SURFACE_WITH_KNOTS((4,4),(3,3),(-3.39528393502485E-6,3.73481232852734E-5),
(-0.00165018033328164,1.),.UNSPECIFIED.)
GEOMETRIC_REPRESENTATION_ITEM()
RATIONAL_B_SPLINE_SURFACE(((1.00048354385565,0.853487571660389,1.),(1.00047110510921,
0.857256476851473,1.),(1.00053193201107,0.838826096655867,1.),(1.00063970687725,
0.806170615310098,0.999999999999999)))
REPRESENTATION_ITEM('')
SURFACE()
);
#2580=(
BOUNDED_SURFACE()
B_SPLINE_SURFACE(3,2,((#387721,#387722,#387723),(#387724,#387725,#387726),
(#387727,#387728,#387729),(#387730,#387731,#387732)),.UNSPECIFIED.,.F.,
 .F.,.F.)
B_SPLINE_SURFACE_WITH_KNOTS((4,4),(3,3),(2.02993869230509E-5,5.39756952687131E-5),
(-0.000116281069453101,1.),.UNSPECIFIED.)
GEOMETRIC_REPRESENTATION_ITEM()
RATIONAL_B_SPLINE_SURFACE(((1.00001770479723,0.923870681143048,1.),(1.00001014104055,
0.956394275543459,1.),(1.0000203730027,0.912397594905651,1.),(1.00003390859455,
0.854195550869809,1.)))
REPRESENTATION_ITEM('')
SURFACE()
);
#2581=(
BOUNDED_SURFACE()
B_SPLINE_SURFACE(3,2,((#387825,#387826,#387827),(#387828,#387829,#387830),
(#387831,#387832,#387833),(#387834,#387835,#387836)),.UNSPECIFIED.,.F.,
 .F.,.F.)
B_SPLINE_SURFACE_WITH_KNOTS((4,4),(3,3),(0.00135801595889393,0.00148409170619832),
(0.,1.),.UNSPECIFIED.)
GEOMETRIC_REPRESENTATION_ITEM()
RATIONAL_B_SPLINE_SURFACE(((1.,0.818301933966442,1.),(1.,0.817226613172366,
1.),(1.,0.816179643373922,1.),(1.,0.815159387863662,1.)))
REPRESENTATION_ITEM('')
SURFACE()
);
#2582=(
BOUNDED_SURFACE()
B_SPLINE_SURFACE(3,2,((#387875,#387876,#387877),(#387878,#387879,#387880),
(#387881,#387882,#387883),(#387884,#387885,#387886)),.UNSPECIFIED.,.F.,
 .F.,.F.)
B_SPLINE_SURFACE_WITH_KNOTS((4,4),(3,3),(-1.54744435122083E-6,1.54744435122081E-5),
(-0.0151698983611594,1.0151698983615),.UNSPECIFIED.)
GEOMETRIC_REPRESENTATION_ITEM()
RATIONAL_B_SPLINE_SURFACE(((1.02018382472826,0.324498219413338,1.02018382472872),
(1.00401234488799,0.865716921710435,1.00401234488809),(1.00033622856778,
0.988747276629712,1.00033622856779),(1.,1.,1.)))
REPRESENTATION_ITEM('')
SURFACE()
);
#2583=(
BOUNDED_SURFACE()
B_SPLINE_SURFACE(3,2,((#387888,#387889,#387890),(#387891,#387892,#387893),
(#387894,#387895,#387896),(#387897,#387898,#387899)),.UNSPECIFIED.,.F.,
 .F.,.F.)
B_SPLINE_SURFACE_WITH_KNOTS((4,4),(3,3),(0.00137194782501028,0.00149814269699235),
(0.,1.),.UNSPECIFIED.)
GEOMETRIC_REPRESENTATION_ITEM()
RATIONAL_B_SPLINE_SURFACE(((1.,0.815158509402319,1.),(1.,0.816179044148163,
1.),(1.,0.817226308119931,1.),(1.,0.818301939488809,1.)))
REPRESENTATION_ITEM('')
SURFACE()
);
#2584=(
BOUNDED_SURFACE()
B_SPLINE_SURFACE(3,2,((#387943,#387944,#387945),(#387946,#387947,#387948),
(#387949,#387950,#387951),(#387952,#387953,#387954)),.UNSPECIFIED.,.F.,
 .F.,.F.)
B_SPLINE_SURFACE_WITH_KNOTS((4,4),(3,3),(1.55009486301137E-5,4.92065510474435E-5),
(-8.13759514136358E-5,1.),.UNSPECIFIED.)
GEOMETRIC_REPRESENTATION_ITEM()
RATIONAL_B_SPLINE_SURFACE(((1.00002372912334,0.854200639599699,1.),(1.00001423585992,
0.912530301180534,1.),(1.0000071055047,0.956341495377437,1.),(1.00001238975907,
0.923873338137028,1.)))
REPRESENTATION_ITEM('')
SURFACE()
);
#2585=(
BOUNDED_SURFACE()
B_SPLINE_SURFACE(3,2,((#387958,#387959,#387960),(#387961,#387962,#387963),
(#387964,#387965,#387966),(#387967,#387968,#387969)),.UNSPECIFIED.,.F.,
 .F.,.F.)
B_SPLINE_SURFACE_WITH_KNOTS((4,4),(3,3),(-3.39934179457858E-6,3.73927597403564E-5),
(-0.00186004067417087,1.0006937331743),.UNSPECIFIED.)
GEOMETRIC_REPRESENTATION_ITEM()
RATIONAL_B_SPLINE_SURFACE(((1.00072100136054,0.806051963875373,1.00026859642687),
(1.00060048440153,0.838470803558666,1.00022369994493),(1.00053106448794,
0.857144632272389,1.00019783877217),(1.00054515072852,0.853355459539116,
1.00020308635434)))
REPRESENTATION_ITEM('')
SURFACE()
);
#2586=(
BOUNDED_SURFACE()
B_SPLINE_SURFACE(3,2,((#387971,#387972,#387973),(#387974,#387975,#387976),
(#387977,#387978,#387979),(#387980,#387981,#387982)),.UNSPECIFIED.,.F.,
 .F.,.F.)
B_SPLINE_SURFACE_WITH_KNOTS((4,4),(3,3),(1.62630325872826E-19,9.54361881492172E-5),
(0.,1.),.UNSPECIFIED.)
GEOMETRIC_REPRESENTATION_ITEM()
RATIONAL_B_SPLINE_SURFACE(((1.,0.816715621142049,1.),(1.,0.815907587407932,
1.),(1.,0.815115959345205,1.),(1.,0.814339887349192,1.)))
REPRESENTATION_ITEM('')
SURFACE()
);
#2587=(
BOUNDED_SURFACE()
B_SPLINE_SURFACE(3,2,((#387984,#387985,#387986),(#387987,#387988,#387989),
(#387990,#387991,#387992),(#387993,#387994,#387995)),.UNSPECIFIED.,.F.,
 .F.,.F.)
B_SPLINE_SURFACE_WITH_KNOTS((4,4),(3,3),(1.25360876193636E-19,4.6819775844821E-5),
(0.,1.),.UNSPECIFIED.)
GEOMETRIC_REPRESENTATION_ITEM()
RATIONAL_B_SPLINE_SURFACE(((1.,0.816715621142052,1.),(1.,0.953638980025202,
1.),(1.,0.954506925408057,1.),(1.,0.816715621142041,1.)))
REPRESENTATION_ITEM('')
SURFACE()
);
#2588=(
BOUNDED_SURFACE()
B_SPLINE_SURFACE(3,2,((#387997,#387998,#387999),(#388000,#388001,#388002),
(#388003,#388004,#388005),(#388006,#388007,#388008)),.UNSPECIFIED.,.F.,
 .F.,.F.)
B_SPLINE_SURFACE_WITH_KNOTS((4,4),(3,3),(-5.42101086242752E-20,9.54361881492177E-5),
(0.,1.),.UNSPECIFIED.)
GEOMETRIC_REPRESENTATION_ITEM()
RATIONAL_B_SPLINE_SURFACE(((1.,0.814339887349194,1.),(1.,0.815115959345217,
1.),(1.,0.815907587407937,1.),(1.,0.816715621142052,1.)))
REPRESENTATION_ITEM('')
SURFACE()
);
#2589=(
BOUNDED_SURFACE()
B_SPLINE_SURFACE(3,2,((#388010,#388011,#388012),(#388013,#388014,#388015),
(#388016,#388017,#388018),(#388019,#388020,#388021)),.UNSPECIFIED.,.F.,
 .F.,.F.)
B_SPLINE_SURFACE_WITH_KNOTS((4,4),(3,3),(-3.3952839350248E-6,3.73481232852735E-5),
(-0.00165018033333831,1.),.UNSPECIFIED.)
GEOMETRIC_REPRESENTATION_ITEM()
RATIONAL_B_SPLINE_SURFACE(((1.00048354385567,0.853487571660397,1.),(1.00047110510922,
0.857256476851433,1.),(1.00053193201109,0.83882609665588,1.),(1.00063970687728,
0.80617061531008,1.)))
REPRESENTATION_ITEM('')
SURFACE()
);
#2590=(
BOUNDED_SURFACE()
B_SPLINE_SURFACE(3,2,((#388025,#388026,#388027),(#388028,#388029,#388030),
(#388031,#388032,#388033),(#388034,#388035,#388036)),.UNSPECIFIED.,.F.,
 .F.,.F.)
B_SPLINE_SURFACE_WITH_KNOTS((4,4),(3,3),(2.0299386923051E-5,5.39756952687129E-5),
(-0.000116281069825858,1.),.UNSPECIFIED.)
GEOMETRIC_REPRESENTATION_ITEM()
RATIONAL_B_SPLINE_SURFACE(((1.00001770479728,0.923870681143017,1.),(1.00001014104058,
0.956394275543444,1.),(1.00002037300277,0.912397594905627,1.),(1.00003390859466,
0.854195550869749,1.)))
REPRESENTATION_ITEM('')
SURFACE()
);
#2591=(
BOUNDED_SURFACE()
B_SPLINE_SURFACE(3,2,((#388129,#388130,#388131),(#388132,#388133,#388134),
(#388135,#388136,#388137),(#388138,#388139,#388140)),.UNSPECIFIED.,.F.,
 .F.,.F.)
B_SPLINE_SURFACE_WITH_KNOTS((4,4),(3,3),(0.00135801595889393,0.00148409170619832),
(0.,1.),.UNSPECIFIED.)
GEOMETRIC_REPRESENTATION_ITEM()
RATIONAL_B_SPLINE_SURFACE(((1.,0.818301933966442,1.),(1.,0.817226613172345,
1.),(1.,0.816179643373941,1.),(1.,0.815159387863652,1.)))
REPRESENTATION_ITEM('')
SURFACE()
);
#2592=(
BOUNDED_SURFACE()
B_SPLINE_SURFACE(3,2,((#388179,#388180,#388181),(#388182,#388183,#388184),
(#388185,#388186,#388187),(#388188,#388189,#388190)),.UNSPECIFIED.,.F.,
 .F.,.F.)
B_SPLINE_SURFACE_WITH_KNOTS((4,4),(3,3),(-1.54744435122098E-6,1.54744435122099E-5),
(-0.0151698983702731,1.),.UNSPECIFIED.)
GEOMETRIC_REPRESENTATION_ITEM()
RATIONAL_B_SPLINE_SURFACE(((1.02018382474057,0.334740937351171,1.),(1.00401234489044,
0.86775307281218,1.),(1.00033622856799,0.988917903080774,1.),(1.,1.,1.)))
REPRESENTATION_ITEM('')
SURFACE()
);
#2593=(
BOUNDED_SURFACE()
B_SPLINE_SURFACE(3,2,((#388192,#388193,#388194),(#388195,#388196,#388197),
(#388198,#388199,#388200),(#388201,#388202,#388203)),.UNSPECIFIED.,.F.,
 .F.,.F.)
B_SPLINE_SURFACE_WITH_KNOTS((4,4),(3,3),(0.00137194782501028,0.00149814269699235),
(0.,1.),.UNSPECIFIED.)
GEOMETRIC_REPRESENTATION_ITEM()
RATIONAL_B_SPLINE_SURFACE(((1.,0.815158509402318,1.),(1.,0.816179044148197,
1.),(1.,0.817226308119904,1.),(1.,0.818301939488812,1.)))
REPRESENTATION_ITEM('')
SURFACE()
);
#2594=(
BOUNDED_SURFACE()
B_SPLINE_SURFACE(3,2,((#388247,#388248,#388249),(#388250,#388251,#388252),
(#388253,#388254,#388255),(#388256,#388257,#388258)),.UNSPECIFIED.,.F.,
 .F.,.F.)
B_SPLINE_SURFACE_WITH_KNOTS((4,4),(3,3),(1.55009486301137E-5,4.92065510474437E-5),
(-8.13759516110161E-5,1.),.UNSPECIFIED.)
GEOMETRIC_REPRESENTATION_ITEM()
RATIONAL_B_SPLINE_SURFACE(((1.00002372912339,0.85420063959966,1.),(1.00001423585996,
0.91253030118053,1.),(1.00000710550472,0.956341495377427,1.),(1.0000123897591,
0.923873338137008,1.)))
REPRESENTATION_ITEM('')
SURFACE()
);
#2595=(
BOUNDED_SURFACE()
B_SPLINE_SURFACE(3,2,((#388262,#388263,#388264),(#388265,#388266,#388267),
(#388268,#388269,#388270),(#388271,#388272,#388273)),.UNSPECIFIED.,.F.,
 .F.,.F.)
B_SPLINE_SURFACE_WITH_KNOTS((4,4),(3,3),(-3.39934179457838E-6,3.73927597403563E-5),
(-0.00186004067450901,1.00069373317437),.UNSPECIFIED.)
GEOMETRIC_REPRESENTATION_ITEM()
RATIONAL_B_SPLINE_SURFACE(((1.00072100136067,0.8060519638753,1.0002685964269),
(1.00060048440164,0.83847080355858,1.00022369994495),(1.00053106448804,
0.857144632272337,1.00019783877219),(1.00054515072862,0.853355459539053,
1.00020308635436)))
REPRESENTATION_ITEM('')
SURFACE()
);
#2596=(
BOUNDED_SURFACE()
B_SPLINE_SURFACE(3,2,((#388275,#388276,#388277),(#388278,#388279,#388280),
(#388281,#388282,#388283),(#388284,#388285,#388286)),.UNSPECIFIED.,.F.,
 .F.,.F.)
B_SPLINE_SURFACE_WITH_KNOTS((4,4),(3,3),(4.33680868994202E-19,9.54361881492176E-5),
(0.,1.),.UNSPECIFIED.)
GEOMETRIC_REPRESENTATION_ITEM()
RATIONAL_B_SPLINE_SURFACE(((1.,0.816715621142048,1.),(1.,0.815907587407924,
1.),(1.,0.815115959345207,1.),(1.,0.8143398873492,1.)))
REPRESENTATION_ITEM('')
SURFACE()
);
#2597=(
BOUNDED_SURFACE()
B_SPLINE_SURFACE(3,2,((#388288,#388289,#388290),(#388291,#388292,#388293),
(#388294,#388295,#388296),(#388297,#388298,#388299)),.UNSPECIFIED.,.F.,
 .F.,.F.)
B_SPLINE_SURFACE_WITH_KNOTS((4,4),(3,3),(6.26804380968182E-20,4.68197758448211E-5),
(0.,1.),.UNSPECIFIED.)
GEOMETRIC_REPRESENTATION_ITEM()
RATIONAL_B_SPLINE_SURFACE(((1.,0.816715621142051,1.),(1.,0.953638980025213,
1.),(1.,0.954506925408048,1.),(1.,0.816715621142054,1.)))
REPRESENTATION_ITEM('')
SURFACE()
);
#2598=(
BOUNDED_SURFACE()
B_SPLINE_SURFACE(3,2,((#388301,#388302,#388303),(#388304,#388305,#388306),
(#388307,#388308,#388309),(#388310,#388311,#388312)),.UNSPECIFIED.,.F.,
 .F.,.F.)
B_SPLINE_SURFACE_WITH_KNOTS((4,4),(3,3),(-1.62630325872826E-19,9.54361881492177E-5),
(0.,1.),.UNSPECIFIED.)
GEOMETRIC_REPRESENTATION_ITEM()
RATIONAL_B_SPLINE_SURFACE(((1.,0.814339887349196,1.),(1.,0.815115959345208,
1.),(1.,0.815907587407945,1.),(1.,0.816715621142051,1.)))
REPRESENTATION_ITEM('')
SURFACE()
);
#2599=(
BOUNDED_SURFACE()
B_SPLINE_SURFACE(3,2,((#388314,#388315,#388316),(#388317,#388318,#388319),
(#388320,#388321,#388322),(#388323,#388324,#388325)),.UNSPECIFIED.,.F.,
 .F.,.F.)
B_SPLINE_SURFACE_WITH_KNOTS((4,4),(3,3),(-3.39528393502485E-6,3.73481232852728E-5),
(-0.00165018033331429,1.),.UNSPECIFIED.)
GEOMETRIC_REPRESENTATION_ITEM()
RATIONAL_B_SPLINE_SURFACE(((1.00048354385566,0.85348757166039,1.),(1.00047110510922,
0.857256476851484,1.),(1.00053193201108,0.838826096655838,1.),(1.00063970687727,
0.806170615310114,1.)))
REPRESENTATION_ITEM('')
SURFACE()
);
#2600=(
BOUNDED_SURFACE()
B_SPLINE_SURFACE(3,2,((#388329,#388330,#388331),(#388332,#388333,#388334),
(#388335,#388336,#388337),(#388338,#388339,#388340)),.UNSPECIFIED.,.F.,
 .F.,.F.)
B_SPLINE_SURFACE_WITH_KNOTS((4,4),(3,3),(2.02993869230509E-5,5.39756952687124E-5),
(-0.000116281070022815,1.),.UNSPECIFIED.)
GEOMETRIC_REPRESENTATION_ITEM()
RATIONAL_B_SPLINE_SURFACE(((1.00001770479731,0.923870681143008,1.),(1.0000101410406,
0.956394275543434,1.),(1.0000203730028,0.912397594905605,1.),(1.00003390859472,
0.854195550869727,1.)))
REPRESENTATION_ITEM('')
SURFACE()
);
#2601=(
BOUNDED_SURFACE()
B_SPLINE_SURFACE(3,2,((#388433,#388434,#388435),(#388436,#388437,#388438),
(#388439,#388440,#388441),(#388442,#388443,#388444)),.UNSPECIFIED.,.F.,
 .F.,.F.)
B_SPLINE_SURFACE_WITH_KNOTS((4,4),(3,3),(0.00135801595889393,0.00148409170619832),
(0.,1.),.UNSPECIFIED.)
GEOMETRIC_REPRESENTATION_ITEM()
RATIONAL_B_SPLINE_SURFACE(((1.,0.818301933966433,1.),(1.,0.817226613172354,
1.),(1.,0.816179643373948,1.),(1.,0.815159387863654,1.)))
REPRESENTATION_ITEM('')
SURFACE()
);
#2602=(
BOUNDED_SURFACE()
B_SPLINE_SURFACE(3,2,((#388483,#388484,#388485),(#388486,#388487,#388488),
(#388489,#388490,#388491),(#388492,#388493,#388494)),.UNSPECIFIED.,.F.,
 .F.,.F.)
B_SPLINE_SURFACE_WITH_KNOTS((4,4),(3,3),(5.90805480709874E-20,1.54744435122067E-5),
(0.,1.),.UNSPECIFIED.)
GEOMETRIC_REPRESENTATION_ITEM()
RATIONAL_B_SPLINE_SURFACE(((1.,0.478041569704953,1.),(1.,0.890533857552143,
1.),(1.,0.990075913815874,1.),(1.,1.,1.)))
REPRESENTATION_ITEM('')
SURFACE()
);
#2603=(
BOUNDED_SURFACE()
B_SPLINE_SURFACE(3,2,((#388496,#388497,#388498),(#388499,#388500,#388501),
(#388502,#388503,#388504),(#388505,#388506,#388507)),.UNSPECIFIED.,.F.,
 .F.,.F.)
B_SPLINE_SURFACE_WITH_KNOTS((4,4),(3,3),(0.00137194782501028,0.00149814269699235),
(0.,1.),.UNSPECIFIED.)
GEOMETRIC_REPRESENTATION_ITEM()
RATIONAL_B_SPLINE_SURFACE(((1.,0.81515850940233,1.),(1.,0.816179044148154,
1.),(1.,0.817226308119924,1.),(1.,0.818301939488809,1.)))
REPRESENTATION_ITEM('')
SURFACE()
);
#2604=(
BOUNDED_SURFACE()
B_SPLINE_SURFACE(3,2,((#388551,#388552,#388553),(#388554,#388555,#388556),
(#388557,#388558,#388559),(#388560,#388561,#388562)),.UNSPECIFIED.,.F.,
 .F.,.F.)
B_SPLINE_SURFACE_WITH_KNOTS((4,4),(3,3),(1.55009486301137E-5,4.92065510474431E-5),
(-8.13759513751905E-5,1.),.UNSPECIFIED.)
GEOMETRIC_REPRESENTATION_ITEM()
RATIONAL_B_SPLINE_SURFACE(((1.00002372912332,0.854200639599697,1.),(1.00001423585992,
0.912530301180547,1.),(1.0000071055047,0.956341495377435,1.),(1.00001238975907,
0.923873338137029,1.)))
REPRESENTATION_ITEM('')
SURFACE()
);
#2605=(
BOUNDED_SURFACE()
B_SPLINE_SURFACE(3,2,((#388566,#388567,#388568),(#388569,#388570,#388571),
(#388572,#388573,#388574),(#388575,#388576,#388577)),.UNSPECIFIED.,.F.,
 .F.,.F.)
B_SPLINE_SURFACE_WITH_KNOTS((4,4),(3,3),(-3.39934179457832E-6,3.73927597403566E-5),
(-0.00186004067413571,1.00069373317433),.UNSPECIFIED.)
GEOMETRIC_REPRESENTATION_ITEM()
RATIONAL_B_SPLINE_SURFACE(((1.00072100136053,0.806051963875365,1.00026859642689),
(1.00060048440152,0.838470803558657,1.00022369994494),(1.00053106448793,
0.857144632272392,1.00019783877218),(1.00054515072851,0.853355459539125,
1.00020308635435)))
REPRESENTATION_ITEM('')
SURFACE()
);
#2606=(
BOUNDED_SURFACE()
B_SPLINE_SURFACE(3,2,((#388579,#388580,#388581),(#388582,#388583,#388584),
(#388585,#388586,#388587),(#388588,#388589,#388590)),.UNSPECIFIED.,.F.,
 .F.,.F.)
B_SPLINE_SURFACE_WITH_KNOTS((4,4),(3,3),(1.0842021724855E-19,9.54361881492174E-5),
(0.,1.),.UNSPECIFIED.)
GEOMETRIC_REPRESENTATION_ITEM()
RATIONAL_B_SPLINE_SURFACE(((1.,0.816715621142049,1.),(1.,0.815907587407935,
1.),(1.,0.815115959345209,1.),(1.,0.814339887349194,1.)))
REPRESENTATION_ITEM('')
SURFACE()
);
#2607=(
BOUNDED_SURFACE()
B_SPLINE_SURFACE(3,2,((#388592,#388593,#388594),(#388595,#388596,#388597),
(#388598,#388599,#388600),(#388601,#388602,#388603)),.UNSPECIFIED.,.F.,
 .F.,.F.)
B_SPLINE_SURFACE_WITH_KNOTS((4,4),(3,3),(-3.06625926906057E-19,4.68197758448209E-5),
(0.,1.),.UNSPECIFIED.)
GEOMETRIC_REPRESENTATION_ITEM()
RATIONAL_B_SPLINE_SURFACE(((1.,0.816715621142046,1.),(1.,0.953638980025209,
1.),(1.,0.954506925408055,1.),(1.,0.81671562114205,1.)))
REPRESENTATION_ITEM('')
SURFACE()
);
#2608=(
BOUNDED_SURFACE()
B_SPLINE_SURFACE(3,2,((#388605,#388606,#388607),(#388608,#388609,#388610),
(#388611,#388612,#388613),(#388614,#388615,#388616)),.UNSPECIFIED.,.F.,
 .F.,.F.)
B_SPLINE_SURFACE_WITH_KNOTS((4,4),(3,3),(-5.42101086242752E-20,9.54361881492177E-5),
(0.,1.),.UNSPECIFIED.)
GEOMETRIC_REPRESENTATION_ITEM()
RATIONAL_B_SPLINE_SURFACE(((1.,0.814339887349194,1.),(1.,0.81511595934521,
1.),(1.,0.815907587407933,1.),(1.,0.816715621142052,1.)))
REPRESENTATION_ITEM('')
SURFACE()
);
#2609=(
BOUNDED_SURFACE()
B_SPLINE_SURFACE(3,2,((#388618,#388619,#388620),(#388621,#388622,#388623),
(#388624,#388625,#388626),(#388627,#388628,#388629)),.UNSPECIFIED.,.F.,
 .F.,.F.)
B_SPLINE_SURFACE_WITH_KNOTS((4,4),(3,3),(-3.3952839350248E-6,3.73481232852734E-5),
(-0.00165018033261607,1.),.UNSPECIFIED.)
GEOMETRIC_REPRESENTATION_ITEM()
RATIONAL_B_SPLINE_SURFACE(((1.00048354385546,0.853487571660518,1.),(1.00047110510902,
0.857256476851525,1.),(1.00053193201086,0.83882609665601,1.),(1.000639706877,
0.806170615310205,1.)))
REPRESENTATION_ITEM('')
SURFACE()
);
#2610=(
BOUNDED_SURFACE()
B_SPLINE_SURFACE(3,2,((#388633,#388634,#388635),(#388636,#388637,#388638),
(#388639,#388640,#388641),(#388642,#388643,#388644)),.UNSPECIFIED.,.F.,
 .F.,.F.)
B_SPLINE_SURFACE_WITH_KNOTS((4,4),(3,3),(2.02993869230509E-5,5.39756952687129E-5),
(-0.000116281069137242,1.),.UNSPECIFIED.)
GEOMETRIC_REPRESENTATION_ITEM()
RATIONAL_B_SPLINE_SURFACE(((1.00001770479718,0.923870681143067,1.),(1.00001014104052,
0.95639427554348,1.),(1.00002037300265,0.912397594905681,1.),(1.00003390859446,
0.854195550869853,1.)))
REPRESENTATION_ITEM('')
SURFACE()
);
#2611=(
BOUNDED_SURFACE()
B_SPLINE_SURFACE(3,2,((#388737,#388738,#388739),(#388740,#388741,#388742),
(#388743,#388744,#388745),(#388746,#388747,#388748)),.UNSPECIFIED.,.F.,
 .F.,.F.)
B_SPLINE_SURFACE_WITH_KNOTS((4,4),(3,3),(0.00135801595889393,0.00148409170619832),
(0.,1.),.UNSPECIFIED.)
GEOMETRIC_REPRESENTATION_ITEM()
RATIONAL_B_SPLINE_SURFACE(((1.,0.818301933966445,1.),(1.,0.817226613172342,
1.),(1.,0.816179643373966,1.),(1.,0.815159387863652,1.)))
REPRESENTATION_ITEM('')
SURFACE()
);
#2612=(
BOUNDED_SURFACE()
B_SPLINE_SURFACE(3,2,((#388787,#388788,#388789),(#388790,#388791,#388792),
(#388793,#388794,#388795),(#388796,#388797,#388798)),.UNSPECIFIED.,.F.,
 .F.,.F.)
B_SPLINE_SURFACE_WITH_KNOTS((4,4),(3,3),(-1.54744435122073E-6,1.54744435122074E-5),
(-0.0151698983599587,1.),.UNSPECIFIED.)
GEOMETRIC_REPRESENTATION_ITEM()
RATIONAL_B_SPLINE_SURFACE(((1.02018382472664,0.334740937357953,1.),(1.00401234488767,
0.867753072813686,1.),(1.00033622856776,0.98891790308083,1.),(1.,1.,1.)))
REPRESENTATION_ITEM('')
SURFACE()
);
#2613=(
BOUNDED_SURFACE()
B_SPLINE_SURFACE(3,2,((#388800,#388801,#388802),(#388803,#388804,#388805),
(#388806,#388807,#388808),(#388809,#388810,#388811)),.UNSPECIFIED.,.F.,
 .F.,.F.)
B_SPLINE_SURFACE_WITH_KNOTS((4,4),(3,3),(0.00137194782501028,0.00149814269699235),
(0.,1.),.UNSPECIFIED.)
GEOMETRIC_REPRESENTATION_ITEM()
RATIONAL_B_SPLINE_SURFACE(((1.,0.815158509402319,1.),(1.,0.81617904414817,
1.),(1.,0.817226308119905,1.),(1.,0.818301939488816,1.)))
REPRESENTATION_ITEM('')
SURFACE()
);
#2614=(
BOUNDED_SURFACE()
B_SPLINE_SURFACE(3,2,((#388855,#388856,#388857),(#388858,#388859,#388860),
(#388861,#388862,#388863),(#388864,#388865,#388866)),.UNSPECIFIED.,.F.,
 .F.,.F.)
B_SPLINE_SURFACE_WITH_KNOTS((4,4),(3,3),(1.55009486301137E-5,4.92065510474434E-5),
(-8.1375951256704E-5,1.),.UNSPECIFIED.)
GEOMETRIC_REPRESENTATION_ITEM()
RATIONAL_B_SPLINE_SURFACE(((1.00002372912329,0.854200639599719,1.),(1.0000142358599,
0.912530301180564,1.),(1.00000710550469,0.956341495377436,1.),(1.00001238975905,
0.923873338137045,1.)))
REPRESENTATION_ITEM('')
SURFACE()
);
#2615=(
BOUNDED_SURFACE()
B_SPLINE_SURFACE(3,2,((#388870,#388871,#388872),(#388873,#388874,#388875),
(#388876,#388877,#388878),(#388879,#388880,#388881)),.UNSPECIFIED.,.F.,
 .F.,.F.)
B_SPLINE_SURFACE_WITH_KNOTS((4,4),(3,3),(-3.39934179457825E-6,3.73927597403566E-5),
(-0.00186004067440102,1.00069373317436),.UNSPECIFIED.)
GEOMETRIC_REPRESENTATION_ITEM()
RATIONAL_B_SPLINE_SURFACE(((1.00072100136063,0.806051963875328,1.0002685964269),
(1.00060048440161,0.838470803558596,1.00022369994495),(1.00053106448801,
0.857144632272367,1.00019783877219),(1.00054515072859,0.853355459539074,
1.00020308635436)))
REPRESENTATION_ITEM('')
SURFACE()
);
#2616=(
BOUNDED_SURFACE()
B_SPLINE_SURFACE(3,2,((#388883,#388884,#388885),(#388886,#388887,#388888),
(#388889,#388890,#388891),(#388892,#388893,#388894)),.UNSPECIFIED.,.F.,
 .F.,.F.)
B_SPLINE_SURFACE_WITH_KNOTS((4,4),(3,3),(3.79470760369927E-19,9.54361881492177E-5),
(0.,1.),.UNSPECIFIED.)
GEOMETRIC_REPRESENTATION_ITEM()
RATIONAL_B_SPLINE_SURFACE(((1.,0.816715621142054,1.),(1.,0.815907587407937,
1.),(1.,0.81511595934522,1.),(1.,0.814339887349198,1.)))
REPRESENTATION_ITEM('')
SURFACE()
);
#2617=(
BOUNDED_SURFACE()
B_SPLINE_SURFACE(3,2,((#388896,#388897,#388898),(#388899,#388900,#388901),
(#388902,#388903,#388904),(#388905,#388906,#388907)),.UNSPECIFIED.,.F.,
 .F.,.F.)
B_SPLINE_SURFACE_WITH_KNOTS((4,4),(3,3),(1.05032085459533E-19,4.68197758448214E-5),
(0.,1.),.UNSPECIFIED.)
GEOMETRIC_REPRESENTATION_ITEM()
RATIONAL_B_SPLINE_SURFACE(((1.,0.816715621142049,1.),(1.,0.953638980025221,
1.),(1.,0.954506925408039,1.),(1.,0.816715621142054,1.)))
REPRESENTATION_ITEM('')
SURFACE()
);
#2618=(
BOUNDED_SURFACE()
B_SPLINE_SURFACE(3,2,((#388909,#388910,#388911),(#388912,#388913,#388914),
(#388915,#388916,#388917),(#388918,#388919,#388920)),.UNSPECIFIED.,.F.,
 .F.,.F.)
B_SPLINE_SURFACE_WITH_KNOTS((4,4),(3,3),(-5.42101086242752E-20,9.54361881492178E-5),
(0.,1.),.UNSPECIFIED.)
GEOMETRIC_REPRESENTATION_ITEM()
RATIONAL_B_SPLINE_SURFACE(((1.,0.814339887349192,1.),(1.,0.815115959345194,
1.),(1.,0.815907587407953,1.),(1.,0.816715621142049,1.)))
REPRESENTATION_ITEM('')
SURFACE()
);
#2619=(
BOUNDED_SURFACE()
B_SPLINE_SURFACE(3,2,((#388922,#388923,#388924),(#388925,#388926,#388927),
(#388928,#388929,#388930),(#388931,#388932,#388933)),.UNSPECIFIED.,.F.,
 .F.,.F.)
B_SPLINE_SURFACE_WITH_KNOTS((4,4),(3,3),(-3.39528393502487E-6,3.73481232852734E-5),
(-0.00165018033251935,1.),.UNSPECIFIED.)
GEOMETRIC_REPRESENTATION_ITEM()
RATIONAL_B_SPLINE_SURFACE(((1.00048354385543,0.85348757166049,1.),(1.00047110510899,
0.857256476851603,1.),(1.00053193201083,0.83882609665598,1.),(1.00063970687696,
0.806170615310246,1.)))
REPRESENTATION_ITEM('')
SURFACE()
);
#2620=(
BOUNDED_SURFACE()
B_SPLINE_SURFACE(3,2,((#388937,#388938,#388939),(#388940,#388941,#388942),
(#388943,#388944,#388945),(#388946,#388947,#388948)),.UNSPECIFIED.,.F.,
 .F.,.F.)
B_SPLINE_SURFACE_WITH_KNOTS((4,4),(3,3),(2.02993869230509E-5,5.39756952686905E-5),
(-0.000116281069650204,1.),.UNSPECIFIED.)
GEOMETRIC_REPRESENTATION_ITEM()
RATIONAL_B_SPLINE_SURFACE(((1.00001770479726,0.923870681143031,1.),(1.00001014104057,
0.956394275543426,1.),(1.00002037300274,0.912397594905714,1.),(1.00003390859461,
0.854195550869881,1.)))
REPRESENTATION_ITEM('')
SURFACE()
);
#2621=(
BOUNDED_SURFACE()
B_SPLINE_SURFACE(3,2,((#389041,#389042,#389043),(#389044,#389045,#389046),
(#389047,#389048,#389049),(#389050,#389051,#389052)),.UNSPECIFIED.,.F.,
 .F.,.F.)
B_SPLINE_SURFACE_WITH_KNOTS((4,4),(3,3),(0.00135801595889393,0.00148409170619832),
(0.,1.),.UNSPECIFIED.)
GEOMETRIC_REPRESENTATION_ITEM()
RATIONAL_B_SPLINE_SURFACE(((1.,0.818301933966442,1.),(1.,0.817226613172343,
1.),(1.,0.816179643373952,1.),(1.,0.815159387863653,1.)))
REPRESENTATION_ITEM('')
SURFACE()
);
#2622=(
BOUNDED_SURFACE()
B_SPLINE_SURFACE(3,2,((#389091,#389092,#389093),(#389094,#389095,#389096),
(#389097,#389098,#389099),(#389100,#389101,#389102)),.UNSPECIFIED.,.F.,
 .F.,.F.)
B_SPLINE_SURFACE_WITH_KNOTS((4,4),(3,3),(-1.54744435122082E-6,1.5474443512208E-5),
(-0.0151698983619477,1.),.UNSPECIFIED.)
GEOMETRIC_REPRESENTATION_ITEM()
RATIONAL_B_SPLINE_SURFACE(((1.02018382472933,0.334740937356649,1.),(1.0040123448882,
0.867753072813339,1.),(1.0003362285678,0.988917903080829,1.),(1.,1.,1.)))
REPRESENTATION_ITEM('')
SURFACE()
);
#2623=(
BOUNDED_SURFACE()
B_SPLINE_SURFACE(3,2,((#389104,#389105,#389106),(#389107,#389108,#389109),
(#389110,#389111,#389112),(#389113,#389114,#389115)),.UNSPECIFIED.,.F.,
 .F.,.F.)
B_SPLINE_SURFACE_WITH_KNOTS((4,4),(3,3),(0.00137194782501028,0.00149814269699235),
(0.,1.),.UNSPECIFIED.)
GEOMETRIC_REPRESENTATION_ITEM()
RATIONAL_B_SPLINE_SURFACE(((1.,0.815158509402328,1.),(1.,0.816179044148159,
1.),(1.,0.81722630811993,1.),(1.,0.818301939488807,1.)))
REPRESENTATION_ITEM('')
SURFACE()
);
#2624=(
BOUNDED_SURFACE()
B_SPLINE_SURFACE(3,2,((#389159,#389160,#389161),(#389162,#389163,#389164),
(#389165,#389166,#389167),(#389168,#389169,#389170)),.UNSPECIFIED.,.F.,
 .F.,.F.)
B_SPLINE_SURFACE_WITH_KNOTS((4,4),(3,3),(1.55009486301137E-5,4.9206551047443E-5),
(-8.13759515487E-5,1.),.UNSPECIFIED.)
GEOMETRIC_REPRESENTATION_ITEM()
RATIONAL_B_SPLINE_SURFACE(((1.00002372912338,0.854200639599678,1.),(1.00001423585995,
0.912530301180521,1.),(1.00000710550471,0.956341495377438,1.),(1.00001238975909,
0.923873338137016,1.)))
REPRESENTATION_ITEM('')
SURFACE()
);
#2625=(
BOUNDED_SURFACE()
B_SPLINE_SURFACE(3,2,((#389174,#389175,#389176),(#389177,#389178,#389179),
(#389180,#389181,#389182),(#389183,#389184,#389185)),.UNSPECIFIED.,.F.,
 .F.,.F.)
B_SPLINE_SURFACE_WITH_KNOTS((4,4),(3,3),(-3.39934179457848E-6,3.73927597403565E-5),
(-0.00186004067432748,1.00069373317439),.UNSPECIFIED.)
GEOMETRIC_REPRESENTATION_ITEM()
RATIONAL_B_SPLINE_SURFACE(((1.0007210013606,0.806051963875316,1.00026859642691),
(1.00060048440158,0.838470803558609,1.00022369994495),(1.00053106448799,
0.857144632272371,1.00019783877219),(1.00054515072856,0.85335545953907,
1.00020308635437)))
REPRESENTATION_ITEM('')
SURFACE()
);
#2626=(
BOUNDED_SURFACE()
B_SPLINE_SURFACE(3,2,((#389187,#389188,#389189),(#389190,#389191,#389192),
(#389193,#389194,#389195),(#389196,#389197,#389198)),.UNSPECIFIED.,.F.,
 .F.,.F.)
B_SPLINE_SURFACE_WITH_KNOTS((4,4),(3,3),(-1.62630325872826E-19,9.5436188149217E-5),
(0.,1.),.UNSPECIFIED.)
GEOMETRIC_REPRESENTATION_ITEM()
RATIONAL_B_SPLINE_SURFACE(((1.,0.816715621142048,1.),(1.,0.815907587407941,
1.),(1.,0.815115959345207,1.),(1.,0.814339887349185,1.)))
REPRESENTATION_ITEM('')
SURFACE()
);
#2627=(
BOUNDED_SURFACE()
B_SPLINE_SURFACE(3,2,((#389200,#389201,#389202),(#389203,#389204,#389205),
(#389206,#389207,#389208),(#389209,#389210,#389211)),.UNSPECIFIED.,.F.,
 .F.,.F.)
B_SPLINE_SURFACE_WITH_KNOTS((4,4),(3,3),(-1.60936259978317E-19,4.68197758448207E-5),
(0.,1.),.UNSPECIFIED.)
GEOMETRIC_REPRESENTATION_ITEM()
RATIONAL_B_SPLINE_SURFACE(((1.,0.816715621142048,1.),(1.,0.953638980025212,
1.),(1.,0.954506925408048,1.),(1.,0.816715621142053,1.)))
REPRESENTATION_ITEM('')
SURFACE()
);
#2628=(
BOUNDED_SURFACE()
B_SPLINE_SURFACE(3,2,((#389213,#389214,#389215),(#389216,#389217,#389218),
(#389219,#389220,#389221),(#389222,#389223,#389224)),.UNSPECIFIED.,.F.,
 .F.,.F.)
B_SPLINE_SURFACE_WITH_KNOTS((4,4),(3,3),(5.42101086242752E-20,9.54361881492175E-5),
(0.,1.),.UNSPECIFIED.)
GEOMETRIC_REPRESENTATION_ITEM()
RATIONAL_B_SPLINE_SURFACE(((1.,0.814339887349189,1.),(1.,0.815115959345207,
1.),(1.,0.815907587407939,1.),(1.,0.816715621142047,1.)))
REPRESENTATION_ITEM('')
SURFACE()
);
#2629=(
BOUNDED_SURFACE()
B_SPLINE_SURFACE(3,2,((#389226,#389227,#389228),(#389229,#389230,#389231),
(#389232,#389233,#389234),(#389235,#389236,#389237)),.UNSPECIFIED.,.F.,
 .F.,.F.)
B_SPLINE_SURFACE_WITH_KNOTS((4,4),(3,3),(-3.39528393502488E-6,3.73481232852735E-5),
(-0.00165018033272199,1.),.UNSPECIFIED.)
GEOMETRIC_REPRESENTATION_ITEM()
RATIONAL_B_SPLINE_SURFACE(((1.00048354385549,0.853487571660471,1.),(1.00047110510905,
0.85725647685156,1.),(1.00053193201089,0.838826096655951,1.),(1.00063970687704,
0.806170615310205,1.)))
REPRESENTATION_ITEM('')
SURFACE()
);
#2630=(
BOUNDED_SURFACE()
B_SPLINE_SURFACE(3,2,((#389241,#389242,#389243),(#389244,#389245,#389246),
(#389247,#389248,#389249),(#389250,#389251,#389252)),.UNSPECIFIED.,.F.,
 .F.,.F.)
B_SPLINE_SURFACE_WITH_KNOTS((4,4),(3,3),(2.0299386923051E-5,5.39756952686902E-5),
(-0.00011628106966309,1.),.UNSPECIFIED.)
GEOMETRIC_REPRESENTATION_ITEM()
RATIONAL_B_SPLINE_SURFACE(((1.00001770479726,0.92387068114303,1.),(1.00001014104057,
0.956394275543435,1.),(1.00002037300274,0.912397594905691,1.),(1.00003390859461,
0.8541955508699,1.)))
REPRESENTATION_ITEM('')
SURFACE()
);
#2631=(
BOUNDED_SURFACE()
B_SPLINE_SURFACE(3,2,((#389345,#389346,#389347),(#389348,#389349,#389350),
(#389351,#389352,#389353),(#389354,#389355,#389356)),.UNSPECIFIED.,.F.,
 .F.,.F.)
B_SPLINE_SURFACE_WITH_KNOTS((4,4),(3,3),(0.00135801595889393,0.00148409170619832),
(0.,1.),.UNSPECIFIED.)
GEOMETRIC_REPRESENTATION_ITEM()
RATIONAL_B_SPLINE_SURFACE(((1.,0.818301933966445,1.),(1.,0.817226613172347,
1.),(1.,0.816179643373956,1.),(1.,0.815159387863658,1.)))
REPRESENTATION_ITEM('')
SURFACE()
);
#2632=(
BOUNDED_SURFACE()
B_SPLINE_SURFACE(3,2,((#389395,#389396,#389397),(#389398,#389399,#389400),
(#389401,#389402,#389403),(#389404,#389405,#389406)),.UNSPECIFIED.,.F.,
 .F.,.F.)
B_SPLINE_SURFACE_WITH_KNOTS((4,4),(3,3),(-1.54744435122081E-6,1.54744435122075E-5),
(-0.0151698983637362,1.),.UNSPECIFIED.)
GEOMETRIC_REPRESENTATION_ITEM()
RATIONAL_B_SPLINE_SURFACE(((1.02018382473174,0.334740937355544,1.),(1.00401234488868,
0.86775307281305,1.),(1.00033622856784,0.988917903080849,1.),(1.,1.,1.)))
REPRESENTATION_ITEM('')
SURFACE()
);
#2633=(
BOUNDED_SURFACE()
B_SPLINE_SURFACE(3,2,((#389408,#389409,#389410),(#389411,#389412,#389413),
(#389414,#389415,#389416),(#389417,#389418,#389419)),.UNSPECIFIED.,.F.,
 .F.,.F.)
B_SPLINE_SURFACE_WITH_KNOTS((4,4),(3,3),(0.00137194782501028,0.00149814269699235),
(0.,1.),.UNSPECIFIED.)
GEOMETRIC_REPRESENTATION_ITEM()
RATIONAL_B_SPLINE_SURFACE(((1.,0.815158509402313,1.),(1.,0.816179044148172,
1.),(1.,0.817226308119923,1.),(1.,0.818301939488807,1.)))
REPRESENTATION_ITEM('')
SURFACE()
);
#2634=(
BOUNDED_SURFACE()
B_SPLINE_SURFACE(3,2,((#389463,#389464,#389465),(#389466,#389467,#389468),
(#389469,#389470,#389471),(#389472,#389473,#389474)),.UNSPECIFIED.,.F.,
 .F.,.F.)
B_SPLINE_SURFACE_WITH_KNOTS((4,4),(3,3),(1.55009486301137E-5,4.9206551047443E-5),
(-8.13759514700875E-5,1.),.UNSPECIFIED.)
GEOMETRIC_REPRESENTATION_ITEM()
RATIONAL_B_SPLINE_SURFACE(((1.00002372912335,0.854200639599689,1.),(1.00001423585993,
0.912530301180527,1.),(1.00000710550471,0.956341495377435,1.),(1.00001238975908,
0.923873338137022,1.)))
REPRESENTATION_ITEM('')
SURFACE()
);
#2635=(
BOUNDED_SURFACE()
B_SPLINE_SURFACE(3,2,((#389478,#389479,#389480),(#389481,#389482,#389483),
(#389484,#389485,#389486),(#389487,#389488,#389489)),.UNSPECIFIED.,.F.,
 .F.,.F.)
B_SPLINE_SURFACE_WITH_KNOTS((4,4),(3,3),(-3.39934179457819E-6,3.73927597403566E-5),
(-0.00186004067485636,1.0006937331747),.UNSPECIFIED.)
GEOMETRIC_REPRESENTATION_ITEM()
RATIONAL_B_SPLINE_SURFACE(((1.00072100136081,0.806051963875156,1.00026859642703),
(1.00060048440176,0.838470803558486,1.00022369994506),(1.00053106448814,
0.857144632272242,1.00019783877228),(1.00054515072872,0.853355459538962,
1.00020308635446)))
REPRESENTATION_ITEM('')
SURFACE()
);
#2636=(
BOUNDED_SURFACE()
B_SPLINE_SURFACE(3,2,((#389491,#389492,#389493),(#389494,#389495,#389496),
(#389497,#389498,#389499),(#389500,#389501,#389502)),.UNSPECIFIED.,.F.,
 .F.,.F.)
B_SPLINE_SURFACE_WITH_KNOTS((4,4),(3,3),(-5.42101086242752E-20,9.54361881492174E-5),
(0.,1.),.UNSPECIFIED.)
GEOMETRIC_REPRESENTATION_ITEM()
RATIONAL_B_SPLINE_SURFACE(((1.,0.816715621142055,1.),(1.,0.815907587407937,
1.),(1.,0.815115959345214,1.),(1.,0.814339887349196,1.)))
REPRESENTATION_ITEM('')
SURFACE()
);
#2637=(
BOUNDED_SURFACE()
B_SPLINE_SURFACE(3,2,((#389504,#389505,#389506),(#389507,#389508,#389509),
(#389510,#389511,#389512),(#389513,#389514,#389515)),.UNSPECIFIED.,.F.,
 .F.,.F.)
B_SPLINE_SURFACE_WITH_KNOTS((4,4),(3,3),(7.96210970419042E-20,4.68197758448209E-5),
(0.,1.),.UNSPECIFIED.)
GEOMETRIC_REPRESENTATION_ITEM()
RATIONAL_B_SPLINE_SURFACE(((1.,0.816715621142049,1.),(1.,0.953638980025211,
1.),(1.,0.954506925408045,1.),(1.,0.816715621142055,1.)))
REPRESENTATION_ITEM('')
SURFACE()
);
#2638=(
BOUNDED_SURFACE()
B_SPLINE_SURFACE(3,2,((#389517,#389518,#389519),(#389520,#389521,#389522),
(#389523,#389524,#389525),(#389526,#389527,#389528)),.UNSPECIFIED.,.F.,
 .F.,.F.)
B_SPLINE_SURFACE_WITH_KNOTS((4,4),(3,3),(1.62630325872826E-19,9.54361881492178E-5),
(0.,1.),.UNSPECIFIED.)
GEOMETRIC_REPRESENTATION_ITEM()
RATIONAL_B_SPLINE_SURFACE(((1.,0.814339887349188,1.),(1.,0.815115959345215,
1.),(1.,0.815907587407936,1.),(1.,0.816715621142051,1.)))
REPRESENTATION_ITEM('')
SURFACE()
);
#2639=(
BOUNDED_SURFACE()
B_SPLINE_SURFACE(3,2,((#389530,#389531,#389532),(#389533,#389534,#389535),
(#389536,#389537,#389538),(#389539,#389540,#389541)),.UNSPECIFIED.,.F.,
 .F.,.F.)
B_SPLINE_SURFACE_WITH_KNOTS((4,4),(3,3),(-3.3952839350249E-6,3.73481232852728E-5),
(-0.00165018033345588,1.),.UNSPECIFIED.)
GEOMETRIC_REPRESENTATION_ITEM()
RATIONAL_B_SPLINE_SURFACE(((1.00048354385571,0.853487571660368,1.),(1.00047110510926,
0.857256476851443,1.),(1.00053193201113,0.838826096655833,1.),(1.00063970687732,
0.806170615310063,1.)))
REPRESENTATION_ITEM('')
SURFACE()
);
#2640=(
BOUNDED_SURFACE()
B_SPLINE_SURFACE(3,2,((#389545,#389546,#389547),(#389548,#389549,#389550),
(#389551,#389552,#389553),(#389554,#389555,#389556)),.UNSPECIFIED.,.F.,
 .F.,.F.)
B_SPLINE_SURFACE_WITH_KNOTS((4,4),(3,3),(2.02993869230511E-5,5.39756952686902E-5),
(-0.000116281069626685,1.),.UNSPECIFIED.)
GEOMETRIC_REPRESENTATION_ITEM()
RATIONAL_B_SPLINE_SURFACE(((1.00001770479725,0.923870681143031,1.),(1.00001014104056,
0.956394275543432,1.),(1.00002037300273,0.9123975949057,1.),(1.0000339085946,
0.854195550869898,1.)))
REPRESENTATION_ITEM('')
SURFACE()
);
#2641=(
BOUNDED_SURFACE()
B_SPLINE_SURFACE(3,2,((#389649,#389650,#389651),(#389652,#389653,#389654),
(#389655,#389656,#389657),(#389658,#389659,#389660)),.UNSPECIFIED.,.F.,
 .F.,.F.)
B_SPLINE_SURFACE_WITH_KNOTS((4,4),(3,3),(0.00135801595889393,0.00148409170619832),
(0.,1.),.UNSPECIFIED.)
GEOMETRIC_REPRESENTATION_ITEM()
RATIONAL_B_SPLINE_SURFACE(((1.,0.818301933966445,1.),(1.,0.817226613172353,
1.),(1.,0.81617964337395,1.),(1.,0.815159387863655,1.)))
REPRESENTATION_ITEM('')
SURFACE()
);
#2642=(
BOUNDED_SURFACE()
B_SPLINE_SURFACE(3,2,((#389699,#389700,#389701),(#389702,#389703,#389704),
(#389705,#389706,#389707),(#389708,#389709,#389710)),.UNSPECIFIED.,.F.,
 .F.,.F.)
B_SPLINE_SURFACE_WITH_KNOTS((4,4),(3,3),(-1.54744435122017E-6,1.54744435122086E-5),
(0.,1.01516989835332),.UNSPECIFIED.)
GEOMETRIC_REPRESENTATION_ITEM()
RATIONAL_B_SPLINE_SURFACE(((1.,0.33474093736242,1.02018382471767),(1.,0.867753072814264,
1.00401234488589),(1.,0.988917903081015,1.00033622856761),(1.,1.,1.)))
REPRESENTATION_ITEM('')
SURFACE()
);
#2643=(
BOUNDED_SURFACE()
B_SPLINE_SURFACE(3,2,((#389712,#389713,#389714),(#389715,#389716,#389717),
(#389718,#389719,#389720),(#389721,#389722,#389723)),.UNSPECIFIED.,.F.,
 .F.,.F.)
B_SPLINE_SURFACE_WITH_KNOTS((4,4),(3,3),(0.00137194782501028,0.00149814269699235),
(0.,1.),.UNSPECIFIED.)
GEOMETRIC_REPRESENTATION_ITEM()
RATIONAL_B_SPLINE_SURFACE(((1.,0.815158509402318,1.),(1.,0.816179044148163,
1.),(1.,0.817226308119936,1.),(1.,0.818301939488807,1.)))
REPRESENTATION_ITEM('')
SURFACE()
);
#2644=(
BOUNDED_SURFACE()
B_SPLINE_SURFACE(3,2,((#389767,#389768,#389769),(#389770,#389771,#389772),
(#389773,#389774,#389775),(#389776,#389777,#389778)),.UNSPECIFIED.,.F.,
 .F.,.F.)
B_SPLINE_SURFACE_WITH_KNOTS((4,4),(3,3),(1.55009486301137E-5,4.92065510474438E-5),
(-8.13759517499485E-5,1.),.UNSPECIFIED.)
GEOMETRIC_REPRESENTATION_ITEM()
RATIONAL_B_SPLINE_SURFACE(((1.00002372912343,0.854200639599646,1.),(1.00001423585998,
0.912530301180521,1.),(1.00000710550473,0.956341495377413,1.),(1.00001238975913,
0.923873338137004,1.)))
REPRESENTATION_ITEM('')
SURFACE()
);
#2645=(
BOUNDED_SURFACE()
B_SPLINE_SURFACE(3,2,((#389782,#389783,#389784),(#389785,#389786,#389787),
(#389788,#389789,#389790),(#389791,#389792,#389793)),.UNSPECIFIED.,.F.,
 .F.,.F.)
B_SPLINE_SURFACE_WITH_KNOTS((4,4),(3,3),(-3.39934179457862E-6,3.73927597403562E-5),
(-0.00186004067474084,1.00069373317454),.UNSPECIFIED.)
GEOMETRIC_REPRESENTATION_ITEM()
RATIONAL_B_SPLINE_SURFACE(((1.00072100136076,0.806051963875226,1.00026859642696),
(1.00060048440172,0.838470803558517,1.000223699945),(1.00053106448811,0.85714463227229,
1.00019783877223),(1.00054515072869,0.853355459538998,1.00020308635441)))
REPRESENTATION_ITEM('')
SURFACE()
);
#2646=(
BOUNDED_SURFACE()
B_SPLINE_SURFACE(3,2,((#389795,#389796,#389797),(#389798,#389799,#389800),
(#389801,#389802,#389803),(#389804,#389805,#389806)),.UNSPECIFIED.,.F.,
 .F.,.F.)
B_SPLINE_SURFACE_WITH_KNOTS((4,4),(3,3),(-1.0842021724855E-19,9.54361881492172E-5),
(0.,1.),.UNSPECIFIED.)
GEOMETRIC_REPRESENTATION_ITEM()
RATIONAL_B_SPLINE_SURFACE(((1.,0.816715621142051,1.),(1.,0.815907587407944,
1.),(1.,0.815115959345209,1.),(1.,0.814339887349197,1.)))
REPRESENTATION_ITEM('')
SURFACE()
);
#2647=(
BOUNDED_SURFACE()
B_SPLINE_SURFACE(3,2,((#389808,#389809,#389810),(#389811,#389812,#389813),
(#389814,#389815,#389816),(#389817,#389818,#389819)),.UNSPECIFIED.,.F.,
 .F.,.F.)
B_SPLINE_SURFACE_WITH_KNOTS((4,4),(3,3),(-1.96511643762998E-19,4.68197758448206E-5),
(0.,1.),.UNSPECIFIED.)
GEOMETRIC_REPRESENTATION_ITEM()
RATIONAL_B_SPLINE_SURFACE(((1.,0.816715621142045,1.),(1.,0.953638980025211,
1.),(1.,0.954506925408055,1.),(1.,0.816715621142051,1.)))
REPRESENTATION_ITEM('')
SURFACE()
);
#2648=(
BOUNDED_SURFACE()
B_SPLINE_SURFACE(3,2,((#389821,#389822,#389823),(#389824,#389825,#389826),
(#389827,#389828,#389829),(#389830,#389831,#389832)),.UNSPECIFIED.,.F.,
 .F.,.F.)
B_SPLINE_SURFACE_WITH_KNOTS((4,4),(3,3),(0.,9.54361881492177E-5),(0.,1.),
 .UNSPECIFIED.)
GEOMETRIC_REPRESENTATION_ITEM()
RATIONAL_B_SPLINE_SURFACE(((1.,0.814339887349196,1.),(1.,0.815115959345193,
1.),(1.,0.815907587407952,1.),(1.,0.816715621142047,1.)))
REPRESENTATION_ITEM('')
SURFACE()
);
#2649=(
BOUNDED_SURFACE()
B_SPLINE_SURFACE(3,2,((#389834,#389835,#389836),(#389837,#389838,#389839),
(#389840,#389841,#389842),(#389843,#389844,#389845)),.UNSPECIFIED.,.F.,
 .F.,.F.)
B_SPLINE_SURFACE_WITH_KNOTS((4,4),(3,3),(-3.39528393502488E-6,3.73481232852735E-5),
(-0.00165018033331416,1.),.UNSPECIFIED.)
GEOMETRIC_REPRESENTATION_ITEM()
RATIONAL_B_SPLINE_SURFACE(((1.00048354385566,0.853487571660399,1.),(1.00047110510922,
0.857256476851447,1.),(1.00053193201108,0.838826096655879,1.),(1.00063970687727,
0.806170615310081,1.)))
REPRESENTATION_ITEM('')
SURFACE()
);
#2650=(
BOUNDED_SURFACE()
B_SPLINE_SURFACE(3,2,((#389849,#389850,#389851),(#389852,#389853,#389854),
(#389855,#389856,#389857),(#389858,#389859,#389860)),.UNSPECIFIED.,.F.,
 .F.,.F.)
B_SPLINE_SURFACE_WITH_KNOTS((4,4),(3,3),(2.02993869230507E-5,5.39756952686892E-5),
(-0.000116281069916757,1.),.UNSPECIFIED.)
GEOMETRIC_REPRESENTATION_ITEM()
RATIONAL_B_SPLINE_SURFACE(((1.0000177047973,0.92387068114301,1.),(1.00001014104059,
0.956394275543412,1.),(1.00002037300278,0.912397594905679,1.),(1.00003390859469,
0.854195550869856,1.)))
REPRESENTATION_ITEM('')
SURFACE()
);
#2651=(
BOUNDED_SURFACE()
B_SPLINE_SURFACE(3,2,((#389953,#389954,#389955),(#389956,#389957,#389958),
(#389959,#389960,#389961),(#389962,#389963,#389964)),.UNSPECIFIED.,.F.,
 .F.,.F.)
B_SPLINE_SURFACE_WITH_KNOTS((4,4),(3,3),(0.00135801595889393,0.00148409170619832),
(0.,1.),.UNSPECIFIED.)
GEOMETRIC_REPRESENTATION_ITEM()
RATIONAL_B_SPLINE_SURFACE(((1.,0.818301933966448,1.),(1.,0.817226613172342,
1.),(1.,0.81617964337396,1.),(1.,0.81515938786366,1.)))
REPRESENTATION_ITEM('')
SURFACE()
);
#2652=(
BOUNDED_SURFACE()
B_SPLINE_SURFACE(3,2,((#390003,#390004,#390005),(#390006,#390007,#390008),
(#390009,#390010,#390011),(#390012,#390013,#390014)),.UNSPECIFIED.,.F.,
 .F.,.F.)
B_SPLINE_SURFACE_WITH_KNOTS((4,4),(3,3),(-1.54744435122075E-6,1.5474443512208E-5),
(-0.0151698983620152,1.),.UNSPECIFIED.)
GEOMETRIC_REPRESENTATION_ITEM()
RATIONAL_B_SPLINE_SURFACE(((1.02018382472942,0.334740937356621,1.),(1.00401234488822,
0.867753072813288,1.),(1.0003362285678,0.988917903080855,1.),(1.,1.,1.)))
REPRESENTATION_ITEM('')
SURFACE()
);
#2653=(
BOUNDED_SURFACE()
B_SPLINE_SURFACE(3,2,((#390016,#390017,#390018),(#390019,#390020,#390021),
(#390022,#390023,#390024),(#390025,#390026,#390027)),.UNSPECIFIED.,.F.,
 .F.,.F.)
B_SPLINE_SURFACE_WITH_KNOTS((4,4),(3,3),(0.00137194782501028,0.00149814269699235),
(0.,1.),.UNSPECIFIED.)
GEOMETRIC_REPRESENTATION_ITEM()
RATIONAL_B_SPLINE_SURFACE(((1.,0.815158509402316,1.),(1.,0.81617904414816,
1.),(1.,0.817226308119934,1.),(1.,0.818301939488799,1.)))
REPRESENTATION_ITEM('')
SURFACE()
);
#2654=(
BOUNDED_SURFACE()
B_SPLINE_SURFACE(3,2,((#390071,#390072,#390073),(#390074,#390075,#390076),
(#390077,#390078,#390079),(#390080,#390081,#390082)),.UNSPECIFIED.,.F.,
 .F.,.F.)
B_SPLINE_SURFACE_WITH_KNOTS((4,4),(3,3),(1.55009486301137E-5,4.92065510474438E-5),
(-8.13759515447854E-5,1.),.UNSPECIFIED.)
GEOMETRIC_REPRESENTATION_ITEM()
RATIONAL_B_SPLINE_SURFACE(((1.00002372912337,0.854200639599677,1.),(1.00001423585995,
0.912530301180528,1.),(1.00000710550471,0.956341495377429,1.),(1.00001238975909,
0.923873338137019,1.)))
REPRESENTATION_ITEM('')
SURFACE()
);
#2655=(
BOUNDED_SURFACE()
B_SPLINE_SURFACE(3,2,((#390086,#390087,#390088),(#390089,#390090,#390091),
(#390092,#390093,#390094),(#390095,#390096,#390097)),.UNSPECIFIED.,.F.,
 .F.,.F.)
B_SPLINE_SURFACE_WITH_KNOTS((4,4),(3,3),(-3.39934179457828E-6,3.73927597403566E-5),
(-0.00186004067387787,1.00069373317419),.UNSPECIFIED.)
GEOMETRIC_REPRESENTATION_ITEM()
RATIONAL_B_SPLINE_SURFACE(((1.00072100136043,0.806051963875447,1.00026859642683),
(1.00060048440144,0.838470803558726,1.00022369994489),(1.00053106448786,
0.857144632272452,1.00019783877214),(1.00054515072843,0.853355459539179,
1.00020308635431)))
REPRESENTATION_ITEM('')
SURFACE()
);
#2656=(
BOUNDED_SURFACE()
B_SPLINE_SURFACE(3,2,((#390099,#390100,#390101),(#390102,#390103,#390104),
(#390105,#390106,#390107),(#390108,#390109,#390110)),.UNSPECIFIED.,.F.,
 .F.,.F.)
B_SPLINE_SURFACE_WITH_KNOTS((4,4),(3,3),(-1.0842021724855E-19,9.54361881492174E-5),
(0.,1.),.UNSPECIFIED.)
GEOMETRIC_REPRESENTATION_ITEM()
RATIONAL_B_SPLINE_SURFACE(((1.,0.816715621142051,1.),(1.,0.815907587407947,
1.),(1.,0.815115959345208,1.),(1.,0.814339887349195,1.)))
REPRESENTATION_ITEM('')
SURFACE()
);
#2657=(
BOUNDED_SURFACE()
B_SPLINE_SURFACE(3,2,((#390112,#390113,#390114),(#390115,#390116,#390117),
(#390118,#390119,#390120),(#390121,#390122,#390123)),.UNSPECIFIED.,.F.,
 .F.,.F.)
B_SPLINE_SURFACE_WITH_KNOTS((4,4),(3,3),(-8.470329472543E-21,4.68197758448207E-5),
(0.,1.),.UNSPECIFIED.)
GEOMETRIC_REPRESENTATION_ITEM()
RATIONAL_B_SPLINE_SURFACE(((1.,0.816715621142051,1.),(1.,0.953638980025211,
1.),(1.,0.954506925408046,1.),(1.,0.816715621142051,1.)))
REPRESENTATION_ITEM('')
SURFACE()
);
#2658=(
BOUNDED_SURFACE()
B_SPLINE_SURFACE(3,2,((#390125,#390126,#390127),(#390128,#390129,#390130),
(#390131,#390132,#390133),(#390134,#390135,#390136)),.UNSPECIFIED.,.F.,
 .F.,.F.)
B_SPLINE_SURFACE_WITH_KNOTS((4,4),(3,3),(-5.42101086242752E-20,9.54361881492177E-5),
(0.,1.),.UNSPECIFIED.)
GEOMETRIC_REPRESENTATION_ITEM()
RATIONAL_B_SPLINE_SURFACE(((1.,0.814339887349193,1.),(1.,0.815115959345206,
1.),(1.,0.815907587407936,1.),(1.,0.816715621142051,1.)))
REPRESENTATION_ITEM('')
SURFACE()
);
#2659=(
BOUNDED_SURFACE()
B_SPLINE_SURFACE(3,2,((#390138,#390139,#390140),(#390141,#390142,#390143),
(#390144,#390145,#390146),(#390147,#390148,#390149)),.UNSPECIFIED.,.F.,
 .F.,.F.)
B_SPLINE_SURFACE_WITH_KNOTS((4,4),(3,3),(-3.39528393502381E-6,3.73481232852733E-5),
(-0.00165018033288198,1.),.UNSPECIFIED.)
GEOMETRIC_REPRESENTATION_ITEM()
RATIONAL_B_SPLINE_SURFACE(((1.00048354385554,0.853487571660452,1.),(1.00047110510909,
0.857256476851522,1.),(1.00053193201094,0.838826096655925,1.),(1.0006397068771,
0.806170615310169,1.)))
REPRESENTATION_ITEM('')
SURFACE()
);
#2660=(
BOUNDED_SURFACE()
B_SPLINE_SURFACE(3,2,((#390153,#390154,#390155),(#390156,#390157,#390158),
(#390159,#390160,#390161),(#390162,#390163,#390164)),.UNSPECIFIED.,.F.,
 .F.,.F.)
B_SPLINE_SURFACE_WITH_KNOTS((4,4),(3,3),(2.02993869230506E-5,5.39756952686901E-5),
(-0.000116281069653534,1.),.UNSPECIFIED.)
GEOMETRIC_REPRESENTATION_ITEM()
RATIONAL_B_SPLINE_SURFACE(((1.00001770479726,0.92387068114303,1.),(1.00001014104057,
0.956394275543427,1.),(1.00002037300274,0.912397594905703,1.),(1.00003390859461,
0.854195550869894,1.)))
REPRESENTATION_ITEM('')
SURFACE()
);
#2661=(
BOUNDED_SURFACE()
B_SPLINE_SURFACE(3,2,((#390257,#390258,#390259),(#390260,#390261,#390262),
(#390263,#390264,#390265),(#390266,#390267,#390268)),.UNSPECIFIED.,.F.,
 .F.,.F.)
B_SPLINE_SURFACE_WITH_KNOTS((4,4),(3,3),(0.00135801595889393,0.00148409170619832),
(0.,1.),.UNSPECIFIED.)
GEOMETRIC_REPRESENTATION_ITEM()
RATIONAL_B_SPLINE_SURFACE(((1.,0.818301933966444,1.),(1.,0.817226613172336,
1.),(1.,0.816179643373953,1.),(1.,0.815159387863656,1.)))
REPRESENTATION_ITEM('')
SURFACE()
);
#2662=(
BOUNDED_SURFACE()
B_SPLINE_SURFACE(3,2,((#390307,#390308,#390309),(#390310,#390311,#390312),
(#390313,#390314,#390315),(#390316,#390317,#390318)),.UNSPECIFIED.,.F.,
 .F.,.F.)
B_SPLINE_SURFACE_WITH_KNOTS((4,4),(3,3),(-1.54744435122082E-6,1.54744435122076E-5),
(-0.0151698983580317,1.),.UNSPECIFIED.)
GEOMETRIC_REPRESENTATION_ITEM()
RATIONAL_B_SPLINE_SURFACE(((1.02018382472404,0.334740937359278,1.),(1.00401234488715,
0.867753072813855,1.),(1.00033622856771,0.988917903080905,1.),(1.,1.,1.)))
REPRESENTATION_ITEM('')
SURFACE()
);
#2663=(
BOUNDED_SURFACE()
B_SPLINE_SURFACE(3,2,((#390320,#390321,#390322),(#390323,#390324,#390325),
(#390326,#390327,#390328),(#390329,#390330,#390331)),.UNSPECIFIED.,.F.,
 .F.,.F.)
B_SPLINE_SURFACE_WITH_KNOTS((4,4),(3,3),(0.00137194782501028,0.00149814269699235),
(0.,1.),.UNSPECIFIED.)
GEOMETRIC_REPRESENTATION_ITEM()
RATIONAL_B_SPLINE_SURFACE(((1.,0.815158509402318,1.),(1.,0.81617904414817,
1.),(1.,0.817226308119915,1.),(1.,0.818301939488809,1.)))
REPRESENTATION_ITEM('')
SURFACE()
);
#2664=(
BOUNDED_SURFACE()
B_SPLINE_SURFACE(3,2,((#390375,#390376,#390377),(#390378,#390379,#390380),
(#390381,#390382,#390383),(#390384,#390385,#390386)),.UNSPECIFIED.,.F.,
 .F.,.F.)
B_SPLINE_SURFACE_WITH_KNOTS((4,4),(3,3),(1.55009486301137E-5,4.92065510474432E-5),
(-8.13759517235604E-5,1.),.UNSPECIFIED.)
GEOMETRIC_REPRESENTATION_ITEM()
RATIONAL_B_SPLINE_SURFACE(((1.00002372912343,0.854200639599652,1.),(1.00001423585998,
0.912530301180515,1.),(1.00000710550473,0.956341495377416,1.),(1.00001238975912,
0.923873338137006,1.)))
REPRESENTATION_ITEM('')
SURFACE()
);
#2665=(
BOUNDED_SURFACE()
B_SPLINE_SURFACE(3,2,((#390390,#390391,#390392),(#390393,#390394,#390395),
(#390396,#390397,#390398),(#390399,#390400,#390401)),.UNSPECIFIED.,.F.,
 .F.,.F.)
B_SPLINE_SURFACE_WITH_KNOTS((4,4),(3,3),(-3.39934179457832E-6,3.73927597403565E-5),
(-0.00186004067364305,1.00069373317418),.UNSPECIFIED.)
GEOMETRIC_REPRESENTATION_ITEM()
RATIONAL_B_SPLINE_SURFACE(((1.00072100136033,0.806051963875482,1.00026859642682),
(1.00060048440136,0.838470803558797,1.00022369994489),(1.00053106448779,
0.857144632272455,1.00019783877213),(1.00054515072836,0.853355459539217,
1.0002030863543)))
REPRESENTATION_ITEM('')
SURFACE()
);
#2666=(
BOUNDED_SURFACE()
B_SPLINE_SURFACE(3,2,((#390403,#390404,#390405),(#390406,#390407,#390408),
(#390409,#390410,#390411),(#390412,#390413,#390414)),.UNSPECIFIED.,.F.,
 .F.,.F.)
B_SPLINE_SURFACE_WITH_KNOTS((4,4),(3,3),(-2.71050543121376E-19,9.54361881492173E-5),
(0.,1.),.UNSPECIFIED.)
GEOMETRIC_REPRESENTATION_ITEM()
RATIONAL_B_SPLINE_SURFACE(((1.,0.816715621142051,1.),(1.,0.815907587407946,
1.),(1.,0.815115959345203,1.),(1.,0.814339887349205,1.)))
REPRESENTATION_ITEM('')
SURFACE()
);
#2667=(
BOUNDED_SURFACE()
B_SPLINE_SURFACE(3,2,((#390416,#390417,#390418),(#390419,#390420,#390421),
(#390422,#390423,#390424),(#390425,#390426,#390427)),.UNSPECIFIED.,.F.,
 .F.,.F.)
B_SPLINE_SURFACE_WITH_KNOTS((4,4),(3,3),(-7.28448334638698E-20,4.68197758448207E-5),
(0.,1.),.UNSPECIFIED.)
GEOMETRIC_REPRESENTATION_ITEM()
RATIONAL_B_SPLINE_SURFACE(((1.,0.81671562114205,1.),(1.,0.953638980025219,
1.),(1.,0.954506925408033,1.),(1.,0.816715621142067,1.)))
REPRESENTATION_ITEM('')
SURFACE()
);
#2668=(
BOUNDED_SURFACE()
B_SPLINE_SURFACE(3,2,((#390429,#390430,#390431),(#390432,#390433,#390434),
(#390435,#390436,#390437),(#390438,#390439,#390440)),.UNSPECIFIED.,.F.,
 .F.,.F.)
B_SPLINE_SURFACE_WITH_KNOTS((4,4),(3,3),(5.42101086242752E-20,9.54361881492178E-5),
(0.,1.),.UNSPECIFIED.)
GEOMETRIC_REPRESENTATION_ITEM()
RATIONAL_B_SPLINE_SURFACE(((1.,0.814339887349195,1.),(1.,0.815115959345213,
1.),(1.,0.815907587407941,1.),(1.,0.81671562114205,1.)))
REPRESENTATION_ITEM('')
SURFACE()
);
#2669=(
BOUNDED_SURFACE()
B_SPLINE_SURFACE(3,2,((#390442,#390443,#390444),(#390445,#390446,#390447),
(#390448,#390449,#390450),(#390451,#390452,#390453)),.UNSPECIFIED.,.F.,
 .F.,.F.)
B_SPLINE_SURFACE_WITH_KNOTS((4,4),(3,3),(-3.39528393502482E-6,3.73481232852735E-5),
(-0.00165018033334558,1.),.UNSPECIFIED.)
GEOMETRIC_REPRESENTATION_ITEM()
RATIONAL_B_SPLINE_SURFACE(((1.00048354385567,0.853487571660392,1.),(1.00047110510922,
0.857256476851449,1.),(1.00053193201109,0.838826096655861,1.),(1.00063970687728,
0.806170615310092,0.999999999999999)))
REPRESENTATION_ITEM('')
SURFACE()
);
#2670=(
BOUNDED_SURFACE()
B_SPLINE_SURFACE(3,2,((#390457,#390458,#390459),(#390460,#390461,#390462),
(#390463,#390464,#390465),(#390466,#390467,#390468)),.UNSPECIFIED.,.F.,
 .F.,.F.)
B_SPLINE_SURFACE_WITH_KNOTS((4,4),(3,3),(2.02993869230509E-5,5.39756952687131E-5),
(-0.000116281069912844,1.),.UNSPECIFIED.)
GEOMETRIC_REPRESENTATION_ITEM()
RATIONAL_B_SPLINE_SURFACE(((1.0000177047973,0.923870681143008,1.),(1.00001014104059,
0.956394275543449,1.),(1.00002037300278,0.912397594905614,1.),(1.00003390859469,
0.854195550869742,1.)))
REPRESENTATION_ITEM('')
SURFACE()
);
#2671=(
BOUNDED_SURFACE()
B_SPLINE_SURFACE(3,2,((#390561,#390562,#390563),(#390564,#390565,#390566),
(#390567,#390568,#390569),(#390570,#390571,#390572)),.UNSPECIFIED.,.F.,
 .F.,.F.)
B_SPLINE_SURFACE_WITH_KNOTS((4,4),(3,3),(0.00135801595889393,0.00148409170619832),
(0.,1.),.UNSPECIFIED.)
GEOMETRIC_REPRESENTATION_ITEM()
RATIONAL_B_SPLINE_SURFACE(((1.,0.818301933966435,1.),(1.,0.817226613172361,
1.),(1.,0.816179643373941,1.),(1.,0.815159387863655,1.)))
REPRESENTATION_ITEM('')
SURFACE()
);
#2672=(
BOUNDED_SURFACE()
B_SPLINE_SURFACE(3,2,((#390611,#390612,#390613),(#390614,#390615,#390616),
(#390617,#390618,#390619),(#390620,#390621,#390622)),.UNSPECIFIED.,.F.,
 .F.,.F.)
B_SPLINE_SURFACE_WITH_KNOTS((4,4),(3,3),(-1.547444351221E-6,1.547444351221E-5),
(-0.0151698983664584,1.),.UNSPECIFIED.)
GEOMETRIC_REPRESENTATION_ITEM()
RATIONAL_B_SPLINE_SURFACE(((1.02018382473542,0.334740937353579,1.),(1.00401234488941,
0.867753072812758,1.),(1.0003362285679,0.988917903080774,1.),(1.,1.,1.)))
REPRESENTATION_ITEM('')
SURFACE()
);
#2673=(
BOUNDED_SURFACE()
B_SPLINE_SURFACE(3,2,((#390624,#390625,#390626),(#390627,#390628,#390629),
(#390630,#390631,#390632),(#390633,#390634,#390635)),.UNSPECIFIED.,.F.,
 .F.,.F.)
B_SPLINE_SURFACE_WITH_KNOTS((4,4),(3,3),(0.00137194782501028,0.00149814269699235),
(0.,1.),.UNSPECIFIED.)
GEOMETRIC_REPRESENTATION_ITEM()
RATIONAL_B_SPLINE_SURFACE(((1.,0.815158509402311,1.),(1.,0.81617904414817,
1.),(1.,0.817226308119933,1.),(1.,0.818301939488804,1.)))
REPRESENTATION_ITEM('')
SURFACE()
);
#2674=(
BOUNDED_SURFACE()
B_SPLINE_SURFACE(3,2,((#390679,#390680,#390681),(#390682,#390683,#390684),
(#390685,#390686,#390687),(#390688,#390689,#390690)),.UNSPECIFIED.,.F.,
 .F.,.F.)
B_SPLINE_SURFACE_WITH_KNOTS((4,4),(3,3),(1.55009486301137E-5,4.92065510474437E-5),
(-8.13759512625954E-5,1.),.UNSPECIFIED.)
GEOMETRIC_REPRESENTATION_ITEM()
RATIONAL_B_SPLINE_SURFACE(((1.00002372912329,0.854200639599705,1.),(1.0000142358599,
0.912530301180581,1.),(1.00000710550469,0.956341495377423,1.),(1.00001238975905,
0.92387333813704,1.)))
REPRESENTATION_ITEM('')
SURFACE()
);
#2675=(
BOUNDED_SURFACE()
B_SPLINE_SURFACE(3,2,((#390694,#390695,#390696),(#390697,#390698,#390699),
(#390700,#390701,#390702),(#390703,#390704,#390705)),.UNSPECIFIED.,.F.,
 .F.,.F.)
B_SPLINE_SURFACE_WITH_KNOTS((4,4),(3,3),(-3.3993417945781E-6,3.73927597403565E-5),
(-0.00186004067444186,1.00069373317443),.UNSPECIFIED.)
GEOMETRIC_REPRESENTATION_ITEM()
RATIONAL_B_SPLINE_SURFACE(((1.00072100136064,0.806051963875309,1.00026859642692),
(1.00060048440162,0.838470803558578,1.00022369994497),(1.00053106448802,
0.857144632272335,1.00019783877221),(1.0005451507286,0.85335545953907,1.00020308635438)))
REPRESENTATION_ITEM('')
SURFACE()
);
#2676=(
BOUNDED_SURFACE()
B_SPLINE_SURFACE(3,2,((#390707,#390708,#390709),(#390710,#390711,#390712),
(#390713,#390714,#390715),(#390716,#390717,#390718)),.UNSPECIFIED.,.F.,
 .F.,.F.)
B_SPLINE_SURFACE_WITH_KNOTS((4,4),(3,3),(-1.62630325872826E-19,9.54361881492174E-5),
(0.,1.),.UNSPECIFIED.)
GEOMETRIC_REPRESENTATION_ITEM()
RATIONAL_B_SPLINE_SURFACE(((1.,0.816715621142052,1.),(1.,0.815907587407941,
1.),(1.,0.815115959345206,1.),(1.,0.814339887349205,1.)))
REPRESENTATION_ITEM('')
SURFACE()
);
#2677=(
BOUNDED_SURFACE()
B_SPLINE_SURFACE(3,2,((#390720,#390721,#390722),(#390723,#390724,#390725),
(#390726,#390727,#390728),(#390729,#390730,#390731)),.UNSPECIFIED.,.F.,
 .F.,.F.)
B_SPLINE_SURFACE_WITH_KNOTS((4,4),(3,3),(-1.62630325872826E-19,4.68197758448203E-5),
(0.,1.),.UNSPECIFIED.)
GEOMETRIC_REPRESENTATION_ITEM()
RATIONAL_B_SPLINE_SURFACE(((1.,0.81671562114205,1.),(1.,0.953638980025207,
1.),(1.,0.954506925408057,1.),(1.,0.816715621142054,1.)))
REPRESENTATION_ITEM('')
SURFACE()
);
#2678=(
BOUNDED_SURFACE()
B_SPLINE_SURFACE(3,2,((#390733,#390734,#390735),(#390736,#390737,#390738),
(#390739,#390740,#390741),(#390742,#390743,#390744)),.UNSPECIFIED.,.F.,
 .F.,.F.)
B_SPLINE_SURFACE_WITH_KNOTS((4,4),(3,3),(0.,9.54361881492176E-5),(0.,1.),
 .UNSPECIFIED.)
GEOMETRIC_REPRESENTATION_ITEM()
RATIONAL_B_SPLINE_SURFACE(((1.,0.814339887349195,1.),(1.,0.815115959345205,
1.),(1.,0.815907587407934,1.),(1.,0.816715621142051,1.)))
REPRESENTATION_ITEM('')
SURFACE()
);
#2679=(
BOUNDED_SURFACE()
B_SPLINE_SURFACE(3,2,((#390746,#390747,#390748),(#390749,#390750,#390751),
(#390752,#390753,#390754),(#390755,#390756,#390757)),.UNSPECIFIED.,.F.,
 .F.,.F.)
B_SPLINE_SURFACE_WITH_KNOTS((4,4),(3,3),(-3.39528393502488E-6,3.73481232852733E-5),
(-0.00165018033319236,1.),.UNSPECIFIED.)
GEOMETRIC_REPRESENTATION_ITEM()
RATIONAL_B_SPLINE_SURFACE(((1.00048354385563,0.853487571660413,1.),(1.00047110510918,
0.857256476851468,1.),(1.00053193201104,0.838826096655893,1.),(1.00063970687722,
0.806170615310112,1.)))
REPRESENTATION_ITEM('')
SURFACE()
);
#2680=(
BOUNDED_SURFACE()
B_SPLINE_SURFACE(3,2,((#390761,#390762,#390763),(#390764,#390765,#390766),
(#390767,#390768,#390769),(#390770,#390771,#390772)),.UNSPECIFIED.,.F.,
 .F.,.F.)
B_SPLINE_SURFACE_WITH_KNOTS((4,4),(3,3),(2.0299386923051E-5,5.39756952687122E-5),
(-0.000116281069487411,1.),.UNSPECIFIED.)
GEOMETRIC_REPRESENTATION_ITEM()
RATIONAL_B_SPLINE_SURFACE(((1.00001770479723,0.923870681143045,1.),(1.00001014104055,
0.956394275543472,1.),(1.00002037300271,0.91239759490564,1.),(1.00003390859456,
0.854195550869798,1.)))
REPRESENTATION_ITEM('')
SURFACE()
);
#2681=(
BOUNDED_SURFACE()
B_SPLINE_SURFACE(3,2,((#390865,#390866,#390867),(#390868,#390869,#390870),
(#390871,#390872,#390873),(#390874,#390875,#390876)),.UNSPECIFIED.,.F.,
 .F.,.F.)
B_SPLINE_SURFACE_WITH_KNOTS((4,4),(3,3),(0.00135801595889393,0.00148409170619832),
(0.,1.),.UNSPECIFIED.)
GEOMETRIC_REPRESENTATION_ITEM()
RATIONAL_B_SPLINE_SURFACE(((1.,0.818301933966441,1.),(1.,0.817226613172357,
1.),(1.,0.816179643373942,1.),(1.,0.815159387863654,1.)))
REPRESENTATION_ITEM('')
SURFACE()
);
#2682=(
BOUNDED_SURFACE()
B_SPLINE_SURFACE(3,2,((#390915,#390916,#390917),(#390918,#390919,#390920),
(#390921,#390922,#390923),(#390924,#390925,#390926)),.UNSPECIFIED.,.F.,
 .F.,.F.)
B_SPLINE_SURFACE_WITH_KNOTS((4,4),(3,3),(-1.5474443512208E-6,1.54744435122079E-5),
(-0.0151698983560359,1.01516989836669),.UNSPECIFIED.)
GEOMETRIC_REPRESENTATION_ITEM()
RATIONAL_B_SPLINE_SURFACE(((1.02018382472135,0.324498219413126,1.02018382473574),
(1.00401234488662,0.865716921710547,1.00401234488948),(1.00033622856767,
0.988747276629689,1.00033622856791),(1.,1.,1.)))
REPRESENTATION_ITEM('')
SURFACE()
);
#2683=(
BOUNDED_SURFACE()
B_SPLINE_SURFACE(3,2,((#390928,#390929,#390930),(#390931,#390932,#390933),
(#390934,#390935,#390936),(#390937,#390938,#390939)),.UNSPECIFIED.,.F.,
 .F.,.F.)
B_SPLINE_SURFACE_WITH_KNOTS((4,4),(3,3),(0.00137194782501028,0.00149814269699235),
(0.,1.),.UNSPECIFIED.)
GEOMETRIC_REPRESENTATION_ITEM()
RATIONAL_B_SPLINE_SURFACE(((1.,0.81515850940232,1.),(1.,0.816179044148155,
1.),(1.,0.817226308119932,1.),(1.,0.818301939488814,1.)))
REPRESENTATION_ITEM('')
SURFACE()
);
#2684=(
BOUNDED_SURFACE()
B_SPLINE_SURFACE(3,2,((#390983,#390984,#390985),(#390986,#390987,#390988),
(#390989,#390990,#390991),(#390992,#390993,#390994)),.UNSPECIFIED.,.F.,
 .F.,.F.)
B_SPLINE_SURFACE_WITH_KNOTS((4,4),(3,3),(1.55009486301137E-5,4.92065510474433E-5),
(-8.13759512421491E-5,1.),.UNSPECIFIED.)
GEOMETRIC_REPRESENTATION_ITEM()
RATIONAL_B_SPLINE_SURFACE(((1.00002372912329,0.854200639599716,1.),(1.00001423585989,
0.912530301180567,1.),(1.00000710550469,0.956341495377428,1.),(1.00001238975905,
0.923873338137046,1.)))
REPRESENTATION_ITEM('')
SURFACE()
);
#2685=(
BOUNDED_SURFACE()
B_SPLINE_SURFACE(3,2,((#390998,#390999,#391000),(#391001,#391002,#391003),
(#391004,#391005,#391006),(#391007,#391008,#391009)),.UNSPECIFIED.,.F.,
 .F.,.F.)
B_SPLINE_SURFACE_WITH_KNOTS((4,4),(3,3),(-3.39934179457794E-6,3.73927597403566E-5),
(-0.00186004067499191,1.0006937331745),.UNSPECIFIED.)
GEOMETRIC_REPRESENTATION_ITEM()
RATIONAL_B_SPLINE_SURFACE(((1.00072100136086,0.806051963875182,1.00026859642695),
(1.0006004844018,0.838470803558485,1.00022369994499),(1.00053106448818,
0.857144632272248,1.00019783877222),(1.00054515072876,0.853355459538966,
1.0002030863544)))
REPRESENTATION_ITEM('')
SURFACE()
);
#2686=(
BOUNDED_SURFACE()
B_SPLINE_SURFACE(3,2,((#391011,#391012,#391013),(#391014,#391015,#391016),
(#391017,#391018,#391019),(#391020,#391021,#391022)),.UNSPECIFIED.,.F.,
 .F.,.F.)
B_SPLINE_SURFACE_WITH_KNOTS((4,4),(3,3),(1.0842021724855E-19,9.54361881492177E-5),
(0.,1.),.UNSPECIFIED.)
GEOMETRIC_REPRESENTATION_ITEM()
RATIONAL_B_SPLINE_SURFACE(((1.,0.816715621142048,1.),(1.,0.815907587407943,
1.),(1.,0.815115959345211,1.),(1.,0.814339887349192,1.)))
REPRESENTATION_ITEM('')
SURFACE()
);
#2687=(
BOUNDED_SURFACE()
B_SPLINE_SURFACE(3,2,((#391024,#391025,#391026),(#391027,#391028,#391029),
(#391030,#391031,#391032),(#391033,#391034,#391035)),.UNSPECIFIED.,.F.,
 .F.,.F.)
B_SPLINE_SURFACE_WITH_KNOTS((4,4),(3,3),(-1.35525271560688E-20,4.68197758448202E-5),
(0.,1.),.UNSPECIFIED.)
GEOMETRIC_REPRESENTATION_ITEM()
RATIONAL_B_SPLINE_SURFACE(((1.,0.816715621142053,1.),(1.,0.953638980025202,
1.),(1.,0.954506925408059,1.),(1.,0.816715621142055,1.)))
REPRESENTATION_ITEM('')
SURFACE()
);
#2688=(
BOUNDED_SURFACE()
B_SPLINE_SURFACE(3,2,((#391037,#391038,#391039),(#391040,#391041,#391042),
(#391043,#391044,#391045),(#391046,#391047,#391048)),.UNSPECIFIED.,.F.,
 .F.,.F.)
B_SPLINE_SURFACE_WITH_KNOTS((4,4),(3,3),(2.16840434497101E-19,9.54361881492179E-5),
(0.,1.),.UNSPECIFIED.)
GEOMETRIC_REPRESENTATION_ITEM()
RATIONAL_B_SPLINE_SURFACE(((1.,0.814339887349196,1.),(1.,0.81511595934521,
1.),(1.,0.815907587407947,1.),(1.,0.816715621142053,1.)))
REPRESENTATION_ITEM('')
SURFACE()
);
#2689=(
BOUNDED_SURFACE()
B_SPLINE_SURFACE(3,2,((#391050,#391051,#391052),(#391053,#391054,#391055),
(#391056,#391057,#391058),(#391059,#391060,#391061)),.UNSPECIFIED.,.F.,
 .F.,.F.)
B_SPLINE_SURFACE_WITH_KNOTS((4,4),(3,3),(-3.39528393502263E-6,3.73481232852728E-5),
(-0.00165018033282337,1.),.UNSPECIFIED.)
GEOMETRIC_REPRESENTATION_ITEM()
RATIONAL_B_SPLINE_SURFACE(((1.00048354385552,0.853487571660466,0.999999999999999),
(1.00047110510907,0.857256476851539,1.),(1.00053193201092,0.838826096655945,
1.),(1.00063970687708,0.806170615310179,0.999999999999999)))
REPRESENTATION_ITEM('')
SURFACE()
);
#2690=(
BOUNDED_SURFACE()
B_SPLINE_SURFACE(3,2,((#391065,#391066,#391067),(#391068,#391069,#391070),
(#391071,#391072,#391073),(#391074,#391075,#391076)),.UNSPECIFIED.,.F.,
 .F.,.F.)
B_SPLINE_SURFACE_WITH_KNOTS((4,4),(3,3),(2.0299386923051E-5,5.39756952687123E-5),
(-0.000116281069803118,1.),.UNSPECIFIED.)
GEOMETRIC_REPRESENTATION_ITEM()
RATIONAL_B_SPLINE_SURFACE(((1.00001770479728,0.923870681143023,1.),(1.00001014104058,
0.956394275543449,1.),(1.00002037300276,0.912397594905616,1.),(1.00003390859465,
0.854195550869764,1.)))
REPRESENTATION_ITEM('')
SURFACE()
);
#2691=(
BOUNDED_SURFACE()
B_SPLINE_SURFACE(3,2,((#391169,#391170,#391171),(#391172,#391173,#391174),
(#391175,#391176,#391177),(#391178,#391179,#391180)),.UNSPECIFIED.,.F.,
 .F.,.F.)
B_SPLINE_SURFACE_WITH_KNOTS((4,4),(3,3),(0.00135801595889393,0.00148409170619832),
(0.,1.),.UNSPECIFIED.)
GEOMETRIC_REPRESENTATION_ITEM()
RATIONAL_B_SPLINE_SURFACE(((1.,0.818301933966442,1.),(1.,0.817226613172347,
1.),(1.,0.816179643373956,1.),(1.,0.815159387863651,1.)))
REPRESENTATION_ITEM('')
SURFACE()
);
#2692=(
BOUNDED_SURFACE()
B_SPLINE_SURFACE(3,2,((#391219,#391220,#391221),(#391222,#391223,#391224),
(#391225,#391226,#391227),(#391228,#391229,#391230)),.UNSPECIFIED.,.F.,
 .F.,.F.)
B_SPLINE_SURFACE_WITH_KNOTS((4,4),(3,3),(-1.54744435122076E-6,1.54744435122077E-5),
(-0.015169898366694,1.015169898356),.UNSPECIFIED.)
GEOMETRIC_REPRESENTATION_ITEM()
RATIONAL_B_SPLINE_SURFACE(((1.02018382473574,0.32449821941326,1.0201838247213),
(1.00401234488948,0.865716921710591,1.00401234488661),(1.00033622856791,
0.988747276629664,1.00033622856767),(1.,1.,1.)))
REPRESENTATION_ITEM('')
SURFACE()
);
#2693=(
BOUNDED_SURFACE()
B_SPLINE_SURFACE(3,2,((#391232,#391233,#391234),(#391235,#391236,#391237),
(#391238,#391239,#391240),(#391241,#391242,#391243)),.UNSPECIFIED.,.F.,
 .F.,.F.)
B_SPLINE_SURFACE_WITH_KNOTS((4,4),(3,3),(0.00137194782501028,0.00149814269699235),
(0.,1.),.UNSPECIFIED.)
GEOMETRIC_REPRESENTATION_ITEM()
RATIONAL_B_SPLINE_SURFACE(((1.,0.815158509402324,1.),(1.,0.816179044148158,
1.),(1.,0.817226308119934,1.),(1.,0.818301939488811,1.)))
REPRESENTATION_ITEM('')
SURFACE()
);
#2694=(
BOUNDED_SURFACE()
B_SPLINE_SURFACE(3,2,((#391287,#391288,#391289),(#391290,#391291,#391292),
(#391293,#391294,#391295),(#391296,#391297,#391298)),.UNSPECIFIED.,.F.,
 .F.,.F.)
B_SPLINE_SURFACE_WITH_KNOTS((4,4),(3,3),(1.55009486301137E-5,4.92065510474431E-5),
(-8.1375951403725E-5,1.),.UNSPECIFIED.)
GEOMETRIC_REPRESENTATION_ITEM()
RATIONAL_B_SPLINE_SURFACE(((1.00002372912333,0.854200639599696,1.),(1.00001423585992,
0.912530301180547,1.),(1.0000071055047,0.956341495377436,1.),(1.00001238975907,
0.923873338137027,1.)))
REPRESENTATION_ITEM('')
SURFACE()
);
#2695=(
BOUNDED_SURFACE()
B_SPLINE_SURFACE(3,2,((#391302,#391303,#391304),(#391305,#391306,#391307),
(#391308,#391309,#391310),(#391311,#391312,#391313)),.UNSPECIFIED.,.F.,
 .F.,.F.)
B_SPLINE_SURFACE_WITH_KNOTS((4,4),(3,3),(-3.39934179457726E-6,3.73927597403567E-5),
(-0.00186004067386771,1.00069373317438),.UNSPECIFIED.)
GEOMETRIC_REPRESENTATION_ITEM()
RATIONAL_B_SPLINE_SURFACE(((1.00072100136042,0.806051963875403,1.0002685964269),
(1.00060048440144,0.838470803558709,1.00022369994495),(1.00053106448786,
0.857144632272417,1.00019783877219),(1.00054515072843,0.853355459539146,
1.00020308635436)))
REPRESENTATION_ITEM('')
SURFACE()
);
#2696=(
BOUNDED_SURFACE()
B_SPLINE_SURFACE(3,2,((#391315,#391316,#391317),(#391318,#391319,#391320),
(#391321,#391322,#391323),(#391324,#391325,#391326)),.UNSPECIFIED.,.F.,
 .F.,.F.)
B_SPLINE_SURFACE_WITH_KNOTS((4,4),(3,3),(0.,9.54361881492175E-5),(0.,1.),
 .UNSPECIFIED.)
GEOMETRIC_REPRESENTATION_ITEM()
RATIONAL_B_SPLINE_SURFACE(((1.,0.816715621142048,1.),(1.,0.815907587407944,
1.),(1.,0.815115959345201,1.),(1.,0.814339887349192,1.)))
REPRESENTATION_ITEM('')
SURFACE()
);
#2697=(
BOUNDED_SURFACE()
B_SPLINE_SURFACE(3,2,((#391328,#391329,#391330),(#391331,#391332,#391333),
(#391334,#391335,#391336),(#391337,#391338,#391339)),.UNSPECIFIED.,.F.,
 .F.,.F.)
B_SPLINE_SURFACE_WITH_KNOTS((4,4),(3,3),(-2.03287907341032E-20,4.68197758448202E-5),
(0.,1.),.UNSPECIFIED.)
GEOMETRIC_REPRESENTATION_ITEM()
RATIONAL_B_SPLINE_SURFACE(((1.,0.816715621142051,1.),(1.,0.953638980025202,
1.),(1.,0.954506925408062,1.),(1.,0.816715621142055,1.)))
REPRESENTATION_ITEM('')
SURFACE()
);
#2698=(
BOUNDED_SURFACE()
B_SPLINE_SURFACE(3,2,((#391341,#391342,#391343),(#391344,#391345,#391346),
(#391347,#391348,#391349),(#391350,#391351,#391352)),.UNSPECIFIED.,.F.,
 .F.,.F.)
B_SPLINE_SURFACE_WITH_KNOTS((4,4),(3,3),(-1.0842021724855E-19,9.54361881492179E-5),
(0.,1.),.UNSPECIFIED.)
GEOMETRIC_REPRESENTATION_ITEM()
RATIONAL_B_SPLINE_SURFACE(((1.,0.814339887349194,1.),(1.,0.815115959345207,
1.),(1.,0.815907587407945,1.),(1.,0.816715621142051,1.)))
REPRESENTATION_ITEM('')
SURFACE()
);
#2699=(
BOUNDED_SURFACE()
B_SPLINE_SURFACE(3,2,((#391354,#391355,#391356),(#391357,#391358,#391359),
(#391360,#391361,#391362),(#391363,#391364,#391365)),.UNSPECIFIED.,.F.,
 .F.,.F.)
B_SPLINE_SURFACE_WITH_KNOTS((4,4),(3,3),(-3.39528393502489E-6,3.73481232852729E-5),
(-0.00165018033268899,1.),.UNSPECIFIED.)
GEOMETRIC_REPRESENTATION_ITEM()
RATIONAL_B_SPLINE_SURFACE(((1.00048354385548,0.853487571660492,1.),(1.00047110510904,
0.85725647685155,1.),(1.00053193201088,0.838826096655953,1.),(1.00063970687702,
0.806170615310211,1.)))
REPRESENTATION_ITEM('')
SURFACE()
);
#2700=(
BOUNDED_SURFACE()
B_SPLINE_SURFACE(3,2,((#391369,#391370,#391371),(#391372,#391373,#391374),
(#391375,#391376,#391377),(#391378,#391379,#391380)),.UNSPECIFIED.,.F.,
 .F.,.F.)
B_SPLINE_SURFACE_WITH_KNOTS((4,4),(3,3),(2.02993869230509E-5,5.39756952687132E-5),
(-0.000116281069788604,1.),.UNSPECIFIED.)
GEOMETRIC_REPRESENTATION_ITEM()
RATIONAL_B_SPLINE_SURFACE(((1.00001770479728,0.923870681143019,1.),(1.00001014104058,
0.956394275543461,1.),(1.00002037300276,0.912397594905618,1.),(1.00003390859465,
0.854195550869757,1.)))
REPRESENTATION_ITEM('')
SURFACE()
);
#2701=(
BOUNDED_SURFACE()
B_SPLINE_SURFACE(3,2,((#391473,#391474,#391475),(#391476,#391477,#391478),
(#391479,#391480,#391481),(#391482,#391483,#391484)),.UNSPECIFIED.,.F.,
 .F.,.F.)
B_SPLINE_SURFACE_WITH_KNOTS((4,4),(3,3),(0.00135801595889393,0.00148409170619832),
(0.,1.),.UNSPECIFIED.)
GEOMETRIC_REPRESENTATION_ITEM()
RATIONAL_B_SPLINE_SURFACE(((1.,0.818301933966439,1.),(1.,0.817226613172347,
1.),(1.,0.816179643373954,1.),(1.,0.815159387863651,1.)))
REPRESENTATION_ITEM('')
SURFACE()
);
#2702=(
BOUNDED_SURFACE()
B_SPLINE_SURFACE(3,2,((#391523,#391524,#391525),(#391526,#391527,#391528),
(#391529,#391530,#391531),(#391532,#391533,#391534)),.UNSPECIFIED.,.F.,
 .F.,.F.)
B_SPLINE_SURFACE_WITH_KNOTS((4,4),(3,3),(-1.54744435122088E-6,1.54744435122086E-5),
(0.,1.01516989836117),.UNSPECIFIED.)
GEOMETRIC_REPRESENTATION_ITEM()
RATIONAL_B_SPLINE_SURFACE(((1.,0.33474093735719,1.02018382472828),(1.,0.867753072813379,
1.004012344888),(1.,0.988917903080892,1.00033622856778),(1.,1.,1.)))
REPRESENTATION_ITEM('')
SURFACE()
);
#2703=(
BOUNDED_SURFACE()
B_SPLINE_SURFACE(3,2,((#391536,#391537,#391538),(#391539,#391540,#391541),
(#391542,#391543,#391544),(#391545,#391546,#391547)),.UNSPECIFIED.,.F.,
 .F.,.F.)
B_SPLINE_SURFACE_WITH_KNOTS((4,4),(3,3),(0.00137194782501028,0.00149814269699235),
(0.,1.),.UNSPECIFIED.)
GEOMETRIC_REPRESENTATION_ITEM()
RATIONAL_B_SPLINE_SURFACE(((1.,0.815158509402315,1.),(1.,0.816179044148166,
1.),(1.,0.817226308119922,1.),(1.,0.81830193948881,1.)))
REPRESENTATION_ITEM('')
SURFACE()
);
#2704=(
BOUNDED_SURFACE()
B_SPLINE_SURFACE(3,2,((#391591,#391592,#391593),(#391594,#391595,#391596),
(#391597,#391598,#391599),(#391600,#391601,#391602)),.UNSPECIFIED.,.F.,
 .F.,.F.)
B_SPLINE_SURFACE_WITH_KNOTS((4,4),(3,3),(1.55009486301138E-5,4.92065510474433E-5),
(-8.13759515113838E-5,1.),.UNSPECIFIED.)
GEOMETRIC_REPRESENTATION_ITEM()
RATIONAL_B_SPLINE_SURFACE(((1.00002372912336,0.854200639599683,1.),(1.00001423585994,
0.912530301180536,1.),(1.00000710550471,0.956341495377428,1.),(1.00001238975909,
0.92387333813702,1.)))
REPRESENTATION_ITEM('')
SURFACE()
);
#2705=(
BOUNDED_SURFACE()
B_SPLINE_SURFACE(3,2,((#391606,#391607,#391608),(#391609,#391610,#391611),
(#391612,#391613,#391614),(#391615,#391616,#391617)),.UNSPECIFIED.,.F.,
 .F.,.F.)
B_SPLINE_SURFACE_WITH_KNOTS((4,4),(3,3),(-3.39934179457829E-6,3.73927597403567E-5),
(-0.00186004067439069,1.00069373317447),.UNSPECIFIED.)
GEOMETRIC_REPRESENTATION_ITEM()
RATIONAL_B_SPLINE_SURFACE(((1.00072100136063,0.806051963875286,1.00026859642694),
(1.00060048440161,0.838470803558599,1.00022369994498),(1.00053106448801,
0.857144632272333,1.00019783877221),(1.00054515072858,0.853355459539056,
1.00020308635439)))
REPRESENTATION_ITEM('')
SURFACE()
);
#2706=(
BOUNDED_SURFACE()
B_SPLINE_SURFACE(3,2,((#391619,#391620,#391621),(#391622,#391623,#391624),
(#391625,#391626,#391627),(#391628,#391629,#391630)),.UNSPECIFIED.,.F.,
 .F.,.F.)
B_SPLINE_SURFACE_WITH_KNOTS((4,4),(3,3),(0.,9.54361881492173E-5),(0.,1.),
 .UNSPECIFIED.)
GEOMETRIC_REPRESENTATION_ITEM()
RATIONAL_B_SPLINE_SURFACE(((1.,0.816715621142043,1.),(1.,0.815907587407943,
1.),(1.,0.815115959345201,1.),(1.,0.814339887349192,1.)))
REPRESENTATION_ITEM('')
SURFACE()
);
#2707=(
BOUNDED_SURFACE()
B_SPLINE_SURFACE(3,2,((#391632,#391633,#391634),(#391635,#391636,#391637),
(#391638,#391639,#391640),(#391641,#391642,#391643)),.UNSPECIFIED.,.F.,
 .F.,.F.)
B_SPLINE_SURFACE_WITH_KNOTS((4,4),(3,3),(3.72694496791892E-20,4.68197758448211E-5),
(0.,1.),.UNSPECIFIED.)
GEOMETRIC_REPRESENTATION_ITEM()
RATIONAL_B_SPLINE_SURFACE(((1.,0.816715621142048,1.),(1.,0.953638980025199,
1.),(1.,0.954506925408065,1.),(1.,0.81671562114205,1.)))
REPRESENTATION_ITEM('')
SURFACE()
);
#2708=(
BOUNDED_SURFACE()
B_SPLINE_SURFACE(3,2,((#391645,#391646,#391647),(#391648,#391649,#391650),
(#391651,#391652,#391653),(#391654,#391655,#391656)),.UNSPECIFIED.,.F.,
 .F.,.F.)
B_SPLINE_SURFACE_WITH_KNOTS((4,4),(3,3),(5.42101086242752E-20,9.54361881492175E-5),
(0.,1.),.UNSPECIFIED.)
GEOMETRIC_REPRESENTATION_ITEM()
RATIONAL_B_SPLINE_SURFACE(((1.,0.814339887349195,1.),(1.,0.815115959345203,
1.),(1.,0.815907587407943,1.),(1.,0.816715621142048,1.)))
REPRESENTATION_ITEM('')
SURFACE()
);
#2709=(
BOUNDED_SURFACE()
B_SPLINE_SURFACE(3,2,((#391658,#391659,#391660),(#391661,#391662,#391663),
(#391664,#391665,#391666),(#391667,#391668,#391669)),.UNSPECIFIED.,.F.,
 .F.,.F.)
B_SPLINE_SURFACE_WITH_KNOTS((4,4),(3,3),(-3.39528393502494E-6,3.73481232852736E-5),
(-0.00165018033281065,1.),.UNSPECIFIED.)
GEOMETRIC_REPRESENTATION_ITEM()
RATIONAL_B_SPLINE_SURFACE(((1.00048354385552,0.853487571660464,1.),(1.00047110510907,
0.857256476851531,1.),(1.00053193201092,0.838826096655946,1.),(1.00063970687707,
0.806170615310178,1.)))
REPRESENTATION_ITEM('')
SURFACE()
);
#2710=(
BOUNDED_SURFACE()
B_SPLINE_SURFACE(3,2,((#391673,#391674,#391675),(#391676,#391677,#391678),
(#391679,#391680,#391681),(#391682,#391683,#391684)),.UNSPECIFIED.,.F.,
 .F.,.F.)
B_SPLINE_SURFACE_WITH_KNOTS((4,4),(3,3),(2.02993869230512E-5,5.39756952686905E-5),
(-0.000116281069867502,1.),.UNSPECIFIED.)
GEOMETRIC_REPRESENTATION_ITEM()
RATIONAL_B_SPLINE_SURFACE(((1.00001770479729,0.923870681143014,1.),(1.00001014104058,
0.956394275543423,1.),(1.00002037300277,0.912397594905681,1.),(1.00003390859467,
0.854195550869863,1.)))
REPRESENTATION_ITEM('')
SURFACE()
);
#2711=(
BOUNDED_SURFACE()
B_SPLINE_SURFACE(3,2,((#391777,#391778,#391779),(#391780,#391781,#391782),
(#391783,#391784,#391785),(#391786,#391787,#391788)),.UNSPECIFIED.,.F.,
 .F.,.F.)
B_SPLINE_SURFACE_WITH_KNOTS((4,4),(3,3),(0.00135801595889393,0.00148409170619832),
(0.,1.),.UNSPECIFIED.)
GEOMETRIC_REPRESENTATION_ITEM()
RATIONAL_B_SPLINE_SURFACE(((1.,0.818301933966447,1.),(1.,0.817226613172343,
1.),(1.,0.816179643373953,1.),(1.,0.815159387863653,1.)))
REPRESENTATION_ITEM('')
SURFACE()
);
#2712=(
BOUNDED_SURFACE()
B_SPLINE_SURFACE(3,2,((#391827,#391828,#391829),(#391830,#391831,#391832),
(#391833,#391834,#391835),(#391836,#391837,#391838)),.UNSPECIFIED.,.F.,
 .F.,.F.)
B_SPLINE_SURFACE_WITH_KNOTS((4,4),(3,3),(-1.54744435122076E-6,1.54744435122075E-5),
(-0.0151698983634846,1.),.UNSPECIFIED.)
GEOMETRIC_REPRESENTATION_ITEM()
RATIONAL_B_SPLINE_SURFACE(((1.0201838247314,0.334740937355646,1.),(1.00401234488862,
0.867753072813101,1.),(1.00033622856784,0.9889179030808,1.),(1.,1.,1.)))
REPRESENTATION_ITEM('')
SURFACE()
);
#2713=(
BOUNDED_SURFACE()
B_SPLINE_SURFACE(3,2,((#391840,#391841,#391842),(#391843,#391844,#391845),
(#391846,#391847,#391848),(#391849,#391850,#391851)),.UNSPECIFIED.,.F.,
 .F.,.F.)
B_SPLINE_SURFACE_WITH_KNOTS((4,4),(3,3),(0.00137194782501028,0.00149814269699235),
(0.,1.),.UNSPECIFIED.)
GEOMETRIC_REPRESENTATION_ITEM()
RATIONAL_B_SPLINE_SURFACE(((1.,0.815158509402315,1.),(1.,0.816179044148159,
1.),(1.,0.817226308119933,1.),(1.,0.818301939488797,1.)))
REPRESENTATION_ITEM('')
SURFACE()
);
#2714=(
BOUNDED_SURFACE()
B_SPLINE_SURFACE(3,2,((#391895,#391896,#391897),(#391898,#391899,#391900),
(#391901,#391902,#391903),(#391904,#391905,#391906)),.UNSPECIFIED.,.F.,
 .F.,.F.)
B_SPLINE_SURFACE_WITH_KNOTS((4,4),(3,3),(1.55009486301138E-5,4.9206551047444E-5),
(-8.13759513100112E-5,1.),.UNSPECIFIED.)
GEOMETRIC_REPRESENTATION_ITEM()
RATIONAL_B_SPLINE_SURFACE(((1.00002372912331,0.854200639599707,1.),(1.0000142358599,
0.912530301180563,1.),(1.00000710550469,0.956341495377437,1.),(1.00001238975906,
0.923873338137034,1.)))
REPRESENTATION_ITEM('')
SURFACE()
);
#2715=(
BOUNDED_SURFACE()
B_SPLINE_SURFACE(3,2,((#391910,#391911,#391912),(#391913,#391914,#391915),
(#391916,#391917,#391918),(#391919,#391920,#391921)),.UNSPECIFIED.,.F.,
 .F.,.F.)
B_SPLINE_SURFACE_WITH_KNOTS((4,4),(3,3),(-3.39934179457842E-6,3.73927597403566E-5),
(-0.00186004067399086,1.00069373317438),.UNSPECIFIED.)
GEOMETRIC_REPRESENTATION_ITEM()
RATIONAL_B_SPLINE_SURFACE(((1.00072100136047,0.806051963875379,1.0002685964269),
(1.00060048440148,0.838470803558684,1.00022369994495),(1.00053106448789,
0.857144632272404,1.00019783877219),(1.00054515072847,0.853355459539131,
1.00020308635436)))
REPRESENTATION_ITEM('')
SURFACE()
);
#2716=(
BOUNDED_SURFACE()
B_SPLINE_SURFACE(3,2,((#391923,#391924,#391925),(#391926,#391927,#391928),
(#391929,#391930,#391931),(#391932,#391933,#391934)),.UNSPECIFIED.,.F.,
 .F.,.F.)
B_SPLINE_SURFACE_WITH_KNOTS((4,4),(3,3),(-5.42101086242752E-20,9.54361881492174E-5),
(0.,1.),.UNSPECIFIED.)
GEOMETRIC_REPRESENTATION_ITEM()
RATIONAL_B_SPLINE_SURFACE(((1.,0.81671562114205,1.),(1.,0.815907587407946,
1.),(1.,0.815115959345202,1.),(1.,0.814339887349197,1.)))
REPRESENTATION_ITEM('')
SURFACE()
);
#2717=(
BOUNDED_SURFACE()
B_SPLINE_SURFACE(3,2,((#391936,#391937,#391938),(#391939,#391940,#391941),
(#391942,#391943,#391944),(#391945,#391946,#391947)),.UNSPECIFIED.,.F.,
 .F.,.F.)
B_SPLINE_SURFACE_WITH_KNOTS((4,4),(3,3),(6.60685698858354E-20,4.68197758448206E-5),
(0.,1.),.UNSPECIFIED.)
GEOMETRIC_REPRESENTATION_ITEM()
RATIONAL_B_SPLINE_SURFACE(((1.,0.816715621142048,1.),(1.,0.95363898002521,
1.),(1.,0.954506925408056,1.),(1.,0.816715621142053,1.)))
REPRESENTATION_ITEM('')
SURFACE()
);
#2718=(
BOUNDED_SURFACE()
B_SPLINE_SURFACE(3,2,((#391949,#391950,#391951),(#391952,#391953,#391954),
(#391955,#391956,#391957),(#391958,#391959,#391960)),.UNSPECIFIED.,.F.,
 .F.,.F.)
B_SPLINE_SURFACE_WITH_KNOTS((4,4),(3,3),(5.42101086242752E-20,9.54361881492175E-5),
(0.,1.),.UNSPECIFIED.)
GEOMETRIC_REPRESENTATION_ITEM()
RATIONAL_B_SPLINE_SURFACE(((1.,0.814339887349195,1.),(1.,0.815115959345198,
1.),(1.,0.815907587407947,1.),(1.,0.816715621142048,1.)))
REPRESENTATION_ITEM('')
SURFACE()
);
#2719=(
BOUNDED_SURFACE()
B_SPLINE_SURFACE(3,2,((#391962,#391963,#391964),(#391965,#391966,#391967),
(#391968,#391969,#391970),(#391971,#391972,#391973)),.UNSPECIFIED.,.F.,
 .F.,.F.)
B_SPLINE_SURFACE_WITH_KNOTS((4,4),(3,3),(-3.39528393502485E-6,3.73481232852736E-5),
(-0.0016501803329349,1.),.UNSPECIFIED.)
GEOMETRIC_REPRESENTATION_ITEM()
RATIONAL_B_SPLINE_SURFACE(((1.00048354385555,0.853487571660447,1.),(1.00047110510911,
0.857256476851509,1.),(1.00053193201096,0.838826096655926,1.),(1.00063970687712,
0.806170615310158,1.)))
REPRESENTATION_ITEM('')
SURFACE()
);
#2720=(
BOUNDED_SURFACE()
B_SPLINE_SURFACE(3,2,((#391977,#391978,#391979),(#391980,#391981,#391982),
(#391983,#391984,#391985),(#391986,#391987,#391988)),.UNSPECIFIED.,.F.,
 .F.,.F.)
B_SPLINE_SURFACE_WITH_KNOTS((4,4),(3,3),(2.02993869230509E-5,5.39756952686908E-5),
(-0.000116281069783489,1.),.UNSPECIFIED.)
GEOMETRIC_REPRESENTATION_ITEM()
RATIONAL_B_SPLINE_SURFACE(((1.00001770479728,0.92387068114302,1.),(1.00001014104058,
0.956394275543422,1.),(1.00002037300276,0.912397594905689,1.),(1.00003390859465,
0.854195550869876,1.)))
REPRESENTATION_ITEM('')
SURFACE()
);
#2721=(
BOUNDED_SURFACE()
B_SPLINE_SURFACE(3,2,((#392081,#392082,#392083),(#392084,#392085,#392086),
(#392087,#392088,#392089),(#392090,#392091,#392092)),.UNSPECIFIED.,.F.,
 .F.,.F.)
B_SPLINE_SURFACE_WITH_KNOTS((4,4),(3,3),(0.00135801595889393,0.00148409170619832),
(0.,1.),.UNSPECIFIED.)
GEOMETRIC_REPRESENTATION_ITEM()
RATIONAL_B_SPLINE_SURFACE(((1.,0.818301933966443,1.),(1.,0.817226613172345,
1.),(1.,0.816179643373947,1.),(1.,0.815159387863655,1.)))
REPRESENTATION_ITEM('')
SURFACE()
);
#2722=(
BOUNDED_SURFACE()
B_SPLINE_SURFACE(3,2,((#392131,#392132,#392133),(#392134,#392135,#392136),
(#392137,#392138,#392139),(#392140,#392141,#392142)),.UNSPECIFIED.,.F.,
 .F.,.F.)
B_SPLINE_SURFACE_WITH_KNOTS((4,4),(3,3),(-1.54744435122035E-6,1.54744435122103E-5),
(-0.0151698983687994,1.01516989835352),.UNSPECIFIED.)
GEOMETRIC_REPRESENTATION_ITEM()
RATIONAL_B_SPLINE_SURFACE(((1.02018382473858,0.324498219413536,1.02018382471794),
(1.00401234489005,0.865716921710479,1.00401234488594),(1.00033622856796,
0.9887472766297,1.00033622856761),(1.,1.,1.)))
REPRESENTATION_ITEM('')
SURFACE()
);
#2723=(
BOUNDED_SURFACE()
B_SPLINE_SURFACE(3,2,((#392144,#392145,#392146),(#392147,#392148,#392149),
(#392150,#392151,#392152),(#392153,#392154,#392155)),.UNSPECIFIED.,.F.,
 .F.,.F.)
B_SPLINE_SURFACE_WITH_KNOTS((4,4),(3,3),(0.00137194782501028,0.00149814269699235),
(0.,1.),.UNSPECIFIED.)
GEOMETRIC_REPRESENTATION_ITEM()
RATIONAL_B_SPLINE_SURFACE(((1.,0.81515850940232,1.),(1.,0.816179044148184,
1.),(1.,0.817226308119919,1.),(1.,0.818301939488813,1.)))
REPRESENTATION_ITEM('')
SURFACE()
);
#2724=(
BOUNDED_SURFACE()
B_SPLINE_SURFACE(3,2,((#392199,#392200,#392201),(#392202,#392203,#392204),
(#392205,#392206,#392207),(#392208,#392209,#392210)),.UNSPECIFIED.,.F.,
 .F.,.F.)
B_SPLINE_SURFACE_WITH_KNOTS((4,4),(3,3),(1.55009486301137E-5,4.92065510474437E-5),
(-8.13759513857627E-5,1.),.UNSPECIFIED.)
GEOMETRIC_REPRESENTATION_ITEM()
RATIONAL_B_SPLINE_SURFACE(((1.00002372912333,0.854200639599689,1.),(1.00001423585992,
0.912530301180556,1.),(1.0000071055047,0.956341495377434,1.),(1.00001238975907,
0.923873338137031,1.)))
REPRESENTATION_ITEM('')
SURFACE()
);
#2725=(
BOUNDED_SURFACE()
B_SPLINE_SURFACE(3,2,((#392214,#392215,#392216),(#392217,#392218,#392219),
(#392220,#392221,#392222),(#392223,#392224,#392225)),.UNSPECIFIED.,.F.,
 .F.,.F.)
B_SPLINE_SURFACE_WITH_KNOTS((4,4),(3,3),(-3.39934179457847E-6,3.73927597403563E-5),
(-0.00186004067427395,1.0006937331744),.UNSPECIFIED.)
GEOMETRIC_REPRESENTATION_ITEM()
RATIONAL_B_SPLINE_SURFACE(((1.00072100136058,0.806051963875343,1.00026859642691),
(1.00060048440157,0.838470803558615,1.00022369994496),(1.00053106448797,
0.857144632272372,1.00019783877219),(1.00054515072855,0.85335545953908,
1.00020308635437)))
REPRESENTATION_ITEM('')
SURFACE()
);
#2726=(
BOUNDED_SURFACE()
B_SPLINE_SURFACE(3,2,((#392227,#392228,#392229),(#392230,#392231,#392232),
(#392233,#392234,#392235),(#392236,#392237,#392238)),.UNSPECIFIED.,.F.,
 .F.,.F.)
B_SPLINE_SURFACE_WITH_KNOTS((4,4),(3,3),(-5.42101086242752E-20,9.54361881492172E-5),
(0.,1.),.UNSPECIFIED.)
GEOMETRIC_REPRESENTATION_ITEM()
RATIONAL_B_SPLINE_SURFACE(((1.,0.816715621142052,1.),(1.,0.81590758740794,
1.),(1.,0.815115959345208,1.),(1.,0.814339887349189,1.)))
REPRESENTATION_ITEM('')
SURFACE()
);
#2727=(
BOUNDED_SURFACE()
B_SPLINE_SURFACE(3,2,((#392240,#392241,#392242),(#392243,#392244,#392245),
(#392246,#392247,#392248),(#392249,#392250,#392251)),.UNSPECIFIED.,.F.,
 .F.,.F.)
B_SPLINE_SURFACE_WITH_KNOTS((4,4),(3,3),(1.52465930505774E-20,4.68197758448212E-5),
(0.,1.),.UNSPECIFIED.)
GEOMETRIC_REPRESENTATION_ITEM()
RATIONAL_B_SPLINE_SURFACE(((1.,0.816715621142048,1.),(1.,0.953638980025214,
1.),(1.,0.95450692540805,1.),(1.,0.816715621142054,1.)))
REPRESENTATION_ITEM('')
SURFACE()
);
#2728=(
BOUNDED_SURFACE()
B_SPLINE_SURFACE(3,2,((#392253,#392254,#392255),(#392256,#392257,#392258),
(#392259,#392260,#392261),(#392262,#392263,#392264)),.UNSPECIFIED.,.F.,
 .F.,.F.)
B_SPLINE_SURFACE_WITH_KNOTS((4,4),(3,3),(2.16840434497101E-19,9.54361881492177E-5),
(0.,1.),.UNSPECIFIED.)
GEOMETRIC_REPRESENTATION_ITEM()
RATIONAL_B_SPLINE_SURFACE(((1.,0.814339887349197,1.),(1.,0.815115959345207,
1.),(1.,0.81590758740794,1.),(1.,0.816715621142055,1.)))
REPRESENTATION_ITEM('')
SURFACE()
);
#2729=(
BOUNDED_SURFACE()
B_SPLINE_SURFACE(3,2,((#392266,#392267,#392268),(#392269,#392270,#392271),
(#392272,#392273,#392274),(#392275,#392276,#392277)),.UNSPECIFIED.,.F.,
 .F.,.F.)
B_SPLINE_SURFACE_WITH_KNOTS((4,4),(3,3),(-3.39528393502276E-6,3.73481232852735E-5),
(-0.00165018033333829,1.),.UNSPECIFIED.)
GEOMETRIC_REPRESENTATION_ITEM()
RATIONAL_B_SPLINE_SURFACE(((1.00048354385567,0.8534875716604,1.),(1.00047110510922,
0.857256476851447,1.),(1.00053193201109,0.838826096655876,1.),(1.00063970687728,
0.806170615310078,1.)))
REPRESENTATION_ITEM('')
SURFACE()
);
#2730=(
BOUNDED_SURFACE()
B_SPLINE_SURFACE(3,2,((#392281,#392282,#392283),(#392284,#392285,#392286),
(#392287,#392288,#392289),(#392290,#392291,#392292)),.UNSPECIFIED.,.F.,
 .F.,.F.)
B_SPLINE_SURFACE_WITH_KNOTS((4,4),(3,3),(2.0299386923051E-5,5.39756952687117E-5),
(-0.00011628106978846,1.),.UNSPECIFIED.)
GEOMETRIC_REPRESENTATION_ITEM()
RATIONAL_B_SPLINE_SURFACE(((1.00001770479728,0.92387068114302,1.),(1.00001014104058,
0.95639427554344,1.),(1.00002037300276,0.912397594905636,1.),(1.00003390859465,
0.85419555086975,1.)))
REPRESENTATION_ITEM('')
SURFACE()
);
#2731=(
BOUNDED_SURFACE()
B_SPLINE_SURFACE(3,2,((#392385,#392386,#392387),(#392388,#392389,#392390),
(#392391,#392392,#392393),(#392394,#392395,#392396)),.UNSPECIFIED.,.F.,
 .F.,.F.)
B_SPLINE_SURFACE_WITH_KNOTS((4,4),(3,3),(0.00135801595889393,0.00148409170619832),
(0.,1.),.UNSPECIFIED.)
GEOMETRIC_REPRESENTATION_ITEM()
RATIONAL_B_SPLINE_SURFACE(((1.,0.818301933966443,1.),(1.,0.817226613172348,
1.),(1.,0.816179643373948,1.),(1.,0.815159387863653,1.)))
REPRESENTATION_ITEM('')
SURFACE()
);
#2732=(
BOUNDED_SURFACE()
B_SPLINE_SURFACE(3,2,((#392435,#392436,#392437),(#392438,#392439,#392440),
(#392441,#392442,#392443),(#392444,#392445,#392446)),.UNSPECIFIED.,.F.,
 .F.,.F.)
B_SPLINE_SURFACE_WITH_KNOTS((4,4),(3,3),(-1.54744435122077E-6,1.54744435122075E-5),
(-0.0151698983695553,1.01516989835249),.UNSPECIFIED.)
GEOMETRIC_REPRESENTATION_ITEM()
RATIONAL_B_SPLINE_SURFACE(((1.0201838247396,0.324498219413675,1.02018382471655),
(1.00401234489024,0.865716921710634,1.00401234488566),(1.00033622856797,
0.988747276629691,1.00033622856759),(1.,1.,1.)))
REPRESENTATION_ITEM('')
SURFACE()
);
#2733=(
BOUNDED_SURFACE()
B_SPLINE_SURFACE(3,2,((#392448,#392449,#392450),(#392451,#392452,#392453),
(#392454,#392455,#392456),(#392457,#392458,#392459)),.UNSPECIFIED.,.F.,
 .F.,.F.)
B_SPLINE_SURFACE_WITH_KNOTS((4,4),(3,3),(0.00137194782501028,0.00149814269699235),
(0.,1.),.UNSPECIFIED.)
GEOMETRIC_REPRESENTATION_ITEM()
RATIONAL_B_SPLINE_SURFACE(((1.,0.815158509402309,1.),(1.,0.816179044148166,
1.),(1.,0.81722630811991,1.),(1.,0.818301939488811,1.)))
REPRESENTATION_ITEM('')
SURFACE()
);
#2734=(
BOUNDED_SURFACE()
B_SPLINE_SURFACE(3,2,((#392503,#392504,#392505),(#392506,#392507,#392508),
(#392509,#392510,#392511),(#392512,#392513,#392514)),.UNSPECIFIED.,.F.,
 .F.,.F.)
B_SPLINE_SURFACE_WITH_KNOTS((4,4),(3,3),(1.55009486301137E-5,4.92065510474435E-5),
(-8.13759514726279E-5,1.),.UNSPECIFIED.)
GEOMETRIC_REPRESENTATION_ITEM()
RATIONAL_B_SPLINE_SURFACE(((1.00002372912335,0.854200639599686,1.),(1.00001423585993,
0.91253030118053,1.),(1.00000710550471,0.956341495377435,1.),(1.00001238975908,
0.923873338137022,1.)))
REPRESENTATION_ITEM('')
SURFACE()
);
#2735=(
BOUNDED_SURFACE()
B_SPLINE_SURFACE(3,2,((#392518,#392519,#392520),(#392521,#392522,#392523),
(#392524,#392525,#392526),(#392527,#392528,#392529)),.UNSPECIFIED.,.F.,
 .F.,.F.)
B_SPLINE_SURFACE_WITH_KNOTS((4,4),(3,3),(-3.39934179457794E-6,3.73927597403566E-5),
(-0.00186004067473901,1.00069373317458),.UNSPECIFIED.)
GEOMETRIC_REPRESENTATION_ITEM()
RATIONAL_B_SPLINE_SURFACE(((1.00072100136076,0.806051963875218,1.00026859642698),
(1.00060048440172,0.838470803558506,1.00022369994502),(1.00053106448811,
0.857144632272285,1.00019783877225),(1.00054515072869,0.853355459538985,
1.00020308635442)))
REPRESENTATION_ITEM('')
SURFACE()
);
#2736=(
BOUNDED_SURFACE()
B_SPLINE_SURFACE(3,2,((#392531,#392532,#392533),(#392534,#392535,#392536),
(#392537,#392538,#392539),(#392540,#392541,#392542)),.UNSPECIFIED.,.F.,
 .F.,.F.)
B_SPLINE_SURFACE_WITH_KNOTS((4,4),(3,3),(1.0842021724855E-19,9.54361881492175E-5),
(0.,1.),.UNSPECIFIED.)
GEOMETRIC_REPRESENTATION_ITEM()
RATIONAL_B_SPLINE_SURFACE(((1.,0.816715621142047,1.),(1.,0.815907587407942,
1.),(1.,0.815115959345205,1.),(1.,0.814339887349193,1.)))
REPRESENTATION_ITEM('')
SURFACE()
);
#2737=(
BOUNDED_SURFACE()
B_SPLINE_SURFACE(3,2,((#392544,#392545,#392546),(#392547,#392548,#392549),
(#392550,#392551,#392552),(#392553,#392554,#392555)),.UNSPECIFIED.,.F.,
 .F.,.F.)
B_SPLINE_SURFACE_WITH_KNOTS((4,4),(3,3),(2.71050543121376E-19,4.68197758448202E-5),
(0.,1.),.UNSPECIFIED.)
GEOMETRIC_REPRESENTATION_ITEM()
RATIONAL_B_SPLINE_SURFACE(((1.,0.81671562114206,1.),(1.,0.953638980025188,
1.),(1.,0.954506925408073,1.),(1.,0.81671562114205,1.)))
REPRESENTATION_ITEM('')
SURFACE()
);
#2738=(
BOUNDED_SURFACE()
B_SPLINE_SURFACE(3,2,((#392557,#392558,#392559),(#392560,#392561,#392562),
(#392563,#392564,#392565),(#392566,#392567,#392568)),.UNSPECIFIED.,.F.,
 .F.,.F.)
B_SPLINE_SURFACE_WITH_KNOTS((4,4),(3,3),(2.16840434497101E-19,9.54361881492178E-5),
(0.,1.),.UNSPECIFIED.)
GEOMETRIC_REPRESENTATION_ITEM()
RATIONAL_B_SPLINE_SURFACE(((1.,0.814339887349199,1.),(1.,0.815115959345194,
1.),(1.,0.81590758740794,1.),(1.,0.816715621142048,1.)))
REPRESENTATION_ITEM('')
SURFACE()
);
#2739=(
BOUNDED_SURFACE()
B_SPLINE_SURFACE(3,2,((#392570,#392571,#392572),(#392573,#392574,#392575),
(#392576,#392577,#392578),(#392579,#392580,#392581)),.UNSPECIFIED.,.F.,
 .F.,.F.)
B_SPLINE_SURFACE_WITH_KNOTS((4,4),(3,3),(-3.39528393502482E-6,3.73481232852722E-5),
(-0.00165018033345345,1.),.UNSPECIFIED.)
GEOMETRIC_REPRESENTATION_ITEM()
RATIONAL_B_SPLINE_SURFACE(((1.0004835438557,0.853487571660372,1.),(1.00047110510926,
0.857256476851432,1.),(1.00053193201113,0.838826096655844,1.),(1.00063970687732,
0.806170615310062,1.)))
REPRESENTATION_ITEM('')
SURFACE()
);
#2740=(
BOUNDED_SURFACE()
B_SPLINE_SURFACE(3,2,((#392585,#392586,#392587),(#392588,#392589,#392590),
(#392591,#392592,#392593),(#392594,#392595,#392596)),.UNSPECIFIED.,.F.,
 .F.,.F.)
B_SPLINE_SURFACE_WITH_KNOTS((4,4),(3,3),(2.02993869230509E-5,5.39756952687131E-5),
(-0.000116281070764672,1.),.UNSPECIFIED.)
GEOMETRIC_REPRESENTATION_ITEM()
RATIONAL_B_SPLINE_SURFACE(((1.00001770479743,0.923870681142944,1.),(1.00001014104066,
0.956394275543422,1.),(1.00002037300293,0.912397594905522,1.),(1.00003390859493,
0.854195550869619,1.)))
REPRESENTATION_ITEM('')
SURFACE()
);
#2741=(
BOUNDED_SURFACE()
B_SPLINE_SURFACE(3,2,((#392689,#392690,#392691),(#392692,#392693,#392694),
(#392695,#392696,#392697),(#392698,#392699,#392700)),.UNSPECIFIED.,.F.,
 .F.,.F.)
B_SPLINE_SURFACE_WITH_KNOTS((4,4),(3,3),(0.00135801595889393,0.00148409170619832),
(0.,1.),.UNSPECIFIED.)
GEOMETRIC_REPRESENTATION_ITEM()
RATIONAL_B_SPLINE_SURFACE(((1.,0.818301933966439,1.),(1.,0.817226613172351,
1.),(1.,0.816179643373943,1.),(1.,0.81515938786366,1.)))
REPRESENTATION_ITEM('')
SURFACE()
);
#2742=(
BOUNDED_SURFACE()
B_SPLINE_SURFACE(3,2,((#392739,#392740,#392741),(#392742,#392743,#392744),
(#392745,#392746,#392747),(#392748,#392749,#392750)),.UNSPECIFIED.,.F.,
 .F.,.F.)
B_SPLINE_SURFACE_WITH_KNOTS((4,4),(3,3),(-1.54744435122084E-6,1.54744435122079E-5),
(-0.0151698983650642,1.),.UNSPECIFIED.)
GEOMETRIC_REPRESENTATION_ITEM()
RATIONAL_B_SPLINE_SURFACE(((1.02018382473354,0.334740937354608,1.),(1.00401234488904,
0.867753072812928,1.),(1.00033622856787,0.988917903080853,1.),(1.,1.,1.)))
REPRESENTATION_ITEM('')
SURFACE()
);
#2743=(
BOUNDED_SURFACE()
B_SPLINE_SURFACE(3,2,((#392752,#392753,#392754),(#392755,#392756,#392757),
(#392758,#392759,#392760),(#392761,#392762,#392763)),.UNSPECIFIED.,.F.,
 .F.,.F.)
B_SPLINE_SURFACE_WITH_KNOTS((4,4),(3,3),(0.00137194782501028,0.00149814269699235),
(0.,1.),.UNSPECIFIED.)
GEOMETRIC_REPRESENTATION_ITEM()
RATIONAL_B_SPLINE_SURFACE(((1.,0.81515850940232,1.),(1.,0.81617904414816,
1.),(1.,0.817226308119934,1.),(1.,0.818301939488798,1.)))
REPRESENTATION_ITEM('')
SURFACE()
);
#2744=(
BOUNDED_SURFACE()
B_SPLINE_SURFACE(3,2,((#392807,#392808,#392809),(#392810,#392811,#392812),
(#392813,#392814,#392815),(#392816,#392817,#392818)),.UNSPECIFIED.,.F.,
 .F.,.F.)
B_SPLINE_SURFACE_WITH_KNOTS((4,4),(3,3),(1.55009486301137E-5,4.92065510474422E-5),
(-8.13759512240223E-5,1.),.UNSPECIFIED.)
GEOMETRIC_REPRESENTATION_ITEM()
RATIONAL_B_SPLINE_SURFACE(((1.00002372912328,0.854200639599726,1.),(1.00001423585989,
0.912530301180556,1.),(1.00000710550469,0.956341495377445,1.),(1.00001238975904,
0.923873338137043,1.)))
REPRESENTATION_ITEM('')
SURFACE()
);
#2745=(
BOUNDED_SURFACE()
B_SPLINE_SURFACE(3,2,((#392822,#392823,#392824),(#392825,#392826,#392827),
(#392828,#392829,#392830),(#392831,#392832,#392833)),.UNSPECIFIED.,.F.,
 .F.,.F.)
B_SPLINE_SURFACE_WITH_KNOTS((4,4),(3,3),(-3.39934179457808E-6,3.73927597403565E-5),
(-0.00186004067398835,1.00069373317426),.UNSPECIFIED.)
GEOMETRIC_REPRESENTATION_ITEM()
RATIONAL_B_SPLINE_SURFACE(((1.00072100136047,0.806051963875403,1.00026859642685),
(1.00060048440148,0.838470803558706,1.00022369994491),(1.00053106448789,
0.857144632272425,1.00019783877215),(1.00054515072846,0.853355459539151,
1.00020308635433)))
REPRESENTATION_ITEM('')
SURFACE()
);
#2746=(
BOUNDED_SURFACE()
B_SPLINE_SURFACE(3,2,((#392835,#392836,#392837),(#392838,#392839,#392840),
(#392841,#392842,#392843),(#392844,#392845,#392846)),.UNSPECIFIED.,.F.,
 .F.,.F.)
B_SPLINE_SURFACE_WITH_KNOTS((4,4),(3,3),(1.62630325872826E-19,9.54361881492174E-5),
(0.,1.),.UNSPECIFIED.)
GEOMETRIC_REPRESENTATION_ITEM()
RATIONAL_B_SPLINE_SURFACE(((1.,0.81671562114205,1.),(1.,0.815907587407942,
1.),(1.,0.815115959345204,1.),(1.,0.814339887349196,1.)))
REPRESENTATION_ITEM('')
SURFACE()
);
#2747=(
BOUNDED_SURFACE()
B_SPLINE_SURFACE(3,2,((#392848,#392849,#392850),(#392851,#392852,#392853),
(#392854,#392855,#392856),(#392857,#392858,#392859)),.UNSPECIFIED.,.F.,
 .F.,.F.)
B_SPLINE_SURFACE_WITH_KNOTS((4,4),(3,3),(-4.67562186884374E-19,4.68197758448209E-5),
(0.,1.),.UNSPECIFIED.)
GEOMETRIC_REPRESENTATION_ITEM()
RATIONAL_B_SPLINE_SURFACE(((1.,0.816715621142041,1.),(1.,0.953638980025197,
1.),(1.,0.954506925408066,1.),(1.,0.816715621142053,1.)))
REPRESENTATION_ITEM('')
SURFACE()
);
#2748=(
BOUNDED_SURFACE()
B_SPLINE_SURFACE(3,2,((#392861,#392862,#392863),(#392864,#392865,#392866),
(#392867,#392868,#392869),(#392870,#392871,#392872)),.UNSPECIFIED.,.F.,
 .F.,.F.)
B_SPLINE_SURFACE_WITH_KNOTS((4,4),(3,3),(0.,9.54361881492174E-5),(0.,1.),
 .UNSPECIFIED.)
GEOMETRIC_REPRESENTATION_ITEM()
RATIONAL_B_SPLINE_SURFACE(((1.,0.814339887349195,1.),(1.,0.815115959345201,
1.),(1.,0.815907587407948,1.),(1.,0.816715621142047,1.)))
REPRESENTATION_ITEM('')
SURFACE()
);
#2749=(
BOUNDED_SURFACE()
B_SPLINE_SURFACE(3,2,((#392874,#392875,#392876),(#392877,#392878,#392879),
(#392880,#392881,#392882),(#392883,#392884,#392885)),.UNSPECIFIED.,.F.,
 .F.,.F.)
B_SPLINE_SURFACE_WITH_KNOTS((4,4),(3,3),(-3.39528393502486E-6,3.73481232852734E-5),
(-0.00165018033326623,1.),.UNSPECIFIED.)
GEOMETRIC_REPRESENTATION_ITEM()
RATIONAL_B_SPLINE_SURFACE(((1.00048354385565,0.853487571660407,1.),(1.0004711051092,
0.857256476851465,1.),(1.00053193201107,0.838826096655872,1.),(1.00063970687725,
0.806170615310097,1.)))
REPRESENTATION_ITEM('')
SURFACE()
);
#2750=(
BOUNDED_SURFACE()
B_SPLINE_SURFACE(3,2,((#392889,#392890,#392891),(#392892,#392893,#392894),
(#392895,#392896,#392897),(#392898,#392899,#392900)),.UNSPECIFIED.,.F.,
 .F.,.F.)
B_SPLINE_SURFACE_WITH_KNOTS((4,4),(3,3),(2.02993869230514E-5,5.39756952687133E-5),
(-0.000116281069893436,1.),.UNSPECIFIED.)
GEOMETRIC_REPRESENTATION_ITEM()
RATIONAL_B_SPLINE_SURFACE(((1.00001770479729,0.923870681143013,1.),(1.00001014104059,
0.956394275543435,1.),(1.00002037300278,0.912397594905628,1.),(1.00003390859468,
0.85419555086974,1.)))
REPRESENTATION_ITEM('')
SURFACE()
);
#2751=(
BOUNDED_SURFACE()
B_SPLINE_SURFACE(3,2,((#392993,#392994,#392995),(#392996,#392997,#392998),
(#392999,#393000,#393001),(#393002,#393003,#393004)),.UNSPECIFIED.,.F.,
 .F.,.F.)
B_SPLINE_SURFACE_WITH_KNOTS((4,4),(3,3),(0.00135801595889393,0.00148409170619832),
(0.,1.),.UNSPECIFIED.)
GEOMETRIC_REPRESENTATION_ITEM()
RATIONAL_B_SPLINE_SURFACE(((1.,0.818301933966445,1.),(1.,0.817226613172342,
1.),(1.,0.816179643373954,1.),(1.,0.815159387863652,1.)))
REPRESENTATION_ITEM('')
SURFACE()
);
#2752=(
BOUNDED_SURFACE()
B_SPLINE_SURFACE(3,2,((#393043,#393044,#393045),(#393046,#393047,#393048),
(#393049,#393050,#393051),(#393052,#393053,#393054)),.UNSPECIFIED.,.F.,
 .F.,.F.)
B_SPLINE_SURFACE_WITH_KNOTS((4,4),(3,3),(-1.54744435122082E-6,1.54744435122082E-5),
(-0.015169898361537,1.01516989836005),.UNSPECIFIED.)
GEOMETRIC_REPRESENTATION_ITEM()
RATIONAL_B_SPLINE_SURFACE(((1.02018382472877,0.324498219414025,1.02018382472676),
(1.00401234488809,0.865716921710696,1.00401234488769),(1.00033622856779,
0.988747276629713,1.00033622856776),(1.,1.,1.)))
REPRESENTATION_ITEM('')
SURFACE()
);
#2753=(
BOUNDED_SURFACE()
B_SPLINE_SURFACE(3,2,((#393056,#393057,#393058),(#393059,#393060,#393061),
(#393062,#393063,#393064),(#393065,#393066,#393067)),.UNSPECIFIED.,.F.,
 .F.,.F.)
B_SPLINE_SURFACE_WITH_KNOTS((4,4),(3,3),(0.00137194782501028,0.00149814269699235),
(0.,1.),.UNSPECIFIED.)
GEOMETRIC_REPRESENTATION_ITEM()
RATIONAL_B_SPLINE_SURFACE(((1.,0.815158509402316,1.),(1.,0.816179044148173,
1.),(1.,0.817226308119922,1.),(1.,0.818301939488805,1.)))
REPRESENTATION_ITEM('')
SURFACE()
);
#2754=(
BOUNDED_SURFACE()
B_SPLINE_SURFACE(3,2,((#393111,#393112,#393113),(#393114,#393115,#393116),
(#393117,#393118,#393119),(#393120,#393121,#393122)),.UNSPECIFIED.,.F.,
 .F.,.F.)
B_SPLINE_SURFACE_WITH_KNOTS((4,4),(3,3),(1.55009486301137E-5,4.92065510474434E-5),
(-8.13759516301738E-5,1.),.UNSPECIFIED.)
GEOMETRIC_REPRESENTATION_ITEM()
RATIONAL_B_SPLINE_SURFACE(((1.0000237291234,0.854200639599662,1.),(1.00001423585996,
0.912530301180526,1.),(1.00000710550472,0.956341495377425,1.),(1.00001238975911,
0.92387333813701,1.)))
REPRESENTATION_ITEM('')
SURFACE()
);
#2755=(
BOUNDED_SURFACE()
B_SPLINE_SURFACE(3,2,((#393126,#393127,#393128),(#393129,#393130,#393131),
(#393132,#393133,#393134),(#393135,#393136,#393137)),.UNSPECIFIED.,.F.,
 .F.,.F.)
B_SPLINE_SURFACE_WITH_KNOTS((4,4),(3,3),(-3.39934179457814E-6,3.73927597403564E-5),
(-0.00186004067407364,1.00069373317444),.UNSPECIFIED.)
GEOMETRIC_REPRESENTATION_ITEM()
RATIONAL_B_SPLINE_SURFACE(((1.0007210013605,0.806051963875375,1.00026859642693),
(1.0006004844015,0.838470803558624,1.00022369994497),(1.00053106448791,
0.857144632272406,1.00019783877221),(1.00054515072849,0.853355459539101,
1.00020308635438)))
REPRESENTATION_ITEM('')
SURFACE()
);
#2756=(
BOUNDED_SURFACE()
B_SPLINE_SURFACE(3,2,((#393139,#393140,#393141),(#393142,#393143,#393144),
(#393145,#393146,#393147),(#393148,#393149,#393150)),.UNSPECIFIED.,.F.,
 .F.,.F.)
B_SPLINE_SURFACE_WITH_KNOTS((4,4),(3,3),(1.0842021724855E-19,9.54361881492174E-5),
(0.,1.),.UNSPECIFIED.)
GEOMETRIC_REPRESENTATION_ITEM()
RATIONAL_B_SPLINE_SURFACE(((1.,0.816715621142047,1.),(1.,0.815907587407939,
1.),(1.,0.815115959345212,1.),(1.,0.814339887349189,1.)))
REPRESENTATION_ITEM('')
SURFACE()
);
#2757=(
BOUNDED_SURFACE()
B_SPLINE_SURFACE(3,2,((#393152,#393153,#393154),(#393155,#393156,#393157),
(#393158,#393159,#393160),(#393161,#393162,#393163)),.UNSPECIFIED.,.F.,
 .F.,.F.)
B_SPLINE_SURFACE_WITH_KNOTS((4,4),(3,3),(1.01643953670516E-20,4.68197758448205E-5),
(0.,1.),.UNSPECIFIED.)
GEOMETRIC_REPRESENTATION_ITEM()
RATIONAL_B_SPLINE_SURFACE(((1.,0.816715621142046,1.),(1.,0.953638980025195,
1.),(1.,0.954506925408074,1.),(1.,0.81671562114205,1.)))
REPRESENTATION_ITEM('')
SURFACE()
);
#2758=(
BOUNDED_SURFACE()
B_SPLINE_SURFACE(3,2,((#393165,#393166,#393167),(#393168,#393169,#393170),
(#393171,#393172,#393173),(#393174,#393175,#393176)),.UNSPECIFIED.,.F.,
 .F.,.F.)
B_SPLINE_SURFACE_WITH_KNOTS((4,4),(3,3),(0.,9.54361881492176E-5),(0.,1.),
 .UNSPECIFIED.)
GEOMETRIC_REPRESENTATION_ITEM()
RATIONAL_B_SPLINE_SURFACE(((1.,0.814339887349195,1.),(1.,0.8151159593452,
1.),(1.,0.815907587407945,1.),(1.,0.816715621142046,1.)))
REPRESENTATION_ITEM('')
SURFACE()
);
#2759=(
BOUNDED_SURFACE()
B_SPLINE_SURFACE(3,2,((#393178,#393179,#393180),(#393181,#393182,#393183),
(#393184,#393185,#393186),(#393187,#393188,#393189)),.UNSPECIFIED.,.F.,
 .F.,.F.)
B_SPLINE_SURFACE_WITH_KNOTS((4,4),(3,3),(-3.39528393502486E-6,3.73481232852736E-5),
(-0.00165018033290617,1.),.UNSPECIFIED.)
GEOMETRIC_REPRESENTATION_ITEM()
RATIONAL_B_SPLINE_SURFACE(((1.00048354385554,0.853487571660446,1.),(1.0004711051091,
0.857256476851517,1.),(1.00053193201095,0.838826096655916,1.),(1.00063970687711,
0.806170615310169,1.)))
REPRESENTATION_ITEM('')
SURFACE()
);
#2760=(
BOUNDED_SURFACE()
B_SPLINE_SURFACE(3,2,((#393193,#393194,#393195),(#393196,#393197,#393198),
(#393199,#393200,#393201),(#393202,#393203,#393204)),.UNSPECIFIED.,.F.,
 .F.,.F.)
B_SPLINE_SURFACE_WITH_KNOTS((4,4),(3,3),(2.02993869230511E-5,5.39756952686905E-5),
(-0.000116281070107644,1.),.UNSPECIFIED.)
GEOMETRIC_REPRESENTATION_ITEM()
RATIONAL_B_SPLINE_SURFACE(((1.00001770479733,0.923870681142993,1.),(1.00001014104061,
0.956394275543421,1.),(1.00002037300282,0.912397594905653,1.),(1.00003390859474,
0.854195550869826,1.)))
REPRESENTATION_ITEM('')
SURFACE()
);
#2761=(
BOUNDED_SURFACE()
B_SPLINE_SURFACE(3,2,((#393297,#393298,#393299),(#393300,#393301,#393302),
(#393303,#393304,#393305),(#393306,#393307,#393308)),.UNSPECIFIED.,.F.,
 .F.,.F.)
B_SPLINE_SURFACE_WITH_KNOTS((4,4),(3,3),(0.00135801595889393,0.00148409170619832),
(0.,1.),.UNSPECIFIED.)
GEOMETRIC_REPRESENTATION_ITEM()
RATIONAL_B_SPLINE_SURFACE(((1.,0.818301933966446,1.),(1.,0.817226613172339,
1.),(1.,0.816179643373962,1.),(1.,0.815159387863655,1.)))
REPRESENTATION_ITEM('')
SURFACE()
);
#2762=(
BOUNDED_SURFACE()
B_SPLINE_SURFACE(3,2,((#393347,#393348,#393349),(#393350,#393351,#393352),
(#393353,#393354,#393355),(#393356,#393357,#393358)),.UNSPECIFIED.,.F.,
 .F.,.F.)
B_SPLINE_SURFACE_WITH_KNOTS((4,4),(3,3),(-1.5474443512208E-6,1.54744435122079E-5),
(-0.0151698983606426,1.01516989836206),.UNSPECIFIED.)
GEOMETRIC_REPRESENTATION_ITEM()
RATIONAL_B_SPLINE_SURFACE(((1.02018382472757,0.32449821941319,1.02018382472948),
(1.00401234488785,0.865716921710622,1.00401234488823),(1.00033622856777,
0.988747276629658,1.00033622856781),(1.,1.,1.)))
REPRESENTATION_ITEM('')
SURFACE()
);
#2763=(
BOUNDED_SURFACE()
B_SPLINE_SURFACE(3,2,((#393360,#393361,#393362),(#393363,#393364,#393365),
(#393366,#393367,#393368),(#393369,#393370,#393371)),.UNSPECIFIED.,.F.,
 .F.,.F.)
B_SPLINE_SURFACE_WITH_KNOTS((4,4),(3,3),(0.00137194782501028,0.00149814269699235),
(0.,1.),.UNSPECIFIED.)
GEOMETRIC_REPRESENTATION_ITEM()
RATIONAL_B_SPLINE_SURFACE(((1.,0.815158509402323,1.),(1.,0.816179044148176,
1.),(1.,0.817226308119921,1.),(1.,0.818301939488808,1.)))
REPRESENTATION_ITEM('')
SURFACE()
);
#2764=(
BOUNDED_SURFACE()
B_SPLINE_SURFACE(3,2,((#393415,#393416,#393417),(#393418,#393419,#393420),
(#393421,#393422,#393423),(#393424,#393425,#393426)),.UNSPECIFIED.,.F.,
 .F.,.F.)
B_SPLINE_SURFACE_WITH_KNOTS((4,4),(3,3),(1.55009486301137E-5,4.92065510474429E-5),
(-8.13759515703415E-5,1.),.UNSPECIFIED.)
GEOMETRIC_REPRESENTATION_ITEM()
RATIONAL_B_SPLINE_SURFACE(((1.00002372912338,0.854200639599671,1.),(1.00001423585995,
0.912530301180536,1.),(1.00000710550472,0.956341495377421,1.),(1.0000123897591,
0.923873338137016,1.)))
REPRESENTATION_ITEM('')
SURFACE()
);
#2765=(
BOUNDED_SURFACE()
B_SPLINE_SURFACE(3,2,((#393430,#393431,#393432),(#393433,#393434,#393435),
(#393436,#393437,#393438),(#393439,#393440,#393441)),.UNSPECIFIED.,.F.,
 .F.,.F.)
B_SPLINE_SURFACE_WITH_KNOTS((4,4),(3,3),(-3.39934179457827E-6,3.73927597403564E-5),
(-0.00186004067416749,1.00069373317441),.UNSPECIFIED.)
GEOMETRIC_REPRESENTATION_ITEM()
RATIONAL_B_SPLINE_SURFACE(((1.00072100136054,0.806051963875334,1.00026859642691),
(1.00060048440153,0.838470803558673,1.00022369994496),(1.00053106448794,
0.857144632272363,1.0001978387722),(1.00054515072852,0.853355459539107,
1.00020308635437)))
REPRESENTATION_ITEM('')
SURFACE()
);
#2766=(
BOUNDED_SURFACE()
B_SPLINE_SURFACE(3,2,((#393443,#393444,#393445),(#393446,#393447,#393448),
(#393449,#393450,#393451),(#393452,#393453,#393454)),.UNSPECIFIED.,.F.,
 .F.,.F.)
B_SPLINE_SURFACE_WITH_KNOTS((4,4),(3,3),(5.42101086242752E-20,9.54361881492173E-5),
(0.,1.),.UNSPECIFIED.)
GEOMETRIC_REPRESENTATION_ITEM()
RATIONAL_B_SPLINE_SURFACE(((1.,0.816715621142053,1.),(1.,0.815907587407943,
1.),(1.,0.815115959345204,1.),(1.,0.814339887349193,1.)))
REPRESENTATION_ITEM('')
SURFACE()
);
#2767=(
BOUNDED_SURFACE()
B_SPLINE_SURFACE(3,2,((#393456,#393457,#393458),(#393459,#393460,#393461),
(#393462,#393463,#393464),(#393465,#393466,#393467)),.UNSPECIFIED.,.F.,
 .F.,.F.)
B_SPLINE_SURFACE_WITH_KNOTS((4,4),(3,3),(-7.45388993583784E-20,4.68197758448203E-5),
(0.,1.),.UNSPECIFIED.)
GEOMETRIC_REPRESENTATION_ITEM()
RATIONAL_B_SPLINE_SURFACE(((1.,0.816715621142046,1.),(1.,0.953638980025215,
1.),(1.,0.954506925408046,1.),(1.,0.816715621142056,1.)))
REPRESENTATION_ITEM('')
SURFACE()
);
#2768=(
BOUNDED_SURFACE()
B_SPLINE_SURFACE(3,2,((#393469,#393470,#393471),(#393472,#393473,#393474),
(#393475,#393476,#393477),(#393478,#393479,#393480)),.UNSPECIFIED.,.F.,
 .F.,.F.)
B_SPLINE_SURFACE_WITH_KNOTS((4,4),(3,3),(-1.0842021724855E-19,9.54361881492176E-5),
(0.,1.),.UNSPECIFIED.)
GEOMETRIC_REPRESENTATION_ITEM()
RATIONAL_B_SPLINE_SURFACE(((1.,0.814339887349194,1.),(1.,0.815115959345214,
1.),(1.,0.81590758740794,1.),(1.,0.816715621142046,1.)))
REPRESENTATION_ITEM('')
SURFACE()
);
#2769=(
BOUNDED_SURFACE()
B_SPLINE_SURFACE(3,2,((#393482,#393483,#393484),(#393485,#393486,#393487),
(#393488,#393489,#393490),(#393491,#393492,#393493)),.UNSPECIFIED.,.F.,
 .F.,.F.)
B_SPLINE_SURFACE_WITH_KNOTS((4,4),(3,3),(-3.39528393502488E-6,3.73481232852734E-5),
(-0.00165018033329553,1.),.UNSPECIFIED.)
GEOMETRIC_REPRESENTATION_ITEM()
RATIONAL_B_SPLINE_SURFACE(((1.00048354385566,0.85348757166039,1.),(1.00047110510921,
0.857256476851485,1.),(1.00053193201108,0.838826096655847,1.),(1.00063970687726,
0.8061706153101,1.)))
REPRESENTATION_ITEM('')
SURFACE()
);
#2770=(
BOUNDED_SURFACE()
B_SPLINE_SURFACE(3,2,((#393497,#393498,#393499),(#393500,#393501,#393502),
(#393503,#393504,#393505),(#393506,#393507,#393508)),.UNSPECIFIED.,.F.,
 .F.,.F.)
B_SPLINE_SURFACE_WITH_KNOTS((4,4),(3,3),(2.02993869230509E-5,5.39756952686905E-5),
(-0.000116281069641126,1.),.UNSPECIFIED.)
GEOMETRIC_REPRESENTATION_ITEM()
RATIONAL_B_SPLINE_SURFACE(((1.00001770479726,0.923870681143033,1.),(1.00001014104056,
0.95639427554342,1.),(1.00002037300274,0.912397594905708,1.),(1.00003390859461,
0.854195550869891,1.)))
REPRESENTATION_ITEM('')
SURFACE()
);
#2771=(
BOUNDED_SURFACE()
B_SPLINE_SURFACE(3,2,((#393601,#393602,#393603),(#393604,#393605,#393606),
(#393607,#393608,#393609),(#393610,#393611,#393612)),.UNSPECIFIED.,.F.,
 .F.,.F.)
B_SPLINE_SURFACE_WITH_KNOTS((4,4),(3,3),(0.00135801595889393,0.00148409170619832),
(0.,1.),.UNSPECIFIED.)
GEOMETRIC_REPRESENTATION_ITEM()
RATIONAL_B_SPLINE_SURFACE(((1.,0.818301933966445,1.),(1.,0.817226613172349,
1.),(1.,0.816179643373947,1.),(1.,0.815159387863652,1.)))
REPRESENTATION_ITEM('')
SURFACE()
);
#2772=(
BOUNDED_SURFACE()
B_SPLINE_SURFACE(3,2,((#393651,#393652,#393653),(#393654,#393655,#393656),
(#393657,#393658,#393659),(#393660,#393661,#393662)),.UNSPECIFIED.,.F.,
 .F.,.F.)
B_SPLINE_SURFACE_WITH_KNOTS((4,4),(3,3),(-1.54744435122075E-6,1.54744435122076E-5),
(-0.0151698983615748,1.),.UNSPECIFIED.)
GEOMETRIC_REPRESENTATION_ITEM()
RATIONAL_B_SPLINE_SURFACE(((1.02018382472883,0.334740937356857,1.),(1.0040123448881,
0.867753072813479,1.),(1.00033622856779,0.988917903080847,1.),(1.,1.,1.)))
REPRESENTATION_ITEM('')
SURFACE()
);
#2773=(
BOUNDED_SURFACE()
B_SPLINE_SURFACE(3,2,((#393664,#393665,#393666),(#393667,#393668,#393669),
(#393670,#393671,#393672),(#393673,#393674,#393675)),.UNSPECIFIED.,.F.,
 .F.,.F.)
B_SPLINE_SURFACE_WITH_KNOTS((4,4),(3,3),(0.00137194782501028,0.00149814269699235),
(0.,1.),.UNSPECIFIED.)
GEOMETRIC_REPRESENTATION_ITEM()
RATIONAL_B_SPLINE_SURFACE(((1.,0.815158509402314,1.),(1.,0.816179044148167,
1.),(1.,0.817226308119939,1.),(1.,0.818301939488801,1.)))
REPRESENTATION_ITEM('')
SURFACE()
);
#2774=(
BOUNDED_SURFACE()
B_SPLINE_SURFACE(3,2,((#393719,#393720,#393721),(#393722,#393723,#393724),
(#393725,#393726,#393727),(#393728,#393729,#393730)),.UNSPECIFIED.,.F.,
 .F.,.F.)
B_SPLINE_SURFACE_WITH_KNOTS((4,4),(3,3),(1.55009486301137E-5,4.92065510474427E-5),
(-8.1375951387387E-5,1.),.UNSPECIFIED.)
GEOMETRIC_REPRESENTATION_ITEM()
RATIONAL_B_SPLINE_SURFACE(((1.00002372912333,0.854200639599705,1.),(1.00001423585992,
0.912530301180535,1.),(1.0000071055047,0.95634149537744,1.),(1.00001238975907,
0.923873338137029,1.)))
REPRESENTATION_ITEM('')
SURFACE()
);
#2775=(
BOUNDED_SURFACE()
B_SPLINE_SURFACE(3,2,((#393734,#393735,#393736),(#393737,#393738,#393739),
(#393740,#393741,#393742),(#393743,#393744,#393745)),.UNSPECIFIED.,.F.,
 .F.,.F.)
B_SPLINE_SURFACE_WITH_KNOTS((4,4),(3,3),(-3.39934179457817E-6,3.73927597403564E-5),
(-0.00186004067389001,1.00069373317438),.UNSPECIFIED.)
GEOMETRIC_REPRESENTATION_ITEM()
RATIONAL_B_SPLINE_SURFACE(((1.00072100136043,0.806051963875405,1.0002685964269),
(1.00060048440144,0.838470803558679,1.00022369994495),(1.00053106448786,
0.857144632272429,1.00019783877219),(1.00054515072844,0.853355459539144,
1.00020308635436)))
REPRESENTATION_ITEM('')
SURFACE()
);
#2776=(
BOUNDED_SURFACE()
B_SPLINE_SURFACE(3,2,((#393747,#393748,#393749),(#393750,#393751,#393752),
(#393753,#393754,#393755),(#393756,#393757,#393758)),.UNSPECIFIED.,.F.,
 .F.,.F.)
B_SPLINE_SURFACE_WITH_KNOTS((4,4),(3,3),(5.42101086242752E-20,9.54361881492175E-5),
(0.,1.),.UNSPECIFIED.)
GEOMETRIC_REPRESENTATION_ITEM()
RATIONAL_B_SPLINE_SURFACE(((1.,0.816715621142047,1.),(1.,0.815907587407949,
1.),(1.,0.8151159593452,1.),(1.,0.814339887349195,1.)))
REPRESENTATION_ITEM('')
SURFACE()
);
#2777=(
BOUNDED_SURFACE()
B_SPLINE_SURFACE(3,2,((#393760,#393761,#393762),(#393763,#393764,#393765),
(#393766,#393767,#393768),(#393769,#393770,#393771)),.UNSPECIFIED.,.F.,
 .F.,.F.)
B_SPLINE_SURFACE_WITH_KNOTS((4,4),(3,3),(3.55753837846806E-20,4.68197758448214E-5),
(0.,1.),.UNSPECIFIED.)
GEOMETRIC_REPRESENTATION_ITEM()
RATIONAL_B_SPLINE_SURFACE(((1.,0.816715621142045,1.),(1.,0.953638980025214,
1.),(1.,0.954506925408051,1.),(1.,0.816715621142053,1.)))
REPRESENTATION_ITEM('')
SURFACE()
);
#2778=(
BOUNDED_SURFACE()
B_SPLINE_SURFACE(3,2,((#393773,#393774,#393775),(#393776,#393777,#393778),
(#393779,#393780,#393781),(#393782,#393783,#393784)),.UNSPECIFIED.,.F.,
 .F.,.F.)
B_SPLINE_SURFACE_WITH_KNOTS((4,4),(3,3),(1.62630325872826E-19,9.54361881492177E-5),
(0.,1.),.UNSPECIFIED.)
GEOMETRIC_REPRESENTATION_ITEM()
RATIONAL_B_SPLINE_SURFACE(((1.,0.814339887349193,1.),(1.,0.81511595934521,
1.),(1.,0.815907587407938,1.),(1.,0.816715621142048,1.)))
REPRESENTATION_ITEM('')
SURFACE()
);
#2779=(
BOUNDED_SURFACE()
B_SPLINE_SURFACE(3,2,((#393786,#393787,#393788),(#393789,#393790,#393791),
(#393792,#393793,#393794),(#393795,#393796,#393797)),.UNSPECIFIED.,.F.,
 .F.,.F.)
B_SPLINE_SURFACE_WITH_KNOTS((4,4),(3,3),(-3.39528393502492E-6,3.73481232852736E-5),
(-0.00165018033285678,1.),.UNSPECIFIED.)
GEOMETRIC_REPRESENTATION_ITEM()
RATIONAL_B_SPLINE_SURFACE(((1.00048354385553,0.85348757166045,1.),(1.00047110510908,
0.857256476851541,1.),(1.00053193201094,0.838826096655928,1.),(1.00063970687709,
0.806170615310183,1.)))
REPRESENTATION_ITEM('')
SURFACE()
);
#2780=(
BOUNDED_SURFACE()
B_SPLINE_SURFACE(3,2,((#393801,#393802,#393803),(#393804,#393805,#393806),
(#393807,#393808,#393809),(#393810,#393811,#393812)),.UNSPECIFIED.,.F.,
 .F.,.F.)
B_SPLINE_SURFACE_WITH_KNOTS((4,4),(3,3),(2.02993869230514E-5,5.39756952686908E-5),
(-0.000116281069724157,1.),.UNSPECIFIED.)
GEOMETRIC_REPRESENTATION_ITEM()
RATIONAL_B_SPLINE_SURFACE(((1.00001770479727,0.923870681143026,1.),(1.00001014104057,
0.95639427554342,1.),(1.00002037300275,0.912397594905702,1.),(1.00003390859463,
0.854195550869877,1.)))
REPRESENTATION_ITEM('')
SURFACE()
);
#2781=(
BOUNDED_SURFACE()
B_SPLINE_SURFACE(3,2,((#393905,#393906,#393907),(#393908,#393909,#393910),
(#393911,#393912,#393913),(#393914,#393915,#393916)),.UNSPECIFIED.,.F.,
 .F.,.F.)
B_SPLINE_SURFACE_WITH_KNOTS((4,4),(3,3),(0.00135801595889393,0.00148409170619832),
(0.,1.),.UNSPECIFIED.)
GEOMETRIC_REPRESENTATION_ITEM()
RATIONAL_B_SPLINE_SURFACE(((1.,0.818301933966443,1.),(1.,0.817226613172343,
1.),(1.,0.816179643373959,1.),(1.,0.815159387863654,1.)))
REPRESENTATION_ITEM('')
SURFACE()
);
#2782=(
BOUNDED_SURFACE()
B_SPLINE_SURFACE(3,2,((#393955,#393956,#393957),(#393958,#393959,#393960),
(#393961,#393962,#393963),(#393964,#393965,#393966)),.UNSPECIFIED.,.F.,
 .F.,.F.)
B_SPLINE_SURFACE_WITH_KNOTS((4,4),(3,3),(-1.54744435122069E-6,1.54744435122075E-5),
(-0.0151698983646716,1.01516989835781),.UNSPECIFIED.)
GEOMETRIC_REPRESENTATION_ITEM()
RATIONAL_B_SPLINE_SURFACE(((1.02018382473301,0.324498219413436,1.02018382472374),
(1.00401234488893,0.865716921710573,1.00401234488709),(1.00033622856786,
0.988747276629695,1.00033622856771),(1.,1.,1.)))
REPRESENTATION_ITEM('')
SURFACE()
);
#2783=(
BOUNDED_SURFACE()
B_SPLINE_SURFACE(3,2,((#393968,#393969,#393970),(#393971,#393972,#393973),
(#393974,#393975,#393976),(#393977,#393978,#393979)),.UNSPECIFIED.,.F.,
 .F.,.F.)
B_SPLINE_SURFACE_WITH_KNOTS((4,4),(3,3),(0.00137194782501028,0.00149814269699235),
(0.,1.),.UNSPECIFIED.)
GEOMETRIC_REPRESENTATION_ITEM()
RATIONAL_B_SPLINE_SURFACE(((1.,0.815158509402317,1.),(1.,0.816179044148163,
1.),(1.,0.817226308119931,1.),(1.,0.818301939488807,1.)))
REPRESENTATION_ITEM('')
SURFACE()
);
#2784=(
BOUNDED_SURFACE()
B_SPLINE_SURFACE(3,2,((#394023,#394024,#394025),(#394026,#394027,#394028),
(#394029,#394030,#394031),(#394032,#394033,#394034)),.UNSPECIFIED.,.F.,
 .F.,.F.)
B_SPLINE_SURFACE_WITH_KNOTS((4,4),(3,3),(1.55009486301137E-5,4.92065510474434E-5),
(-8.13759515344749E-5,1.),.UNSPECIFIED.)
GEOMETRIC_REPRESENTATION_ITEM()
RATIONAL_B_SPLINE_SURFACE(((1.00002372912337,0.854200639599674,1.),(1.00001423585994,
0.912530301180545,1.),(1.00000710550471,0.956341495377423,1.),(1.00001238975909,
0.92387333813702,1.)))
REPRESENTATION_ITEM('')
SURFACE()
);
#2785=(
BOUNDED_SURFACE()
B_SPLINE_SURFACE(3,2,((#394038,#394039,#394040),(#394041,#394042,#394043),
(#394044,#394045,#394046),(#394047,#394048,#394049)),.UNSPECIFIED.,.F.,
 .F.,.F.)
B_SPLINE_SURFACE_WITH_KNOTS((4,4),(3,3),(-3.39934179457785E-6,3.73927597403566E-5),
(-0.00186004067389604,1.00069373317456),.UNSPECIFIED.)
GEOMETRIC_REPRESENTATION_ITEM()
RATIONAL_B_SPLINE_SURFACE(((1.00072100136043,0.80605196387536,1.00026859642697),
(1.00060048440145,0.838470803558678,1.00022369994501),(1.00053106448786,
0.857144632272387,1.00019783877224),(1.00054515072844,0.853355459539119,
1.00020308635442)))
REPRESENTATION_ITEM('')
SURFACE()
);
#2786=(
BOUNDED_SURFACE()
B_SPLINE_SURFACE(3,2,((#394051,#394052,#394053),(#394054,#394055,#394056),
(#394057,#394058,#394059),(#394060,#394061,#394062)),.UNSPECIFIED.,.F.,
 .F.,.F.)
B_SPLINE_SURFACE_WITH_KNOTS((4,4),(3,3),(-5.42101086242752E-20,9.54361881492175E-5),
(0.,1.),.UNSPECIFIED.)
GEOMETRIC_REPRESENTATION_ITEM()
RATIONAL_B_SPLINE_SURFACE(((1.,0.81671562114205,1.),(1.,0.815907587407957,
1.),(1.,0.815115959345192,1.),(1.,0.814339887349193,1.)))
REPRESENTATION_ITEM('')
SURFACE()
);
#2787=(
BOUNDED_SURFACE()
B_SPLINE_SURFACE(3,2,((#394064,#394065,#394066),(#394067,#394068,#394069),
(#394070,#394071,#394072),(#394073,#394074,#394075)),.UNSPECIFIED.,.F.,
 .F.,.F.)
B_SPLINE_SURFACE_WITH_KNOTS((4,4),(3,3),(2.79520872593919E-19,4.68197758448212E-5),
(0.,1.),.UNSPECIFIED.)
GEOMETRIC_REPRESENTATION_ITEM()
RATIONAL_B_SPLINE_SURFACE(((1.,0.81671562114205,1.),(1.,0.953638980025211,
1.),(1.,0.954506925408057,1.),(1.,0.81671562114205,1.)))
REPRESENTATION_ITEM('')
SURFACE()
);
#2788=(
BOUNDED_SURFACE()
B_SPLINE_SURFACE(3,2,((#394077,#394078,#394079),(#394080,#394081,#394082),
(#394083,#394084,#394085),(#394086,#394087,#394088)),.UNSPECIFIED.,.F.,
 .F.,.F.)
B_SPLINE_SURFACE_WITH_KNOTS((4,4),(3,3),(0.,9.54361881492179E-5),(0.,1.),
 .UNSPECIFIED.)
GEOMETRIC_REPRESENTATION_ITEM()
RATIONAL_B_SPLINE_SURFACE(((1.,0.814339887349193,1.),(1.,0.815115959345207,
1.),(1.,0.815907587407936,1.),(1.,0.81671562114205,1.)))
REPRESENTATION_ITEM('')
SURFACE()
);
#2789=(
BOUNDED_SURFACE()
B_SPLINE_SURFACE(3,2,((#394090,#394091,#394092),(#394093,#394094,#394095),
(#394096,#394097,#394098),(#394099,#394100,#394101)),.UNSPECIFIED.,.F.,
 .F.,.F.)
B_SPLINE_SURFACE_WITH_KNOTS((4,4),(3,3),(-3.39528393502486E-6,3.73481232852728E-5),
(-0.00165018033346268,1.),.UNSPECIFIED.)
GEOMETRIC_REPRESENTATION_ITEM()
RATIONAL_B_SPLINE_SURFACE(((1.00048354385571,0.853487571660363,1.),(1.00047110510926,
0.857256476851452,1.),(1.00053193201113,0.838826096655833,1.),(1.00063970687733,
0.80617061531006,1.)))
REPRESENTATION_ITEM('')
SURFACE()
);
#2790=(
BOUNDED_SURFACE()
B_SPLINE_SURFACE(3,2,((#394105,#394106,#394107),(#394108,#394109,#394110),
(#394111,#394112,#394113),(#394114,#394115,#394116)),.UNSPECIFIED.,.F.,
 .F.,.F.)
B_SPLINE_SURFACE_WITH_KNOTS((4,4),(3,3),(2.02993869230509E-5,5.39756952686905E-5),
(-0.000116281070001636,1.),.UNSPECIFIED.)
GEOMETRIC_REPRESENTATION_ITEM()
RATIONAL_B_SPLINE_SURFACE(((1.00001770479731,0.923870681143004,1.),(1.0000101410406,
0.956394275543415,1.),(1.0000203730028,0.912397594905674,1.),(1.00003390859471,
0.854195550869838,1.)))
REPRESENTATION_ITEM('')
SURFACE()
);
#2791=(
BOUNDED_SURFACE()
B_SPLINE_SURFACE(3,2,((#394209,#394210,#394211),(#394212,#394213,#394214),
(#394215,#394216,#394217),(#394218,#394219,#394220)),.UNSPECIFIED.,.F.,
 .F.,.F.)
B_SPLINE_SURFACE_WITH_KNOTS((4,4),(3,3),(0.00135801595889393,0.00148409170619832),
(0.,1.),.UNSPECIFIED.)
GEOMETRIC_REPRESENTATION_ITEM()
RATIONAL_B_SPLINE_SURFACE(((1.,0.818301933966442,1.),(1.,0.817226613172347,
1.),(1.,0.816179643373947,1.),(1.,0.815159387863655,1.)))
REPRESENTATION_ITEM('')
SURFACE()
);
#2792=(
BOUNDED_SURFACE()
B_SPLINE_SURFACE(3,2,((#394259,#394260,#394261),(#394262,#394263,#394264),
(#394265,#394266,#394267),(#394268,#394269,#394270)),.UNSPECIFIED.,.F.,
 .F.,.F.)
B_SPLINE_SURFACE_WITH_KNOTS((4,4),(3,3),(3.43048343637992E-20,1.54744435122082E-5),
(0.,1.),.UNSPECIFIED.)
GEOMETRIC_REPRESENTATION_ITEM()
RATIONAL_B_SPLINE_SURFACE(((1.,0.478041569704948,1.),(1.,0.890533857552087,
1.),(1.,0.990075913815913,1.),(1.,1.,1.)))
REPRESENTATION_ITEM('')
SURFACE()
);
#2793=(
BOUNDED_SURFACE()
B_SPLINE_SURFACE(3,2,((#394272,#394273,#394274),(#394275,#394276,#394277),
(#394278,#394279,#394280),(#394281,#394282,#394283)),.UNSPECIFIED.,.F.,
 .F.,.F.)
B_SPLINE_SURFACE_WITH_KNOTS((4,4),(3,3),(0.00137194782501028,0.00149814269699235),
(0.,1.),.UNSPECIFIED.)
GEOMETRIC_REPRESENTATION_ITEM()
RATIONAL_B_SPLINE_SURFACE(((1.,0.815158509402316,1.),(1.,0.816179044148169,
1.),(1.,0.817226308119927,1.),(1.,0.818301939488802,1.)))
REPRESENTATION_ITEM('')
SURFACE()
);
#2794=(
BOUNDED_SURFACE()
B_SPLINE_SURFACE(3,2,((#394327,#394328,#394329),(#394330,#394331,#394332),
(#394333,#394334,#394335),(#394336,#394337,#394338)),.UNSPECIFIED.,.F.,
 .F.,.F.)
B_SPLINE_SURFACE_WITH_KNOTS((4,4),(3,3),(1.55009486301137E-5,4.92065510474435E-5),
(-8.1375951522669E-5,1.),.UNSPECIFIED.)
GEOMETRIC_REPRESENTATION_ITEM()
RATIONAL_B_SPLINE_SURFACE(((1.00002372912337,0.854200639599685,1.),(1.00001423585994,
0.912530301180533,1.),(1.00000710550471,0.956341495377427,1.),(1.00001238975909,
0.92387333813702,1.)))
REPRESENTATION_ITEM('')
SURFACE()
);
#2795=(
BOUNDED_SURFACE()
B_SPLINE_SURFACE(3,2,((#394342,#394343,#394344),(#394345,#394346,#394347),
(#394348,#394349,#394350),(#394351,#394352,#394353)),.UNSPECIFIED.,.F.,
 .F.,.F.)
B_SPLINE_SURFACE_WITH_KNOTS((4,4),(3,3),(-3.39934179457797E-6,3.73927597403568E-5),
(-0.00186004067438382,1.00069373317431),.UNSPECIFIED.)
GEOMETRIC_REPRESENTATION_ITEM()
RATIONAL_B_SPLINE_SURFACE(((1.00072100136062,0.806051963875329,1.00026859642688),
(1.0006004844016,0.83847080355862,1.00022369994493),(1.000531064488,0.857144632272351,
1.00019783877217),(1.00054515072858,0.85335545953909,1.00020308635434)))
REPRESENTATION_ITEM('')
SURFACE()
);
#2796=(
BOUNDED_SURFACE()
B_SPLINE_SURFACE(3,2,((#394355,#394356,#394357),(#394358,#394359,#394360),
(#394361,#394362,#394363),(#394364,#394365,#394366)),.UNSPECIFIED.,.F.,
 .F.,.F.)
B_SPLINE_SURFACE_WITH_KNOTS((4,4),(3,3),(-2.71050543121376E-19,9.54361881492169E-5),
(0.,1.),.UNSPECIFIED.)
GEOMETRIC_REPRESENTATION_ITEM()
RATIONAL_B_SPLINE_SURFACE(((1.,0.81671562114205,1.),(1.,0.815907587407938,
1.),(1.,0.81511595934521,1.),(1.,0.814339887349194,1.)))
REPRESENTATION_ITEM('')
SURFACE()
);
#2797=(
BOUNDED_SURFACE()
B_SPLINE_SURFACE(3,2,((#394368,#394369,#394370),(#394371,#394372,#394373),
(#394374,#394375,#394376),(#394377,#394378,#394379)),.UNSPECIFIED.,.F.,
 .F.,.F.)
B_SPLINE_SURFACE_WITH_KNOTS((4,4),(3,3),(-2.37169225231204E-20,4.68197758448205E-5),
(0.,1.),.UNSPECIFIED.)
GEOMETRIC_REPRESENTATION_ITEM()
RATIONAL_B_SPLINE_SURFACE(((1.,0.816715621142046,1.),(1.,0.953638980025212,
1.),(1.,0.954506925408045,1.),(1.,0.816715621142057,1.)))
REPRESENTATION_ITEM('')
SURFACE()
);
#2798=(
BOUNDED_SURFACE()
B_SPLINE_SURFACE(3,2,((#394381,#394382,#394383),(#394384,#394385,#394386),
(#394387,#394388,#394389),(#394390,#394391,#394392)),.UNSPECIFIED.,.F.,
 .F.,.F.)
B_SPLINE_SURFACE_WITH_KNOTS((4,4),(3,3),(1.62630325872826E-19,9.54361881492178E-5),
(0.,1.),.UNSPECIFIED.)
GEOMETRIC_REPRESENTATION_ITEM()
RATIONAL_B_SPLINE_SURFACE(((1.,0.814339887349195,1.),(1.,0.815115959345209,
1.),(1.,0.81590758740794,1.),(1.,0.816715621142049,1.)))
REPRESENTATION_ITEM('')
SURFACE()
);
#2799=(
BOUNDED_SURFACE()
B_SPLINE_SURFACE(3,2,((#394394,#394395,#394396),(#394397,#394398,#394399),
(#394400,#394401,#394402),(#394403,#394404,#394405)),.UNSPECIFIED.,.F.,
 .F.,.F.)
B_SPLINE_SURFACE_WITH_KNOTS((4,4),(3,3),(-3.39528393502483E-6,3.73481232852736E-5),
(-0.00165018033284259,1.),.UNSPECIFIED.)
GEOMETRIC_REPRESENTATION_ITEM()
RATIONAL_B_SPLINE_SURFACE(((1.00048354385553,0.853487571660465,1.),(1.00047110510908,
0.857256476851521,1.),(1.00053193201093,0.838826096655951,1.),(1.00063970687708,
0.806170615310176,1.)))
REPRESENTATION_ITEM('')
SURFACE()
);
#2800=(
BOUNDED_SURFACE()
B_SPLINE_SURFACE(3,2,((#394409,#394410,#394411),(#394412,#394413,#394414),
(#394415,#394416,#394417),(#394418,#394419,#394420)),.UNSPECIFIED.,.F.,
 .F.,.F.)
B_SPLINE_SURFACE_WITH_KNOTS((4,4),(3,3),(2.02993869230506E-5,5.39756952686903E-5),
(-0.000116281070056919,1.),.UNSPECIFIED.)
GEOMETRIC_REPRESENTATION_ITEM()
RATIONAL_B_SPLINE_SURFACE(((1.00001770479732,0.923870681142999,1.),(1.0000101410406,
0.95639427554342,1.),(1.00002037300281,0.912397594905655,1.),(1.00003390859473,
0.854195550869835,1.)))
REPRESENTATION_ITEM('')
SURFACE()
);
#2801=(
BOUNDED_SURFACE()
B_SPLINE_SURFACE(3,2,((#394513,#394514,#394515),(#394516,#394517,#394518),
(#394519,#394520,#394521),(#394522,#394523,#394524)),.UNSPECIFIED.,.F.,
 .F.,.F.)
B_SPLINE_SURFACE_WITH_KNOTS((4,4),(3,3),(0.00135801595889393,0.00148409170619832),
(0.,1.),.UNSPECIFIED.)
GEOMETRIC_REPRESENTATION_ITEM()
RATIONAL_B_SPLINE_SURFACE(((1.,0.818301933966447,1.),(1.,0.817226613172351,
1.),(1.,0.816179643373952,1.),(1.,0.815159387863656,1.)))
REPRESENTATION_ITEM('')
SURFACE()
);
#2802=(
BOUNDED_SURFACE()
B_SPLINE_SURFACE(3,2,((#394563,#394564,#394565),(#394566,#394567,#394568),
(#394569,#394570,#394571),(#394572,#394573,#394574)),.UNSPECIFIED.,.F.,
 .F.,.F.)
B_SPLINE_SURFACE_WITH_KNOTS((4,4),(3,3),(-1.54744435122069E-6,1.54744435122074E-5),
(-0.0151698983592225,1.),.UNSPECIFIED.)
GEOMETRIC_REPRESENTATION_ITEM()
RATIONAL_B_SPLINE_SURFACE(((1.02018382472565,0.334740937358353,1.),(1.00401234488747,
0.867753072813766,1.),(1.00033622856774,0.988917903080832,1.),(1.,1.,1.)))
REPRESENTATION_ITEM('')
SURFACE()
);
#2803=(
BOUNDED_SURFACE()
B_SPLINE_SURFACE(3,2,((#394576,#394577,#394578),(#394579,#394580,#394581),
(#394582,#394583,#394584),(#394585,#394586,#394587)),.UNSPECIFIED.,.F.,
 .F.,.F.)
B_SPLINE_SURFACE_WITH_KNOTS((4,4),(3,3),(0.00137194782501028,0.00149814269699235),
(0.,1.),.UNSPECIFIED.)
GEOMETRIC_REPRESENTATION_ITEM()
RATIONAL_B_SPLINE_SURFACE(((1.,0.81515850940232,1.),(1.,0.816179044148164,
1.),(1.,0.817226308119926,1.),(1.,0.818301939488812,1.)))
REPRESENTATION_ITEM('')
SURFACE()
);
#2804=(
BOUNDED_SURFACE()
B_SPLINE_SURFACE(3,2,((#394631,#394632,#394633),(#394634,#394635,#394636),
(#394637,#394638,#394639),(#394640,#394641,#394642)),.UNSPECIFIED.,.F.,
 .F.,.F.)
B_SPLINE_SURFACE_WITH_KNOTS((4,4),(3,3),(1.55009486301137E-5,4.9206551047443E-5),
(-8.13759512517913E-5,1.),.UNSPECIFIED.)
GEOMETRIC_REPRESENTATION_ITEM()
RATIONAL_B_SPLINE_SURFACE(((1.00002372912329,0.85420063959972,1.),(1.00001423585989,
0.912530301180554,1.),(1.00000710550469,0.956341495377446,1.),(1.00001238975905,
0.923873338137039,1.)))
REPRESENTATION_ITEM('')
SURFACE()
);
#2805=(
BOUNDED_SURFACE()
B_SPLINE_SURFACE(3,2,((#394646,#394647,#394648),(#394649,#394650,#394651),
(#394652,#394653,#394654),(#394655,#394656,#394657)),.UNSPECIFIED.,.F.,
 .F.,.F.)
B_SPLINE_SURFACE_WITH_KNOTS((4,4),(3,3),(-3.39934179457793E-6,3.73927597403567E-5),
(-0.00186004067460027,1.00069373317475),.UNSPECIFIED.)
GEOMETRIC_REPRESENTATION_ITEM()
RATIONAL_B_SPLINE_SURFACE(((1.00072100136071,0.806051963875212,1.00026859642704),
(1.00060048440167,0.838470803558519,1.00022369994507),(1.00053106448807,
0.857144632272275,1.00019783877229),(1.00054515072864,0.853355459538997,
1.00020308635447)))
REPRESENTATION_ITEM('')
SURFACE()
);
#2806=(
BOUNDED_SURFACE()
B_SPLINE_SURFACE(3,2,((#394659,#394660,#394661),(#394662,#394663,#394664),
(#394665,#394666,#394667),(#394668,#394669,#394670)),.UNSPECIFIED.,.F.,
 .F.,.F.)
B_SPLINE_SURFACE_WITH_KNOTS((4,4),(3,3),(-1.62630325872826E-19,9.54361881492172E-5),
(0.,1.),.UNSPECIFIED.)
GEOMETRIC_REPRESENTATION_ITEM()
RATIONAL_B_SPLINE_SURFACE(((1.,0.816715621142052,1.),(1.,0.815907587407936,
1.),(1.,0.815115959345212,1.),(1.,0.814339887349197,1.)))
REPRESENTATION_ITEM('')
SURFACE()
);
#2807=(
BOUNDED_SURFACE()
B_SPLINE_SURFACE(3,2,((#394672,#394673,#394674),(#394675,#394676,#394677),
(#394678,#394679,#394680),(#394681,#394682,#394683)),.UNSPECIFIED.,.F.,
 .F.,.F.)
B_SPLINE_SURFACE_WITH_KNOTS((4,4),(3,3),(5.9292306307801E-20,4.68197758448215E-5),
(0.,1.),.UNSPECIFIED.)
GEOMETRIC_REPRESENTATION_ITEM()
RATIONAL_B_SPLINE_SURFACE(((1.,0.816715621142048,1.),(1.,0.953638980025212,
1.),(1.,0.95450692540805,1.),(1.,0.816715621142047,1.)))
REPRESENTATION_ITEM('')
SURFACE()
);
#2808=(
BOUNDED_SURFACE()
B_SPLINE_SURFACE(3,2,((#394685,#394686,#394687),(#394688,#394689,#394690),
(#394691,#394692,#394693),(#394694,#394695,#394696)),.UNSPECIFIED.,.F.,
 .F.,.F.)
B_SPLINE_SURFACE_WITH_KNOTS((4,4),(3,3),(-1.0842021724855E-19,9.54361881492175E-5),
(0.,1.),.UNSPECIFIED.)
GEOMETRIC_REPRESENTATION_ITEM()
RATIONAL_B_SPLINE_SURFACE(((1.,0.814339887349196,1.),(1.,0.815115959345207,
1.),(1.,0.815907587407945,1.),(1.,0.816715621142051,1.)))
REPRESENTATION_ITEM('')
SURFACE()
);
#2809=(
BOUNDED_SURFACE()
B_SPLINE_SURFACE(3,2,((#394698,#394699,#394700),(#394701,#394702,#394703),
(#394704,#394705,#394706),(#394707,#394708,#394709)),.UNSPECIFIED.,.F.,
 .F.,.F.)
B_SPLINE_SURFACE_WITH_KNOTS((4,4),(3,3),(-3.39528393502488E-6,3.73481232852737E-5),
(-0.00165018033318095,1.),.UNSPECIFIED.)
GEOMETRIC_REPRESENTATION_ITEM()
RATIONAL_B_SPLINE_SURFACE(((1.00048354385562,0.853487571660418,1.),(1.00047110510918,
0.857256476851478,1.),(1.00053193201104,0.838826096655891,1.),(1.00063970687722,
0.806170615310113,1.)))
REPRESENTATION_ITEM('')
SURFACE()
);
#2810=(
BOUNDED_SURFACE()
B_SPLINE_SURFACE(3,2,((#394713,#394714,#394715),(#394716,#394717,#394718),
(#394719,#394720,#394721),(#394722,#394723,#394724)),.UNSPECIFIED.,.F.,
 .F.,.F.)
B_SPLINE_SURFACE_WITH_KNOTS((4,4),(3,3),(2.02993869230509E-5,5.39756952686907E-5),
(-0.000116281069535401,1.),.UNSPECIFIED.)
GEOMETRIC_REPRESENTATION_ITEM()
RATIONAL_B_SPLINE_SURFACE(((1.00001770479724,0.923870681143039,1.),(1.00001014104056,
0.956394275543436,1.),(1.00002037300272,0.912397594905709,1.),(1.00003390859458,
0.854195550869909,1.)))
REPRESENTATION_ITEM('')
SURFACE()
);
#2811=(
BOUNDED_SURFACE()
B_SPLINE_SURFACE(3,2,((#394817,#394818,#394819),(#394820,#394821,#394822),
(#394823,#394824,#394825),(#394826,#394827,#394828)),.UNSPECIFIED.,.F.,
 .F.,.F.)
B_SPLINE_SURFACE_WITH_KNOTS((4,4),(3,3),(0.00135801595889393,0.00148409170619832),
(0.,1.),.UNSPECIFIED.)
GEOMETRIC_REPRESENTATION_ITEM()
RATIONAL_B_SPLINE_SURFACE(((1.,0.818301933966442,1.),(1.,0.817226613172344,
1.),(1.,0.816179643373945,1.),(1.,0.815159387863654,1.)))
REPRESENTATION_ITEM('')
SURFACE()
);
#2812=(
BOUNDED_SURFACE()
B_SPLINE_SURFACE(3,2,((#394867,#394868,#394869),(#394870,#394871,#394872),
(#394873,#394874,#394875),(#394876,#394877,#394878)),.UNSPECIFIED.,.F.,
 .F.,.F.)
B_SPLINE_SURFACE_WITH_KNOTS((4,4),(3,3),(-1.54744435122077E-6,1.54744435122079E-5),
(0.,1.01516989836551),.UNSPECIFIED.)
GEOMETRIC_REPRESENTATION_ITEM()
RATIONAL_B_SPLINE_SURFACE(((1.,0.334740937354324,1.02018382473414),(1.,
0.867753072812859,1.00401234488916),(1.,0.988917903080846,1.00033622856788),
(1.,1.,1.)))
REPRESENTATION_ITEM('')
SURFACE()
);
#2813=(
BOUNDED_SURFACE()
B_SPLINE_SURFACE(3,2,((#394880,#394881,#394882),(#394883,#394884,#394885),
(#394886,#394887,#394888),(#394889,#394890,#394891)),.UNSPECIFIED.,.F.,
 .F.,.F.)
B_SPLINE_SURFACE_WITH_KNOTS((4,4),(3,3),(0.00137194782501028,0.00149814269699235),
(0.,1.),.UNSPECIFIED.)
GEOMETRIC_REPRESENTATION_ITEM()
RATIONAL_B_SPLINE_SURFACE(((1.,0.815158509402316,1.),(1.,0.816179044148155,
1.),(1.,0.817226308119926,1.),(1.,0.818301939488808,1.)))
REPRESENTATION_ITEM('')
SURFACE()
);
#2814=(
BOUNDED_SURFACE()
B_SPLINE_SURFACE(3,2,((#394935,#394936,#394937),(#394938,#394939,#394940),
(#394941,#394942,#394943),(#394944,#394945,#394946)),.UNSPECIFIED.,.F.,
 .F.,.F.)
B_SPLINE_SURFACE_WITH_KNOTS((4,4),(3,3),(1.55009486301137E-5,4.92065510474433E-5),
(-8.13759514709342E-5,1.),.UNSPECIFIED.)
GEOMETRIC_REPRESENTATION_ITEM()
RATIONAL_B_SPLINE_SURFACE(((1.00002372912335,0.854200639599687,1.),(1.00001423585993,
0.912530301180535,1.),(1.00000710550471,0.956341495377432,1.),(1.00001238975908,
0.923873338137023,1.)))
REPRESENTATION_ITEM('')
SURFACE()
);
#2815=(
BOUNDED_SURFACE()
B_SPLINE_SURFACE(3,2,((#394950,#394951,#394952),(#394953,#394954,#394955),
(#394956,#394957,#394958),(#394959,#394960,#394961)),.UNSPECIFIED.,.F.,
 .F.,.F.)
B_SPLINE_SURFACE_WITH_KNOTS((4,4),(3,3),(-3.39934179457828E-6,3.73927597403565E-5),
(-0.00186004067401879,1.00069373317445),.UNSPECIFIED.)
GEOMETRIC_REPRESENTATION_ITEM()
RATIONAL_B_SPLINE_SURFACE(((1.00072100136048,0.806051963875363,1.00026859642693),
(1.00060048440149,0.838470803558657,1.00022369994497),(1.0005310644879,
0.857144632272393,1.00019783877221),(1.00054515072847,0.85335545953911,
1.00020308635438)))
REPRESENTATION_ITEM('')
SURFACE()
);
#2816=(
BOUNDED_SURFACE()
B_SPLINE_SURFACE(3,2,((#394963,#394964,#394965),(#394966,#394967,#394968),
(#394969,#394970,#394971),(#394972,#394973,#394974)),.UNSPECIFIED.,.F.,
 .F.,.F.)
B_SPLINE_SURFACE_WITH_KNOTS((4,4),(3,3),(1.62630325872826E-19,9.54361881492177E-5),
(0.,1.),.UNSPECIFIED.)
GEOMETRIC_REPRESENTATION_ITEM()
RATIONAL_B_SPLINE_SURFACE(((1.,0.816715621142046,1.),(1.,0.815907587407939,
1.),(1.,0.815115959345208,1.),(1.,0.814339887349188,1.)))
REPRESENTATION_ITEM('')
SURFACE()
);
#2817=(
BOUNDED_SURFACE()
B_SPLINE_SURFACE(3,2,((#394976,#394977,#394978),(#394979,#394980,#394981),
(#394982,#394983,#394984),(#394985,#394986,#394987)),.UNSPECIFIED.,.F.,
 .F.,.F.)
B_SPLINE_SURFACE_WITH_KNOTS((4,4),(3,3),(9.99498877760074E-20,4.68197758448203E-5),
(0.,1.),.UNSPECIFIED.)
GEOMETRIC_REPRESENTATION_ITEM()
RATIONAL_B_SPLINE_SURFACE(((1.,0.816715621142051,1.),(1.,0.953638980025203,
1.),(1.,0.954506925408057,1.),(1.,0.816715621142053,1.)))
REPRESENTATION_ITEM('')
SURFACE()
);
#2818=(
BOUNDED_SURFACE()
B_SPLINE_SURFACE(3,2,((#394989,#394990,#394991),(#394992,#394993,#394994),
(#394995,#394996,#394997),(#394998,#394999,#395000)),.UNSPECIFIED.,.F.,
 .F.,.F.)
B_SPLINE_SURFACE_WITH_KNOTS((4,4),(3,3),(-1.0842021724855E-19,9.54361881492176E-5),
(0.,1.),.UNSPECIFIED.)
GEOMETRIC_REPRESENTATION_ITEM()
RATIONAL_B_SPLINE_SURFACE(((1.,0.814339887349193,1.),(1.,0.815115959345199,
1.),(1.,0.815907587407946,1.),(1.,0.816715621142045,1.)))
REPRESENTATION_ITEM('')
SURFACE()
);
#2819=(
BOUNDED_SURFACE()
B_SPLINE_SURFACE(3,2,((#395002,#395003,#395004),(#395005,#395006,#395007),
(#395008,#395009,#395010),(#395011,#395012,#395013)),.UNSPECIFIED.,.F.,
 .F.,.F.)
B_SPLINE_SURFACE_WITH_KNOTS((4,4),(3,3),(-3.39528393502487E-6,3.73481232852732E-5),
(-0.00165018033287617,1.),.UNSPECIFIED.)
GEOMETRIC_REPRESENTATION_ITEM()
RATIONAL_B_SPLINE_SURFACE(((1.00048354385554,0.85348757166045,1.),(1.00047110510909,
0.857256476851514,1.),(1.00053193201094,0.838826096655938,1.),(1.0006397068771,
0.806170615310168,1.)))
REPRESENTATION_ITEM('')
SURFACE()
);
#2820=(
BOUNDED_SURFACE()
B_SPLINE_SURFACE(3,2,((#395017,#395018,#395019),(#395020,#395021,#395022),
(#395023,#395024,#395025),(#395026,#395027,#395028)),.UNSPECIFIED.,.F.,
 .F.,.F.)
B_SPLINE_SURFACE_WITH_KNOTS((4,4),(3,3),(2.02993869230513E-5,5.397569526869E-5),
(-0.000116281070601051,1.),.UNSPECIFIED.)
GEOMETRIC_REPRESENTATION_ITEM()
RATIONAL_B_SPLINE_SURFACE(((1.0000177047974,0.923870681142957,1.),(1.00001014104065,
0.956394275543391,1.),(1.0000203730029,0.912397594905618,1.),(1.00003390859489,
0.854195550869751,1.)))
REPRESENTATION_ITEM('')
SURFACE()
);
#2821=(
BOUNDED_SURFACE()
B_SPLINE_SURFACE(3,2,((#395121,#395122,#395123),(#395124,#395125,#395126),
(#395127,#395128,#395129),(#395130,#395131,#395132)),.UNSPECIFIED.,.F.,
 .F.,.F.)
B_SPLINE_SURFACE_WITH_KNOTS((4,4),(3,3),(0.00135801595889393,0.00148409170619832),
(0.,1.),.UNSPECIFIED.)
GEOMETRIC_REPRESENTATION_ITEM()
RATIONAL_B_SPLINE_SURFACE(((1.,0.818301933966445,1.),(1.,0.817226613172345,
1.),(1.,0.816179643373958,1.),(1.,0.815159387863655,1.)))
REPRESENTATION_ITEM('')
SURFACE()
);
#2822=(
BOUNDED_SURFACE()
B_SPLINE_SURFACE(3,2,((#395171,#395172,#395173),(#395174,#395175,#395176),
(#395177,#395178,#395179),(#395180,#395181,#395182)),.UNSPECIFIED.,.F.,
 .F.,.F.)
B_SPLINE_SURFACE_WITH_KNOTS((4,4),(3,3),(-1.54744435122066E-6,1.54744435122077E-5),
(-0.0151698983594881,1.0151698983631),.UNSPECIFIED.)
GEOMETRIC_REPRESENTATION_ITEM()
RATIONAL_B_SPLINE_SURFACE(((1.02018382472601,0.324498219413288,1.02018382473088),
(1.00401234488754,0.865716921710537,1.00401234488851),(1.00033622856775,
0.988747276629672,1.00033622856783),(1.,1.,1.)))
REPRESENTATION_ITEM('')
SURFACE()
);
#2823=(
BOUNDED_SURFACE()
B_SPLINE_SURFACE(3,2,((#395184,#395185,#395186),(#395187,#395188,#395189),
(#395190,#395191,#395192),(#395193,#395194,#395195)),.UNSPECIFIED.,.F.,
 .F.,.F.)
B_SPLINE_SURFACE_WITH_KNOTS((4,4),(3,3),(0.00137194782501028,0.00149814269699235),
(0.,1.),.UNSPECIFIED.)
GEOMETRIC_REPRESENTATION_ITEM()
RATIONAL_B_SPLINE_SURFACE(((1.,0.815158509402318,1.),(1.,0.816179044148161,
1.),(1.,0.817226308119921,1.),(1.,0.818301939488807,1.)))
REPRESENTATION_ITEM('')
SURFACE()
);
#2824=(
BOUNDED_SURFACE()
B_SPLINE_SURFACE(3,2,((#395239,#395240,#395241),(#395242,#395243,#395244),
(#395245,#395246,#395247),(#395248,#395249,#395250)),.UNSPECIFIED.,.F.,
 .F.,.F.)
B_SPLINE_SURFACE_WITH_KNOTS((4,4),(3,3),(1.55009486301137E-5,4.92065510474435E-5),
(-8.13759515122868E-5,1.),.UNSPECIFIED.)
GEOMETRIC_REPRESENTATION_ITEM()
RATIONAL_B_SPLINE_SURFACE(((1.00002372912337,0.85420063959968,1.),(1.00001423585994,
0.912530301180539,1.),(1.00000710550471,0.956341495377423,1.),(1.00001238975909,
0.923873338137018,1.)))
REPRESENTATION_ITEM('')
SURFACE()
);
#2825=(
BOUNDED_SURFACE()
B_SPLINE_SURFACE(3,2,((#395254,#395255,#395256),(#395257,#395258,#395259),
(#395260,#395261,#395262),(#395263,#395264,#395265)),.UNSPECIFIED.,.F.,
 .F.,.F.)
B_SPLINE_SURFACE_WITH_KNOTS((4,4),(3,3),(-3.39934179457826E-6,3.73927597403567E-5),
(-0.00186004067395861,1.00069373317436),.UNSPECIFIED.)
GEOMETRIC_REPRESENTATION_ITEM()
RATIONAL_B_SPLINE_SURFACE(((1.00072100136046,0.806051963875392,1.0002685964269),
(1.00060048440147,0.838470803558698,1.00022369994495),(1.00053106448788,
0.857144632272418,1.00019783877219),(1.00054515072846,0.85335545953914,
1.00020308635436)))
REPRESENTATION_ITEM('')
SURFACE()
);
#2826=(
BOUNDED_SURFACE()
B_SPLINE_SURFACE(3,2,((#395267,#395268,#395269),(#395270,#395271,#395272),
(#395273,#395274,#395275),(#395276,#395277,#395278)),.UNSPECIFIED.,.F.,
 .F.,.F.)
B_SPLINE_SURFACE_WITH_KNOTS((4,4),(3,3),(-1.62630325872826E-19,9.54361881492171E-5),
(0.,1.),.UNSPECIFIED.)
GEOMETRIC_REPRESENTATION_ITEM()
RATIONAL_B_SPLINE_SURFACE(((1.,0.816715621142051,1.),(1.,0.815907587407945,
1.),(1.,0.815115959345208,1.),(1.,0.814339887349197,1.)))
REPRESENTATION_ITEM('')
SURFACE()
);
#2827=(
BOUNDED_SURFACE()
B_SPLINE_SURFACE(3,2,((#395280,#395281,#395282),(#395283,#395284,#395285),
(#395286,#395287,#395288),(#395289,#395290,#395291)),.UNSPECIFIED.,.F.,
 .F.,.F.)
B_SPLINE_SURFACE_WITH_KNOTS((4,4),(3,3),(4.57397791517322E-20,4.68197758448206E-5),
(0.,1.),.UNSPECIFIED.)
GEOMETRIC_REPRESENTATION_ITEM()
RATIONAL_B_SPLINE_SURFACE(((1.,0.81671562114205,1.),(1.,0.953638980025207,
1.),(1.,0.954506925408057,1.),(1.,0.816715621142058,1.)))
REPRESENTATION_ITEM('')
SURFACE()
);
#2828=(
BOUNDED_SURFACE()
B_SPLINE_SURFACE(3,2,((#395293,#395294,#395295),(#395296,#395297,#395298),
(#395299,#395300,#395301),(#395302,#395303,#395304)),.UNSPECIFIED.,.F.,
 .F.,.F.)
B_SPLINE_SURFACE_WITH_KNOTS((4,4),(3,3),(1.0842021724855E-19,9.54361881492178E-5),
(0.,1.),.UNSPECIFIED.)
GEOMETRIC_REPRESENTATION_ITEM()
RATIONAL_B_SPLINE_SURFACE(((1.,0.814339887349192,1.),(1.,0.815115959345201,
1.),(1.,0.815907587407939,1.),(1.,0.816715621142047,1.)))
REPRESENTATION_ITEM('')
SURFACE()
);
#2829=(
BOUNDED_SURFACE()
B_SPLINE_SURFACE(3,2,((#395306,#395307,#395308),(#395309,#395310,#395311),
(#395312,#395313,#395314),(#395315,#395316,#395317)),.UNSPECIFIED.,.F.,
 .F.,.F.)
B_SPLINE_SURFACE_WITH_KNOTS((4,4),(3,3),(-3.39528393502489E-6,3.73481232852737E-5),
(-0.00165018033293757,1.),.UNSPECIFIED.)
GEOMETRIC_REPRESENTATION_ITEM()
RATIONAL_B_SPLINE_SURFACE(((1.00048354385555,0.853487571660446,1.),(1.00047110510911,
0.857256476851515,1.),(1.00053193201096,0.838826096655921,1.),(1.00063970687712,
0.806170615310158,1.)))
REPRESENTATION_ITEM('')
SURFACE()
);
#2830=(
BOUNDED_SURFACE()
B_SPLINE_SURFACE(3,2,((#395321,#395322,#395323),(#395324,#395325,#395326),
(#395327,#395328,#395329),(#395330,#395331,#395332)),.UNSPECIFIED.,.F.,
 .F.,.F.)
B_SPLINE_SURFACE_WITH_KNOTS((4,4),(3,3),(2.02993869230509E-5,5.39756952686902E-5),
(-0.000116281069873628,1.),.UNSPECIFIED.)
GEOMETRIC_REPRESENTATION_ITEM()
RATIONAL_B_SPLINE_SURFACE(((1.00001770479729,0.923870681143014,1.),(1.00001014104058,
0.95639427554342,1.),(1.00002037300278,0.912397594905681,1.),(1.00003390859467,
0.854195550869857,1.)))
REPRESENTATION_ITEM('')
SURFACE()
);
#2831=(
BOUNDED_SURFACE()
B_SPLINE_SURFACE(3,2,((#395425,#395426,#395427),(#395428,#395429,#395430),
(#395431,#395432,#395433),(#395434,#395435,#395436)),.UNSPECIFIED.,.F.,
 .F.,.F.)
B_SPLINE_SURFACE_WITH_KNOTS((4,4),(3,3),(0.00135801595889393,0.00148409170619832),
(0.,1.),.UNSPECIFIED.)
GEOMETRIC_REPRESENTATION_ITEM()
RATIONAL_B_SPLINE_SURFACE(((1.,0.818301933966442,1.),(1.,0.817226613172343,
1.),(1.,0.816179643373955,1.),(1.,0.815159387863651,1.)))
REPRESENTATION_ITEM('')
SURFACE()
);
#2832=(
BOUNDED_SURFACE()
B_SPLINE_SURFACE(3,2,((#395475,#395476,#395477),(#395478,#395479,#395480),
(#395481,#395482,#395483),(#395484,#395485,#395486)),.UNSPECIFIED.,.F.,
 .F.,.F.)
B_SPLINE_SURFACE_WITH_KNOTS((4,4),(3,3),(-1.54744435122069E-6,1.54744435122075E-5),
(-0.0151698983687385,1.01516989835399),.UNSPECIFIED.)
GEOMETRIC_REPRESENTATION_ITEM()
RATIONAL_B_SPLINE_SURFACE(((1.0201838247385,0.324498219413267,1.02018382471858),
(1.00401234489003,0.865716921710468,1.00401234488607),(1.00033622856795,
0.988747276629697,1.00033622856762),(1.,1.,1.)))
REPRESENTATION_ITEM('')
SURFACE()
);
#2833=(
BOUNDED_SURFACE()
B_SPLINE_SURFACE(3,2,((#395488,#395489,#395490),(#395491,#395492,#395493),
(#395494,#395495,#395496),(#395497,#395498,#395499)),.UNSPECIFIED.,.F.,
 .F.,.F.)
B_SPLINE_SURFACE_WITH_KNOTS((4,4),(3,3),(0.00137194782501028,0.00149814269699235),
(0.,1.),.UNSPECIFIED.)
GEOMETRIC_REPRESENTATION_ITEM()
RATIONAL_B_SPLINE_SURFACE(((1.,0.815158509402313,1.),(1.,0.816179044148156,
1.),(1.,0.817226308119923,1.),(1.,0.818301939488804,1.)))
REPRESENTATION_ITEM('')
SURFACE()
);
#2834=(
BOUNDED_SURFACE()
B_SPLINE_SURFACE(3,2,((#395543,#395544,#395545),(#395546,#395547,#395548),
(#395549,#395550,#395551),(#395552,#395553,#395554)),.UNSPECIFIED.,.F.,
 .F.,.F.)
B_SPLINE_SURFACE_WITH_KNOTS((4,4),(3,3),(1.55009486301137E-5,4.92065510474425E-5),
(-8.1375951558491E-5,1.),.UNSPECIFIED.)
GEOMETRIC_REPRESENTATION_ITEM()
RATIONAL_B_SPLINE_SURFACE(((1.00002372912338,0.854200639599676,1.),(1.00001423585995,
0.91253030118053,1.),(1.00000710550471,0.956341495377426,1.),(1.0000123897591,
0.923873338137015,1.)))
REPRESENTATION_ITEM('')
SURFACE()
);
#2835=(
BOUNDED_SURFACE()
B_SPLINE_SURFACE(3,2,((#395558,#395559,#395560),(#395561,#395562,#395563),
(#395564,#395565,#395566),(#395567,#395568,#395569)),.UNSPECIFIED.,.F.,
 .F.,.F.)
B_SPLINE_SURFACE_WITH_KNOTS((4,4),(3,3),(-3.3993417945782E-6,3.73927597403566E-5),
(-0.00186004067410343,1.00069373317431),.UNSPECIFIED.)
GEOMETRIC_REPRESENTATION_ITEM()
RATIONAL_B_SPLINE_SURFACE(((1.00072100136051,0.806051963875371,1.00026859642688),
(1.00060048440151,0.838470803558661,1.00022369994493),(1.00053106448792,
0.857144632272405,1.00019783877217),(1.0005451507285,0.853355459539116,
1.00020308635434)))
REPRESENTATION_ITEM('')
SURFACE()
);
#2836=(
BOUNDED_SURFACE()
B_SPLINE_SURFACE(3,2,((#395571,#395572,#395573),(#395574,#395575,#395576),
(#395577,#395578,#395579),(#395580,#395581,#395582)),.UNSPECIFIED.,.F.,
 .F.,.F.)
B_SPLINE_SURFACE_WITH_KNOTS((4,4),(3,3),(-2.16840434497101E-19,9.54361881492175E-5),
(0.,1.),.UNSPECIFIED.)
GEOMETRIC_REPRESENTATION_ITEM()
RATIONAL_B_SPLINE_SURFACE(((1.,0.816715621142046,1.),(1.,0.815907587407944,
1.),(1.,0.815115959345203,1.),(1.,0.814339887349189,1.)))
REPRESENTATION_ITEM('')
SURFACE()
);
#2837=(
BOUNDED_SURFACE()
B_SPLINE_SURFACE(3,2,((#395584,#395585,#395586),(#395587,#395588,#395589),
(#395590,#395591,#395592),(#395593,#395594,#395595)),.UNSPECIFIED.,.F.,
 .F.,.F.)
B_SPLINE_SURFACE_WITH_KNOTS((4,4),(3,3),(3.3881317890172E-20,4.68197758448206E-5),
(0.,1.),.UNSPECIFIED.)
GEOMETRIC_REPRESENTATION_ITEM()
RATIONAL_B_SPLINE_SURFACE(((1.,0.816715621142054,1.),(1.,0.953638980025203,
1.),(1.,0.954506925408048,1.),(1.,0.81671562114206,1.)))
REPRESENTATION_ITEM('')
SURFACE()
);
#2838=(
BOUNDED_SURFACE()
B_SPLINE_SURFACE(3,2,((#395597,#395598,#395599),(#395600,#395601,#395602),
(#395603,#395604,#395605),(#395606,#395607,#395608)),.UNSPECIFIED.,.F.,
 .F.,.F.)
B_SPLINE_SURFACE_WITH_KNOTS((4,4),(3,3),(1.62630325872826E-19,9.54361881492176E-5),
(0.,1.),.UNSPECIFIED.)
GEOMETRIC_REPRESENTATION_ITEM()
RATIONAL_B_SPLINE_SURFACE(((1.,0.814339887349188,1.),(1.,0.815115959345208,
1.),(1.,0.815907587407938,1.),(1.,0.816715621142049,1.)))
REPRESENTATION_ITEM('')
SURFACE()
);
#2839=(
BOUNDED_SURFACE()
B_SPLINE_SURFACE(3,2,((#395610,#395611,#395612),(#395613,#395614,#395615),
(#395616,#395617,#395618),(#395619,#395620,#395621)),.UNSPECIFIED.,.F.,
 .F.,.F.)
B_SPLINE_SURFACE_WITH_KNOTS((4,4),(3,3),(-3.3952839350249E-6,3.73481232852737E-5),
(-0.00165018033274544,1.),.UNSPECIFIED.)
GEOMETRIC_REPRESENTATION_ITEM()
RATIONAL_B_SPLINE_SURFACE(((1.0004835438555,0.853487571660473,1.),(1.00047110510905,
0.857256476851541,1.),(1.0005319320109,0.838826096655948,1.),(1.00063970687705,
0.806170615310199,1.)))
REPRESENTATION_ITEM('')
SURFACE()
);
#2840=(
BOUNDED_SURFACE()
B_SPLINE_SURFACE(3,2,((#395625,#395626,#395627),(#395628,#395629,#395630),
(#395631,#395632,#395633),(#395634,#395635,#395636)),.UNSPECIFIED.,.F.,
 .F.,.F.)
B_SPLINE_SURFACE_WITH_KNOTS((4,4),(3,3),(2.02993869230511E-5,5.39756952686902E-5),
(-0.000116281070168245,1.),.UNSPECIFIED.)
GEOMETRIC_REPRESENTATION_ITEM()
RATIONAL_B_SPLINE_SURFACE(((1.00001770479734,0.92387068114299,1.),(1.00001014104061,
0.956394275543405,1.),(1.00002037300283,0.912397594905657,1.),(1.00003390859476,
0.854195550869819,1.)))
REPRESENTATION_ITEM('')
SURFACE()
);
#2841=(
BOUNDED_SURFACE()
B_SPLINE_SURFACE(3,2,((#395729,#395730,#395731),(#395732,#395733,#395734),
(#395735,#395736,#395737),(#395738,#395739,#395740)),.UNSPECIFIED.,.F.,
 .F.,.F.)
B_SPLINE_SURFACE_WITH_KNOTS((4,4),(3,3),(0.00135801595889393,0.00148409170619832),
(0.,1.),.UNSPECIFIED.)
GEOMETRIC_REPRESENTATION_ITEM()
RATIONAL_B_SPLINE_SURFACE(((1.,0.818301933966444,1.),(1.,0.817226613172339,
1.),(1.,0.816179643373955,1.),(1.,0.815159387863653,1.)))
REPRESENTATION_ITEM('')
SURFACE()
);
#2842=(
BOUNDED_SURFACE()
B_SPLINE_SURFACE(3,2,((#395779,#395780,#395781),(#395782,#395783,#395784),
(#395785,#395786,#395787),(#395788,#395789,#395790)),.UNSPECIFIED.,.F.,
 .F.,.F.)
B_SPLINE_SURFACE_WITH_KNOTS((4,4),(3,3),(-1.54744435122071E-6,1.54744435122069E-5),
(-0.0151698983631405,1.01516989835935),.UNSPECIFIED.)
GEOMETRIC_REPRESENTATION_ITEM()
RATIONAL_B_SPLINE_SURFACE(((1.02018382473094,0.324498219413405,1.02018382472582),
(1.00401234488852,0.865716921710534,1.00401234488751),(1.00033622856783,
0.988747276629699,1.00033622856774),(1.,1.,1.)))
REPRESENTATION_ITEM('')
SURFACE()
);
#2843=(
BOUNDED_SURFACE()
B_SPLINE_SURFACE(3,2,((#395792,#395793,#395794),(#395795,#395796,#395797),
(#395798,#395799,#395800),(#395801,#395802,#395803)),.UNSPECIFIED.,.F.,
 .F.,.F.)
B_SPLINE_SURFACE_WITH_KNOTS((4,4),(3,3),(0.00137194782501028,0.00149814269699235),
(0.,1.),.UNSPECIFIED.)
GEOMETRIC_REPRESENTATION_ITEM()
RATIONAL_B_SPLINE_SURFACE(((1.,0.815158509402317,1.),(1.,0.816179044148151,
1.),(1.,0.817226308119928,1.),(1.,0.818301939488808,1.)))
REPRESENTATION_ITEM('')
SURFACE()
);
#2844=(
BOUNDED_SURFACE()
B_SPLINE_SURFACE(3,2,((#395847,#395848,#395849),(#395850,#395851,#395852),
(#395853,#395854,#395855),(#395856,#395857,#395858)),.UNSPECIFIED.,.F.,
 .F.,.F.)
B_SPLINE_SURFACE_WITH_KNOTS((4,4),(3,3),(1.55009486301137E-5,4.9206551047443E-5),
(-8.13759515172332E-5,1.),.UNSPECIFIED.)
GEOMETRIC_REPRESENTATION_ITEM()
RATIONAL_B_SPLINE_SURFACE(((1.00002372912337,0.854200639599675,1.),(1.00001423585994,
0.912530301180543,1.),(1.00000710550471,0.956341495377428,1.),(1.00001238975909,
0.923873338137019,1.)))
REPRESENTATION_ITEM('')
SURFACE()
);
#2845=(
BOUNDED_SURFACE()
B_SPLINE_SURFACE(3,2,((#395862,#395863,#395864),(#395865,#395866,#395867),
(#395868,#395869,#395870),(#395871,#395872,#395873)),.UNSPECIFIED.,.F.,
 .F.,.F.)
B_SPLINE_SURFACE_WITH_KNOTS((4,4),(3,3),(-3.39934179457809E-6,3.73927597403566E-5),
(-0.0018600406740949,1.00069373317436),.UNSPECIFIED.)
GEOMETRIC_REPRESENTATION_ITEM()
RATIONAL_B_SPLINE_SURFACE(((1.00072100136051,0.806051963875365,1.0002685964269),
(1.00060048440151,0.83847080355867,1.00022369994495),(1.00053106448792,
0.85714463227239,1.00019783877218),(1.0005451507285,0.853355459539117,1.00020308635436)))
REPRESENTATION_ITEM('')
SURFACE()
);
#2846=(
BOUNDED_SURFACE()
B_SPLINE_SURFACE(3,2,((#395875,#395876,#395877),(#395878,#395879,#395880),
(#395881,#395882,#395883),(#395884,#395885,#395886)),.UNSPECIFIED.,.F.,
 .F.,.F.)
B_SPLINE_SURFACE_WITH_KNOTS((4,4),(3,3),(-5.42101086242752E-20,9.54361881492176E-5),
(0.,1.),.UNSPECIFIED.)
GEOMETRIC_REPRESENTATION_ITEM()
RATIONAL_B_SPLINE_SURFACE(((1.,0.816715621142048,1.),(1.,0.81590758740794,
1.),(1.,0.815115959345207,1.),(1.,0.814339887349192,1.)))
REPRESENTATION_ITEM('')
SURFACE()
);
#2847=(
BOUNDED_SURFACE()
B_SPLINE_SURFACE(3,2,((#395888,#395889,#395890),(#395891,#395892,#395893),
(#395894,#395895,#395896),(#395897,#395898,#395899)),.UNSPECIFIED.,.F.,
 .F.,.F.)
B_SPLINE_SURFACE_WITH_KNOTS((4,4),(3,3),(1.03338019565025E-19,4.68197758448208E-5),
(0.,1.),.UNSPECIFIED.)
GEOMETRIC_REPRESENTATION_ITEM()
RATIONAL_B_SPLINE_SURFACE(((1.,0.816715621142046,1.),(1.,0.953638980025206,
1.),(1.,0.954506925408053,1.),(1.,0.816715621142057,1.)))
REPRESENTATION_ITEM('')
SURFACE()
);
#2848=(
BOUNDED_SURFACE()
B_SPLINE_SURFACE(3,2,((#395901,#395902,#395903),(#395904,#395905,#395906),
(#395907,#395908,#395909),(#395910,#395911,#395912)),.UNSPECIFIED.,.F.,
 .F.,.F.)
B_SPLINE_SURFACE_WITH_KNOTS((4,4),(3,3),(5.42101086242752E-20,9.54361881492177E-5),
(0.,1.),.UNSPECIFIED.)
GEOMETRIC_REPRESENTATION_ITEM()
RATIONAL_B_SPLINE_SURFACE(((1.,0.814339887349189,1.),(1.,0.815115959345208,
1.),(1.,0.815907587407936,1.),(1.,0.816715621142047,1.)))
REPRESENTATION_ITEM('')
SURFACE()
);
#2849=(
BOUNDED_SURFACE()
B_SPLINE_SURFACE(3,2,((#395914,#395915,#395916),(#395917,#395918,#395919),
(#395920,#395921,#395922),(#395923,#395924,#395925)),.UNSPECIFIED.,.F.,
 .F.,.F.)
B_SPLINE_SURFACE_WITH_KNOTS((4,4),(3,3),(-3.39528393502485E-6,3.73481232852736E-5),
(-0.00165018033331714,1.),.UNSPECIFIED.)
GEOMETRIC_REPRESENTATION_ITEM()
RATIONAL_B_SPLINE_SURFACE(((1.00048354385567,0.853487571660372,1.),(1.00047110510922,
0.857256476851477,1.),(1.00053193201108,0.838826096655848,1.),(1.00063970687727,
0.80617061531009,1.)))
REPRESENTATION_ITEM('')
SURFACE()
);
#2850=(
BOUNDED_SURFACE()
B_SPLINE_SURFACE(3,2,((#395929,#395930,#395931),(#395932,#395933,#395934),
(#395935,#395936,#395937),(#395938,#395939,#395940)),.UNSPECIFIED.,.F.,
 .F.,.F.)
B_SPLINE_SURFACE_WITH_KNOTS((4,4),(3,3),(2.02993869230511E-5,5.39756952686902E-5),
(-0.000116281069525557,1.),.UNSPECIFIED.)
GEOMETRIC_REPRESENTATION_ITEM()
RATIONAL_B_SPLINE_SURFACE(((1.00001770479724,0.923870681143036,1.),(1.00001014104055,
0.956394275543452,1.),(1.00002037300272,0.912397594905699,1.),(1.00003390859457,
0.854195550869911,1.)))
REPRESENTATION_ITEM('')
SURFACE()
);
#2851=(
BOUNDED_SURFACE()
B_SPLINE_SURFACE(3,2,((#396033,#396034,#396035),(#396036,#396037,#396038),
(#396039,#396040,#396041),(#396042,#396043,#396044)),.UNSPECIFIED.,.F.,
 .F.,.F.)
B_SPLINE_SURFACE_WITH_KNOTS((4,4),(3,3),(0.00135801595889393,0.00148409170619832),
(0.,1.),.UNSPECIFIED.)
GEOMETRIC_REPRESENTATION_ITEM()
RATIONAL_B_SPLINE_SURFACE(((1.,0.818301933966435,1.),(1.,0.817226613172344,
1.),(1.,0.816179643373953,1.),(1.,0.815159387863652,1.)))
REPRESENTATION_ITEM('')
SURFACE()
);
#2852=(
BOUNDED_SURFACE()
B_SPLINE_SURFACE(3,2,((#396083,#396084,#396085),(#396086,#396087,#396088),
(#396089,#396090,#396091),(#396092,#396093,#396094)),.UNSPECIFIED.,.F.,
 .F.,.F.)
B_SPLINE_SURFACE_WITH_KNOTS((4,4),(3,3),(-1.54744435122072E-6,1.54744435122074E-5),
(-0.0151698983584628,1.),.UNSPECIFIED.)
GEOMETRIC_REPRESENTATION_ITEM()
RATIONAL_B_SPLINE_SURFACE(((1.02018382472462,0.334740937358972,1.),(1.00401234488727,
0.867753072813783,1.),(1.00033622856772,0.988917903080908,1.),(1.,1.,1.)))
REPRESENTATION_ITEM('')
SURFACE()
);
#2853=(
BOUNDED_SURFACE()
B_SPLINE_SURFACE(3,2,((#396096,#396097,#396098),(#396099,#396100,#396101),
(#396102,#396103,#396104),(#396105,#396106,#396107)),.UNSPECIFIED.,.F.,
 .F.,.F.)
B_SPLINE_SURFACE_WITH_KNOTS((4,4),(3,3),(0.00137194782501028,0.00149814269699235),
(0.,1.),.UNSPECIFIED.)
GEOMETRIC_REPRESENTATION_ITEM()
RATIONAL_B_SPLINE_SURFACE(((1.,0.815158509402318,1.),(1.,0.816179044148147,
1.),(1.,0.817226308119945,1.),(1.,0.818301939488798,1.)))
REPRESENTATION_ITEM('')
SURFACE()
);
#2854=(
BOUNDED_SURFACE()
B_SPLINE_SURFACE(3,2,((#396151,#396152,#396153),(#396154,#396155,#396156),
(#396157,#396158,#396159),(#396160,#396161,#396162)),.UNSPECIFIED.,.F.,
 .F.,.F.)
B_SPLINE_SURFACE_WITH_KNOTS((4,4),(3,3),(1.55009486301138E-5,4.92065510474431E-5),
(-8.13759513618527E-5,1.),.UNSPECIFIED.)
GEOMETRIC_REPRESENTATION_ITEM()
RATIONAL_B_SPLINE_SURFACE(((1.00002372912332,0.854200639599699,1.),(1.00001423585991,
0.912530301180549,1.),(1.0000071055047,0.956341495377427,1.),(1.00001238975907,
0.923873338137033,1.)))
REPRESENTATION_ITEM('')
SURFACE()
);
#2855=(
BOUNDED_SURFACE()
B_SPLINE_SURFACE(3,2,((#396166,#396167,#396168),(#396169,#396170,#396171),
(#396172,#396173,#396174),(#396175,#396176,#396177)),.UNSPECIFIED.,.F.,
 .F.,.F.)
B_SPLINE_SURFACE_WITH_KNOTS((4,4),(3,3),(-3.39934179457828E-6,3.73927597403566E-5),
(-0.00186004067405741,1.00069373317425),.UNSPECIFIED.)
GEOMETRIC_REPRESENTATION_ITEM()
RATIONAL_B_SPLINE_SURFACE(((1.0007210013605,0.80605196387541,1.00026859642685),
(1.0006004844015,0.838470803558664,1.00022369994491),(1.00053106448791,
0.857144632272433,1.00019783877215),(1.00054515072849,0.853355459539133,
1.00020308635433)))
REPRESENTATION_ITEM('')
SURFACE()
);
#2856=(
BOUNDED_SURFACE()
B_SPLINE_SURFACE(3,2,((#396179,#396180,#396181),(#396182,#396183,#396184),
(#396185,#396186,#396187),(#396188,#396189,#396190)),.UNSPECIFIED.,.F.,
 .F.,.F.)
B_SPLINE_SURFACE_WITH_KNOTS((4,4),(3,3),(5.42101086242752E-20,9.54361881492173E-5),
(0.,1.),.UNSPECIFIED.)
GEOMETRIC_REPRESENTATION_ITEM()
RATIONAL_B_SPLINE_SURFACE(((1.,0.816715621142047,1.),(1.,0.815907587407945,
1.),(1.,0.815115959345203,1.),(1.,0.814339887349192,1.)))
REPRESENTATION_ITEM('')
SURFACE()
);
#2857=(
BOUNDED_SURFACE()
B_SPLINE_SURFACE(3,2,((#396192,#396193,#396194),(#396195,#396196,#396197),
(#396198,#396199,#396200),(#396201,#396202,#396203)),.UNSPECIFIED.,.F.,
 .F.,.F.)
B_SPLINE_SURFACE_WITH_KNOTS((4,4),(3,3),(-1.6940658945086E-19,4.68197758448211E-5),
(0.,1.),.UNSPECIFIED.)
GEOMETRIC_REPRESENTATION_ITEM()
RATIONAL_B_SPLINE_SURFACE(((1.,0.816715621142047,1.),(1.,0.953638980025217,
1.),(1.,0.954506925408042,1.),(1.,0.816715621142054,1.)))
REPRESENTATION_ITEM('')
SURFACE()
);
#2858=(
BOUNDED_SURFACE()
B_SPLINE_SURFACE(3,2,((#396205,#396206,#396207),(#396208,#396209,#396210),
(#396211,#396212,#396213),(#396214,#396215,#396216)),.UNSPECIFIED.,.F.,
 .F.,.F.)
B_SPLINE_SURFACE_WITH_KNOTS((4,4),(3,3),(5.42101086242752E-20,9.54361881492176E-5),
(0.,1.),.UNSPECIFIED.)
GEOMETRIC_REPRESENTATION_ITEM()
RATIONAL_B_SPLINE_SURFACE(((1.,0.814339887349192,1.),(1.,0.815115959345213,
1.),(1.,0.815907587407945,1.),(1.,0.816715621142048,1.)))
REPRESENTATION_ITEM('')
SURFACE()
);
#2859=(
BOUNDED_SURFACE()
B_SPLINE_SURFACE(3,2,((#396218,#396219,#396220),(#396221,#396222,#396223),
(#396224,#396225,#396226),(#396227,#396228,#396229)),.UNSPECIFIED.,.F.,
 .F.,.F.)
B_SPLINE_SURFACE_WITH_KNOTS((4,4),(3,3),(-3.39528393502489E-6,3.73481232852737E-5),
(-0.00165018033303416,1.),.UNSPECIFIED.)
GEOMETRIC_REPRESENTATION_ITEM()
RATIONAL_B_SPLINE_SURFACE(((1.00048354385558,0.853487571660428,1.),(1.00047110510914,
0.857256476851519,1.),(1.00053193201099,0.838826096655876,1.),(1.00063970687716,
0.80617061531015,0.999999999999999)))
REPRESENTATION_ITEM('')
SURFACE()
);
#2860=(
BOUNDED_SURFACE()
B_SPLINE_SURFACE(3,2,((#396233,#396234,#396235),(#396236,#396237,#396238),
(#396239,#396240,#396241),(#396242,#396243,#396244)),.UNSPECIFIED.,.F.,
 .F.,.F.)
B_SPLINE_SURFACE_WITH_KNOTS((4,4),(3,3),(2.02993869230509E-5,5.39756952686906E-5),
(-0.000116281069786927,1.),.UNSPECIFIED.)
GEOMETRIC_REPRESENTATION_ITEM()
RATIONAL_B_SPLINE_SURFACE(((1.00001770479728,0.923870681143016,1.),(1.00001014104058,
0.956394275543437,1.),(1.00002037300276,0.912397594905671,1.),(1.00003390859465,
0.854195550869887,1.)))
REPRESENTATION_ITEM('')
SURFACE()
);
#2861=(
BOUNDED_SURFACE()
B_SPLINE_SURFACE(3,2,((#396337,#396338,#396339),(#396340,#396341,#396342),
(#396343,#396344,#396345),(#396346,#396347,#396348)),.UNSPECIFIED.,.F.,
 .F.,.F.)
B_SPLINE_SURFACE_WITH_KNOTS((4,4),(3,3),(0.00135801595889393,0.00148409170619832),
(0.,1.),.UNSPECIFIED.)
GEOMETRIC_REPRESENTATION_ITEM()
RATIONAL_B_SPLINE_SURFACE(((1.,0.818301933966445,1.),(1.,0.817226613172349,
1.),(1.,0.816179643373948,1.),(1.,0.815159387863656,1.)))
REPRESENTATION_ITEM('')
SURFACE()
);
#2862=(
BOUNDED_SURFACE()
B_SPLINE_SURFACE(3,2,((#396387,#396388,#396389),(#396390,#396391,#396392),
(#396393,#396394,#396395),(#396396,#396397,#396398)),.UNSPECIFIED.,.F.,
 .F.,.F.)
B_SPLINE_SURFACE_WITH_KNOTS((4,4),(3,3),(-1.54744435122057E-6,1.54744435122063E-5),
(-0.0151698983656125,1.01516989835623),.UNSPECIFIED.)
GEOMETRIC_REPRESENTATION_ITEM()
RATIONAL_B_SPLINE_SURFACE(((1.02018382473428,0.32449821941383,1.02018382472161),
(1.00401234488918,0.865716921710735,1.00401234488667),(1.00033622856789,
0.988747276629634,1.00033622856767),(1.,1.,1.)))
REPRESENTATION_ITEM('')
SURFACE()
);
#2863=(
BOUNDED_SURFACE()
B_SPLINE_SURFACE(3,2,((#396400,#396401,#396402),(#396403,#396404,#396405),
(#396406,#396407,#396408),(#396409,#396410,#396411)),.UNSPECIFIED.,.F.,
 .F.,.F.)
B_SPLINE_SURFACE_WITH_KNOTS((4,4),(3,3),(0.00137194782501028,0.00149814269699235),
(0.,1.),.UNSPECIFIED.)
GEOMETRIC_REPRESENTATION_ITEM()
RATIONAL_B_SPLINE_SURFACE(((1.,0.815158509402319,1.),(1.,0.81617904414816,
1.),(1.,0.817226308119937,1.),(1.,0.81830193948881,1.)))
REPRESENTATION_ITEM('')
SURFACE()
);
#2864=(
BOUNDED_SURFACE()
B_SPLINE_SURFACE(3,2,((#396455,#396456,#396457),(#396458,#396459,#396460),
(#396461,#396462,#396463),(#396464,#396465,#396466)),.UNSPECIFIED.,.F.,
 .F.,.F.)
B_SPLINE_SURFACE_WITH_KNOTS((4,4),(3,3),(1.55009486301137E-5,4.92065510474434E-5),
(-8.137595126164E-5,1.),.UNSPECIFIED.)
GEOMETRIC_REPRESENTATION_ITEM()
RATIONAL_B_SPLINE_SURFACE(((1.00002372912329,0.854200639599716,1.),(1.0000142358599,
0.912530301180545,1.),(1.00000710550469,0.956341495377451,1.),(1.00001238975905,
0.923873338137038,1.)))
REPRESENTATION_ITEM('')
SURFACE()
);
#2865=(
BOUNDED_SURFACE()
B_SPLINE_SURFACE(3,2,((#396470,#396471,#396472),(#396473,#396474,#396475),
(#396476,#396477,#396478),(#396479,#396480,#396481)),.UNSPECIFIED.,.F.,
 .F.,.F.)
B_SPLINE_SURFACE_WITH_KNOTS((4,4),(3,3),(-3.39934179457798E-6,3.73927597403568E-5),
(-0.00186004067401208,1.0006937331744),.UNSPECIFIED.)
GEOMETRIC_REPRESENTATION_ITEM()
RATIONAL_B_SPLINE_SURFACE(((1.00072100136048,0.806051963875378,1.00026859642691),
(1.00060048440148,0.838470803558667,1.00022369994496),(1.0005310644879,
0.857144632272393,1.00019783877219),(1.00054515072847,0.85335545953913,
1.00020308635437)))
REPRESENTATION_ITEM('')
SURFACE()
);
#2866=(
BOUNDED_SURFACE()
B_SPLINE_SURFACE(3,2,((#396483,#396484,#396485),(#396486,#396487,#396488),
(#396489,#396490,#396491),(#396492,#396493,#396494)),.UNSPECIFIED.,.F.,
 .F.,.F.)
B_SPLINE_SURFACE_WITH_KNOTS((4,4),(3,3),(-2.71050543121376E-19,9.54361881492172E-5),
(0.,1.),.UNSPECIFIED.)
GEOMETRIC_REPRESENTATION_ITEM()
RATIONAL_B_SPLINE_SURFACE(((1.,0.816715621142058,1.),(1.,0.815907587407936,
1.),(1.,0.815115959345221,1.),(1.,0.814339887349188,1.)))
REPRESENTATION_ITEM('')
SURFACE()
);
#2867=(
BOUNDED_SURFACE()
B_SPLINE_SURFACE(3,2,((#396496,#396497,#396498),(#396499,#396500,#396501),
(#396502,#396503,#396504),(#396505,#396506,#396507)),.UNSPECIFIED.,.F.,
 .F.,.F.)
B_SPLINE_SURFACE_WITH_KNOTS((4,4),(3,3),(-3.06625926906057E-19,4.68197758448208E-5),
(0.,1.),.UNSPECIFIED.)
GEOMETRIC_REPRESENTATION_ITEM()
RATIONAL_B_SPLINE_SURFACE(((1.,0.816715621142045,1.),(1.,0.953638980025204,
1.),(1.,0.954506925408053,1.),(1.,0.816715621142051,1.)))
REPRESENTATION_ITEM('')
SURFACE()
);
#2868=(
BOUNDED_SURFACE()
B_SPLINE_SURFACE(3,2,((#396509,#396510,#396511),(#396512,#396513,#396514),
(#396515,#396516,#396517),(#396518,#396519,#396520)),.UNSPECIFIED.,.F.,
 .F.,.F.)
B_SPLINE_SURFACE_WITH_KNOTS((4,4),(3,3),(-3.25260651745651E-19,9.54361881492173E-5),
(0.,1.),.UNSPECIFIED.)
GEOMETRIC_REPRESENTATION_ITEM()
RATIONAL_B_SPLINE_SURFACE(((1.,0.814339887349194,1.),(1.,0.815115959345209,
1.),(1.,0.815907587407937,1.),(1.,0.816715621142051,1.)))
REPRESENTATION_ITEM('')
SURFACE()
);
#2869=(
BOUNDED_SURFACE()
B_SPLINE_SURFACE(3,2,((#396522,#396523,#396524),(#396525,#396526,#396527),
(#396528,#396529,#396530),(#396531,#396532,#396533)),.UNSPECIFIED.,.F.,
 .F.,.F.)
B_SPLINE_SURFACE_WITH_KNOTS((4,4),(3,3),(-3.39528393502371E-6,3.73481232852731E-5),
(-0.00165018033284349,1.),.UNSPECIFIED.)
GEOMETRIC_REPRESENTATION_ITEM()
RATIONAL_B_SPLINE_SURFACE(((1.00048354385553,0.853487571660481,1.),(1.00047110510908,
0.857256476851499,1.),(1.00053193201093,0.838826096655967,1.),(1.00063970687708,
0.806170615310163,1.)))
REPRESENTATION_ITEM('')
SURFACE()
);
#2870=(
BOUNDED_SURFACE()
B_SPLINE_SURFACE(3,2,((#396537,#396538,#396539),(#396540,#396541,#396542),
(#396543,#396544,#396545),(#396546,#396547,#396548)),.UNSPECIFIED.,.F.,
 .F.,.F.)
B_SPLINE_SURFACE_WITH_KNOTS((4,4),(3,3),(2.02993869230509E-5,5.3975695268713E-5),
(-0.000116281069995185,1.),.UNSPECIFIED.)
GEOMETRIC_REPRESENTATION_ITEM()
RATIONAL_B_SPLINE_SURFACE(((1.00001770479731,0.923870681143002,1.),(1.0000101410406,
0.956394275543429,1.),(1.0000203730028,0.912397594905616,1.),(1.00003390859471,
0.854195550869726,1.)))
REPRESENTATION_ITEM('')
SURFACE()
);
#2871=(
BOUNDED_SURFACE()
B_SPLINE_SURFACE(3,2,((#396641,#396642,#396643),(#396644,#396645,#396646),
(#396647,#396648,#396649),(#396650,#396651,#396652)),.UNSPECIFIED.,.F.,
 .F.,.F.)
B_SPLINE_SURFACE_WITH_KNOTS((4,4),(3,3),(0.00135801595889393,0.00148409170619832),
(0.,1.),.UNSPECIFIED.)
GEOMETRIC_REPRESENTATION_ITEM()
RATIONAL_B_SPLINE_SURFACE(((1.,0.81830193396645,1.),(1.,0.817226613172347,
1.),(1.,0.816179643373947,1.),(1.,0.815159387863661,1.)))
REPRESENTATION_ITEM('')
SURFACE()
);
#2872=(
BOUNDED_SURFACE()
B_SPLINE_SURFACE(3,2,((#396691,#396692,#396693),(#396694,#396695,#396696),
(#396697,#396698,#396699),(#396700,#396701,#396702)),.UNSPECIFIED.,.F.,
 .F.,.F.)
B_SPLINE_SURFACE_WITH_KNOTS((4,4),(3,3),(-1.54744435122069E-6,1.54744435122069E-5),
(-0.0151698983596124,1.01516989836293),.UNSPECIFIED.)
GEOMETRIC_REPRESENTATION_ITEM()
RATIONAL_B_SPLINE_SURFACE(((1.02018382472617,0.324498219413415,1.02018382473066),
(1.00401234488758,0.865716921710511,1.00401234488847),(1.00033622856775,
0.988747276629721,1.00033622856782),(1.,1.,1.)))
REPRESENTATION_ITEM('')
SURFACE()
);
#2873=(
BOUNDED_SURFACE()
B_SPLINE_SURFACE(3,2,((#396704,#396705,#396706),(#396707,#396708,#396709),
(#396710,#396711,#396712),(#396713,#396714,#396715)),.UNSPECIFIED.,.F.,
 .F.,.F.)
B_SPLINE_SURFACE_WITH_KNOTS((4,4),(3,3),(0.00137194782501028,0.00149814269699235),
(0.,1.),.UNSPECIFIED.)
GEOMETRIC_REPRESENTATION_ITEM()
RATIONAL_B_SPLINE_SURFACE(((1.,0.815158509402317,1.),(1.,0.816179044148172,
1.),(1.,0.817226308119915,1.),(1.,0.818301939488811,1.)))
REPRESENTATION_ITEM('')
SURFACE()
);
#2874=(
BOUNDED_SURFACE()
B_SPLINE_SURFACE(3,2,((#396759,#396760,#396761),(#396762,#396763,#396764),
(#396765,#396766,#396767),(#396768,#396769,#396770)),.UNSPECIFIED.,.F.,
 .F.,.F.)
B_SPLINE_SURFACE_WITH_KNOTS((4,4),(3,3),(1.55009486301137E-5,4.92065510474434E-5),
(-8.1375951822287E-5,1.),.UNSPECIFIED.)
GEOMETRIC_REPRESENTATION_ITEM()
RATIONAL_B_SPLINE_SURFACE(((1.00002372912346,0.854200639599639,1.),(1.00001423585999,
0.912530301180504,1.),(1.00000710550474,0.95634149537741,1.),(1.00001238975914,
0.923873338137001,1.)))
REPRESENTATION_ITEM('')
SURFACE()
);
#2875=(
BOUNDED_SURFACE()
B_SPLINE_SURFACE(3,2,((#396774,#396775,#396776),(#396777,#396778,#396779),
(#396780,#396781,#396782),(#396783,#396784,#396785)),.UNSPECIFIED.,.F.,
 .F.,.F.)
B_SPLINE_SURFACE_WITH_KNOTS((4,4),(3,3),(-3.39934179457806E-6,3.73927597403567E-5),
(-0.00186004067406807,1.00069373317433),.UNSPECIFIED.)
GEOMETRIC_REPRESENTATION_ITEM()
RATIONAL_B_SPLINE_SURFACE(((1.0007210013605,0.806051963875368,1.00026859642689),
(1.0006004844015,0.838470803558668,1.00022369994494),(1.00053106448791,
0.857144632272412,1.00019783877218),(1.00054515072849,0.853355459539114,
1.00020308635435)))
REPRESENTATION_ITEM('')
SURFACE()
);
#2876=(
BOUNDED_SURFACE()
B_SPLINE_SURFACE(3,2,((#396787,#396788,#396789),(#396790,#396791,#396792),
(#396793,#396794,#396795),(#396796,#396797,#396798)),.UNSPECIFIED.,.F.,
 .F.,.F.)
B_SPLINE_SURFACE_WITH_KNOTS((4,4),(3,3),(-5.42101086242752E-20,9.54361881492173E-5),
(0.,1.),.UNSPECIFIED.)
GEOMETRIC_REPRESENTATION_ITEM()
RATIONAL_B_SPLINE_SURFACE(((1.,0.81671562114205,1.),(1.,0.815907587407947,
1.),(1.,0.815115959345199,1.),(1.,0.814339887349193,1.)))
REPRESENTATION_ITEM('')
SURFACE()
);
#2877=(
BOUNDED_SURFACE()
B_SPLINE_SURFACE(3,2,((#396800,#396801,#396802),(#396803,#396804,#396805),
(#396806,#396807,#396808),(#396809,#396810,#396811)),.UNSPECIFIED.,.F.,
 .F.,.F.)
B_SPLINE_SURFACE_WITH_KNOTS((4,4),(3,3),(7.79270311473956E-20,4.6819775844821E-5),
(0.,1.),.UNSPECIFIED.)
GEOMETRIC_REPRESENTATION_ITEM()
RATIONAL_B_SPLINE_SURFACE(((1.,0.81671562114205,1.),(1.,0.953638980025221,
1.),(1.,0.954506925408034,1.),(1.,0.816715621142064,1.)))
REPRESENTATION_ITEM('')
SURFACE()
);
#2878=(
BOUNDED_SURFACE()
B_SPLINE_SURFACE(3,2,((#396813,#396814,#396815),(#396816,#396817,#396818),
(#396819,#396820,#396821),(#396822,#396823,#396824)),.UNSPECIFIED.,.F.,
 .F.,.F.)
B_SPLINE_SURFACE_WITH_KNOTS((4,4),(3,3),(1.0842021724855E-19,9.54361881492179E-5),
(0.,1.),.UNSPECIFIED.)
GEOMETRIC_REPRESENTATION_ITEM()
RATIONAL_B_SPLINE_SURFACE(((1.,0.814339887349205,1.),(1.,0.815115959345194,
1.),(1.,0.815907587407962,1.),(1.,0.816715621142051,1.)))
REPRESENTATION_ITEM('')
SURFACE()
);
#2879=(
BOUNDED_SURFACE()
B_SPLINE_SURFACE(3,2,((#396826,#396827,#396828),(#396829,#396830,#396831),
(#396832,#396833,#396834),(#396835,#396836,#396837)),.UNSPECIFIED.,.F.,
 .F.,.F.)
B_SPLINE_SURFACE_WITH_KNOTS((4,4),(3,3),(-3.39528393502484E-6,3.73481232852731E-5),
(-0.00165018033298142,1.),.UNSPECIFIED.)
GEOMETRIC_REPRESENTATION_ITEM()
RATIONAL_B_SPLINE_SURFACE(((1.00048354385557,0.853487571660459,1.),(1.00047110510912,
0.857256476851485,1.),(1.00053193201098,0.838826096655939,1.),(1.00063970687714,
0.806170615310147,1.)))
REPRESENTATION_ITEM('')
SURFACE()
);
#2880=(
BOUNDED_SURFACE()
B_SPLINE_SURFACE(3,2,((#396841,#396842,#396843),(#396844,#396845,#396846),
(#396847,#396848,#396849),(#396850,#396851,#396852)),.UNSPECIFIED.,.F.,
 .F.,.F.)
B_SPLINE_SURFACE_WITH_KNOTS((4,4),(3,3),(2.02993869230509E-5,5.3975695268712E-5),
(-0.00011628106945422,1.),.UNSPECIFIED.)
GEOMETRIC_REPRESENTATION_ITEM()
RATIONAL_B_SPLINE_SURFACE(((1.00001770479723,0.923870681143046,1.),(1.00001014104055,
0.956394275543465,1.),(1.0000203730027,0.912397594905649,1.),(1.00003390859455,
0.854195550869809,1.)))
REPRESENTATION_ITEM('')
SURFACE()
);
#2881=(
BOUNDED_SURFACE()
B_SPLINE_SURFACE(3,2,((#396945,#396946,#396947),(#396948,#396949,#396950),
(#396951,#396952,#396953),(#396954,#396955,#396956)),.UNSPECIFIED.,.F.,
 .F.,.F.)
B_SPLINE_SURFACE_WITH_KNOTS((4,4),(3,3),(0.00135801595889393,0.00148409170619832),
(0.,1.),.UNSPECIFIED.)
GEOMETRIC_REPRESENTATION_ITEM()
RATIONAL_B_SPLINE_SURFACE(((1.,0.818301933966443,1.),(1.,0.817226613172376,
1.),(1.,0.816179643373924,1.),(1.,0.815159387863663,1.)))
REPRESENTATION_ITEM('')
SURFACE()
);
#2882=(
BOUNDED_SURFACE()
B_SPLINE_SURFACE(3,2,((#396995,#396996,#396997),(#396998,#396999,#397000),
(#397001,#397002,#397003),(#397004,#397005,#397006)),.UNSPECIFIED.,.F.,
 .F.,.F.)
B_SPLINE_SURFACE_WITH_KNOTS((4,4),(3,3),(-1.5474443512208E-6,1.54744435122078E-5),
(-0.0151698983647775,1.),.UNSPECIFIED.)
GEOMETRIC_REPRESENTATION_ITEM()
RATIONAL_B_SPLINE_SURFACE(((1.02018382473315,0.334740937354771,1.),(1.00401234488896,
0.867753072812997,1.),(1.00033622856787,0.988917903080786,1.),(1.,1.,1.)))
REPRESENTATION_ITEM('')
SURFACE()
);
#2883=(
BOUNDED_SURFACE()
B_SPLINE_SURFACE(3,2,((#397008,#397009,#397010),(#397011,#397012,#397013),
(#397014,#397015,#397016),(#397017,#397018,#397019)),.UNSPECIFIED.,.F.,
 .F.,.F.)
B_SPLINE_SURFACE_WITH_KNOTS((4,4),(3,3),(0.00137194782501028,0.00149814269699235),
(0.,1.),.UNSPECIFIED.)
GEOMETRIC_REPRESENTATION_ITEM()
RATIONAL_B_SPLINE_SURFACE(((1.,0.815158509402318,1.),(1.,0.816179044148164,
1.),(1.,0.81722630811994,1.),(1.,0.818301939488808,1.)))
REPRESENTATION_ITEM('')
SURFACE()
);
#2884=(
BOUNDED_SURFACE()
B_SPLINE_SURFACE(3,2,((#397063,#397064,#397065),(#397066,#397067,#397068),
(#397069,#397070,#397071),(#397072,#397073,#397074)),.UNSPECIFIED.,.F.,
 .F.,.F.)
B_SPLINE_SURFACE_WITH_KNOTS((4,4),(3,3),(1.55009486301137E-5,4.92065510474432E-5),
(-8.13759513958142E-5,1.),.UNSPECIFIED.)
GEOMETRIC_REPRESENTATION_ITEM()
RATIONAL_B_SPLINE_SURFACE(((1.00002372912333,0.854200639599695,1.),(1.00001423585992,
0.912530301180542,1.),(1.0000071055047,0.956341495377438,1.),(1.00001238975907,
0.923873338137029,1.)))
REPRESENTATION_ITEM('')
SURFACE()
);
#2885=(
BOUNDED_SURFACE()
B_SPLINE_SURFACE(3,2,((#397078,#397079,#397080),(#397081,#397082,#397083),
(#397084,#397085,#397086),(#397087,#397088,#397089)),.UNSPECIFIED.,.F.,
 .F.,.F.)
B_SPLINE_SURFACE_WITH_KNOTS((4,4),(3,3),(-3.39934179457826E-6,3.73927597403565E-5),
(-0.00186004067394221,1.00069373317415),.UNSPECIFIED.)
GEOMETRIC_REPRESENTATION_ITEM()
RATIONAL_B_SPLINE_SURFACE(((1.00072100136045,0.806051963875464,1.00026859642681),
(1.00060048440146,0.838470803558715,1.00022369994488),(1.00053106448788,
0.857144632272451,1.00019783877212),(1.00054515072845,0.853355459539171,
1.0002030863543)))
REPRESENTATION_ITEM('')
SURFACE()
);
#2886=(
BOUNDED_SURFACE()
B_SPLINE_SURFACE(3,2,((#397091,#397092,#397093),(#397094,#397095,#397096),
(#397097,#397098,#397099),(#397100,#397101,#397102)),.UNSPECIFIED.,.F.,
 .F.,.F.)
B_SPLINE_SURFACE_WITH_KNOTS((4,4),(3,3),(-2.71050543121376E-19,9.54361881492172E-5),
(0.,1.),.UNSPECIFIED.)
GEOMETRIC_REPRESENTATION_ITEM()
RATIONAL_B_SPLINE_SURFACE(((1.,0.81671562114205,1.),(1.,0.815907587407935,
1.),(1.,0.815115959345205,1.),(1.,0.814339887349194,1.)))
REPRESENTATION_ITEM('')
SURFACE()
);
#2887=(
BOUNDED_SURFACE()
B_SPLINE_SURFACE(3,2,((#397104,#397105,#397106),(#397107,#397108,#397109),
(#397110,#397111,#397112),(#397113,#397114,#397115)),.UNSPECIFIED.,.F.,
 .F.,.F.)
B_SPLINE_SURFACE_WITH_KNOTS((4,4),(3,3),(1.38913403349705E-19,4.68197758448206E-5),
(0.,1.),.UNSPECIFIED.)
GEOMETRIC_REPRESENTATION_ITEM()
RATIONAL_B_SPLINE_SURFACE(((1.,0.816715621142052,1.),(1.,0.953638980025209,
1.),(1.,0.954506925408051,1.),(1.,0.816715621142057,1.)))
REPRESENTATION_ITEM('')
SURFACE()
);
#2888=(
BOUNDED_SURFACE()
B_SPLINE_SURFACE(3,2,((#397117,#397118,#397119),(#397120,#397121,#397122),
(#397123,#397124,#397125),(#397126,#397127,#397128)),.UNSPECIFIED.,.F.,
 .F.,.F.)
B_SPLINE_SURFACE_WITH_KNOTS((4,4),(3,3),(-1.0842021724855E-19,9.54361881492178E-5),
(0.,1.),.UNSPECIFIED.)
GEOMETRIC_REPRESENTATION_ITEM()
RATIONAL_B_SPLINE_SURFACE(((1.,0.814339887349202,1.),(1.,0.815115959345215,
1.),(1.,0.815907587407934,1.),(1.,0.816715621142051,1.)))
REPRESENTATION_ITEM('')
SURFACE()
);
#2889=(
BOUNDED_SURFACE()
B_SPLINE_SURFACE(3,2,((#397130,#397131,#397132),(#397133,#397134,#397135),
(#397136,#397137,#397138),(#397139,#397140,#397141)),.UNSPECIFIED.,.F.,
 .F.,.F.)
B_SPLINE_SURFACE_WITH_KNOTS((4,4),(3,3),(-3.39528393502384E-6,3.73481232852732E-5),
(-0.00165018033264819,1.),.UNSPECIFIED.)
GEOMETRIC_REPRESENTATION_ITEM()
RATIONAL_B_SPLINE_SURFACE(((1.00048354385547,0.853487571660489,1.),(1.00047110510903,
0.857256476851558,1.),(1.00053193201087,0.838826096655971,1.),(1.00063970687701,
0.806170615310218,1.)))
REPRESENTATION_ITEM('')
SURFACE()
);
#2890=(
BOUNDED_SURFACE()
B_SPLINE_SURFACE(3,2,((#397145,#397146,#397147),(#397148,#397149,#397150),
(#397151,#397152,#397153),(#397154,#397155,#397156)),.UNSPECIFIED.,.F.,
 .F.,.F.)
B_SPLINE_SURFACE_WITH_KNOTS((4,4),(3,3),(2.0299386923051E-5,5.39756952687132E-5),
(-0.000116281069686216,1.),.UNSPECIFIED.)
GEOMETRIC_REPRESENTATION_ITEM()
RATIONAL_B_SPLINE_SURFACE(((1.00001770479726,0.923870681143028,1.),(1.00001014104057,
0.956394275543452,1.),(1.00002037300274,0.912397594905648,1.),(1.00003390859462,
0.85419555086976,1.)))
REPRESENTATION_ITEM('')
SURFACE()
);
#2891=(
BOUNDED_SURFACE()
B_SPLINE_SURFACE(3,2,((#397249,#397250,#397251),(#397252,#397253,#397254),
(#397255,#397256,#397257),(#397258,#397259,#397260)),.UNSPECIFIED.,.F.,
 .F.,.F.)
B_SPLINE_SURFACE_WITH_KNOTS((4,4),(3,3),(0.00135801595889393,0.00148409170619832),
(0.,1.),.UNSPECIFIED.)
GEOMETRIC_REPRESENTATION_ITEM()
RATIONAL_B_SPLINE_SURFACE(((1.,0.818301933966443,1.),(1.,0.81722661317235,
1.),(1.,0.816179643373951,1.),(1.,0.815159387863653,1.)))
REPRESENTATION_ITEM('')
SURFACE()
);
#2892=(
BOUNDED_SURFACE()
B_SPLINE_SURFACE(3,2,((#397299,#397300,#397301),(#397302,#397303,#397304),
(#397305,#397306,#397307),(#397308,#397309,#397310)),.UNSPECIFIED.,.F.,
 .F.,.F.)
B_SPLINE_SURFACE_WITH_KNOTS((4,4),(3,3),(-1.54744435122068E-6,1.54744435122077E-5),
(-0.0151698983618832,1.01516989836046),.UNSPECIFIED.)
GEOMETRIC_REPRESENTATION_ITEM()
RATIONAL_B_SPLINE_SURFACE(((1.02018382472924,0.324498219413552,1.02018382472731),
(1.00401234488819,0.865716921710482,1.00401234488781),(1.0003362285678,
0.98874727662976,1.00033622856777),(1.,1.,1.)))
REPRESENTATION_ITEM('')
SURFACE()
);
#2893=(
BOUNDED_SURFACE()
B_SPLINE_SURFACE(3,2,((#397312,#397313,#397314),(#397315,#397316,#397317),
(#397318,#397319,#397320),(#397321,#397322,#397323)),.UNSPECIFIED.,.F.,
 .F.,.F.)
B_SPLINE_SURFACE_WITH_KNOTS((4,4),(3,3),(0.00137194782501028,0.00149814269699235),
(0.,1.),.UNSPECIFIED.)
GEOMETRIC_REPRESENTATION_ITEM()
RATIONAL_B_SPLINE_SURFACE(((1.,0.815158509402319,1.),(1.,0.816179044148173,
1.),(1.,0.817226308119922,1.),(1.,0.818301939488809,1.)))
REPRESENTATION_ITEM('')
SURFACE()
);
#2894=(
BOUNDED_SURFACE()
B_SPLINE_SURFACE(3,2,((#397367,#397368,#397369),(#397370,#397371,#397372),
(#397373,#397374,#397375),(#397376,#397377,#397378)),.UNSPECIFIED.,.F.,
 .F.,.F.)
B_SPLINE_SURFACE_WITH_KNOTS((4,4),(3,3),(1.55009486301137E-5,4.92065510474431E-5),
(-8.13759512503572E-5,1.),.UNSPECIFIED.)
GEOMETRIC_REPRESENTATION_ITEM()
RATIONAL_B_SPLINE_SURFACE(((1.00002372912329,0.854200639599723,1.),(1.00001423585989,
0.912530301180552,1.),(1.00000710550469,0.956341495377439,1.),(1.00001238975905,
0.923873338137042,1.)))
REPRESENTATION_ITEM('')
SURFACE()
);
#2895=(
BOUNDED_SURFACE()
B_SPLINE_SURFACE(3,2,((#397382,#397383,#397384),(#397385,#397386,#397387),
(#397388,#397389,#397390),(#397391,#397392,#397393)),.UNSPECIFIED.,.F.,
 .F.,.F.)
B_SPLINE_SURFACE_WITH_KNOTS((4,4),(3,3),(-3.39934179457864E-6,3.73927597403564E-5),
(-0.00186004067415249,1.00069373317438),.UNSPECIFIED.)
GEOMETRIC_REPRESENTATION_ITEM()
RATIONAL_B_SPLINE_SURFACE(((1.00072100136053,0.806051963875349,1.0002685964269),
(1.00060048440153,0.838470803558665,1.00022369994495),(1.00053106448794,
0.857144632272378,1.00019783877219),(1.00054515072851,0.853355459539108,
1.00020308635436)))
REPRESENTATION_ITEM('')
SURFACE()
);
#2896=(
BOUNDED_SURFACE()
B_SPLINE_SURFACE(3,2,((#397395,#397396,#397397),(#397398,#397399,#397400),
(#397401,#397402,#397403),(#397404,#397405,#397406)),.UNSPECIFIED.,.F.,
 .F.,.F.)
B_SPLINE_SURFACE_WITH_KNOTS((4,4),(3,3),(5.42101086242752E-20,9.54361881492173E-5),
(0.,1.),.UNSPECIFIED.)
GEOMETRIC_REPRESENTATION_ITEM()
RATIONAL_B_SPLINE_SURFACE(((1.,0.81671562114205,1.),(1.,0.815907587407942,
1.),(1.,0.815115959345208,1.),(1.,0.814339887349183,1.)))
REPRESENTATION_ITEM('')
SURFACE()
);
#2897=(
BOUNDED_SURFACE()
B_SPLINE_SURFACE(3,2,((#397408,#397409,#397410),(#397411,#397412,#397413),
(#397414,#397415,#397416),(#397417,#397418,#397419)),.UNSPECIFIED.,.F.,
 .F.,.F.)
B_SPLINE_SURFACE_WITH_KNOTS((4,4),(3,3),(-1.01643953670516E-20,4.68197758448209E-5),
(0.,1.),.UNSPECIFIED.)
GEOMETRIC_REPRESENTATION_ITEM()
RATIONAL_B_SPLINE_SURFACE(((1.,0.816715621142051,1.),(1.,0.953638980025216,
1.),(1.,0.954506925408042,1.),(1.,0.816715621142057,1.)))
REPRESENTATION_ITEM('')
SURFACE()
);
#2898=(
BOUNDED_SURFACE()
B_SPLINE_SURFACE(3,2,((#397421,#397422,#397423),(#397424,#397425,#397426),
(#397427,#397428,#397429),(#397430,#397431,#397432)),.UNSPECIFIED.,.F.,
 .F.,.F.)
B_SPLINE_SURFACE_WITH_KNOTS((4,4),(3,3),(-5.42101086242752E-20,9.54361881492176E-5),
(0.,1.),.UNSPECIFIED.)
GEOMETRIC_REPRESENTATION_ITEM()
RATIONAL_B_SPLINE_SURFACE(((1.,0.814339887349195,1.),(1.,0.8151159593452,
1.),(1.,0.815907587407949,1.),(1.,0.816715621142051,1.)))
REPRESENTATION_ITEM('')
SURFACE()
);
#2899=(
BOUNDED_SURFACE()
B_SPLINE_SURFACE(3,2,((#397434,#397435,#397436),(#397437,#397438,#397439),
(#397440,#397441,#397442),(#397443,#397444,#397445)),.UNSPECIFIED.,.F.,
 .F.,.F.)
B_SPLINE_SURFACE_WITH_KNOTS((4,4),(3,3),(-3.3952839350248E-6,3.73481232852737E-5),
(-0.00165018033327807,1.),.UNSPECIFIED.)
GEOMETRIC_REPRESENTATION_ITEM()
RATIONAL_B_SPLINE_SURFACE(((1.00048354385565,0.853487571660403,1.),(1.00047110510921,
0.857256476851452,1.),(1.00053193201107,0.838826096655878,1.),(1.00063970687725,
0.806170615310095,1.)))
REPRESENTATION_ITEM('')
SURFACE()
);
#2900=(
BOUNDED_SURFACE()
B_SPLINE_SURFACE(3,2,((#397449,#397450,#397451),(#397452,#397453,#397454),
(#397455,#397456,#397457),(#397458,#397459,#397460)),.UNSPECIFIED.,.F.,
 .F.,.F.)
B_SPLINE_SURFACE_WITH_KNOTS((4,4),(3,3),(2.02993869230509E-5,5.39756952687128E-5),
(-0.000116281069711852,1.),.UNSPECIFIED.)
GEOMETRIC_REPRESENTATION_ITEM()
RATIONAL_B_SPLINE_SURFACE(((1.00001770479727,0.923870681143028,1.),(1.00001014104057,
0.956394275543455,1.),(1.00002037300275,0.912397594905626,1.),(1.00003390859463,
0.854195550869769,1.)))
REPRESENTATION_ITEM('')
SURFACE()
);
#2901=(
BOUNDED_SURFACE()
B_SPLINE_SURFACE(3,2,((#397553,#397554,#397555),(#397556,#397557,#397558),
(#397559,#397560,#397561),(#397562,#397563,#397564)),.UNSPECIFIED.,.F.,
 .F.,.F.)
B_SPLINE_SURFACE_WITH_KNOTS((4,4),(3,3),(0.00135801595889393,0.00148409170619832),
(0.,1.),.UNSPECIFIED.)
GEOMETRIC_REPRESENTATION_ITEM()
RATIONAL_B_SPLINE_SURFACE(((1.,0.818301933966442,1.),(1.,0.817226613172341,
1.),(1.,0.816179643373949,1.),(1.,0.815159387863656,1.)))
REPRESENTATION_ITEM('')
SURFACE()
);
#2902=(
BOUNDED_SURFACE()
B_SPLINE_SURFACE(3,2,((#397603,#397604,#397605),(#397606,#397607,#397608),
(#397609,#397610,#397611),(#397612,#397613,#397614)),.UNSPECIFIED.,.F.,
 .F.,.F.)
B_SPLINE_SURFACE_WITH_KNOTS((4,4),(3,3),(-1.54744435121991E-6,1.54744435122074E-5),
(-0.0151698983710202,1.),.UNSPECIFIED.)
GEOMETRIC_REPRESENTATION_ITEM()
RATIONAL_B_SPLINE_SURFACE(((1.02018382474158,0.334740937350775,1.),(1.00401234489064,
0.867753072812127,1.),(1.00033622856801,0.988917903080755,1.),(1.,1.,1.)))
REPRESENTATION_ITEM('')
SURFACE()
);
#2903=(
BOUNDED_SURFACE()
B_SPLINE_SURFACE(3,2,((#397616,#397617,#397618),(#397619,#397620,#397621),
(#397622,#397623,#397624),(#397625,#397626,#397627)),.UNSPECIFIED.,.F.,
 .F.,.F.)
B_SPLINE_SURFACE_WITH_KNOTS((4,4),(3,3),(0.00137194782501028,0.00149814269699235),
(0.,1.),.UNSPECIFIED.)
GEOMETRIC_REPRESENTATION_ITEM()
RATIONAL_B_SPLINE_SURFACE(((1.,0.815158509402318,1.),(1.,0.816179044148172,
1.),(1.,0.81722630811991,1.),(1.,0.818301939488818,1.)))
REPRESENTATION_ITEM('')
SURFACE()
);
#2904=(
BOUNDED_SURFACE()
B_SPLINE_SURFACE(3,2,((#397671,#397672,#397673),(#397674,#397675,#397676),
(#397677,#397678,#397679),(#397680,#397681,#397682)),.UNSPECIFIED.,.F.,
 .F.,.F.)
B_SPLINE_SURFACE_WITH_KNOTS((4,4),(3,3),(1.55009486301137E-5,4.92065510474433E-5),
(-8.13759517002211E-5,1.),.UNSPECIFIED.)
GEOMETRIC_REPRESENTATION_ITEM()
RATIONAL_B_SPLINE_SURFACE(((1.00002372912342,0.85420063959964,1.),(1.00001423585997,
0.912530301180541,1.),(1.00000710550473,0.956341495377402,1.),(1.00001238975912,
0.923873338137012,1.)))
REPRESENTATION_ITEM('')
SURFACE()
);
#2905=(
BOUNDED_SURFACE()
B_SPLINE_SURFACE(3,2,((#397686,#397687,#397688),(#397689,#397690,#397691),
(#397692,#397693,#397694),(#397695,#397696,#397697)),.UNSPECIFIED.,.F.,
 .F.,.F.)
B_SPLINE_SURFACE_WITH_KNOTS((4,4),(3,3),(-3.39934179457822E-6,3.73927597403565E-5),
(-0.00186004067409689,1.00069373317422),.UNSPECIFIED.)
GEOMETRIC_REPRESENTATION_ITEM()
RATIONAL_B_SPLINE_SURFACE(((1.00072100136051,0.806051963875408,1.00026859642684),
(1.00060048440151,0.838470803558674,1.0002236999449),(1.00053106448792,
0.857144632272417,1.00019783877215),(1.0005451507285,0.853355459539137,
1.00020308635432)))
REPRESENTATION_ITEM('')
SURFACE()
);
#2906=(
BOUNDED_SURFACE()
B_SPLINE_SURFACE(3,2,((#397699,#397700,#397701),(#397702,#397703,#397704),
(#397705,#397706,#397707),(#397708,#397709,#397710)),.UNSPECIFIED.,.F.,
 .F.,.F.)
B_SPLINE_SURFACE_WITH_KNOTS((4,4),(3,3),(0.,9.54361881492174E-5),(0.,1.),
 .UNSPECIFIED.)
GEOMETRIC_REPRESENTATION_ITEM()
RATIONAL_B_SPLINE_SURFACE(((1.,0.81671562114205,1.),(1.,0.815907587407957,
1.),(1.,0.815115959345199,1.),(1.,0.814339887349194,1.)))
REPRESENTATION_ITEM('')
SURFACE()
);
#2907=(
BOUNDED_SURFACE()
B_SPLINE_SURFACE(3,2,((#397712,#397713,#397714),(#397715,#397716,#397717),
(#397718,#397719,#397720),(#397721,#397722,#397723)),.UNSPECIFIED.,.F.,
 .F.,.F.)
B_SPLINE_SURFACE_WITH_KNOTS((4,4),(3,3),(-2.03287907341032E-20,4.68197758448207E-5),
(0.,1.),.UNSPECIFIED.)
GEOMETRIC_REPRESENTATION_ITEM()
RATIONAL_B_SPLINE_SURFACE(((1.,0.816715621142051,1.),(1.,0.953638980025206,
1.),(1.,0.95450692540804,1.),(1.,0.81671562114206,1.)))
REPRESENTATION_ITEM('')
SURFACE()
);
#2908=(
BOUNDED_SURFACE()
B_SPLINE_SURFACE(3,2,((#397725,#397726,#397727),(#397728,#397729,#397730),
(#397731,#397732,#397733),(#397734,#397735,#397736)),.UNSPECIFIED.,.F.,
 .F.,.F.)
B_SPLINE_SURFACE_WITH_KNOTS((4,4),(3,3),(-1.0842021724855E-19,9.54361881492177E-5),
(0.,1.),.UNSPECIFIED.)
GEOMETRIC_REPRESENTATION_ITEM()
RATIONAL_B_SPLINE_SURFACE(((1.,0.814339887349194,1.),(1.,0.815115959345219,
1.),(1.,0.81590758740793,1.),(1.,0.816715621142051,1.)))
REPRESENTATION_ITEM('')
SURFACE()
);
#2909=(
BOUNDED_SURFACE()
B_SPLINE_SURFACE(3,2,((#397738,#397739,#397740),(#397741,#397742,#397743),
(#397744,#397745,#397746),(#397747,#397748,#397749)),.UNSPECIFIED.,.F.,
 .F.,.F.)
B_SPLINE_SURFACE_WITH_KNOTS((4,4),(3,3),(-3.39528393502491E-6,3.73481232852735E-5),
(-0.00165018033281841,1.),.UNSPECIFIED.)
GEOMETRIC_REPRESENTATION_ITEM()
RATIONAL_B_SPLINE_SURFACE(((1.00048354385552,0.853487571660464,1.),(1.00047110510907,
0.85725647685154,1.),(1.00053193201092,0.838826096655927,1.),(1.00063970687707,
0.8061706153102,1.)))
REPRESENTATION_ITEM('')
SURFACE()
);
#2910=(
BOUNDED_SURFACE()
B_SPLINE_SURFACE(3,2,((#397753,#397754,#397755),(#397756,#397757,#397758),
(#397759,#397760,#397761),(#397762,#397763,#397764)),.UNSPECIFIED.,.F.,
 .F.,.F.)
B_SPLINE_SURFACE_WITH_KNOTS((4,4),(3,3),(2.02993869230509E-5,5.39756952687121E-5),
(-0.000116281069798229,1.),.UNSPECIFIED.)
GEOMETRIC_REPRESENTATION_ITEM()
RATIONAL_B_SPLINE_SURFACE(((1.00001770479728,0.92387068114302,1.),(1.00001014104058,
0.956394275543454,1.),(1.00002037300276,0.912397594905629,1.),(1.00003390859465,
0.854195550869759,1.)))
REPRESENTATION_ITEM('')
SURFACE()
);
#2911=(
BOUNDED_SURFACE()
B_SPLINE_SURFACE(3,2,((#397857,#397858,#397859),(#397860,#397861,#397862),
(#397863,#397864,#397865),(#397866,#397867,#397868)),.UNSPECIFIED.,.F.,
 .F.,.F.)
B_SPLINE_SURFACE_WITH_KNOTS((4,4),(3,3),(0.00135801595889393,0.00148409170619832),
(0.,1.),.UNSPECIFIED.)
GEOMETRIC_REPRESENTATION_ITEM()
RATIONAL_B_SPLINE_SURFACE(((1.,0.818301933966453,1.),(1.,0.817226613172341,
1.),(1.,0.816179643373938,1.),(1.,0.815159387863655,1.)))
REPRESENTATION_ITEM('')
SURFACE()
);
#2912=(
BOUNDED_SURFACE()
B_SPLINE_SURFACE(3,2,((#397907,#397908,#397909),(#397910,#397911,#397912),
(#397913,#397914,#397915),(#397916,#397917,#397918)),.UNSPECIFIED.,.F.,
 .F.,.F.)
B_SPLINE_SURFACE_WITH_KNOTS((4,4),(3,3),(-1.54744435122067E-6,1.54744435122074E-5),
(-0.0151698983708486,1.01516989835091),.UNSPECIFIED.)
GEOMETRIC_REPRESENTATION_ITEM()
RATIONAL_B_SPLINE_SURFACE(((1.02018382474135,0.324498219413826,1.02018382471442),
(1.00401234489059,0.865716921710718,1.00401234488524),(1.000336228568,0.9887472766297,
1.00033622856755),(1.,1.,1.)))
REPRESENTATION_ITEM('')
SURFACE()
);
#2913=(
BOUNDED_SURFACE()
B_SPLINE_SURFACE(3,2,((#397920,#397921,#397922),(#397923,#397924,#397925),
(#397926,#397927,#397928),(#397929,#397930,#397931)),.UNSPECIFIED.,.F.,
 .F.,.F.)
B_SPLINE_SURFACE_WITH_KNOTS((4,4),(3,3),(0.00137194782501028,0.00149814269699235),
(0.,1.),.UNSPECIFIED.)
GEOMETRIC_REPRESENTATION_ITEM()
RATIONAL_B_SPLINE_SURFACE(((1.,0.815158509402318,1.),(1.,0.816179044148168,
1.),(1.,0.817226308119929,1.),(1.,0.818301939488811,1.)))
REPRESENTATION_ITEM('')
SURFACE()
);
#2914=(
BOUNDED_SURFACE()
B_SPLINE_SURFACE(3,2,((#397975,#397976,#397977),(#397978,#397979,#397980),
(#397981,#397982,#397983),(#397984,#397985,#397986)),.UNSPECIFIED.,.F.,
 .F.,.F.)
B_SPLINE_SURFACE_WITH_KNOTS((4,4),(3,3),(1.55009486301137E-5,4.92065510474431E-5),
(-8.13759513342479E-5,1.),.UNSPECIFIED.)
GEOMETRIC_REPRESENTATION_ITEM()
RATIONAL_B_SPLINE_SURFACE(((1.00002372912331,0.854200639599702,1.),(1.00001423585991,
0.912530301180565,1.),(1.00000710550469,0.95634149537742,1.),(1.00001238975906,
0.923873338137036,1.)))
REPRESENTATION_ITEM('')
SURFACE()
);
#2915=(
BOUNDED_SURFACE()
B_SPLINE_SURFACE(3,2,((#397990,#397991,#397992),(#397993,#397994,#397995),
(#397996,#397997,#397998),(#397999,#398000,#398001)),.UNSPECIFIED.,.F.,
 .F.,.F.)
B_SPLINE_SURFACE_WITH_KNOTS((4,4),(3,3),(-3.39934179457801E-6,3.73927597403567E-5),
(-0.00186004067410277,1.00069373317419),.UNSPECIFIED.)
GEOMETRIC_REPRESENTATION_ITEM()
RATIONAL_B_SPLINE_SURFACE(((1.00072100136051,0.806051963875423,1.00026859642683),
(1.00060048440151,0.838470803558641,1.00022369994489),(1.00053106448792,
0.857144632272466,1.00019783877214),(1.0005451507285,0.853355459539117,
1.00020308635431)))
REPRESENTATION_ITEM('')
SURFACE()
);
#2916=(
BOUNDED_SURFACE()
B_SPLINE_SURFACE(3,2,((#398003,#398004,#398005),(#398006,#398007,#398008),
(#398009,#398010,#398011),(#398012,#398013,#398014)),.UNSPECIFIED.,.F.,
 .F.,.F.)
B_SPLINE_SURFACE_WITH_KNOTS((4,4),(3,3),(0.,9.54361881492176E-5),(0.,1.),
 .UNSPECIFIED.)
GEOMETRIC_REPRESENTATION_ITEM()
RATIONAL_B_SPLINE_SURFACE(((1.,0.816715621142051,1.),(1.,0.815907587407931,
1.),(1.,0.815115959345217,1.),(1.,0.814339887349183,1.)))
REPRESENTATION_ITEM('')
SURFACE()
);
#2917=(
BOUNDED_SURFACE()
B_SPLINE_SURFACE(3,2,((#398016,#398017,#398018),(#398019,#398020,#398021),
(#398022,#398023,#398024),(#398025,#398026,#398027)),.UNSPECIFIED.,.F.,
 .F.,.F.)
B_SPLINE_SURFACE_WITH_KNOTS((4,4),(3,3),(-1.37219337455197E-19,4.68197758448213E-5),
(0.,1.),.UNSPECIFIED.)
GEOMETRIC_REPRESENTATION_ITEM()
RATIONAL_B_SPLINE_SURFACE(((1.,0.816715621142045,1.),(1.,0.953638980025202,
1.),(1.,0.95450692540806,1.),(1.,0.816715621142052,1.)))
REPRESENTATION_ITEM('')
SURFACE()
);
#2918=(
BOUNDED_SURFACE()
B_SPLINE_SURFACE(3,2,((#398029,#398030,#398031),(#398032,#398033,#398034),
(#398035,#398036,#398037),(#398038,#398039,#398040)),.UNSPECIFIED.,.F.,
 .F.,.F.)
B_SPLINE_SURFACE_WITH_KNOTS((4,4),(3,3),(-1.0842021724855E-19,9.54361881492175E-5),
(0.,1.),.UNSPECIFIED.)
GEOMETRIC_REPRESENTATION_ITEM()
RATIONAL_B_SPLINE_SURFACE(((1.,0.814339887349196,1.),(1.,0.81511595934521,
1.),(1.,0.815907587407948,1.),(1.,0.816715621142052,1.)))
REPRESENTATION_ITEM('')
SURFACE()
);
#2919=(
BOUNDED_SURFACE()
B_SPLINE_SURFACE(3,2,((#398042,#398043,#398044),(#398045,#398046,#398047),
(#398048,#398049,#398050),(#398051,#398052,#398053)),.UNSPECIFIED.,.F.,
 .F.,.F.)
B_SPLINE_SURFACE_WITH_KNOTS((4,4),(3,3),(-3.39528393502481E-6,3.73481232852722E-5),
(-0.0016501803332717,1.),.UNSPECIFIED.)
GEOMETRIC_REPRESENTATION_ITEM()
RATIONAL_B_SPLINE_SURFACE(((1.00048354385565,0.853487571660418,1.),(1.0004711051092,
0.857256476851432,1.),(1.00053193201107,0.838826096655909,1.),(1.00063970687725,
0.806170615310093,1.)))
REPRESENTATION_ITEM('')
SURFACE()
);
#2920=(
BOUNDED_SURFACE()
B_SPLINE_SURFACE(3,2,((#398057,#398058,#398059),(#398060,#398061,#398062),
(#398063,#398064,#398065),(#398066,#398067,#398068)),.UNSPECIFIED.,.F.,
 .F.,.F.)
B_SPLINE_SURFACE_WITH_KNOTS((4,4),(3,3),(2.0299386923051E-5,5.39756952687124E-5),
(-0.00011628106957775,1.),.UNSPECIFIED.)
GEOMETRIC_REPRESENTATION_ITEM()
RATIONAL_B_SPLINE_SURFACE(((1.00001770479725,0.923870681143034,1.),(1.00001014104056,
0.95639427554345,1.),(1.00002037300272,0.912397594905659,1.),(1.00003390859459,
0.854195550869787,1.)))
REPRESENTATION_ITEM('')
SURFACE()
);
#2921=(
BOUNDED_SURFACE()
B_SPLINE_SURFACE(3,2,((#398161,#398162,#398163),(#398164,#398165,#398166),
(#398167,#398168,#398169),(#398170,#398171,#398172)),.UNSPECIFIED.,.F.,
 .F.,.F.)
B_SPLINE_SURFACE_WITH_KNOTS((4,4),(3,3),(0.00135801595889393,0.00148409170619832),
(0.,1.),.UNSPECIFIED.)
GEOMETRIC_REPRESENTATION_ITEM()
RATIONAL_B_SPLINE_SURFACE(((1.,0.81830193396644,1.),(1.,0.817226613172329,
1.),(1.,0.816179643373962,1.),(1.,0.815159387863652,1.)))
REPRESENTATION_ITEM('')
SURFACE()
);
#2922=(
BOUNDED_SURFACE()
B_SPLINE_SURFACE(3,2,((#398211,#398212,#398213),(#398214,#398215,#398216),
(#398217,#398218,#398219),(#398220,#398221,#398222)),.UNSPECIFIED.,.F.,
 .F.,.F.)
B_SPLINE_SURFACE_WITH_KNOTS((4,4),(3,3),(-1.54744435122089E-6,1.5474443512209E-5),
(-0.0151698983635135,1.01516989835912),.UNSPECIFIED.)
GEOMETRIC_REPRESENTATION_ITEM()
RATIONAL_B_SPLINE_SURFACE(((1.02018382473144,0.32449821941329,1.02018382472551),
(1.00401234488862,0.865716921710548,1.00401234488744),(1.00033622856784,
0.988747276629661,1.00033622856774),(1.,1.,1.)))
REPRESENTATION_ITEM('')
SURFACE()
);
#2923=(
BOUNDED_SURFACE()
B_SPLINE_SURFACE(3,2,((#398224,#398225,#398226),(#398227,#398228,#398229),
(#398230,#398231,#398232),(#398233,#398234,#398235)),.UNSPECIFIED.,.F.,
 .F.,.F.)
B_SPLINE_SURFACE_WITH_KNOTS((4,4),(3,3),(0.00137194782501028,0.00149814269699235),
(0.,1.),.UNSPECIFIED.)
GEOMETRIC_REPRESENTATION_ITEM()
RATIONAL_B_SPLINE_SURFACE(((1.,0.815158509402317,1.),(1.,0.816179044148169,
1.),(1.,0.817226308119919,1.),(1.,0.818301939488809,1.)))
REPRESENTATION_ITEM('')
SURFACE()
);
#2924=(
BOUNDED_SURFACE()
B_SPLINE_SURFACE(3,2,((#398279,#398280,#398281),(#398282,#398283,#398284),
(#398285,#398286,#398287),(#398288,#398289,#398290)),.UNSPECIFIED.,.F.,
 .F.,.F.)
B_SPLINE_SURFACE_WITH_KNOTS((4,4),(3,3),(1.55009486301137E-5,4.92065510474432E-5),
(-8.1375951632858E-5,1.),.UNSPECIFIED.)
GEOMETRIC_REPRESENTATION_ITEM()
RATIONAL_B_SPLINE_SURFACE(((1.0000237291234,0.854200639599664,1.),(1.00001423585996,
0.912530301180503,1.),(1.00000710550472,0.956341495377435,1.),(1.00001238975911,
0.923873338137011,1.)))
REPRESENTATION_ITEM('')
SURFACE()
);
#2925=(
BOUNDED_SURFACE()
B_SPLINE_SURFACE(3,2,((#398294,#398295,#398296),(#398297,#398298,#398299),
(#398300,#398301,#398302),(#398303,#398304,#398305)),.UNSPECIFIED.,.F.,
 .F.,.F.)
B_SPLINE_SURFACE_WITH_KNOTS((4,4),(3,3),(-3.39934179457874E-6,3.73927597403563E-5),
(-0.00186004067438938,1.00069373317449),.UNSPECIFIED.)
GEOMETRIC_REPRESENTATION_ITEM()
RATIONAL_B_SPLINE_SURFACE(((1.00072100136062,0.806051963875284,1.00026859642694),
(1.0006004844016,0.83847080355859,1.00022369994499),(1.000531064488,0.857144632272337,
1.00019783877222),(1.00054515072858,0.853355459539054,1.0002030863544)))
REPRESENTATION_ITEM('')
SURFACE()
);
#2926=(
BOUNDED_SURFACE()
B_SPLINE_SURFACE(3,2,((#398307,#398308,#398309),(#398310,#398311,#398312),
(#398313,#398314,#398315),(#398316,#398317,#398318)),.UNSPECIFIED.,.F.,
 .F.,.F.)
B_SPLINE_SURFACE_WITH_KNOTS((4,4),(3,3),(-1.0842021724855E-19,9.54361881492171E-5),
(0.,1.),.UNSPECIFIED.)
GEOMETRIC_REPRESENTATION_ITEM()
RATIONAL_B_SPLINE_SURFACE(((1.,0.816715621142048,1.),(1.,0.815907587407952,
1.),(1.,0.815115959345191,1.),(1.,0.814339887349191,1.)))
REPRESENTATION_ITEM('')
SURFACE()
);
#2927=(
BOUNDED_SURFACE()
B_SPLINE_SURFACE(3,2,((#398320,#398321,#398322),(#398323,#398324,#398325),
(#398326,#398327,#398328),(#398329,#398330,#398331)),.UNSPECIFIED.,.F.,
 .F.,.F.)
B_SPLINE_SURFACE_WITH_KNOTS((4,4),(3,3),(3.64224167319349E-19,4.68197758448205E-5),
(0.,1.),.UNSPECIFIED.)
GEOMETRIC_REPRESENTATION_ITEM()
RATIONAL_B_SPLINE_SURFACE(((1.,0.816715621142056,1.),(1.,0.953638980025198,
1.),(1.,0.954506925408059,1.),(1.,0.816715621142056,1.)))
REPRESENTATION_ITEM('')
SURFACE()
);
#2928=(
BOUNDED_SURFACE()
B_SPLINE_SURFACE(3,2,((#398333,#398334,#398335),(#398336,#398337,#398338),
(#398339,#398340,#398341),(#398342,#398343,#398344)),.UNSPECIFIED.,.F.,
 .F.,.F.)
B_SPLINE_SURFACE_WITH_KNOTS((4,4),(3,3),(1.0842021724855E-19,9.54361881492179E-5),
(0.,1.),.UNSPECIFIED.)
GEOMETRIC_REPRESENTATION_ITEM()
RATIONAL_B_SPLINE_SURFACE(((1.,0.814339887349194,1.),(1.,0.815115959345204,
1.),(1.,0.815907587407948,1.),(1.,0.81671562114205,1.)))
REPRESENTATION_ITEM('')
SURFACE()
);
#2929=(
BOUNDED_SURFACE()
B_SPLINE_SURFACE(3,2,((#398346,#398347,#398348),(#398349,#398350,#398351),
(#398352,#398353,#398354),(#398355,#398356,#398357)),.UNSPECIFIED.,.F.,
 .F.,.F.)
B_SPLINE_SURFACE_WITH_KNOTS((4,4),(3,3),(-3.39528393502483E-6,3.73481232852738E-5),
(-0.00165018033340518,1.),.UNSPECIFIED.)
GEOMETRIC_REPRESENTATION_ITEM()
RATIONAL_B_SPLINE_SURFACE(((1.00048354385569,0.853487571660378,1.),(1.00047110510924,
0.857256476851447,1.),(1.00053193201111,0.83882609665586,1.),(1.0006397068773,
0.806170615310066,1.)))
REPRESENTATION_ITEM('')
SURFACE()
);
#2930=(
BOUNDED_SURFACE()
B_SPLINE_SURFACE(3,2,((#398361,#398362,#398363),(#398364,#398365,#398366),
(#398367,#398368,#398369),(#398370,#398371,#398372)),.UNSPECIFIED.,.F.,
 .F.,.F.)
B_SPLINE_SURFACE_WITH_KNOTS((4,4),(3,3),(2.02993869230509E-5,5.39756952687129E-5),
(-0.000116281069815165,1.),.UNSPECIFIED.)
GEOMETRIC_REPRESENTATION_ITEM()
RATIONAL_B_SPLINE_SURFACE(((1.00001770479728,0.923870681143013,1.),(1.00001014104058,
0.956394275543449,1.),(1.00002037300277,0.91239759490563,1.),(1.00003390859466,
0.85419555086975,1.)))
REPRESENTATION_ITEM('')
SURFACE()
);
#2931=(
BOUNDED_SURFACE()
B_SPLINE_SURFACE(3,2,((#398465,#398466,#398467),(#398468,#398469,#398470),
(#398471,#398472,#398473),(#398474,#398475,#398476)),.UNSPECIFIED.,.F.,
 .F.,.F.)
B_SPLINE_SURFACE_WITH_KNOTS((4,4),(3,3),(0.00135801595889393,0.00148409170619832),
(0.,1.),.UNSPECIFIED.)
GEOMETRIC_REPRESENTATION_ITEM()
RATIONAL_B_SPLINE_SURFACE(((1.,0.818301933966442,1.),(1.,0.817226613172341,
1.),(1.,0.81617964337395,1.),(1.,0.815159387863652,1.)))
REPRESENTATION_ITEM('')
SURFACE()
);
#2932=(
BOUNDED_SURFACE()
B_SPLINE_SURFACE(3,2,((#398515,#398516,#398517),(#398518,#398519,#398520),
(#398521,#398522,#398523),(#398524,#398525,#398526)),.UNSPECIFIED.,.F.,
 .F.,.F.)
B_SPLINE_SURFACE_WITH_KNOTS((4,4),(3,3),(-1.54744435122074E-6,1.54744435122072E-5),
(-0.015169898358919,1.01516989836333),.UNSPECIFIED.)
GEOMETRIC_REPRESENTATION_ITEM()
RATIONAL_B_SPLINE_SURFACE(((1.02018382472524,0.324498219413669,1.02018382473119),
(1.00401234488739,0.865716921710439,1.00401234488858),(1.00033622856773,
0.988747276629761,1.00033622856783),(1.,1.,1.)))
REPRESENTATION_ITEM('')
SURFACE()
);
#2933=(
BOUNDED_SURFACE()
B_SPLINE_SURFACE(3,2,((#398528,#398529,#398530),(#398531,#398532,#398533),
(#398534,#398535,#398536),(#398537,#398538,#398539)),.UNSPECIFIED.,.F.,
 .F.,.F.)
B_SPLINE_SURFACE_WITH_KNOTS((4,4),(3,3),(0.00137194782501028,0.00149814269699235),
(0.,1.),.UNSPECIFIED.)
GEOMETRIC_REPRESENTATION_ITEM()
RATIONAL_B_SPLINE_SURFACE(((1.,0.815158509402318,1.),(1.,0.816179044148164,
1.),(1.,0.817226308119921,1.),(1.,0.818301939488808,1.)))
REPRESENTATION_ITEM('')
SURFACE()
);
#2934=(
BOUNDED_SURFACE()
B_SPLINE_SURFACE(3,2,((#398583,#398584,#398585),(#398586,#398587,#398588),
(#398589,#398590,#398591),(#398592,#398593,#398594)),.UNSPECIFIED.,.F.,
 .F.,.F.)
B_SPLINE_SURFACE_WITH_KNOTS((4,4),(3,3),(1.55009486301137E-5,4.92065510474435E-5),
(-8.13759518653072E-5,1.),.UNSPECIFIED.)
GEOMETRIC_REPRESENTATION_ITEM()
RATIONAL_B_SPLINE_SURFACE(((1.00002372912347,0.854200639599629,1.),(1.00001423586,
0.912530301180511,1.),(1.00000710550474,0.956341495377406,1.),(1.00001238975914,
0.923873338136994,1.)))
REPRESENTATION_ITEM('')
SURFACE()
);
#2935=(
BOUNDED_SURFACE()
B_SPLINE_SURFACE(3,2,((#398598,#398599,#398600),(#398601,#398602,#398603),
(#398604,#398605,#398606),(#398607,#398608,#398609)),.UNSPECIFIED.,.F.,
 .F.,.F.)
B_SPLINE_SURFACE_WITH_KNOTS((4,4),(3,3),(-3.39934179457845E-6,3.73927597403565E-5),
(-0.00186004067405994,1.00069373317426),.UNSPECIFIED.)
GEOMETRIC_REPRESENTATION_ITEM()
RATIONAL_B_SPLINE_SURFACE(((1.0007210013605,0.806051963875394,1.00026859642686),
(1.0006004844015,0.83847080355868,1.00022369994491),(1.00053106448791,0.857144632272414,
1.00019783877215),(1.00054515072849,0.853355459539135,1.00020308635433)))
REPRESENTATION_ITEM('')
SURFACE()
);
#2936=(
BOUNDED_SURFACE()
B_SPLINE_SURFACE(3,2,((#398611,#398612,#398613),(#398614,#398615,#398616),
(#398617,#398618,#398619),(#398620,#398621,#398622)),.UNSPECIFIED.,.F.,
 .F.,.F.)
B_SPLINE_SURFACE_WITH_KNOTS((4,4),(3,3),(-5.42101086242752E-20,9.54361881492175E-5),
(0.,1.),.UNSPECIFIED.)
GEOMETRIC_REPRESENTATION_ITEM()
RATIONAL_B_SPLINE_SURFACE(((1.,0.816715621142049,1.),(1.,0.815907587407938,
1.),(1.,0.815115959345205,1.),(1.,0.81433988734919,1.)))
REPRESENTATION_ITEM('')
SURFACE()
);
#2937=(
BOUNDED_SURFACE()
B_SPLINE_SURFACE(3,2,((#398624,#398625,#398626),(#398627,#398628,#398629),
(#398630,#398631,#398632),(#398633,#398634,#398635)),.UNSPECIFIED.,.F.,
 .F.,.F.)
B_SPLINE_SURFACE_WITH_KNOTS((4,4),(3,3),(2.64274279543342E-19,4.68197758448213E-5),
(0.,1.),.UNSPECIFIED.)
GEOMETRIC_REPRESENTATION_ITEM()
RATIONAL_B_SPLINE_SURFACE(((1.,0.81671562114205,1.),(1.,0.953638980025202,
1.),(1.,0.95450692540806,1.),(1.,0.816715621142055,1.)))
REPRESENTATION_ITEM('')
SURFACE()
);
#2938=(
BOUNDED_SURFACE()
B_SPLINE_SURFACE(3,2,((#398637,#398638,#398639),(#398640,#398641,#398642),
(#398643,#398644,#398645),(#398646,#398647,#398648)),.UNSPECIFIED.,.F.,
 .F.,.F.)
B_SPLINE_SURFACE_WITH_KNOTS((4,4),(3,3),(-1.0842021724855E-19,9.54361881492178E-5),
(0.,1.),.UNSPECIFIED.)
GEOMETRIC_REPRESENTATION_ITEM()
RATIONAL_B_SPLINE_SURFACE(((1.,0.814339887349194,1.),(1.,0.815115959345202,
1.),(1.,0.815907587407945,1.),(1.,0.81671562114205,1.)))
REPRESENTATION_ITEM('')
SURFACE()
);
#2939=(
BOUNDED_SURFACE()
B_SPLINE_SURFACE(3,2,((#398650,#398651,#398652),(#398653,#398654,#398655),
(#398656,#398657,#398658),(#398659,#398660,#398661)),.UNSPECIFIED.,.F.,
 .F.,.F.)
B_SPLINE_SURFACE_WITH_KNOTS((4,4),(3,3),(-3.39528393502484E-6,3.73481232852732E-5),
(-0.00165018033312451,1.),.UNSPECIFIED.)
GEOMETRIC_REPRESENTATION_ITEM()
RATIONAL_B_SPLINE_SURFACE(((1.00048354385561,0.853487571660429,1.),(1.00047110510916,
0.857256476851488,1.),(1.00053193201102,0.838826096655901,1.),(1.00063970687719,
0.806170615310121,1.)))
REPRESENTATION_ITEM('')
SURFACE()
);
#2940=(
BOUNDED_SURFACE()
B_SPLINE_SURFACE(3,2,((#398665,#398666,#398667),(#398668,#398669,#398670),
(#398671,#398672,#398673),(#398674,#398675,#398676)),.UNSPECIFIED.,.F.,
 .F.,.F.)
B_SPLINE_SURFACE_WITH_KNOTS((4,4),(3,3),(2.02993869230509E-5,5.39756952687132E-5),
(-0.000116281069764964,1.),.UNSPECIFIED.)
GEOMETRIC_REPRESENTATION_ITEM()
RATIONAL_B_SPLINE_SURFACE(((1.00001770479727,0.923870681143023,1.),(1.00001014104058,
0.956394275543448,1.),(1.00002037300276,0.912397594905643,1.),(1.00003390859464,
0.854195550869757,1.)))
REPRESENTATION_ITEM('')
SURFACE()
);
#2941=(
BOUNDED_SURFACE()
B_SPLINE_SURFACE(3,2,((#398769,#398770,#398771),(#398772,#398773,#398774),
(#398775,#398776,#398777),(#398778,#398779,#398780)),.UNSPECIFIED.,.F.,
 .F.,.F.)
B_SPLINE_SURFACE_WITH_KNOTS((4,4),(3,3),(0.00135801595889393,0.00148409170619832),
(0.,1.),.UNSPECIFIED.)
GEOMETRIC_REPRESENTATION_ITEM()
RATIONAL_B_SPLINE_SURFACE(((1.,0.818301933966446,1.),(1.,0.817226613172346,
1.),(1.,0.816179643373953,1.),(1.,0.815159387863655,1.)))
REPRESENTATION_ITEM('')
SURFACE()
);
#2942=(
BOUNDED_SURFACE()
B_SPLINE_SURFACE(3,2,((#398819,#398820,#398821),(#398822,#398823,#398824),
(#398825,#398826,#398827),(#398828,#398829,#398830)),.UNSPECIFIED.,.F.,
 .F.,.F.)
B_SPLINE_SURFACE_WITH_KNOTS((4,4),(3,3),(-1.54744435122087E-6,1.54744435122095E-5),
(-0.0151698983679368,1.015169898355),.UNSPECIFIED.)
GEOMETRIC_REPRESENTATION_ITEM()
RATIONAL_B_SPLINE_SURFACE(((1.02018382473742,0.324498219413098,1.02018382471995),
(1.00401234488981,0.865716921710379,1.00401234488634),(1.00033622856794,
0.988747276629715,1.00033622856764),(1.,1.,1.)))
REPRESENTATION_ITEM('')
SURFACE()
);
#2943=(
BOUNDED_SURFACE()
B_SPLINE_SURFACE(3,2,((#398832,#398833,#398834),(#398835,#398836,#398837),
(#398838,#398839,#398840),(#398841,#398842,#398843)),.UNSPECIFIED.,.F.,
 .F.,.F.)
B_SPLINE_SURFACE_WITH_KNOTS((4,4),(3,3),(0.00137194782501028,0.00149814269699235),
(0.,1.),.UNSPECIFIED.)
GEOMETRIC_REPRESENTATION_ITEM()
RATIONAL_B_SPLINE_SURFACE(((1.,0.815158509402317,1.),(1.,0.81617904414817,
1.),(1.,0.817226308119926,1.),(1.,0.818301939488808,1.)))
REPRESENTATION_ITEM('')
SURFACE()
);
#2944=(
BOUNDED_SURFACE()
B_SPLINE_SURFACE(3,2,((#398887,#398888,#398889),(#398890,#398891,#398892),
(#398893,#398894,#398895),(#398896,#398897,#398898)),.UNSPECIFIED.,.F.,
 .F.,.F.)
B_SPLINE_SURFACE_WITH_KNOTS((4,4),(3,3),(1.55009486301137E-5,4.92065510474438E-5),
(-8.13759514719951E-5,1.),.UNSPECIFIED.)
GEOMETRIC_REPRESENTATION_ITEM()
RATIONAL_B_SPLINE_SURFACE(((1.00002372912335,0.854200639599683,1.),(1.00001423585993,
0.912530301180541,1.),(1.00000710550471,0.956341495377434,1.),(1.00001238975908,
0.923873338137023,1.)))
REPRESENTATION_ITEM('')
SURFACE()
);
#2945=(
BOUNDED_SURFACE()
B_SPLINE_SURFACE(3,2,((#398902,#398903,#398904),(#398905,#398906,#398907),
(#398908,#398909,#398910),(#398911,#398912,#398913)),.UNSPECIFIED.,.F.,
 .F.,.F.)
B_SPLINE_SURFACE_WITH_KNOTS((4,4),(3,3),(-3.39934179457794E-6,3.73927597403563E-5),
(-0.00186004067477698,1.00069373317471),.UNSPECIFIED.)
GEOMETRIC_REPRESENTATION_ITEM()
RATIONAL_B_SPLINE_SURFACE(((1.00072100136078,0.80605196387518,1.00026859642703),
(1.00060048440173,0.838470803558503,1.00022369994506),(1.00053106448812,
0.857144632272239,1.00019783877228),(1.0005451507287,0.853355459538978,
1.00020308635446)))
REPRESENTATION_ITEM('')
SURFACE()
);
#2946=(
BOUNDED_SURFACE()
B_SPLINE_SURFACE(3,2,((#398915,#398916,#398917),(#398918,#398919,#398920),
(#398921,#398922,#398923),(#398924,#398925,#398926)),.UNSPECIFIED.,.F.,
 .F.,.F.)
B_SPLINE_SURFACE_WITH_KNOTS((4,4),(3,3),(-1.0842021724855E-19,9.54361881492173E-5),
(0.,1.),.UNSPECIFIED.)
GEOMETRIC_REPRESENTATION_ITEM()
RATIONAL_B_SPLINE_SURFACE(((1.,0.816715621142054,1.),(1.,0.815907587407935,
1.),(1.,0.815115959345215,1.),(1.,0.814339887349195,1.)))
REPRESENTATION_ITEM('')
SURFACE()
);
#2947=(
BOUNDED_SURFACE()
B_SPLINE_SURFACE(3,2,((#398928,#398929,#398930),(#398931,#398932,#398933),
(#398934,#398935,#398936),(#398937,#398938,#398939)),.UNSPECIFIED.,.F.,
 .F.,.F.)
B_SPLINE_SURFACE_WITH_KNOTS((4,4),(3,3),(-1.8126505071242E-19,4.68197758448207E-5),
(0.,1.),.UNSPECIFIED.)
GEOMETRIC_REPRESENTATION_ITEM()
RATIONAL_B_SPLINE_SURFACE(((1.,0.816715621142049,1.),(1.,0.953638980025206,
1.),(1.,0.954506925408054,1.),(1.,0.816715621142056,1.)))
REPRESENTATION_ITEM('')
SURFACE()
);
#2948=(
BOUNDED_SURFACE()
B_SPLINE_SURFACE(3,2,((#398941,#398942,#398943),(#398944,#398945,#398946),
(#398947,#398948,#398949),(#398950,#398951,#398952)),.UNSPECIFIED.,.F.,
 .F.,.F.)
B_SPLINE_SURFACE_WITH_KNOTS((4,4),(3,3),(2.16840434497101E-19,9.54361881492176E-5),
(0.,1.),.UNSPECIFIED.)
GEOMETRIC_REPRESENTATION_ITEM()
RATIONAL_B_SPLINE_SURFACE(((1.,0.814339887349194,1.),(1.,0.815115959345205,
1.),(1.,0.815907587407941,1.),(1.,0.816715621142049,1.)))
REPRESENTATION_ITEM('')
SURFACE()
);
#2949=(
BOUNDED_SURFACE()
B_SPLINE_SURFACE(3,2,((#398954,#398955,#398956),(#398957,#398958,#398959),
(#398960,#398961,#398962),(#398963,#398964,#398965)),.UNSPECIFIED.,.F.,
 .F.,.F.)
B_SPLINE_SURFACE_WITH_KNOTS((4,4),(3,3),(-3.39528393502485E-6,3.7348123285274E-5),
(-0.00165018033347468,1.),.UNSPECIFIED.)
GEOMETRIC_REPRESENTATION_ITEM()
RATIONAL_B_SPLINE_SURFACE(((1.00048354385571,0.853487571660368,1.),(1.00047110510926,
0.857256476851433,1.),(1.00053193201114,0.838826096655843,1.),(1.00063970687733,
0.80617061531005,0.999999999999999)))
REPRESENTATION_ITEM('')
SURFACE()
);
#2950=(
BOUNDED_SURFACE()
B_SPLINE_SURFACE(3,2,((#398969,#398970,#398971),(#398972,#398973,#398974),
(#398975,#398976,#398977),(#398978,#398979,#398980)),.UNSPECIFIED.,.F.,
 .F.,.F.)
B_SPLINE_SURFACE_WITH_KNOTS((4,4),(3,3),(2.02993869230511E-5,5.39756952687125E-5),
(-0.000116281069576731,1.),.UNSPECIFIED.)
GEOMETRIC_REPRESENTATION_ITEM()
RATIONAL_B_SPLINE_SURFACE(((1.00001770479725,0.923870681143036,1.),(1.00001014104056,
0.956394275543457,1.),(1.00002037300272,0.912397594905648,1.),(1.00003390859459,
0.854195550869787,1.)))
REPRESENTATION_ITEM('')
SURFACE()
);
#2951=(
BOUNDED_SURFACE()
B_SPLINE_SURFACE(3,2,((#399073,#399074,#399075),(#399076,#399077,#399078),
(#399079,#399080,#399081),(#399082,#399083,#399084)),.UNSPECIFIED.,.F.,
 .F.,.F.)
B_SPLINE_SURFACE_WITH_KNOTS((4,4),(3,3),(0.00135801595889393,0.00148409170619832),
(0.,1.),.UNSPECIFIED.)
GEOMETRIC_REPRESENTATION_ITEM()
RATIONAL_B_SPLINE_SURFACE(((1.,0.818301933966439,1.),(1.,0.817226613172357,
1.),(1.,0.816179643373936,1.),(1.,0.815159387863655,1.)))
REPRESENTATION_ITEM('')
SURFACE()
);
#2952=(
BOUNDED_SURFACE()
B_SPLINE_SURFACE(3,2,((#399123,#399124,#399125),(#399126,#399127,#399128),
(#399129,#399130,#399131),(#399132,#399133,#399134)),.UNSPECIFIED.,.F.,
 .F.,.F.)
B_SPLINE_SURFACE_WITH_KNOTS((4,4),(3,3),(-1.54744435122104E-6,1.54744435122105E-5),
(-0.015169898368822,1.01516989835412),.UNSPECIFIED.)
GEOMETRIC_REPRESENTATION_ITEM()
RATIONAL_B_SPLINE_SURFACE(((1.02018382473861,0.324498219413095,1.02018382471876),
(1.00401234489005,0.865716921710323,1.00401234488611),(1.00033622856795,
0.98874727662973,1.00033622856762),(1.,1.,1.)))
REPRESENTATION_ITEM('')
SURFACE()
);
#2953=(
BOUNDED_SURFACE()
B_SPLINE_SURFACE(3,2,((#399136,#399137,#399138),(#399139,#399140,#399141),
(#399142,#399143,#399144),(#399145,#399146,#399147)),.UNSPECIFIED.,.F.,
 .F.,.F.)
B_SPLINE_SURFACE_WITH_KNOTS((4,4),(3,3),(0.00137194782501028,0.00149814269699235),
(0.,1.),.UNSPECIFIED.)
GEOMETRIC_REPRESENTATION_ITEM()
RATIONAL_B_SPLINE_SURFACE(((1.,0.815158509402313,1.),(1.,0.816179044148173,
1.),(1.,0.817226308119917,1.),(1.,0.818301939488807,1.)))
REPRESENTATION_ITEM('')
SURFACE()
);
#2954=(
BOUNDED_SURFACE()
B_SPLINE_SURFACE(3,2,((#399191,#399192,#399193),(#399194,#399195,#399196),
(#399197,#399198,#399199),(#399200,#399201,#399202)),.UNSPECIFIED.,.F.,
 .F.,.F.)
B_SPLINE_SURFACE_WITH_KNOTS((4,4),(3,3),(1.55009486301138E-5,4.92065510474443E-5),
(-8.13759510935406E-5,1.),.UNSPECIFIED.)
GEOMETRIC_REPRESENTATION_ITEM()
RATIONAL_B_SPLINE_SURFACE(((1.00002372912324,0.854200639599743,1.),(1.00001423585987,
0.912530301180569,1.),(1.00000710550467,0.956341495377446,1.),(1.00001238975903,
0.923873338137053,1.)))
REPRESENTATION_ITEM('')
SURFACE()
);
#2955=(
BOUNDED_SURFACE()
B_SPLINE_SURFACE(3,2,((#399206,#399207,#399208),(#399209,#399210,#399211),
(#399212,#399213,#399214),(#399215,#399216,#399217)),.UNSPECIFIED.,.F.,
 .F.,.F.)
B_SPLINE_SURFACE_WITH_KNOTS((4,4),(3,3),(-3.39934179457821E-6,3.73927597403565E-5),
(-0.00186004067401852,1.00069373317405),.UNSPECIFIED.)
GEOMETRIC_REPRESENTATION_ITEM()
RATIONAL_B_SPLINE_SURFACE(((1.00072100136048,0.80605196387546,1.00026859642678),
(1.00060048440149,0.838470803558704,1.00022369994485),(1.0005310644879,
0.85714463227246,1.0001978387721),(1.00054515072847,0.853355459539171,1.00020308635427)))
REPRESENTATION_ITEM('')
SURFACE()
);
#2956=(
BOUNDED_SURFACE()
B_SPLINE_SURFACE(3,2,((#399219,#399220,#399221),(#399222,#399223,#399224),
(#399225,#399226,#399227),(#399228,#399229,#399230)),.UNSPECIFIED.,.F.,
 .F.,.F.)
B_SPLINE_SURFACE_WITH_KNOTS((4,4),(3,3),(-1.62630325872826E-19,9.54361881492172E-5),
(0.,1.),.UNSPECIFIED.)
GEOMETRIC_REPRESENTATION_ITEM()
RATIONAL_B_SPLINE_SURFACE(((1.,0.816715621142047,1.),(1.,0.815907587407934,
1.),(1.,0.815115959345204,1.),(1.,0.814339887349192,1.)))
REPRESENTATION_ITEM('')
SURFACE()
);
#2957=(
BOUNDED_SURFACE()
B_SPLINE_SURFACE(3,2,((#399232,#399233,#399234),(#399235,#399236,#399237),
(#399238,#399239,#399240),(#399241,#399242,#399243)),.UNSPECIFIED.,.F.,
 .F.,.F.)
B_SPLINE_SURFACE_WITH_KNOTS((4,4),(3,3),(-1.89735380184963E-19,4.68197758448202E-5),
(0.,1.),.UNSPECIFIED.)
GEOMETRIC_REPRESENTATION_ITEM()
RATIONAL_B_SPLINE_SURFACE(((1.,0.816715621142049,1.),(1.,0.953638980025202,
1.),(1.,0.954506925408058,1.),(1.,0.816715621142054,1.)))
REPRESENTATION_ITEM('')
SURFACE()
);
#2958=(
BOUNDED_SURFACE()
B_SPLINE_SURFACE(3,2,((#399245,#399246,#399247),(#399248,#399249,#399250),
(#399251,#399252,#399253),(#399254,#399255,#399256)),.UNSPECIFIED.,.F.,
 .F.,.F.)
B_SPLINE_SURFACE_WITH_KNOTS((4,4),(3,3),(-5.42101086242752E-20,9.54361881492178E-5),
(0.,1.),.UNSPECIFIED.)
GEOMETRIC_REPRESENTATION_ITEM()
RATIONAL_B_SPLINE_SURFACE(((1.,0.81433988734919,1.),(1.,0.815115959345203,
1.),(1.,0.815907587407937,1.),(1.,0.816715621142049,1.)))
REPRESENTATION_ITEM('')
SURFACE()
);
#2959=(
BOUNDED_SURFACE()
B_SPLINE_SURFACE(3,2,((#399258,#399259,#399260),(#399261,#399262,#399263),
(#399264,#399265,#399266),(#399267,#399268,#399269)),.UNSPECIFIED.,.F.,
 .F.,.F.)
B_SPLINE_SURFACE_WITH_KNOTS((4,4),(3,3),(-3.39528393502489E-6,3.73481232852725E-5),
(-0.00165018033329913,1.),.UNSPECIFIED.)
GEOMETRIC_REPRESENTATION_ITEM()
RATIONAL_B_SPLINE_SURFACE(((1.00048354385566,0.853487571660391,1.),(1.00047110510921,
0.857256476851463,1.),(1.00053193201108,0.838826096655849,1.),(1.00063970687726,
0.80617061531011,0.999999999999999)))
REPRESENTATION_ITEM('')
SURFACE()
);
#2960=(
BOUNDED_SURFACE()
B_SPLINE_SURFACE(3,2,((#399273,#399274,#399275),(#399276,#399277,#399278),
(#399279,#399280,#399281),(#399282,#399283,#399284)),.UNSPECIFIED.,.F.,
 .F.,.F.)
B_SPLINE_SURFACE_WITH_KNOTS((4,4),(3,3),(2.02993869230512E-5,5.39756952687125E-5),
(-0.000116281069426136,1.),.UNSPECIFIED.)
GEOMETRIC_REPRESENTATION_ITEM()
RATIONAL_B_SPLINE_SURFACE(((1.00001770479722,0.92387068114305,1.),(1.00001014104055,
0.956394275543467,1.),(1.0000203730027,0.912397594905656,1.),(1.00003390859454,
0.854195550869809,1.)))
REPRESENTATION_ITEM('')
SURFACE()
);
#2961=(
BOUNDED_SURFACE()
B_SPLINE_SURFACE(3,2,((#399377,#399378,#399379),(#399380,#399381,#399382),
(#399383,#399384,#399385),(#399386,#399387,#399388)),.UNSPECIFIED.,.F.,
 .F.,.F.)
B_SPLINE_SURFACE_WITH_KNOTS((4,4),(3,3),(0.00135801595889393,0.00148409170619832),
(0.,1.),.UNSPECIFIED.)
GEOMETRIC_REPRESENTATION_ITEM()
RATIONAL_B_SPLINE_SURFACE(((1.,0.818301933966445,1.),(1.,0.817226613172349,
1.),(1.,0.816179643373958,1.),(1.,0.815159387863658,1.)))
REPRESENTATION_ITEM('')
SURFACE()
);
#2962=(
BOUNDED_SURFACE()
B_SPLINE_SURFACE(3,2,((#399427,#399428,#399429),(#399430,#399431,#399432),
(#399433,#399434,#399435),(#399436,#399437,#399438)),.UNSPECIFIED.,.F.,
 .F.,.F.)
B_SPLINE_SURFACE_WITH_KNOTS((4,4),(3,3),(3.91752738105114E-20,1.54744435122074E-5),
(0.,1.),.UNSPECIFIED.)
GEOMETRIC_REPRESENTATION_ITEM()
RATIONAL_B_SPLINE_SURFACE(((1.,0.478041569704954,1.),(1.,0.890533857552083,
1.),(1.,0.990075913815909,1.),(1.,1.,1.)))
REPRESENTATION_ITEM('')
SURFACE()
);
#2963=(
BOUNDED_SURFACE()
B_SPLINE_SURFACE(3,2,((#399440,#399441,#399442),(#399443,#399444,#399445),
(#399446,#399447,#399448),(#399449,#399450,#399451)),.UNSPECIFIED.,.F.,
 .F.,.F.)
B_SPLINE_SURFACE_WITH_KNOTS((4,4),(3,3),(0.00137194782501028,0.00149814269699235),
(0.,1.),.UNSPECIFIED.)
GEOMETRIC_REPRESENTATION_ITEM()
RATIONAL_B_SPLINE_SURFACE(((1.,0.815158509402317,1.),(1.,0.816179044148163,
1.),(1.,0.817226308119927,1.),(1.,0.818301939488798,1.)))
REPRESENTATION_ITEM('')
SURFACE()
);
#2964=(
BOUNDED_SURFACE()
B_SPLINE_SURFACE(3,2,((#399495,#399496,#399497),(#399498,#399499,#399500),
(#399501,#399502,#399503),(#399504,#399505,#399506)),.UNSPECIFIED.,.F.,
 .F.,.F.)
B_SPLINE_SURFACE_WITH_KNOTS((4,4),(3,3),(1.55009486301137E-5,4.92065510474427E-5),
(-8.13759517743486E-5,1.),.UNSPECIFIED.)
GEOMETRIC_REPRESENTATION_ITEM()
RATIONAL_B_SPLINE_SURFACE(((1.00002372912344,0.854200639599642,1.),(1.00001423585999,
0.912530301180501,1.),(1.00000710550473,0.95634149537743,1.),(1.00001238975913,
0.923873338136998,1.)))
REPRESENTATION_ITEM('')
SURFACE()
);
#2965=(
BOUNDED_SURFACE()
B_SPLINE_SURFACE(3,2,((#399510,#399511,#399512),(#399513,#399514,#399515),
(#399516,#399517,#399518),(#399519,#399520,#399521)),.UNSPECIFIED.,.F.,
 .F.,.F.)
B_SPLINE_SURFACE_WITH_KNOTS((4,4),(3,3),(-3.39934179457844E-6,3.73927597403567E-5),
(-0.00186004067380532,1.00069373317436),.UNSPECIFIED.)
GEOMETRIC_REPRESENTATION_ITEM()
RATIONAL_B_SPLINE_SURFACE(((1.0007210013604,0.806051963875427,1.00026859642689),
(1.00060048440142,0.838470803558702,1.00022369994494),(1.00053106448784,
0.857144632272448,1.00019783877218),(1.00054515072841,0.853355459539161,
1.00020308635436)))
REPRESENTATION_ITEM('')
SURFACE()
);
#2966=(
BOUNDED_SURFACE()
B_SPLINE_SURFACE(3,2,((#399523,#399524,#399525),(#399526,#399527,#399528),
(#399529,#399530,#399531),(#399532,#399533,#399534)),.UNSPECIFIED.,.F.,
 .F.,.F.)
B_SPLINE_SURFACE_WITH_KNOTS((4,4),(3,3),(-5.42101086242752E-20,9.54361881492172E-5),
(0.,1.),.UNSPECIFIED.)
GEOMETRIC_REPRESENTATION_ITEM()
RATIONAL_B_SPLINE_SURFACE(((1.,0.816715621142047,1.),(1.,0.815907587407954,
1.),(1.,0.815115959345199,1.),(1.,0.814339887349199,1.)))
REPRESENTATION_ITEM('')
SURFACE()
);
#2967=(
BOUNDED_SURFACE()
B_SPLINE_SURFACE(3,2,((#399536,#399537,#399538),(#399539,#399540,#399541),
(#399542,#399543,#399544),(#399545,#399546,#399547)),.UNSPECIFIED.,.F.,
 .F.,.F.)
B_SPLINE_SURFACE_WITH_KNOTS((4,4),(3,3),(-4.60785923306339E-19,4.68197758448207E-5),
(0.,1.),.UNSPECIFIED.)
GEOMETRIC_REPRESENTATION_ITEM()
RATIONAL_B_SPLINE_SURFACE(((1.,0.816715621142045,1.),(1.,0.953638980025201,
1.),(1.,0.954506925408062,1.),(1.,0.816715621142047,1.)))
REPRESENTATION_ITEM('')
SURFACE()
);
#2968=(
BOUNDED_SURFACE()
B_SPLINE_SURFACE(3,2,((#399549,#399550,#399551),(#399552,#399553,#399554),
(#399555,#399556,#399557),(#399558,#399559,#399560)),.UNSPECIFIED.,.F.,
 .F.,.F.)
B_SPLINE_SURFACE_WITH_KNOTS((4,4),(3,3),(-1.0842021724855E-19,9.54361881492174E-5),
(0.,1.),.UNSPECIFIED.)
GEOMETRIC_REPRESENTATION_ITEM()
RATIONAL_B_SPLINE_SURFACE(((1.,0.814339887349193,1.),(1.,0.815115959345205,
1.),(1.,0.815907587407938,1.),(1.,0.816715621142051,1.)))
REPRESENTATION_ITEM('')
SURFACE()
);
#2969=(
BOUNDED_SURFACE()
B_SPLINE_SURFACE(3,2,((#399562,#399563,#399564),(#399565,#399566,#399567),
(#399568,#399569,#399570),(#399571,#399572,#399573)),.UNSPECIFIED.,.F.,
 .F.,.F.)
B_SPLINE_SURFACE_WITH_KNOTS((4,4),(3,3),(-3.39528393502485E-6,3.73481232852737E-5),
(-0.00165018033257718,1.),.UNSPECIFIED.)
GEOMETRIC_REPRESENTATION_ITEM()
RATIONAL_B_SPLINE_SURFACE(((1.00048354385545,0.853487571660499,1.),(1.000471105109,
0.85725647685156,1.),(1.00053193201085,0.838826096655988,1.),(1.00063970687698,
0.806170615310227,1.)))
REPRESENTATION_ITEM('')
SURFACE()
);
#2970=(
BOUNDED_SURFACE()
B_SPLINE_SURFACE(3,2,((#399577,#399578,#399579),(#399580,#399581,#399582),
(#399583,#399584,#399585),(#399586,#399587,#399588)),.UNSPECIFIED.,.F.,
 .F.,.F.)
B_SPLINE_SURFACE_WITH_KNOTS((4,4),(3,3),(2.0299386923051E-5,5.39756952687121E-5),
(-0.000116281070730535,1.),.UNSPECIFIED.)
GEOMETRIC_REPRESENTATION_ITEM()
RATIONAL_B_SPLINE_SURFACE(((1.00001770479742,0.923870681142948,1.),(1.00001014104066,
0.9563942755434,1.),(1.00002037300293,0.912397594905555,1.),(1.00003390859492,
0.854195550869617,1.)))
REPRESENTATION_ITEM('')
SURFACE()
);
#2971=(
BOUNDED_SURFACE()
B_SPLINE_SURFACE(3,2,((#399681,#399682,#399683),(#399684,#399685,#399686),
(#399687,#399688,#399689),(#399690,#399691,#399692)),.UNSPECIFIED.,.F.,
 .F.,.F.)
B_SPLINE_SURFACE_WITH_KNOTS((4,4),(3,3),(0.00135801595889393,0.00148409170619832),
(0.,1.),.UNSPECIFIED.)
GEOMETRIC_REPRESENTATION_ITEM()
RATIONAL_B_SPLINE_SURFACE(((1.,0.818301933966444,1.),(1.,0.817226613172335,
1.),(1.,0.816179643373969,1.),(1.,0.815159387863651,1.)))
REPRESENTATION_ITEM('')
SURFACE()
);
#2972=(
BOUNDED_SURFACE()
B_SPLINE_SURFACE(3,2,((#399731,#399732,#399733),(#399734,#399735,#399736),
(#399737,#399738,#399739),(#399740,#399741,#399742)),.UNSPECIFIED.,.F.,
 .F.,.F.)
B_SPLINE_SURFACE_WITH_KNOTS((4,4),(3,3),(-1.54744435122074E-6,1.54744435122078E-5),
(-0.0151698983613399,1.01516989836114),.UNSPECIFIED.)
GEOMETRIC_REPRESENTATION_ITEM()
RATIONAL_B_SPLINE_SURFACE(((1.02018382472851,0.324498219413358,1.02018382472825),
(1.00401234488804,0.865716921710615,1.00401234488799),(1.00033622856779,
0.988747276629691,1.00033622856778),(1.,1.,1.)))
REPRESENTATION_ITEM('')
SURFACE()
);
#2973=(
BOUNDED_SURFACE()
B_SPLINE_SURFACE(3,2,((#399744,#399745,#399746),(#399747,#399748,#399749),
(#399750,#399751,#399752),(#399753,#399754,#399755)),.UNSPECIFIED.,.F.,
 .F.,.F.)
B_SPLINE_SURFACE_WITH_KNOTS((4,4),(3,3),(0.00137194782501028,0.00149814269699235),
(0.,1.),.UNSPECIFIED.)
GEOMETRIC_REPRESENTATION_ITEM()
RATIONAL_B_SPLINE_SURFACE(((1.,0.815158509402308,1.),(1.,0.816179044148165,
1.),(1.,0.817226308119931,1.),(1.,0.818301939488802,1.)))
REPRESENTATION_ITEM('')
SURFACE()
);
#2974=(
BOUNDED_SURFACE()
B_SPLINE_SURFACE(3,2,((#399799,#399800,#399801),(#399802,#399803,#399804),
(#399805,#399806,#399807),(#399808,#399809,#399810)),.UNSPECIFIED.,.F.,
 .F.,.F.)
B_SPLINE_SURFACE_WITH_KNOTS((4,4),(3,3),(1.55009486301137E-5,4.92065510474429E-5),
(-8.13759509738754E-5,1.),.UNSPECIFIED.)
GEOMETRIC_REPRESENTATION_ITEM()
RATIONAL_B_SPLINE_SURFACE(((1.00002372912321,0.854200639599766,1.),(1.00001423585985,
0.912530301180572,1.),(1.00000710550466,0.956341495377455,1.),(1.00001238975901,
0.923873338137061,1.)))
REPRESENTATION_ITEM('')
SURFACE()
);
#2975=(
BOUNDED_SURFACE()
B_SPLINE_SURFACE(3,2,((#399814,#399815,#399816),(#399817,#399818,#399819),
(#399820,#399821,#399822),(#399823,#399824,#399825)),.UNSPECIFIED.,.F.,
 .F.,.F.)
B_SPLINE_SURFACE_WITH_KNOTS((4,4),(3,3),(-3.39934179457793E-6,3.73927597403565E-5),
(-0.0018600406739492,1.00069373317436),.UNSPECIFIED.)
GEOMETRIC_REPRESENTATION_ITEM()
RATIONAL_B_SPLINE_SURFACE(((1.00072100136045,0.806051963875388,1.0002685964269),
(1.00060048440146,0.8384708035587,1.00022369994495),(1.00053106448788,0.857144632272405,
1.00019783877218),(1.00054515072845,0.853355459539143,1.00020308635436)))
REPRESENTATION_ITEM('')
SURFACE()
);
#2976=(
BOUNDED_SURFACE()
B_SPLINE_SURFACE(3,2,((#399827,#399828,#399829),(#399830,#399831,#399832),
(#399833,#399834,#399835),(#399836,#399837,#399838)),.UNSPECIFIED.,.F.,
 .F.,.F.)
B_SPLINE_SURFACE_WITH_KNOTS((4,4),(3,3),(1.0842021724855E-19,9.54361881492174E-5),
(0.,1.),.UNSPECIFIED.)
GEOMETRIC_REPRESENTATION_ITEM()
RATIONAL_B_SPLINE_SURFACE(((1.,0.816715621142051,1.),(1.,0.815907587407938,
1.),(1.,0.815115959345202,1.),(1.,0.814339887349196,1.)))
REPRESENTATION_ITEM('')
SURFACE()
);
#2977=(
BOUNDED_SURFACE()
B_SPLINE_SURFACE(3,2,((#399840,#399841,#399842),(#399843,#399844,#399845),
(#399846,#399847,#399848),(#399849,#399850,#399851)),.UNSPECIFIED.,.F.,
 .F.,.F.)
B_SPLINE_SURFACE_WITH_KNOTS((4,4),(3,3),(1.47383732822248E-19,4.68197758448205E-5),
(0.,1.),.UNSPECIFIED.)
GEOMETRIC_REPRESENTATION_ITEM()
RATIONAL_B_SPLINE_SURFACE(((1.,0.81671562114205,1.),(1.,0.953638980025207,
1.),(1.,0.95450692540805,1.),(1.,0.816715621142057,1.)))
REPRESENTATION_ITEM('')
SURFACE()
);
#2978=(
BOUNDED_SURFACE()
B_SPLINE_SURFACE(3,2,((#399853,#399854,#399855),(#399856,#399857,#399858),
(#399859,#399860,#399861),(#399862,#399863,#399864)),.UNSPECIFIED.,.F.,
 .F.,.F.)
B_SPLINE_SURFACE_WITH_KNOTS((4,4),(3,3),(1.0842021724855E-19,9.54361881492178E-5),
(0.,1.),.UNSPECIFIED.)
GEOMETRIC_REPRESENTATION_ITEM()
RATIONAL_B_SPLINE_SURFACE(((1.,0.814339887349195,1.),(1.,0.815115959345184,
1.),(1.,0.815907587407959,1.),(1.,0.81671562114205,1.)))
REPRESENTATION_ITEM('')
SURFACE()
);
#2979=(
BOUNDED_SURFACE()
B_SPLINE_SURFACE(3,2,((#399866,#399867,#399868),(#399869,#399870,#399871),
(#399872,#399873,#399874),(#399875,#399876,#399877)),.UNSPECIFIED.,.F.,
 .F.,.F.)
B_SPLINE_SURFACE_WITH_KNOTS((4,4),(3,3),(-3.3952839350249E-6,3.73481232852728E-5),
(-0.00165018033329724,1.),.UNSPECIFIED.)
GEOMETRIC_REPRESENTATION_ITEM()
RATIONAL_B_SPLINE_SURFACE(((1.00048354385566,0.853487571660387,1.),(1.00047110510921,
0.857256476851467,1.),(1.00053193201108,0.838826096655857,1.),(1.00063970687726,
0.806170615310098,1.)))
REPRESENTATION_ITEM('')
SURFACE()
);
#2980=(
BOUNDED_SURFACE()
B_SPLINE_SURFACE(3,2,((#399881,#399882,#399883),(#399884,#399885,#399886),
(#399887,#399888,#399889),(#399890,#399891,#399892)),.UNSPECIFIED.,.F.,
 .F.,.F.)
B_SPLINE_SURFACE_WITH_KNOTS((4,4),(3,3),(2.02993869230513E-5,5.39756952686905E-5),
(-0.000116281069768348,1.),.UNSPECIFIED.)
GEOMETRIC_REPRESENTATION_ITEM()
RATIONAL_B_SPLINE_SURFACE(((1.00001770479727,0.923870681143019,1.),(1.00001014104058,
0.956394275543429,1.),(1.00002037300276,0.912397594905682,1.),(1.00003390859464,
0.854195550869875,1.)))
REPRESENTATION_ITEM('')
SURFACE()
);
#2981=(
BOUNDED_SURFACE()
B_SPLINE_SURFACE(3,2,((#399985,#399986,#399987),(#399988,#399989,#399990),
(#399991,#399992,#399993),(#399994,#399995,#399996)),.UNSPECIFIED.,.F.,
 .F.,.F.)
B_SPLINE_SURFACE_WITH_KNOTS((4,4),(3,3),(0.00135801595889393,0.00148409170619832),
(0.,1.),.UNSPECIFIED.)
GEOMETRIC_REPRESENTATION_ITEM()
RATIONAL_B_SPLINE_SURFACE(((1.,0.818301933966446,1.),(1.,0.817226613172338,
1.),(1.,0.816179643373962,1.),(1.,0.815159387863655,1.)))
REPRESENTATION_ITEM('')
SURFACE()
);
#2982=(
BOUNDED_SURFACE()
B_SPLINE_SURFACE(3,2,((#400035,#400036,#400037),(#400038,#400039,#400040),
(#400041,#400042,#400043),(#400044,#400045,#400046)),.UNSPECIFIED.,.F.,
 .F.,.F.)
B_SPLINE_SURFACE_WITH_KNOTS((4,4),(3,3),(-1.54744435122077E-6,1.54744435122077E-5),
(-0.0151698983622635,1.0151698983599),.UNSPECIFIED.)
GEOMETRIC_REPRESENTATION_ITEM()
RATIONAL_B_SPLINE_SURFACE(((1.02018382472975,0.324498219413619,1.02018382472657),
(1.00401234488829,0.865716921710638,1.00401234488765),(1.00033622856781,
0.988747276629694,1.00033622856776),(1.,1.,1.)))
REPRESENTATION_ITEM('')
SURFACE()
);
#2983=(
BOUNDED_SURFACE()
B_SPLINE_SURFACE(3,2,((#400048,#400049,#400050),(#400051,#400052,#400053),
(#400054,#400055,#400056),(#400057,#400058,#400059)),.UNSPECIFIED.,.F.,
 .F.,.F.)
B_SPLINE_SURFACE_WITH_KNOTS((4,4),(3,3),(0.00137194782501028,0.00149814269699235),
(0.,1.),.UNSPECIFIED.)
GEOMETRIC_REPRESENTATION_ITEM()
RATIONAL_B_SPLINE_SURFACE(((1.,0.815158509402316,1.),(1.,0.816179044148169,
1.),(1.,0.817226308119926,1.),(1.,0.8183019394888,1.)))
REPRESENTATION_ITEM('')
SURFACE()
);
#2984=(
BOUNDED_SURFACE()
B_SPLINE_SURFACE(3,2,((#400103,#400104,#400105),(#400106,#400107,#400108),
(#400109,#400110,#400111),(#400112,#400113,#400114)),.UNSPECIFIED.,.F.,
 .F.,.F.)
B_SPLINE_SURFACE_WITH_KNOTS((4,4),(3,3),(1.55009486301137E-5,4.9206551047443E-5),
(-8.13759515176208E-5,1.),.UNSPECIFIED.)
GEOMETRIC_REPRESENTATION_ITEM()
RATIONAL_B_SPLINE_SURFACE(((1.00002372912337,0.85420063959968,1.),(1.00001423585994,
0.912530301180536,1.),(1.00000710550471,0.956341495377428,1.),(1.00001238975909,
0.923873338137019,1.)))
REPRESENTATION_ITEM('')
SURFACE()
);
#2985=(
BOUNDED_SURFACE()
B_SPLINE_SURFACE(3,2,((#400118,#400119,#400120),(#400121,#400122,#400123),
(#400124,#400125,#400126),(#400127,#400128,#400129)),.UNSPECIFIED.,.F.,
 .F.,.F.)
B_SPLINE_SURFACE_WITH_KNOTS((4,4),(3,3),(-3.39934179457841E-6,3.73927597403565E-5),
(-0.00186004067418672,1.00069373317461),.UNSPECIFIED.)
GEOMETRIC_REPRESENTATION_ITEM()
RATIONAL_B_SPLINE_SURFACE(((1.00072100136055,0.806051963875299,1.00026859642699),
(1.00060048440154,0.838470803558624,1.00022369994503),(1.00053106448795,
0.857144632272335,1.00019783877226),(1.00054515072852,0.853355459539078,
1.00020308635443)))
REPRESENTATION_ITEM('')
SURFACE()
);
#2986=(
BOUNDED_SURFACE()
B_SPLINE_SURFACE(3,2,((#400131,#400132,#400133),(#400134,#400135,#400136),
(#400137,#400138,#400139),(#400140,#400141,#400142)),.UNSPECIFIED.,.F.,
 .F.,.F.)
B_SPLINE_SURFACE_WITH_KNOTS((4,4),(3,3),(-1.62630325872826E-19,9.54361881492173E-5),
(0.,1.),.UNSPECIFIED.)
GEOMETRIC_REPRESENTATION_ITEM()
RATIONAL_B_SPLINE_SURFACE(((1.,0.816715621142052,1.),(1.,0.815907587407943,
1.),(1.,0.815115959345206,1.),(1.,0.814339887349198,1.)))
REPRESENTATION_ITEM('')
SURFACE()
);
#2987=(
BOUNDED_SURFACE()
B_SPLINE_SURFACE(3,2,((#400144,#400145,#400146),(#400147,#400148,#400149),
(#400150,#400151,#400152),(#400153,#400154,#400155)),.UNSPECIFIED.,.F.,
 .F.,.F.)
B_SPLINE_SURFACE_WITH_KNOTS((4,4),(3,3),(-1.86347248395946E-19,4.68197758448201E-5),
(0.,1.),.UNSPECIFIED.)
GEOMETRIC_REPRESENTATION_ITEM()
RATIONAL_B_SPLINE_SURFACE(((1.,0.81671562114205,1.),(1.,0.953638980025198,
1.),(1.,0.954506925408061,1.),(1.,0.816715621142052,1.)))
REPRESENTATION_ITEM('')
SURFACE()
);
#2988=(
BOUNDED_SURFACE()
B_SPLINE_SURFACE(3,2,((#400157,#400158,#400159),(#400160,#400161,#400162),
(#400163,#400164,#400165),(#400166,#400167,#400168)),.UNSPECIFIED.,.F.,
 .F.,.F.)
B_SPLINE_SURFACE_WITH_KNOTS((4,4),(3,3),(1.0842021724855E-19,9.54361881492174E-5),
(0.,1.),.UNSPECIFIED.)
GEOMETRIC_REPRESENTATION_ITEM()
RATIONAL_B_SPLINE_SURFACE(((1.,0.814339887349194,1.),(1.,0.815115959345208,
1.),(1.,0.815907587407941,1.),(1.,0.81671562114205,1.)))
REPRESENTATION_ITEM('')
SURFACE()
);
#2989=(
BOUNDED_SURFACE()
B_SPLINE_SURFACE(3,2,((#400170,#400171,#400172),(#400173,#400174,#400175),
(#400176,#400177,#400178),(#400179,#400180,#400181)),.UNSPECIFIED.,.F.,
 .F.,.F.)
B_SPLINE_SURFACE_WITH_KNOTS((4,4),(3,3),(-3.39528393502491E-6,3.73481232852729E-5),
(-0.00165018033330832,1.),.UNSPECIFIED.)
GEOMETRIC_REPRESENTATION_ITEM()
RATIONAL_B_SPLINE_SURFACE(((1.00048354385566,0.853487571660394,1.),(1.00047110510921,
0.857256476851454,1.),(1.00053193201108,0.838826096655882,1.),(1.00063970687726,
0.806170615310084,1.)))
REPRESENTATION_ITEM('')
SURFACE()
);
#2990=(
BOUNDED_SURFACE()
B_SPLINE_SURFACE(3,2,((#400185,#400186,#400187),(#400188,#400189,#400190),
(#400191,#400192,#400193),(#400194,#400195,#400196)),.UNSPECIFIED.,.F.,
 .F.,.F.)
B_SPLINE_SURFACE_WITH_KNOTS((4,4),(3,3),(2.02993869230508E-5,5.39756952687126E-5),
(-0.000116281069690976,1.),.UNSPECIFIED.)
GEOMETRIC_REPRESENTATION_ITEM()
RATIONAL_B_SPLINE_SURFACE(((1.00001770479726,0.923870681143028,1.),(1.00001014104057,
0.956394275543463,1.),(1.00002037300274,0.912397594905633,1.),(1.00003390859462,
0.854195550869773,1.)))
REPRESENTATION_ITEM('')
SURFACE()
);
#2991=(
BOUNDED_SURFACE()
B_SPLINE_SURFACE(3,2,((#400289,#400290,#400291),(#400292,#400293,#400294),
(#400295,#400296,#400297),(#400298,#400299,#400300)),.UNSPECIFIED.,.F.,
 .F.,.F.)
B_SPLINE_SURFACE_WITH_KNOTS((4,4),(3,3),(0.00135801595889393,0.00148409170619832),
(0.,1.),.UNSPECIFIED.)
GEOMETRIC_REPRESENTATION_ITEM()
RATIONAL_B_SPLINE_SURFACE(((1.,0.818301933966441,1.),(1.,0.817226613172331,
1.),(1.,0.816179643373969,1.),(1.,0.815159387863649,1.)))
REPRESENTATION_ITEM('')
SURFACE()
);
#2992=(
BOUNDED_SURFACE()
B_SPLINE_SURFACE(3,2,((#400339,#400340,#400341),(#400342,#400343,#400344),
(#400345,#400346,#400347),(#400348,#400349,#400350)),.UNSPECIFIED.,.F.,
 .F.,.F.)
B_SPLINE_SURFACE_WITH_KNOTS((4,4),(3,3),(-1.54744435121998E-6,1.54744435122074E-5),
(0.,1.01516989835084),.UNSPECIFIED.)
GEOMETRIC_REPRESENTATION_ITEM()
RATIONAL_B_SPLINE_SURFACE(((1.,0.334740937363976,1.02018382471433),(1.,
0.867753072814783,1.00401234488522),(1.,0.98891790308095,1.00033622856755),
(1.,1.,1.)))
REPRESENTATION_ITEM('')
SURFACE()
);
#2993=(
BOUNDED_SURFACE()
B_SPLINE_SURFACE(3,2,((#400352,#400353,#400354),(#400355,#400356,#400357),
(#400358,#400359,#400360),(#400361,#400362,#400363)),.UNSPECIFIED.,.F.,
 .F.,.F.)
B_SPLINE_SURFACE_WITH_KNOTS((4,4),(3,3),(0.00137194782501028,0.00149814269699235),
(0.,1.),.UNSPECIFIED.)
GEOMETRIC_REPRESENTATION_ITEM()
RATIONAL_B_SPLINE_SURFACE(((1.,0.815158509402317,1.),(1.,0.816179044148169,
1.),(1.,0.81722630811993,1.),(1.,0.818301939488802,1.)))
REPRESENTATION_ITEM('')
SURFACE()
);
#2994=(
BOUNDED_SURFACE()
B_SPLINE_SURFACE(3,2,((#400407,#400408,#400409),(#400410,#400411,#400412),
(#400413,#400414,#400415),(#400416,#400417,#400418)),.UNSPECIFIED.,.F.,
 .F.,.F.)
B_SPLINE_SURFACE_WITH_KNOTS((4,4),(3,3),(1.55009486301137E-5,4.92065510474433E-5),
(-8.1375951657446E-5,1.),.UNSPECIFIED.)
GEOMETRIC_REPRESENTATION_ITEM()
RATIONAL_B_SPLINE_SURFACE(((1.00002372912341,0.854200639599655,1.),(1.00001423585997,
0.912530301180528,1.),(1.00000710550472,0.956341495377426,1.),(1.00001238975911,
0.92387333813701,1.)))
REPRESENTATION_ITEM('')
SURFACE()
);
#2995=(
BOUNDED_SURFACE()
B_SPLINE_SURFACE(3,2,((#400422,#400423,#400424),(#400425,#400426,#400427),
(#400428,#400429,#400430),(#400431,#400432,#400433)),.UNSPECIFIED.,.F.,
 .F.,.F.)
B_SPLINE_SURFACE_WITH_KNOTS((4,4),(3,3),(-3.39934179457807E-6,3.73927597403566E-5),
(-0.00186004067478061,1.00069373317481),.UNSPECIFIED.)
GEOMETRIC_REPRESENTATION_ITEM()
RATIONAL_B_SPLINE_SURFACE(((1.00072100136078,0.806051963875142,1.00026859642707),
(1.00060048440173,0.838470803558472,1.00022369994509),(1.00053106448812,
0.857144632272242,1.00019783877231),(1.0005451507287,0.853355459538941,
1.00020308635449)))
REPRESENTATION_ITEM('')
SURFACE()
);
#2996=(
BOUNDED_SURFACE()
B_SPLINE_SURFACE(3,2,((#400435,#400436,#400437),(#400438,#400439,#400440),
(#400441,#400442,#400443),(#400444,#400445,#400446)),.UNSPECIFIED.,.F.,
 .F.,.F.)
B_SPLINE_SURFACE_WITH_KNOTS((4,4),(3,3),(0.,9.54361881492173E-5),(0.,1.),
 .UNSPECIFIED.)
GEOMETRIC_REPRESENTATION_ITEM()
RATIONAL_B_SPLINE_SURFACE(((1.,0.81671562114205,1.),(1.,0.815907587407937,
1.),(1.,0.815115959345202,1.),(1.,0.814339887349193,1.)))
REPRESENTATION_ITEM('')
SURFACE()
);
#2997=(
BOUNDED_SURFACE()
B_SPLINE_SURFACE(3,2,((#400448,#400449,#400450),(#400451,#400452,#400453),
(#400454,#400455,#400456),(#400457,#400458,#400459)),.UNSPECIFIED.,.F.,
 .F.,.F.)
B_SPLINE_SURFACE_WITH_KNOTS((4,4),(3,3),(4.47233396150271E-19,4.68197758448205E-5),
(0.,1.),.UNSPECIFIED.)
GEOMETRIC_REPRESENTATION_ITEM()
RATIONAL_B_SPLINE_SURFACE(((1.,0.81671562114205,1.),(1.,0.953638980025206,
1.),(1.,0.954506925408054,1.),(1.,0.816715621142053,1.)))
REPRESENTATION_ITEM('')
SURFACE()
);
#2998=(
BOUNDED_SURFACE()
B_SPLINE_SURFACE(3,2,((#400461,#400462,#400463),(#400464,#400465,#400466),
(#400467,#400468,#400469),(#400470,#400471,#400472)),.UNSPECIFIED.,.F.,
 .F.,.F.)
B_SPLINE_SURFACE_WITH_KNOTS((4,4),(3,3),(-2.16840434497101E-19,9.54361881492177E-5),
(0.,1.),.UNSPECIFIED.)
GEOMETRIC_REPRESENTATION_ITEM()
RATIONAL_B_SPLINE_SURFACE(((1.,0.814339887349193,1.),(1.,0.815115959345207,
1.),(1.,0.815907587407941,1.),(1.,0.81671562114205,1.)))
REPRESENTATION_ITEM('')
SURFACE()
);
#2999=(
BOUNDED_SURFACE()
B_SPLINE_SURFACE(3,2,((#400474,#400475,#400476),(#400477,#400478,#400479),
(#400480,#400481,#400482),(#400483,#400484,#400485)),.UNSPECIFIED.,.F.,
 .F.,.F.)
B_SPLINE_SURFACE_WITH_KNOTS((4,4),(3,3),(-3.39528393502376E-6,3.73481232852733E-5),
(-0.00165018033265501,1.),.UNSPECIFIED.)
GEOMETRIC_REPRESENTATION_ITEM()
RATIONAL_B_SPLINE_SURFACE(((1.00048354385547,0.853487571660489,1.),(1.00047110510903,
0.857256476851551,1.),(1.00053193201087,0.838826096655975,1.),(1.00063970687701,
0.806170615310217,1.)))
REPRESENTATION_ITEM('')
SURFACE()
);
#3000=(
BOUNDED_SURFACE()
B_SPLINE_SURFACE(3,2,((#400489,#400490,#400491),(#400492,#400493,#400494),
(#400495,#400496,#400497),(#400498,#400499,#400500)),.UNSPECIFIED.,.F.,
 .F.,.F.)
B_SPLINE_SURFACE_WITH_KNOTS((4,4),(3,3),(2.02993869230507E-5,5.3975695268713E-5),
(-0.000116281069929633,1.),.UNSPECIFIED.)
GEOMETRIC_REPRESENTATION_ITEM()
RATIONAL_B_SPLINE_SURFACE(((1.0000177047973,0.923870681143012,1.),(1.00001014104059,
0.956394275543438,1.),(1.00002037300279,0.912397594905633,1.),(1.00003390859469,
0.854195550869724,1.)))
REPRESENTATION_ITEM('')
SURFACE()
);
#3001=(
BOUNDED_SURFACE()
B_SPLINE_SURFACE(3,2,((#400593,#400594,#400595),(#400596,#400597,#400598),
(#400599,#400600,#400601),(#400602,#400603,#400604)),.UNSPECIFIED.,.F.,
 .F.,.F.)
B_SPLINE_SURFACE_WITH_KNOTS((4,4),(3,3),(0.00135801595889393,0.00148409170619832),
(0.,1.),.UNSPECIFIED.)
GEOMETRIC_REPRESENTATION_ITEM()
RATIONAL_B_SPLINE_SURFACE(((1.,0.818301933966445,1.),(1.,0.817226613172345,
1.),(1.,0.816179643373948,1.),(1.,0.815159387863651,1.)))
REPRESENTATION_ITEM('')
SURFACE()
);
#3002=(
BOUNDED_SURFACE()
B_SPLINE_SURFACE(3,2,((#400643,#400644,#400645),(#400646,#400647,#400648),
(#400649,#400650,#400651),(#400652,#400653,#400654)),.UNSPECIFIED.,.F.,
 .F.,.F.)
B_SPLINE_SURFACE_WITH_KNOTS((4,4),(3,3),(-1.54744435122071E-6,1.5474443512207E-5),
(-0.0151698983637522,1.),.UNSPECIFIED.)
GEOMETRIC_REPRESENTATION_ITEM()
RATIONAL_B_SPLINE_SURFACE(((1.02018382473177,0.334740937355425,1.),(1.00401234488869,
0.867753072813156,1.),(1.00033622856784,0.988917903080815,1.),(1.,1.,1.)))
REPRESENTATION_ITEM('')
SURFACE()
);
#3003=(
BOUNDED_SURFACE()
B_SPLINE_SURFACE(3,2,((#400656,#400657,#400658),(#400659,#400660,#400661),
(#400662,#400663,#400664),(#400665,#400666,#400667)),.UNSPECIFIED.,.F.,
 .F.,.F.)
B_SPLINE_SURFACE_WITH_KNOTS((4,4),(3,3),(0.00137194782501028,0.00149814269699235),
(0.,1.),.UNSPECIFIED.)
GEOMETRIC_REPRESENTATION_ITEM()
RATIONAL_B_SPLINE_SURFACE(((1.,0.815158509402319,1.),(1.,0.816179044148169,
1.),(1.,0.817226308119925,1.),(1.,0.818301939488808,1.)))
REPRESENTATION_ITEM('')
SURFACE()
);
#3004=(
BOUNDED_SURFACE()
B_SPLINE_SURFACE(3,2,((#400711,#400712,#400713),(#400714,#400715,#400716),
(#400717,#400718,#400719),(#400720,#400721,#400722)),.UNSPECIFIED.,.F.,
 .F.,.F.)
B_SPLINE_SURFACE_WITH_KNOTS((4,4),(3,3),(1.55009486301137E-5,4.92065510474432E-5),
(-8.13759513806331E-5,1.),.UNSPECIFIED.)
GEOMETRIC_REPRESENTATION_ITEM()
RATIONAL_B_SPLINE_SURFACE(((1.00002372912333,0.854200639599697,1.),(1.00001423585992,
0.912530301180547,1.),(1.0000071055047,0.956341495377435,1.),(1.00001238975907,
0.92387333813703,1.)))
REPRESENTATION_ITEM('')
SURFACE()
);
#3005=(
BOUNDED_SURFACE()
B_SPLINE_SURFACE(3,2,((#400726,#400727,#400728),(#400729,#400730,#400731),
(#400732,#400733,#400734),(#400735,#400736,#400737)),.UNSPECIFIED.,.F.,
 .F.,.F.)
B_SPLINE_SURFACE_WITH_KNOTS((4,4),(3,3),(-3.39934179457817E-6,3.73927597403566E-5),
(-0.00186004067470975,1.00069373317475),.UNSPECIFIED.)
GEOMETRIC_REPRESENTATION_ITEM()
RATIONAL_B_SPLINE_SURFACE(((1.00072100136075,0.806051963875176,1.00026859642705),
(1.00060048440171,0.838470803558489,1.00022369994507),(1.0005310644881,
0.857144632272263,1.0001978387723),(1.00054515072868,0.853355459538963,
1.00020308635447)))
REPRESENTATION_ITEM('')
SURFACE()
);
#3006=(
BOUNDED_SURFACE()
B_SPLINE_SURFACE(3,2,((#400739,#400740,#400741),(#400742,#400743,#400744),
(#400745,#400746,#400747),(#400748,#400749,#400750)),.UNSPECIFIED.,.F.,
 .F.,.F.)
B_SPLINE_SURFACE_WITH_KNOTS((4,4),(3,3),(1.0842021724855E-19,9.54361881492173E-5),
(0.,1.),.UNSPECIFIED.)
GEOMETRIC_REPRESENTATION_ITEM()
RATIONAL_B_SPLINE_SURFACE(((1.,0.816715621142048,1.),(1.,0.815907587407936,
1.),(1.,0.815115959345214,1.),(1.,0.81433988734919,1.)))
REPRESENTATION_ITEM('')
SURFACE()
);
#3007=(
BOUNDED_SURFACE()
B_SPLINE_SURFACE(3,2,((#400752,#400753,#400754),(#400755,#400756,#400757),
(#400758,#400759,#400760),(#400761,#400762,#400763)),.UNSPECIFIED.,.F.,
 .F.,.F.)
B_SPLINE_SURFACE_WITH_KNOTS((4,4),(3,3),(1.01643953670516E-20,4.68197758448207E-5),
(0.,1.),.UNSPECIFIED.)
GEOMETRIC_REPRESENTATION_ITEM()
RATIONAL_B_SPLINE_SURFACE(((1.,0.816715621142052,1.),(1.,0.9536389800252,
1.),(1.,0.954506925408064,1.),(1.,0.816715621142051,1.)))
REPRESENTATION_ITEM('')
SURFACE()
);
#3008=(
BOUNDED_SURFACE()
B_SPLINE_SURFACE(3,2,((#400765,#400766,#400767),(#400768,#400769,#400770),
(#400771,#400772,#400773),(#400774,#400775,#400776)),.UNSPECIFIED.,.F.,
 .F.,.F.)
B_SPLINE_SURFACE_WITH_KNOTS((4,4),(3,3),(0.,9.5436188149218E-5),(0.,1.),
 .UNSPECIFIED.)
GEOMETRIC_REPRESENTATION_ITEM()
RATIONAL_B_SPLINE_SURFACE(((1.,0.814339887349194,1.),(1.,0.815115959345198,
1.),(1.,0.815907587407943,1.),(1.,0.816715621142052,1.)))
REPRESENTATION_ITEM('')
SURFACE()
);
#3009=(
BOUNDED_SURFACE()
B_SPLINE_SURFACE(3,2,((#400778,#400779,#400780),(#400781,#400782,#400783),
(#400784,#400785,#400786),(#400787,#400788,#400789)),.UNSPECIFIED.,.F.,
 .F.,.F.)
B_SPLINE_SURFACE_WITH_KNOTS((4,4),(3,3),(-3.39528393502483E-6,3.73481232852733E-5),
(-0.00165018033317789,1.),.UNSPECIFIED.)
GEOMETRIC_REPRESENTATION_ITEM()
RATIONAL_B_SPLINE_SURFACE(((1.00048354385562,0.853487571660412,1.),(1.00047110510918,
0.857256476851481,1.),(1.00053193201104,0.838826096655889,1.),(1.00063970687721,
0.806170615310112,1.)))
REPRESENTATION_ITEM('')
SURFACE()
);
#3010=(
BOUNDED_SURFACE()
B_SPLINE_SURFACE(3,2,((#400793,#400794,#400795),(#400796,#400797,#400798),
(#400799,#400800,#400801),(#400802,#400803,#400804)),.UNSPECIFIED.,.F.,
 .F.,.F.)
B_SPLINE_SURFACE_WITH_KNOTS((4,4),(3,3),(2.02993869230513E-5,5.39756952686903E-5),
(-0.000116281069625813,1.),.UNSPECIFIED.)
GEOMETRIC_REPRESENTATION_ITEM()
RATIONAL_B_SPLINE_SURFACE(((1.00001770479725,0.923870681143032,1.),(1.00001014104056,
0.956394275543427,1.),(1.00002037300273,0.912397594905699,1.),(1.0000339085946,
0.8541955508699,1.)))
REPRESENTATION_ITEM('')
SURFACE()
);
#3011=(
BOUNDED_SURFACE()
B_SPLINE_SURFACE(3,2,((#400897,#400898,#400899),(#400900,#400901,#400902),
(#400903,#400904,#400905),(#400906,#400907,#400908)),.UNSPECIFIED.,.F.,
 .F.,.F.)
B_SPLINE_SURFACE_WITH_KNOTS((4,4),(3,3),(0.00135801595889393,0.00148409170619832),
(0.,1.),.UNSPECIFIED.)
GEOMETRIC_REPRESENTATION_ITEM()
RATIONAL_B_SPLINE_SURFACE(((1.,0.818301933966444,1.),(1.,0.817226613172345,
1.),(1.,0.816179643373944,1.),(1.,0.815159387863653,1.)))
REPRESENTATION_ITEM('')
SURFACE()
);
#3012=(
BOUNDED_SURFACE()
B_SPLINE_SURFACE(3,2,((#400947,#400948,#400949),(#400950,#400951,#400952),
(#400953,#400954,#400955),(#400956,#400957,#400958)),.UNSPECIFIED.,.F.,
 .F.,.F.)
B_SPLINE_SURFACE_WITH_KNOTS((4,4),(3,3),(-1.54744435122073E-6,1.54744435122075E-5),
(-0.0151698983625013,1.),.UNSPECIFIED.)
GEOMETRIC_REPRESENTATION_ITEM()
RATIONAL_B_SPLINE_SURFACE(((1.02018382473008,0.334740937356303,1.),(1.00401234488835,
0.867753072813278,1.),(1.00033622856781,0.98891790308083,1.),(1.,1.,1.)))
REPRESENTATION_ITEM('')
SURFACE()
);
#3013=(
BOUNDED_SURFACE()
B_SPLINE_SURFACE(3,2,((#400960,#400961,#400962),(#400963,#400964,#400965),
(#400966,#400967,#400968),(#400969,#400970,#400971)),.UNSPECIFIED.,.F.,
 .F.,.F.)
B_SPLINE_SURFACE_WITH_KNOTS((4,4),(3,3),(0.00137194782501028,0.00149814269699235),
(0.,1.),.UNSPECIFIED.)
GEOMETRIC_REPRESENTATION_ITEM()
RATIONAL_B_SPLINE_SURFACE(((1.,0.815158509402321,1.),(1.,0.816179044148159,
1.),(1.,0.817226308119919,1.),(1.,0.818301939488811,1.)))
REPRESENTATION_ITEM('')
SURFACE()
);
#3014=(
BOUNDED_SURFACE()
B_SPLINE_SURFACE(3,2,((#401015,#401016,#401017),(#401018,#401019,#401020),
(#401021,#401022,#401023),(#401024,#401025,#401026)),.UNSPECIFIED.,.F.,
 .F.,.F.)
B_SPLINE_SURFACE_WITH_KNOTS((4,4),(3,3),(1.55009486301137E-5,4.92065510474426E-5),
(-8.13759514346884E-5,1.),.UNSPECIFIED.)
GEOMETRIC_REPRESENTATION_ITEM()
RATIONAL_B_SPLINE_SURFACE(((1.00002372912334,0.854200639599699,1.),(1.00001423585993,
0.912530301180536,1.),(1.0000071055047,0.956341495377432,1.),(1.00001238975908,
0.923873338137028,1.)))
REPRESENTATION_ITEM('')
SURFACE()
);
#3015=(
BOUNDED_SURFACE()
B_SPLINE_SURFACE(3,2,((#401030,#401031,#401032),(#401033,#401034,#401035),
(#401036,#401037,#401038),(#401039,#401040,#401041)),.UNSPECIFIED.,.F.,
 .F.,.F.)
B_SPLINE_SURFACE_WITH_KNOTS((4,4),(3,3),(-3.39934179457863E-6,3.73927597403564E-5),
(-0.00186004067392485,1.00069373317437),.UNSPECIFIED.)
GEOMETRIC_REPRESENTATION_ITEM()
RATIONAL_B_SPLINE_SURFACE(((1.00072100136044,0.806051963875394,1.0002685964269),
(1.00060048440145,0.838470803558699,1.00022369994495),(1.00053106448787,
0.8571446322724,1.00019783877219),(1.00054515072845,0.853355459539153,1.00020308635436)))
REPRESENTATION_ITEM('')
SURFACE()
);
#3016=(
BOUNDED_SURFACE()
B_SPLINE_SURFACE(3,2,((#401043,#401044,#401045),(#401046,#401047,#401048),
(#401049,#401050,#401051),(#401052,#401053,#401054)),.UNSPECIFIED.,.F.,
 .F.,.F.)
B_SPLINE_SURFACE_WITH_KNOTS((4,4),(3,3),(-5.42101086242752E-20,9.54361881492172E-5),
(0.,1.),.UNSPECIFIED.)
GEOMETRIC_REPRESENTATION_ITEM()
RATIONAL_B_SPLINE_SURFACE(((1.,0.81671562114205,1.),(1.,0.815907587407929,
1.),(1.,0.815115959345219,1.),(1.,0.814339887349188,1.)))
REPRESENTATION_ITEM('')
SURFACE()
);
#3017=(
BOUNDED_SURFACE()
B_SPLINE_SURFACE(3,2,((#401056,#401057,#401058),(#401059,#401060,#401061),
(#401062,#401063,#401064),(#401065,#401066,#401067)),.UNSPECIFIED.,.F.,
 .F.,.F.)
B_SPLINE_SURFACE_WITH_KNOTS((4,4),(3,3),(1.0842021724855E-19,4.6819775844821E-5),
(0.,1.),.UNSPECIFIED.)
GEOMETRIC_REPRESENTATION_ITEM()
RATIONAL_B_SPLINE_SURFACE(((1.,0.816715621142049,1.),(1.,0.953638980025214,
1.),(1.,0.954506925408049,1.),(1.,0.81671562114205,1.)))
REPRESENTATION_ITEM('')
SURFACE()
);
#3018=(
BOUNDED_SURFACE()
B_SPLINE_SURFACE(3,2,((#401069,#401070,#401071),(#401072,#401073,#401074),
(#401075,#401076,#401077),(#401078,#401079,#401080)),.UNSPECIFIED.,.F.,
 .F.,.F.)
B_SPLINE_SURFACE_WITH_KNOTS((4,4),(3,3),(0.,9.54361881492176E-5),(0.,1.),
 .UNSPECIFIED.)
GEOMETRIC_REPRESENTATION_ITEM()
RATIONAL_B_SPLINE_SURFACE(((1.,0.814339887349192,1.),(1.,0.815115959345197,
1.),(1.,0.815907587407954,1.),(1.,0.816715621142049,1.)))
REPRESENTATION_ITEM('')
SURFACE()
);
#3019=(
BOUNDED_SURFACE()
B_SPLINE_SURFACE(3,2,((#401082,#401083,#401084),(#401085,#401086,#401087),
(#401088,#401089,#401090),(#401091,#401092,#401093)),.UNSPECIFIED.,.F.,
 .F.,.F.)
B_SPLINE_SURFACE_WITH_KNOTS((4,4),(3,3),(-3.39528393502374E-6,3.73481232852735E-5),
(-0.00165018033314802,1.),.UNSPECIFIED.)
GEOMETRIC_REPRESENTATION_ITEM()
RATIONAL_B_SPLINE_SURFACE(((1.00048354385562,0.853487571660416,1.),(1.00047110510917,
0.857256476851484,1.),(1.00053193201103,0.838826096655888,1.),(1.0006397068772,
0.806170615310112,1.)))
REPRESENTATION_ITEM('')
SURFACE()
);
#3020=(
BOUNDED_SURFACE()
B_SPLINE_SURFACE(3,2,((#401097,#401098,#401099),(#401100,#401101,#401102),
(#401103,#401104,#401105),(#401106,#401107,#401108)),.UNSPECIFIED.,.F.,
 .F.,.F.)
B_SPLINE_SURFACE_WITH_KNOTS((4,4),(3,3),(2.02993869230511E-5,5.39756952686907E-5),
(-0.000116281069653282,1.),.UNSPECIFIED.)
GEOMETRIC_REPRESENTATION_ITEM()
RATIONAL_B_SPLINE_SURFACE(((1.00001770479726,0.92387068114303,1.),(1.00001014104057,
0.956394275543435,1.),(1.00002037300274,0.912397594905695,1.),(1.00003390859461,
0.854195550869892,1.)))
REPRESENTATION_ITEM('')
SURFACE()
);
#3021=(
BOUNDED_SURFACE()
B_SPLINE_SURFACE(3,2,((#401201,#401202,#401203),(#401204,#401205,#401206),
(#401207,#401208,#401209),(#401210,#401211,#401212)),.UNSPECIFIED.,.F.,
 .F.,.F.)
B_SPLINE_SURFACE_WITH_KNOTS((4,4),(3,3),(0.00135801595889393,0.00148409170619832),
(0.,1.),.UNSPECIFIED.)
GEOMETRIC_REPRESENTATION_ITEM()
RATIONAL_B_SPLINE_SURFACE(((1.,0.818301933966434,1.),(1.,0.817226613172369,
1.),(1.,0.816179643373941,1.),(1.,0.815159387863662,1.)))
REPRESENTATION_ITEM('')
SURFACE()
);
#3022=(
BOUNDED_SURFACE()
B_SPLINE_SURFACE(3,2,((#401251,#401252,#401253),(#401254,#401255,#401256),
(#401257,#401258,#401259),(#401260,#401261,#401262)),.UNSPECIFIED.,.F.,
 .F.,.F.)
B_SPLINE_SURFACE_WITH_KNOTS((4,4),(3,3),(-1.54744435122073E-6,1.54744435122075E-5),
(-0.0151698983614576,1.01516989836034),.UNSPECIFIED.)
GEOMETRIC_REPRESENTATION_ITEM()
RATIONAL_B_SPLINE_SURFACE(((1.02018382472867,0.32449821941385,1.02018382472716),
(1.00401234488807,0.86571692171071,1.00401234488777),(1.00033622856779,
0.988747276629654,1.00033622856777),(1.,1.,1.)))
REPRESENTATION_ITEM('')
SURFACE()
);
#3023=(
BOUNDED_SURFACE()
B_SPLINE_SURFACE(3,2,((#401264,#401265,#401266),(#401267,#401268,#401269),
(#401270,#401271,#401272),(#401273,#401274,#401275)),.UNSPECIFIED.,.F.,
 .F.,.F.)
B_SPLINE_SURFACE_WITH_KNOTS((4,4),(3,3),(0.00137194782501028,0.00149814269699235),
(0.,1.),.UNSPECIFIED.)
GEOMETRIC_REPRESENTATION_ITEM()
RATIONAL_B_SPLINE_SURFACE(((1.,0.815158509402314,1.),(1.,0.816179044148169,
1.),(1.,0.817226308119935,1.),(1.,0.818301939488798,1.)))
REPRESENTATION_ITEM('')
SURFACE()
);
#3024=(
BOUNDED_SURFACE()
B_SPLINE_SURFACE(3,2,((#401319,#401320,#401321),(#401322,#401323,#401324),
(#401325,#401326,#401327),(#401328,#401329,#401330)),.UNSPECIFIED.,.F.,
 .F.,.F.)
B_SPLINE_SURFACE_WITH_KNOTS((4,4),(3,3),(1.55009486301137E-5,4.9206551047443E-5),
(-8.13759512452905E-5,1.),.UNSPECIFIED.)
GEOMETRIC_REPRESENTATION_ITEM()
RATIONAL_B_SPLINE_SURFACE(((1.00002372912329,0.85420063959972,1.),(1.00001423585989,
0.912530301180559,1.),(1.00000710550469,0.95634149537744,1.),(1.00001238975905,
0.923873338137041,1.)))
REPRESENTATION_ITEM('')
SURFACE()
);
#3025=(
BOUNDED_SURFACE()
B_SPLINE_SURFACE(3,2,((#401334,#401335,#401336),(#401337,#401338,#401339),
(#401340,#401341,#401342),(#401343,#401344,#401345)),.UNSPECIFIED.,.F.,
 .F.,.F.)
B_SPLINE_SURFACE_WITH_KNOTS((4,4),(3,3),(-3.39934179457794E-6,3.73927597403568E-5),
(-0.00186004067403676,1.00069373317385),.UNSPECIFIED.)
GEOMETRIC_REPRESENTATION_ITEM()
RATIONAL_B_SPLINE_SURFACE(((1.00072100136049,0.806051963875495,1.0002685964267),
(1.00060048440149,0.838470803558738,1.00022369994478),(1.0005310644879,
0.8571446322725,1.00019783877204),(1.00054515072848,0.853355459539201,1.00020308635421)))
REPRESENTATION_ITEM('')
SURFACE()
);
#3026=(
BOUNDED_SURFACE()
B_SPLINE_SURFACE(3,2,((#401347,#401348,#401349),(#401350,#401351,#401352),
(#401353,#401354,#401355),(#401356,#401357,#401358)),.UNSPECIFIED.,.F.,
 .F.,.F.)
B_SPLINE_SURFACE_WITH_KNOTS((4,4),(3,3),(0.,9.54361881492172E-5),(0.,1.),
 .UNSPECIFIED.)
GEOMETRIC_REPRESENTATION_ITEM()
RATIONAL_B_SPLINE_SURFACE(((1.,0.816715621142058,1.),(1.,0.815907587407938,
1.),(1.,0.815115959345213,1.),(1.,0.814339887349197,1.)))
REPRESENTATION_ITEM('')
SURFACE()
);
#3027=(
BOUNDED_SURFACE()
B_SPLINE_SURFACE(3,2,((#401360,#401361,#401362),(#401363,#401364,#401365),
(#401366,#401367,#401368),(#401369,#401370,#401371)),.UNSPECIFIED.,.F.,
 .F.,.F.)
B_SPLINE_SURFACE_WITH_KNOTS((4,4),(3,3),(1.91429446079472E-19,4.68197758448204E-5),
(0.,1.),.UNSPECIFIED.)
GEOMETRIC_REPRESENTATION_ITEM()
RATIONAL_B_SPLINE_SURFACE(((1.,0.816715621142047,1.),(1.,0.953638980025218,
1.),(1.,0.954506925408038,1.),(1.,0.816715621142058,1.)))
REPRESENTATION_ITEM('')
SURFACE()
);
#3028=(
BOUNDED_SURFACE()
B_SPLINE_SURFACE(3,2,((#401373,#401374,#401375),(#401376,#401377,#401378),
(#401379,#401380,#401381),(#401382,#401383,#401384)),.UNSPECIFIED.,.F.,
 .F.,.F.)
B_SPLINE_SURFACE_WITH_KNOTS((4,4),(3,3),(1.62630325872826E-19,9.54361881492179E-5),
(0.,1.),.UNSPECIFIED.)
GEOMETRIC_REPRESENTATION_ITEM()
RATIONAL_B_SPLINE_SURFACE(((1.,0.814339887349189,1.),(1.,0.815115959345212,
1.),(1.,0.81590758740794,1.),(1.,0.816715621142047,1.)))
REPRESENTATION_ITEM('')
SURFACE()
);
#3029=(
BOUNDED_SURFACE()
B_SPLINE_SURFACE(3,2,((#401386,#401387,#401388),(#401389,#401390,#401391),
(#401392,#401393,#401394),(#401395,#401396,#401397)),.UNSPECIFIED.,.F.,
 .F.,.F.)
B_SPLINE_SURFACE_WITH_KNOTS((4,4),(3,3),(-3.39528393502484E-6,3.73481232852723E-5),
(-0.00165018033327953,1.),.UNSPECIFIED.)
GEOMETRIC_REPRESENTATION_ITEM()
RATIONAL_B_SPLINE_SURFACE(((1.00048354385565,0.85348757166039,1.),(1.00047110510921,
0.857256476851472,1.),(1.00053193201107,0.838826096655868,1.),(1.00063970687725,
0.8061706153101,1.)))
REPRESENTATION_ITEM('')
SURFACE()
);
#3030=(
BOUNDED_SURFACE()
B_SPLINE_SURFACE(3,2,((#401401,#401402,#401403),(#401404,#401405,#401406),
(#401407,#401408,#401409),(#401410,#401411,#401412)),.UNSPECIFIED.,.F.,
 .F.,.F.)
B_SPLINE_SURFACE_WITH_KNOTS((4,4),(3,3),(2.02993869230511E-5,5.39756952686904E-5),
(-0.000116281070078735,1.),.UNSPECIFIED.)
GEOMETRIC_REPRESENTATION_ITEM()
RATIONAL_B_SPLINE_SURFACE(((1.00001770479732,0.923870681142998,1.),(1.0000101410406,
0.956394275543412,1.),(1.00002037300281,0.912397594905667,1.),(1.00003390859473,
0.854195550869826,1.)))
REPRESENTATION_ITEM('')
SURFACE()
);
#3031=(
BOUNDED_SURFACE()
B_SPLINE_SURFACE(3,2,((#401505,#401506,#401507),(#401508,#401509,#401510),
(#401511,#401512,#401513),(#401514,#401515,#401516)),.UNSPECIFIED.,.F.,
 .F.,.F.)
B_SPLINE_SURFACE_WITH_KNOTS((4,4),(3,3),(0.00135801595889393,0.00148409170619832),
(0.,1.),.UNSPECIFIED.)
GEOMETRIC_REPRESENTATION_ITEM()
RATIONAL_B_SPLINE_SURFACE(((1.,0.818301933966433,1.),(1.,0.81722661317235,
1.),(1.,0.816179643373951,1.),(1.,0.815159387863659,1.)))
REPRESENTATION_ITEM('')
SURFACE()
);
#3032=(
BOUNDED_SURFACE()
B_SPLINE_SURFACE(3,2,((#401555,#401556,#401557),(#401558,#401559,#401560),
(#401561,#401562,#401563),(#401564,#401565,#401566)),.UNSPECIFIED.,.F.,
 .F.,.F.)
B_SPLINE_SURFACE_WITH_KNOTS((4,4),(3,3),(-1.54744435122067E-6,1.54744435122071E-5),
(-0.0151698983645437,1.01516989835833),.UNSPECIFIED.)
GEOMETRIC_REPRESENTATION_ITEM()
RATIONAL_B_SPLINE_SURFACE(((1.02018382473283,0.324498219413116,1.02018382472444),
(1.0040123448889,0.86571692171053,1.00401234488723),(1.00033622856786,0.988747276629684,
1.00033622856772),(1.,1.,1.)))
REPRESENTATION_ITEM('')
SURFACE()
);
#3033=(
BOUNDED_SURFACE()
B_SPLINE_SURFACE(3,2,((#401568,#401569,#401570),(#401571,#401572,#401573),
(#401574,#401575,#401576),(#401577,#401578,#401579)),.UNSPECIFIED.,.F.,
 .F.,.F.)
B_SPLINE_SURFACE_WITH_KNOTS((4,4),(3,3),(0.00137194782501028,0.00149814269699235),
(0.,1.),.UNSPECIFIED.)
GEOMETRIC_REPRESENTATION_ITEM()
RATIONAL_B_SPLINE_SURFACE(((1.,0.815158509402314,1.),(1.,0.81617904414816,
1.),(1.,0.817226308119927,1.),(1.,0.818301939488808,1.)))
REPRESENTATION_ITEM('')
SURFACE()
);
#3034=(
BOUNDED_SURFACE()
B_SPLINE_SURFACE(3,2,((#401623,#401624,#401625),(#401626,#401627,#401628),
(#401629,#401630,#401631),(#401632,#401633,#401634)),.UNSPECIFIED.,.F.,
 .F.,.F.)
B_SPLINE_SURFACE_WITH_KNOTS((4,4),(3,3),(1.55009486301138E-5,4.92065510474435E-5),
(-8.13759512394683E-5,1.),.UNSPECIFIED.)
GEOMETRIC_REPRESENTATION_ITEM()
RATIONAL_B_SPLINE_SURFACE(((1.00002372912329,0.854200639599714,1.),(1.00001423585989,
0.912530301180566,1.),(1.00000710550469,0.956341495377436,1.),(1.00001238975905,
0.92387333813704,1.)))
REPRESENTATION_ITEM('')
SURFACE()
);
#3035=(
BOUNDED_SURFACE()
B_SPLINE_SURFACE(3,2,((#401638,#401639,#401640),(#401641,#401642,#401643),
(#401644,#401645,#401646),(#401647,#401648,#401649)),.UNSPECIFIED.,.F.,
 .F.,.F.)
B_SPLINE_SURFACE_WITH_KNOTS((4,4),(3,3),(-3.39934179457784E-6,3.73927597403568E-5),
(-0.001860040674796,1.00069373317472),.UNSPECIFIED.)
GEOMETRIC_REPRESENTATION_ITEM()
RATIONAL_B_SPLINE_SURFACE(((1.00072100136078,0.806051963875152,1.00026859642704),
(1.00060048440174,0.838470803558502,1.00022369994506),(1.00053106448812,
0.857144632272237,1.00019783877229),(1.0005451507287,0.85335545953896,1.00020308635446)))
REPRESENTATION_ITEM('')
SURFACE()
);
#3036=(
BOUNDED_SURFACE()
B_SPLINE_SURFACE(3,2,((#401651,#401652,#401653),(#401654,#401655,#401656),
(#401657,#401658,#401659),(#401660,#401661,#401662)),.UNSPECIFIED.,.F.,
 .F.,.F.)
B_SPLINE_SURFACE_WITH_KNOTS((4,4),(3,3),(-1.62630325872826E-19,9.54361881492172E-5),
(0.,1.),.UNSPECIFIED.)
GEOMETRIC_REPRESENTATION_ITEM()
RATIONAL_B_SPLINE_SURFACE(((1.,0.816715621142042,1.),(1.,0.815907587407949,
1.),(1.,0.815115959345201,1.),(1.,0.814339887349195,1.)))
REPRESENTATION_ITEM('')
SURFACE()
);
#3037=(
BOUNDED_SURFACE()
B_SPLINE_SURFACE(3,2,((#401664,#401665,#401666),(#401667,#401668,#401669),
(#401670,#401671,#401672),(#401673,#401674,#401675)),.UNSPECIFIED.,.F.,
 .F.,.F.)
B_SPLINE_SURFACE_WITH_KNOTS((4,4),(3,3),(4.2351647362715E-20,4.6819775844821E-5),
(0.,1.),.UNSPECIFIED.)
GEOMETRIC_REPRESENTATION_ITEM()
RATIONAL_B_SPLINE_SURFACE(((1.,0.816715621142047,1.),(1.,0.953638980025218,
1.),(1.,0.954506925408044,1.),(1.,0.816715621142054,1.)))
REPRESENTATION_ITEM('')
SURFACE()
);
#3038=(
BOUNDED_SURFACE()
B_SPLINE_SURFACE(3,2,((#401677,#401678,#401679),(#401680,#401681,#401682),
(#401683,#401684,#401685),(#401686,#401687,#401688)),.UNSPECIFIED.,.F.,
 .F.,.F.)
B_SPLINE_SURFACE_WITH_KNOTS((4,4),(3,3),(-1.0842021724855E-19,9.54361881492177E-5),
(0.,1.),.UNSPECIFIED.)
GEOMETRIC_REPRESENTATION_ITEM()
RATIONAL_B_SPLINE_SURFACE(((1.,0.814339887349196,1.),(1.,0.815115959345204,
1.),(1.,0.81590758740794,1.),(1.,0.816715621142047,1.)))
REPRESENTATION_ITEM('')
SURFACE()
);
#3039=(
BOUNDED_SURFACE()
B_SPLINE_SURFACE(3,2,((#401690,#401691,#401692),(#401693,#401694,#401695),
(#401696,#401697,#401698),(#401699,#401700,#401701)),.UNSPECIFIED.,.F.,
 .F.,.F.)
B_SPLINE_SURFACE_WITH_KNOTS((4,4),(3,3),(-3.39528393502374E-6,3.73481232852733E-5),
(-0.00165018033334311,1.),.UNSPECIFIED.)
GEOMETRIC_REPRESENTATION_ITEM()
RATIONAL_B_SPLINE_SURFACE(((1.00048354385567,0.853487571660385,1.),(1.00047110510922,
0.857256476851452,1.),(1.00053193201109,0.838826096655862,1.),(1.00063970687728,
0.80617061531008,1.)))
REPRESENTATION_ITEM('')
SURFACE()
);
#3040=(
BOUNDED_SURFACE()
B_SPLINE_SURFACE(3,2,((#401705,#401706,#401707),(#401708,#401709,#401710),
(#401711,#401712,#401713),(#401714,#401715,#401716)),.UNSPECIFIED.,.F.,
 .F.,.F.)
B_SPLINE_SURFACE_WITH_KNOTS((4,4),(3,3),(2.02993869230507E-5,5.39756952686899E-5),
(-0.000116281069940536,1.),.UNSPECIFIED.)
GEOMETRIC_REPRESENTATION_ITEM()
RATIONAL_B_SPLINE_SURFACE(((1.0000177047973,0.923870681143011,1.),(1.00001014104059,
0.95639427554341,1.),(1.00002037300279,0.912397594905685,1.),(1.00003390859469,
0.854195550869851,1.)))
REPRESENTATION_ITEM('')
SURFACE()
);
#3041=(
BOUNDED_SURFACE()
B_SPLINE_SURFACE(3,2,((#401809,#401810,#401811),(#401812,#401813,#401814),
(#401815,#401816,#401817),(#401818,#401819,#401820)),.UNSPECIFIED.,.F.,
 .F.,.F.)
B_SPLINE_SURFACE_WITH_KNOTS((4,4),(3,3),(0.00135801595889393,0.00148409170619832),
(0.,1.),.UNSPECIFIED.)
GEOMETRIC_REPRESENTATION_ITEM()
RATIONAL_B_SPLINE_SURFACE(((1.,0.818301933966449,1.),(1.,0.817226613172348,
1.),(1.,0.816179643373952,1.),(1.,0.815159387863656,1.)))
REPRESENTATION_ITEM('')
SURFACE()
);
#3042=(
BOUNDED_SURFACE()
B_SPLINE_SURFACE(3,2,((#401859,#401860,#401861),(#401862,#401863,#401864),
(#401865,#401866,#401867),(#401868,#401869,#401870)),.UNSPECIFIED.,.F.,
 .F.,.F.)
B_SPLINE_SURFACE_WITH_KNOTS((4,4),(3,3),(-1.5474443512208E-6,1.54744435122078E-5),
(-0.0151698983646347,1.),.UNSPECIFIED.)
GEOMETRIC_REPRESENTATION_ITEM()
RATIONAL_B_SPLINE_SURFACE(((1.02018382473296,0.334740937354848,1.),(1.00401234488892,
0.867753072812993,1.),(1.00033622856786,0.988917903080814,1.),(1.,1.,1.)))
REPRESENTATION_ITEM('')
SURFACE()
);
#3043=(
BOUNDED_SURFACE()
B_SPLINE_SURFACE(3,2,((#401872,#401873,#401874),(#401875,#401876,#401877),
(#401878,#401879,#401880),(#401881,#401882,#401883)),.UNSPECIFIED.,.F.,
 .F.,.F.)
B_SPLINE_SURFACE_WITH_KNOTS((4,4),(3,3),(0.00137194782501028,0.00149814269699235),
(0.,1.),.UNSPECIFIED.)
GEOMETRIC_REPRESENTATION_ITEM()
RATIONAL_B_SPLINE_SURFACE(((1.,0.81515850940232,1.),(1.,0.816179044148161,
1.),(1.,0.817226308119925,1.),(1.,0.818301939488814,1.)))
REPRESENTATION_ITEM('')
SURFACE()
);
#3044=(
BOUNDED_SURFACE()
B_SPLINE_SURFACE(3,2,((#401927,#401928,#401929),(#401930,#401931,#401932),
(#401933,#401934,#401935),(#401936,#401937,#401938)),.UNSPECIFIED.,.F.,
 .F.,.F.)
B_SPLINE_SURFACE_WITH_KNOTS((4,4),(3,3),(1.55009486301137E-5,4.92065510474434E-5),
(-8.13759515589481E-5,1.),.UNSPECIFIED.)
GEOMETRIC_REPRESENTATION_ITEM()
RATIONAL_B_SPLINE_SURFACE(((1.00002372912338,0.854200639599674,1.),(1.00001423585995,
0.912530301180525,1.),(1.00000710550471,0.956341495377429,1.),(1.0000123897591,
0.923873338137018,1.)))
REPRESENTATION_ITEM('')
SURFACE()
);
#3045=(
BOUNDED_SURFACE()
B_SPLINE_SURFACE(3,2,((#401942,#401943,#401944),(#401945,#401946,#401947),
(#401948,#401949,#401950),(#401951,#401952,#401953)),.UNSPECIFIED.,.F.,
 .F.,.F.)
B_SPLINE_SURFACE_WITH_KNOTS((4,4),(3,3),(-3.39934179457785E-6,3.73927597403568E-5),
(-0.00186004067443997,1.00069373317459),.UNSPECIFIED.)
GEOMETRIC_REPRESENTATION_ITEM()
RATIONAL_B_SPLINE_SURFACE(((1.00072100136064,0.806051963875255,1.00026859642698),
(1.00060048440162,0.838470803558584,1.00022369994502),(1.00053106448802,
0.857144632272302,1.00019783877225),(1.0005451507286,0.853355459539047,
1.00020308635443)))
REPRESENTATION_ITEM('')
SURFACE()
);
#3046=(
BOUNDED_SURFACE()
B_SPLINE_SURFACE(3,2,((#401955,#401956,#401957),(#401958,#401959,#401960),
(#401961,#401962,#401963),(#401964,#401965,#401966)),.UNSPECIFIED.,.F.,
 .F.,.F.)
B_SPLINE_SURFACE_WITH_KNOTS((4,4),(3,3),(2.16840434497101E-19,9.54361881492174E-5),
(0.,1.),.UNSPECIFIED.)
GEOMETRIC_REPRESENTATION_ITEM()
RATIONAL_B_SPLINE_SURFACE(((1.,0.816715621142055,1.),(1.,0.815907587407941,
1.),(1.,0.815115959345212,1.),(1.,0.814339887349196,1.)))
REPRESENTATION_ITEM('')
SURFACE()
);
#3047=(
BOUNDED_SURFACE()
B_SPLINE_SURFACE(3,2,((#401968,#401969,#401970),(#401971,#401972,#401973),
(#401974,#401975,#401976),(#401977,#401978,#401979)),.UNSPECIFIED.,.F.,
 .F.,.F.)
B_SPLINE_SURFACE_WITH_KNOTS((4,4),(3,3),(3.10014058695074E-19,4.68197758448212E-5),
(0.,1.),.UNSPECIFIED.)
GEOMETRIC_REPRESENTATION_ITEM()
RATIONAL_B_SPLINE_SURFACE(((1.,0.816715621142044,1.),(1.,0.95363898002522,
1.),(1.,0.954506925408041,1.),(1.,0.816715621142055,1.)))
REPRESENTATION_ITEM('')
SURFACE()
);
#3048=(
BOUNDED_SURFACE()
B_SPLINE_SURFACE(3,2,((#401981,#401982,#401983),(#401984,#401985,#401986),
(#401987,#401988,#401989),(#401990,#401991,#401992)),.UNSPECIFIED.,.F.,
 .F.,.F.)
B_SPLINE_SURFACE_WITH_KNOTS((4,4),(3,3),(2.16840434497101E-19,9.54361881492178E-5),
(0.,1.),.UNSPECIFIED.)
GEOMETRIC_REPRESENTATION_ITEM()
RATIONAL_B_SPLINE_SURFACE(((1.,0.814339887349193,1.),(1.,0.815115959345206,
1.),(1.,0.815907587407946,1.),(1.,0.816715621142047,1.)))
REPRESENTATION_ITEM('')
SURFACE()
);
#3049=(
BOUNDED_SURFACE()
B_SPLINE_SURFACE(3,2,((#401994,#401995,#401996),(#401997,#401998,#401999),
(#402000,#402001,#402002),(#402003,#402004,#402005)),.UNSPECIFIED.,.F.,
 .F.,.F.)
B_SPLINE_SURFACE_WITH_KNOTS((4,4),(3,3),(-3.39528393502495E-6,3.7348123285273E-5),
(-0.00165018033346878,1.),.UNSPECIFIED.)
GEOMETRIC_REPRESENTATION_ITEM()
RATIONAL_B_SPLINE_SURFACE(((1.00048354385571,0.853487571660368,1.),(1.00047110510926,
0.857256476851447,1.),(1.00053193201113,0.838826096655836,1.),(1.00063970687733,
0.806170615310062,1.)))
REPRESENTATION_ITEM('')
SURFACE()
);
#3050=(
BOUNDED_SURFACE()
B_SPLINE_SURFACE(3,2,((#402009,#402010,#402011),(#402012,#402013,#402014),
(#402015,#402016,#402017),(#402018,#402019,#402020)),.UNSPECIFIED.,.F.,
 .F.,.F.)
B_SPLINE_SURFACE_WITH_KNOTS((4,4),(3,3),(2.02993869230511E-5,5.39756952686901E-5),
(-0.000116281069764521,1.),.UNSPECIFIED.)
GEOMETRIC_REPRESENTATION_ITEM()
RATIONAL_B_SPLINE_SURFACE(((1.00001770479727,0.92387068114302,1.),(1.00001014104058,
0.956394275543423,1.),(1.00002037300276,0.912397594905696,1.),(1.00003390859464,
0.854195550869868,1.)))
REPRESENTATION_ITEM('')
SURFACE()
);
#3051=(
BOUNDED_SURFACE()
B_SPLINE_SURFACE(3,2,((#402113,#402114,#402115),(#402116,#402117,#402118),
(#402119,#402120,#402121),(#402122,#402123,#402124)),.UNSPECIFIED.,.F.,
 .F.,.F.)
B_SPLINE_SURFACE_WITH_KNOTS((4,4),(3,3),(0.00135801595889393,0.00148409170619832),
(0.,1.),.UNSPECIFIED.)
GEOMETRIC_REPRESENTATION_ITEM()
RATIONAL_B_SPLINE_SURFACE(((1.,0.818301933966446,1.),(1.,0.817226613172357,
1.),(1.,0.81617964337394,1.),(1.,0.815159387863662,1.)))
REPRESENTATION_ITEM('')
SURFACE()
);
#3052=(
BOUNDED_SURFACE()
B_SPLINE_SURFACE(3,2,((#402163,#402164,#402165),(#402166,#402167,#402168),
(#402169,#402170,#402171),(#402172,#402173,#402174)),.UNSPECIFIED.,.F.,
 .F.,.F.)
B_SPLINE_SURFACE_WITH_KNOTS((4,4),(3,3),(-1.54744435122075E-6,1.5474443512207E-5),
(0.,1.01516989835802),.UNSPECIFIED.)
GEOMETRIC_REPRESENTATION_ITEM()
RATIONAL_B_SPLINE_SURFACE(((1.,0.33474093735925,1.02018382472402),(1.,0.867753072813741,
1.00401234488715),(1.,0.988917903080923,1.00033622856771),(1.,1.,1.)))
REPRESENTATION_ITEM('')
SURFACE()
);
#3053=(
BOUNDED_SURFACE()
B_SPLINE_SURFACE(3,2,((#402176,#402177,#402178),(#402179,#402180,#402181),
(#402182,#402183,#402184),(#402185,#402186,#402187)),.UNSPECIFIED.,.F.,
 .F.,.F.)
B_SPLINE_SURFACE_WITH_KNOTS((4,4),(3,3),(0.00137194782501028,0.00149814269699235),
(0.,1.),.UNSPECIFIED.)
GEOMETRIC_REPRESENTATION_ITEM()
RATIONAL_B_SPLINE_SURFACE(((1.,0.815158509402314,1.),(1.,0.816179044148173,
1.),(1.,0.817226308119935,1.),(1.,0.818301939488801,1.)))
REPRESENTATION_ITEM('')
SURFACE()
);
#3054=(
BOUNDED_SURFACE()
B_SPLINE_SURFACE(3,2,((#402231,#402232,#402233),(#402234,#402235,#402236),
(#402237,#402238,#402239),(#402240,#402241,#402242)),.UNSPECIFIED.,.F.,
 .F.,.F.)
B_SPLINE_SURFACE_WITH_KNOTS((4,4),(3,3),(1.55009486301137E-5,4.92065510474435E-5),
(-8.13759513899056E-5,1.),.UNSPECIFIED.)
GEOMETRIC_REPRESENTATION_ITEM()
RATIONAL_B_SPLINE_SURFACE(((1.00002372912333,0.854200639599704,1.),(1.00001423585992,
0.912530301180536,1.),(1.0000071055047,0.956341495377438,1.),(1.00001238975907,
0.923873338137032,1.)))
REPRESENTATION_ITEM('')
SURFACE()
);
#3055=(
BOUNDED_SURFACE()
B_SPLINE_SURFACE(3,2,((#402246,#402247,#402248),(#402249,#402250,#402251),
(#402252,#402253,#402254),(#402255,#402256,#402257)),.UNSPECIFIED.,.F.,
 .F.,.F.)
B_SPLINE_SURFACE_WITH_KNOTS((4,4),(3,3),(-3.39934179457833E-6,3.73927597403565E-5),
(-0.00186004067416003,1.00069373317436),.UNSPECIFIED.)
GEOMETRIC_REPRESENTATION_ITEM()
RATIONAL_B_SPLINE_SURFACE(((1.00072100136054,0.80605196387537,1.00026859642689),
(1.00060048440153,0.838470803558641,1.00022369994495),(1.00053106448794,
0.8571446322724,1.00019783877218),(1.00054515072851,0.853355459539105,1.00020308635436)))
REPRESENTATION_ITEM('')
SURFACE()
);
#3056=(
BOUNDED_SURFACE()
B_SPLINE_SURFACE(3,2,((#402259,#402260,#402261),(#402262,#402263,#402264),
(#402265,#402266,#402267),(#402268,#402269,#402270)),.UNSPECIFIED.,.F.,
 .F.,.F.)
B_SPLINE_SURFACE_WITH_KNOTS((4,4),(3,3),(-2.16840434497101E-19,9.54361881492173E-5),
(0.,1.),.UNSPECIFIED.)
GEOMETRIC_REPRESENTATION_ITEM()
RATIONAL_B_SPLINE_SURFACE(((1.,0.81671562114205,1.),(1.,0.815907587407941,
1.),(1.,0.815115959345207,1.),(1.,0.814339887349197,1.)))
REPRESENTATION_ITEM('')
SURFACE()
);
#3057=(
BOUNDED_SURFACE()
B_SPLINE_SURFACE(3,2,((#402272,#402273,#402274),(#402275,#402276,#402277),
(#402278,#402279,#402280),(#402281,#402282,#402283)),.UNSPECIFIED.,.F.,
 .F.,.F.)
B_SPLINE_SURFACE_WITH_KNOTS((4,4),(3,3),(-2.87991202066462E-19,4.68197758448209E-5),
(0.,1.),.UNSPECIFIED.)
GEOMETRIC_REPRESENTATION_ITEM()
RATIONAL_B_SPLINE_SURFACE(((1.,0.816715621142049,1.),(1.,0.953638980025204,
1.),(1.,0.954506925408058,1.),(1.,0.816715621142057,1.)))
REPRESENTATION_ITEM('')
SURFACE()
);
#3058=(
BOUNDED_SURFACE()
B_SPLINE_SURFACE(3,2,((#402285,#402286,#402287),(#402288,#402289,#402290),
(#402291,#402292,#402293),(#402294,#402295,#402296)),.UNSPECIFIED.,.F.,
 .F.,.F.)
B_SPLINE_SURFACE_WITH_KNOTS((4,4),(3,3),(1.62630325872826E-19,9.54361881492178E-5),
(0.,1.),.UNSPECIFIED.)
GEOMETRIC_REPRESENTATION_ITEM()
RATIONAL_B_SPLINE_SURFACE(((1.,0.814339887349197,1.),(1.,0.815115959345213,
1.),(1.,0.815907587407937,1.),(1.,0.816715621142052,1.)))
REPRESENTATION_ITEM('')
SURFACE()
);
#3059=(
BOUNDED_SURFACE()
B_SPLINE_SURFACE(3,2,((#402298,#402299,#402300),(#402301,#402302,#402303),
(#402304,#402305,#402306),(#402307,#402308,#402309)),.UNSPECIFIED.,.F.,
 .F.,.F.)
B_SPLINE_SURFACE_WITH_KNOTS((4,4),(3,3),(-3.39528393502494E-6,3.73481232852724E-5),
(-0.00165018033326561,1.),.UNSPECIFIED.)
GEOMETRIC_REPRESENTATION_ITEM()
RATIONAL_B_SPLINE_SURFACE(((1.00048354385565,0.853487571660401,1.),(1.0004711051092,
0.857256476851465,1.),(1.00053193201107,0.838826096655876,1.),(1.00063970687725,
0.8061706153101,1.)))
REPRESENTATION_ITEM('')
SURFACE()
);
#3060=(
BOUNDED_SURFACE()
B_SPLINE_SURFACE(3,2,((#402313,#402314,#402315),(#402316,#402317,#402318),
(#402319,#402320,#402321),(#402322,#402323,#402324)),.UNSPECIFIED.,.F.,
 .F.,.F.)
B_SPLINE_SURFACE_WITH_KNOTS((4,4),(3,3),(2.02993869230509E-5,5.39756952686898E-5),
(-0.000116281069845253,1.),.UNSPECIFIED.)
GEOMETRIC_REPRESENTATION_ITEM()
RATIONAL_B_SPLINE_SURFACE(((1.00001770479729,0.923870681143014,1.),(1.00001014104058,
0.956394275543427,1.),(1.00002037300277,0.912397594905681,1.),(1.00003390859467,
0.854195550869864,1.)))
REPRESENTATION_ITEM('')
SURFACE()
);
#3061=(
BOUNDED_SURFACE()
B_SPLINE_SURFACE(3,2,((#402417,#402418,#402419),(#402420,#402421,#402422),
(#402423,#402424,#402425),(#402426,#402427,#402428)),.UNSPECIFIED.,.F.,
 .F.,.F.)
B_SPLINE_SURFACE_WITH_KNOTS((4,4),(3,3),(0.00135801595889393,0.00148409170619832),
(0.,1.),.UNSPECIFIED.)
GEOMETRIC_REPRESENTATION_ITEM()
RATIONAL_B_SPLINE_SURFACE(((1.,0.818301933966443,1.),(1.,0.817226613172338,
1.),(1.,0.816179643373947,1.),(1.,0.815159387863652,1.)))
REPRESENTATION_ITEM('')
SURFACE()
);
#3062=(
BOUNDED_SURFACE()
B_SPLINE_SURFACE(3,2,((#402467,#402468,#402469),(#402470,#402471,#402472),
(#402473,#402474,#402475),(#402476,#402477,#402478)),.UNSPECIFIED.,.F.,
 .F.,.F.)
B_SPLINE_SURFACE_WITH_KNOTS((4,4),(3,3),(-1.54744435122089E-6,1.54744435122086E-5),
(-0.0151698983679409,1.),.UNSPECIFIED.)
GEOMETRIC_REPRESENTATION_ITEM()
RATIONAL_B_SPLINE_SURFACE(((1.02018382473742,0.334740937352698,1.),(1.00401234488981,
0.867753072812613,1.),(1.00033622856794,0.988917903080764,1.),(1.,1.,1.)))
REPRESENTATION_ITEM('')
SURFACE()
);
#3063=(
BOUNDED_SURFACE()
B_SPLINE_SURFACE(3,2,((#402480,#402481,#402482),(#402483,#402484,#402485),
(#402486,#402487,#402488),(#402489,#402490,#402491)),.UNSPECIFIED.,.F.,
 .F.,.F.)
B_SPLINE_SURFACE_WITH_KNOTS((4,4),(3,3),(0.00137194782501028,0.00149814269699235),
(0.,1.),.UNSPECIFIED.)
GEOMETRIC_REPRESENTATION_ITEM()
RATIONAL_B_SPLINE_SURFACE(((1.,0.815158509402319,1.),(1.,0.81617904414817,
1.),(1.,0.817226308119927,1.),(1.,0.818301939488815,1.)))
REPRESENTATION_ITEM('')
SURFACE()
);
#3064=(
BOUNDED_SURFACE()
B_SPLINE_SURFACE(3,2,((#402535,#402536,#402537),(#402538,#402539,#402540),
(#402541,#402542,#402543),(#402544,#402545,#402546)),.UNSPECIFIED.,.F.,
 .F.,.F.)
B_SPLINE_SURFACE_WITH_KNOTS((4,4),(3,3),(1.55009486301137E-5,4.92065510474433E-5),
(-8.13759512715114E-5,1.),.UNSPECIFIED.)
GEOMETRIC_REPRESENTATION_ITEM()
RATIONAL_B_SPLINE_SURFACE(((1.00002372912329,0.85420063959972,1.),(1.0000142358599,
0.912530301180555,1.),(1.00000710550469,0.956341495377441,1.),(1.00001238975905,
0.923873338137036,1.)))
REPRESENTATION_ITEM('')
SURFACE()
);
#3065=(
BOUNDED_SURFACE()
B_SPLINE_SURFACE(3,2,((#402550,#402551,#402552),(#402553,#402554,#402555),
(#402556,#402557,#402558),(#402559,#402560,#402561)),.UNSPECIFIED.,.F.,
 .F.,.F.)
B_SPLINE_SURFACE_WITH_KNOTS((4,4),(3,3),(-3.39934179457849E-6,3.73927597403563E-5),
(-0.00186004067427479,1.00069373317438),.UNSPECIFIED.)
GEOMETRIC_REPRESENTATION_ITEM()
RATIONAL_B_SPLINE_SURFACE(((1.00072100136058,0.806051963875348,1.0002685964269),
(1.00060048440157,0.838470803558596,1.00022369994495),(1.00053106448797,
0.857144632272381,1.00019783877219),(1.00054515072855,0.853355459539078,
1.00020308635436)))
REPRESENTATION_ITEM('')
SURFACE()
);
#3066=(
BOUNDED_SURFACE()
B_SPLINE_SURFACE(3,2,((#402563,#402564,#402565),(#402566,#402567,#402568),
(#402569,#402570,#402571),(#402572,#402573,#402574)),.UNSPECIFIED.,.F.,
 .F.,.F.)
B_SPLINE_SURFACE_WITH_KNOTS((4,4),(3,3),(-3.79470760369927E-19,9.54361881492171E-5),
(0.,1.),.UNSPECIFIED.)
GEOMETRIC_REPRESENTATION_ITEM()
RATIONAL_B_SPLINE_SURFACE(((1.,0.816715621142048,1.),(1.,0.815907587407932,
1.),(1.,0.815115959345209,1.),(1.,0.81433988734919,1.)))
REPRESENTATION_ITEM('')
SURFACE()
);
#3067=(
BOUNDED_SURFACE()
B_SPLINE_SURFACE(3,2,((#402576,#402577,#402578),(#402579,#402580,#402581),
(#402582,#402583,#402584),(#402585,#402586,#402587)),.UNSPECIFIED.,.F.,
 .F.,.F.)
B_SPLINE_SURFACE_WITH_KNOTS((4,4),(3,3),(-1.28749007982654E-19,4.68197758448209E-5),
(0.,1.),.UNSPECIFIED.)
GEOMETRIC_REPRESENTATION_ITEM()
RATIONAL_B_SPLINE_SURFACE(((1.,0.816715621142051,1.),(1.,0.953638980025206,
1.),(1.,0.954506925408048,1.),(1.,0.816715621142061,1.)))
REPRESENTATION_ITEM('')
SURFACE()
);
#3068=(
BOUNDED_SURFACE()
B_SPLINE_SURFACE(3,2,((#402589,#402590,#402591),(#402592,#402593,#402594),
(#402595,#402596,#402597),(#402598,#402599,#402600)),.UNSPECIFIED.,.F.,
 .F.,.F.)
B_SPLINE_SURFACE_WITH_KNOTS((4,4),(3,3),(-1.0842021724855E-19,9.54361881492177E-5),
(0.,1.),.UNSPECIFIED.)
GEOMETRIC_REPRESENTATION_ITEM()
RATIONAL_B_SPLINE_SURFACE(((1.,0.814339887349197,1.),(1.,0.815115959345209,
1.),(1.,0.815907587407942,1.),(1.,0.816715621142054,1.)))
REPRESENTATION_ITEM('')
SURFACE()
);
#3069=(
BOUNDED_SURFACE()
B_SPLINE_SURFACE(3,2,((#402602,#402603,#402604),(#402605,#402606,#402607),
(#402608,#402609,#402610),(#402611,#402612,#402613)),.UNSPECIFIED.,.F.,
 .F.,.F.)
B_SPLINE_SURFACE_WITH_KNOTS((4,4),(3,3),(-3.39528393502479E-6,3.73481232852735E-5),
(-0.00165018033315628,1.),.UNSPECIFIED.)
GEOMETRIC_REPRESENTATION_ITEM()
RATIONAL_B_SPLINE_SURFACE(((1.00048354385562,0.853487571660415,1.),(1.00047110510917,
0.857256476851483,1.),(1.00053193201103,0.838826096655902,1.),(1.00063970687721,
0.806170615310112,0.999999999999999)))
REPRESENTATION_ITEM('')
SURFACE()
);
#3070=(
BOUNDED_SURFACE()
B_SPLINE_SURFACE(3,2,((#402617,#402618,#402619),(#402620,#402621,#402622),
(#402623,#402624,#402625),(#402626,#402627,#402628)),.UNSPECIFIED.,.F.,
 .F.,.F.)
B_SPLINE_SURFACE_WITH_KNOTS((4,4),(3,3),(2.02993869230511E-5,5.39756952686902E-5),
(-0.000116281069516842,1.),.UNSPECIFIED.)
GEOMETRIC_REPRESENTATION_ITEM()
RATIONAL_B_SPLINE_SURFACE(((1.00001770479724,0.923870681143042,1.),(1.00001014104055,
0.956394275543434,1.),(1.00002037300271,0.912397594905713,1.),(1.00003390859457,
0.85419555086991,1.)))
REPRESENTATION_ITEM('')
SURFACE()
);
#3071=(
BOUNDED_SURFACE()
B_SPLINE_SURFACE(3,2,((#402721,#402722,#402723),(#402724,#402725,#402726),
(#402727,#402728,#402729),(#402730,#402731,#402732)),.UNSPECIFIED.,.F.,
 .F.,.F.)
B_SPLINE_SURFACE_WITH_KNOTS((4,4),(3,3),(0.00135801595889393,0.00148409170619832),
(0.,1.),.UNSPECIFIED.)
GEOMETRIC_REPRESENTATION_ITEM()
RATIONAL_B_SPLINE_SURFACE(((1.,0.818301933966441,1.),(1.,0.817226613172343,
1.),(1.,0.816179643373954,1.),(1.,0.815159387863651,1.)))
REPRESENTATION_ITEM('')
SURFACE()
);
#3072=(
BOUNDED_SURFACE()
B_SPLINE_SURFACE(3,2,((#402771,#402772,#402773),(#402774,#402775,#402776),
(#402777,#402778,#402779),(#402780,#402781,#402782)),.UNSPECIFIED.,.F.,
 .F.,.F.)
B_SPLINE_SURFACE_WITH_KNOTS((4,4),(3,3),(-1.54744435122074E-6,1.54744435122071E-5),
(-0.0151698983619576,1.01516989836059),.UNSPECIFIED.)
GEOMETRIC_REPRESENTATION_ITEM()
RATIONAL_B_SPLINE_SURFACE(((1.02018382472934,0.324498219413315,1.02018382472749),
(1.0040123448882,0.865716921710694,1.00401234488783),(1.0003362285678,0.988747276629597,
1.00033622856777),(1.,1.,1.)))
REPRESENTATION_ITEM('')
SURFACE()
);
#3073=(
BOUNDED_SURFACE()
B_SPLINE_SURFACE(3,2,((#402784,#402785,#402786),(#402787,#402788,#402789),
(#402790,#402791,#402792),(#402793,#402794,#402795)),.UNSPECIFIED.,.F.,
 .F.,.F.)
B_SPLINE_SURFACE_WITH_KNOTS((4,4),(3,3),(0.00137194782501028,0.00149814269699235),
(0.,1.),.UNSPECIFIED.)
GEOMETRIC_REPRESENTATION_ITEM()
RATIONAL_B_SPLINE_SURFACE(((1.,0.815158509402318,1.),(1.,0.816179044148166,
1.),(1.,0.817226308119925,1.),(1.,0.818301939488809,1.)))
REPRESENTATION_ITEM('')
SURFACE()
);
#3074=(
BOUNDED_SURFACE()
B_SPLINE_SURFACE(3,2,((#402839,#402840,#402841),(#402842,#402843,#402844),
(#402845,#402846,#402847),(#402848,#402849,#402850)),.UNSPECIFIED.,.F.,
 .F.,.F.)
B_SPLINE_SURFACE_WITH_KNOTS((4,4),(3,3),(1.55009486301137E-5,4.9206551047443E-5),
(-8.13759517604745E-5,1.),.UNSPECIFIED.)
GEOMETRIC_REPRESENTATION_ITEM()
RATIONAL_B_SPLINE_SURFACE(((1.00002372912344,0.854200639599649,1.),(1.00001423585998,
0.912530301180504,1.),(1.00000710550473,0.956341495377428,1.),(1.00001238975913,
0.923873338137001,1.)))
REPRESENTATION_ITEM('')
SURFACE()
);
#3075=(
BOUNDED_SURFACE()
B_SPLINE_SURFACE(3,2,((#402854,#402855,#402856),(#402857,#402858,#402859),
(#402860,#402861,#402862),(#402863,#402864,#402865)),.UNSPECIFIED.,.F.,
 .F.,.F.)
B_SPLINE_SURFACE_WITH_KNOTS((4,4),(3,3),(-3.39934179457832E-6,3.73927597403565E-5),
(-0.00186004067362119,1.00069373317417),.UNSPECIFIED.)
GEOMETRIC_REPRESENTATION_ITEM()
RATIONAL_B_SPLINE_SURFACE(((1.00072100136033,0.806051963875496,1.00026859642682),
(1.00060048440136,0.838470803558756,1.00022369994489),(1.00053106448778,
0.857144632272493,1.00019783877213),(1.00054515072836,0.853355459539209,
1.0002030863543)))
REPRESENTATION_ITEM('')
SURFACE()
);
#3076=(
BOUNDED_SURFACE()
B_SPLINE_SURFACE(3,2,((#402867,#402868,#402869),(#402870,#402871,#402872),
(#402873,#402874,#402875),(#402876,#402877,#402878)),.UNSPECIFIED.,.F.,
 .F.,.F.)
B_SPLINE_SURFACE_WITH_KNOTS((4,4),(3,3),(5.42101086242752E-20,9.54361881492173E-5),
(0.,1.),.UNSPECIFIED.)
GEOMETRIC_REPRESENTATION_ITEM()
RATIONAL_B_SPLINE_SURFACE(((1.,0.816715621142048,1.),(1.,0.815907587407936,
1.),(1.,0.81511595934521,1.),(1.,0.81433988734919,1.)))
REPRESENTATION_ITEM('')
SURFACE()
);
#3077=(
BOUNDED_SURFACE()
B_SPLINE_SURFACE(3,2,((#402880,#402881,#402882),(#402883,#402884,#402885),
(#402886,#402887,#402888),(#402889,#402890,#402891)),.UNSPECIFIED.,.F.,
 .F.,.F.)
B_SPLINE_SURFACE_WITH_KNOTS((4,4),(3,3),(1.54159996400283E-19,4.68197758448206E-5),
(0.,1.),.UNSPECIFIED.)
GEOMETRIC_REPRESENTATION_ITEM()
RATIONAL_B_SPLINE_SURFACE(((1.,0.81671562114205,1.),(1.,0.953638980025216,
1.),(1.,0.954506925408041,1.),(1.,0.816715621142061,1.)))
REPRESENTATION_ITEM('')
SURFACE()
);
#3078=(
BOUNDED_SURFACE()
B_SPLINE_SURFACE(3,2,((#402893,#402894,#402895),(#402896,#402897,#402898),
(#402899,#402900,#402901),(#402902,#402903,#402904)),.UNSPECIFIED.,.F.,
 .F.,.F.)
B_SPLINE_SURFACE_WITH_KNOTS((4,4),(3,3),(-1.62630325872826E-19,9.54361881492177E-5),
(0.,1.),.UNSPECIFIED.)
GEOMETRIC_REPRESENTATION_ITEM()
RATIONAL_B_SPLINE_SURFACE(((1.,0.814339887349192,1.),(1.,0.815115959345203,
1.),(1.,0.815907587407944,1.),(1.,0.816715621142047,1.)))
REPRESENTATION_ITEM('')
SURFACE()
);
#3079=(
BOUNDED_SURFACE()
B_SPLINE_SURFACE(3,2,((#402906,#402907,#402908),(#402909,#402910,#402911),
(#402912,#402913,#402914),(#402915,#402916,#402917)),.UNSPECIFIED.,.F.,
 .F.,.F.)
B_SPLINE_SURFACE_WITH_KNOTS((4,4),(3,3),(-3.39528393502487E-6,3.73481232852725E-5),
(-0.00165018033253464,1.),.UNSPECIFIED.)
GEOMETRIC_REPRESENTATION_ITEM()
RATIONAL_B_SPLINE_SURFACE(((1.00048354385544,0.853487571660502,1.),(1.00047110510899,
0.857256476851569,1.),(1.00053193201083,0.83882609665599,1.),(1.00063970687696,
0.806170615310237,1.)))
REPRESENTATION_ITEM('')
SURFACE()
);
#3080=(
BOUNDED_SURFACE()
B_SPLINE_SURFACE(3,2,((#402921,#402922,#402923),(#402924,#402925,#402926),
(#402927,#402928,#402929),(#402930,#402931,#402932)),.UNSPECIFIED.,.F.,
 .F.,.F.)
B_SPLINE_SURFACE_WITH_KNOTS((4,4),(3,3),(2.02993869230508E-5,5.39756952686905E-5),
(-0.000116281070005832,1.),.UNSPECIFIED.)
GEOMETRIC_REPRESENTATION_ITEM()
RATIONAL_B_SPLINE_SURFACE(((1.00001770479731,0.923870681143002,1.),(1.0000101410406,
0.956394275543423,1.),(1.0000203730028,0.912397594905659,1.),(1.00003390859471,
0.854195550869846,1.)))
REPRESENTATION_ITEM('')
SURFACE()
);
#3081=(
BOUNDED_SURFACE()
B_SPLINE_SURFACE(3,2,((#403025,#403026,#403027),(#403028,#403029,#403030),
(#403031,#403032,#403033),(#403034,#403035,#403036)),.UNSPECIFIED.,.F.,
 .F.,.F.)
B_SPLINE_SURFACE_WITH_KNOTS((4,4),(3,3),(0.00135801595889393,0.00148409170619832),
(0.,1.),.UNSPECIFIED.)
GEOMETRIC_REPRESENTATION_ITEM()
RATIONAL_B_SPLINE_SURFACE(((1.,0.818301933966442,1.),(1.,0.817226613172342,
1.),(1.,0.816179643373958,1.),(1.,0.815159387863653,1.)))
REPRESENTATION_ITEM('')
SURFACE()
);
#3082=(
BOUNDED_SURFACE()
B_SPLINE_SURFACE(3,2,((#403075,#403076,#403077),(#403078,#403079,#403080),
(#403081,#403082,#403083),(#403084,#403085,#403086)),.UNSPECIFIED.,.F.,
 .F.,.F.)
B_SPLINE_SURFACE_WITH_KNOTS((4,4),(3,3),(-1.54744435122088E-6,1.54744435122089E-5),
(-0.0151698983713734,1.),.UNSPECIFIED.)
GEOMETRIC_REPRESENTATION_ITEM()
RATIONAL_B_SPLINE_SURFACE(((1.02018382474206,0.334740937350499,1.),(1.00401234489073,
0.86775307281208,1.),(1.00033622856801,0.988917903080762,1.),(1.,1.,1.)))
REPRESENTATION_ITEM('')
SURFACE()
);
#3083=(
BOUNDED_SURFACE()
B_SPLINE_SURFACE(3,2,((#403088,#403089,#403090),(#403091,#403092,#403093),
(#403094,#403095,#403096),(#403097,#403098,#403099)),.UNSPECIFIED.,.F.,
 .F.,.F.)
B_SPLINE_SURFACE_WITH_KNOTS((4,4),(3,3),(0.00137194782501028,0.00149814269699235),
(0.,1.),.UNSPECIFIED.)
GEOMETRIC_REPRESENTATION_ITEM()
RATIONAL_B_SPLINE_SURFACE(((1.,0.815158509402318,1.),(1.,0.816179044148161,
1.),(1.,0.817226308119928,1.),(1.,0.818301939488811,1.)))
REPRESENTATION_ITEM('')
SURFACE()
);
#3084=(
BOUNDED_SURFACE()
B_SPLINE_SURFACE(3,2,((#403143,#403144,#403145),(#403146,#403147,#403148),
(#403149,#403150,#403151),(#403152,#403153,#403154)),.UNSPECIFIED.,.F.,
 .F.,.F.)
B_SPLINE_SURFACE_WITH_KNOTS((4,4),(3,3),(1.55009486301138E-5,4.92065510474435E-5),
(-8.13759517814764E-5,1.),.UNSPECIFIED.)
GEOMETRIC_REPRESENTATION_ITEM()
RATIONAL_B_SPLINE_SURFACE(((1.00002372912344,0.854200639599645,1.),(1.00001423585999,
0.91253030118051,1.),(1.00000710550473,0.956341495377427,1.),(1.00001238975913,
0.923873338136997,1.)))
REPRESENTATION_ITEM('')
SURFACE()
);
#3085=(
BOUNDED_SURFACE()
B_SPLINE_SURFACE(3,2,((#403158,#403159,#403160),(#403161,#403162,#403163),
(#403164,#403165,#403166),(#403167,#403168,#403169)),.UNSPECIFIED.,.F.,
 .F.,.F.)
B_SPLINE_SURFACE_WITH_KNOTS((4,4),(3,3),(-3.39934179457815E-6,3.73927597403564E-5),
(-0.00186004067386607,1.0006937331742),.UNSPECIFIED.)
GEOMETRIC_REPRESENTATION_ITEM()
RATIONAL_B_SPLINE_SURFACE(((1.00072100136042,0.806051963875458,1.00026859642683),
(1.00060048440144,0.838470803558717,1.0002236999449),(1.00053106448786,
0.857144632272456,1.00019783877214),(1.00054515072843,0.853355459539174,
1.00020308635431)))
REPRESENTATION_ITEM('')
SURFACE()
);
#3086=(
BOUNDED_SURFACE()
B_SPLINE_SURFACE(3,2,((#403171,#403172,#403173),(#403174,#403175,#403176),
(#403177,#403178,#403179),(#403180,#403181,#403182)),.UNSPECIFIED.,.F.,
 .F.,.F.)
B_SPLINE_SURFACE_WITH_KNOTS((4,4),(3,3),(0.,9.54361881492175E-5),(0.,1.),
 .UNSPECIFIED.)
GEOMETRIC_REPRESENTATION_ITEM()
RATIONAL_B_SPLINE_SURFACE(((1.,0.816715621142046,1.),(1.,0.815907587407946,
1.),(1.,0.8151159593452,1.),(1.,0.814339887349193,1.)))
REPRESENTATION_ITEM('')
SURFACE()
);
#3087=(
BOUNDED_SURFACE()
B_SPLINE_SURFACE(3,2,((#403184,#403185,#403186),(#403187,#403188,#403189),
(#403190,#403191,#403192),(#403193,#403194,#403195)),.UNSPECIFIED.,.F.,
 .F.,.F.)
B_SPLINE_SURFACE_WITH_KNOTS((4,4),(3,3),(1.15196480826585E-19,4.68197758448212E-5),
(0.,1.),.UNSPECIFIED.)
GEOMETRIC_REPRESENTATION_ITEM()
RATIONAL_B_SPLINE_SURFACE(((1.,0.816715621142048,1.),(1.,0.953638980025211,
1.),(1.,0.954506925408052,1.),(1.,0.816715621142046,1.)))
REPRESENTATION_ITEM('')
SURFACE()
);
#3088=(
BOUNDED_SURFACE()
B_SPLINE_SURFACE(3,2,((#403197,#403198,#403199),(#403200,#403201,#403202),
(#403203,#403204,#403205),(#403206,#403207,#403208)),.UNSPECIFIED.,.F.,
 .F.,.F.)
B_SPLINE_SURFACE_WITH_KNOTS((4,4),(3,3),(1.0842021724855E-19,9.54361881492177E-5),
(0.,1.),.UNSPECIFIED.)
GEOMETRIC_REPRESENTATION_ITEM()
RATIONAL_B_SPLINE_SURFACE(((1.,0.814339887349194,1.),(1.,0.815115959345202,
1.),(1.,0.815907587407943,1.),(1.,0.81671562114205,1.)))
REPRESENTATION_ITEM('')
SURFACE()
);
#3089=(
BOUNDED_SURFACE()
B_SPLINE_SURFACE(3,2,((#403210,#403211,#403212),(#403213,#403214,#403215),
(#403216,#403217,#403218),(#403219,#403220,#403221)),.UNSPECIFIED.,.F.,
 .F.,.F.)
B_SPLINE_SURFACE_WITH_KNOTS((4,4),(3,3),(-3.39528393502489E-6,3.73481232852738E-5),
(-0.00165018033274941,1.),.UNSPECIFIED.)
GEOMETRIC_REPRESENTATION_ITEM()
RATIONAL_B_SPLINE_SURFACE(((1.0004835438555,0.853487571660473,1.),(1.00047110510905,
0.857256476851541,1.),(1.0005319320109,0.838826096655956,1.),(1.00063970687705,
0.806170615310195,1.)))
REPRESENTATION_ITEM('')
SURFACE()
);
#3090=(
BOUNDED_SURFACE()
B_SPLINE_SURFACE(3,2,((#403225,#403226,#403227),(#403228,#403229,#403230),
(#403231,#403232,#403233),(#403234,#403235,#403236)),.UNSPECIFIED.,.F.,
 .F.,.F.)
B_SPLINE_SURFACE_WITH_KNOTS((4,4),(3,3),(2.02993869230509E-5,5.39756952686902E-5),
(-0.000116281069780791,1.),.UNSPECIFIED.)
GEOMETRIC_REPRESENTATION_ITEM()
RATIONAL_B_SPLINE_SURFACE(((1.00001770479728,0.923870681143022,1.),(1.00001014104058,
0.956394275543426,1.),(1.00002037300276,0.912397594905692,1.),(1.00003390859465,
0.854195550869869,1.)))
REPRESENTATION_ITEM('')
SURFACE()
);
#3091=(
BOUNDED_SURFACE()
B_SPLINE_SURFACE(3,2,((#403329,#403330,#403331),(#403332,#403333,#403334),
(#403335,#403336,#403337),(#403338,#403339,#403340)),.UNSPECIFIED.,.F.,
 .F.,.F.)
B_SPLINE_SURFACE_WITH_KNOTS((4,4),(3,3),(0.00135801595889393,0.00148409170619832),
(0.,1.),.UNSPECIFIED.)
GEOMETRIC_REPRESENTATION_ITEM()
RATIONAL_B_SPLINE_SURFACE(((1.,0.818301933966445,1.),(1.,0.817226613172349,
1.),(1.,0.816179643373942,1.),(1.,0.81515938786366,1.)))
REPRESENTATION_ITEM('')
SURFACE()
);
#3092=(
BOUNDED_SURFACE()
B_SPLINE_SURFACE(3,2,((#403379,#403380,#403381),(#403382,#403383,#403384),
(#403385,#403386,#403387),(#403388,#403389,#403390)),.UNSPECIFIED.,.F.,
 .F.,.F.)
B_SPLINE_SURFACE_WITH_KNOTS((4,4),(3,3),(-1.5474443512208E-6,1.54744435122077E-5),
(-0.0151698983618865,1.01516989836038),.UNSPECIFIED.)
GEOMETRIC_REPRESENTATION_ITEM()
RATIONAL_B_SPLINE_SURFACE(((1.02018382472925,0.324498219413554,1.02018382472721),
(1.00401234488819,0.865716921710617,1.00401234488778),(1.0003362285678,
0.988747276629687,1.00033622856777),(1.,1.,1.)))
REPRESENTATION_ITEM('')
SURFACE()
);
#3093=(
BOUNDED_SURFACE()
B_SPLINE_SURFACE(3,2,((#403392,#403393,#403394),(#403395,#403396,#403397),
(#403398,#403399,#403400),(#403401,#403402,#403403)),.UNSPECIFIED.,.F.,
 .F.,.F.)
B_SPLINE_SURFACE_WITH_KNOTS((4,4),(3,3),(0.00137194782501028,0.00149814269699235),
(0.,1.),.UNSPECIFIED.)
GEOMETRIC_REPRESENTATION_ITEM()
RATIONAL_B_SPLINE_SURFACE(((1.,0.815158509402316,1.),(1.,0.816179044148174,
1.),(1.,0.817226308119917,1.),(1.,0.818301939488799,1.)))
REPRESENTATION_ITEM('')
SURFACE()
);
#3094=(
BOUNDED_SURFACE()
B_SPLINE_SURFACE(3,2,((#403447,#403448,#403449),(#403450,#403451,#403452),
(#403453,#403454,#403455),(#403456,#403457,#403458)),.UNSPECIFIED.,.F.,
 .F.,.F.)
B_SPLINE_SURFACE_WITH_KNOTS((4,4),(3,3),(1.55009486301137E-5,4.92065510474433E-5),
(-8.13759517061083E-5,1.),.UNSPECIFIED.)
GEOMETRIC_REPRESENTATION_ITEM()
RATIONAL_B_SPLINE_SURFACE(((1.00002372912342,0.854200639599651,1.),(1.00001423585997,
0.912530301180521,1.),(1.00000710550473,0.956341495377419,1.),(1.00001238975912,
0.923873338137002,1.)))
REPRESENTATION_ITEM('')
SURFACE()
);
#3095=(
BOUNDED_SURFACE()
B_SPLINE_SURFACE(3,2,((#403462,#403463,#403464),(#403465,#403466,#403467),
(#403468,#403469,#403470),(#403471,#403472,#403473)),.UNSPECIFIED.,.F.,
 .F.,.F.)
B_SPLINE_SURFACE_WITH_KNOTS((4,4),(3,3),(-3.3993417945782E-6,3.73927597403566E-5),
(-0.00186004067396171,1.00069373317445),.UNSPECIFIED.)
GEOMETRIC_REPRESENTATION_ITEM()
RATIONAL_B_SPLINE_SURFACE(((1.00072100136046,0.80605196387537,1.00026859642693),
(1.00060048440147,0.8384708035587,1.00022369994497),(1.00053106448788,0.857144632272388,
1.00019783877221),(1.00054515072846,0.853355459539131,1.00020308635438)))
REPRESENTATION_ITEM('')
SURFACE()
);
#3096=(
BOUNDED_SURFACE()
B_SPLINE_SURFACE(3,2,((#403475,#403476,#403477),(#403478,#403479,#403480),
(#403481,#403482,#403483),(#403484,#403485,#403486)),.UNSPECIFIED.,.F.,
 .F.,.F.)
B_SPLINE_SURFACE_WITH_KNOTS((4,4),(3,3),(3.25260651745651E-19,9.54361881492175E-5),
(0.,1.),.UNSPECIFIED.)
GEOMETRIC_REPRESENTATION_ITEM()
RATIONAL_B_SPLINE_SURFACE(((1.,0.81671562114205,1.),(1.,0.815907587407942,
1.),(1.,0.815115959345214,1.),(1.,0.814339887349196,1.)))
REPRESENTATION_ITEM('')
SURFACE()
);
#3097=(
BOUNDED_SURFACE()
B_SPLINE_SURFACE(3,2,((#403488,#403489,#403490),(#403491,#403492,#403493),
(#403494,#403495,#403496),(#403497,#403498,#403499)),.UNSPECIFIED.,.F.,
 .F.,.F.)
B_SPLINE_SURFACE_WITH_KNOTS((4,4),(3,3),(1.8126505071242E-19,4.68197758448212E-5),
(0.,1.),.UNSPECIFIED.)
GEOMETRIC_REPRESENTATION_ITEM()
RATIONAL_B_SPLINE_SURFACE(((1.,0.816715621142049,1.),(1.,0.953638980025205,
1.),(1.,0.954506925408058,1.),(1.,0.816715621142051,1.)))
REPRESENTATION_ITEM('')
SURFACE()
);
#3098=(
BOUNDED_SURFACE()
B_SPLINE_SURFACE(3,2,((#403501,#403502,#403503),(#403504,#403505,#403506),
(#403507,#403508,#403509),(#403510,#403511,#403512)),.UNSPECIFIED.,.F.,
 .F.,.F.)
B_SPLINE_SURFACE_WITH_KNOTS((4,4),(3,3),(2.71050543121376E-19,9.54361881492178E-5),
(0.,1.),.UNSPECIFIED.)
GEOMETRIC_REPRESENTATION_ITEM()
RATIONAL_B_SPLINE_SURFACE(((1.,0.814339887349193,1.),(1.,0.815115959345211,
1.),(1.,0.815907587407943,1.),(1.,0.816715621142048,1.)))
REPRESENTATION_ITEM('')
SURFACE()
);
#3099=(
BOUNDED_SURFACE()
B_SPLINE_SURFACE(3,2,((#403514,#403515,#403516),(#403517,#403518,#403519),
(#403520,#403521,#403522),(#403523,#403524,#403525)),.UNSPECIFIED.,.F.,
 .F.,.F.)
B_SPLINE_SURFACE_WITH_KNOTS((4,4),(3,3),(-3.39528393502497E-6,3.73481232852735E-5),
(-0.00165018033334449,1.),.UNSPECIFIED.)
GEOMETRIC_REPRESENTATION_ITEM()
RATIONAL_B_SPLINE_SURFACE(((1.00048354385567,0.853487571660367,1.),(1.00047110510922,
0.857256476851486,1.),(1.00053193201109,0.838826096655839,1.),(1.00063970687728,
0.806170615310088,1.)))
REPRESENTATION_ITEM('')
SURFACE()
);
#3100=(
BOUNDED_SURFACE()
B_SPLINE_SURFACE(3,2,((#403529,#403530,#403531),(#403532,#403533,#403534),
(#403535,#403536,#403537),(#403538,#403539,#403540)),.UNSPECIFIED.,.F.,
 .F.,.F.)
B_SPLINE_SURFACE_WITH_KNOTS((4,4),(3,3),(2.0299386923051E-5,5.39756952686908E-5),
(-0.000116281069556606,1.),.UNSPECIFIED.)
GEOMETRIC_REPRESENTATION_ITEM()
RATIONAL_B_SPLINE_SURFACE(((1.00001770479724,0.923870681143038,1.),(1.00001014104056,
0.956394275543434,1.),(1.00002037300272,0.912397594905709,1.),(1.00003390859458,
0.854195550869906,1.)))
REPRESENTATION_ITEM('')
SURFACE()
);
#3101=(
BOUNDED_SURFACE()
B_SPLINE_SURFACE(3,2,((#403633,#403634,#403635),(#403636,#403637,#403638),
(#403639,#403640,#403641),(#403642,#403643,#403644)),.UNSPECIFIED.,.F.,
 .F.,.F.)
B_SPLINE_SURFACE_WITH_KNOTS((4,4),(3,3),(0.00135801595889393,0.00148409170619832),
(0.,1.),.UNSPECIFIED.)
GEOMETRIC_REPRESENTATION_ITEM()
RATIONAL_B_SPLINE_SURFACE(((1.,0.818301933966442,1.),(1.,0.817226613172335,
1.),(1.,0.816179643373966,1.),(1.,0.815159387863648,1.)))
REPRESENTATION_ITEM('')
SURFACE()
);
#3102=(
BOUNDED_SURFACE()
B_SPLINE_SURFACE(3,2,((#403683,#403684,#403685),(#403686,#403687,#403688),
(#403689,#403690,#403691),(#403692,#403693,#403694)),.UNSPECIFIED.,.F.,
 .F.,.F.)
B_SPLINE_SURFACE_WITH_KNOTS((4,4),(3,3),(-1.54744435122071E-6,1.54744435122068E-5),
(-0.0151698983644995,1.01516989835826),.UNSPECIFIED.)
GEOMETRIC_REPRESENTATION_ITEM()
RATIONAL_B_SPLINE_SURFACE(((1.02018382473277,0.32449821941328,1.02018382472435),
(1.00401234488889,0.865716921710489,1.00401234488721),(1.00033622856786,
0.988747276629715,1.00033622856772),(1.,1.,1.)))
REPRESENTATION_ITEM('')
SURFACE()
);
#3103=(
BOUNDED_SURFACE()
B_SPLINE_SURFACE(3,2,((#403696,#403697,#403698),(#403699,#403700,#403701),
(#403702,#403703,#403704),(#403705,#403706,#403707)),.UNSPECIFIED.,.F.,
 .F.,.F.)
B_SPLINE_SURFACE_WITH_KNOTS((4,4),(3,3),(0.00137194782501028,0.00149814269699235),
(0.,1.),.UNSPECIFIED.)
GEOMETRIC_REPRESENTATION_ITEM()
RATIONAL_B_SPLINE_SURFACE(((1.,0.815158509402313,1.),(1.,0.816179044148176,
1.),(1.,0.817226308119907,1.),(1.,0.818301939488817,1.)))
REPRESENTATION_ITEM('')
SURFACE()
);
#3104=(
BOUNDED_SURFACE()
B_SPLINE_SURFACE(3,2,((#403751,#403752,#403753),(#403754,#403755,#403756),
(#403757,#403758,#403759),(#403760,#403761,#403762)),.UNSPECIFIED.,.F.,
 .F.,.F.)
B_SPLINE_SURFACE_WITH_KNOTS((4,4),(3,3),(1.55009486301137E-5,4.92065510474431E-5),
(-8.13759512659326E-5,1.),.UNSPECIFIED.)
GEOMETRIC_REPRESENTATION_ITEM()
RATIONAL_B_SPLINE_SURFACE(((1.00002372912329,0.854200639599712,1.),(1.0000142358599,
0.912530301180562,1.),(1.00000710550469,0.95634149537744,1.),(1.00001238975905,
0.923873338137042,1.)))
REPRESENTATION_ITEM('')
SURFACE()
);
#3105=(
BOUNDED_SURFACE()
B_SPLINE_SURFACE(3,2,((#403766,#403767,#403768),(#403769,#403770,#403771),
(#403772,#403773,#403774),(#403775,#403776,#403777)),.UNSPECIFIED.,.F.,
 .F.,.F.)
B_SPLINE_SURFACE_WITH_KNOTS((4,4),(3,3),(-3.3993417945782E-6,3.73927597403566E-5),
(-0.00186004067380188,1.00069373317431),.UNSPECIFIED.)
GEOMETRIC_REPRESENTATION_ITEM()
RATIONAL_B_SPLINE_SURFACE(((1.0007210013604,0.806051963875434,1.00026859642688),
(1.00060048440142,0.838470803558721,1.00022369994493),(1.00053106448784,
0.857144632272437,1.00019783877217),(1.00054515072841,0.853355459539169,
1.00020308635434)))
REPRESENTATION_ITEM('')
SURFACE()
);
#3106=(
BOUNDED_SURFACE()
B_SPLINE_SURFACE(3,2,((#403779,#403780,#403781),(#403782,#403783,#403784),
(#403785,#403786,#403787),(#403788,#403789,#403790)),.UNSPECIFIED.,.F.,
 .F.,.F.)
B_SPLINE_SURFACE_WITH_KNOTS((4,4),(3,3),(-5.42101086242752E-20,9.54361881492174E-5),
(0.,1.),.UNSPECIFIED.)
GEOMETRIC_REPRESENTATION_ITEM()
RATIONAL_B_SPLINE_SURFACE(((1.,0.816715621142048,1.),(1.,0.815907587407946,
1.),(1.,0.815115959345197,1.),(1.,0.814339887349194,1.)))
REPRESENTATION_ITEM('')
SURFACE()
);
#3107=(
BOUNDED_SURFACE()
B_SPLINE_SURFACE(3,2,((#403792,#403793,#403794),(#403795,#403796,#403797),
(#403798,#403799,#403800),(#403801,#403802,#403803)),.UNSPECIFIED.,.F.,
 .F.,.F.)
B_SPLINE_SURFACE_WITH_KNOTS((4,4),(3,3),(-1.79570984817912E-19,4.6819775844821E-5),
(0.,1.),.UNSPECIFIED.)
GEOMETRIC_REPRESENTATION_ITEM()
RATIONAL_B_SPLINE_SURFACE(((1.,0.816715621142045,1.),(1.,0.953638980025212,
1.),(1.,0.954506925408055,1.),(1.,0.816715621142048,1.)))
REPRESENTATION_ITEM('')
SURFACE()
);
#3108=(
BOUNDED_SURFACE()
B_SPLINE_SURFACE(3,2,((#403805,#403806,#403807),(#403808,#403809,#403810),
(#403811,#403812,#403813),(#403814,#403815,#403816)),.UNSPECIFIED.,.F.,
 .F.,.F.)
B_SPLINE_SURFACE_WITH_KNOTS((4,4),(3,3),(-1.0842021724855E-19,9.54361881492175E-5),
(0.,1.),.UNSPECIFIED.)
GEOMETRIC_REPRESENTATION_ITEM()
RATIONAL_B_SPLINE_SURFACE(((1.,0.814339887349193,1.),(1.,0.815115959345213,
1.),(1.,0.815907587407938,1.),(1.,0.816715621142047,1.)))
REPRESENTATION_ITEM('')
SURFACE()
);
#3109=(
BOUNDED_SURFACE()
B_SPLINE_SURFACE(3,2,((#403818,#403819,#403820),(#403821,#403822,#403823),
(#403824,#403825,#403826),(#403827,#403828,#403829)),.UNSPECIFIED.,.F.,
 .F.,.F.)
B_SPLINE_SURFACE_WITH_KNOTS((4,4),(3,3),(-3.39528393502377E-6,3.73481232852734E-5),
(-0.00165018033347931,1.),.UNSPECIFIED.)
GEOMETRIC_REPRESENTATION_ITEM()
RATIONAL_B_SPLINE_SURFACE(((1.00048354385571,0.853487571660351,1.),(1.00047110510926,
0.857256476851438,1.),(1.00053193201114,0.838826096655829,1.),(1.00063970687733,
0.806170615310052,1.)))
REPRESENTATION_ITEM('')
SURFACE()
);
#3110=(
BOUNDED_SURFACE()
B_SPLINE_SURFACE(3,2,((#403833,#403834,#403835),(#403836,#403837,#403838),
(#403839,#403840,#403841),(#403842,#403843,#403844)),.UNSPECIFIED.,.F.,
 .F.,.F.)
B_SPLINE_SURFACE_WITH_KNOTS((4,4),(3,3),(2.02993869230509E-5,5.39756952687133E-5),
(-0.000116281070048236,1.),.UNSPECIFIED.)
GEOMETRIC_REPRESENTATION_ITEM()
RATIONAL_B_SPLINE_SURFACE(((1.00001770479732,0.923870681142996,1.),(1.0000101410406,
0.95639427554344,1.),(1.00002037300281,0.912397594905617,1.),(1.00003390859473,
0.854195550869708,1.)))
REPRESENTATION_ITEM('')
SURFACE()
);
#3111=(
BOUNDED_SURFACE()
B_SPLINE_SURFACE(3,2,((#403937,#403938,#403939),(#403940,#403941,#403942),
(#403943,#403944,#403945),(#403946,#403947,#403948)),.UNSPECIFIED.,.F.,
 .F.,.F.)
B_SPLINE_SURFACE_WITH_KNOTS((4,4),(3,3),(0.00135801595889393,0.00148409170619832),
(0.,1.),.UNSPECIFIED.)
GEOMETRIC_REPRESENTATION_ITEM()
RATIONAL_B_SPLINE_SURFACE(((1.,0.818301933966445,1.),(1.,0.817226613172346,
1.),(1.,0.81617964337396,1.),(1.,0.815159387863655,1.)))
REPRESENTATION_ITEM('')
SURFACE()
);
#3112=(
BOUNDED_SURFACE()
B_SPLINE_SURFACE(3,2,((#403987,#403988,#403989),(#403990,#403991,#403992),
(#403993,#403994,#403995),(#403996,#403997,#403998)),.UNSPECIFIED.,.F.,
 .F.,.F.)
B_SPLINE_SURFACE_WITH_KNOTS((4,4),(3,3),(-1.54744435122081E-6,1.54744435122075E-5),
(-0.015169898363464,1.0151698983591),.UNSPECIFIED.)
GEOMETRIC_REPRESENTATION_ITEM()
RATIONAL_B_SPLINE_SURFACE(((1.02018382473138,0.324498219413331,1.02018382472549),
(1.00401234488861,0.865716921710593,1.00401234488744),(1.00033622856784,
0.988747276629696,1.00033622856774),(1.,1.,1.)))
REPRESENTATION_ITEM('')
SURFACE()
);
#3113=(
BOUNDED_SURFACE()
B_SPLINE_SURFACE(3,2,((#404000,#404001,#404002),(#404003,#404004,#404005),
(#404006,#404007,#404008),(#404009,#404010,#404011)),.UNSPECIFIED.,.F.,
 .F.,.F.)
B_SPLINE_SURFACE_WITH_KNOTS((4,4),(3,3),(0.00137194782501028,0.00149814269699235),
(0.,1.),.UNSPECIFIED.)
GEOMETRIC_REPRESENTATION_ITEM()
RATIONAL_B_SPLINE_SURFACE(((1.,0.815158509402319,1.),(1.,0.816179044148164,
1.),(1.,0.817226308119929,1.),(1.,0.818301939488808,1.)))
REPRESENTATION_ITEM('')
SURFACE()
);
#3114=(
BOUNDED_SURFACE()
B_SPLINE_SURFACE(3,2,((#404055,#404056,#404057),(#404058,#404059,#404060),
(#404061,#404062,#404063),(#404064,#404065,#404066)),.UNSPECIFIED.,.F.,
 .F.,.F.)
B_SPLINE_SURFACE_WITH_KNOTS((4,4),(3,3),(1.55009486301137E-5,4.9206551047443E-5),
(-8.13759512613473E-5,1.),.UNSPECIFIED.)
GEOMETRIC_REPRESENTATION_ITEM()
RATIONAL_B_SPLINE_SURFACE(((1.00002372912329,0.854200639599707,1.),(1.0000142358599,
0.912530301180568,1.),(1.00000710550469,0.956341495377435,1.),(1.00001238975905,
0.923873338137041,1.)))
REPRESENTATION_ITEM('')
SURFACE()
);
#3115=(
BOUNDED_SURFACE()
B_SPLINE_SURFACE(3,2,((#404070,#404071,#404072),(#404073,#404074,#404075),
(#404076,#404077,#404078),(#404079,#404080,#404081)),.UNSPECIFIED.,.F.,
 .F.,.F.)
B_SPLINE_SURFACE_WITH_KNOTS((4,4),(3,3),(-3.39934179457856E-6,3.73927597403564E-5),
(-0.0018600406739503,1.0006937331742),.UNSPECIFIED.)
GEOMETRIC_REPRESENTATION_ITEM()
RATIONAL_B_SPLINE_SURFACE(((1.00072100136045,0.806051963875425,1.00026859642683),
(1.00060048440146,0.838470803558715,1.0002236999449),(1.00053106448788,
0.857144632272439,1.00019783877214),(1.00054515072845,0.853355459539172,
1.00020308635431)))
REPRESENTATION_ITEM('')
SURFACE()
);
#3116=(
BOUNDED_SURFACE()
B_SPLINE_SURFACE(3,2,((#404083,#404084,#404085),(#404086,#404087,#404088),
(#404089,#404090,#404091),(#404092,#404093,#404094)),.UNSPECIFIED.,.F.,
 .F.,.F.)
B_SPLINE_SURFACE_WITH_KNOTS((4,4),(3,3),(1.62630325872826E-19,9.54361881492171E-5),
(0.,1.),.UNSPECIFIED.)
GEOMETRIC_REPRESENTATION_ITEM()
RATIONAL_B_SPLINE_SURFACE(((1.,0.816715621142057,1.),(1.,0.815907587407945,
1.),(1.,0.815115959345199,1.),(1.,0.814339887349194,1.)))
REPRESENTATION_ITEM('')
SURFACE()
);
#3117=(
BOUNDED_SURFACE()
B_SPLINE_SURFACE(3,2,((#404096,#404097,#404098),(#404099,#404100,#404101),
(#404102,#404103,#404104),(#404105,#404106,#404107)),.UNSPECIFIED.,.F.,
 .F.,.F.)
B_SPLINE_SURFACE_WITH_KNOTS((4,4),(3,3),(-2.5410988417629E-20,4.68197758448212E-5),
(0.,1.),.UNSPECIFIED.)
GEOMETRIC_REPRESENTATION_ITEM()
RATIONAL_B_SPLINE_SURFACE(((1.,0.81671562114206,1.),(1.,0.953638980025189,
1.),(1.,0.954506925408053,1.),(1.,0.816715621142049,1.)))
REPRESENTATION_ITEM('')
SURFACE()
);
#3118=(
BOUNDED_SURFACE()
B_SPLINE_SURFACE(3,2,((#404109,#404110,#404111),(#404112,#404113,#404114),
(#404115,#404116,#404117),(#404118,#404119,#404120)),.UNSPECIFIED.,.F.,
 .F.,.F.)
B_SPLINE_SURFACE_WITH_KNOTS((4,4),(3,3),(0.,9.54361881492177E-5),(0.,1.),
 .UNSPECIFIED.)
GEOMETRIC_REPRESENTATION_ITEM()
RATIONAL_B_SPLINE_SURFACE(((1.,0.814339887349206,1.),(1.,0.815115959345194,
1.),(1.,0.815907587407949,1.),(1.,0.816715621142061,1.)))
REPRESENTATION_ITEM('')
SURFACE()
);
#3119=(
BOUNDED_SURFACE()
B_SPLINE_SURFACE(3,2,((#404122,#404123,#404124),(#404125,#404126,#404127),
(#404128,#404129,#404130),(#404131,#404132,#404133)),.UNSPECIFIED.,.F.,
 .F.,.F.)
B_SPLINE_SURFACE_WITH_KNOTS((4,4),(3,3),(-3.39528393502479E-6,3.73481232852728E-5),
(-0.0016501803332698,1.),.UNSPECIFIED.)
GEOMETRIC_REPRESENTATION_ITEM()
RATIONAL_B_SPLINE_SURFACE(((1.00048354385565,0.853487571660401,1.),(1.0004711051092,
0.857256476851457,1.),(1.00053193201107,0.83882609665588,1.),(1.00063970687725,
0.806170615310097,1.)))
REPRESENTATION_ITEM('')
SURFACE()
);
#3120=(
BOUNDED_SURFACE()
B_SPLINE_SURFACE(3,2,((#404137,#404138,#404139),(#404140,#404141,#404142),
(#404143,#404144,#404145),(#404146,#404147,#404148)),.UNSPECIFIED.,.F.,
 .F.,.F.)
B_SPLINE_SURFACE_WITH_KNOTS((4,4),(3,3),(2.0299386923051E-5,5.39756952687124E-5),
(-0.000116281069954705,1.),.UNSPECIFIED.)
GEOMETRIC_REPRESENTATION_ITEM()
RATIONAL_B_SPLINE_SURFACE(((1.0000177047973,0.923870681143004,1.),(1.00001014104059,
0.956394275543448,1.),(1.00002037300279,0.912397594905612,1.),(1.0000339085947,
0.854195550869733,1.)))
REPRESENTATION_ITEM('')
SURFACE()
);
#3121=(
BOUNDED_SURFACE()
B_SPLINE_SURFACE(3,2,((#404241,#404242,#404243),(#404244,#404245,#404246),
(#404247,#404248,#404249),(#404250,#404251,#404252)),.UNSPECIFIED.,.F.,
 .F.,.F.)
B_SPLINE_SURFACE_WITH_KNOTS((4,4),(3,3),(0.00135801595889393,0.00148409170619832),
(0.,1.),.UNSPECIFIED.)
GEOMETRIC_REPRESENTATION_ITEM()
RATIONAL_B_SPLINE_SURFACE(((1.,0.818301933966446,1.),(1.,0.817226613172337,
1.),(1.,0.816179643373957,1.),(1.,0.815159387863657,1.)))
REPRESENTATION_ITEM('')
SURFACE()
);
#3122=(
BOUNDED_SURFACE()
B_SPLINE_SURFACE(3,2,((#404291,#404292,#404293),(#404294,#404295,#404296),
(#404297,#404298,#404299),(#404300,#404301,#404302)),.UNSPECIFIED.,.F.,
 .F.,.F.)
B_SPLINE_SURFACE_WITH_KNOTS((4,4),(3,3),(-1.54744435122086E-6,1.54744435122091E-5),
(-0.0151698983689157,1.0151698983533),.UNSPECIFIED.)
GEOMETRIC_REPRESENTATION_ITEM()
RATIONAL_B_SPLINE_SURFACE(((1.02018382473874,0.324498219413532,1.02018382471765),
(1.00401234489008,0.865716921710509,1.00401234488588),(1.00033622856796,
0.988747276629715,1.00033622856761),(1.,1.,1.)))
REPRESENTATION_ITEM('')
SURFACE()
);
#3123=(
BOUNDED_SURFACE()
B_SPLINE_SURFACE(3,2,((#404304,#404305,#404306),(#404307,#404308,#404309),
(#404310,#404311,#404312),(#404313,#404314,#404315)),.UNSPECIFIED.,.F.,
 .F.,.F.)
B_SPLINE_SURFACE_WITH_KNOTS((4,4),(3,3),(0.00137194782501028,0.00149814269699235),
(0.,1.),.UNSPECIFIED.)
GEOMETRIC_REPRESENTATION_ITEM()
RATIONAL_B_SPLINE_SURFACE(((1.,0.815158509402316,1.),(1.,0.816179044148173,
1.),(1.,0.81722630811992,1.),(1.,0.818301939488806,1.)))
REPRESENTATION_ITEM('')
SURFACE()
);
#3124=(
BOUNDED_SURFACE()
B_SPLINE_SURFACE(3,2,((#404359,#404360,#404361),(#404362,#404363,#404364),
(#404365,#404366,#404367),(#404368,#404369,#404370)),.UNSPECIFIED.,.F.,
 .F.,.F.)
B_SPLINE_SURFACE_WITH_KNOTS((4,4),(3,3),(1.55009486301137E-5,4.92065510474437E-5),
(-8.13759512178582E-5,1.),.UNSPECIFIED.)
GEOMETRIC_REPRESENTATION_ITEM()
RATIONAL_B_SPLINE_SURFACE(((1.00002372912328,0.854200639599716,1.),(1.00001423585989,
0.912530301180565,1.),(1.00000710550468,0.956341495377443,1.),(1.00001238975904,
0.923873338137041,1.)))
REPRESENTATION_ITEM('')
SURFACE()
);
#3125=(
BOUNDED_SURFACE()
B_SPLINE_SURFACE(3,2,((#404374,#404375,#404376),(#404377,#404378,#404379),
(#404380,#404381,#404382),(#404383,#404384,#404385)),.UNSPECIFIED.,.F.,
 .F.,.F.)
B_SPLINE_SURFACE_WITH_KNOTS((4,4),(3,3),(-3.3993417945784E-6,3.73927597403564E-5),
(-0.00186004067426403,1.0006937331744),.UNSPECIFIED.)
GEOMETRIC_REPRESENTATION_ITEM()
RATIONAL_B_SPLINE_SURFACE(((1.00072100136058,0.806051963875325,1.00026859642691),
(1.00060048440156,0.838470803558652,1.00022369994496),(1.00053106448797,
0.85714463227235,1.00019783877219),(1.00054515072855,0.853355459539107,
1.00020308635437)))
REPRESENTATION_ITEM('')
SURFACE()
);
#3126=(
BOUNDED_SURFACE()
B_SPLINE_SURFACE(3,2,((#404387,#404388,#404389),(#404390,#404391,#404392),
(#404393,#404394,#404395),(#404396,#404397,#404398)),.UNSPECIFIED.,.F.,
 .F.,.F.)
B_SPLINE_SURFACE_WITH_KNOTS((4,4),(3,3),(1.0842021724855E-19,9.54361881492173E-5),
(0.,1.),.UNSPECIFIED.)
GEOMETRIC_REPRESENTATION_ITEM()
RATIONAL_B_SPLINE_SURFACE(((1.,0.816715621142061,1.),(1.,0.815907587407937,
1.),(1.,0.815115959345211,1.),(1.,0.814339887349197,1.)))
REPRESENTATION_ITEM('')
SURFACE()
);
#3127=(
BOUNDED_SURFACE()
B_SPLINE_SURFACE(3,2,((#404400,#404401,#404402),(#404403,#404404,#404405),
(#404406,#404407,#404408),(#404409,#404410,#404411)),.UNSPECIFIED.,.F.,
 .F.,.F.)
B_SPLINE_SURFACE_WITH_KNOTS((4,4),(3,3),(6.7762635780344E-20,4.6819775844821E-5),
(0.,1.),.UNSPECIFIED.)
GEOMETRIC_REPRESENTATION_ITEM()
RATIONAL_B_SPLINE_SURFACE(((1.,0.816715621142037,1.),(1.,0.953638980025224,
1.),(1.,0.954506925408043,1.),(1.,0.816715621142053,1.)))
REPRESENTATION_ITEM('')
SURFACE()
);
#3128=(
BOUNDED_SURFACE()
B_SPLINE_SURFACE(3,2,((#404413,#404414,#404415),(#404416,#404417,#404418),
(#404419,#404420,#404421),(#404422,#404423,#404424)),.UNSPECIFIED.,.F.,
 .F.,.F.)
B_SPLINE_SURFACE_WITH_KNOTS((4,4),(3,3),(-2.16840434497101E-19,9.54361881492175E-5),
(0.,1.),.UNSPECIFIED.)
GEOMETRIC_REPRESENTATION_ITEM()
RATIONAL_B_SPLINE_SURFACE(((1.,0.814339887349194,1.),(1.,0.815115959345198,
1.),(1.,0.815907587407953,1.),(1.,0.816715621142038,1.)))
REPRESENTATION_ITEM('')
SURFACE()
);
#3129=(
BOUNDED_SURFACE()
B_SPLINE_SURFACE(3,2,((#404426,#404427,#404428),(#404429,#404430,#404431),
(#404432,#404433,#404434),(#404435,#404436,#404437)),.UNSPECIFIED.,.F.,
 .F.,.F.)
B_SPLINE_SURFACE_WITH_KNOTS((4,4),(3,3),(-3.39528393502481E-6,3.73481232852735E-5),
(-0.00165018033338635,1.),.UNSPECIFIED.)
GEOMETRIC_REPRESENTATION_ITEM()
RATIONAL_B_SPLINE_SURFACE(((1.00048354385569,0.853487571660377,1.),(1.00047110510924,
0.857256476851453,1.),(1.00053193201111,0.838826096655834,1.),(1.0006397068773,
0.806170615310088,1.)))
REPRESENTATION_ITEM('')
SURFACE()
);
#3130=(
BOUNDED_SURFACE()
B_SPLINE_SURFACE(3,2,((#404441,#404442,#404443),(#404444,#404445,#404446),
(#404447,#404448,#404449),(#404450,#404451,#404452)),.UNSPECIFIED.,.F.,
 .F.,.F.)
B_SPLINE_SURFACE_WITH_KNOTS((4,4),(3,3),(2.0299386923051E-5,5.39756952687122E-5),
(-0.000116281070054044,1.),.UNSPECIFIED.)
GEOMETRIC_REPRESENTATION_ITEM()
RATIONAL_B_SPLINE_SURFACE(((1.00001770479732,0.923870681142996,1.),(1.0000101410406,
0.956394275543441,1.),(1.00002037300281,0.912397594905597,1.),(1.00003390859473,
0.854195550869718,1.)))
REPRESENTATION_ITEM('')
SURFACE()
);
#3131=(
BOUNDED_SURFACE()
B_SPLINE_SURFACE(3,2,((#404545,#404546,#404547),(#404548,#404549,#404550),
(#404551,#404552,#404553),(#404554,#404555,#404556)),.UNSPECIFIED.,.F.,
 .F.,.F.)
B_SPLINE_SURFACE_WITH_KNOTS((4,4),(3,3),(0.00135801595889393,0.00148409170619832),
(0.,1.),.UNSPECIFIED.)
GEOMETRIC_REPRESENTATION_ITEM()
RATIONAL_B_SPLINE_SURFACE(((1.,0.818301933966443,1.),(1.,0.817226613172337,
1.),(1.,0.816179643373948,1.),(1.,0.815159387863655,1.)))
REPRESENTATION_ITEM('')
SURFACE()
);
#3132=(
BOUNDED_SURFACE()
B_SPLINE_SURFACE(3,2,((#404595,#404596,#404597),(#404598,#404599,#404600),
(#404601,#404602,#404603),(#404604,#404605,#404606)),.UNSPECIFIED.,.F.,
 .F.,.F.)
B_SPLINE_SURFACE_WITH_KNOTS((4,4),(3,3),(-1.54744435122076E-6,1.54744435122076E-5),
(-0.0151698983610561,1.),.UNSPECIFIED.)
GEOMETRIC_REPRESENTATION_ITEM()
RATIONAL_B_SPLINE_SURFACE(((1.02018382472812,0.334740937357287,1.),(1.00401234488797,
0.867753072813418,1.),(1.00033622856778,0.988917903080862,1.),(1.,1.,1.)))
REPRESENTATION_ITEM('')
SURFACE()
);
#3133=(
BOUNDED_SURFACE()
B_SPLINE_SURFACE(3,2,((#404608,#404609,#404610),(#404611,#404612,#404613),
(#404614,#404615,#404616),(#404617,#404618,#404619)),.UNSPECIFIED.,.F.,
 .F.,.F.)
B_SPLINE_SURFACE_WITH_KNOTS((4,4),(3,3),(0.00137194782501028,0.00149814269699235),
(0.,1.),.UNSPECIFIED.)
GEOMETRIC_REPRESENTATION_ITEM()
RATIONAL_B_SPLINE_SURFACE(((1.,0.815158509402307,1.),(1.,0.816179044148172,
1.),(1.,0.817226308119919,1.),(1.,0.818301939488809,1.)))
REPRESENTATION_ITEM('')
SURFACE()
);
#3134=(
BOUNDED_SURFACE()
B_SPLINE_SURFACE(3,2,((#404663,#404664,#404665),(#404666,#404667,#404668),
(#404669,#404670,#404671),(#404672,#404673,#404674)),.UNSPECIFIED.,.F.,
 .F.,.F.)
B_SPLINE_SURFACE_WITH_KNOTS((4,4),(3,3),(1.55009486301137E-5,4.92065510474431E-5),
(-8.13759512799104E-5,1.),.UNSPECIFIED.)
GEOMETRIC_REPRESENTATION_ITEM()
RATIONAL_B_SPLINE_SURFACE(((1.0000237291233,0.854200639599719,1.),(1.0000142358599,
0.912530301180548,1.),(1.00000710550469,0.956341495377441,1.),(1.00001238975905,
0.923873338137039,1.)))
REPRESENTATION_ITEM('')
SURFACE()
);
#3135=(
BOUNDED_SURFACE()
B_SPLINE_SURFACE(3,2,((#404678,#404679,#404680),(#404681,#404682,#404683),
(#404684,#404685,#404686),(#404687,#404688,#404689)),.UNSPECIFIED.,.F.,
 .F.,.F.)
B_SPLINE_SURFACE_WITH_KNOTS((4,4),(3,3),(-3.39934179457821E-6,3.73927597403565E-5),
(-0.00186004067423112,1.00069373317435),.UNSPECIFIED.)
GEOMETRIC_REPRESENTATION_ITEM()
RATIONAL_B_SPLINE_SURFACE(((1.00072100136056,0.806051963875339,1.00026859642689),
(1.00060048440155,0.83847080355866,1.00022369994494),(1.00053106448796,
0.857144632272363,1.00019783877218),(1.00054515072854,0.853355459539103,
1.00020308635435)))
REPRESENTATION_ITEM('')
SURFACE()
);
#3136=(
BOUNDED_SURFACE()
B_SPLINE_SURFACE(3,2,((#404691,#404692,#404693),(#404694,#404695,#404696),
(#404697,#404698,#404699),(#404700,#404701,#404702)),.UNSPECIFIED.,.F.,
 .F.,.F.)
B_SPLINE_SURFACE_WITH_KNOTS((4,4),(3,3),(0.,9.54361881492174E-5),(0.,1.),
 .UNSPECIFIED.)
GEOMETRIC_REPRESENTATION_ITEM()
RATIONAL_B_SPLINE_SURFACE(((1.,0.816715621142057,1.),(1.,0.815907587407932,
1.),(1.,0.81511595934521,1.),(1.,0.814339887349193,1.)))
REPRESENTATION_ITEM('')
SURFACE()
);
#3137=(
BOUNDED_SURFACE()
B_SPLINE_SURFACE(3,2,((#404704,#404705,#404706),(#404707,#404708,#404709),
(#404710,#404711,#404712),(#404713,#404714,#404715)),.UNSPECIFIED.,.F.,
 .F.,.F.)
B_SPLINE_SURFACE_WITH_KNOTS((4,4),(3,3),(0.,4.68197758448209E-5),(0.,1.),
 .UNSPECIFIED.)
GEOMETRIC_REPRESENTATION_ITEM()
RATIONAL_B_SPLINE_SURFACE(((1.,0.816715621142057,1.),(1.,0.953638980025206,
1.),(1.,0.954506925408047,1.),(1.,0.816715621142055,1.)))
REPRESENTATION_ITEM('')
SURFACE()
);
#3138=(
BOUNDED_SURFACE()
B_SPLINE_SURFACE(3,2,((#404717,#404718,#404719),(#404720,#404721,#404722),
(#404723,#404724,#404725),(#404726,#404727,#404728)),.UNSPECIFIED.,.F.,
 .F.,.F.)
B_SPLINE_SURFACE_WITH_KNOTS((4,4),(3,3),(0.,9.54361881492177E-5),(0.,1.),
 .UNSPECIFIED.)
GEOMETRIC_REPRESENTATION_ITEM()
RATIONAL_B_SPLINE_SURFACE(((1.,0.814339887349193,1.),(1.,0.815115959345207,
1.),(1.,0.815907587407933,1.),(1.,0.816715621142057,1.)))
REPRESENTATION_ITEM('')
SURFACE()
);
#3139=(
BOUNDED_SURFACE()
B_SPLINE_SURFACE(3,2,((#404730,#404731,#404732),(#404733,#404734,#404735),
(#404736,#404737,#404738),(#404739,#404740,#404741)),.UNSPECIFIED.,.F.,
 .F.,.F.)
B_SPLINE_SURFACE_WITH_KNOTS((4,4),(3,3),(-3.39528393502487E-6,3.73481232852736E-5),
(-0.00165018033284231,1.),.UNSPECIFIED.)
GEOMETRIC_REPRESENTATION_ITEM()
RATIONAL_B_SPLINE_SURFACE(((1.00048354385553,0.853487571660461,1.),(1.00047110510908,
0.857256476851525,1.),(1.00053193201093,0.83882609665593,1.),(1.00063970687708,
0.806170615310182,1.)))
REPRESENTATION_ITEM('')
SURFACE()
);
#3140=(
BOUNDED_SURFACE()
B_SPLINE_SURFACE(3,2,((#404745,#404746,#404747),(#404748,#404749,#404750),
(#404751,#404752,#404753),(#404754,#404755,#404756)),.UNSPECIFIED.,.F.,
 .F.,.F.)
B_SPLINE_SURFACE_WITH_KNOTS((4,4),(3,3),(2.02993869230509E-5,5.39756952686906E-5),
(-0.000116281069559425,1.),.UNSPECIFIED.)
GEOMETRIC_REPRESENTATION_ITEM()
RATIONAL_B_SPLINE_SURFACE(((1.00001770479724,0.923870681143036,1.),(1.00001014104056,
0.956394275543435,1.),(1.00002037300272,0.912397594905716,1.),(1.00003390859458,
0.854195550869901,1.)))
REPRESENTATION_ITEM('')
SURFACE()
);
#3141=(
BOUNDED_SURFACE()
B_SPLINE_SURFACE(3,2,((#404849,#404850,#404851),(#404852,#404853,#404854),
(#404855,#404856,#404857),(#404858,#404859,#404860)),.UNSPECIFIED.,.F.,
 .F.,.F.)
B_SPLINE_SURFACE_WITH_KNOTS((4,4),(3,3),(0.00135801595889393,0.00148409170619832),
(0.,1.),.UNSPECIFIED.)
GEOMETRIC_REPRESENTATION_ITEM()
RATIONAL_B_SPLINE_SURFACE(((1.,0.818301933966444,1.),(1.,0.817226613172348,
1.),(1.,0.816179643373956,1.),(1.,0.815159387863656,1.)))
REPRESENTATION_ITEM('')
SURFACE()
);
#3142=(
BOUNDED_SURFACE()
B_SPLINE_SURFACE(3,2,((#404899,#404900,#404901),(#404902,#404903,#404904),
(#404905,#404906,#404907),(#404908,#404909,#404910)),.UNSPECIFIED.,.F.,
 .F.,.F.)
B_SPLINE_SURFACE_WITH_KNOTS((4,4),(3,3),(4.06575814682064E-20,1.54744435122071E-5),
(0.,1.),.UNSPECIFIED.)
GEOMETRIC_REPRESENTATION_ITEM()
RATIONAL_B_SPLINE_SURFACE(((1.,0.478041569704941,1.),(1.,0.890533857552089,
1.),(1.,0.990075913815898,1.),(1.,1.,1.)))
REPRESENTATION_ITEM('')
SURFACE()
);
#3143=(
BOUNDED_SURFACE()
B_SPLINE_SURFACE(3,2,((#404912,#404913,#404914),(#404915,#404916,#404917),
(#404918,#404919,#404920),(#404921,#404922,#404923)),.UNSPECIFIED.,.F.,
 .F.,.F.)
B_SPLINE_SURFACE_WITH_KNOTS((4,4),(3,3),(0.00137194782501028,0.00149814269699235),
(0.,1.),.UNSPECIFIED.)
GEOMETRIC_REPRESENTATION_ITEM()
RATIONAL_B_SPLINE_SURFACE(((1.,0.815158509402317,1.),(1.,0.816179044148144,
1.),(1.,0.817226308119948,1.),(1.,0.818301939488799,1.)))
REPRESENTATION_ITEM('')
SURFACE()
);
#3144=(
BOUNDED_SURFACE()
B_SPLINE_SURFACE(3,2,((#404967,#404968,#404969),(#404970,#404971,#404972),
(#404973,#404974,#404975),(#404976,#404977,#404978)),.UNSPECIFIED.,.F.,
 .F.,.F.)
B_SPLINE_SURFACE_WITH_KNOTS((4,4),(3,3),(1.55009486301137E-5,4.92065510474435E-5),
(-8.13759517818879E-5,1.),.UNSPECIFIED.)
GEOMETRIC_REPRESENTATION_ITEM()
RATIONAL_B_SPLINE_SURFACE(((1.00002372912344,0.854200639599641,1.),(1.00001423585999,
0.912530301180507,1.),(1.00000710550473,0.956341495377427,1.),(1.00001238975913,
0.923873338136997,1.)))
REPRESENTATION_ITEM('')
SURFACE()
);
#3145=(
BOUNDED_SURFACE()
B_SPLINE_SURFACE(3,2,((#404982,#404983,#404984),(#404985,#404986,#404987),
(#404988,#404989,#404990),(#404991,#404992,#404993)),.UNSPECIFIED.,.F.,
 .F.,.F.)
B_SPLINE_SURFACE_WITH_KNOTS((4,4),(3,3),(-3.39934179457839E-6,3.73927597403565E-5),
(-0.00186004067408013,1.00069373317433),.UNSPECIFIED.)
GEOMETRIC_REPRESENTATION_ITEM()
RATIONAL_B_SPLINE_SURFACE(((1.0007210013605,0.806051963875374,1.00026859642689),
(1.0006004844015,0.838470803558685,1.00022369994494),(1.00053106448792,
0.857144632272391,1.00019783877218),(1.00054515072849,0.85335545953913,
1.00020308635435)))
REPRESENTATION_ITEM('')
SURFACE()
);
#3146=(
BOUNDED_SURFACE()
B_SPLINE_SURFACE(3,2,((#404995,#404996,#404997),(#404998,#404999,#405000),
(#405001,#405002,#405003),(#405004,#405005,#405006)),.UNSPECIFIED.,.F.,
 .F.,.F.)
B_SPLINE_SURFACE_WITH_KNOTS((4,4),(3,3),(-1.62630325872826E-19,9.54361881492173E-5),
(0.,1.),.UNSPECIFIED.)
GEOMETRIC_REPRESENTATION_ITEM()
RATIONAL_B_SPLINE_SURFACE(((1.,0.816715621142041,1.),(1.,0.815907587407958,
1.),(1.,0.815115959345198,1.),(1.,0.814339887349188,1.)))
REPRESENTATION_ITEM('')
SURFACE()
);
#3147=(
BOUNDED_SURFACE()
B_SPLINE_SURFACE(3,2,((#405008,#405009,#405010),(#405011,#405012,#405013),
(#405014,#405015,#405016),(#405017,#405018,#405019)),.UNSPECIFIED.,.F.,
 .F.,.F.)
B_SPLINE_SURFACE_WITH_KNOTS((4,4),(3,3),(-2.18534500391609E-19,4.68197758448207E-5),
(0.,1.),.UNSPECIFIED.)
GEOMETRIC_REPRESENTATION_ITEM()
RATIONAL_B_SPLINE_SURFACE(((1.,0.816715621142048,1.),(1.,0.953638980025177,
1.),(1.,0.954506925408093,1.),(1.,0.816715621142042,1.)))
REPRESENTATION_ITEM('')
SURFACE()
);
#3148=(
BOUNDED_SURFACE()
B_SPLINE_SURFACE(3,2,((#405021,#405022,#405023),(#405024,#405025,#405026),
(#405027,#405028,#405029),(#405030,#405031,#405032)),.UNSPECIFIED.,.F.,
 .F.,.F.)
B_SPLINE_SURFACE_WITH_KNOTS((4,4),(3,3),(1.62630325872826E-19,9.54361881492177E-5),
(0.,1.),.UNSPECIFIED.)
GEOMETRIC_REPRESENTATION_ITEM()
RATIONAL_B_SPLINE_SURFACE(((1.,0.814339887349193,1.),(1.,0.815115959345219,
1.),(1.,0.815907587407931,1.),(1.,0.816715621142048,1.)))
REPRESENTATION_ITEM('')
SURFACE()
);
#3149=(
BOUNDED_SURFACE()
B_SPLINE_SURFACE(3,2,((#405034,#405035,#405036),(#405037,#405038,#405039),
(#405040,#405041,#405042),(#405043,#405044,#405045)),.UNSPECIFIED.,.F.,
 .F.,.F.)
B_SPLINE_SURFACE_WITH_KNOTS((4,4),(3,3),(-3.39528393502487E-6,3.73481232852729E-5),
(-0.00165018033325894,1.),.UNSPECIFIED.)
GEOMETRIC_REPRESENTATION_ITEM()
RATIONAL_B_SPLINE_SURFACE(((1.00048354385565,0.853487571660394,1.),(1.0004711051092,
0.857256476851486,1.),(1.00053193201107,0.838826096655843,1.),(1.00063970687725,
0.806170615310116,1.)))
REPRESENTATION_ITEM('')
SURFACE()
);
#3150=(
BOUNDED_SURFACE()
B_SPLINE_SURFACE(3,2,((#405049,#405050,#405051),(#405052,#405053,#405054),
(#405055,#405056,#405057),(#405058,#405059,#405060)),.UNSPECIFIED.,.F.,
 .F.,.F.)
B_SPLINE_SURFACE_WITH_KNOTS((4,4),(3,3),(2.02993869230509E-5,5.3975695268713E-5),
(-0.000116281070087646,1.),.UNSPECIFIED.)
GEOMETRIC_REPRESENTATION_ITEM()
RATIONAL_B_SPLINE_SURFACE(((1.00001770479732,0.923870681142998,1.),(1.0000101410406,
0.956394275543433,1.),(1.00002037300281,0.912397594905605,1.),(1.00003390859474,
0.854195550869712,1.)))
REPRESENTATION_ITEM('')
SURFACE()
);
#3151=(
BOUNDED_SURFACE()
B_SPLINE_SURFACE(3,2,((#405153,#405154,#405155),(#405156,#405157,#405158),
(#405159,#405160,#405161),(#405162,#405163,#405164)),.UNSPECIFIED.,.F.,
 .F.,.F.)
B_SPLINE_SURFACE_WITH_KNOTS((4,4),(3,3),(0.00135801595889393,0.00148409170619832),
(0.,1.),.UNSPECIFIED.)
GEOMETRIC_REPRESENTATION_ITEM()
RATIONAL_B_SPLINE_SURFACE(((1.,0.818301933966444,1.),(1.,0.817226613172336,
1.),(1.,0.816179643373948,1.),(1.,0.815159387863655,1.)))
REPRESENTATION_ITEM('')
SURFACE()
);
#3152=(
BOUNDED_SURFACE()
B_SPLINE_SURFACE(3,2,((#405203,#405204,#405205),(#405206,#405207,#405208),
(#405209,#405210,#405211),(#405212,#405213,#405214)),.UNSPECIFIED.,.F.,
 .F.,.F.)
B_SPLINE_SURFACE_WITH_KNOTS((4,4),(3,3),(-1.54744435122067E-6,1.54744435122073E-5),
(-0.0151698983595576,1.),.UNSPECIFIED.)
GEOMETRIC_REPRESENTATION_ITEM()
RATIONAL_B_SPLINE_SURFACE(((1.0201838247261,0.33474093735822,1.),(1.00401234488756,
0.867753072813637,1.),(1.00033622856775,0.988917903080848,1.),(1.,1.,1.)))
REPRESENTATION_ITEM('')
SURFACE()
);
#3153=(
BOUNDED_SURFACE()
B_SPLINE_SURFACE(3,2,((#405216,#405217,#405218),(#405219,#405220,#405221),
(#405222,#405223,#405224),(#405225,#405226,#405227)),.UNSPECIFIED.,.F.,
 .F.,.F.)
B_SPLINE_SURFACE_WITH_KNOTS((4,4),(3,3),(0.00137194782501028,0.00149814269699235),
(0.,1.),.UNSPECIFIED.)
GEOMETRIC_REPRESENTATION_ITEM()
RATIONAL_B_SPLINE_SURFACE(((1.,0.81515850940232,1.),(1.,0.816179044148172,
1.),(1.,0.81722630811993,1.),(1.,0.818301939488811,1.)))
REPRESENTATION_ITEM('')
SURFACE()
);
#3154=(
BOUNDED_SURFACE()
B_SPLINE_SURFACE(3,2,((#405271,#405272,#405273),(#405274,#405275,#405276),
(#405277,#405278,#405279),(#405280,#405281,#405282)),.UNSPECIFIED.,.F.,
 .F.,.F.)
B_SPLINE_SURFACE_WITH_KNOTS((4,4),(3,3),(1.55009486301137E-5,4.92065510474429E-5),
(-8.1375951146008E-5,1.),.UNSPECIFIED.)
GEOMETRIC_REPRESENTATION_ITEM()
RATIONAL_B_SPLINE_SURFACE(((1.00002372912326,0.854200639599736,1.),(1.00001423585988,
0.912530301180571,1.),(1.00000710550468,0.956341495377441,1.),(1.00001238975903,
0.92387333813705,1.)))
REPRESENTATION_ITEM('')
SURFACE()
);
#3155=(
BOUNDED_SURFACE()
B_SPLINE_SURFACE(3,2,((#405286,#405287,#405288),(#405289,#405290,#405291),
(#405292,#405293,#405294),(#405295,#405296,#405297)),.UNSPECIFIED.,.F.,
 .F.,.F.)
B_SPLINE_SURFACE_WITH_KNOTS((4,4),(3,3),(-3.39934179457831E-6,3.73927597403567E-5),
(-0.00186004067387599,1.00069373317442),.UNSPECIFIED.)
GEOMETRIC_REPRESENTATION_ITEM()
RATIONAL_B_SPLINE_SURFACE(((1.00072100136043,0.806051963875394,1.00026859642692),
(1.00060048440144,0.8384708035587,1.00022369994497),(1.00053106448786,0.857144632272403,
1.0001978387722),(1.00054515072843,0.853355459539154,1.00020308635438)))
REPRESENTATION_ITEM('')
SURFACE()
);
#3156=(
BOUNDED_SURFACE()
B_SPLINE_SURFACE(3,2,((#405299,#405300,#405301),(#405302,#405303,#405304),
(#405305,#405306,#405307),(#405308,#405309,#405310)),.UNSPECIFIED.,.F.,
 .F.,.F.)
B_SPLINE_SURFACE_WITH_KNOTS((4,4),(3,3),(0.,9.54361881492172E-5),(0.,1.),
 .UNSPECIFIED.)
GEOMETRIC_REPRESENTATION_ITEM()
RATIONAL_B_SPLINE_SURFACE(((1.,0.816715621142041,1.),(1.,0.815907587407948,
1.),(1.,0.8151159593452,1.),(1.,0.81433988734919,1.)))
REPRESENTATION_ITEM('')
SURFACE()
);
#3157=(
BOUNDED_SURFACE()
B_SPLINE_SURFACE(3,2,((#405312,#405313,#405314),(#405315,#405316,#405317),
(#405318,#405319,#405320),(#405321,#405322,#405323)),.UNSPECIFIED.,.F.,
 .F.,.F.)
B_SPLINE_SURFACE_WITH_KNOTS((4,4),(3,3),(2.3039296165317E-19,4.68197758448208E-5),
(0.,1.),.UNSPECIFIED.)
GEOMETRIC_REPRESENTATION_ITEM()
RATIONAL_B_SPLINE_SURFACE(((1.,0.816715621142044,1.),(1.,0.95363898002521,
1.),(1.,0.954506925408057,1.),(1.,0.816715621142057,1.)))
REPRESENTATION_ITEM('')
SURFACE()
);
#3158=(
BOUNDED_SURFACE()
B_SPLINE_SURFACE(3,2,((#405325,#405326,#405327),(#405328,#405329,#405330),
(#405331,#405332,#405333),(#405334,#405335,#405336)),.UNSPECIFIED.,.F.,
 .F.,.F.)
B_SPLINE_SURFACE_WITH_KNOTS((4,4),(3,3),(-5.42101086242752E-20,9.54361881492175E-5),
(0.,1.),.UNSPECIFIED.)
GEOMETRIC_REPRESENTATION_ITEM()
RATIONAL_B_SPLINE_SURFACE(((1.,0.814339887349189,1.),(1.,0.81511595934523,
1.),(1.,0.815907587407935,1.),(1.,0.816715621142044,1.)))
REPRESENTATION_ITEM('')
SURFACE()
);
#3159=(
BOUNDED_SURFACE()
B_SPLINE_SURFACE(3,2,((#405338,#405339,#405340),(#405341,#405342,#405343),
(#405344,#405345,#405346),(#405347,#405348,#405349)),.UNSPECIFIED.,.F.,
 .F.,.F.)
B_SPLINE_SURFACE_WITH_KNOTS((4,4),(3,3),(-3.3952839350249E-6,3.73481232852736E-5),
(-0.00165018033293838,1.),.UNSPECIFIED.)
GEOMETRIC_REPRESENTATION_ITEM()
RATIONAL_B_SPLINE_SURFACE(((1.00048354385555,0.853487571660468,1.),(1.00047110510911,
0.857256476851485,1.),(1.00053193201096,0.83882609665595,1.),(1.00063970687712,
0.806170615310157,1.)))
REPRESENTATION_ITEM('')
SURFACE()
);
#3160=(
BOUNDED_SURFACE()
B_SPLINE_SURFACE(3,2,((#405353,#405354,#405355),(#405356,#405357,#405358),
(#405359,#405360,#405361),(#405362,#405363,#405364)),.UNSPECIFIED.,.F.,
 .F.,.F.)
B_SPLINE_SURFACE_WITH_KNOTS((4,4),(3,3),(2.0299386923051E-5,5.3975695268713E-5),
(-0.000116281069768265,1.),.UNSPECIFIED.)
GEOMETRIC_REPRESENTATION_ITEM()
RATIONAL_B_SPLINE_SURFACE(((1.00001770479727,0.923870681143019,1.),(1.00001014104058,
0.95639427554345,1.),(1.00002037300276,0.912397594905637,1.),(1.00003390859464,
0.854195550869751,1.)))
REPRESENTATION_ITEM('')
SURFACE()
);
#3161=(
BOUNDED_SURFACE()
B_SPLINE_SURFACE(3,2,((#405457,#405458,#405459),(#405460,#405461,#405462),
(#405463,#405464,#405465),(#405466,#405467,#405468)),.UNSPECIFIED.,.F.,
 .F.,.F.)
B_SPLINE_SURFACE_WITH_KNOTS((4,4),(3,3),(0.00135801595889393,0.00148409170619832),
(0.,1.),.UNSPECIFIED.)
GEOMETRIC_REPRESENTATION_ITEM()
RATIONAL_B_SPLINE_SURFACE(((1.,0.818301933966443,1.),(1.,0.817226613172352,
1.),(1.,0.816179643373961,1.),(1.,0.815159387863647,1.)))
REPRESENTATION_ITEM('')
SURFACE()
);
#3162=(
BOUNDED_SURFACE()
B_SPLINE_SURFACE(3,2,((#405507,#405508,#405509),(#405510,#405511,#405512),
(#405513,#405514,#405515),(#405516,#405517,#405518)),.UNSPECIFIED.,.F.,
 .F.,.F.)
B_SPLINE_SURFACE_WITH_KNOTS((4,4),(3,3),(-1.54744435122026E-6,1.54744435122097E-5),
(-0.0151698983659335,1.),.UNSPECIFIED.)
GEOMETRIC_REPRESENTATION_ITEM()
RATIONAL_B_SPLINE_SURFACE(((1.02018382473471,0.334740937354024,1.),(1.00401234488928,
0.867753072812738,1.),(1.00033622856789,0.988917903080813,1.),(1.,1.,1.)))
REPRESENTATION_ITEM('')
SURFACE()
);
#3163=(
BOUNDED_SURFACE()
B_SPLINE_SURFACE(3,2,((#405520,#405521,#405522),(#405523,#405524,#405525),
(#405526,#405527,#405528),(#405529,#405530,#405531)),.UNSPECIFIED.,.F.,
 .F.,.F.)
B_SPLINE_SURFACE_WITH_KNOTS((4,4),(3,3),(0.00137194782501028,0.00149814269699235),
(0.,1.),.UNSPECIFIED.)
GEOMETRIC_REPRESENTATION_ITEM()
RATIONAL_B_SPLINE_SURFACE(((1.,0.815158509402312,1.),(1.,0.816179044148169,
1.),(1.,0.817226308119936,1.),(1.,0.818301939488803,1.)))
REPRESENTATION_ITEM('')
SURFACE()
);
#3164=(
BOUNDED_SURFACE()
B_SPLINE_SURFACE(3,2,((#405575,#405576,#405577),(#405578,#405579,#405580),
(#405581,#405582,#405583),(#405584,#405585,#405586)),.UNSPECIFIED.,.F.,
 .F.,.F.)
B_SPLINE_SURFACE_WITH_KNOTS((4,4),(3,3),(1.55009486301137E-5,4.92065510474438E-5),
(-8.13759512935703E-5,1.),.UNSPECIFIED.)
GEOMETRIC_REPRESENTATION_ITEM()
RATIONAL_B_SPLINE_SURFACE(((1.0000237291233,0.854200639599709,1.),(1.0000142358599,
0.912530301180559,1.),(1.00000710550469,0.956341495377438,1.),(1.00001238975906,
0.923873338137037,1.)))
REPRESENTATION_ITEM('')
SURFACE()
);
#3165=(
BOUNDED_SURFACE()
B_SPLINE_SURFACE(3,2,((#405590,#405591,#405592),(#405593,#405594,#405595),
(#405596,#405597,#405598),(#405599,#405600,#405601)),.UNSPECIFIED.,.F.,
 .F.,.F.)
B_SPLINE_SURFACE_WITH_KNOTS((4,4),(3,3),(-3.39934179457839E-6,3.73927597403563E-5),
(-0.00186004067454099,1.00069373317433),.UNSPECIFIED.)
GEOMETRIC_REPRESENTATION_ITEM()
RATIONAL_B_SPLINE_SURFACE(((1.00072100136068,0.80605196387532,1.00026859642688),
(1.00060048440165,0.838470803558564,1.00022369994494),(1.00053106448805,
0.857144632272353,1.00019783877218),(1.00054515072863,0.853355459539056,
1.00020308635435)))
REPRESENTATION_ITEM('')
SURFACE()
);
#3166=(
BOUNDED_SURFACE()
B_SPLINE_SURFACE(3,2,((#405603,#405604,#405605),(#405606,#405607,#405608),
(#405609,#405610,#405611),(#405612,#405613,#405614)),.UNSPECIFIED.,.F.,
 .F.,.F.)
B_SPLINE_SURFACE_WITH_KNOTS((4,4),(3,3),(-5.42101086242752E-20,9.54361881492174E-5),
(0.,1.),.UNSPECIFIED.)
GEOMETRIC_REPRESENTATION_ITEM()
RATIONAL_B_SPLINE_SURFACE(((1.,0.816715621142051,1.),(1.,0.815907587407935,
1.),(1.,0.815115959345206,1.),(1.,0.814339887349197,1.)))
REPRESENTATION_ITEM('')
SURFACE()
);
#3167=(
BOUNDED_SURFACE()
B_SPLINE_SURFACE(3,2,((#405616,#405617,#405618),(#405619,#405620,#405621),
(#405622,#405623,#405624),(#405625,#405626,#405627)),.UNSPECIFIED.,.F.,
 .F.,.F.)
B_SPLINE_SURFACE_WITH_KNOTS((4,4),(3,3),(-1.6940658945086E-19,4.68197758448204E-5),
(0.,1.),.UNSPECIFIED.)
GEOMETRIC_REPRESENTATION_ITEM()
RATIONAL_B_SPLINE_SURFACE(((1.,0.81671562114205,1.),(1.,0.953638980025204,
1.),(1.,0.954506925408062,1.),(1.,0.81671562114205,1.)))
REPRESENTATION_ITEM('')
SURFACE()
);
#3168=(
BOUNDED_SURFACE()
B_SPLINE_SURFACE(3,2,((#405629,#405630,#405631),(#405632,#405633,#405634),
(#405635,#405636,#405637),(#405638,#405639,#405640)),.UNSPECIFIED.,.F.,
 .F.,.F.)
B_SPLINE_SURFACE_WITH_KNOTS((4,4),(3,3),(-3.25260651745651E-19,9.54361881492175E-5),
(0.,1.),.UNSPECIFIED.)
GEOMETRIC_REPRESENTATION_ITEM()
RATIONAL_B_SPLINE_SURFACE(((1.,0.814339887349189,1.),(1.,0.815115959345215,
1.),(1.,0.815907587407932,1.),(1.,0.81671562114205,1.)))
REPRESENTATION_ITEM('')
SURFACE()
);
#3169=(
BOUNDED_SURFACE()
B_SPLINE_SURFACE(3,2,((#405642,#405643,#405644),(#405645,#405646,#405647),
(#405648,#405649,#405650),(#405651,#405652,#405653)),.UNSPECIFIED.,.F.,
 .F.,.F.)
B_SPLINE_SURFACE_WITH_KNOTS((4,4),(3,3),(-3.39528393502489E-6,3.73481232852736E-5),
(-0.00165018033330409,1.),.UNSPECIFIED.)
GEOMETRIC_REPRESENTATION_ITEM()
RATIONAL_B_SPLINE_SURFACE(((1.00048354385566,0.853487571660407,1.),(1.00047110510921,
0.857256476851462,1.),(1.00053193201108,0.838826096655856,1.),(1.00063970687726,
0.806170615310109,1.)))
REPRESENTATION_ITEM('')
SURFACE()
);
#3170=(
BOUNDED_SURFACE()
B_SPLINE_SURFACE(3,2,((#405657,#405658,#405659),(#405660,#405661,#405662),
(#405663,#405664,#405665),(#405666,#405667,#405668)),.UNSPECIFIED.,.F.,
 .F.,.F.)
B_SPLINE_SURFACE_WITH_KNOTS((4,4),(3,3),(2.02993869230511E-5,5.39756952687126E-5),
(-0.000116281069505731,1.),.UNSPECIFIED.)
GEOMETRIC_REPRESENTATION_ITEM()
RATIONAL_B_SPLINE_SURFACE(((1.00001770479723,0.923870681143043,1.),(1.00001014104055,
0.956394275543463,1.),(1.00002037300271,0.912397594905643,1.),(1.00003390859457,
0.854195550869798,1.)))
REPRESENTATION_ITEM('')
SURFACE()
);
#3171=(
BOUNDED_SURFACE()
B_SPLINE_SURFACE(3,2,((#405761,#405762,#405763),(#405764,#405765,#405766),
(#405767,#405768,#405769),(#405770,#405771,#405772)),.UNSPECIFIED.,.F.,
 .F.,.F.)
B_SPLINE_SURFACE_WITH_KNOTS((4,4),(3,3),(0.00135801595889393,0.00148409170619832),
(0.,1.),.UNSPECIFIED.)
GEOMETRIC_REPRESENTATION_ITEM()
RATIONAL_B_SPLINE_SURFACE(((1.,0.818301933966442,1.),(1.,0.817226613172354,
1.),(1.,0.816179643373949,1.),(1.,0.815159387863654,1.)))
REPRESENTATION_ITEM('')
SURFACE()
);
#3172=(
BOUNDED_SURFACE()
B_SPLINE_SURFACE(3,2,((#405811,#405812,#405813),(#405814,#405815,#405816),
(#405817,#405818,#405819),(#405820,#405821,#405822)),.UNSPECIFIED.,.F.,
 .F.,.F.)
B_SPLINE_SURFACE_WITH_KNOTS((4,4),(3,3),(-1.54744435122082E-6,1.54744435122081E-5),
(-0.015169898361091,1.),.UNSPECIFIED.)
GEOMETRIC_REPRESENTATION_ITEM()
RATIONAL_B_SPLINE_SURFACE(((1.02018382472817,0.334740937357215,1.),(1.00401234488797,
0.867753072813476,1.),(1.00033622856778,0.988917903080883,1.),(1.,1.,1.)))
REPRESENTATION_ITEM('')
SURFACE()
);
#3173=(
BOUNDED_SURFACE()
B_SPLINE_SURFACE(3,2,((#405824,#405825,#405826),(#405827,#405828,#405829),
(#405830,#405831,#405832),(#405833,#405834,#405835)),.UNSPECIFIED.,.F.,
 .F.,.F.)
B_SPLINE_SURFACE_WITH_KNOTS((4,4),(3,3),(0.00137194782501028,0.00149814269699235),
(0.,1.),.UNSPECIFIED.)
GEOMETRIC_REPRESENTATION_ITEM()
RATIONAL_B_SPLINE_SURFACE(((1.,0.815158509402314,1.),(1.,0.816179044148165,
1.),(1.,0.817226308119932,1.),(1.,0.818301939488806,1.)))
REPRESENTATION_ITEM('')
SURFACE()
);
#3174=(
BOUNDED_SURFACE()
B_SPLINE_SURFACE(3,2,((#405879,#405880,#405881),(#405882,#405883,#405884),
(#405885,#405886,#405887),(#405888,#405889,#405890)),.UNSPECIFIED.,.F.,
 .F.,.F.)
B_SPLINE_SURFACE_WITH_KNOTS((4,4),(3,3),(1.55009486301137E-5,4.92065510474431E-5),
(-8.13759513357166E-5,1.),.UNSPECIFIED.)
GEOMETRIC_REPRESENTATION_ITEM()
RATIONAL_B_SPLINE_SURFACE(((1.00002372912331,0.854200639599699,1.),(1.00001423585991,
0.912530301180558,1.),(1.00000710550469,0.956341495377437,1.),(1.00001238975906,
0.92387333813703,1.)))
REPRESENTATION_ITEM('')
SURFACE()
);
#3175=(
BOUNDED_SURFACE()
B_SPLINE_SURFACE(3,2,((#405894,#405895,#405896),(#405897,#405898,#405899),
(#405900,#405901,#405902),(#405903,#405904,#405905)),.UNSPECIFIED.,.F.,
 .F.,.F.)
B_SPLINE_SURFACE_WITH_KNOTS((4,4),(3,3),(-3.39934179457816E-6,3.73927597403566E-5),
(-0.0018600406740343,1.00069373317451),.UNSPECIFIED.)
GEOMETRIC_REPRESENTATION_ITEM()
RATIONAL_B_SPLINE_SURFACE(((1.00072100136049,0.806051963875347,1.00026859642695),
(1.00060048440149,0.838470803558664,1.00022369994499),(1.0005310644879,
0.857144632272365,1.00019783877223),(1.00054515072848,0.853355459539118,
1.0002030863544)))
REPRESENTATION_ITEM('')
SURFACE()
);
#3176=(
BOUNDED_SURFACE()
B_SPLINE_SURFACE(3,2,((#405907,#405908,#405909),(#405910,#405911,#405912),
(#405913,#405914,#405915),(#405916,#405917,#405918)),.UNSPECIFIED.,.F.,
 .F.,.F.)
B_SPLINE_SURFACE_WITH_KNOTS((4,4),(3,3),(-5.42101086242752E-20,9.54361881492174E-5),
(0.,1.),.UNSPECIFIED.)
GEOMETRIC_REPRESENTATION_ITEM()
RATIONAL_B_SPLINE_SURFACE(((1.,0.816715621142048,1.),(1.,0.81590758740793,
1.),(1.,0.815115959345223,1.),(1.,0.814339887349182,1.)))
REPRESENTATION_ITEM('')
SURFACE()
);
#3177=(
BOUNDED_SURFACE()
B_SPLINE_SURFACE(3,2,((#405920,#405921,#405922),(#405923,#405924,#405925),
(#405926,#405927,#405928),(#405929,#405930,#405931)),.UNSPECIFIED.,.F.,
 .F.,.F.)
B_SPLINE_SURFACE_WITH_KNOTS((4,4),(3,3),(-1.52465930505774E-20,4.6819775844821E-5),
(0.,1.),.UNSPECIFIED.)
GEOMETRIC_REPRESENTATION_ITEM()
RATIONAL_B_SPLINE_SURFACE(((1.,0.816715621142048,1.),(1.,0.953638980025194,
1.),(1.,0.954506925408067,1.),(1.,0.81671562114205,1.)))
REPRESENTATION_ITEM('')
SURFACE()
);
#3178=(
BOUNDED_SURFACE()
B_SPLINE_SURFACE(3,2,((#405933,#405934,#405935),(#405936,#405937,#405938),
(#405939,#405940,#405941),(#405942,#405943,#405944)),.UNSPECIFIED.,.F.,
 .F.,.F.)
B_SPLINE_SURFACE_WITH_KNOTS((4,4),(3,3),(-5.42101086242752E-20,9.54361881492175E-5),
(0.,1.),.UNSPECIFIED.)
GEOMETRIC_REPRESENTATION_ITEM()
RATIONAL_B_SPLINE_SURFACE(((1.,0.814339887349192,1.),(1.,0.815115959345209,
1.),(1.,0.815907587407939,1.),(1.,0.816715621142048,1.)))
REPRESENTATION_ITEM('')
SURFACE()
);
#3179=(
BOUNDED_SURFACE()
B_SPLINE_SURFACE(3,2,((#405946,#405947,#405948),(#405949,#405950,#405951),
(#405952,#405953,#405954),(#405955,#405956,#405957)),.UNSPECIFIED.,.F.,
 .F.,.F.)
B_SPLINE_SURFACE_WITH_KNOTS((4,4),(3,3),(-3.39528393502372E-6,3.73481232852733E-5),
(-0.00165018033253919,1.),.UNSPECIFIED.)
GEOMETRIC_REPRESENTATION_ITEM()
RATIONAL_B_SPLINE_SURFACE(((1.00048354385544,0.853487571660503,1.),(1.00047110510899,
0.857256476851567,1.),(1.00053193201083,0.838826096655973,1.),(1.00063970687697,
0.806170615310248,1.)))
REPRESENTATION_ITEM('')
SURFACE()
);
#3180=(
BOUNDED_SURFACE()
B_SPLINE_SURFACE(3,2,((#405961,#405962,#405963),(#405964,#405965,#405966),
(#405967,#405968,#405969),(#405970,#405971,#405972)),.UNSPECIFIED.,.F.,
 .F.,.F.)
B_SPLINE_SURFACE_WITH_KNOTS((4,4),(3,3),(2.0299386923051E-5,5.39756952687123E-5),
(-0.000116281069828518,1.),.UNSPECIFIED.)
GEOMETRIC_REPRESENTATION_ITEM()
RATIONAL_B_SPLINE_SURFACE(((1.00001770479728,0.923870681143012,1.),(1.00001014104058,
0.956394275543464,1.),(1.00002037300277,0.912397594905604,1.),(1.00003390859466,
0.854195550869756,1.)))
REPRESENTATION_ITEM('')
SURFACE()
);
#3181=(
BOUNDED_SURFACE()
B_SPLINE_SURFACE(3,2,((#406065,#406066,#406067),(#406068,#406069,#406070),
(#406071,#406072,#406073),(#406074,#406075,#406076)),.UNSPECIFIED.,.F.,
 .F.,.F.)
B_SPLINE_SURFACE_WITH_KNOTS((4,4),(3,3),(0.00135801595889393,0.00148409170619832),
(0.,1.),.UNSPECIFIED.)
GEOMETRIC_REPRESENTATION_ITEM()
RATIONAL_B_SPLINE_SURFACE(((1.,0.818301933966443,1.),(1.,0.817226613172342,
1.),(1.,0.816179643373952,1.),(1.,0.815159387863651,1.)))
REPRESENTATION_ITEM('')
SURFACE()
);
#3182=(
BOUNDED_SURFACE()
B_SPLINE_SURFACE(3,2,((#406115,#406116,#406117),(#406118,#406119,#406120),
(#406121,#406122,#406123),(#406124,#406125,#406126)),.UNSPECIFIED.,.F.,
 .F.,.F.)
B_SPLINE_SURFACE_WITH_KNOTS((4,4),(3,3),(-1.54744435122067E-6,1.54744435122067E-5),
(-0.0151698983602967,1.),.UNSPECIFIED.)
GEOMETRIC_REPRESENTATION_ITEM()
RATIONAL_B_SPLINE_SURFACE(((1.0201838247271,0.334740937357766,1.),(1.00401234488776,
0.867753072813545,1.),(1.00033622856776,0.988917903080887,1.),(1.,1.,1.)))
REPRESENTATION_ITEM('')
SURFACE()
);
#3183=(
BOUNDED_SURFACE()
B_SPLINE_SURFACE(3,2,((#406128,#406129,#406130),(#406131,#406132,#406133),
(#406134,#406135,#406136),(#406137,#406138,#406139)),.UNSPECIFIED.,.F.,
 .F.,.F.)
B_SPLINE_SURFACE_WITH_KNOTS((4,4),(3,3),(0.00137194782501028,0.00149814269699235),
(0.,1.),.UNSPECIFIED.)
GEOMETRIC_REPRESENTATION_ITEM()
RATIONAL_B_SPLINE_SURFACE(((1.,0.815158509402321,1.),(1.,0.816179044148165,
1.),(1.,0.817226308119932,1.),(1.,0.818301939488811,1.)))
REPRESENTATION_ITEM('')
SURFACE()
);
#3184=(
BOUNDED_SURFACE()
B_SPLINE_SURFACE(3,2,((#406183,#406184,#406185),(#406186,#406187,#406188),
(#406189,#406190,#406191),(#406192,#406193,#406194)),.UNSPECIFIED.,.F.,
 .F.,.F.)
B_SPLINE_SURFACE_WITH_KNOTS((4,4),(3,3),(1.55009486301137E-5,4.92065510474429E-5),
(-8.13759516652293E-5,1.),.UNSPECIFIED.)
GEOMETRIC_REPRESENTATION_ITEM()
RATIONAL_B_SPLINE_SURFACE(((1.00002372912341,0.854200639599659,1.),(1.00001423585997,
0.912530301180516,1.),(1.00000710550472,0.95634149537743,1.),(1.00001238975911,
0.923873338137006,1.)))
REPRESENTATION_ITEM('')
SURFACE()
);
#3185=(
BOUNDED_SURFACE()
B_SPLINE_SURFACE(3,2,((#406198,#406199,#406200),(#406201,#406202,#406203),
(#406204,#406205,#406206),(#406207,#406208,#406209)),.UNSPECIFIED.,.F.,
 .F.,.F.)
B_SPLINE_SURFACE_WITH_KNOTS((4,4),(3,3),(-3.39934179457825E-6,3.73927597403566E-5),
(-0.00186004067403026,1.00069373317436),.UNSPECIFIED.)
GEOMETRIC_REPRESENTATION_ITEM()
RATIONAL_B_SPLINE_SURFACE(((1.00072100136049,0.806051963875376,1.00026859642689),
(1.00060048440149,0.838470803558669,1.00022369994495),(1.0005310644879,
0.857144632272403,1.00019783877218),(1.00054515072848,0.853355459539127,
1.00020308635436)))
REPRESENTATION_ITEM('')
SURFACE()
);
#3186=(
BOUNDED_SURFACE()
B_SPLINE_SURFACE(3,2,((#406211,#406212,#406213),(#406214,#406215,#406216),
(#406217,#406218,#406219),(#406220,#406221,#406222)),.UNSPECIFIED.,.F.,
 .F.,.F.)
B_SPLINE_SURFACE_WITH_KNOTS((4,4),(3,3),(-5.42101086242752E-20,9.54361881492172E-5),
(0.,1.),.UNSPECIFIED.)
GEOMETRIC_REPRESENTATION_ITEM()
RATIONAL_B_SPLINE_SURFACE(((1.,0.81671562114205,1.),(1.,0.815907587407941,
1.),(1.,0.815115959345202,1.),(1.,0.814339887349194,1.)))
REPRESENTATION_ITEM('')
SURFACE()
);
#3187=(
BOUNDED_SURFACE()
B_SPLINE_SURFACE(3,2,((#406224,#406225,#406226),(#406227,#406228,#406229),
(#406230,#406231,#406232),(#406233,#406234,#406235)),.UNSPECIFIED.,.F.,
 .F.,.F.)
B_SPLINE_SURFACE_WITH_KNOTS((4,4),(3,3),(-2.03287907341032E-20,4.68197758448218E-5),
(0.,1.),.UNSPECIFIED.)
GEOMETRIC_REPRESENTATION_ITEM()
RATIONAL_B_SPLINE_SURFACE(((1.,0.816715621142045,1.),(1.,0.953638980025206,
1.),(1.,0.954506925408059,1.),(1.,0.816715621142049,1.)))
REPRESENTATION_ITEM('')
SURFACE()
);
#3188=(
BOUNDED_SURFACE()
B_SPLINE_SURFACE(3,2,((#406237,#406238,#406239),(#406240,#406241,#406242),
(#406243,#406244,#406245),(#406246,#406247,#406248)),.UNSPECIFIED.,.F.,
 .F.,.F.)
B_SPLINE_SURFACE_WITH_KNOTS((4,4),(3,3),(0.,9.54361881492173E-5),(0.,1.),
 .UNSPECIFIED.)
GEOMETRIC_REPRESENTATION_ITEM()
RATIONAL_B_SPLINE_SURFACE(((1.,0.814339887349198,1.),(1.,0.815115959345204,
1.),(1.,0.815907587407952,1.),(1.,0.816715621142052,1.)))
REPRESENTATION_ITEM('')
SURFACE()
);
#3189=(
BOUNDED_SURFACE()
B_SPLINE_SURFACE(3,2,((#406250,#406251,#406252),(#406253,#406254,#406255),
(#406256,#406257,#406258),(#406259,#406260,#406261)),.UNSPECIFIED.,.F.,
 .F.,.F.)
B_SPLINE_SURFACE_WITH_KNOTS((4,4),(3,3),(-3.39528393502492E-6,3.73481232852737E-5),
(-0.00165018033268536,1.),.UNSPECIFIED.)
GEOMETRIC_REPRESENTATION_ITEM()
RATIONAL_B_SPLINE_SURFACE(((1.00048354385548,0.853487571660492,1.),(1.00047110510904,
0.857256476851538,1.),(1.00053193201088,0.838826096655981,1.),(1.00063970687702,
0.806170615310209,1.)))
REPRESENTATION_ITEM('')
SURFACE()
);
#3190=(
BOUNDED_SURFACE()
B_SPLINE_SURFACE(3,2,((#406265,#406266,#406267),(#406268,#406269,#406270),
(#406271,#406272,#406273),(#406274,#406275,#406276)),.UNSPECIFIED.,.F.,
 .F.,.F.)
B_SPLINE_SURFACE_WITH_KNOTS((4,4),(3,3),(2.0299386923051E-5,5.39756952687129E-5),
(-0.000116281069912106,1.),.UNSPECIFIED.)
GEOMETRIC_REPRESENTATION_ITEM()
RATIONAL_B_SPLINE_SURFACE(((1.0000177047973,0.923870681143004,1.),(1.00001014104059,
0.956394275543463,1.),(1.00002037300278,0.912397594905594,1.),(1.00003390859469,
0.854195550869741,1.)))
REPRESENTATION_ITEM('')
SURFACE()
);
#3191=(
BOUNDED_SURFACE()
B_SPLINE_SURFACE(3,2,((#406369,#406370,#406371),(#406372,#406373,#406374),
(#406375,#406376,#406377),(#406378,#406379,#406380)),.UNSPECIFIED.,.F.,
 .F.,.F.)
B_SPLINE_SURFACE_WITH_KNOTS((4,4),(3,3),(0.00135801595889393,0.00148409170619832),
(0.,1.),.UNSPECIFIED.)
GEOMETRIC_REPRESENTATION_ITEM()
RATIONAL_B_SPLINE_SURFACE(((1.,0.818301933966445,1.),(1.,0.81722661317235,
1.),(1.,0.816179643373955,1.),(1.,0.815159387863658,1.)))
REPRESENTATION_ITEM('')
SURFACE()
);
#3192=(
BOUNDED_SURFACE()
B_SPLINE_SURFACE(3,2,((#406419,#406420,#406421),(#406422,#406423,#406424),
(#406425,#406426,#406427),(#406428,#406429,#406430)),.UNSPECIFIED.,.F.,
 .F.,.F.)
B_SPLINE_SURFACE_WITH_KNOTS((4,4),(3,3),(-1.54744435122074E-6,1.54744435122073E-5),
(-0.015169898360452,1.),.UNSPECIFIED.)
GEOMETRIC_REPRESENTATION_ITEM()
RATIONAL_B_SPLINE_SURFACE(((1.02018382472731,0.334740937357643,1.),(1.0040123448878,
0.86775307281355,1.),(1.00033622856777,0.988917903080834,1.),(1.,1.,1.)))
REPRESENTATION_ITEM('')
SURFACE()
);
#3193=(
BOUNDED_SURFACE()
B_SPLINE_SURFACE(3,2,((#406432,#406433,#406434),(#406435,#406436,#406437),
(#406438,#406439,#406440),(#406441,#406442,#406443)),.UNSPECIFIED.,.F.,
 .F.,.F.)
B_SPLINE_SURFACE_WITH_KNOTS((4,4),(3,3),(0.00137194782501028,0.00149814269699235),
(0.,1.),.UNSPECIFIED.)
GEOMETRIC_REPRESENTATION_ITEM()
RATIONAL_B_SPLINE_SURFACE(((1.,0.815158509402315,1.),(1.,0.816179044148178,
1.),(1.,0.817226308119919,1.),(1.,0.81830193948881,1.)))
REPRESENTATION_ITEM('')
SURFACE()
);
#3194=(
BOUNDED_SURFACE()
B_SPLINE_SURFACE(3,2,((#406487,#406488,#406489),(#406490,#406491,#406492),
(#406493,#406494,#406495),(#406496,#406497,#406498)),.UNSPECIFIED.,.F.,
 .F.,.F.)
B_SPLINE_SURFACE_WITH_KNOTS((4,4),(3,3),(1.55009486301138E-5,4.92065510474426E-5),
(-8.13759513231332E-5,1.),.UNSPECIFIED.)
GEOMETRIC_REPRESENTATION_ITEM()
RATIONAL_B_SPLINE_SURFACE(((1.00002372912331,0.85420063959971,1.),(1.00001423585991,
0.912530301180546,1.),(1.00000710550469,0.956341495377441,1.),(1.00001238975906,
0.923873338137034,1.)))
REPRESENTATION_ITEM('')
SURFACE()
);
#3195=(
BOUNDED_SURFACE()
B_SPLINE_SURFACE(3,2,((#406502,#406503,#406504),(#406505,#406506,#406507),
(#406508,#406509,#406510),(#406511,#406512,#406513)),.UNSPECIFIED.,.F.,
 .F.,.F.)
B_SPLINE_SURFACE_WITH_KNOTS((4,4),(3,3),(-3.39934179457787E-6,3.73927597403566E-5),
(-0.00186004067382816,1.00069373317414),.UNSPECIFIED.)
GEOMETRIC_REPRESENTATION_ITEM()
RATIONAL_B_SPLINE_SURFACE(((1.00072100136041,0.806051963875452,1.00026859642681),
(1.00060048440142,0.838470803558758,1.00022369994488),(1.00053106448784,
0.857144632272456,1.00019783877212),(1.00054515072842,0.853355459539199,
1.00020308635429)))
REPRESENTATION_ITEM('')
SURFACE()
);
#3196=(
BOUNDED_SURFACE()
B_SPLINE_SURFACE(3,2,((#406515,#406516,#406517),(#406518,#406519,#406520),
(#406521,#406522,#406523),(#406524,#406525,#406526)),.UNSPECIFIED.,.F.,
 .F.,.F.)
B_SPLINE_SURFACE_WITH_KNOTS((4,4),(3,3),(2.16840434497101E-19,9.54361881492174E-5),
(0.,1.),.UNSPECIFIED.)
GEOMETRIC_REPRESENTATION_ITEM()
RATIONAL_B_SPLINE_SURFACE(((1.,0.81671562114205,1.),(1.,0.815907587407943,
1.),(1.,0.815115959345212,1.),(1.,0.814339887349199,1.)))
REPRESENTATION_ITEM('')
SURFACE()
);
#3197=(
BOUNDED_SURFACE()
B_SPLINE_SURFACE(3,2,((#406528,#406529,#406530),(#406531,#406532,#406533),
(#406534,#406535,#406536),(#406537,#406538,#406539)),.UNSPECIFIED.,.F.,
 .F.,.F.)
B_SPLINE_SURFACE_WITH_KNOTS((4,4),(3,3),(-2.72744609015885E-19,4.68197758448208E-5),
(0.,1.),.UNSPECIFIED.)
GEOMETRIC_REPRESENTATION_ITEM()
RATIONAL_B_SPLINE_SURFACE(((1.,0.816715621142048,1.),(1.,0.953638980025201,
1.),(1.,0.954506925408066,1.),(1.,0.81671562114205,1.)))
REPRESENTATION_ITEM('')
SURFACE()
);
#3198=(
BOUNDED_SURFACE()
B_SPLINE_SURFACE(3,2,((#406541,#406542,#406543),(#406544,#406545,#406546),
(#406547,#406548,#406549),(#406550,#406551,#406552)),.UNSPECIFIED.,.F.,
 .F.,.F.)
B_SPLINE_SURFACE_WITH_KNOTS((4,4),(3,3),(-3.79470760369927E-19,9.54361881492174E-5),
(0.,1.),.UNSPECIFIED.)
GEOMETRIC_REPRESENTATION_ITEM()
RATIONAL_B_SPLINE_SURFACE(((1.,0.814339887349195,1.),(1.,0.8151159593452,
1.),(1.,0.815907587407948,1.),(1.,0.816715621142048,1.)))
REPRESENTATION_ITEM('')
SURFACE()
);
#3199=(
BOUNDED_SURFACE()
B_SPLINE_SURFACE(3,2,((#406554,#406555,#406556),(#406557,#406558,#406559),
(#406560,#406561,#406562),(#406563,#406564,#406565)),.UNSPECIFIED.,.F.,
 .F.,.F.)
B_SPLINE_SURFACE_WITH_KNOTS((4,4),(3,3),(-3.39528393502476E-6,3.73481232852733E-5),
(-0.00165018033344203,1.),.UNSPECIFIED.)
GEOMETRIC_REPRESENTATION_ITEM()
RATIONAL_B_SPLINE_SURFACE(((1.0004835438557,0.853487571660372,1.),(1.00047110510925,
0.85725647685145,1.),(1.00053193201113,0.838826096655834,1.),(1.00063970687732,
0.806170615310065,1.)))
REPRESENTATION_ITEM('')
SURFACE()
);
#3200=(
BOUNDED_SURFACE()
B_SPLINE_SURFACE(3,2,((#406569,#406570,#406571),(#406572,#406573,#406574),
(#406575,#406576,#406577),(#406578,#406579,#406580)),.UNSPECIFIED.,.F.,
 .F.,.F.)
B_SPLINE_SURFACE_WITH_KNOTS((4,4),(3,3),(2.02993869230512E-5,5.39756952687121E-5),
(-0.000116281069696749,1.),.UNSPECIFIED.)
GEOMETRIC_REPRESENTATION_ITEM()
RATIONAL_B_SPLINE_SURFACE(((1.00001770479726,0.923870681143028,1.),(1.00001014104057,
0.956394275543456,1.),(1.00002037300274,0.912397594905636,1.),(1.00003390859462,
0.854195550869775,1.)))
REPRESENTATION_ITEM('')
SURFACE()
);
#3201=(
BOUNDED_SURFACE()
B_SPLINE_SURFACE(3,2,((#406673,#406674,#406675),(#406676,#406677,#406678),
(#406679,#406680,#406681),(#406682,#406683,#406684)),.UNSPECIFIED.,.F.,
 .F.,.F.)
B_SPLINE_SURFACE_WITH_KNOTS((4,4),(3,3),(0.00135801595889393,0.00148409170619832),
(0.,1.),.UNSPECIFIED.)
GEOMETRIC_REPRESENTATION_ITEM()
RATIONAL_B_SPLINE_SURFACE(((1.,0.818301933966447,1.),(1.,0.81722661317234,
1.),(1.,0.816179643373958,1.),(1.,0.815159387863653,1.)))
REPRESENTATION_ITEM('')
SURFACE()
);
#3202=(
BOUNDED_SURFACE()
B_SPLINE_SURFACE(3,2,((#406723,#406724,#406725),(#406726,#406727,#406728),
(#406729,#406730,#406731),(#406732,#406733,#406734)),.UNSPECIFIED.,.F.,
 .F.,.F.)
B_SPLINE_SURFACE_WITH_KNOTS((4,4),(3,3),(-1.54744435122086E-6,1.54744435122082E-5),
(-0.0151698983584593,1.),.UNSPECIFIED.)
GEOMETRIC_REPRESENTATION_ITEM()
RATIONAL_B_SPLINE_SURFACE(((1.02018382472462,0.334740937358951,1.),(1.00401234488727,
0.867753072813709,1.),(1.00033622856772,0.988917903080944,1.),(1.,1.,1.)))
REPRESENTATION_ITEM('')
SURFACE()
);
#3203=(
BOUNDED_SURFACE()
B_SPLINE_SURFACE(3,2,((#406736,#406737,#406738),(#406739,#406740,#406741),
(#406742,#406743,#406744),(#406745,#406746,#406747)),.UNSPECIFIED.,.F.,
 .F.,.F.)
B_SPLINE_SURFACE_WITH_KNOTS((4,4),(3,3),(0.00137194782501028,0.00149814269699235),
(0.,1.),.UNSPECIFIED.)
GEOMETRIC_REPRESENTATION_ITEM()
RATIONAL_B_SPLINE_SURFACE(((1.,0.815158509402315,1.),(1.,0.816179044148163,
1.),(1.,0.817226308119928,1.),(1.,0.818301939488807,1.)))
REPRESENTATION_ITEM('')
SURFACE()
);
#3204=(
BOUNDED_SURFACE()
B_SPLINE_SURFACE(3,2,((#406791,#406792,#406793),(#406794,#406795,#406796),
(#406797,#406798,#406799),(#406800,#406801,#406802)),.UNSPECIFIED.,.F.,
 .F.,.F.)
B_SPLINE_SURFACE_WITH_KNOTS((4,4),(3,3),(1.55009486301138E-5,4.92065510474432E-5),
(-8.13759515373864E-5,1.),.UNSPECIFIED.)
GEOMETRIC_REPRESENTATION_ITEM()
RATIONAL_B_SPLINE_SURFACE(((1.00002372912337,0.854200639599679,1.),(1.00001423585994,
0.912530301180528,1.),(1.00000710550471,0.956341495377432,1.),(1.00001238975909,
0.923873338137018,1.)))
REPRESENTATION_ITEM('')
SURFACE()
);
#3205=(
BOUNDED_SURFACE()
B_SPLINE_SURFACE(3,2,((#406806,#406807,#406808),(#406809,#406810,#406811),
(#406812,#406813,#406814),(#406815,#406816,#406817)),.UNSPECIFIED.,.F.,
 .F.,.F.)
B_SPLINE_SURFACE_WITH_KNOTS((4,4),(3,3),(-3.39934179457858E-6,3.73927597403565E-5),
(-0.00186004067447938,1.00069373317472),.UNSPECIFIED.)
GEOMETRIC_REPRESENTATION_ITEM()
RATIONAL_B_SPLINE_SURFACE(((1.00072100136066,0.806051963875218,1.00026859642704),
(1.00060048440163,0.838470803558548,1.00022369994506),(1.00053106448803,
0.857144632272291,1.00019783877229),(1.00054515072861,0.853355459539002,
1.00020308635446)))
REPRESENTATION_ITEM('')
SURFACE()
);
#3206=(
BOUNDED_SURFACE()
B_SPLINE_SURFACE(3,2,((#406819,#406820,#406821),(#406822,#406823,#406824),
(#406825,#406826,#406827),(#406828,#406829,#406830)),.UNSPECIFIED.,.F.,
 .F.,.F.)
B_SPLINE_SURFACE_WITH_KNOTS((4,4),(3,3),(-5.42101086242752E-20,9.54361881492173E-5),
(0.,1.),.UNSPECIFIED.)
GEOMETRIC_REPRESENTATION_ITEM()
RATIONAL_B_SPLINE_SURFACE(((1.,0.81671562114205,1.),(1.,0.815907587407935,
1.),(1.,0.815115959345209,1.),(1.,0.814339887349193,1.)))
REPRESENTATION_ITEM('')
SURFACE()
);
#3207=(
BOUNDED_SURFACE()
B_SPLINE_SURFACE(3,2,((#406832,#406833,#406834),(#406835,#406836,#406837),
(#406838,#406839,#406840),(#406841,#406842,#406843)),.UNSPECIFIED.,.F.,
 .F.,.F.)
B_SPLINE_SURFACE_WITH_KNOTS((4,4),(3,3),(9.14795583034644E-20,4.68197758448201E-5),
(0.,1.),.UNSPECIFIED.)
GEOMETRIC_REPRESENTATION_ITEM()
RATIONAL_B_SPLINE_SURFACE(((1.,0.816715621142048,1.),(1.,0.953638980025215,
1.),(1.,0.954506925408048,1.),(1.,0.81671562114206,1.)))
REPRESENTATION_ITEM('')
SURFACE()
);
#3208=(
BOUNDED_SURFACE()
B_SPLINE_SURFACE(3,2,((#406845,#406846,#406847),(#406848,#406849,#406850),
(#406851,#406852,#406853),(#406854,#406855,#406856)),.UNSPECIFIED.,.F.,
 .F.,.F.)
B_SPLINE_SURFACE_WITH_KNOTS((4,4),(3,3),(0.,9.54361881492178E-5),(0.,1.),
 .UNSPECIFIED.)
GEOMETRIC_REPRESENTATION_ITEM()
RATIONAL_B_SPLINE_SURFACE(((1.,0.814339887349195,1.),(1.,0.815115959345203,
1.),(1.,0.815907587407945,1.),(1.,0.816715621142048,1.)))
REPRESENTATION_ITEM('')
SURFACE()
);
#3209=(
BOUNDED_SURFACE()
B_SPLINE_SURFACE(3,2,((#406858,#406859,#406860),(#406861,#406862,#406863),
(#406864,#406865,#406866),(#406867,#406868,#406869)),.UNSPECIFIED.,.F.,
 .F.,.F.)
B_SPLINE_SURFACE_WITH_KNOTS((4,4),(3,3),(-3.39528393502485E-6,3.73481232852737E-5),
(-0.001650180332763,1.),.UNSPECIFIED.)
GEOMETRIC_REPRESENTATION_ITEM()
RATIONAL_B_SPLINE_SURFACE(((1.0004835438555,0.853487571660472,1.),(1.00047110510906,
0.857256476851533,1.),(1.00053193201091,0.838826096655957,1.),(1.00063970687705,
0.806170615310193,0.999999999999999)))
REPRESENTATION_ITEM('')
SURFACE()
);
#3210=(
BOUNDED_SURFACE()
B_SPLINE_SURFACE(3,2,((#406873,#406874,#406875),(#406876,#406877,#406878),
(#406879,#406880,#406881),(#406882,#406883,#406884)),.UNSPECIFIED.,.F.,
 .F.,.F.)
B_SPLINE_SURFACE_WITH_KNOTS((4,4),(3,3),(2.02993869230511E-5,5.39756952687121E-5),
(-0.000116281069947723,1.),.UNSPECIFIED.)
GEOMETRIC_REPRESENTATION_ITEM()
RATIONAL_B_SPLINE_SURFACE(((1.0000177047973,0.923870681143008,1.),(1.00001014104059,
0.956394275543438,1.),(1.00002037300279,0.912397594905621,1.),(1.0000339085947,
0.854195550869734,1.)))
REPRESENTATION_ITEM('')
SURFACE()
);
#3211=(
BOUNDED_SURFACE()
B_SPLINE_SURFACE(3,2,((#406977,#406978,#406979),(#406980,#406981,#406982),
(#406983,#406984,#406985),(#406986,#406987,#406988)),.UNSPECIFIED.,.F.,
 .F.,.F.)
B_SPLINE_SURFACE_WITH_KNOTS((4,4),(3,3),(0.00135801595889393,0.00148409170619832),
(0.,1.),.UNSPECIFIED.)
GEOMETRIC_REPRESENTATION_ITEM()
RATIONAL_B_SPLINE_SURFACE(((1.,0.818301933966446,1.),(1.,0.817226613172351,
1.),(1.,0.816179643373943,1.),(1.,0.815159387863657,1.)))
REPRESENTATION_ITEM('')
SURFACE()
);
#3212=(
BOUNDED_SURFACE()
B_SPLINE_SURFACE(3,2,((#407027,#407028,#407029),(#407030,#407031,#407032),
(#407033,#407034,#407035),(#407036,#407037,#407038)),.UNSPECIFIED.,.F.,
 .F.,.F.)
B_SPLINE_SURFACE_WITH_KNOTS((4,4),(3,3),(-1.54744435122082E-6,1.5474443512208E-5),
(-0.0151698983592207,1.01516989836348),.UNSPECIFIED.)
GEOMETRIC_REPRESENTATION_ITEM()
RATIONAL_B_SPLINE_SURFACE(((1.02018382472565,0.324498219413281,1.02018382473139),
(1.00401234488747,0.865716921710482,1.00401234488862),(1.00033622856774,
0.98874727662973,1.00033622856783),(1.,1.,1.)))
REPRESENTATION_ITEM('')
SURFACE()
);
#3213=(
BOUNDED_SURFACE()
B_SPLINE_SURFACE(3,2,((#407040,#407041,#407042),(#407043,#407044,#407045),
(#407046,#407047,#407048),(#407049,#407050,#407051)),.UNSPECIFIED.,.F.,
 .F.,.F.)
B_SPLINE_SURFACE_WITH_KNOTS((4,4),(3,3),(0.00137194782501028,0.00149814269699235),
(0.,1.),.UNSPECIFIED.)
GEOMETRIC_REPRESENTATION_ITEM()
RATIONAL_B_SPLINE_SURFACE(((1.,0.815158509402314,1.),(1.,0.816179044148161,
1.),(1.,0.817226308119928,1.),(1.,0.818301939488807,1.)))
REPRESENTATION_ITEM('')
SURFACE()
);
#3214=(
BOUNDED_SURFACE()
B_SPLINE_SURFACE(3,2,((#407095,#407096,#407097),(#407098,#407099,#407100),
(#407101,#407102,#407103),(#407104,#407105,#407106)),.UNSPECIFIED.,.F.,
 .F.,.F.)
B_SPLINE_SURFACE_WITH_KNOTS((4,4),(3,3),(1.55009486301137E-5,4.92065510474436E-5),
(-8.13759513776842E-5,1.),.UNSPECIFIED.)
GEOMETRIC_REPRESENTATION_ITEM()
RATIONAL_B_SPLINE_SURFACE(((1.00002372912333,0.854200639599703,1.),(1.00001423585992,
0.912530301180543,1.),(1.0000071055047,0.956341495377434,1.),(1.00001238975907,
0.92387333813703,1.)))
REPRESENTATION_ITEM('')
SURFACE()
);
#3215=(
BOUNDED_SURFACE()
B_SPLINE_SURFACE(3,2,((#407110,#407111,#407112),(#407113,#407114,#407115),
(#407116,#407117,#407118),(#407119,#407120,#407121)),.UNSPECIFIED.,.F.,
 .F.,.F.)
B_SPLINE_SURFACE_WITH_KNOTS((4,4),(3,3),(-3.39934179457812E-6,3.73927597403563E-5),
(-0.00186004067419253,1.00069373317458),.UNSPECIFIED.)
GEOMETRIC_REPRESENTATION_ITEM()
RATIONAL_B_SPLINE_SURFACE(((1.00072100136055,0.806051963875307,1.00026859642698),
(1.00060048440154,0.838470803558622,1.00022369994502),(1.00053106448795,
0.85714463227235,1.00019783877225),(1.00054515072852,0.853355459539066,
1.00020308635442)))
REPRESENTATION_ITEM('')
SURFACE()
);
#3216=(
BOUNDED_SURFACE()
B_SPLINE_SURFACE(3,2,((#407123,#407124,#407125),(#407126,#407127,#407128),
(#407129,#407130,#407131),(#407132,#407133,#407134)),.UNSPECIFIED.,.F.,
 .F.,.F.)
B_SPLINE_SURFACE_WITH_KNOTS((4,4),(3,3),(1.0842021724855E-19,9.54361881492175E-5),
(0.,1.),.UNSPECIFIED.)
GEOMETRIC_REPRESENTATION_ITEM()
RATIONAL_B_SPLINE_SURFACE(((1.,0.816715621142052,1.),(1.,0.815907587407936,
1.),(1.,0.815115959345211,1.),(1.,0.814339887349192,1.)))
REPRESENTATION_ITEM('')
SURFACE()
);
#3217=(
BOUNDED_SURFACE()
B_SPLINE_SURFACE(3,2,((#407136,#407137,#407138),(#407139,#407140,#407141),
(#407142,#407143,#407144),(#407145,#407146,#407147)),.UNSPECIFIED.,.F.,
 .F.,.F.)
B_SPLINE_SURFACE_WITH_KNOTS((4,4),(3,3),(-2.50721752387273E-19,4.68197758448202E-5),
(0.,1.),.UNSPECIFIED.)
GEOMETRIC_REPRESENTATION_ITEM()
RATIONAL_B_SPLINE_SURFACE(((1.,0.816715621142048,1.),(1.,0.953638980025203,
1.),(1.,0.95450692540806,1.),(1.,0.816715621142054,1.)))
REPRESENTATION_ITEM('')
SURFACE()
);
#3218=(
BOUNDED_SURFACE()
B_SPLINE_SURFACE(3,2,((#407149,#407150,#407151),(#407152,#407153,#407154),
(#407155,#407156,#407157),(#407158,#407159,#407160)),.UNSPECIFIED.,.F.,
 .F.,.F.)
B_SPLINE_SURFACE_WITH_KNOTS((4,4),(3,3),(2.16840434497101E-19,9.54361881492177E-5),
(0.,1.),.UNSPECIFIED.)
GEOMETRIC_REPRESENTATION_ITEM()
RATIONAL_B_SPLINE_SURFACE(((1.,0.81433988734919,1.),(1.,0.815115959345201,
1.),(1.,0.81590758740794,1.),(1.,0.816715621142048,1.)))
REPRESENTATION_ITEM('')
SURFACE()
);
#3219=(
BOUNDED_SURFACE()
B_SPLINE_SURFACE(3,2,((#407162,#407163,#407164),(#407165,#407166,#407167),
(#407168,#407169,#407170),(#407171,#407172,#407173)),.UNSPECIFIED.,.F.,
 .F.,.F.)
B_SPLINE_SURFACE_WITH_KNOTS((4,4),(3,3),(-3.39528393502494E-6,3.73481232852734E-5),
(-0.00165018033333615,1.),.UNSPECIFIED.)
GEOMETRIC_REPRESENTATION_ITEM()
RATIONAL_B_SPLINE_SURFACE(((1.00048354385567,0.853487571660389,1.),(1.00047110510922,
0.857256476851451,1.),(1.00053193201109,0.838826096655853,1.),(1.00063970687728,
0.806170615310085,1.)))
REPRESENTATION_ITEM('')
SURFACE()
);
#3220=(
BOUNDED_SURFACE()
B_SPLINE_SURFACE(3,2,((#407177,#407178,#407179),(#407180,#407181,#407182),
(#407183,#407184,#407185),(#407186,#407187,#407188)),.UNSPECIFIED.,.F.,
 .F.,.F.)
B_SPLINE_SURFACE_WITH_KNOTS((4,4),(3,3),(2.02993869230512E-5,5.39756952687125E-5),
(-0.000116281069885172,1.),.UNSPECIFIED.)
GEOMETRIC_REPRESENTATION_ITEM()
RATIONAL_B_SPLINE_SURFACE(((1.00001770479729,0.923870681143012,1.),(1.00001014104059,
0.956394275543446,1.),(1.00002037300278,0.912397594905608,1.),(1.00003390859468,
0.854195550869753,1.)))
REPRESENTATION_ITEM('')
SURFACE()
);
#3221=(
BOUNDED_SURFACE()
B_SPLINE_SURFACE(3,2,((#407281,#407282,#407283),(#407284,#407285,#407286),
(#407287,#407288,#407289),(#407290,#407291,#407292)),.UNSPECIFIED.,.F.,
 .F.,.F.)
B_SPLINE_SURFACE_WITH_KNOTS((4,4),(3,3),(0.00135801595889393,0.00148409170619832),
(0.,1.),.UNSPECIFIED.)
GEOMETRIC_REPRESENTATION_ITEM()
RATIONAL_B_SPLINE_SURFACE(((1.,0.818301933966446,1.),(1.,0.817226613172354,
1.),(1.,0.816179643373942,1.),(1.,0.815159387863656,1.)))
REPRESENTATION_ITEM('')
SURFACE()
);
#3222=(
BOUNDED_SURFACE()
B_SPLINE_SURFACE(3,2,((#407331,#407332,#407333),(#407334,#407335,#407336),
(#407337,#407338,#407339),(#407340,#407341,#407342)),.UNSPECIFIED.,.F.,
 .F.,.F.)
B_SPLINE_SURFACE_WITH_KNOTS((4,4),(3,3),(-1.54744435122079E-6,1.54744435122076E-5),
(-0.0151698983713926,1.),.UNSPECIFIED.)
GEOMETRIC_REPRESENTATION_ITEM()
RATIONAL_B_SPLINE_SURFACE(((1.02018382474208,0.334740937350454,1.),(1.00401234489074,
0.867753072812112,1.),(1.00033622856801,0.988917903080724,1.),(1.,1.,1.)))
REPRESENTATION_ITEM('')
SURFACE()
);
#3223=(
BOUNDED_SURFACE()
B_SPLINE_SURFACE(3,2,((#407344,#407345,#407346),(#407347,#407348,#407349),
(#407350,#407351,#407352),(#407353,#407354,#407355)),.UNSPECIFIED.,.F.,
 .F.,.F.)
B_SPLINE_SURFACE_WITH_KNOTS((4,4),(3,3),(0.00137194782501028,0.00149814269699235),
(0.,1.),.UNSPECIFIED.)
GEOMETRIC_REPRESENTATION_ITEM()
RATIONAL_B_SPLINE_SURFACE(((1.,0.815158509402318,1.),(1.,0.816179044148164,
1.),(1.,0.817226308119933,1.),(1.,0.818301939488801,1.)))
REPRESENTATION_ITEM('')
SURFACE()
);
#3224=(
BOUNDED_SURFACE()
B_SPLINE_SURFACE(3,2,((#407399,#407400,#407401),(#407402,#407403,#407404),
(#407405,#407406,#407407),(#407408,#407409,#407410)),.UNSPECIFIED.,.F.,
 .F.,.F.)
B_SPLINE_SURFACE_WITH_KNOTS((4,4),(3,3),(1.55009486301138E-5,4.92065510474433E-5),
(-8.13759511895836E-5,1.),.UNSPECIFIED.)
GEOMETRIC_REPRESENTATION_ITEM()
RATIONAL_B_SPLINE_SURFACE(((1.00002372912327,0.854200639599731,1.),(1.00001423585988,
0.91253030118056,1.),(1.00000710550468,0.956341495377448,1.),(1.00001238975904,
0.923873338137045,1.)))
REPRESENTATION_ITEM('')
SURFACE()
);
#3225=(
BOUNDED_SURFACE()
B_SPLINE_SURFACE(3,2,((#407414,#407415,#407416),(#407417,#407418,#407419),
(#407420,#407421,#407422),(#407423,#407424,#407425)),.UNSPECIFIED.,.F.,
 .F.,.F.)
B_SPLINE_SURFACE_WITH_KNOTS((4,4),(3,3),(-3.39934179457792E-6,3.73927597403563E-5),
(-0.00186004067408231,1.00069373317463),.UNSPECIFIED.)
GEOMETRIC_REPRESENTATION_ITEM()
RATIONAL_B_SPLINE_SURFACE(((1.00072100136051,0.806051963875312,1.000268596427),
(1.00060048440151,0.838470803558632,1.00022369994503),(1.00053106448792,
0.857144632272357,1.00019783877226),(1.00054515072849,0.853355459539082,
1.00020308635444)))
REPRESENTATION_ITEM('')
SURFACE()
);
#3226=(
BOUNDED_SURFACE()
B_SPLINE_SURFACE(3,2,((#407427,#407428,#407429),(#407430,#407431,#407432),
(#407433,#407434,#407435),(#407436,#407437,#407438)),.UNSPECIFIED.,.F.,
 .F.,.F.)
B_SPLINE_SURFACE_WITH_KNOTS((4,4),(3,3),(2.71050543121376E-19,9.54361881492175E-5),
(0.,1.),.UNSPECIFIED.)
GEOMETRIC_REPRESENTATION_ITEM()
RATIONAL_B_SPLINE_SURFACE(((1.,0.81671562114205,1.),(1.,0.81590758740794,
1.),(1.,0.815115959345207,1.),(1.,0.814339887349193,1.)))
REPRESENTATION_ITEM('')
SURFACE()
);
#3227=(
BOUNDED_SURFACE()
B_SPLINE_SURFACE(3,2,((#407440,#407441,#407442),(#407443,#407444,#407445),
(#407446,#407447,#407448),(#407449,#407450,#407451)),.UNSPECIFIED.,.F.,
 .F.,.F.)
B_SPLINE_SURFACE_WITH_KNOTS((4,4),(3,3),(-2.71050543121376E-20,4.68197758448206E-5),
(0.,1.),.UNSPECIFIED.)
GEOMETRIC_REPRESENTATION_ITEM()
RATIONAL_B_SPLINE_SURFACE(((1.,0.816715621142048,1.),(1.,0.953638980025207,
1.),(1.,0.954506925408056,1.),(1.,0.81671562114205,1.)))
REPRESENTATION_ITEM('')
SURFACE()
);
#3228=(
BOUNDED_SURFACE()
B_SPLINE_SURFACE(3,2,((#407453,#407454,#407455),(#407456,#407457,#407458),
(#407459,#407460,#407461),(#407462,#407463,#407464)),.UNSPECIFIED.,.F.,
 .F.,.F.)
B_SPLINE_SURFACE_WITH_KNOTS((4,4),(3,3),(0.,9.54361881492175E-5),(0.,1.),
 .UNSPECIFIED.)
GEOMETRIC_REPRESENTATION_ITEM()
RATIONAL_B_SPLINE_SURFACE(((1.,0.814339887349194,1.),(1.,0.815115959345203,
1.),(1.,0.815907587407944,1.),(1.,0.816715621142048,1.)))
REPRESENTATION_ITEM('')
SURFACE()
);
#3229=(
BOUNDED_SURFACE()
B_SPLINE_SURFACE(3,2,((#407466,#407467,#407468),(#407469,#407470,#407471),
(#407472,#407473,#407474),(#407475,#407476,#407477)),.UNSPECIFIED.,.F.,
 .F.,.F.)
B_SPLINE_SURFACE_WITH_KNOTS((4,4),(3,3),(-3.39528393502488E-6,3.7348123285273E-5),
(-0.00165018033331949,1.),.UNSPECIFIED.)
GEOMETRIC_REPRESENTATION_ITEM()
RATIONAL_B_SPLINE_SURFACE(((1.00048354385567,0.853487571660389,1.),(1.00047110510922,
0.857256476851462,1.),(1.00053193201109,0.838826096655859,1.),(1.00063970687727,
0.806170615310095,1.)))
REPRESENTATION_ITEM('')
SURFACE()
);
#3230=(
BOUNDED_SURFACE()
B_SPLINE_SURFACE(3,2,((#407481,#407482,#407483),(#407484,#407485,#407486),
(#407487,#407488,#407489),(#407490,#407491,#407492)),.UNSPECIFIED.,.F.,
 .F.,.F.)
B_SPLINE_SURFACE_WITH_KNOTS((4,4),(3,3),(2.02993869230515E-5,5.39756952687123E-5),
(-0.000116281070470176,1.),.UNSPECIFIED.)
GEOMETRIC_REPRESENTATION_ITEM()
RATIONAL_B_SPLINE_SURFACE(((1.00001770479738,0.923870681142967,1.),(1.00001014104064,
0.95639427554342,1.),(1.00002037300288,0.912397594905563,1.),(1.00003390859485,
0.854195550869658,1.)))
REPRESENTATION_ITEM('')
SURFACE()
);
#3231=(
BOUNDED_SURFACE()
B_SPLINE_SURFACE(3,2,((#407585,#407586,#407587),(#407588,#407589,#407590),
(#407591,#407592,#407593),(#407594,#407595,#407596)),.UNSPECIFIED.,.F.,
 .F.,.F.)
B_SPLINE_SURFACE_WITH_KNOTS((4,4),(3,3),(0.00135801595889393,0.00148409170619832),
(0.,1.),.UNSPECIFIED.)
GEOMETRIC_REPRESENTATION_ITEM()
RATIONAL_B_SPLINE_SURFACE(((1.,0.818301933966439,1.),(1.,0.817226613172349,
1.),(1.,0.816179643373947,1.),(1.,0.815159387863649,1.)))
REPRESENTATION_ITEM('')
SURFACE()
);
#3232=(
BOUNDED_SURFACE()
B_SPLINE_SURFACE(3,2,((#407635,#407636,#407637),(#407638,#407639,#407640),
(#407641,#407642,#407643),(#407644,#407645,#407646)),.UNSPECIFIED.,.F.,
 .F.,.F.)
B_SPLINE_SURFACE_WITH_KNOTS((4,4),(3,3),(1.24937359720009E-20,1.5474443512209E-5),
(0.,1.),.UNSPECIFIED.)
GEOMETRIC_REPRESENTATION_ITEM()
RATIONAL_B_SPLINE_SURFACE(((1.,0.478041569704913,1.),(1.,0.890533857551977,
1.),(1.,0.990075913815931,1.),(1.,1.,1.)))
REPRESENTATION_ITEM('')
SURFACE()
);
#3233=(
BOUNDED_SURFACE()
B_SPLINE_SURFACE(3,2,((#407648,#407649,#407650),(#407651,#407652,#407653),
(#407654,#407655,#407656),(#407657,#407658,#407659)),.UNSPECIFIED.,.F.,
 .F.,.F.)
B_SPLINE_SURFACE_WITH_KNOTS((4,4),(3,3),(0.00137194782501028,0.00149814269699235),
(0.,1.),.UNSPECIFIED.)
GEOMETRIC_REPRESENTATION_ITEM()
RATIONAL_B_SPLINE_SURFACE(((1.,0.81515850940232,1.),(1.,0.816179044148162,
1.),(1.,0.817226308119929,1.),(1.,0.818301939488808,1.)))
REPRESENTATION_ITEM('')
SURFACE()
);
#3234=(
BOUNDED_SURFACE()
B_SPLINE_SURFACE(3,2,((#407703,#407704,#407705),(#407706,#407707,#407708),
(#407709,#407710,#407711),(#407712,#407713,#407714)),.UNSPECIFIED.,.F.,
 .F.,.F.)
B_SPLINE_SURFACE_WITH_KNOTS((4,4),(3,3),(1.55009486301137E-5,4.9206551047444E-5),
(-8.13759515126626E-5,1.),.UNSPECIFIED.)
GEOMETRIC_REPRESENTATION_ITEM()
RATIONAL_B_SPLINE_SURFACE(((1.00002372912336,0.854200639599676,1.),(1.00001423585994,
0.912530301180537,1.),(1.00000710550471,0.956341495377424,1.),(1.00001238975909,
0.923873338137019,1.)))
REPRESENTATION_ITEM('')
SURFACE()
);
#3235=(
BOUNDED_SURFACE()
B_SPLINE_SURFACE(3,2,((#407718,#407719,#407720),(#407721,#407722,#407723),
(#407724,#407725,#407726),(#407727,#407728,#407729)),.UNSPECIFIED.,.F.,
 .F.,.F.)
B_SPLINE_SURFACE_WITH_KNOTS((4,4),(3,3),(-3.39934179457807E-6,3.73927597403565E-5),
(-0.00186004067470178,1.00069373317451),.UNSPECIFIED.)
GEOMETRIC_REPRESENTATION_ITEM()
RATIONAL_B_SPLINE_SURFACE(((1.00072100136075,0.806051963875235,1.00026859642695),
(1.00060048440171,0.838470803558528,1.00022369994499),(1.00053106448809,
0.85714463227229,1.00019783877223),(1.00054515072867,0.853355459539005,
1.0002030863544)))
REPRESENTATION_ITEM('')
SURFACE()
);
#3236=(
BOUNDED_SURFACE()
B_SPLINE_SURFACE(3,2,((#407731,#407732,#407733),(#407734,#407735,#407736),
(#407737,#407738,#407739),(#407740,#407741,#407742)),.UNSPECIFIED.,.F.,
 .F.,.F.)
B_SPLINE_SURFACE_WITH_KNOTS((4,4),(3,3),(2.16840434497101E-19,9.54361881492175E-5),
(0.,1.),.UNSPECIFIED.)
GEOMETRIC_REPRESENTATION_ITEM()
RATIONAL_B_SPLINE_SURFACE(((1.,0.816715621142047,1.),(1.,0.815907587407948,
1.),(1.,0.815115959345199,1.),(1.,0.814339887349196,1.)))
REPRESENTATION_ITEM('')
SURFACE()
);
#3237=(
BOUNDED_SURFACE()
B_SPLINE_SURFACE(3,2,((#407744,#407745,#407746),(#407747,#407748,#407749),
(#407750,#407751,#407752),(#407753,#407754,#407755)),.UNSPECIFIED.,.F.,
 .F.,.F.)
B_SPLINE_SURFACE_WITH_KNOTS((4,4),(3,3),(1.71100655345369E-19,4.68197758448206E-5),
(0.,1.),.UNSPECIFIED.)
GEOMETRIC_REPRESENTATION_ITEM()
RATIONAL_B_SPLINE_SURFACE(((1.,0.816715621142055,1.),(1.,0.9536389800252,
1.),(1.,0.95450692540806,1.),(1.,0.816715621142053,1.)))
REPRESENTATION_ITEM('')
SURFACE()
);
#3238=(
BOUNDED_SURFACE()
B_SPLINE_SURFACE(3,2,((#407757,#407758,#407759),(#407760,#407761,#407762),
(#407763,#407764,#407765),(#407766,#407767,#407768)),.UNSPECIFIED.,.F.,
 .F.,.F.)
B_SPLINE_SURFACE_WITH_KNOTS((4,4),(3,3),(-1.62630325872826E-19,9.54361881492177E-5),
(0.,1.),.UNSPECIFIED.)
GEOMETRIC_REPRESENTATION_ITEM()
RATIONAL_B_SPLINE_SURFACE(((1.,0.814339887349195,1.),(1.,0.81511595934521,
1.),(1.,0.815907587407946,1.),(1.,0.816715621142055,1.)))
REPRESENTATION_ITEM('')
SURFACE()
);
#3239=(
BOUNDED_SURFACE()
B_SPLINE_SURFACE(3,2,((#407770,#407771,#407772),(#407773,#407774,#407775),
(#407776,#407777,#407778),(#407779,#407780,#407781)),.UNSPECIFIED.,.F.,
 .F.,.F.)
B_SPLINE_SURFACE_WITH_KNOTS((4,4),(3,3),(-3.3952839350238E-6,3.73481232852729E-5),
(-0.00165018033326818,1.),.UNSPECIFIED.)
GEOMETRIC_REPRESENTATION_ITEM()
RATIONAL_B_SPLINE_SURFACE(((1.00048354385565,0.853487571660405,1.),(1.0004711051092,
0.85725647685147,1.),(1.00053193201107,0.838826096655865,1.),(1.00063970687725,
0.806170615310107,1.)))
REPRESENTATION_ITEM('')
SURFACE()
);
#3240=(
BOUNDED_SURFACE()
B_SPLINE_SURFACE(3,2,((#407785,#407786,#407787),(#407788,#407789,#407790),
(#407791,#407792,#407793),(#407794,#407795,#407796)),.UNSPECIFIED.,.F.,
 .F.,.F.)
B_SPLINE_SURFACE_WITH_KNOTS((4,4),(3,3),(2.02993869230506E-5,5.39756952687124E-5),
(-0.000116281069760664,1.),.UNSPECIFIED.)
GEOMETRIC_REPRESENTATION_ITEM()
RATIONAL_B_SPLINE_SURFACE(((1.00001770479727,0.923870681143024,1.),(1.00001014104057,
0.956394275543451,1.),(1.00002037300276,0.912397594905623,1.),(1.00003390859464,
0.854195550869758,1.)))
REPRESENTATION_ITEM('')
SURFACE()
);
#3241=(
BOUNDED_SURFACE()
B_SPLINE_SURFACE(3,2,((#407889,#407890,#407891),(#407892,#407893,#407894),
(#407895,#407896,#407897),(#407898,#407899,#407900)),.UNSPECIFIED.,.F.,
 .F.,.F.)
B_SPLINE_SURFACE_WITH_KNOTS((4,4),(3,3),(0.00135801595889393,0.00148409170619832),
(0.,1.),.UNSPECIFIED.)
GEOMETRIC_REPRESENTATION_ITEM()
RATIONAL_B_SPLINE_SURFACE(((1.,0.818301933966445,1.),(1.,0.817226613172328,
1.),(1.,0.816179643373974,1.),(1.,0.815159387863655,1.)))
REPRESENTATION_ITEM('')
SURFACE()
);
#3242=(
BOUNDED_SURFACE()
B_SPLINE_SURFACE(3,2,((#407939,#407940,#407941),(#407942,#407943,#407944),
(#407945,#407946,#407947),(#407948,#407949,#407950)),.UNSPECIFIED.,.F.,
 .F.,.F.)
B_SPLINE_SURFACE_WITH_KNOTS((4,4),(3,3),(-1.5474443512208E-6,1.54744435122079E-5),
(-0.0151698983581421,1.),.UNSPECIFIED.)
GEOMETRIC_REPRESENTATION_ITEM()
RATIONAL_B_SPLINE_SURFACE(((1.02018382472419,0.334740937359151,1.),(1.00401234488718,
0.86775307281386,1.),(1.00033622856772,0.988917903080911,1.),(1.,1.,1.)))
REPRESENTATION_ITEM('')
SURFACE()
);
#3243=(
BOUNDED_SURFACE()
B_SPLINE_SURFACE(3,2,((#407952,#407953,#407954),(#407955,#407956,#407957),
(#407958,#407959,#407960),(#407961,#407962,#407963)),.UNSPECIFIED.,.F.,
 .F.,.F.)
B_SPLINE_SURFACE_WITH_KNOTS((4,4),(3,3),(0.00137194782501028,0.00149814269699235),
(0.,1.),.UNSPECIFIED.)
GEOMETRIC_REPRESENTATION_ITEM()
RATIONAL_B_SPLINE_SURFACE(((1.,0.815158509402316,1.),(1.,0.816179044148151,
1.),(1.,0.817226308119921,1.),(1.,0.818301939488809,1.)))
REPRESENTATION_ITEM('')
SURFACE()
);
#3244=(
BOUNDED_SURFACE()
B_SPLINE_SURFACE(3,2,((#408007,#408008,#408009),(#408010,#408011,#408012),
(#408013,#408014,#408015),(#408016,#408017,#408018)),.UNSPECIFIED.,.F.,
 .F.,.F.)
B_SPLINE_SURFACE_WITH_KNOTS((4,4),(3,3),(1.55009486301138E-5,4.92065510474427E-5),
(-8.13759513980918E-5,1.),.UNSPECIFIED.)
GEOMETRIC_REPRESENTATION_ITEM()
RATIONAL_B_SPLINE_SURFACE(((1.00002372912333,0.854200639599699,1.),(1.00001423585992,
0.912530301180542,1.),(1.0000071055047,0.956341495377437,1.),(1.00001238975907,
0.923873338137028,1.)))
REPRESENTATION_ITEM('')
SURFACE()
);
#3245=(
BOUNDED_SURFACE()
B_SPLINE_SURFACE(3,2,((#408022,#408023,#408024),(#408025,#408026,#408027),
(#408028,#408029,#408030),(#408031,#408032,#408033)),.UNSPECIFIED.,.F.,
 .F.,.F.)
B_SPLINE_SURFACE_WITH_KNOTS((4,4),(3,3),(-3.3993417945781E-6,3.73927597403565E-5),
(-0.00186004067393523,1.00069373317419),.UNSPECIFIED.)
GEOMETRIC_REPRESENTATION_ITEM()
RATIONAL_B_SPLINE_SURFACE(((1.00072100136045,0.806051963875439,1.00026859642683),
(1.00060048440146,0.838470803558701,1.00022369994489),(1.00053106448788,
0.857144632272456,1.00019783877214),(1.00054515072845,0.853355459539164,
1.00020308635431)))
REPRESENTATION_ITEM('')
SURFACE()
);
#3246=(
BOUNDED_SURFACE()
B_SPLINE_SURFACE(3,2,((#408035,#408036,#408037),(#408038,#408039,#408040),
(#408041,#408042,#408043),(#408044,#408045,#408046)),.UNSPECIFIED.,.F.,
 .F.,.F.)
B_SPLINE_SURFACE_WITH_KNOTS((4,4),(3,3),(-1.62630325872826E-19,9.54361881492173E-5),
(0.,1.),.UNSPECIFIED.)
GEOMETRIC_REPRESENTATION_ITEM()
RATIONAL_B_SPLINE_SURFACE(((1.,0.81671562114205,1.),(1.,0.815907587407941,
1.),(1.,0.815115959345208,1.),(1.,0.814339887349192,1.)))
REPRESENTATION_ITEM('')
SURFACE()
);
#3247=(
BOUNDED_SURFACE()
B_SPLINE_SURFACE(3,2,((#408048,#408049,#408050),(#408051,#408052,#408053),
(#408054,#408055,#408056),(#408057,#408058,#408059)),.UNSPECIFIED.,.F.,
 .F.,.F.)
B_SPLINE_SURFACE_WITH_KNOTS((4,4),(3,3),(7.45388993583784E-20,4.68197758448203E-5),
(0.,1.),.UNSPECIFIED.)
GEOMETRIC_REPRESENTATION_ITEM()
RATIONAL_B_SPLINE_SURFACE(((1.,0.816715621142041,1.),(1.,0.953638980025206,
1.),(1.,0.954506925408059,1.),(1.,0.816715621142055,1.)))
REPRESENTATION_ITEM('')
SURFACE()
);
#3248=(
BOUNDED_SURFACE()
B_SPLINE_SURFACE(3,2,((#408061,#408062,#408063),(#408064,#408065,#408066),
(#408067,#408068,#408069),(#408070,#408071,#408072)),.UNSPECIFIED.,.F.,
 .F.,.F.)
B_SPLINE_SURFACE_WITH_KNOTS((4,4),(3,3),(-1.0842021724855E-19,9.54361881492176E-5),
(0.,1.),.UNSPECIFIED.)
GEOMETRIC_REPRESENTATION_ITEM()
RATIONAL_B_SPLINE_SURFACE(((1.,0.814339887349189,1.),(1.,0.815115959345212,
1.),(1.,0.815907587407938,1.),(1.,0.816715621142046,1.)))
REPRESENTATION_ITEM('')
SURFACE()
);
#3249=(
BOUNDED_SURFACE()
B_SPLINE_SURFACE(3,2,((#408074,#408075,#408076),(#408077,#408078,#408079),
(#408080,#408081,#408082),(#408083,#408084,#408085)),.UNSPECIFIED.,.F.,
 .F.,.F.)
B_SPLINE_SURFACE_WITH_KNOTS((4,4),(3,3),(-3.39528393502485E-6,3.73481232852729E-5),
(-0.00165018033279177,1.),.UNSPECIFIED.)
GEOMETRIC_REPRESENTATION_ITEM()
RATIONAL_B_SPLINE_SURFACE(((1.00048354385551,0.853487571660467,1.),(1.00047110510907,
0.857256476851533,1.),(1.00053193201091,0.838826096655952,1.),(1.00063970687706,
0.806170615310181,0.999999999999999)))
REPRESENTATION_ITEM('')
SURFACE()
);
#3250=(
BOUNDED_SURFACE()
B_SPLINE_SURFACE(3,2,((#408089,#408090,#408091),(#408092,#408093,#408094),
(#408095,#408096,#408097),(#408098,#408099,#408100)),.UNSPECIFIED.,.F.,
 .F.,.F.)
B_SPLINE_SURFACE_WITH_KNOTS((4,4),(3,3),(2.0299386923051E-5,5.39756952686906E-5),
(-0.000116281069637203,1.),.UNSPECIFIED.)
GEOMETRIC_REPRESENTATION_ITEM()
RATIONAL_B_SPLINE_SURFACE(((1.00001770479725,0.92387068114303,1.),(1.00001014104056,
0.956394275543433,1.),(1.00002037300273,0.912397594905709,1.),(1.00003390859461,
0.854195550869884,1.)))
REPRESENTATION_ITEM('')
SURFACE()
);
#3251=(
BOUNDED_SURFACE()
B_SPLINE_SURFACE(3,2,((#408193,#408194,#408195),(#408196,#408197,#408198),
(#408199,#408200,#408201),(#408202,#408203,#408204)),.UNSPECIFIED.,.F.,
 .F.,.F.)
B_SPLINE_SURFACE_WITH_KNOTS((4,4),(3,3),(0.00135801595889393,0.00148409170619832),
(0.,1.),.UNSPECIFIED.)
GEOMETRIC_REPRESENTATION_ITEM()
RATIONAL_B_SPLINE_SURFACE(((1.,0.818301933966446,1.),(1.,0.817226613172344,
1.),(1.,0.81617964337396,1.),(1.,0.815159387863656,1.)))
REPRESENTATION_ITEM('')
SURFACE()
);
#3252=(
BOUNDED_SURFACE()
B_SPLINE_SURFACE(3,2,((#408243,#408244,#408245),(#408246,#408247,#408248),
(#408249,#408250,#408251),(#408252,#408253,#408254)),.UNSPECIFIED.,.F.,
 .F.,.F.)
B_SPLINE_SURFACE_WITH_KNOTS((4,4),(3,3),(-1.54744435122072E-6,1.54744435122074E-5),
(-0.0151698983608262,1.),.UNSPECIFIED.)
GEOMETRIC_REPRESENTATION_ITEM()
RATIONAL_B_SPLINE_SURFACE(((1.02018382472781,0.33474093735738,1.),(1.0040123448879,
0.867753072813488,1.),(1.00033622856778,0.988917903080869,1.),(1.,1.,1.)))
REPRESENTATION_ITEM('')
SURFACE()
);
#3253=(
BOUNDED_SURFACE()
B_SPLINE_SURFACE(3,2,((#408256,#408257,#408258),(#408259,#408260,#408261),
(#408262,#408263,#408264),(#408265,#408266,#408267)),.UNSPECIFIED.,.F.,
 .F.,.F.)
B_SPLINE_SURFACE_WITH_KNOTS((4,4),(3,3),(0.00137194782501028,0.00149814269699235),
(0.,1.),.UNSPECIFIED.)
GEOMETRIC_REPRESENTATION_ITEM()
RATIONAL_B_SPLINE_SURFACE(((1.,0.815158509402327,1.),(1.,0.816179044148159,
1.),(1.,0.817226308119928,1.),(1.,0.818301939488813,1.)))
REPRESENTATION_ITEM('')
SURFACE()
);
#3254=(
BOUNDED_SURFACE()
B_SPLINE_SURFACE(3,2,((#408311,#408312,#408313),(#408314,#408315,#408316),
(#408317,#408318,#408319),(#408320,#408321,#408322)),.UNSPECIFIED.,.F.,
 .F.,.F.)
B_SPLINE_SURFACE_WITH_KNOTS((4,4),(3,3),(1.55009486301138E-5,4.92065510474431E-5),
(-8.13759512660296E-5,1.),.UNSPECIFIED.)
GEOMETRIC_REPRESENTATION_ITEM()
RATIONAL_B_SPLINE_SURFACE(((1.00002372912329,0.854200639599717,1.),(1.0000142358599,
0.912530301180557,1.),(1.00000710550469,0.956341495377438,1.),(1.00001238975905,
0.92387333813704,1.)))
REPRESENTATION_ITEM('')
SURFACE()
);
#3255=(
BOUNDED_SURFACE()
B_SPLINE_SURFACE(3,2,((#408326,#408327,#408328),(#408329,#408330,#408331),
(#408332,#408333,#408334),(#408335,#408336,#408337)),.UNSPECIFIED.,.F.,
 .F.,.F.)
B_SPLINE_SURFACE_WITH_KNOTS((4,4),(3,3),(-3.39934179457814E-6,3.73927597403565E-5),
(-0.00186004067420733,1.00069373317452),.UNSPECIFIED.)
GEOMETRIC_REPRESENTATION_ITEM()
RATIONAL_B_SPLINE_SURFACE(((1.00072100136055,0.806051963875316,1.00026859642696),
(1.00060048440155,0.838470803558624,1.000223699945),(1.00053106448795,0.857144632272353,
1.00019783877223),(1.00054515072853,0.853355459539081,1.00020308635441)))
REPRESENTATION_ITEM('')
SURFACE()
);
#3256=(
BOUNDED_SURFACE()
B_SPLINE_SURFACE(3,2,((#408339,#408340,#408341),(#408342,#408343,#408344),
(#408345,#408346,#408347),(#408348,#408349,#408350)),.UNSPECIFIED.,.F.,
 .F.,.F.)
B_SPLINE_SURFACE_WITH_KNOTS((4,4),(3,3),(-5.42101086242752E-20,9.54361881492175E-5),
(0.,1.),.UNSPECIFIED.)
GEOMETRIC_REPRESENTATION_ITEM()
RATIONAL_B_SPLINE_SURFACE(((1.,0.816715621142055,1.),(1.,0.81590758740794,
1.),(1.,0.815115959345211,1.),(1.,0.814339887349194,1.)))
REPRESENTATION_ITEM('')
SURFACE()
);
#3257=(
BOUNDED_SURFACE()
B_SPLINE_SURFACE(3,2,((#408352,#408353,#408354),(#408355,#408356,#408357),
(#408358,#408359,#408360),(#408361,#408362,#408363)),.UNSPECIFIED.,.F.,
 .F.,.F.)
B_SPLINE_SURFACE_WITH_KNOTS((4,4),(3,3),(0.,4.68197758448204E-5),(0.,1.),
 .UNSPECIFIED.)
GEOMETRIC_REPRESENTATION_ITEM()
RATIONAL_B_SPLINE_SURFACE(((1.,0.816715621142046,1.),(1.,0.953638980025203,
1.),(1.,0.954506925408058,1.),(1.,0.816715621142054,1.)))
REPRESENTATION_ITEM('')
SURFACE()
);
#3258=(
BOUNDED_SURFACE()
B_SPLINE_SURFACE(3,2,((#408365,#408366,#408367),(#408368,#408369,#408370),
(#408371,#408372,#408373),(#408374,#408375,#408376)),.UNSPECIFIED.,.F.,
 .F.,.F.)
B_SPLINE_SURFACE_WITH_KNOTS((4,4),(3,3),(-1.62630325872826E-19,9.54361881492175E-5),
(0.,1.),.UNSPECIFIED.)
GEOMETRIC_REPRESENTATION_ITEM()
RATIONAL_B_SPLINE_SURFACE(((1.,0.814339887349194,1.),(1.,0.815115959345217,
1.),(1.,0.815907587407947,1.),(1.,0.816715621142046,1.)))
REPRESENTATION_ITEM('')
SURFACE()
);
#3259=(
BOUNDED_SURFACE()
B_SPLINE_SURFACE(3,2,((#408378,#408379,#408380),(#408381,#408382,#408383),
(#408384,#408385,#408386),(#408387,#408388,#408389)),.UNSPECIFIED.,.F.,
 .F.,.F.)
B_SPLINE_SURFACE_WITH_KNOTS((4,4),(3,3),(-3.39528393502482E-6,3.73481232852737E-5),
(-0.00165018033328133,1.),.UNSPECIFIED.)
GEOMETRIC_REPRESENTATION_ITEM()
RATIONAL_B_SPLINE_SURFACE(((1.00048354385565,0.853487571660392,1.),(1.00047110510921,
0.857256476851488,1.),(1.00053193201107,0.838826096655856,1.),(1.00063970687725,
0.8061706153101,1.)))
REPRESENTATION_ITEM('')
SURFACE()
);
#3260=(
BOUNDED_SURFACE()
B_SPLINE_SURFACE(3,2,((#408393,#408394,#408395),(#408396,#408397,#408398),
(#408399,#408400,#408401),(#408402,#408403,#408404)),.UNSPECIFIED.,.F.,
 .F.,.F.)
B_SPLINE_SURFACE_WITH_KNOTS((4,4),(3,3),(2.02993869230512E-5,5.39756952686903E-5),
(-0.000116281070068554,1.),.UNSPECIFIED.)
GEOMETRIC_REPRESENTATION_ITEM()
RATIONAL_B_SPLINE_SURFACE(((1.00001770479732,0.923870681143002,1.),(1.0000101410406,
0.956394275543405,1.),(1.00002037300281,0.91239759490567,1.),(1.00003390859473,
0.854195550869827,1.)))
REPRESENTATION_ITEM('')
SURFACE()
);
#3261=(
BOUNDED_SURFACE()
B_SPLINE_SURFACE(3,2,((#408497,#408498,#408499),(#408500,#408501,#408502),
(#408503,#408504,#408505),(#408506,#408507,#408508)),.UNSPECIFIED.,.F.,
 .F.,.F.)
B_SPLINE_SURFACE_WITH_KNOTS((4,4),(3,3),(0.00135801595889393,0.00148409170619832),
(0.,1.),.UNSPECIFIED.)
GEOMETRIC_REPRESENTATION_ITEM()
RATIONAL_B_SPLINE_SURFACE(((1.,0.818301933966445,1.),(1.,0.81722661317235,
1.),(1.,0.816179643373944,1.),(1.,0.815159387863652,1.)))
REPRESENTATION_ITEM('')
SURFACE()
);
#3262=(
BOUNDED_SURFACE()
B_SPLINE_SURFACE(3,2,((#408547,#408548,#408549),(#408550,#408551,#408552),
(#408553,#408554,#408555),(#408556,#408557,#408558)),.UNSPECIFIED.,.F.,
 .F.,.F.)
B_SPLINE_SURFACE_WITH_KNOTS((4,4),(3,3),(-1.54744435122071E-6,1.54744435122076E-5),
(-0.0151698983676148,1.),.UNSPECIFIED.)
GEOMETRIC_REPRESENTATION_ITEM()
RATIONAL_B_SPLINE_SURFACE(((1.02018382473698,0.3347409373529,1.),(1.00401234488972,
0.867753072812631,1.),(1.00033622856793,0.98891790308079,1.),(1.,1.,1.)))
REPRESENTATION_ITEM('')
SURFACE()
);
#3263=(
BOUNDED_SURFACE()
B_SPLINE_SURFACE(3,2,((#408560,#408561,#408562),(#408563,#408564,#408565),
(#408566,#408567,#408568),(#408569,#408570,#408571)),.UNSPECIFIED.,.F.,
 .F.,.F.)
B_SPLINE_SURFACE_WITH_KNOTS((4,4),(3,3),(0.00137194782501028,0.00149814269699235),
(0.,1.),.UNSPECIFIED.)
GEOMETRIC_REPRESENTATION_ITEM()
RATIONAL_B_SPLINE_SURFACE(((1.,0.815158509402318,1.),(1.,0.816179044148164,
1.),(1.,0.817226308119926,1.),(1.,0.818301939488811,1.)))
REPRESENTATION_ITEM('')
SURFACE()
);
#3264=(
BOUNDED_SURFACE()
B_SPLINE_SURFACE(3,2,((#408615,#408616,#408617),(#408618,#408619,#408620),
(#408621,#408622,#408623),(#408624,#408625,#408626)),.UNSPECIFIED.,.F.,
 .F.,.F.)
B_SPLINE_SURFACE_WITH_KNOTS((4,4),(3,3),(1.55009486301137E-5,4.92065510474429E-5),
(-8.13759514211941E-5,1.),.UNSPECIFIED.)
GEOMETRIC_REPRESENTATION_ITEM()
RATIONAL_B_SPLINE_SURFACE(((1.00002372912334,0.8542006395997,1.),(1.00001423585992,
0.912530301180531,1.),(1.0000071055047,0.956341495377438,1.),(1.00001238975908,
0.923873338137026,1.)))
REPRESENTATION_ITEM('')
SURFACE()
);
#3265=(
BOUNDED_SURFACE()
B_SPLINE_SURFACE(3,2,((#408630,#408631,#408632),(#408633,#408634,#408635),
(#408636,#408637,#408638),(#408639,#408640,#408641)),.UNSPECIFIED.,.F.,
 .F.,.F.)
B_SPLINE_SURFACE_WITH_KNOTS((4,4),(3,3),(-3.39934179457818E-6,3.73927597403565E-5),
(-0.00186004067459443,1.00069373317435),.UNSPECIFIED.)
GEOMETRIC_REPRESENTATION_ITEM()
RATIONAL_B_SPLINE_SURFACE(((1.0007210013607,0.80605196387529,1.00026859642689),
(1.00060048440167,0.838470803558563,1.00022369994494),(1.00053106448806,
0.85714463227233,1.00019783877218),(1.00054515072864,0.853355459539047,
1.00020308635435)))
REPRESENTATION_ITEM('')
SURFACE()
);
#3266=(
BOUNDED_SURFACE()
B_SPLINE_SURFACE(3,2,((#408643,#408644,#408645),(#408646,#408647,#408648),
(#408649,#408650,#408651),(#408652,#408653,#408654)),.UNSPECIFIED.,.F.,
 .F.,.F.)
B_SPLINE_SURFACE_WITH_KNOTS((4,4),(3,3),(5.42101086242752E-20,9.54361881492175E-5),
(0.,1.),.UNSPECIFIED.)
GEOMETRIC_REPRESENTATION_ITEM()
RATIONAL_B_SPLINE_SURFACE(((1.,0.816715621142041,1.),(1.,0.815907587407951,
1.),(1.,0.815115959345192,1.),(1.,0.81433988734919,1.)))
REPRESENTATION_ITEM('')
SURFACE()
);
#3267=(
BOUNDED_SURFACE()
B_SPLINE_SURFACE(3,2,((#408656,#408657,#408658),(#408659,#408660,#408661),
(#408662,#408663,#408664),(#408665,#408666,#408667)),.UNSPECIFIED.,.F.,
 .F.,.F.)
B_SPLINE_SURFACE_WITH_KNOTS((4,4),(3,3),(6.94567016748526E-20,4.68197758448217E-5),
(0.,1.),.UNSPECIFIED.)
GEOMETRIC_REPRESENTATION_ITEM()
RATIONAL_B_SPLINE_SURFACE(((1.,0.816715621142048,1.),(1.,0.953638980025213,
1.),(1.,0.954506925408052,1.),(1.,0.816715621142053,1.)))
REPRESENTATION_ITEM('')
SURFACE()
);
#3268=(
BOUNDED_SURFACE()
B_SPLINE_SURFACE(3,2,((#408669,#408670,#408671),(#408672,#408673,#408674),
(#408675,#408676,#408677),(#408678,#408679,#408680)),.UNSPECIFIED.,.F.,
 .F.,.F.)
B_SPLINE_SURFACE_WITH_KNOTS((4,4),(3,3),(-5.42101086242752E-20,9.54361881492176E-5),
(0.,1.),.UNSPECIFIED.)
GEOMETRIC_REPRESENTATION_ITEM()
RATIONAL_B_SPLINE_SURFACE(((1.,0.81433988734919,1.),(1.,0.815115959345202,
1.),(1.,0.815907587407945,1.),(1.,0.816715621142048,1.)))
REPRESENTATION_ITEM('')
SURFACE()
);
#3269=(
BOUNDED_SURFACE()
B_SPLINE_SURFACE(3,2,((#408682,#408683,#408684),(#408685,#408686,#408687),
(#408688,#408689,#408690),(#408691,#408692,#408693)),.UNSPECIFIED.,.F.,
 .F.,.F.)
B_SPLINE_SURFACE_WITH_KNOTS((4,4),(3,3),(-3.39528393502486E-6,3.73481232852737E-5),
(-0.00165018033291492,1.),.UNSPECIFIED.)
GEOMETRIC_REPRESENTATION_ITEM()
RATIONAL_B_SPLINE_SURFACE(((1.00048354385555,0.853487571660454,1.),(1.0004711051091,
0.857256476851512,1.),(1.00053193201096,0.838826096655924,1.),(1.00063970687711,
0.806170615310167,1.)))
REPRESENTATION_ITEM('')
SURFACE()
);
#3270=(
BOUNDED_SURFACE()
B_SPLINE_SURFACE(3,2,((#408697,#408698,#408699),(#408700,#408701,#408702),
(#408703,#408704,#408705),(#408706,#408707,#408708)),.UNSPECIFIED.,.F.,
 .F.,.F.)
B_SPLINE_SURFACE_WITH_KNOTS((4,4),(3,3),(2.02993869230508E-5,5.39756952686901E-5),
(-0.000116281069843854,1.),.UNSPECIFIED.)
GEOMETRIC_REPRESENTATION_ITEM()
RATIONAL_B_SPLINE_SURFACE(((1.00001770479729,0.923870681143018,1.),(1.00001014104058,
0.956394275543418,1.),(1.00002037300277,0.912397594905681,1.),(1.00003390859467,
0.854195550869865,1.)))
REPRESENTATION_ITEM('')
SURFACE()
);
#3271=(
BOUNDED_SURFACE()
B_SPLINE_SURFACE(3,2,((#408801,#408802,#408803),(#408804,#408805,#408806),
(#408807,#408808,#408809),(#408810,#408811,#408812)),.UNSPECIFIED.,.F.,
 .F.,.F.)
B_SPLINE_SURFACE_WITH_KNOTS((4,4),(3,3),(0.00135801595889393,0.00148409170619832),
(0.,1.),.UNSPECIFIED.)
GEOMETRIC_REPRESENTATION_ITEM()
RATIONAL_B_SPLINE_SURFACE(((1.,0.818301933966443,1.),(1.,0.817226613172335,
1.),(1.,0.816179643373956,1.),(1.,0.815159387863654,1.)))
REPRESENTATION_ITEM('')
SURFACE()
);
#3272=(
BOUNDED_SURFACE()
B_SPLINE_SURFACE(3,2,((#408851,#408852,#408853),(#408854,#408855,#408856),
(#408857,#408858,#408859),(#408860,#408861,#408862)),.UNSPECIFIED.,.F.,
 .F.,.F.)
B_SPLINE_SURFACE_WITH_KNOTS((4,4),(3,3),(-1.54744435122086E-6,1.54744435122079E-5),
(-0.015169898363146,1.),.UNSPECIFIED.)
GEOMETRIC_REPRESENTATION_ITEM()
RATIONAL_B_SPLINE_SURFACE(((1.02018382473095,0.334740937355848,1.),(1.00401234488852,
0.867753072813226,1.),(1.00033622856783,0.988917903080852,1.),(1.,1.,1.)))
REPRESENTATION_ITEM('')
SURFACE()
);
#3273=(
BOUNDED_SURFACE()
B_SPLINE_SURFACE(3,2,((#408864,#408865,#408866),(#408867,#408868,#408869),
(#408870,#408871,#408872),(#408873,#408874,#408875)),.UNSPECIFIED.,.F.,
 .F.,.F.)
B_SPLINE_SURFACE_WITH_KNOTS((4,4),(3,3),(0.00137194782501028,0.00149814269699235),
(0.,1.),.UNSPECIFIED.)
GEOMETRIC_REPRESENTATION_ITEM()
RATIONAL_B_SPLINE_SURFACE(((1.,0.815158509402317,1.),(1.,0.816179044148165,
1.),(1.,0.817226308119923,1.),(1.,0.81830193948881,1.)))
REPRESENTATION_ITEM('')
SURFACE()
);
#3274=(
BOUNDED_SURFACE()
B_SPLINE_SURFACE(3,2,((#408919,#408920,#408921),(#408922,#408923,#408924),
(#408925,#408926,#408927),(#408928,#408929,#408930)),.UNSPECIFIED.,.F.,
 .F.,.F.)
B_SPLINE_SURFACE_WITH_KNOTS((4,4),(3,3),(1.55009486301137E-5,4.92065510474431E-5),
(-8.13759512802933E-5,1.),.UNSPECIFIED.)
GEOMETRIC_REPRESENTATION_ITEM()
RATIONAL_B_SPLINE_SURFACE(((1.0000237291233,0.85420063959972,1.),(1.0000142358599,
0.912530301180552,1.),(1.00000710550469,0.956341495377443,1.),(1.00001238975905,
0.923873338137036,1.)))
REPRESENTATION_ITEM('')
SURFACE()
);
#3275=(
BOUNDED_SURFACE()
B_SPLINE_SURFACE(3,2,((#408934,#408935,#408936),(#408937,#408938,#408939),
(#408940,#408941,#408942),(#408943,#408944,#408945)),.UNSPECIFIED.,.F.,
 .F.,.F.)
B_SPLINE_SURFACE_WITH_KNOTS((4,4),(3,3),(-3.39934179457827E-6,3.73927597403564E-5),
(-0.00186004067454373,1.0006937331745),.UNSPECIFIED.)
GEOMETRIC_REPRESENTATION_ITEM()
RATIONAL_B_SPLINE_SURFACE(((1.00072100136068,0.806051963875258,1.00026859642695),
(1.00060048440166,0.838470803558567,1.00022369994499),(1.00053106448805,
0.85714463227231,1.00019783877222),(1.00054515072863,0.853355459539032,
1.0002030863544)))
REPRESENTATION_ITEM('')
SURFACE()
);
#3276=(
BOUNDED_SURFACE()
B_SPLINE_SURFACE(3,2,((#408947,#408948,#408949),(#408950,#408951,#408952),
(#408953,#408954,#408955),(#408956,#408957,#408958)),.UNSPECIFIED.,.F.,
 .F.,.F.)
B_SPLINE_SURFACE_WITH_KNOTS((4,4),(3,3),(1.62630325872826E-19,9.54361881492177E-5),
(0.,1.),.UNSPECIFIED.)
GEOMETRIC_REPRESENTATION_ITEM()
RATIONAL_B_SPLINE_SURFACE(((1.,0.81671562114205,1.),(1.,0.815907587407935,
1.),(1.,0.815115959345204,1.),(1.,0.814339887349198,1.)))
REPRESENTATION_ITEM('')
SURFACE()
);
#3277=(
BOUNDED_SURFACE()
B_SPLINE_SURFACE(3,2,((#408960,#408961,#408962),(#408963,#408964,#408965),
(#408966,#408967,#408968),(#408969,#408970,#408971)),.UNSPECIFIED.,.F.,
 .F.,.F.)
B_SPLINE_SURFACE_WITH_KNOTS((4,4),(3,3),(-2.87991202066462E-20,4.68197758448205E-5),
(0.,1.),.UNSPECIFIED.)
GEOMETRIC_REPRESENTATION_ITEM()
RATIONAL_B_SPLINE_SURFACE(((1.,0.816715621142046,1.),(1.,0.953638980025209,
1.),(1.,0.954506925408056,1.),(1.,0.816715621142056,1.)))
REPRESENTATION_ITEM('')
SURFACE()
);
#3278=(
BOUNDED_SURFACE()
B_SPLINE_SURFACE(3,2,((#408973,#408974,#408975),(#408976,#408977,#408978),
(#408979,#408980,#408981),(#408982,#408983,#408984)),.UNSPECIFIED.,.F.,
 .F.,.F.)
B_SPLINE_SURFACE_WITH_KNOTS((4,4),(3,3),(1.0842021724855E-19,9.54361881492178E-5),
(0.,1.),.UNSPECIFIED.)
GEOMETRIC_REPRESENTATION_ITEM()
RATIONAL_B_SPLINE_SURFACE(((1.,0.814339887349193,1.),(1.,0.815115959345203,
1.),(1.,0.815907587407949,1.),(1.,0.81671562114205,1.)))
REPRESENTATION_ITEM('')
SURFACE()
);
#3279=(
BOUNDED_SURFACE()
B_SPLINE_SURFACE(3,2,((#408986,#408987,#408988),(#408989,#408990,#408991),
(#408992,#408993,#408994),(#408995,#408996,#408997)),.UNSPECIFIED.,.F.,
 .F.,.F.)
B_SPLINE_SURFACE_WITH_KNOTS((4,4),(3,3),(-3.39528393502482E-6,3.73481232852731E-5),
(-0.00165018033344248,1.),.UNSPECIFIED.)
GEOMETRIC_REPRESENTATION_ITEM()
RATIONAL_B_SPLINE_SURFACE(((1.0004835438557,0.85348757166038,1.),(1.00047110510925,
0.857256476851433,1.),(1.00053193201113,0.838826096655854,1.),(1.00063970687732,
0.806170615310058,1.)))
REPRESENTATION_ITEM('')
SURFACE()
);
#3280=(
BOUNDED_SURFACE()
B_SPLINE_SURFACE(3,2,((#409001,#409002,#409003),(#409004,#409005,#409006),
(#409007,#409008,#409009),(#409010,#409011,#409012)),.UNSPECIFIED.,.F.,
 .F.,.F.)
B_SPLINE_SURFACE_WITH_KNOTS((4,4),(3,3),(2.02993869230511E-5,5.39756952686911E-5),
(-0.000116281070020795,1.),.UNSPECIFIED.)
GEOMETRIC_REPRESENTATION_ITEM()
RATIONAL_B_SPLINE_SURFACE(((1.00001770479731,0.923870681143002,1.),(1.0000101410406,
0.956394275543419,1.),(1.0000203730028,0.912397594905663,1.),(1.00003390859472,
0.854195550869841,1.)))
REPRESENTATION_ITEM('')
SURFACE()
);
#3281=(
BOUNDED_SURFACE()
B_SPLINE_SURFACE(3,2,((#409105,#409106,#409107),(#409108,#409109,#409110),
(#409111,#409112,#409113),(#409114,#409115,#409116)),.UNSPECIFIED.,.F.,
 .F.,.F.)
B_SPLINE_SURFACE_WITH_KNOTS((4,4),(3,3),(0.00135801595889393,0.00148409170619832),
(0.,1.),.UNSPECIFIED.)
GEOMETRIC_REPRESENTATION_ITEM()
RATIONAL_B_SPLINE_SURFACE(((1.,0.818301933966442,1.),(1.,0.817226613172329,
1.),(1.,0.816179643373963,1.),(1.,0.81515938786365,1.)))
REPRESENTATION_ITEM('')
SURFACE()
);
#3282=(
BOUNDED_SURFACE()
B_SPLINE_SURFACE(3,2,((#409155,#409156,#409157),(#409158,#409159,#409160),
(#409161,#409162,#409163),(#409164,#409165,#409166)),.UNSPECIFIED.,.F.,
 .F.,.F.)
B_SPLINE_SURFACE_WITH_KNOTS((4,4),(3,3),(-1.54744435122071E-6,1.5474443512207E-5),
(-0.015169898364808,1.),.UNSPECIFIED.)
GEOMETRIC_REPRESENTATION_ITEM()
RATIONAL_B_SPLINE_SURFACE(((1.02018382473319,0.334740937354758,1.),(1.00401234488897,
0.867753072813005,1.),(1.00033622856787,0.988917903080771,1.),(1.,1.,1.)))
REPRESENTATION_ITEM('')
SURFACE()
);
#3283=(
BOUNDED_SURFACE()
B_SPLINE_SURFACE(3,2,((#409168,#409169,#409170),(#409171,#409172,#409173),
(#409174,#409175,#409176),(#409177,#409178,#409179)),.UNSPECIFIED.,.F.,
 .F.,.F.)
B_SPLINE_SURFACE_WITH_KNOTS((4,4),(3,3),(0.00137194782501028,0.00149814269699235),
(0.,1.),.UNSPECIFIED.)
GEOMETRIC_REPRESENTATION_ITEM()
RATIONAL_B_SPLINE_SURFACE(((1.,0.815158509402313,1.),(1.,0.816179044148174,
1.),(1.,0.817226308119912,1.),(1.,0.818301939488812,1.)))
REPRESENTATION_ITEM('')
SURFACE()
);
#3284=(
BOUNDED_SURFACE()
B_SPLINE_SURFACE(3,2,((#409223,#409224,#409225),(#409226,#409227,#409228),
(#409229,#409230,#409231),(#409232,#409233,#409234)),.UNSPECIFIED.,.F.,
 .F.,.F.)
B_SPLINE_SURFACE_WITH_KNOTS((4,4),(3,3),(1.55009486301138E-5,4.92065510474437E-5),
(-8.13759515121529E-5,1.),.UNSPECIFIED.)
GEOMETRIC_REPRESENTATION_ITEM()
RATIONAL_B_SPLINE_SURFACE(((1.00002372912336,0.854200639599686,1.),(1.00001423585994,
0.912530301180531,1.),(1.00000710550471,0.956341495377431,1.),(1.00001238975909,
0.923873338137019,1.)))
REPRESENTATION_ITEM('')
SURFACE()
);
#3285=(
BOUNDED_SURFACE()
B_SPLINE_SURFACE(3,2,((#409238,#409239,#409240),(#409241,#409242,#409243),
(#409244,#409245,#409246),(#409247,#409248,#409249)),.UNSPECIFIED.,.F.,
 .F.,.F.)
B_SPLINE_SURFACE_WITH_KNOTS((4,4),(3,3),(-3.39934179457835E-6,3.73927597403565E-5),
(-0.0018600406742466,1.0006937331745),.UNSPECIFIED.)
GEOMETRIC_REPRESENTATION_ITEM()
RATIONAL_B_SPLINE_SURFACE(((1.00072100136057,0.806051963875303,1.00026859642695),
(1.00060048440156,0.838470803558628,1.00022369994499),(1.00053106448796,
0.857144632272343,1.00019783877222),(1.00054515072854,0.853355459539073,
1.0002030863544)))
REPRESENTATION_ITEM('')
SURFACE()
);
#3286=(
BOUNDED_SURFACE()
B_SPLINE_SURFACE(3,2,((#409251,#409252,#409253),(#409254,#409255,#409256),
(#409257,#409258,#409259),(#409260,#409261,#409262)),.UNSPECIFIED.,.F.,
 .F.,.F.)
B_SPLINE_SURFACE_WITH_KNOTS((4,4),(3,3),(-5.42101086242752E-20,9.54361881492175E-5),
(0.,1.),.UNSPECIFIED.)
GEOMETRIC_REPRESENTATION_ITEM()
RATIONAL_B_SPLINE_SURFACE(((1.,0.816715621142046,1.),(1.,0.815907587407942,
1.),(1.,0.815115959345197,1.),(1.,0.814339887349194,1.)))
REPRESENTATION_ITEM('')
SURFACE()
);
#3287=(
BOUNDED_SURFACE()
B_SPLINE_SURFACE(3,2,((#409264,#409265,#409266),(#409267,#409268,#409269),
(#409270,#409271,#409272),(#409273,#409274,#409275)),.UNSPECIFIED.,.F.,
 .F.,.F.)
B_SPLINE_SURFACE_WITH_KNOTS((4,4),(3,3),(-2.37169225231204E-20,4.68197758448207E-5),
(0.,1.),.UNSPECIFIED.)
GEOMETRIC_REPRESENTATION_ITEM()
RATIONAL_B_SPLINE_SURFACE(((1.,0.816715621142046,1.),(1.,0.953638980025198,
1.),(1.,0.954506925408069,1.),(1.,0.816715621142046,1.)))
REPRESENTATION_ITEM('')
SURFACE()
);
#3288=(
BOUNDED_SURFACE()
B_SPLINE_SURFACE(3,2,((#409277,#409278,#409279),(#409280,#409281,#409282),
(#409283,#409284,#409285),(#409286,#409287,#409288)),.UNSPECIFIED.,.F.,
 .F.,.F.)
B_SPLINE_SURFACE_WITH_KNOTS((4,4),(3,3),(5.42101086242752E-20,9.54361881492178E-5),
(0.,1.),.UNSPECIFIED.)
GEOMETRIC_REPRESENTATION_ITEM()
RATIONAL_B_SPLINE_SURFACE(((1.,0.814339887349192,1.),(1.,0.815115959345201,
1.),(1.,0.815907587407946,1.),(1.,0.816715621142046,1.)))
REPRESENTATION_ITEM('')
SURFACE()
);
#3289=(
BOUNDED_SURFACE()
B_SPLINE_SURFACE(3,2,((#409290,#409291,#409292),(#409293,#409294,#409295),
(#409296,#409297,#409298),(#409299,#409300,#409301)),.UNSPECIFIED.,.F.,
 .F.,.F.)
B_SPLINE_SURFACE_WITH_KNOTS((4,4),(3,3),(-3.39528393502488E-6,3.73481232852737E-5),
(-0.00165018033279429,1.),.UNSPECIFIED.)
GEOMETRIC_REPRESENTATION_ITEM()
RATIONAL_B_SPLINE_SURFACE(((1.00048354385551,0.853487571660467,1.),(1.00047110510907,
0.857256476851531,1.),(1.00053193201092,0.838826096655951,1.),(1.00063970687707,
0.806170615310183,1.)))
REPRESENTATION_ITEM('')
SURFACE()
);
#3290=(
BOUNDED_SURFACE()
B_SPLINE_SURFACE(3,2,((#409305,#409306,#409307),(#409308,#409309,#409310),
(#409311,#409312,#409313),(#409314,#409315,#409316)),.UNSPECIFIED.,.F.,
 .F.,.F.)
B_SPLINE_SURFACE_WITH_KNOTS((4,4),(3,3),(2.0299386923051E-5,5.39756952686907E-5),
(-0.000116281069868689,1.),.UNSPECIFIED.)
GEOMETRIC_REPRESENTATION_ITEM()
RATIONAL_B_SPLINE_SURFACE(((1.00001770479729,0.923870681143011,1.),(1.00001014104058,
0.95639427554342,1.),(1.00002037300278,0.912397594905679,1.),(1.00003390859467,
0.854195550869862,1.)))
REPRESENTATION_ITEM('')
SURFACE()
);
#3291=(
BOUNDED_SURFACE()
B_SPLINE_SURFACE(3,2,((#409409,#409410,#409411),(#409412,#409413,#409414),
(#409415,#409416,#409417),(#409418,#409419,#409420)),.UNSPECIFIED.,.F.,
 .F.,.F.)
B_SPLINE_SURFACE_WITH_KNOTS((4,4),(3,3),(0.00135801595889393,0.00148409170619832),
(0.,1.),.UNSPECIFIED.)
GEOMETRIC_REPRESENTATION_ITEM()
RATIONAL_B_SPLINE_SURFACE(((1.,0.818301933966443,1.),(1.,0.817226613172361,
1.),(1.,0.816179643373939,1.),(1.,0.815159387863656,1.)))
REPRESENTATION_ITEM('')
SURFACE()
);
#3292=(
BOUNDED_SURFACE()
B_SPLINE_SURFACE(3,2,((#409459,#409460,#409461),(#409462,#409463,#409464),
(#409465,#409466,#409467),(#409468,#409469,#409470)),.UNSPECIFIED.,.F.,
 .F.,.F.)
B_SPLINE_SURFACE_WITH_KNOTS((4,4),(3,3),(-1.5474443512207E-6,1.54744435122074E-5),
(-0.015169898372212,1.),.UNSPECIFIED.)
GEOMETRIC_REPRESENTATION_ITEM()
RATIONAL_B_SPLINE_SURFACE(((1.02018382474319,0.33474093734983,1.),(1.00401234489096,
0.867753072812112,1.),(1.00033622856803,0.988917903080659,1.),(1.,1.,1.)))
REPRESENTATION_ITEM('')
SURFACE()
);
#3293=(
BOUNDED_SURFACE()
B_SPLINE_SURFACE(3,2,((#409472,#409473,#409474),(#409475,#409476,#409477),
(#409478,#409479,#409480),(#409481,#409482,#409483)),.UNSPECIFIED.,.F.,
 .F.,.F.)
B_SPLINE_SURFACE_WITH_KNOTS((4,4),(3,3),(0.00137194782501028,0.00149814269699235),
(0.,1.),.UNSPECIFIED.)
GEOMETRIC_REPRESENTATION_ITEM()
RATIONAL_B_SPLINE_SURFACE(((1.,0.815158509402317,1.),(1.,0.816179044148169,
1.),(1.,0.817226308119918,1.),(1.,0.81830193948881,1.)))
REPRESENTATION_ITEM('')
SURFACE()
);
#3294=(
BOUNDED_SURFACE()
B_SPLINE_SURFACE(3,2,((#409527,#409528,#409529),(#409530,#409531,#409532),
(#409533,#409534,#409535),(#409536,#409537,#409538)),.UNSPECIFIED.,.F.,
 .F.,.F.)
B_SPLINE_SURFACE_WITH_KNOTS((4,4),(3,3),(1.55009486301137E-5,4.92065510474436E-5),
(-8.13759515650707E-5,1.),.UNSPECIFIED.)
GEOMETRIC_REPRESENTATION_ITEM()
RATIONAL_B_SPLINE_SURFACE(((1.00002372912338,0.85420063959967,1.),(1.00001423585995,
0.912530301180529,1.),(1.00000710550471,0.956341495377431,1.),(1.0000123897591,
0.923873338137015,1.)))
REPRESENTATION_ITEM('')
SURFACE()
);
#3295=(
BOUNDED_SURFACE()
B_SPLINE_SURFACE(3,2,((#409542,#409543,#409544),(#409545,#409546,#409547),
(#409548,#409549,#409550),(#409551,#409552,#409553)),.UNSPECIFIED.,.F.,
 .F.,.F.)
B_SPLINE_SURFACE_WITH_KNOTS((4,4),(3,3),(-3.3993417945787E-6,3.73927597403563E-5),
(-0.00186004067399629,1.00069373317423),.UNSPECIFIED.)
GEOMETRIC_REPRESENTATION_ITEM()
RATIONAL_B_SPLINE_SURFACE(((1.00072100136047,0.806051963875404,1.00026859642685),
(1.00060048440148,0.838470803558721,1.0002236999449),(1.00053106448789,
0.857144632272418,1.00019783877215),(1.00054515072847,0.853355459539159,
1.00020308635432)))
REPRESENTATION_ITEM('')
SURFACE()
);
#3296=(
BOUNDED_SURFACE()
B_SPLINE_SURFACE(3,2,((#409555,#409556,#409557),(#409558,#409559,#409560),
(#409561,#409562,#409563),(#409564,#409565,#409566)),.UNSPECIFIED.,.F.,
 .F.,.F.)
B_SPLINE_SURFACE_WITH_KNOTS((4,4),(3,3),(1.0842021724855E-19,9.54361881492172E-5),
(0.,1.),.UNSPECIFIED.)
GEOMETRIC_REPRESENTATION_ITEM()
RATIONAL_B_SPLINE_SURFACE(((1.,0.816715621142052,1.),(1.,0.81590758740794,
1.),(1.,0.815115959345197,1.),(1.,0.814339887349202,1.)))
REPRESENTATION_ITEM('')
SURFACE()
);
#3297=(
BOUNDED_SURFACE()
B_SPLINE_SURFACE(3,2,((#409568,#409569,#409570),(#409571,#409572,#409573),
(#409574,#409575,#409576),(#409577,#409578,#409579)),.UNSPECIFIED.,.F.,
 .F.,.F.)
B_SPLINE_SURFACE_WITH_KNOTS((4,4),(3,3),(5.9292306307801E-20,4.68197758448208E-5),
(0.,1.),.UNSPECIFIED.)
GEOMETRIC_REPRESENTATION_ITEM()
RATIONAL_B_SPLINE_SURFACE(((1.,0.816715621142048,1.),(1.,0.953638980025209,
1.),(1.,0.954506925408052,1.),(1.,0.816715621142059,1.)))
REPRESENTATION_ITEM('')
SURFACE()
);
#3298=(
BOUNDED_SURFACE()
B_SPLINE_SURFACE(3,2,((#409581,#409582,#409583),(#409584,#409585,#409586),
(#409587,#409588,#409589),(#409590,#409591,#409592)),.UNSPECIFIED.,.F.,
 .F.,.F.)
B_SPLINE_SURFACE_WITH_KNOTS((4,4),(3,3),(-5.42101086242752E-20,9.54361881492178E-5),
(0.,1.),.UNSPECIFIED.)
GEOMETRIC_REPRESENTATION_ITEM()
RATIONAL_B_SPLINE_SURFACE(((1.,0.814339887349196,1.),(1.,0.815115959345204,
1.),(1.,0.815907587407944,1.),(1.,0.816715621142048,1.)))
REPRESENTATION_ITEM('')
SURFACE()
);
#3299=(
BOUNDED_SURFACE()
B_SPLINE_SURFACE(3,2,((#409594,#409595,#409596),(#409597,#409598,#409599),
(#409600,#409601,#409602),(#409603,#409604,#409605)),.UNSPECIFIED.,.F.,
 .F.,.F.)
B_SPLINE_SURFACE_WITH_KNOTS((4,4),(3,3),(-3.39528393502484E-6,3.7348123285273E-5),
(-0.00165018033307088,1.),.UNSPECIFIED.)
GEOMETRIC_REPRESENTATION_ITEM()
RATIONAL_B_SPLINE_SURFACE(((1.00048354385559,0.85348757166043,1.),(1.00047110510915,
0.857256476851486,1.),(1.000531932011,0.838826096655913,1.),(1.00063970687717,
0.806170615310131,1.)))
REPRESENTATION_ITEM('')
SURFACE()
);
#3300=(
BOUNDED_SURFACE()
B_SPLINE_SURFACE(3,2,((#409609,#409610,#409611),(#409612,#409613,#409614),
(#409615,#409616,#409617),(#409618,#409619,#409620)),.UNSPECIFIED.,.F.,
 .F.,.F.)
B_SPLINE_SURFACE_WITH_KNOTS((4,4),(3,3),(2.02993869230509E-5,5.39756952686903E-5),
(-0.000116281069956809,1.),.UNSPECIFIED.)
GEOMETRIC_REPRESENTATION_ITEM()
RATIONAL_B_SPLINE_SURFACE(((1.0000177047973,0.923870681143007,1.),(1.00001014104059,
0.956394275543409,1.),(1.00002037300279,0.912397594905683,1.),(1.0000339085947,
0.854195550869847,1.)))
REPRESENTATION_ITEM('')
SURFACE()
);
#3301=(
BOUNDED_SURFACE()
B_SPLINE_SURFACE(1,2,((#420151,#420152,#420153,#420154,#420155,#420156,
#420157,#420158,#420159,#420160,#420161,#420162,#420163,#420164,#420165,
#420166,#420167,#420168,#420169,#420170,#420171,#420172,#420173,#420174,
#420175,#420176,#420177,#420178,#420179,#420180,#420181,#420182,#420183,
#420184,#420185,#420186,#420187,#420188,#420189,#420190,#420191,#420192,
#420193,#420194,#420195,#420196,#420197,#420198,#420199,#420200,#420201,
#420202,#420203,#420204,#420205,#420206,#420207,#420208,#420209,#420210,
#420211,#420212,#420213,#420214,#420215,#420216,#420217,#420218,#420219,
#420220,#420221,#420222,#420223,#420224,#420225,#420226,#420227,#420228,
#420229,#420230,#420231,#420232,#420233,#420234,#420235,#420236,#420237,
#420238,#420239,#420240,#420241,#420242,#420243,#420244,#420245,#420246,
#420247,#420248,#420249,#420250,#420251,#420252,#420253,#420254,#420255,
#420256,#420257,#420258,#420259,#420260,#420261,#420262,#420263,#420264,
#420265,#420266,#420267,#420268,#420269,#420270,#420271,#420272,#420273,
#420274,#420275,#420276,#420277,#420278,#420279,#420280,#420281,#420282,
#420283,#420284,#420285,#420286,#420287,#420288,#420289,#420290,#420291,
#420292,#420293,#420294,#420295,#420296,#420297,#420298,#420299,#420300,
#420301,#420302,#420303,#420304,#420305,#420306,#420307,#420308,#420309,
#420310,#420311,#420312,#420313,#420314,#420315,#420316,#420317,#420318,
#420319,#420320,#420321,#420322,#420323,#420324,#420325,#420326,#420327,
#420328,#420329,#420330,#420331,#420332,#420333,#420334,#420335,#420336,
#420337,#420338,#420339,#420340,#420341,#420342,#420343,#420344,#420345,
#420346,#420347,#420348,#420349,#420350,#420351,#420352,#420353,#420354,
#420355,#420356,#420357,#420358,#420359,#420360,#420361,#420362,#420363,
#420364,#420365,#420366,#420367,#420368,#420369,#420370,#420371,#420372,
#420373,#420374,#420375,#420376,#420377,#420378,#420379,#420380,#420381,
#420382,#420383,#420384,#420385,#420386,#420387,#420388,#420389,#420390,
#420391,#420392,#420393,#420394,#420395,#420396,#420397,#420398,#420399,
#420400,#420401,#420402,#420403,#420404,#420405,#420406,#420407,#420408,
#420409,#420410,#420411,#420412,#420413,#420414,#420415,#420416,#420417,
#420418,#420419,#420420,#420421,#420422,#420423,#420424,#420425,#420426,
#420427,#420428,#420429,#420430,#420431,#420432,#420433,#420434,#420435,
#420436,#420437,#420438,#420439,#420440,#420441,#420442,#420443,#420444,
#420445,#420446,#420447,#420448,#420449,#420450,#420451,#420452,#420453,
#420454,#420455,#420456,#420457,#420458,#420459,#420460,#420461,#420462,
#420463,#420464,#420465,#420466,#420467,#420468,#420469,#420470,#420471,
#420472,#420473,#420474,#420475,#420476,#420477,#420478,#420479,#420480,
#420481,#420482,#420483,#420484,#420485,#420486,#420487,#420488,#420489,
#420490,#420491,#420492,#420493,#420494,#420495,#420496,#420497,#420498,
#420499,#420500,#420501,#420502,#420503,#420504,#420505,#420506,#420507,
#420508,#420509,#420510,#420511,#420512,#420513,#420514,#420515,#420516,
#420517,#420518,#420519,#420520,#420521,#420522,#420523,#420524,#420525,
#420526,#420527,#420528,#420529,#420530,#420531,#420532,#420533,#420534,
#420535,#420536,#420537,#420538,#420539,#420540,#420541,#420542,#420543,
#420544,#420545,#420546,#420547,#420548,#420549,#420550,#420551,#420552,
#420553,#420554,#420555,#420556,#420557,#420558,#420559,#420560,#420561,
#420562,#420563,#420564,#420565,#420566,#420567,#420568,#420569,#420570,
#420571,#420572,#420573,#420574,#420575,#420576,#420577,#420578,#420579,
#420580,#420581,#420582,#420583,#420584,#420585,#420586,#420587,#420588,
#420589,#420590,#420591,#420592,#420593,#420594,#420595,#420596,#420597,
#420598,#420599,#420600,#420601,#420602,#420603,#420604,#420605,#420606,
#420607,#420608,#420609,#420610,#420611,#420612,#420613,#420614,#420615,
#420616,#420617,#420618,#420619,#420620,#420621,#420622,#420623,#420624,
#420625,#420626,#420627,#420628,#420629,#420630,#420631,#420632,#420633,
#420634,#420635,#420636,#420637,#420638,#420639,#420640,#420641,#420642,
#420643,#420644,#420645,#420646,#420647,#420648,#420649,#420650,#420651,
#420652,#420653,#420654,#420655,#420656,#420657,#420658,#420659,#420660,
#420661,#420662,#420663,#420664,#420665,#420666,#420667,#420668,#420669,
#420670,#420671,#420672,#420673,#420674,#420675,#420676,#420677,#420678,
#420679,#420680,#420681,#420682,#420683,#420684,#420685,#420686,#420687,
#420688,#420689,#420690,#420691,#420692,#420693,#420694,#420695,#420696,
#420697,#420698,#420699,#420700,#420701,#420702,#420703,#420704,#420705,
#420706,#420707,#420708,#420709,#420710,#420711,#420712,#420713,#420714,
#420715,#420716,#420717,#420718,#420719,#420720,#420721,#420722,#420723,
#420724,#420725,#420726,#420727,#420728,#420729,#420730,#420731,#420732,
#420733,#420734,#420735,#420736,#420737,#420738,#420739,#420740,#420741,
#420742,#420743,#420744,#420745,#420746,#420747,#420748,#420749,#420750,
#420751,#420752,#420753,#420754,#420755,#420756,#420757,#420758,#420759,
#420760,#420761,#420762,#420763),(#420764,#420765,#420766,#420767,#420768,
#420769,#420770,#420771,#420772,#420773,#420774,#420775,#420776,#420777,
#420778,#420779,#420780,#420781,#420782,#420783,#420784,#420785,#420786,
#420787,#420788,#420789,#420790,#420791,#420792,#420793,#420794,#420795,
#420796,#420797,#420798,#420799,#420800,#420801,#420802,#420803,#420804,
#420805,#420806,#420807,#420808,#420809,#420810,#420811,#420812,#420813,
#420814,#420815,#420816,#420817,#420818,#420819,#420820,#420821,#420822,
#420823,#420824,#420825,#420826,#420827,#420828,#420829,#420830,#420831,
#420832,#420833,#420834,#420835,#420836,#420837,#420838,#420839,#420840,
#420841,#420842,#420843,#420844,#420845,#420846,#420847,#420848,#420849,
#420850,#420851,#420852,#420853,#420854,#420855,#420856,#420857,#420858,
#420859,#420860,#420861,#420862,#420863,#420864,#420865,#420866,#420867,
#420868,#420869,#420870,#420871,#420872,#420873,#420874,#420875,#420876,
#420877,#420878,#420879,#420880,#420881,#420882,#420883,#420884,#420885,
#420886,#420887,#420888,#420889,#420890,#420891,#420892,#420893,#420894,
#420895,#420896,#420897,#420898,#420899,#420900,#420901,#420902,#420903,
#420904,#420905,#420906,#420907,#420908,#420909,#420910,#420911,#420912,
#420913,#420914,#420915,#420916,#420917,#420918,#420919,#420920,#420921,
#420922,#420923,#420924,#420925,#420926,#420927,#420928,#420929,#420930,
#420931,#420932,#420933,#420934,#420935,#420936,#420937,#420938,#420939,
#420940,#420941,#420942,#420943,#420944,#420945,#420946,#420947,#420948,
#420949,#420950,#420951,#420952,#420953,#420954,#420955,#420956,#420957,
#420958,#420959,#420960,#420961,#420962,#420963,#420964,#420965,#420966,
#420967,#420968,#420969,#420970,#420971,#420972,#420973,#420974,#420975,
#420976,#420977,#420978,#420979,#420980,#420981,#420982,#420983,#420984,
#420985,#420986,#420987,#420988,#420989,#420990,#420991,#420992,#420993,
#420994,#420995,#420996,#420997,#420998,#420999,#421000,#421001,#421002,
#421003,#421004,#421005,#421006,#421007,#421008,#421009,#421010,#421011,
#421012,#421013,#421014,#421015,#421016,#421017,#421018,#421019,#421020,
#421021,#421022,#421023,#421024,#421025,#421026,#421027,#421028,#421029,
#421030,#421031,#421032,#421033,#421034,#421035,#421036,#421037,#421038,
#421039,#421040,#421041,#421042,#421043,#421044,#421045,#421046,#421047,
#421048,#421049,#421050,#421051,#421052,#421053,#421054,#421055,#421056,
#421057,#421058,#421059,#421060,#421061,#421062,#421063,#421064,#421065,
#421066,#421067,#421068,#421069,#421070,#421071,#421072,#421073,#421074,
#421075,#421076,#421077,#421078,#421079,#421080,#421081,#421082,#421083,
#421084,#421085,#421086,#421087,#421088,#421089,#421090,#421091,#421092,
#421093,#421094,#421095,#421096,#421097,#421098,#421099,#421100,#421101,
#421102,#421103,#421104,#421105,#421106,#421107,#421108,#421109,#421110,
#421111,#421112,#421113,#421114,#421115,#421116,#421117,#421118,#421119,
#421120,#421121,#421122,#421123,#421124,#421125,#421126,#421127,#421128,
#421129,#421130,#421131,#421132,#421133,#421134,#421135,#421136,#421137,
#421138,#421139,#421140,#421141,#421142,#421143,#421144,#421145,#421146,
#421147,#421148,#421149,#421150,#421151,#421152,#421153,#421154,#421155,
#421156,#421157,#421158,#421159,#421160,#421161,#421162,#421163,#421164,
#421165,#421166,#421167,#421168,#421169,#421170,#421171,#421172,#421173,
#421174,#421175,#421176,#421177,#421178,#421179,#421180,#421181,#421182,
#421183,#421184,#421185,#421186,#421187,#421188,#421189,#421190,#421191,
#421192,#421193,#421194,#421195,#421196,#421197,#421198,#421199,#421200,
#421201,#421202,#421203,#421204,#421205,#421206,#421207,#421208,#421209,
#421210,#421211,#421212,#421213,#421214,#421215,#421216,#421217,#421218,
#421219,#421220,#421221,#421222,#421223,#421224,#421225,#421226,#421227,
#421228,#421229,#421230,#421231,#421232,#421233,#421234,#421235,#421236,
#421237,#421238,#421239,#421240,#421241,#421242,#421243,#421244,#421245,
#421246,#421247,#421248,#421249,#421250,#421251,#421252,#421253,#421254,
#421255,#421256,#421257,#421258,#421259,#421260,#421261,#421262,#421263,
#421264,#421265,#421266,#421267,#421268,#421269,#421270,#421271,#421272,
#421273,#421274,#421275,#421276,#421277,#421278,#421279,#421280,#421281,
#421282,#421283,#421284,#421285,#421286,#421287,#421288,#421289,#421290,
#421291,#421292,#421293,#421294,#421295,#421296,#421297,#421298,#421299,
#421300,#421301,#421302,#421303,#421304,#421305,#421306,#421307,#421308,
#421309,#421310,#421311,#421312,#421313,#421314,#421315,#421316,#421317,
#421318,#421319,#421320,#421321,#421322,#421323,#421324,#421325,#421326,
#421327,#421328,#421329,#421330,#421331,#421332,#421333,#421334,#421335,
#421336,#421337,#421338,#421339,#421340,#421341,#421342,#421343,#421344,
#421345,#421346,#421347,#421348,#421349,#421350,#421351,#421352,#421353,
#421354,#421355,#421356,#421357,#421358,#421359,#421360,#421361,#421362,
#421363,#421364,#421365,#421366,#421367,#421368,#421369,#421370,#421371,
#421372,#421373,#421374,#421375,#421376)),.UNSPECIFIED.,.F.,.F.,.F.)
B_SPLINE_SURFACE_WITH_KNOTS((2,2),(3,2,2,2,2,2,2,2,2,2,2,2,2,2,2,2,2,2,
2,2,2,2,2,2,2,2,2,2,2,2,2,2,2,2,2,2,2,2,2,2,2,2,2,2,2,2,2,2,2,2,2,2,2,2,
2,2,2,2,2,2,2,2,2,2,2,2,2,2,2,2,2,2,2,2,2,2,2,2,2,2,2,2,2,2,2,2,2,2,2,2,
2,2,2,2,2,2,2,2,2,2,2,2,2,2,2,2,2,2,2,2,2,2,2,2,2,2,2,2,2,2,2,2,2,2,2,2,
2,2,2,2,2,2,2,2,2,2,2,2,2,2,2,2,2,2,2,2,2,2,2,2,2,2,2,2,2,2,2,2,2,2,2,2,
2,2,2,2,2,2,2,2,2,2,2,2,2,2,2,2,2,2,2,2,2,2,2,2,2,2,2,2,2,2,2,2,2,2,2,2,
2,2,2,2,2,2,2,2,2,2,2,2,2,2,2,2,2,2,2,2,2,2,2,2,2,2,2,2,2,2,2,2,2,2,2,2,
2,2,2,2,2,2,2,2,2,2,2,2,2,2,2,2,2,2,2,2,2,2,2,2,2,2,2,2,2,2,2,2,2,2,2,2,
2,2,2,2,2,2,2,2,2,2,2,2,2,2,2,2,2,2,2,2,2,2,2,2,2,2,2,2,2,2,2,2,2,2,2,2,
3),(0.,1.00001492288347),(0.,0.00326797385620915,0.0065359477124183,0.00980392156862745,
0.0130718954248366,0.0163398692810458,0.0196078431372549,0.0228758169934641,
0.0261437908496732,0.0294117647058824,0.0326797385620915,0.0359477124183007,
0.0392156862745098,0.042483660130719,0.0457516339869281,0.0490196078431373,
0.0522875816993464,0.0555555555555556,0.0588235294117647,0.0620915032679739,
0.065359477124183,0.0686274509803922,0.0718954248366013,0.0751633986928105,
0.0784313725490196,0.0816993464052288,0.0849673202614379,0.0882352941176471,
0.0915032679738562,0.0947712418300654,0.0980392156862745,0.101307189542484,
0.104575163398693,0.107843137254902,0.111111111111111,0.11437908496732,
0.117647058823529,0.120915032679739,0.124183006535948,0.127450980392157,
0.130718954248366,0.133986928104575,0.137254901960784,0.140522875816993,
0.143790849673203,0.147058823529412,0.150326797385621,0.15359477124183,
0.156862745098039,0.160130718954248,0.163398692810458,0.166666666666667,
0.169934640522876,0.173202614379085,0.176470588235294,0.179738562091503,
0.183006535947712,0.186274509803922,0.189542483660131,0.19281045751634,
0.196078431372549,0.199346405228758,0.202614379084967,0.205882352941176,
0.209150326797386,0.212418300653595,0.215686274509804,0.218954248366013,
0.222222222222222,0.225490196078431,0.228758169934641,0.23202614379085,
0.235294117647059,0.238562091503268,0.241830065359477,0.245098039215686,
0.248366013071895,0.251633986928105,0.254901960784314,0.258169934640523,
0.261437908496732,0.264705882352941,0.26797385620915,0.271241830065359,
0.274509803921569,0.277777777777778,0.281045751633987,0.284313725490196,
0.287581699346405,0.290849673202614,0.294117647058824,0.297385620915033,
0.300653594771242,0.303921568627451,0.30718954248366,0.310457516339869,
0.313725490196078,0.316993464052288,0.320261437908497,0.323529411764706,
0.326797385620915,0.330065359477124,0.333333333333333,0.336601307189543,
0.339869281045752,0.343137254901961,0.34640522875817,0.349673202614379,
0.352941176470588,0.356209150326797,0.359477124183007,0.362745098039216,
0.366013071895425,0.369281045751634,0.372549019607843,0.375816993464052,
0.379084967320261,0.382352941176471,0.38562091503268,0.388888888888889,
0.392156862745098,0.395424836601307,0.398692810457516,0.401960784313726,
0.405228758169935,0.408496732026144,0.411764705882353,0.415032679738562,
0.418300653594771,0.42156862745098,0.42483660130719,0.428104575163399,0.431372549019608,
0.434640522875817,0.437908496732026,0.441176470588235,0.444444444444444,
0.447712418300654,0.450980392156863,0.454248366013072,0.457516339869281,
0.46078431372549,0.464052287581699,0.467320261437909,0.470588235294118,
0.473856209150327,0.477124183006536,0.480392156862745,0.483660130718954,
0.486928104575163,0.490196078431373,0.493464052287582,0.496732026143791,
0.5,0.503267973856209,0.506535947712418,0.509803921568627,0.513071895424837,
0.516339869281046,0.519607843137255,0.522875816993464,0.526143790849673,
0.529411764705882,0.532679738562091,0.535947712418301,0.53921568627451,
0.542483660130719,0.545751633986928,0.549019607843137,0.552287581699346,
0.555555555555556,0.558823529411765,0.562091503267974,0.565359477124183,
0.568627450980392,0.571895424836601,0.57516339869281,0.57843137254902,0.581699346405229,
0.584967320261438,0.588235294117647,0.591503267973856,0.594771241830065,
0.598039215686274,0.601307189542484,0.604575163398693,0.607843137254902,
0.611111111111111,0.61437908496732,0.617647058823529,0.620915032679739,
0.624183006535948,0.627450980392157,0.630718954248366,0.633986928104575,
0.637254901960784,0.640522875816993,0.643790849673203,0.647058823529412,
0.650326797385621,0.65359477124183,0.656862745098039,0.660130718954248,
0.663398692810457,0.666666666666667,0.669934640522876,0.673202614379085,
0.676470588235294,0.679738562091503,0.683006535947712,0.686274509803922,
0.689542483660131,0.69281045751634,0.696078431372549,0.699346405228758,
0.702614379084967,0.705882352941177,0.709150326797386,0.712418300653595,
0.715686274509804,0.718954248366013,0.722222222222222,0.725490196078431,
0.72875816993464,0.73202614379085,0.735294117647059,0.738562091503268,0.741830065359477,
0.745098039215686,0.748366013071895,0.751633986928105,0.754901960784314,
0.758169934640523,0.761437908496732,0.764705882352941,0.76797385620915,
0.77124183006536,0.774509803921569,0.777777777777778,0.781045751633987,
0.784313725490196,0.787581699346405,0.790849673202614,0.794117647058823,
0.797385620915033,0.800653594771242,0.803921568627451,0.80718954248366,
0.810457516339869,0.813725490196078,0.816993464052288,0.820261437908497,
0.823529411764706,0.826797385620915,0.830065359477124,0.833333333333333,
0.836601307189543,0.839869281045752,0.843137254901961,0.84640522875817,
0.849673202614379,0.852941176470588,0.856209150326797,0.859477124183007,
0.862745098039216,0.866013071895425,0.869281045751634,0.872549019607843,
0.875816993464052,0.879084967320261,0.882352941176471,0.88562091503268,
0.888888888888889,0.892156862745098,0.895424836601307,0.898692810457516,
0.901960784313726,0.905228758169935,0.908496732026144,0.911764705882353,
0.915032679738562,0.918300653594771,0.92156862745098,0.92483660130719,0.928104575163399,
0.931372549019608,0.934640522875817,0.937908496732026,0.941176470588235,
0.944444444444444,0.947712418300654,0.950980392156863,0.954248366013072,
0.957516339869281,0.96078431372549,0.964052287581699,0.967320261437909,
0.970588235294118,0.973856209150327,0.977124183006536,0.980392156862745,
0.983660130718954,0.986928104575163,0.990196078431373,0.993464052287582,
0.996732026143791,1.),.UNSPECIFIED.)
GEOMETRIC_REPRESENTATION_ITEM()
RATIONAL_B_SPLINE_SURFACE(((1.,0.866025403784439,1.,0.866025403784439,1.,
0.866025403784439,1.,0.866025403784439,1.,0.866025403784439,1.,0.866025403784439,
1.,0.866025403784439,1.,0.866025403784439,1.,0.866025403784439,1.,0.866025403784439,
1.,0.866025403784439,1.,0.866025403784439,1.,0.866025403784439,1.,0.866025403784439,
1.,0.866025403784439,1.,0.866025403784439,1.,0.866025403784439,1.,0.866025403784439,
1.,0.866025403784439,1.,0.866025403784439,1.,0.866025403784439,1.,0.866025403784439,
1.,0.866025403784439,1.,0.866025403784439,1.,0.866025403784439,1.,0.866025403784439,
1.,0.866025403784439,1.,0.866025403784439,1.,0.866025403784439,1.,0.866025403784439,
1.,0.866025403784439,1.,0.866025403784439,1.,0.866025403784439,1.,0.866025403784439,
1.,0.866025403784439,1.,0.866025403784439,1.,0.866025403784439,1.,0.866025403784439,
1.,0.866025403784439,1.,0.866025403784439,1.,0.866025403784439,1.,0.866025403784439,
1.,0.866025403784439,1.,0.866025403784439,1.,0.866025403784439,1.,0.866025403784439,
1.,0.866025403784439,1.,0.866025403784439,1.,0.866025403784439,1.,0.866025403784439,
1.,0.866025403784439,1.,0.866025403784439,1.,0.866025403784439,1.,0.866025403784439,
1.,0.866025403784439,1.,0.866025403784439,1.,0.866025403784439,1.,0.866025403784439,
1.,0.866025403784439,1.,0.866025403784439,1.,0.866025403784439,1.,0.866025403784439,
1.,0.866025403784439,1.,0.866025403784439,1.,0.866025403784439,1.,0.866025403784439,
1.,0.866025403784439,1.,0.866025403784439,1.,0.866025403784439,1.,0.866025403784439,
1.,0.866025403784439,1.,0.866025403784439,1.,0.866025403784439,1.,0.866025403784439,
1.,0.866025403784439,1.,0.866025403784439,1.,0.866025403784439,1.,0.866025403784439,
1.,0.866025403784439,1.,0.866025403784439,1.,0.866025403784439,1.,0.866025403784439,
1.,0.866025403784439,1.,0.866025403784439,1.,0.866025403784439,1.,0.866025403784439,
1.,0.866025403784439,1.,0.866025403784439,1.,0.866025403784439,1.,0.866025403784439,
1.,0.866025403784439,1.,0.866025403784439,1.,0.866025403784439,1.,0.866025403784439,
1.,0.866025403784439,1.,0.866025403784439,1.,0.866025403784439,1.,0.866025403784439,
1.,0.866025403784439,1.,0.866025403784439,1.,0.866025403784439,1.,0.866025403784439,
1.,0.866025403784439,1.,0.866025403784439,1.,0.866025403784439,1.,0.866025403784439,
1.,0.866025403784439,1.,0.866025403784439,1.,0.866025403784439,1.,0.866025403784439,
1.,0.866025403784439,1.,0.866025403784439,1.,0.866025403784439,1.,0.866025403784439,
1.,0.866025403784439,1.,0.866025403784439,1.,0.866025403784439,1.,0.866025403784439,
1.,0.866025403784439,1.,0.866025403784439,1.,0.866025403784439,1.,0.866025403784439,
1.,0.866025403784439,1.,0.866025403784439,1.,0.866025403784439,1.,0.866025403784439,
1.,0.866025403784439,1.,0.866025403784439,1.,0.866025403784439,1.,0.866025403784439,
1.,0.866025403784439,1.,0.866025403784439,1.,0.866025403784439,1.,0.866025403784439,
1.,0.866025403784439,1.,0.866025403784439,1.,0.866025403784439,1.,0.866025403784439,
1.,0.866025403784439,1.,0.866025403784439,1.,0.866025403784439,1.,0.866025403784439,
1.,0.866025403784439,1.,0.866025403784439,1.,0.866025403784439,1.,0.866025403784439,
1.,0.866025403784439,1.,0.866025403784439,1.,0.866025403784439,1.,0.866025403784439,
1.,0.866025403784439,1.,0.866025403784439,1.,0.866025403784439,1.,0.866025403784439,
1.,0.866025403784439,1.,0.866025403784439,1.,0.866025403784439,1.,0.866025403784439,
1.,0.866025403784439,1.,0.866025403784439,1.,0.866025403784439,1.,0.866025403784439,
1.,0.866025403784439,1.,0.866025403784439,1.,0.866025403784439,1.,0.866025403784439,
1.,0.866025403784439,1.,0.866025403784439,1.,0.866025403784439,1.,0.866025403784439,
1.,0.866025403784439,1.,0.866025403784439,1.,0.866025403784439,1.,0.866025403784439,
1.,0.866025403784439,1.,0.866025403784439,1.,0.866025403784439,1.,0.866025403784439,
1.,0.866025403784439,1.,0.866025403784439,1.,0.866025403784439,1.,0.866025403784439,
1.,0.866025403784439,1.,0.866025403784439,1.,0.866025403784439,1.,0.866025403784439,
1.,0.866025403784439,1.,0.866025403784439,1.,0.866025403784439,1.,0.866025403784439,
1.,0.866025403784439,1.,0.866025403784439,1.,0.866025403784439,1.,0.866025403784439,
1.,0.866025403784439,1.,0.866025403784439,1.,0.866025403784439,1.,0.866025403784439,
1.,0.866025403784439,1.,0.866025403784439,1.,0.866025403784439,1.,0.866025403784439,
1.,0.866025403784439,1.,0.866025403784439,1.,0.866025403784439,1.,0.866025403784439,
1.,0.866025403784439,1.,0.866025403784439,1.,0.866025403784439,1.,0.866025403784439,
1.,0.866025403784439,1.,0.866025403784439,1.,0.866025403784439,1.,0.866025403784439,
1.,0.866025403784439,1.,0.866025403784439,1.,0.866025403784439,1.,0.866025403784439,
1.,0.866025403784439,1.,0.866025403784439,1.,0.866025403784439,1.,0.866025403784439,
1.,0.866025403784439,1.,0.866025403784439,1.,0.866025403784439,1.,0.866025403784439,
1.,0.866025403784439,1.,0.866025403784439,1.,0.866025403784439,1.,0.866025403784439,
1.,0.866025403784439,1.,0.866025403784439,1.,0.866025403784439,1.,0.866025403784439,
1.,0.866025403784439,1.,0.866025403784439,1.,0.866025403784439,1.,0.866025403784439,
1.,0.866025403784439,1.,0.866025403784439,1.,0.866025403784439,1.,0.866025403784439,
1.,0.866025403784439,1.,0.866025403784439,1.,0.866025403784439,1.,0.866025403784439,
1.,0.866025403784439,1.,0.866025403784439,1.,0.866025403784439,1.,0.866025403784439,
1.,0.866025403784439,1.,0.866025403784439,1.,0.866025403784439,1.,0.866025403784439,
1.,0.866025403784439,1.,0.866025403784439,1.,0.866025403784439,1.,0.866025403784439,
1.,0.866025403784439,1.,0.866025403784439,1.,0.866025403784439,1.,0.866025403784439,
1.,0.866025403784439,1.,0.866025403784439,1.,0.866025403784439,1.,0.866025403784439,
1.,0.866025403784439,1.,0.866025403784439,1.,0.866025403784439,1.,0.866025403784439,
1.,0.866025403784439,1.,0.866025403784439,1.,0.866025403784439,1.,0.866025403784439,
1.,0.866025403784439,1.,0.866025403784439,1.,0.866025403784439,1.,0.866025403784439,
1.,0.866025403784439,1.,0.866025403784439,1.,0.866025403784439,1.,0.866025403784439,
1.,0.866025403784439,1.,0.866025403784439,1.,0.866025403784439,1.,0.866025403784439,
1.,0.866025403784439,1.,0.866025403784439,1.,0.866025403784439,1.,0.866025403784439,
1.,0.866025403784439,1.,0.866025403784439,1.,0.866025403784439,1.,0.866025403784439,
1.,0.866025403784439,1.,0.866025403784439,1.,0.866025403784439,1.,0.866025403784439,
1.,0.866025403784439,1.,0.866025403784439,1.,0.866025403784439,1.,0.866025403784439,
1.,0.866025403784439,1.,0.866025403784439,1.,0.866025403784439,1.,0.866025403784439,
1.),(1.,0.866025403784439,1.,0.866025403784439,1.,0.866025403784439,1.,
0.866025403784439,1.,0.866025403784439,1.,0.866025403784439,1.,0.866025403784439,
1.,0.866025403784439,1.,0.866025403784439,1.,0.866025403784439,1.,0.866025403784439,
1.,0.866025403784439,1.,0.866025403784439,1.,0.866025403784439,1.,0.866025403784439,
1.,0.866025403784439,1.,0.866025403784439,1.,0.866025403784439,1.,0.866025403784439,
1.,0.866025403784439,1.,0.866025403784439,1.,0.866025403784439,1.,0.866025403784439,
1.,0.866025403784439,1.,0.866025403784439,1.,0.866025403784439,1.,0.866025403784439,
1.,0.866025403784439,1.,0.866025403784439,1.,0.866025403784439,1.,0.866025403784439,
1.,0.866025403784439,1.,0.866025403784439,1.,0.866025403784439,1.,0.866025403784439,
1.,0.866025403784439,1.,0.866025403784439,1.,0.866025403784439,1.,0.866025403784439,
1.,0.866025403784439,1.,0.866025403784439,1.,0.866025403784439,1.,0.866025403784439,
1.,0.866025403784439,1.,0.866025403784439,1.,0.866025403784439,1.,0.866025403784439,
1.,0.866025403784439,1.,0.866025403784439,1.,0.866025403784439,1.,0.866025403784439,
1.,0.866025403784439,1.,0.866025403784439,1.,0.866025403784439,1.,0.866025403784439,
1.,0.866025403784439,1.,0.866025403784439,1.,0.866025403784439,1.,0.866025403784439,
1.,0.866025403784439,1.,0.866025403784439,1.,0.866025403784439,1.,0.866025403784439,
1.,0.866025403784439,1.,0.866025403784439,1.,0.866025403784439,1.,0.866025403784439,
1.,0.866025403784439,1.,0.866025403784439,1.,0.866025403784439,1.,0.866025403784439,
1.,0.866025403784439,1.,0.866025403784439,1.,0.866025403784439,1.,0.866025403784439,
1.,0.866025403784439,1.,0.866025403784439,1.,0.866025403784439,1.,0.866025403784439,
1.,0.866025403784439,1.,0.866025403784439,1.,0.866025403784439,1.,0.866025403784439,
1.,0.866025403784439,1.,0.866025403784439,1.,0.866025403784439,1.,0.866025403784439,
1.,0.866025403784439,1.,0.866025403784439,1.,0.866025403784439,1.,0.866025403784439,
1.,0.866025403784439,1.,0.866025403784439,1.,0.866025403784439,1.,0.866025403784439,
1.,0.866025403784439,1.,0.866025403784439,1.,0.866025403784439,1.,0.866025403784439,
1.,0.866025403784439,1.,0.866025403784439,1.,0.866025403784439,1.,0.866025403784439,
1.,0.866025403784439,1.,0.866025403784439,1.,0.866025403784439,1.,0.866025403784439,
1.,0.866025403784439,1.,0.866025403784439,1.,0.866025403784439,1.,0.866025403784439,
1.,0.866025403784439,1.,0.866025403784439,1.,0.866025403784439,1.,0.866025403784439,
1.,0.866025403784439,1.,0.866025403784439,1.,0.866025403784439,1.,0.866025403784439,
1.,0.866025403784439,1.,0.866025403784439,1.,0.866025403784439,1.,0.866025403784439,
1.,0.866025403784439,1.,0.866025403784439,1.,0.866025403784439,1.,0.866025403784439,
1.,0.866025403784439,1.,0.866025403784439,1.,0.866025403784439,1.,0.866025403784439,
1.,0.866025403784439,1.,0.866025403784439,1.,0.866025403784439,1.,0.866025403784439,
1.,0.866025403784439,1.,0.866025403784439,1.,0.866025403784439,1.,0.866025403784439,
1.,0.866025403784439,1.,0.866025403784439,1.,0.866025403784439,1.,0.866025403784439,
1.,0.866025403784439,1.,0.866025403784439,1.,0.866025403784439,1.,0.866025403784439,
1.,0.866025403784439,1.,0.866025403784439,1.,0.866025403784439,1.,0.866025403784439,
1.,0.866025403784439,1.,0.866025403784439,1.,0.866025403784439,1.,0.866025403784439,
1.,0.866025403784439,1.,0.866025403784439,1.,0.866025403784439,1.,0.866025403784439,
1.,0.866025403784439,1.,0.866025403784439,1.,0.866025403784439,1.,0.866025403784439,
1.,0.866025403784439,1.,0.866025403784439,1.,0.866025403784439,1.,0.866025403784439,
1.,0.866025403784439,1.,0.866025403784439,1.,0.866025403784439,1.,0.866025403784439,
1.,0.866025403784439,1.,0.866025403784439,1.,0.866025403784439,1.,0.866025403784439,
1.,0.866025403784439,1.,0.866025403784439,1.,0.866025403784439,1.,0.866025403784439,
1.,0.866025403784439,1.,0.866025403784439,1.,0.866025403784439,1.,0.866025403784439,
1.,0.866025403784439,1.,0.866025403784439,1.,0.866025403784439,1.,0.866025403784439,
1.,0.866025403784439,1.,0.866025403784439,1.,0.866025403784439,1.,0.866025403784439,
1.,0.866025403784439,1.,0.866025403784439,1.,0.866025403784439,1.,0.866025403784439,
1.,0.866025403784439,1.,0.866025403784439,1.,0.866025403784439,1.,0.866025403784439,
1.,0.866025403784439,1.,0.866025403784439,1.,0.866025403784439,1.,0.866025403784439,
1.,0.866025403784439,1.,0.866025403784439,1.,0.866025403784439,1.,0.866025403784439,
1.,0.866025403784439,1.,0.866025403784439,1.,0.866025403784439,1.,0.866025403784439,
1.,0.866025403784439,1.,0.866025403784439,1.,0.866025403784439,1.,0.866025403784439,
1.,0.866025403784439,1.,0.866025403784439,1.,0.866025403784439,1.,0.866025403784439,
1.,0.866025403784439,1.,0.866025403784439,1.,0.866025403784439,1.,0.866025403784439,
1.,0.866025403784439,1.,0.866025403784439,1.,0.866025403784439,1.,0.866025403784439,
1.,0.866025403784439,1.,0.866025403784439,1.,0.866025403784439,1.,0.866025403784439,
1.,0.866025403784439,1.,0.866025403784439,1.,0.866025403784439,1.,0.866025403784439,
1.,0.866025403784439,1.,0.866025403784439,1.,0.866025403784439,1.,0.866025403784439,
1.,0.866025403784439,1.,0.866025403784439,1.,0.866025403784439,1.,0.866025403784439,
1.,0.866025403784439,1.,0.866025403784439,1.,0.866025403784439,1.,0.866025403784439,
1.,0.866025403784439,1.,0.866025403784439,1.,0.866025403784439,1.,0.866025403784439,
1.,0.866025403784439,1.,0.866025403784439,1.,0.866025403784439,1.,0.866025403784439,
1.,0.866025403784439,1.,0.866025403784439,1.,0.866025403784439,1.,0.866025403784439,
1.,0.866025403784439,1.,0.866025403784439,1.,0.866025403784439,1.,0.866025403784439,
1.,0.866025403784439,1.,0.866025403784439,1.,0.866025403784439,1.,0.866025403784439,
1.,0.866025403784439,1.,0.866025403784439,1.,0.866025403784439,1.,0.866025403784439,
1.,0.866025403784439,1.,0.866025403784439,1.,0.866025403784439,1.,0.866025403784439,
1.,0.866025403784439,1.,0.866025403784439,1.,0.866025403784439,1.,0.866025403784439,
1.,0.866025403784439,1.,0.866025403784439,1.,0.866025403784439,1.,0.866025403784439,
1.,0.866025403784439,1.,0.866025403784439,1.,0.866025403784439,1.,0.866025403784439,
1.,0.866025403784439,1.,0.866025403784439,1.,0.866025403784439,1.,0.866025403784439,
1.,0.866025403784439,1.,0.866025403784439,1.,0.866025403784439,1.,0.866025403784439,
1.,0.866025403784439,1.,0.866025403784439,1.,0.866025403784439,1.,0.866025403784439,
1.,0.866025403784439,1.,0.866025403784439,1.,0.866025403784439,1.,0.866025403784439,
1.,0.866025403784439,1.,0.866025403784439,1.,0.866025403784439,1.)))
REPRESENTATION_ITEM('')
SURFACE()
);
#3302=(
BOUNDED_SURFACE()
B_SPLINE_SURFACE(1,2,((#421390,#421391,#421392,#421393,#421394,#421395,
#421396,#421397,#421398,#421399,#421400,#421401,#421402,#421403,#421404,
#421405,#421406,#421407,#421408,#421409,#421410,#421411,#421412,#421413,
#421414,#421415,#421416,#421417,#421418,#421419,#421420,#421421,#421422,
#421423,#421424,#421425,#421426,#421427,#421428,#421429,#421430,#421431,
#421432,#421433,#421434,#421435,#421436,#421437,#421438,#421439,#421440,
#421441,#421442,#421443,#421444,#421445,#421446,#421447,#421448,#421449,
#421450,#421451,#421452,#421453,#421454,#421455,#421456,#421457,#421458,
#421459,#421460,#421461,#421462,#421463,#421464,#421465,#421466,#421467,
#421468,#421469,#421470,#421471,#421472,#421473,#421474,#421475,#421476,
#421477,#421478,#421479,#421480,#421481,#421482,#421483,#421484,#421485,
#421486,#421487,#421488,#421489,#421490,#421491,#421492,#421493,#421494,
#421495,#421496,#421497,#421498,#421499,#421500,#421501,#421502,#421503,
#421504,#421505,#421506,#421507,#421508,#421509,#421510,#421511,#421512,
#421513,#421514,#421515,#421516,#421517,#421518,#421519,#421520,#421521,
#421522,#421523,#421524,#421525,#421526,#421527,#421528,#421529,#421530,
#421531,#421532,#421533,#421534,#421535,#421536,#421537,#421538,#421539,
#421540,#421541,#421542,#421543,#421544,#421545,#421546,#421547,#421548,
#421549,#421550,#421551,#421552,#421553,#421554,#421555,#421556,#421557,
#421558,#421559,#421560,#421561,#421562,#421563,#421564,#421565,#421566,
#421567,#421568,#421569,#421570,#421571,#421572,#421573,#421574,#421575,
#421576,#421577,#421578,#421579,#421580,#421581,#421582,#421583,#421584,
#421585,#421586,#421587,#421588,#421589,#421590,#421591,#421592,#421593,
#421594,#421595,#421596,#421597,#421598,#421599,#421600,#421601,#421602,
#421603,#421604,#421605,#421606,#421607,#421608,#421609,#421610,#421611,
#421612,#421613,#421614,#421615,#421616,#421617,#421618,#421619,#421620,
#421621,#421622,#421623,#421624,#421625,#421626,#421627,#421628,#421629,
#421630,#421631,#421632,#421633,#421634,#421635,#421636,#421637,#421638,
#421639,#421640,#421641,#421642,#421643,#421644,#421645,#421646,#421647,
#421648,#421649,#421650,#421651,#421652,#421653,#421654,#421655,#421656,
#421657,#421658,#421659,#421660,#421661,#421662,#421663,#421664,#421665,
#421666,#421667,#421668,#421669,#421670,#421671,#421672,#421673,#421674,
#421675,#421676,#421677,#421678,#421679,#421680,#421681,#421682,#421683,
#421684,#421685,#421686,#421687,#421688,#421689,#421690,#421691,#421692,
#421693,#421694,#421695,#421696,#421697,#421698,#421699,#421700,#421701,
#421702,#421703,#421704,#421705,#421706,#421707,#421708,#421709,#421710,
#421711,#421712,#421713,#421714,#421715,#421716,#421717,#421718,#421719,
#421720,#421721,#421722,#421723,#421724,#421725,#421726,#421727,#421728,
#421729,#421730,#421731,#421732,#421733,#421734,#421735,#421736,#421737,
#421738,#421739,#421740,#421741,#421742,#421743,#421744,#421745,#421746,
#421747,#421748,#421749,#421750,#421751,#421752,#421753,#421754,#421755,
#421756,#421757,#421758,#421759,#421760,#421761,#421762,#421763,#421764,
#421765,#421766,#421767,#421768,#421769,#421770,#421771,#421772,#421773,
#421774,#421775,#421776,#421777,#421778,#421779,#421780,#421781,#421782,
#421783,#421784,#421785,#421786,#421787,#421788,#421789,#421790,#421791,
#421792,#421793,#421794,#421795,#421796,#421797,#421798,#421799,#421800,
#421801,#421802,#421803,#421804,#421805,#421806,#421807,#421808,#421809,
#421810,#421811,#421812,#421813,#421814,#421815,#421816,#421817,#421818,
#421819,#421820,#421821,#421822,#421823,#421824,#421825,#421826,#421827,
#421828,#421829,#421830,#421831,#421832,#421833,#421834,#421835,#421836,
#421837,#421838,#421839,#421840,#421841,#421842,#421843,#421844,#421845,
#421846,#421847,#421848,#421849,#421850,#421851,#421852,#421853,#421854,
#421855,#421856,#421857,#421858,#421859,#421860,#421861,#421862,#421863,
#421864,#421865,#421866,#421867,#421868,#421869,#421870,#421871,#421872,
#421873,#421874,#421875,#421876,#421877,#421878,#421879,#421880,#421881,
#421882,#421883,#421884,#421885,#421886,#421887,#421888,#421889,#421890,
#421891,#421892,#421893,#421894,#421895,#421896,#421897,#421898,#421899,
#421900,#421901,#421902,#421903,#421904,#421905,#421906,#421907,#421908,
#421909,#421910,#421911,#421912,#421913,#421914,#421915,#421916,#421917,
#421918,#421919,#421920,#421921,#421922,#421923,#421924,#421925,#421926,
#421927,#421928,#421929,#421930,#421931,#421932,#421933,#421934,#421935,
#421936,#421937,#421938,#421939,#421940,#421941,#421942,#421943,#421944,
#421945,#421946,#421947,#421948,#421949,#421950,#421951,#421952,#421953,
#421954,#421955,#421956,#421957,#421958,#421959,#421960,#421961,#421962,
#421963,#421964,#421965,#421966,#421967,#421968,#421969,#421970,#421971,
#421972,#421973,#421974,#421975,#421976,#421977,#421978,#421979,#421980,
#421981,#421982,#421983,#421984,#421985,#421986,#421987,#421988,#421989,
#421990,#421991,#421992,#421993,#421994,#421995,#421996,#421997,#421998,
#421999,#422000,#422001,#422002),(#422003,#422004,#422005,#422006,#422007,
#422008,#422009,#422010,#422011,#422012,#422013,#422014,#422015,#422016,
#422017,#422018,#422019,#422020,#422021,#422022,#422023,#422024,#422025,
#422026,#422027,#422028,#422029,#422030,#422031,#422032,#422033,#422034,
#422035,#422036,#422037,#422038,#422039,#422040,#422041,#422042,#422043,
#422044,#422045,#422046,#422047,#422048,#422049,#422050,#422051,#422052,
#422053,#422054,#422055,#422056,#422057,#422058,#422059,#422060,#422061,
#422062,#422063,#422064,#422065,#422066,#422067,#422068,#422069,#422070,
#422071,#422072,#422073,#422074,#422075,#422076,#422077,#422078,#422079,
#422080,#422081,#422082,#422083,#422084,#422085,#422086,#422087,#422088,
#422089,#422090,#422091,#422092,#422093,#422094,#422095,#422096,#422097,
#422098,#422099,#422100,#422101,#422102,#422103,#422104,#422105,#422106,
#422107,#422108,#422109,#422110,#422111,#422112,#422113,#422114,#422115,
#422116,#422117,#422118,#422119,#422120,#422121,#422122,#422123,#422124,
#422125,#422126,#422127,#422128,#422129,#422130,#422131,#422132,#422133,
#422134,#422135,#422136,#422137,#422138,#422139,#422140,#422141,#422142,
#422143,#422144,#422145,#422146,#422147,#422148,#422149,#422150,#422151,
#422152,#422153,#422154,#422155,#422156,#422157,#422158,#422159,#422160,
#422161,#422162,#422163,#422164,#422165,#422166,#422167,#422168,#422169,
#422170,#422171,#422172,#422173,#422174,#422175,#422176,#422177,#422178,
#422179,#422180,#422181,#422182,#422183,#422184,#422185,#422186,#422187,
#422188,#422189,#422190,#422191,#422192,#422193,#422194,#422195,#422196,
#422197,#422198,#422199,#422200,#422201,#422202,#422203,#422204,#422205,
#422206,#422207,#422208,#422209,#422210,#422211,#422212,#422213,#422214,
#422215,#422216,#422217,#422218,#422219,#422220,#422221,#422222,#422223,
#422224,#422225,#422226,#422227,#422228,#422229,#422230,#422231,#422232,
#422233,#422234,#422235,#422236,#422237,#422238,#422239,#422240,#422241,
#422242,#422243,#422244,#422245,#422246,#422247,#422248,#422249,#422250,
#422251,#422252,#422253,#422254,#422255,#422256,#422257,#422258,#422259,
#422260,#422261,#422262,#422263,#422264,#422265,#422266,#422267,#422268,
#422269,#422270,#422271,#422272,#422273,#422274,#422275,#422276,#422277,
#422278,#422279,#422280,#422281,#422282,#422283,#422284,#422285,#422286,
#422287,#422288,#422289,#422290,#422291,#422292,#422293,#422294,#422295,
#422296,#422297,#422298,#422299,#422300,#422301,#422302,#422303,#422304,
#422305,#422306,#422307,#422308,#422309,#422310,#422311,#422312,#422313,
#422314,#422315,#422316,#422317,#422318,#422319,#422320,#422321,#422322,
#422323,#422324,#422325,#422326,#422327,#422328,#422329,#422330,#422331,
#422332,#422333,#422334,#422335,#422336,#422337,#422338,#422339,#422340,
#422341,#422342,#422343,#422344,#422345,#422346,#422347,#422348,#422349,
#422350,#422351,#422352,#422353,#422354,#422355,#422356,#422357,#422358,
#422359,#422360,#422361,#422362,#422363,#422364,#422365,#422366,#422367,
#422368,#422369,#422370,#422371,#422372,#422373,#422374,#422375,#422376,
#422377,#422378,#422379,#422380,#422381,#422382,#422383,#422384,#422385,
#422386,#422387,#422388,#422389,#422390,#422391,#422392,#422393,#422394,
#422395,#422396,#422397,#422398,#422399,#422400,#422401,#422402,#422403,
#422404,#422405,#422406,#422407,#422408,#422409,#422410,#422411,#422412,
#422413,#422414,#422415,#422416,#422417,#422418,#422419,#422420,#422421,
#422422,#422423,#422424,#422425,#422426,#422427,#422428,#422429,#422430,
#422431,#422432,#422433,#422434,#422435,#422436,#422437,#422438,#422439,
#422440,#422441,#422442,#422443,#422444,#422445,#422446,#422447,#422448,
#422449,#422450,#422451,#422452,#422453,#422454,#422455,#422456,#422457,
#422458,#422459,#422460,#422461,#422462,#422463,#422464,#422465,#422466,
#422467,#422468,#422469,#422470,#422471,#422472,#422473,#422474,#422475,
#422476,#422477,#422478,#422479,#422480,#422481,#422482,#422483,#422484,
#422485,#422486,#422487,#422488,#422489,#422490,#422491,#422492,#422493,
#422494,#422495,#422496,#422497,#422498,#422499,#422500,#422501,#422502,
#422503,#422504,#422505,#422506,#422507,#422508,#422509,#422510,#422511,
#422512,#422513,#422514,#422515,#422516,#422517,#422518,#422519,#422520,
#422521,#422522,#422523,#422524,#422525,#422526,#422527,#422528,#422529,
#422530,#422531,#422532,#422533,#422534,#422535,#422536,#422537,#422538,
#422539,#422540,#422541,#422542,#422543,#422544,#422545,#422546,#422547,
#422548,#422549,#422550,#422551,#422552,#422553,#422554,#422555,#422556,
#422557,#422558,#422559,#422560,#422561,#422562,#422563,#422564,#422565,
#422566,#422567,#422568,#422569,#422570,#422571,#422572,#422573,#422574,
#422575,#422576,#422577,#422578,#422579,#422580,#422581,#422582,#422583,
#422584,#422585,#422586,#422587,#422588,#422589,#422590,#422591,#422592,
#422593,#422594,#422595,#422596,#422597,#422598,#422599,#422600,#422601,
#422602,#422603,#422604,#422605,#422606,#422607,#422608,#422609,#422610,
#422611,#422612,#422613,#422614,#422615)),.UNSPECIFIED.,.F.,.F.,.F.)
B_SPLINE_SURFACE_WITH_KNOTS((2,2),(3,2,2,2,2,2,2,2,2,2,2,2,2,2,2,2,2,2,
2,2,2,2,2,2,2,2,2,2,2,2,2,2,2,2,2,2,2,2,2,2,2,2,2,2,2,2,2,2,2,2,2,2,2,2,
2,2,2,2,2,2,2,2,2,2,2,2,2,2,2,2,2,2,2,2,2,2,2,2,2,2,2,2,2,2,2,2,2,2,2,2,
2,2,2,2,2,2,2,2,2,2,2,2,2,2,2,2,2,2,2,2,2,2,2,2,2,2,2,2,2,2,2,2,2,2,2,2,
2,2,2,2,2,2,2,2,2,2,2,2,2,2,2,2,2,2,2,2,2,2,2,2,2,2,2,2,2,2,2,2,2,2,2,2,
2,2,2,2,2,2,2,2,2,2,2,2,2,2,2,2,2,2,2,2,2,2,2,2,2,2,2,2,2,2,2,2,2,2,2,2,
2,2,2,2,2,2,2,2,2,2,2,2,2,2,2,2,2,2,2,2,2,2,2,2,2,2,2,2,2,2,2,2,2,2,2,2,
2,2,2,2,2,2,2,2,2,2,2,2,2,2,2,2,2,2,2,2,2,2,2,2,2,2,2,2,2,2,2,2,2,2,2,2,
2,2,2,2,2,2,2,2,2,2,2,2,2,2,2,2,2,2,2,2,2,2,2,2,2,2,2,2,2,2,2,2,2,2,2,2,
3),(0.,1.),(0.,0.00326797385620915,0.0065359477124183,0.00980392156862745,
0.0130718954248366,0.0163398692810458,0.0196078431372549,0.0228758169934641,
0.0261437908496732,0.0294117647058824,0.0326797385620915,0.0359477124183007,
0.0392156862745098,0.042483660130719,0.0457516339869281,0.0490196078431373,
0.0522875816993464,0.0555555555555556,0.0588235294117647,0.0620915032679739,
0.065359477124183,0.0686274509803922,0.0718954248366013,0.0751633986928105,
0.0784313725490196,0.0816993464052288,0.0849673202614379,0.0882352941176471,
0.0915032679738562,0.0947712418300654,0.0980392156862745,0.101307189542484,
0.104575163398693,0.107843137254902,0.111111111111111,0.11437908496732,
0.117647058823529,0.120915032679739,0.124183006535948,0.127450980392157,
0.130718954248366,0.133986928104575,0.137254901960784,0.140522875816993,
0.143790849673203,0.147058823529412,0.150326797385621,0.15359477124183,
0.156862745098039,0.160130718954248,0.163398692810458,0.166666666666667,
0.169934640522876,0.173202614379085,0.176470588235294,0.179738562091503,
0.183006535947712,0.186274509803922,0.189542483660131,0.19281045751634,
0.196078431372549,0.199346405228758,0.202614379084967,0.205882352941176,
0.209150326797386,0.212418300653595,0.215686274509804,0.218954248366013,
0.222222222222222,0.225490196078431,0.228758169934641,0.23202614379085,
0.235294117647059,0.238562091503268,0.241830065359477,0.245098039215686,
0.248366013071895,0.251633986928105,0.254901960784314,0.258169934640523,
0.261437908496732,0.264705882352941,0.26797385620915,0.271241830065359,
0.274509803921569,0.277777777777778,0.281045751633987,0.284313725490196,
0.287581699346405,0.290849673202614,0.294117647058824,0.297385620915033,
0.300653594771242,0.303921568627451,0.30718954248366,0.310457516339869,
0.313725490196078,0.316993464052288,0.320261437908497,0.323529411764706,
0.326797385620915,0.330065359477124,0.333333333333333,0.336601307189543,
0.339869281045752,0.343137254901961,0.34640522875817,0.349673202614379,
0.352941176470588,0.356209150326797,0.359477124183007,0.362745098039216,
0.366013071895425,0.369281045751634,0.372549019607843,0.375816993464052,
0.379084967320261,0.382352941176471,0.38562091503268,0.388888888888889,
0.392156862745098,0.395424836601307,0.398692810457516,0.401960784313726,
0.405228758169935,0.408496732026144,0.411764705882353,0.415032679738562,
0.418300653594771,0.42156862745098,0.42483660130719,0.428104575163399,0.431372549019608,
0.434640522875817,0.437908496732026,0.441176470588235,0.444444444444444,
0.447712418300654,0.450980392156863,0.454248366013072,0.457516339869281,
0.46078431372549,0.464052287581699,0.467320261437909,0.470588235294118,
0.473856209150327,0.477124183006536,0.480392156862745,0.483660130718954,
0.486928104575163,0.490196078431373,0.493464052287582,0.496732026143791,
0.5,0.503267973856209,0.506535947712418,0.509803921568627,0.513071895424837,
0.516339869281046,0.519607843137255,0.522875816993464,0.526143790849673,
0.529411764705882,0.532679738562091,0.535947712418301,0.53921568627451,
0.542483660130719,0.545751633986928,0.549019607843137,0.552287581699346,
0.555555555555556,0.558823529411765,0.562091503267974,0.565359477124183,
0.568627450980392,0.571895424836601,0.57516339869281,0.57843137254902,0.581699346405229,
0.584967320261438,0.588235294117647,0.591503267973856,0.594771241830065,
0.598039215686274,0.601307189542484,0.604575163398693,0.607843137254902,
0.611111111111111,0.61437908496732,0.617647058823529,0.620915032679739,
0.624183006535948,0.627450980392157,0.630718954248366,0.633986928104575,
0.637254901960784,0.640522875816993,0.643790849673203,0.647058823529412,
0.650326797385621,0.65359477124183,0.656862745098039,0.660130718954248,
0.663398692810457,0.666666666666667,0.669934640522876,0.673202614379085,
0.676470588235294,0.679738562091503,0.683006535947712,0.686274509803922,
0.689542483660131,0.69281045751634,0.696078431372549,0.699346405228758,
0.702614379084967,0.705882352941177,0.709150326797386,0.712418300653595,
0.715686274509804,0.718954248366013,0.722222222222222,0.725490196078431,
0.72875816993464,0.73202614379085,0.735294117647059,0.738562091503268,0.741830065359477,
0.745098039215686,0.748366013071895,0.751633986928105,0.754901960784314,
0.758169934640523,0.761437908496732,0.764705882352941,0.76797385620915,
0.77124183006536,0.774509803921569,0.777777777777778,0.781045751633987,
0.784313725490196,0.787581699346405,0.790849673202614,0.794117647058823,
0.797385620915033,0.800653594771242,0.803921568627451,0.80718954248366,
0.810457516339869,0.813725490196078,0.816993464052288,0.820261437908497,
0.823529411764706,0.826797385620915,0.830065359477124,0.833333333333333,
0.836601307189543,0.839869281045752,0.843137254901961,0.84640522875817,
0.849673202614379,0.852941176470588,0.856209150326797,0.859477124183007,
0.862745098039216,0.866013071895425,0.869281045751634,0.872549019607843,
0.875816993464052,0.879084967320261,0.882352941176471,0.88562091503268,
0.888888888888889,0.892156862745098,0.895424836601307,0.898692810457516,
0.901960784313726,0.905228758169935,0.908496732026144,0.911764705882353,
0.915032679738562,0.918300653594771,0.92156862745098,0.92483660130719,0.928104575163399,
0.931372549019608,0.934640522875817,0.937908496732026,0.941176470588235,
0.944444444444444,0.947712418300654,0.950980392156863,0.954248366013072,
0.957516339869281,0.96078431372549,0.964052287581699,0.967320261437909,
0.970588235294118,0.973856209150327,0.977124183006536,0.980392156862745,
0.983660130718954,0.986928104575163,0.990196078431373,0.993464052287582,
0.996732026143791,1.),.UNSPECIFIED.)
GEOMETRIC_REPRESENTATION_ITEM()
RATIONAL_B_SPLINE_SURFACE(((1.,0.866025403784439,1.,0.866025403784439,1.,
0.866025403784439,1.,0.866025403784439,1.,0.866025403784439,1.,0.866025403784439,
1.,0.866025403784439,1.,0.866025403784439,1.,0.866025403784439,1.,0.866025403784439,
1.,0.866025403784439,1.,0.866025403784439,1.,0.866025403784439,1.,0.866025403784439,
1.,0.866025403784439,1.,0.866025403784439,1.,0.866025403784439,1.,0.866025403784439,
1.,0.866025403784439,1.,0.866025403784439,1.,0.866025403784439,1.,0.866025403784439,
1.,0.866025403784439,1.,0.866025403784439,1.,0.866025403784439,1.,0.866025403784439,
1.,0.866025403784439,1.,0.866025403784439,1.,0.866025403784439,1.,0.866025403784439,
1.,0.866025403784439,1.,0.866025403784439,1.,0.866025403784439,1.,0.866025403784439,
1.,0.866025403784439,1.,0.866025403784439,1.,0.866025403784439,1.,0.866025403784439,
1.,0.866025403784439,1.,0.866025403784439,1.,0.866025403784439,1.,0.866025403784439,
1.,0.866025403784439,1.,0.866025403784439,1.,0.866025403784439,1.,0.866025403784439,
1.,0.866025403784439,1.,0.866025403784439,1.,0.866025403784439,1.,0.866025403784439,
1.,0.866025403784439,1.,0.866025403784439,1.,0.866025403784439,1.,0.866025403784439,
1.,0.866025403784439,1.,0.866025403784439,1.,0.866025403784439,1.,0.866025403784439,
1.,0.866025403784439,1.,0.866025403784439,1.,0.866025403784439,1.,0.866025403784439,
1.,0.866025403784439,1.,0.866025403784439,1.,0.866025403784439,1.,0.866025403784439,
1.,0.866025403784439,1.,0.866025403784439,1.,0.866025403784439,1.,0.866025403784439,
1.,0.866025403784439,1.,0.866025403784439,1.,0.866025403784439,1.,0.866025403784439,
1.,0.866025403784439,1.,0.866025403784439,1.,0.866025403784439,1.,0.866025403784439,
1.,0.866025403784439,1.,0.866025403784439,1.,0.866025403784439,1.,0.866025403784439,
1.,0.866025403784439,1.,0.866025403784439,1.,0.866025403784439,1.,0.866025403784439,
1.,0.866025403784439,1.,0.866025403784439,1.,0.866025403784439,1.,0.866025403784439,
1.,0.866025403784439,1.,0.866025403784439,1.,0.866025403784439,1.,0.866025403784439,
1.,0.866025403784439,1.,0.866025403784439,1.,0.866025403784439,1.,0.866025403784439,
1.,0.866025403784439,1.,0.866025403784439,1.,0.866025403784439,1.,0.866025403784439,
1.,0.866025403784439,1.,0.866025403784439,1.,0.866025403784439,1.,0.866025403784439,
1.,0.866025403784439,1.,0.866025403784439,1.,0.866025403784439,1.,0.866025403784439,
1.,0.866025403784439,1.,0.866025403784439,1.,0.866025403784439,1.,0.866025403784439,
1.,0.866025403784439,1.,0.866025403784439,1.,0.866025403784439,1.,0.866025403784439,
1.,0.866025403784439,1.,0.866025403784439,1.,0.866025403784439,1.,0.866025403784439,
1.,0.866025403784439,1.,0.866025403784439,1.,0.866025403784439,1.,0.866025403784439,
1.,0.866025403784439,1.,0.866025403784439,1.,0.866025403784439,1.,0.866025403784439,
1.,0.866025403784439,1.,0.866025403784439,1.,0.866025403784439,1.,0.866025403784439,
1.,0.866025403784439,1.,0.866025403784439,1.,0.866025403784439,1.,0.866025403784439,
1.,0.866025403784439,1.,0.866025403784439,1.,0.866025403784439,1.,0.866025403784439,
1.,0.866025403784439,1.,0.866025403784439,1.,0.866025403784439,1.,0.866025403784439,
1.,0.866025403784439,1.,0.866025403784439,1.,0.866025403784439,1.,0.866025403784439,
1.,0.866025403784439,1.,0.866025403784439,1.,0.866025403784439,1.,0.866025403784439,
1.,0.866025403784439,1.,0.866025403784439,1.,0.866025403784439,1.,0.866025403784439,
1.,0.866025403784439,1.,0.866025403784439,1.,0.866025403784439,1.,0.866025403784439,
1.,0.866025403784439,1.,0.866025403784439,1.,0.866025403784439,1.,0.866025403784439,
1.,0.866025403784439,1.,0.866025403784439,1.,0.866025403784439,1.,0.866025403784439,
1.,0.866025403784439,1.,0.866025403784439,1.,0.866025403784439,1.,0.866025403784439,
1.,0.866025403784439,1.,0.866025403784439,1.,0.866025403784439,1.,0.866025403784439,
1.,0.866025403784439,1.,0.866025403784439,1.,0.866025403784439,1.,0.866025403784439,
1.,0.866025403784439,1.,0.866025403784439,1.,0.866025403784439,1.,0.866025403784439,
1.,0.866025403784439,1.,0.866025403784439,1.,0.866025403784439,1.,0.866025403784439,
1.,0.866025403784439,1.,0.866025403784439,1.,0.866025403784439,1.,0.866025403784439,
1.,0.866025403784439,1.,0.866025403784439,1.,0.866025403784439,1.,0.866025403784439,
1.,0.866025403784439,1.,0.866025403784439,1.,0.866025403784439,1.,0.866025403784439,
1.,0.866025403784439,1.,0.866025403784439,1.,0.866025403784439,1.,0.866025403784439,
1.,0.866025403784439,1.,0.866025403784439,1.,0.866025403784439,1.,0.866025403784439,
1.,0.866025403784439,1.,0.866025403784439,1.,0.866025403784439,1.,0.866025403784439,
1.,0.866025403784439,1.,0.866025403784439,1.,0.866025403784439,1.,0.866025403784439,
1.,0.866025403784439,1.,0.866025403784439,1.,0.866025403784439,1.,0.866025403784439,
1.,0.866025403784439,1.,0.866025403784439,1.,0.866025403784439,1.,0.866025403784439,
1.,0.866025403784439,1.,0.866025403784439,1.,0.866025403784439,1.,0.866025403784439,
1.,0.866025403784439,1.,0.866025403784439,1.,0.866025403784439,1.,0.866025403784439,
1.,0.866025403784439,1.,0.866025403784439,1.,0.866025403784439,1.,0.866025403784439,
1.,0.866025403784439,1.,0.866025403784439,1.,0.866025403784439,1.,0.866025403784439,
1.,0.866025403784439,1.,0.866025403784439,1.,0.866025403784439,1.,0.866025403784439,
1.,0.866025403784439,1.,0.866025403784439,1.,0.866025403784439,1.,0.866025403784439,
1.,0.866025403784439,1.,0.866025403784439,1.,0.866025403784439,1.,0.866025403784439,
1.,0.866025403784439,1.,0.866025403784439,1.,0.866025403784439,1.,0.866025403784439,
1.,0.866025403784439,1.,0.866025403784439,1.,0.866025403784439,1.,0.866025403784439,
1.,0.866025403784439,1.,0.866025403784439,1.,0.866025403784439,1.,0.866025403784439,
1.,0.866025403784439,1.,0.866025403784439,1.,0.866025403784439,1.,0.866025403784439,
1.,0.866025403784439,1.,0.866025403784439,1.,0.866025403784439,1.,0.866025403784439,
1.,0.866025403784439,1.,0.866025403784439,1.,0.866025403784439,1.,0.866025403784439,
1.,0.866025403784439,1.,0.866025403784439,1.,0.866025403784439,1.,0.866025403784439,
1.,0.866025403784439,1.,0.866025403784439,1.,0.866025403784439,1.,0.866025403784439,
1.,0.866025403784439,1.,0.866025403784439,1.,0.866025403784439,1.,0.866025403784439,
1.,0.866025403784439,1.,0.866025403784439,1.,0.866025403784439,1.,0.866025403784439,
1.,0.866025403784439,1.,0.866025403784439,1.,0.866025403784439,1.,0.866025403784439,
1.,0.866025403784439,1.,0.866025403784439,1.,0.866025403784439,1.,0.866025403784439,
1.,0.866025403784439,1.,0.866025403784439,1.,0.866025403784439,1.,0.866025403784439,
1.),(1.,0.866025403784439,1.,0.866025403784439,1.,0.866025403784439,1.,
0.866025403784439,1.,0.866025403784439,1.,0.866025403784439,1.,0.866025403784439,
1.,0.866025403784439,1.,0.866025403784439,1.,0.866025403784439,1.,0.866025403784439,
1.,0.866025403784439,1.,0.866025403784439,1.,0.866025403784439,1.,0.866025403784439,
1.,0.866025403784439,1.,0.866025403784439,1.,0.866025403784439,1.,0.866025403784439,
1.,0.866025403784439,1.,0.866025403784439,1.,0.866025403784439,1.,0.866025403784439,
1.,0.866025403784439,1.,0.866025403784439,1.,0.866025403784439,1.,0.866025403784439,
1.,0.866025403784439,1.,0.866025403784439,1.,0.866025403784439,1.,0.866025403784439,
1.,0.866025403784439,1.,0.866025403784439,1.,0.866025403784439,1.,0.866025403784439,
1.,0.866025403784439,1.,0.866025403784439,1.,0.866025403784439,1.,0.866025403784439,
1.,0.866025403784439,1.,0.866025403784439,1.,0.866025403784439,1.,0.866025403784439,
1.,0.866025403784439,1.,0.866025403784439,1.,0.866025403784439,1.,0.866025403784439,
1.,0.866025403784439,1.,0.866025403784439,1.,0.866025403784439,1.,0.866025403784439,
1.,0.866025403784439,1.,0.866025403784439,1.,0.866025403784439,1.,0.866025403784439,
1.,0.866025403784439,1.,0.866025403784439,1.,0.866025403784439,1.,0.866025403784439,
1.,0.866025403784439,1.,0.866025403784439,1.,0.866025403784439,1.,0.866025403784439,
1.,0.866025403784439,1.,0.866025403784439,1.,0.866025403784439,1.,0.866025403784439,
1.,0.866025403784439,1.,0.866025403784439,1.,0.866025403784439,1.,0.866025403784439,
1.,0.866025403784439,1.,0.866025403784439,1.,0.866025403784439,1.,0.866025403784439,
1.,0.866025403784439,1.,0.866025403784439,1.,0.866025403784439,1.,0.866025403784439,
1.,0.866025403784439,1.,0.866025403784439,1.,0.866025403784439,1.,0.866025403784439,
1.,0.866025403784439,1.,0.866025403784439,1.,0.866025403784439,1.,0.866025403784439,
1.,0.866025403784439,1.,0.866025403784439,1.,0.866025403784439,1.,0.866025403784439,
1.,0.866025403784439,1.,0.866025403784439,1.,0.866025403784439,1.,0.866025403784439,
1.,0.866025403784439,1.,0.866025403784439,1.,0.866025403784439,1.,0.866025403784439,
1.,0.866025403784439,1.,0.866025403784439,1.,0.866025403784439,1.,0.866025403784439,
1.,0.866025403784439,1.,0.866025403784439,1.,0.866025403784439,1.,0.866025403784439,
1.,0.866025403784439,1.,0.866025403784439,1.,0.866025403784439,1.,0.866025403784439,
1.,0.866025403784439,1.,0.866025403784439,1.,0.866025403784439,1.,0.866025403784439,
1.,0.866025403784439,1.,0.866025403784439,1.,0.866025403784439,1.,0.866025403784439,
1.,0.866025403784439,1.,0.866025403784439,1.,0.866025403784439,1.,0.866025403784439,
1.,0.866025403784439,1.,0.866025403784439,1.,0.866025403784439,1.,0.866025403784439,
1.,0.866025403784439,1.,0.866025403784439,1.,0.866025403784439,1.,0.866025403784439,
1.,0.866025403784439,1.,0.866025403784439,1.,0.866025403784439,1.,0.866025403784439,
1.,0.866025403784439,1.,0.866025403784439,1.,0.866025403784439,1.,0.866025403784439,
1.,0.866025403784439,1.,0.866025403784439,1.,0.866025403784439,1.,0.866025403784439,
1.,0.866025403784439,1.,0.866025403784439,1.,0.866025403784439,1.,0.866025403784439,
1.,0.866025403784439,1.,0.866025403784439,1.,0.866025403784439,1.,0.866025403784439,
1.,0.866025403784439,1.,0.866025403784439,1.,0.866025403784439,1.,0.866025403784439,
1.,0.866025403784439,1.,0.866025403784439,1.,0.866025403784439,1.,0.866025403784439,
1.,0.866025403784439,1.,0.866025403784439,1.,0.866025403784439,1.,0.866025403784439,
1.,0.866025403784439,1.,0.866025403784439,1.,0.866025403784439,1.,0.866025403784439,
1.,0.866025403784439,1.,0.866025403784439,1.,0.866025403784439,1.,0.866025403784439,
1.,0.866025403784439,1.,0.866025403784439,1.,0.866025403784439,1.,0.866025403784439,
1.,0.866025403784439,1.,0.866025403784439,1.,0.866025403784439,1.,0.866025403784439,
1.,0.866025403784439,1.,0.866025403784439,1.,0.866025403784439,1.,0.866025403784439,
1.,0.866025403784439,1.,0.866025403784439,1.,0.866025403784439,1.,0.866025403784439,
1.,0.866025403784439,1.,0.866025403784439,1.,0.866025403784439,1.,0.866025403784439,
1.,0.866025403784439,1.,0.866025403784439,1.,0.866025403784439,1.,0.866025403784439,
1.,0.866025403784439,1.,0.866025403784439,1.,0.866025403784439,1.,0.866025403784439,
1.,0.866025403784439,1.,0.866025403784439,1.,0.866025403784439,1.,0.866025403784439,
1.,0.866025403784439,1.,0.866025403784439,1.,0.866025403784439,1.,0.866025403784439,
1.,0.866025403784439,1.,0.866025403784439,1.,0.866025403784439,1.,0.866025403784439,
1.,0.866025403784439,1.,0.866025403784439,1.,0.866025403784439,1.,0.866025403784439,
1.,0.866025403784439,1.,0.866025403784439,1.,0.866025403784439,1.,0.866025403784439,
1.,0.866025403784439,1.,0.866025403784439,1.,0.866025403784439,1.,0.866025403784439,
1.,0.866025403784439,1.,0.866025403784439,1.,0.866025403784439,1.,0.866025403784439,
1.,0.866025403784439,1.,0.866025403784439,1.,0.866025403784439,1.,0.866025403784439,
1.,0.866025403784439,1.,0.866025403784439,1.,0.866025403784439,1.,0.866025403784439,
1.,0.866025403784439,1.,0.866025403784439,1.,0.866025403784439,1.,0.866025403784439,
1.,0.866025403784439,1.,0.866025403784439,1.,0.866025403784439,1.,0.866025403784439,
1.,0.866025403784439,1.,0.866025403784439,1.,0.866025403784439,1.,0.866025403784439,
1.,0.866025403784439,1.,0.866025403784439,1.,0.866025403784439,1.,0.866025403784439,
1.,0.866025403784439,1.,0.866025403784439,1.,0.866025403784439,1.,0.866025403784439,
1.,0.866025403784439,1.,0.866025403784439,1.,0.866025403784439,1.,0.866025403784439,
1.,0.866025403784439,1.,0.866025403784439,1.,0.866025403784439,1.,0.866025403784439,
1.,0.866025403784439,1.,0.866025403784439,1.,0.866025403784439,1.,0.866025403784439,
1.,0.866025403784439,1.,0.866025403784439,1.,0.866025403784439,1.,0.866025403784439,
1.,0.866025403784439,1.,0.866025403784439,1.,0.866025403784439,1.,0.866025403784439,
1.,0.866025403784439,1.,0.866025403784439,1.,0.866025403784439,1.,0.866025403784439,
1.,0.866025403784439,1.,0.866025403784439,1.,0.866025403784439,1.,0.866025403784439,
1.,0.866025403784439,1.,0.866025403784439,1.,0.866025403784439,1.,0.866025403784439,
1.,0.866025403784439,1.,0.866025403784439,1.,0.866025403784439,1.,0.866025403784439,
1.,0.866025403784439,1.,0.866025403784439,1.,0.866025403784439,1.,0.866025403784439,
1.,0.866025403784439,1.,0.866025403784439,1.,0.866025403784439,1.,0.866025403784439,
1.,0.866025403784439,1.,0.866025403784439,1.,0.866025403784439,1.,0.866025403784439,
1.,0.866025403784439,1.,0.866025403784439,1.,0.866025403784439,1.)))
REPRESENTATION_ITEM('')
SURFACE()
);
#3303=(
BOUNDED_SURFACE()
B_SPLINE_SURFACE(3,2,((#422661,#422662,#422663),(#422664,#422665,#422666),
(#422667,#422668,#422669),(#422670,#422671,#422672)),.UNSPECIFIED.,.F.,
 .F.,.F.)
B_SPLINE_SURFACE_WITH_KNOTS((4,4),(3,3),(0.,0.000101260117256738),(0.,1.),
 .UNSPECIFIED.)
GEOMETRIC_REPRESENTATION_ITEM()
RATIONAL_B_SPLINE_SURFACE(((1.,0.79661527883517,1.),(1.,0.795896038055943,
1.),(1.,0.795193354661341,1.),(1.,0.794506193185546,1.)))
REPRESENTATION_ITEM('')
SURFACE()
);
#3304=(
BOUNDED_SURFACE()
B_SPLINE_SURFACE(3,2,((#422705,#422706,#422707),(#422708,#422709,#422710),
(#422711,#422712,#422713),(#422714,#422715,#422716),(#422717,#422718,#422719),
(#422720,#422721,#422722)),.UNSPECIFIED.,.F.,.F.,.F.)
B_SPLINE_SURFACE_WITH_KNOTS((4,2,4),(3,3),(0.,1.66936432462295E-5,3.33872864924589E-5),
(0.,1.),.UNSPECIFIED.)
GEOMETRIC_REPRESENTATION_ITEM()
RATIONAL_B_SPLINE_SURFACE(((1.,0.796615278835174,1.),(1.,0.862310524418132,
1.),(1.,0.923774472010522,1.),(1.,0.923983993203425,1.),(1.,0.862574873720951,
1.),(1.,0.796615278835179,1.)))
REPRESENTATION_ITEM('')
SURFACE()
);
#3305=(
BOUNDED_SURFACE()
B_SPLINE_SURFACE(3,2,((#422724,#422725,#422726),(#422727,#422728,#422729),
(#422730,#422731,#422732),(#422733,#422734,#422735)),.UNSPECIFIED.,.F.,
 .F.,.F.)
B_SPLINE_SURFACE_WITH_KNOTS((4,4),(3,3),(2.85968127239939E-5,9.24681548475817E-5),
(-0.00167900678656536,1.01130827127815),.UNSPECIFIED.)
GEOMETRIC_REPRESENTATION_ITEM()
RATIONAL_B_SPLINE_SURFACE(((1.00059040895218,0.822187541868277,1.00401468696654),
(1.0003652771814,0.889990093671579,1.00248382673389),(1.00016469515013,
0.950399042257932,1.0011199008251),(1.00025604273993,0.922888044286083,
1.0017410499063)))
REPRESENTATION_ITEM('')
SURFACE()
);
#3306=(
BOUNDED_SURFACE()
B_SPLINE_SURFACE(3,2,((#422736,#422737,#422738),(#422739,#422740,#422741),
(#422742,#422743,#422744),(#422745,#422746,#422747)),.UNSPECIFIED.,.F.,
 .F.,.F.)
B_SPLINE_SURFACE_WITH_KNOTS((4,4),(3,3),(-5.22358356749212E-6,5.74594192424277E-5),
(-0.00127120052043463,1.),.UNSPECIFIED.)
GEOMETRIC_REPRESENTATION_ITEM()
RATIONAL_B_SPLINE_SURFACE(((1.0005444931317,0.785835073638803,1.),(1.0004770776747,
0.812351526358854,1.),(1.00044031788582,0.826810216506326,1.),(1.00044777653314,
0.823876514387264,1.)))
REPRESENTATION_ITEM('')
SURFACE()
);
#3307=(
BOUNDED_SURFACE()
B_SPLINE_SURFACE(3,2,((#422749,#422750,#422751),(#422752,#422753,#422754),
(#422755,#422756,#422757),(#422758,#422759,#422760)),.UNSPECIFIED.,.F.,
 .F.,.F.)
B_SPLINE_SURFACE_WITH_KNOTS((4,4),(3,3),(0.,0.000101244905251112),(0.,1.),
 .UNSPECIFIED.)
GEOMETRIC_REPRESENTATION_ITEM()
RATIONAL_B_SPLINE_SURFACE(((1.,0.79661527883517,1.),(1.,0.795896146109807,
1.),(1.,0.795193565796486,1.),(1.,0.794506502889904,1.)))
REPRESENTATION_ITEM('')
SURFACE()
);
#3308=(
BOUNDED_SURFACE()
B_SPLINE_SURFACE(3,2,((#422795,#422796,#422797),(#422798,#422799,#422800),
(#422801,#422802,#422803),(#422804,#422805,#422806)),.UNSPECIFIED.,.F.,
 .F.,.F.)
B_SPLINE_SURFACE_WITH_KNOTS((4,4),(3,3),(-2.71050543121376E-20,4.88747512969881E-5),
(-0.000215805215330801,1.),.UNSPECIFIED.)
GEOMETRIC_REPRESENTATION_ITEM()
RATIONAL_B_SPLINE_SURFACE(((1.00008915600332,0.79343408549978,1.),(1.00008930224985,
0.793095246303315,1.),(1.00008944684607,0.792760230720596,1.),(1.00008958984386,
0.792428918540619,1.)))
REPRESENTATION_ITEM('')
SURFACE()
);
#3309=(
BOUNDED_SURFACE()
B_SPLINE_SURFACE(3,2,((#422808,#422809,#422810),(#422811,#422812,#422813),
(#422814,#422815,#422816),(#422817,#422818,#422819)),.UNSPECIFIED.,.F.,
 .F.,.F.)
B_SPLINE_SURFACE_WITH_KNOTS((4,4),(3,3),(3.22980774337779E-5,9.63764854872251E-5),
(-0.00154325936372869,1.01095292447549),.UNSPECIFIED.)
GEOMETRIC_REPRESENTATION_ITEM()
RATIONAL_B_SPLINE_SURFACE(((1.00023530983299,0.922925743796161,1.00168574728332),
(1.00015136166126,0.950422439594214,1.0010843469906),(1.00033574337398,
0.890029368953955,1.00240524789549),(1.00054260094221,0.822274473168324,
1.0038871646486)))
REPRESENTATION_ITEM('')
SURFACE()
);
#3310=(
BOUNDED_SURFACE()
B_SPLINE_SURFACE(3,2,((#422821,#422822,#422823),(#422824,#422825,#422826),
(#422827,#422828,#422829),(#422830,#422831,#422832),(#422833,#422834,#422835),
(#422836,#422837,#422838)),.UNSPECIFIED.,.F.,.F.,.F.)
B_SPLINE_SURFACE_WITH_KNOTS((4,2,4),(3,3),(3.11708124589583E-19,7.62675010863197E-5,
0.000152535002172639),(0.,1.02152348203076),.UNSPECIFIED.)
GEOMETRIC_REPRESENTATION_ITEM()
RATIONAL_B_SPLINE_SURFACE(((1.,0.789033595401239,1.00908146323695),(1.,
0.857071781054831,1.00615262590431),(1.,0.92208726471071,1.00335390671593),
(1.,0.922394466502383,1.00334068261145),(1.,0.85722438459903,1.00614605678503),
(1.,0.789033595401632,1.00908146323693)))
REPRESENTATION_ITEM('')
SURFACE()
);
#3311=(
BOUNDED_SURFACE()
B_SPLINE_SURFACE(3,2,((#422842,#422843,#422844),(#422845,#422846,#422847),
(#422848,#422849,#422850),(#422851,#422852,#422853)),.UNSPECIFIED.,.F.,
 .F.,.F.)
B_SPLINE_SURFACE_WITH_KNOTS((4,4),(3,3),(3.25260651745651E-19,4.88747512969884E-5),
(-0.000215489857776029,1.),.UNSPECIFIED.)
GEOMETRIC_REPRESENTATION_ITEM()
RATIONAL_B_SPLINE_SURFACE(((1.00008945889744,0.79242898398559,1.),(1.00008931610865,
0.792760296061139,1.),(1.00008917172378,0.793095311538206,1.),(1.000089025691,
0.793434150627846,1.)))
REPRESENTATION_ITEM('')
SURFACE()
);
#3312=(
BOUNDED_SURFACE()
B_SPLINE_SURFACE(3,2,((#422855,#422856,#422857),(#422858,#422859,#422860),
(#422861,#422862,#422863),(#422864,#422865,#422866)),.UNSPECIFIED.,.F.,
 .F.,.F.)
B_SPLINE_SURFACE_WITH_KNOTS((4,4),(3,3),(-5.21974905013087E-6,5.74172395514396E-5),
(-0.00139822857750329,1.00051312364072),.UNSPECIFIED.)
GEOMETRIC_REPRESENTATION_ITEM()
RATIONAL_B_SPLINE_SURFACE(((1.00049256947248,0.823768952244012,1.00018060397851),
(1.00048448215719,0.826662424388296,1.00017763870884),(1.00052427784026,
0.812424361909377,1.00019223006923),(1.00059912365861,0.785646094632743,
1.00021967280233)))
REPRESENTATION_ITEM('')
SURFACE()
);
#3313=(
BOUNDED_SURFACE()
B_SPLINE_SURFACE(3,2,((#422965,#422966,#422967),(#422968,#422969,#422970),
(#422971,#422972,#422973),(#422974,#422975,#422976)),.UNSPECIFIED.,.F.,
 .F.,.F.)
B_SPLINE_SURFACE_WITH_KNOTS((4,4),(3,3),(0.,0.000101260117256738),(0.,1.),
 .UNSPECIFIED.)
GEOMETRIC_REPRESENTATION_ITEM()
RATIONAL_B_SPLINE_SURFACE(((1.,0.796615278835177,1.),(1.,0.795896038055936,
1.),(1.,0.795193354661342,1.),(1.,0.794506193185541,1.)))
REPRESENTATION_ITEM('')
SURFACE()
);
#3314=(
BOUNDED_SURFACE()
B_SPLINE_SURFACE(3,2,((#423014,#423015,#423016),(#423017,#423018,#423019),
(#423020,#423021,#423022),(#423023,#423024,#423025),(#423026,#423027,#423028),
(#423029,#423030,#423031)),.UNSPECIFIED.,.F.,.F.,.F.)
B_SPLINE_SURFACE_WITH_KNOTS((4,2,4),(3,3),(-9.82558218814988E-20,1.66936432462292E-5,
3.33872864924585E-5),(0.,1.),.UNSPECIFIED.)
GEOMETRIC_REPRESENTATION_ITEM()
RATIONAL_B_SPLINE_SURFACE(((1.,0.796615278835176,1.),(1.,0.862310524418132,
1.),(1.,0.923774472010523,1.),(1.,0.923983993203417,1.),(1.,0.86257487372095,
1.),(1.,0.796615278835183,1.)))
REPRESENTATION_ITEM('')
SURFACE()
);
#3315=(
BOUNDED_SURFACE()
B_SPLINE_SURFACE(3,2,((#423068,#423069,#423070),(#423071,#423072,#423073),
(#423074,#423075,#423076),(#423077,#423078,#423079)),.UNSPECIFIED.,.F.,
 .F.,.F.)
B_SPLINE_SURFACE_WITH_KNOTS((4,4),(3,3),(-2.16840434497101E-19,0.000101244905251112),
(0.,1.),.UNSPECIFIED.)
GEOMETRIC_REPRESENTATION_ITEM()
RATIONAL_B_SPLINE_SURFACE(((1.,0.796615278835171,1.),(1.,0.795896146109795,
1.),(1.,0.795193565796499,1.),(1.,0.794506502889901,1.)))
REPRESENTATION_ITEM('')
SURFACE()
);
#3316=(
BOUNDED_SURFACE()
B_SPLINE_SURFACE(3,2,((#423115,#423116,#423117),(#423118,#423119,#423120),
(#423121,#423122,#423123),(#423124,#423125,#423126)),.UNSPECIFIED.,.F.,
 .F.,.F.)
B_SPLINE_SURFACE_WITH_KNOTS((4,4),(3,3),(2.85968127239939E-5,9.24681548475818E-5),
(-0.0016790067865349,1.01130827127819),.UNSPECIFIED.)
GEOMETRIC_REPRESENTATION_ITEM()
RATIONAL_B_SPLINE_SURFACE(((1.00059040895216,0.822187541868271,1.00401468696656),
(1.00036527718139,0.889990093671581,1.0024838267339),(1.00016469515013,
0.950399042257933,1.00111990082511),(1.00025604273992,0.922888044286082,
1.00174104990631)))
REPRESENTATION_ITEM('')
SURFACE()
);
#3317=(
BOUNDED_SURFACE()
B_SPLINE_SURFACE(3,2,((#423130,#423131,#423132),(#423133,#423134,#423135),
(#423136,#423137,#423138),(#423139,#423140,#423141)),.UNSPECIFIED.,.F.,
 .F.,.F.)
B_SPLINE_SURFACE_WITH_KNOTS((4,4),(3,3),(-5.22358356749282E-6,5.74594192424278E-5),
(-0.00127120052060601,1.),.UNSPECIFIED.)
GEOMETRIC_REPRESENTATION_ITEM()
RATIONAL_B_SPLINE_SURFACE(((1.00054449313177,0.785835073638756,1.),(1.00047707767477,
0.81235152635884,1.),(1.00044031788588,0.826810216506276,1.),(1.0004477765332,
0.823876514387247,1.)))
REPRESENTATION_ITEM('')
SURFACE()
);
#3318=(
BOUNDED_SURFACE()
B_SPLINE_SURFACE(3,2,((#423143,#423144,#423145),(#423146,#423147,#423148),
(#423149,#423150,#423151),(#423152,#423153,#423154)),.UNSPECIFIED.,.F.,
 .F.,.F.)
B_SPLINE_SURFACE_WITH_KNOTS((4,4),(3,3),(1.0842021724855E-19,4.88747512969881E-5),
(-0.000215805215834578,1.),.UNSPECIFIED.)
GEOMETRIC_REPRESENTATION_ITEM()
RATIONAL_B_SPLINE_SURFACE(((1.00008915600353,0.793434085499676,1.),(1.00008930225006,
0.793095246303207,1.),(1.00008944684628,0.792760230720503,1.),(1.00008958984407,
0.792428918540515,1.)))
REPRESENTATION_ITEM('')
SURFACE()
);
#3319=(
BOUNDED_SURFACE()
B_SPLINE_SURFACE(3,2,((#423156,#423157,#423158),(#423159,#423160,#423161),
(#423162,#423163,#423164),(#423165,#423166,#423167),(#423168,#423169,#423170),
(#423171,#423172,#423173)),.UNSPECIFIED.,.F.,.F.,.F.)
B_SPLINE_SURFACE_WITH_KNOTS((4,2,4),(3,3),(1.6940658945086E-19,7.62675010863196E-5,
0.000152535002172639),(0.,1.0215234820306),.UNSPECIFIED.)
GEOMETRIC_REPRESENTATION_ITEM()
RATIONAL_B_SPLINE_SURFACE(((1.,0.789033595401268,1.00908146323688),(1.,
0.857071781054856,1.00615262590426),(1.,0.922087264710712,1.00335390671591),
(1.,0.922394466502396,1.00334068261142),(1.,0.857224384599053,1.00614605678498),
(1.,0.789033595401663,1.00908146323686)))
REPRESENTATION_ITEM('')
SURFACE()
);
#3320=(
BOUNDED_SURFACE()
B_SPLINE_SURFACE(3,2,((#423175,#423176,#423177),(#423178,#423179,#423180),
(#423181,#423182,#423183),(#423184,#423185,#423186)),.UNSPECIFIED.,.F.,
 .F.,.F.)
B_SPLINE_SURFACE_WITH_KNOTS((4,4),(3,3),(1.62630325872826E-19,4.88747512969884E-5),
(-0.000215489857172023,1.),.UNSPECIFIED.)
GEOMETRIC_REPRESENTATION_ITEM()
RATIONAL_B_SPLINE_SURFACE(((1.00008945889719,0.792428983985717,1.),(1.0000893161084,
0.792760296061256,1.),(1.00008917172353,0.793095311538344,1.),(1.00008902569076,
0.793434150627968,1.)))
REPRESENTATION_ITEM('')
SURFACE()
);
#3321=(
BOUNDED_SURFACE()
B_SPLINE_SURFACE(3,2,((#423188,#423189,#423190),(#423191,#423192,#423193),
(#423194,#423195,#423196),(#423197,#423198,#423199)),.UNSPECIFIED.,.F.,
 .F.,.F.)
B_SPLINE_SURFACE_WITH_KNOTS((4,4),(3,3),(-5.21974905013089E-6,5.74172395514394E-5),
(-0.00139822857781282,1.00051312364071),.UNSPECIFIED.)
GEOMETRIC_REPRESENTATION_ITEM()
RATIONAL_B_SPLINE_SURFACE(((1.00049256947259,0.823768952243961,1.00018060397851),
(1.0004844821573,0.826662424388242,1.00017763870884),(1.00052427784038,
0.812424361909329,1.00019223006923),(1.00059912365874,0.785646094632678,
1.00021967280233)))
REPRESENTATION_ITEM('')
SURFACE()
);
#3322=(
BOUNDED_SURFACE()
B_SPLINE_SURFACE(3,2,((#423203,#423204,#423205),(#423206,#423207,#423208),
(#423209,#423210,#423211),(#423212,#423213,#423214)),.UNSPECIFIED.,.F.,
 .F.,.F.)
B_SPLINE_SURFACE_WITH_KNOTS((4,4),(3,3),(3.2298077433778E-5,9.63764854872258E-5),
(-0.00154325936401433,1.01095292447554),.UNSPECIFIED.)
GEOMETRIC_REPRESENTATION_ITEM()
RATIONAL_B_SPLINE_SURFACE(((1.00023530983303,0.922925743796134,1.00168574728333),
(1.00015136166128,0.950422439594194,1.00108434699061),(1.00033574337404,
0.890029368953921,1.0024052478955),(1.00054260094231,0.822274473168267,
1.00388716464862)))
REPRESENTATION_ITEM('')
SURFACE()
);
#3323=(
BOUNDED_SURFACE()
B_SPLINE_SURFACE(3,2,((#423314,#423315,#423316),(#423317,#423318,#423319),
(#423320,#423321,#423322),(#423323,#423324,#423325)),.UNSPECIFIED.,.F.,
 .F.,.F.)
B_SPLINE_SURFACE_WITH_KNOTS((4,4),(3,3),(0.,0.000101260117256737),(0.,1.),
 .UNSPECIFIED.)
GEOMETRIC_REPRESENTATION_ITEM()
RATIONAL_B_SPLINE_SURFACE(((1.,0.796615278835173,1.),(1.,0.795896038055955,
1.),(1.,0.795193354661339,1.),(1.,0.794506193185541,1.)))
REPRESENTATION_ITEM('')
SURFACE()
);
#3324=(
BOUNDED_SURFACE()
B_SPLINE_SURFACE(3,2,((#423363,#423364,#423365),(#423366,#423367,#423368),
(#423369,#423370,#423371),(#423372,#423373,#423374),(#423375,#423376,#423377),
(#423378,#423379,#423380)),.UNSPECIFIED.,.F.,.F.,.F.)
B_SPLINE_SURFACE_WITH_KNOTS((4,2,4),(3,3),(1.575481281893E-19,1.66936432462295E-5,
3.33872864924588E-5),(0.,1.),.UNSPECIFIED.)
GEOMETRIC_REPRESENTATION_ITEM()
RATIONAL_B_SPLINE_SURFACE(((1.,0.796615278835179,1.),(1.,0.862310524418127,
1.),(1.,0.923774472010525,1.),(1.,0.923983993203428,1.),(1.,0.86257487372094,
1.),(1.,0.796615278835181,1.)))
REPRESENTATION_ITEM('')
SURFACE()
);
#3325=(
BOUNDED_SURFACE()
B_SPLINE_SURFACE(3,2,((#423417,#423418,#423419),(#423420,#423421,#423422),
(#423423,#423424,#423425),(#423426,#423427,#423428)),.UNSPECIFIED.,.F.,
 .F.,.F.)
B_SPLINE_SURFACE_WITH_KNOTS((4,4),(3,3),(-2.16840434497101E-19,0.000101244905251112),
(0.,1.),.UNSPECIFIED.)
GEOMETRIC_REPRESENTATION_ITEM()
RATIONAL_B_SPLINE_SURFACE(((1.,0.79661527883517,1.),(1.,0.795896146109793,
1.),(1.,0.795193565796494,1.),(1.,0.794506502889899,1.)))
REPRESENTATION_ITEM('')
SURFACE()
);
#3326=(
BOUNDED_SURFACE()
B_SPLINE_SURFACE(3,2,((#423464,#423465,#423466),(#423467,#423468,#423469),
(#423470,#423471,#423472),(#423473,#423474,#423475)),.UNSPECIFIED.,.F.,
 .F.,.F.)
B_SPLINE_SURFACE_WITH_KNOTS((4,4),(3,3),(2.85968127239939E-5,9.24681548475817E-5),
(-0.00167900678765756,1.01130827127822),.UNSPECIFIED.)
GEOMETRIC_REPRESENTATION_ITEM()
RATIONAL_B_SPLINE_SURFACE(((1.00059040895256,0.822187541868073,1.00401468696657),
(1.00036527718164,0.889990093671443,1.00248382673391),(1.00016469515024,
0.95039904225788,1.00111990082511),(1.00025604274009,0.922888044285994,
1.00174104990631)))
REPRESENTATION_ITEM('')
SURFACE()
);
#3327=(
BOUNDED_SURFACE()
B_SPLINE_SURFACE(3,2,((#423479,#423480,#423481),(#423482,#423483,#423484),
(#423485,#423486,#423487),(#423488,#423489,#423490)),.UNSPECIFIED.,.F.,
 .F.,.F.)
B_SPLINE_SURFACE_WITH_KNOTS((4,4),(3,3),(-5.22358356749279E-6,5.74594192424278E-5),
(-0.00127120052058266,1.),.UNSPECIFIED.)
GEOMETRIC_REPRESENTATION_ITEM()
RATIONAL_B_SPLINE_SURFACE(((1.00054449313176,0.785835073638761,1.),(1.00047707767476,
0.812351526358851,1.),(1.00044031788587,0.826810216506278,1.),(1.0004477765332,
0.823876514387255,1.)))
REPRESENTATION_ITEM('')
SURFACE()
);
#3328=(
BOUNDED_SURFACE()
B_SPLINE_SURFACE(3,2,((#423492,#423493,#423494),(#423495,#423496,#423497),
(#423498,#423499,#423500),(#423501,#423502,#423503)),.UNSPECIFIED.,.F.,
 .F.,.F.)
B_SPLINE_SURFACE_WITH_KNOTS((4,4),(3,3),(-5.96311194867027E-19,4.88747512969881E-5),
(-0.000215805215785883,1.),.UNSPECIFIED.)
GEOMETRIC_REPRESENTATION_ITEM()
RATIONAL_B_SPLINE_SURFACE(((1.00008915600351,0.793434085499684,1.),(1.00008930225004,
0.793095246303244,1.),(1.00008944684626,0.79276023072049,1.),(1.00008958984405,
0.792428918540532,1.)))
REPRESENTATION_ITEM('')
SURFACE()
);
#3329=(
BOUNDED_SURFACE()
B_SPLINE_SURFACE(3,2,((#423505,#423506,#423507),(#423508,#423509,#423510),
(#423511,#423512,#423513),(#423514,#423515,#423516),(#423517,#423518,#423519),
(#423520,#423521,#423522)),.UNSPECIFIED.,.F.,.F.,.F.)
B_SPLINE_SURFACE_WITH_KNOTS((4,2,4),(3,3),(1.76182853028894E-19,7.62675010863197E-5,
0.000152535002172639),(0.,1.0215234820307),.UNSPECIFIED.)
GEOMETRIC_REPRESENTATION_ITEM()
RATIONAL_B_SPLINE_SURFACE(((1.,0.789033595401244,1.00908146323693),(1.,
0.857071781054812,1.00615262590429),(1.,0.922087264710758,1.00335390671592),
(1.,0.922394466502343,1.00334068261144),(1.,0.857224384599075,1.00614605678501),
(1.,0.789033595401637,1.00908146323691)))
REPRESENTATION_ITEM('')
SURFACE()
);
#3330=(
BOUNDED_SURFACE()
B_SPLINE_SURFACE(3,2,((#423524,#423525,#423526),(#423527,#423528,#423529),
(#423530,#423531,#423532),(#423533,#423534,#423535)),.UNSPECIFIED.,.F.,
 .F.,.F.)
B_SPLINE_SURFACE_WITH_KNOTS((4,4),(3,3),(5.42101086242752E-20,4.88747512969881E-5),
(-0.00021548985687673,1.),.UNSPECIFIED.)
GEOMETRIC_REPRESENTATION_ITEM()
RATIONAL_B_SPLINE_SURFACE(((1.00008945889707,0.792428983985781,1.),(1.00008931610828,
0.792760296061318,1.),(1.00008917172341,0.793095311538399,1.),(1.00008902569063,
0.793434150628026,1.)))
REPRESENTATION_ITEM('')
SURFACE()
);
#3331=(
BOUNDED_SURFACE()
B_SPLINE_SURFACE(3,2,((#423537,#423538,#423539),(#423540,#423541,#423542),
(#423543,#423544,#423545),(#423546,#423547,#423548)),.UNSPECIFIED.,.F.,
 .F.,.F.)
B_SPLINE_SURFACE_WITH_KNOTS((4,4),(3,3),(-5.2197490501309E-6,5.74172395514395E-5),
(-0.00139822857796642,1.00051312364078),.UNSPECIFIED.)
GEOMETRIC_REPRESENTATION_ITEM()
RATIONAL_B_SPLINE_SURFACE(((1.00049256947265,0.82376895224392,1.00018060397853),
(1.00048448215735,0.826662424388195,1.00017763870886),(1.00052427784044,
0.81242436190929,1.00019223006926),(1.0005991236588,0.785646094632626,1.00021967280236)))
REPRESENTATION_ITEM('')
SURFACE()
);
#3332=(
BOUNDED_SURFACE()
B_SPLINE_SURFACE(3,2,((#423552,#423553,#423554),(#423555,#423556,#423557),
(#423558,#423559,#423560),(#423561,#423562,#423563)),.UNSPECIFIED.,.F.,
 .F.,.F.)
B_SPLINE_SURFACE_WITH_KNOTS((4,4),(3,3),(3.2298077433778E-5,9.6376485487226E-5),
(-0.00154325936299762,1.01095292447557),.UNSPECIFIED.)
GEOMETRIC_REPRESENTATION_ITEM()
RATIONAL_B_SPLINE_SURFACE(((1.00023530983288,0.922925743796211,1.00168574728333),
(1.00015136166118,0.950422439594257,1.00108434699061),(1.00033574337382,
0.89002936895402,1.00240524789551),(1.00054260094195,0.822274473168449,
1.00388716464863)))
REPRESENTATION_ITEM('')
SURFACE()
);
#3333=(
BOUNDED_SURFACE()
B_SPLINE_SURFACE(3,2,((#423663,#423664,#423665),(#423666,#423667,#423668),
(#423669,#423670,#423671),(#423672,#423673,#423674)),.UNSPECIFIED.,.F.,
 .F.,.F.)
B_SPLINE_SURFACE_WITH_KNOTS((4,4),(3,3),(0.,0.000101260117256738),(0.,1.),
 .UNSPECIFIED.)
GEOMETRIC_REPRESENTATION_ITEM()
RATIONAL_B_SPLINE_SURFACE(((1.,0.796615278835171,1.),(1.,0.795896038055935,
1.),(1.,0.795193354661353,1.),(1.,0.794506193185547,1.)))
REPRESENTATION_ITEM('')
SURFACE()
);
#3334=(
BOUNDED_SURFACE()
B_SPLINE_SURFACE(3,2,((#423712,#423713,#423714),(#423715,#423716,#423717),
(#423718,#423719,#423720),(#423721,#423722,#423723),(#423724,#423725,#423726),
(#423727,#423728,#423729)),.UNSPECIFIED.,.F.,.F.,.F.)
B_SPLINE_SURFACE_WITH_KNOTS((4,2,4),(3,3),(2.62580213648833E-19,1.66936432462296E-5,
3.33872864924589E-5),(0.,1.),.UNSPECIFIED.)
GEOMETRIC_REPRESENTATION_ITEM()
RATIONAL_B_SPLINE_SURFACE(((1.,0.796615278835186,1.),(1.,0.86231052441813,
1.),(1.,0.923774472010517,1.),(1.,0.923983993203428,1.),(1.,0.862574873720945,
1.),(1.,0.796615278835189,1.)))
REPRESENTATION_ITEM('')
SURFACE()
);
#3335=(
BOUNDED_SURFACE()
B_SPLINE_SURFACE(3,2,((#423766,#423767,#423768),(#423769,#423770,#423771),
(#423772,#423773,#423774),(#423775,#423776,#423777)),.UNSPECIFIED.,.F.,
 .F.,.F.)
B_SPLINE_SURFACE_WITH_KNOTS((4,4),(3,3),(-2.16840434497101E-19,0.000101244905251112),
(0.,1.),.UNSPECIFIED.)
GEOMETRIC_REPRESENTATION_ITEM()
RATIONAL_B_SPLINE_SURFACE(((1.,0.796615278835176,1.),(1.,0.795896146109783,
1.),(1.,0.795193565796507,1.),(1.,0.794506502889895,1.)))
REPRESENTATION_ITEM('')
SURFACE()
);
#3336=(
BOUNDED_SURFACE()
B_SPLINE_SURFACE(3,2,((#423813,#423814,#423815),(#423816,#423817,#423818),
(#423819,#423820,#423821),(#423822,#423823,#423824)),.UNSPECIFIED.,.F.,
 .F.,.F.)
B_SPLINE_SURFACE_WITH_KNOTS((4,4),(3,3),(2.85968127239939E-5,9.24681548475817E-5),
(-0.00167900678632471,1.0113082712783),.UNSPECIFIED.)
GEOMETRIC_REPRESENTATION_ITEM()
RATIONAL_B_SPLINE_SURFACE(((1.00059040895209,0.822187541868296,1.00401468696659),
(1.00036527718135,0.889990093671586,1.00248382673393),(1.00016469515011,
0.950399042257937,1.00111990082512),(1.00025604273989,0.922888044286091,
1.00174104990632)))
REPRESENTATION_ITEM('')
SURFACE()
);
#3337=(
BOUNDED_SURFACE()
B_SPLINE_SURFACE(3,2,((#423828,#423829,#423830),(#423831,#423832,#423833),
(#423834,#423835,#423836),(#423837,#423838,#423839)),.UNSPECIFIED.,.F.,
 .F.,.F.)
B_SPLINE_SURFACE_WITH_KNOTS((4,4),(3,3),(-5.22358356749309E-6,5.74594192424276E-5),
(-0.00127120052057909,1.),.UNSPECIFIED.)
GEOMETRIC_REPRESENTATION_ITEM()
RATIONAL_B_SPLINE_SURFACE(((1.00054449313176,0.785835073638766,1.),(1.00047707767476,
0.812351526358829,1.),(1.00044031788587,0.826810216506286,1.),(1.00044777653319,
0.823876514387251,1.)))
REPRESENTATION_ITEM('')
SURFACE()
);
#3338=(
BOUNDED_SURFACE()
B_SPLINE_SURFACE(3,2,((#423841,#423842,#423843),(#423844,#423845,#423846),
(#423847,#423848,#423849),(#423850,#423851,#423852)),.UNSPECIFIED.,.F.,
 .F.,.F.)
B_SPLINE_SURFACE_WITH_KNOTS((4,4),(3,3),(1.89735380184963E-19,4.88747512969881E-5),
(-0.000215805215101959,1.),.UNSPECIFIED.)
GEOMETRIC_REPRESENTATION_ITEM()
RATIONAL_B_SPLINE_SURFACE(((1.00008915600322,0.793434085499828,1.),(1.00008930224975,
0.793095246303358,1.),(1.00008944684597,0.792760230720646,1.),(1.00008958984377,
0.792428918540672,1.)))
REPRESENTATION_ITEM('')
SURFACE()
);
#3339=(
BOUNDED_SURFACE()
B_SPLINE_SURFACE(3,2,((#423854,#423855,#423856),(#423857,#423858,#423859),
(#423860,#423861,#423862),(#423863,#423864,#423865),(#423866,#423867,#423868),
(#423869,#423870,#423871)),.UNSPECIFIED.,.F.,.F.,.F.)
B_SPLINE_SURFACE_WITH_KNOTS((4,2,4),(3,3),(3.59141969635823E-19,7.62675010863197E-5,
0.000152535002172639),(0.,1.02152348203076),.UNSPECIFIED.)
GEOMETRIC_REPRESENTATION_ITEM()
RATIONAL_B_SPLINE_SURFACE(((1.,0.789033595401229,1.00908146323695),(1.,
0.857071781054903,1.00615262590431),(1.,0.92208726471063,1.00335390671594),
(1.,0.922394466502466,1.00334068261144),(1.,0.857224384598969,1.00614605678503),
(1.,0.789033595401633,1.00908146323693)))
REPRESENTATION_ITEM('')
SURFACE()
);
#3340=(
BOUNDED_SURFACE()
B_SPLINE_SURFACE(3,2,((#423873,#423874,#423875),(#423876,#423877,#423878),
(#423879,#423880,#423881),(#423882,#423883,#423884)),.UNSPECIFIED.,.F.,
 .F.,.F.)
B_SPLINE_SURFACE_WITH_KNOTS((4,4),(3,3),(2.71050543121376E-19,4.88747512969885E-5),
(-0.000215489856772561,1.),.UNSPECIFIED.)
GEOMETRIC_REPRESENTATION_ITEM()
RATIONAL_B_SPLINE_SURFACE(((1.00008945889702,0.7924289839858,1.),(1.00008931610824,
0.792760296061343,1.),(1.00008917172336,0.793095311538421,1.),(1.00008902569059,
0.793434150628045,1.)))
REPRESENTATION_ITEM('')
SURFACE()
);
#3341=(
BOUNDED_SURFACE()
B_SPLINE_SURFACE(3,2,((#423886,#423887,#423888),(#423889,#423890,#423891),
(#423892,#423893,#423894),(#423895,#423896,#423897)),.UNSPECIFIED.,.F.,
 .F.,.F.)
B_SPLINE_SURFACE_WITH_KNOTS((4,4),(3,3),(-5.21974905013086E-6,5.74172395514396E-5),
(-0.0013982285779389,1.00051312364084),.UNSPECIFIED.)
GEOMETRIC_REPRESENTATION_ITEM()
RATIONAL_B_SPLINE_SURFACE(((1.00049256947264,0.823768952243901,1.00018060397855),
(1.00048448215734,0.826662424388219,1.00017763870888),(1.00052427784043,
0.812424361909253,1.00019223006928),(1.00059912365879,0.785646094632636,
1.00021967280238)))
REPRESENTATION_ITEM('')
SURFACE()
);
#3342=(
BOUNDED_SURFACE()
B_SPLINE_SURFACE(3,2,((#423901,#423902,#423903),(#423904,#423905,#423906),
(#423907,#423908,#423909),(#423910,#423911,#423912)),.UNSPECIFIED.,.F.,
 .F.,.F.)
B_SPLINE_SURFACE_WITH_KNOTS((4,4),(3,3),(3.2298077433778E-5,9.63764854872258E-5),
(-0.00154325936356293,1.01095292447534),.UNSPECIFIED.)
GEOMETRIC_REPRESENTATION_ITEM()
RATIONAL_B_SPLINE_SURFACE(((1.00023530983296,0.922925743796183,1.00168574728329),
(1.00015136166124,0.950422439594232,1.00108434699059),(1.00033574337395,
0.890029368953982,1.00240524789546),(1.00054260094215,0.822274473168385,
1.00388716464855)))
REPRESENTATION_ITEM('')
SURFACE()
);
#3343=(
BOUNDED_SURFACE()
B_SPLINE_SURFACE(3,2,((#424012,#424013,#424014),(#424015,#424016,#424017),
(#424018,#424019,#424020),(#424021,#424022,#424023)),.UNSPECIFIED.,.F.,
 .F.,.F.)
B_SPLINE_SURFACE_WITH_KNOTS((4,4),(3,3),(-2.16840434497101E-19,0.000101260117256738),
(0.,1.),.UNSPECIFIED.)
GEOMETRIC_REPRESENTATION_ITEM()
RATIONAL_B_SPLINE_SURFACE(((1.,0.796615278835176,1.),(1.,0.795896038055943,
1.),(1.,0.795193354661342,1.),(1.,0.794506193185552,1.)))
REPRESENTATION_ITEM('')
SURFACE()
);
#3344=(
BOUNDED_SURFACE()
B_SPLINE_SURFACE(3,2,((#424061,#424062,#424063),(#424064,#424065,#424066),
(#424067,#424068,#424069),(#424070,#424071,#424072),(#424073,#424074,#424075),
(#424076,#424077,#424078)),.UNSPECIFIED.,.F.,.F.,.F.)
B_SPLINE_SURFACE_WITH_KNOTS((4,2,4),(3,3),(-1.66018457661843E-19,1.66936432462294E-5,
3.33872864924589E-5),(0.,1.),.UNSPECIFIED.)
GEOMETRIC_REPRESENTATION_ITEM()
RATIONAL_B_SPLINE_SURFACE(((1.,0.796615278835178,1.),(1.,0.862310524418132,
1.),(1.,0.923774472010519,1.),(1.,0.923983993203425,1.),(1.,0.862574873720943,
1.),(1.,0.79661527883518,1.)))
REPRESENTATION_ITEM('')
SURFACE()
);
#3345=(
BOUNDED_SURFACE()
B_SPLINE_SURFACE(3,2,((#424115,#424116,#424117),(#424118,#424119,#424120),
(#424121,#424122,#424123),(#424124,#424125,#424126)),.UNSPECIFIED.,.F.,
 .F.,.F.)
B_SPLINE_SURFACE_WITH_KNOTS((4,4),(3,3),(0.,0.000101244905251112),(0.,1.),
 .UNSPECIFIED.)
GEOMETRIC_REPRESENTATION_ITEM()
RATIONAL_B_SPLINE_SURFACE(((1.,0.796615278835177,1.),(1.,0.795896146109792,
1.),(1.,0.795193565796491,1.),(1.,0.794506502889901,1.)))
REPRESENTATION_ITEM('')
SURFACE()
);
#3346=(
BOUNDED_SURFACE()
B_SPLINE_SURFACE(3,2,((#424162,#424163,#424164),(#424165,#424166,#424167),
(#424168,#424169,#424170),(#424171,#424172,#424173)),.UNSPECIFIED.,.F.,
 .F.,.F.)
B_SPLINE_SURFACE_WITH_KNOTS((4,4),(3,3),(2.85968127239939E-5,9.24681548475815E-5),
(-0.00167900678742142,1.01130827127822),.UNSPECIFIED.)
GEOMETRIC_REPRESENTATION_ITEM()
RATIONAL_B_SPLINE_SURFACE(((1.00059040895248,0.822187541868115,1.00401468696657),
(1.00036527718159,0.889990093671472,1.00248382673391),(1.00016469515022,
0.950399042257889,1.00111990082511),(1.00025604274006,0.922888044286012,
1.00174104990631)))
REPRESENTATION_ITEM('')
SURFACE()
);
#3347=(
BOUNDED_SURFACE()
B_SPLINE_SURFACE(3,2,((#424177,#424178,#424179),(#424180,#424181,#424182),
(#424183,#424184,#424185),(#424186,#424187,#424188)),.UNSPECIFIED.,.F.,
 .F.,.F.)
B_SPLINE_SURFACE_WITH_KNOTS((4,4),(3,3),(-5.22358356749289E-6,5.74594192424278E-5),
(-0.00127120052080811,1.),.UNSPECIFIED.)
GEOMETRIC_REPRESENTATION_ITEM()
RATIONAL_B_SPLINE_SURFACE(((1.00054449313186,0.785835073638708,1.),(1.00047707767484,
0.812351526358813,1.),(1.00044031788595,0.826810216506238,1.),(1.00044777653328,
0.823876514387215,1.)))
REPRESENTATION_ITEM('')
SURFACE()
);
#3348=(
BOUNDED_SURFACE()
B_SPLINE_SURFACE(3,2,((#424190,#424191,#424192),(#424193,#424194,#424195),
(#424196,#424197,#424198),(#424199,#424200,#424201)),.UNSPECIFIED.,.F.,
 .F.,.F.)
B_SPLINE_SURFACE_WITH_KNOTS((4,4),(3,3),(-1.0842021724855E-19,4.88747512969879E-5),
(-0.000215805215245615,1.),.UNSPECIFIED.)
GEOMETRIC_REPRESENTATION_ITEM()
RATIONAL_B_SPLINE_SURFACE(((1.00008915600328,0.793434085499795,1.),(1.00008930224981,
0.793095246303348,1.),(1.00008944684603,0.792760230720603,1.),(1.00008958984383,
0.792428918540643,1.)))
REPRESENTATION_ITEM('')
SURFACE()
);
#3349=(
BOUNDED_SURFACE()
B_SPLINE_SURFACE(3,2,((#424203,#424204,#424205),(#424206,#424207,#424208),
(#424209,#424210,#424211),(#424212,#424213,#424214),(#424215,#424216,#424217),
(#424218,#424219,#424220)),.UNSPECIFIED.,.F.,.F.,.F.)
B_SPLINE_SURFACE_WITH_KNOTS((4,2,4),(3,3),(2.10064170919066E-19,7.62675010863197E-5,
0.000152535002172639),(0.,1.02152348203067),.UNSPECIFIED.)
GEOMETRIC_REPRESENTATION_ITEM()
RATIONAL_B_SPLINE_SURFACE(((1.,0.789033595401254,1.00908146323691),(1.,
0.857071781054834,1.00615262590428),(1.,0.922087264710736,1.00335390671592),
(1.,0.922394466502371,1.00334068261143),(1.,0.857224384599062,1.006146056785),
(1.,0.789033595401649,1.00908146323689)))
REPRESENTATION_ITEM('')
SURFACE()
);
#3350=(
BOUNDED_SURFACE()
B_SPLINE_SURFACE(3,2,((#424222,#424223,#424224),(#424225,#424226,#424227),
(#424228,#424229,#424230),(#424231,#424232,#424233)),.UNSPECIFIED.,.F.,
 .F.,.F.)
B_SPLINE_SURFACE_WITH_KNOTS((4,4),(3,3),(2.16840434497101E-19,4.88747512969881E-5),
(-0.000215489857883573,1.),.UNSPECIFIED.)
GEOMETRIC_REPRESENTATION_ITEM()
RATIONAL_B_SPLINE_SURFACE(((1.00008945889748,0.792428983985569,1.),(1.0000893161087,
0.792760296061112,1.),(1.00008917172382,0.793095311538197,1.),(1.00008902569105,
0.79343415062782,1.)))
REPRESENTATION_ITEM('')
SURFACE()
);
#3351=(
BOUNDED_SURFACE()
B_SPLINE_SURFACE(3,2,((#424235,#424236,#424237),(#424238,#424239,#424240),
(#424241,#424242,#424243),(#424244,#424245,#424246)),.UNSPECIFIED.,.F.,
 .F.,.F.)
B_SPLINE_SURFACE_WITH_KNOTS((4,4),(3,3),(-5.21974905013082E-6,5.74172395514397E-5),
(-0.00139822857780422,1.00051312364062),.UNSPECIFIED.)
GEOMETRIC_REPRESENTATION_ITEM()
RATIONAL_B_SPLINE_SURFACE(((1.00049256947259,0.823768952243966,1.00018060397847),
(1.00048448215729,0.826662424388277,1.0001776387088),(1.00052427784038,
0.812424361909331,1.00019223006919),(1.00059912365873,0.785646094632703,
1.00021967280229)))
REPRESENTATION_ITEM('')
SURFACE()
);
#3352=(
BOUNDED_SURFACE()
B_SPLINE_SURFACE(3,2,((#424250,#424251,#424252),(#424253,#424254,#424255),
(#424256,#424257,#424258),(#424259,#424260,#424261)),.UNSPECIFIED.,.F.,
 .F.,.F.)
B_SPLINE_SURFACE_WITH_KNOTS((4,4),(3,3),(3.22980774337779E-5,9.63764854872256E-5),
(-0.00154325936392538,1.0109529244754),.UNSPECIFIED.)
GEOMETRIC_REPRESENTATION_ITEM()
RATIONAL_B_SPLINE_SURFACE(((1.00023530983302,0.922925743796147,1.0016857472833),
(1.00015136166127,0.950422439594223,1.00108434699059),(1.00033574337402,
0.890029368953931,1.00240524789547),(1.00054260094228,0.822274473168306,
1.00388716464857)))
REPRESENTATION_ITEM('')
SURFACE()
);
#3353=(
BOUNDED_SURFACE()
B_SPLINE_SURFACE(3,2,((#424361,#424362,#424363),(#424364,#424365,#424366),
(#424367,#424368,#424369),(#424370,#424371,#424372)),.UNSPECIFIED.,.F.,
 .F.,.F.)
B_SPLINE_SURFACE_WITH_KNOTS((4,4),(3,3),(0.,0.000101260117256738),(0.,1.),
 .UNSPECIFIED.)
GEOMETRIC_REPRESENTATION_ITEM()
RATIONAL_B_SPLINE_SURFACE(((1.,0.796615278835174,1.),(1.,0.795896038055941,
1.),(1.,0.795193354661351,1.),(1.,0.794506193185546,1.)))
REPRESENTATION_ITEM('')
SURFACE()
);
#3354=(
BOUNDED_SURFACE()
B_SPLINE_SURFACE(3,2,((#424410,#424411,#424412),(#424413,#424414,#424415),
(#424416,#424417,#424418),(#424419,#424420,#424421),(#424422,#424423,#424424),
(#424425,#424426,#424427)),.UNSPECIFIED.,.F.,.F.,.F.)
B_SPLINE_SURFACE_WITH_KNOTS((4,2,4),(3,3),(-8.470329472543E-20,1.66936432462293E-5,
3.33872864924587E-5),(0.,1.),.UNSPECIFIED.)
GEOMETRIC_REPRESENTATION_ITEM()
RATIONAL_B_SPLINE_SURFACE(((1.,0.796615278835174,1.),(1.,0.862310524418127,
1.),(1.,0.923774472010521,1.),(1.,0.923983993203427,1.),(1.,0.862574873720952,
1.),(1.,0.79661527883518,1.)))
REPRESENTATION_ITEM('')
SURFACE()
);
#3355=(
BOUNDED_SURFACE()
B_SPLINE_SURFACE(3,2,((#424464,#424465,#424466),(#424467,#424468,#424469),
(#424470,#424471,#424472),(#424473,#424474,#424475)),.UNSPECIFIED.,.F.,
 .F.,.F.)
B_SPLINE_SURFACE_WITH_KNOTS((4,4),(3,3),(0.,0.000101244905251112),(0.,1.),
 .UNSPECIFIED.)
GEOMETRIC_REPRESENTATION_ITEM()
RATIONAL_B_SPLINE_SURFACE(((1.,0.796615278835171,1.),(1.,0.79589614610979,
1.),(1.,0.795193565796499,1.),(1.,0.7945065028899,1.)))
REPRESENTATION_ITEM('')
SURFACE()
);
#3356=(
BOUNDED_SURFACE()
B_SPLINE_SURFACE(3,2,((#424511,#424512,#424513),(#424514,#424515,#424516),
(#424517,#424518,#424519),(#424520,#424521,#424522)),.UNSPECIFIED.,.F.,
 .F.,.F.)
B_SPLINE_SURFACE_WITH_KNOTS((4,4),(3,3),(2.85968127239939E-5,9.24681548475818E-5),
(-0.00167900678672291,1.01130827127837),.UNSPECIFIED.)
GEOMETRIC_REPRESENTATION_ITEM()
RATIONAL_B_SPLINE_SURFACE(((1.00059040895223,0.822187541868208,1.00401468696662),
(1.00036527718144,0.889990093671545,1.00248382673394),(1.00016469515015,
0.950399042257912,1.00111990082512),(1.00025604273995,0.922888044286054,
1.00174104990633)))
REPRESENTATION_ITEM('')
SURFACE()
);
#3357=(
BOUNDED_SURFACE()
B_SPLINE_SURFACE(3,2,((#424526,#424527,#424528),(#424529,#424530,#424531),
(#424532,#424533,#424534),(#424535,#424536,#424537)),.UNSPECIFIED.,.F.,
 .F.,.F.)
B_SPLINE_SURFACE_WITH_KNOTS((4,4),(3,3),(-5.22358356749156E-6,5.74594192424276E-5),
(-0.00127120052070892,1.),.UNSPECIFIED.)
GEOMETRIC_REPRESENTATION_ITEM()
RATIONAL_B_SPLINE_SURFACE(((1.00054449313182,0.785835073638731,1.),(1.00047707767481,
0.812351526358835,1.),(1.00044031788592,0.826810216506248,1.),(1.00044777653324,
0.823876514387235,1.)))
REPRESENTATION_ITEM('')
SURFACE()
);
#3358=(
BOUNDED_SURFACE()
B_SPLINE_SURFACE(3,2,((#424539,#424540,#424541),(#424542,#424543,#424544),
(#424545,#424546,#424547),(#424548,#424549,#424550)),.UNSPECIFIED.,.F.,
 .F.,.F.)
B_SPLINE_SURFACE_WITH_KNOTS((4,4),(3,3),(-1.62630325872826E-19,4.8874751296988E-5),
(-0.000215805215067234,1.),.UNSPECIFIED.)
GEOMETRIC_REPRESENTATION_ITEM()
RATIONAL_B_SPLINE_SURFACE(((1.00008915600321,0.793434085499832,1.),(1.00008930224974,
0.793095246303371,1.),(1.00008944684596,0.792760230720652,1.),(1.00008958984375,
0.792428918540681,1.)))
REPRESENTATION_ITEM('')
SURFACE()
);
#3359=(
BOUNDED_SURFACE()
B_SPLINE_SURFACE(3,2,((#424552,#424553,#424554),(#424555,#424556,#424557),
(#424558,#424559,#424560),(#424561,#424562,#424563),(#424564,#424565,#424566),
(#424567,#424568,#424569)),.UNSPECIFIED.,.F.,.F.,.F.)
B_SPLINE_SURFACE_WITH_KNOTS((4,2,4),(3,3),(6.09863722023096E-20,7.62675010863196E-5,
0.000152535002172639),(0.,1.02152348203075),.UNSPECIFIED.)
GEOMETRIC_REPRESENTATION_ITEM()
RATIONAL_B_SPLINE_SURFACE(((1.,0.789033595401234,1.00908146323695),(1.,
0.857071781054814,1.00615262590431),(1.,0.922087264710743,1.00335390671593),
(1.,0.922394466502349,1.00334068261145),(1.,0.857224384599061,1.00614605678502),
(1.,0.789033595401633,1.00908146323693)))
REPRESENTATION_ITEM('')
SURFACE()
);
#3360=(
BOUNDED_SURFACE()
B_SPLINE_SURFACE(3,2,((#424571,#424572,#424573),(#424574,#424575,#424576),
(#424577,#424578,#424579),(#424580,#424581,#424582)),.UNSPECIFIED.,.F.,
 .F.,.F.)
B_SPLINE_SURFACE_WITH_KNOTS((4,4),(3,3),(3.25260651745651E-19,4.88747512969883E-5),
(-0.000215489856881676,1.),.UNSPECIFIED.)
GEOMETRIC_REPRESENTATION_ITEM()
RATIONAL_B_SPLINE_SURFACE(((1.00008945889707,0.792428983985777,1.),(1.00008931610828,
0.792760296061325,1.),(1.00008917172341,0.793095311538386,1.),(1.00008902569064,
0.793434150628026,1.)))
REPRESENTATION_ITEM('')
SURFACE()
);
#3361=(
BOUNDED_SURFACE()
B_SPLINE_SURFACE(3,2,((#424584,#424585,#424586),(#424587,#424588,#424589),
(#424590,#424591,#424592),(#424593,#424594,#424595)),.UNSPECIFIED.,.F.,
 .F.,.F.)
B_SPLINE_SURFACE_WITH_KNOTS((4,4),(3,3),(-5.21974905013085E-6,5.74172395514399E-5),
(-0.00139822857782877,1.00051312364113),.UNSPECIFIED.)
GEOMETRIC_REPRESENTATION_ITEM()
RATIONAL_B_SPLINE_SURFACE(((1.0004925694726,0.823768952243877,1.00018060397866),
(1.0004844821573,0.826662424388176,1.00017763870898),(1.00052427784039,
0.812424361909237,1.00019223006939),(1.00059912365874,0.785646094632581,
1.00021967280251)))
REPRESENTATION_ITEM('')
SURFACE()
);
#3362=(
BOUNDED_SURFACE()
B_SPLINE_SURFACE(3,2,((#424599,#424600,#424601),(#424602,#424603,#424604),
(#424605,#424606,#424607),(#424608,#424609,#424610)),.UNSPECIFIED.,.F.,
 .F.,.F.)
B_SPLINE_SURFACE_WITH_KNOTS((4,4),(3,3),(3.22980774337781E-5,9.63764854872251E-5),
(-0.00154325936250836,1.01095292447547),.UNSPECIFIED.)
GEOMETRIC_REPRESENTATION_ITEM()
RATIONAL_B_SPLINE_SURFACE(((1.0002353098328,0.922925743796259,1.00168574728331),
(1.00015136166114,0.950422439594272,1.0010843469906),(1.00033574337372,
0.890029368954089,1.00240524789548),(1.00054260094178,0.822274473168546,
1.00388716464859)))
REPRESENTATION_ITEM('')
SURFACE()
);
#3363=(
BOUNDED_SURFACE()
B_SPLINE_SURFACE(3,2,((#424710,#424711,#424712),(#424713,#424714,#424715),
(#424716,#424717,#424718),(#424719,#424720,#424721)),.UNSPECIFIED.,.F.,
 .F.,.F.)
B_SPLINE_SURFACE_WITH_KNOTS((4,4),(3,3),(0.,0.000101260117256738),(0.,1.),
 .UNSPECIFIED.)
GEOMETRIC_REPRESENTATION_ITEM()
RATIONAL_B_SPLINE_SURFACE(((1.,0.796615278835171,1.),(1.,0.795896038055945,
1.),(1.,0.795193354661335,1.),(1.,0.794506193185544,1.)))
REPRESENTATION_ITEM('')
SURFACE()
);
#3364=(
BOUNDED_SURFACE()
B_SPLINE_SURFACE(3,2,((#424759,#424760,#424761),(#424762,#424763,#424764),
(#424765,#424766,#424767),(#424768,#424769,#424770),(#424771,#424772,#424773),
(#424774,#424775,#424776)),.UNSPECIFIED.,.F.,.F.,.F.)
B_SPLINE_SURFACE_WITH_KNOTS((4,2,4),(3,3),(-3.11708124589583E-19,1.66936432462293E-5,
3.33872864924589E-5),(0.,1.),.UNSPECIFIED.)
GEOMETRIC_REPRESENTATION_ITEM()
RATIONAL_B_SPLINE_SURFACE(((1.,0.796615278835172,1.),(1.,0.862310524418136,
1.),(1.,0.923774472010518,1.),(1.,0.923983993203427,1.),(1.,0.862574873720949,
1.),(1.,0.796615278835185,1.)))
REPRESENTATION_ITEM('')
SURFACE()
);
#3365=(
BOUNDED_SURFACE()
B_SPLINE_SURFACE(3,2,((#424813,#424814,#424815),(#424816,#424817,#424818),
(#424819,#424820,#424821),(#424822,#424823,#424824)),.UNSPECIFIED.,.F.,
 .F.,.F.)
B_SPLINE_SURFACE_WITH_KNOTS((4,4),(3,3),(0.,0.000101244905251112),(0.,1.),
 .UNSPECIFIED.)
GEOMETRIC_REPRESENTATION_ITEM()
RATIONAL_B_SPLINE_SURFACE(((1.,0.796615278835172,1.),(1.,0.795896146109796,
1.),(1.,0.795193565796497,1.),(1.,0.794506502889904,1.)))
REPRESENTATION_ITEM('')
SURFACE()
);
#3366=(
BOUNDED_SURFACE()
B_SPLINE_SURFACE(3,2,((#424860,#424861,#424862),(#424863,#424864,#424865),
(#424866,#424867,#424868),(#424869,#424870,#424871)),.UNSPECIFIED.,.F.,
 .F.,.F.)
B_SPLINE_SURFACE_WITH_KNOTS((4,4),(3,3),(2.85968127239939E-5,9.24681548475822E-5),
(-0.00167900678647274,1.01130827127832),.UNSPECIFIED.)
GEOMETRIC_REPRESENTATION_ITEM()
RATIONAL_B_SPLINE_SURFACE(((1.00059040895214,0.82218754186827,1.0040146869666),
(1.00036527718138,0.889990093671564,1.00248382673393),(1.00016469515012,
0.950399042257935,1.00111990082512),(1.00025604273991,0.922888044286078,
1.00174104990633)))
REPRESENTATION_ITEM('')
SURFACE()
);
#3367=(
BOUNDED_SURFACE()
B_SPLINE_SURFACE(3,2,((#424875,#424876,#424877),(#424878,#424879,#424880),
(#424881,#424882,#424883),(#424884,#424885,#424886)),.UNSPECIFIED.,.F.,
 .F.,.F.)
B_SPLINE_SURFACE_WITH_KNOTS((4,4),(3,3),(-5.22358356749317E-6,5.74594192424277E-5),
(-0.0012712005206476,1.),.UNSPECIFIED.)
GEOMETRIC_REPRESENTATION_ITEM()
RATIONAL_B_SPLINE_SURFACE(((1.00054449313179,0.785835073638738,1.),(1.00047707767478,
0.812351526358837,1.),(1.0004403178859,0.826810216506266,1.),(1.00044777653322,
0.823876514387239,1.)))
REPRESENTATION_ITEM('')
SURFACE()
);
#3368=(
BOUNDED_SURFACE()
B_SPLINE_SURFACE(3,2,((#424888,#424889,#424890),(#424891,#424892,#424893),
(#424894,#424895,#424896),(#424897,#424898,#424899)),.UNSPECIFIED.,.F.,
 .F.,.F.)
B_SPLINE_SURFACE_WITH_KNOTS((4,4),(3,3),(-2.71050543121376E-19,4.8874751296988E-5),
(-0.000215805215662181,1.),.UNSPECIFIED.)
GEOMETRIC_REPRESENTATION_ITEM()
RATIONAL_B_SPLINE_SURFACE(((1.00008915600345,0.793434085499707,1.),(1.00008930224999,
0.793095246303258,1.),(1.00008944684621,0.792760230720517,1.),(1.000089589844,
0.792428918540555,1.)))
REPRESENTATION_ITEM('')
SURFACE()
);
#3369=(
BOUNDED_SURFACE()
B_SPLINE_SURFACE(3,2,((#424901,#424902,#424903),(#424904,#424905,#424906),
(#424907,#424908,#424909),(#424910,#424911,#424912),(#424913,#424914,#424915),
(#424916,#424917,#424918)),.UNSPECIFIED.,.F.,.F.,.F.)
B_SPLINE_SURFACE_WITH_KNOTS((4,2,4),(3,3),(3.32036915323686E-19,7.62675010863199E-5,
0.000152535002172639),(0.,1.02152348203075),.UNSPECIFIED.)
GEOMETRIC_REPRESENTATION_ITEM()
RATIONAL_B_SPLINE_SURFACE(((1.,0.789033595401233,1.00908146323695),(1.,
0.857071781054844,1.00615262590431),(1.,0.922087264710704,1.00335390671593),
(1.,0.922394466502388,1.00334068261145),(1.,0.857224384599028,1.00614605678503),
(1.,0.789033595401637,1.00908146323693)))
REPRESENTATION_ITEM('')
SURFACE()
);
#3370=(
BOUNDED_SURFACE()
B_SPLINE_SURFACE(3,2,((#424920,#424921,#424922),(#424923,#424924,#424925),
(#424926,#424927,#424928),(#424929,#424930,#424931)),.UNSPECIFIED.,.F.,
 .F.,.F.)
B_SPLINE_SURFACE_WITH_KNOTS((4,4),(3,3),(2.43945488809238E-19,4.88747512969883E-5),
(-0.000215489857039072,1.),.UNSPECIFIED.)
GEOMETRIC_REPRESENTATION_ITEM()
RATIONAL_B_SPLINE_SURFACE(((1.00008945889713,0.792428983985745,1.),(1.00008931610835,
0.792760296061297,1.),(1.00008917172347,0.793095311538356,1.),(1.0000890256907,
0.793434150627995,1.)))
REPRESENTATION_ITEM('')
SURFACE()
);
#3371=(
BOUNDED_SURFACE()
B_SPLINE_SURFACE(3,2,((#424933,#424934,#424935),(#424936,#424937,#424938),
(#424939,#424940,#424941),(#424942,#424943,#424944)),.UNSPECIFIED.,.F.,
 .F.,.F.)
B_SPLINE_SURFACE_WITH_KNOTS((4,4),(3,3),(-5.21974905012875E-6,5.74172395514397E-5),
(-0.00139822857739768,1.00051312364068),.UNSPECIFIED.)
GEOMETRIC_REPRESENTATION_ITEM()
RATIONAL_B_SPLINE_SURFACE(((1.00049256947245,0.82376895224404,1.0001806039785),
(1.00048448215715,0.826662424388324,1.00017763870882),(1.00052427784022,
0.812424361909407,1.00019223006921),(1.00059912365856,0.785646094632773,
1.00021967280231)))
REPRESENTATION_ITEM('')
SURFACE()
);
#3372=(
BOUNDED_SURFACE()
B_SPLINE_SURFACE(3,2,((#424948,#424949,#424950),(#424951,#424952,#424953),
(#424954,#424955,#424956),(#424957,#424958,#424959)),.UNSPECIFIED.,.F.,
 .F.,.F.)
B_SPLINE_SURFACE_WITH_KNOTS((4,4),(3,3),(3.22980774337779E-5,9.63764854872251E-5),
(-0.0015432593636694,1.01095292447539),.UNSPECIFIED.)
GEOMETRIC_REPRESENTATION_ITEM()
RATIONAL_B_SPLINE_SURFACE(((1.00023530983298,0.922925743796173,1.0016857472833),
(1.00015136166125,0.950422439594226,1.00108434699059),(1.00033574337397,
0.890029368953967,1.00240524789547),(1.00054260094219,0.822274473168352,
1.00388716464857)))
REPRESENTATION_ITEM('')
SURFACE()
);
#3373=(
BOUNDED_SURFACE()
B_SPLINE_SURFACE(3,2,((#425059,#425060,#425061),(#425062,#425063,#425064),
(#425065,#425066,#425067),(#425068,#425069,#425070)),.UNSPECIFIED.,.F.,
 .F.,.F.)
B_SPLINE_SURFACE_WITH_KNOTS((4,4),(3,3),(0.,0.000101260117256738),(0.,1.),
 .UNSPECIFIED.)
GEOMETRIC_REPRESENTATION_ITEM()
RATIONAL_B_SPLINE_SURFACE(((1.,0.796615278835169,1.),(1.,0.795896038055937,
1.),(1.,0.795193354661346,1.),(1.,0.794506193185544,1.)))
REPRESENTATION_ITEM('')
SURFACE()
);
#3374=(
BOUNDED_SURFACE()
B_SPLINE_SURFACE(3,2,((#425108,#425109,#425110),(#425111,#425112,#425113),
(#425114,#425115,#425116),(#425117,#425118,#425119),(#425120,#425121,#425122),
(#425123,#425124,#425125)),.UNSPECIFIED.,.F.,.F.,.F.)
B_SPLINE_SURFACE_WITH_KNOTS((4,2,4),(3,3),(7.45388993583784E-20,1.66936432462296E-5,
3.3387286492459E-5),(0.,1.),.UNSPECIFIED.)
GEOMETRIC_REPRESENTATION_ITEM()
RATIONAL_B_SPLINE_SURFACE(((1.,0.796615278835178,1.),(1.,0.862310524418132,
1.),(1.,0.923774472010522,1.),(1.,0.923983993203424,1.),(1.,0.862574873720963,
1.),(1.,0.796615278835185,1.)))
REPRESENTATION_ITEM('')
SURFACE()
);
#3375=(
BOUNDED_SURFACE()
B_SPLINE_SURFACE(3,2,((#425162,#425163,#425164),(#425165,#425166,#425167),
(#425168,#425169,#425170),(#425171,#425172,#425173)),.UNSPECIFIED.,.F.,
 .F.,.F.)
B_SPLINE_SURFACE_WITH_KNOTS((4,4),(3,3),(0.,0.000101244905251112),(0.,1.),
 .UNSPECIFIED.)
GEOMETRIC_REPRESENTATION_ITEM()
RATIONAL_B_SPLINE_SURFACE(((1.,0.796615278835173,1.),(1.,0.79589614610979,
1.),(1.,0.7951935657965,1.),(1.,0.794506502889901,1.)))
REPRESENTATION_ITEM('')
SURFACE()
);
#3376=(
BOUNDED_SURFACE()
B_SPLINE_SURFACE(3,2,((#425209,#425210,#425211),(#425212,#425213,#425214),
(#425215,#425216,#425217),(#425218,#425219,#425220)),.UNSPECIFIED.,.F.,
 .F.,.F.)
B_SPLINE_SURFACE_WITH_KNOTS((4,4),(3,3),(2.85968127239939E-5,9.24681548475816E-5),
(-0.00167900678789399,1.01130827127835),.UNSPECIFIED.)
GEOMETRIC_REPRESENTATION_ITEM()
RATIONAL_B_SPLINE_SURFACE(((1.00059040895264,0.822187541868006,1.00401468696661),
(1.00036527718169,0.889990093671416,1.00248382673394),(1.00016469515026,
0.950399042257849,1.00111990082512),(1.00025604274013,0.922888044285966,
1.00174104990633)))
REPRESENTATION_ITEM('')
SURFACE()
);
#3377=(
BOUNDED_SURFACE()
B_SPLINE_SURFACE(3,2,((#425224,#425225,#425226),(#425227,#425228,#425229),
(#425230,#425231,#425232),(#425233,#425234,#425235)),.UNSPECIFIED.,.F.,
 .F.,.F.)
B_SPLINE_SURFACE_WITH_KNOTS((4,4),(3,3),(-5.22358356749295E-6,5.74594192424276E-5),
(-0.00127120052076198,1.),.UNSPECIFIED.)
GEOMETRIC_REPRESENTATION_ITEM()
RATIONAL_B_SPLINE_SURFACE(((1.00054449313184,0.785835073638721,1.),(1.00047707767483,
0.812351526358804,1.),(1.00044031788594,0.826810216506243,1.),(1.00044777653326,
0.823876514387219,1.)))
REPRESENTATION_ITEM('')
SURFACE()
);
#3378=(
BOUNDED_SURFACE()
B_SPLINE_SURFACE(3,2,((#425237,#425238,#425239),(#425240,#425241,#425242),
(#425243,#425244,#425245),(#425246,#425247,#425248)),.UNSPECIFIED.,.F.,
 .F.,.F.)
B_SPLINE_SURFACE_WITH_KNOTS((4,4),(3,3),(-4.60785923306339E-19,4.88747512969881E-5),
(-0.000215805215153769,1.),.UNSPECIFIED.)
GEOMETRIC_REPRESENTATION_ITEM()
RATIONAL_B_SPLINE_SURFACE(((1.00008915600324,0.793434085499811,1.),(1.00008930224978,
0.793095246303347,1.),(1.000089446846,0.792760230720631,1.),(1.00008958984379,
0.792428918540661,1.)))
REPRESENTATION_ITEM('')
SURFACE()
);
#3379=(
BOUNDED_SURFACE()
B_SPLINE_SURFACE(3,2,((#425250,#425251,#425252),(#425253,#425254,#425255),
(#425256,#425257,#425258),(#425259,#425260,#425261),(#425262,#425263,#425264),
(#425265,#425266,#425267)),.UNSPECIFIED.,.F.,.F.,.F.)
B_SPLINE_SURFACE_WITH_KNOTS((4,2,4),(3,3),(2.84603070277445E-19,7.62675010863198E-5,
0.000152535002172639),(0.,1.02152348203076),.UNSPECIFIED.)
GEOMETRIC_REPRESENTATION_ITEM()
RATIONAL_B_SPLINE_SURFACE(((1.,0.789033595401233,1.00908146323695),(1.,
0.857071781054873,1.00615262590431),(1.,0.922087264710668,1.00335390671593),
(1.,0.92239446650242,1.00334068261145),(1.,0.85722438459901,1.00614605678503),
(1.,0.789033595401633,1.00908146323693)))
REPRESENTATION_ITEM('')
SURFACE()
);
#3380=(
BOUNDED_SURFACE()
B_SPLINE_SURFACE(3,2,((#425269,#425270,#425271),(#425272,#425273,#425274),
(#425275,#425276,#425277),(#425278,#425279,#425280)),.UNSPECIFIED.,.F.,
 .F.,.F.)
B_SPLINE_SURFACE_WITH_KNOTS((4,4),(3,3),(5.42101086242752E-20,4.88747512969882E-5),
(-0.000215489857037421,1.),.UNSPECIFIED.)
GEOMETRIC_REPRESENTATION_ITEM()
RATIONAL_B_SPLINE_SURFACE(((1.00008945889713,0.792428983985742,1.),(1.00008931610835,
0.792760296061293,1.),(1.00008917172347,0.793095311538357,1.),(1.0000890256907,
0.793434150627994,1.)))
REPRESENTATION_ITEM('')
SURFACE()
);
#3381=(
BOUNDED_SURFACE()
B_SPLINE_SURFACE(3,2,((#425282,#425283,#425284),(#425285,#425286,#425287),
(#425288,#425289,#425290),(#425291,#425292,#425293)),.UNSPECIFIED.,.F.,
 .F.,.F.)
B_SPLINE_SURFACE_WITH_KNOTS((4,4),(3,3),(-5.21974905013094E-6,5.74172395514394E-5),
(-0.00139822857773127,1.00051312364078),.UNSPECIFIED.)
GEOMETRIC_REPRESENTATION_ITEM()
RATIONAL_B_SPLINE_SURFACE(((1.00049256947256,0.823768952243962,1.00018060397853),
(1.00048448215727,0.826662424388245,1.00017763870886),(1.00052427784035,
0.812424361909327,1.00019223006925),(1.0005991236587,0.785646094632678,
1.00021967280236)))
REPRESENTATION_ITEM('')
SURFACE()
);
#3382=(
BOUNDED_SURFACE()
B_SPLINE_SURFACE(3,2,((#425297,#425298,#425299),(#425300,#425301,#425302),
(#425303,#425304,#425305),(#425306,#425307,#425308)),.UNSPECIFIED.,.F.,
 .F.,.F.)
B_SPLINE_SURFACE_WITH_KNOTS((4,4),(3,3),(3.22980774337777E-5,9.63764854872245E-5),
(-0.00154325936314989,1.01095292447545),.UNSPECIFIED.)
GEOMETRIC_REPRESENTATION_ITEM()
RATIONAL_B_SPLINE_SURFACE(((1.0002353098329,0.922925743796211,1.00168574728331),
(1.0001513616612,0.950422439594239,1.0010843469906),(1.00033574337386,0.890029368954025,
1.00240524789548),(1.00054260094201,0.822274473168434,1.00388716464859)))
REPRESENTATION_ITEM('')
SURFACE()
);
#3383=(
BOUNDED_SURFACE()
B_SPLINE_SURFACE(3,2,((#425408,#425409,#425410),(#425411,#425412,#425413),
(#425414,#425415,#425416),(#425417,#425418,#425419)),.UNSPECIFIED.,.F.,
 .F.,.F.)
B_SPLINE_SURFACE_WITH_KNOTS((4,4),(3,3),(0.,0.000101260117256736),(0.,1.),
 .UNSPECIFIED.)
GEOMETRIC_REPRESENTATION_ITEM()
RATIONAL_B_SPLINE_SURFACE(((1.,0.796615278835174,1.),(1.,0.795896038055937,
1.),(1.,0.795193354661362,1.),(1.,0.794506193185534,1.)))
REPRESENTATION_ITEM('')
SURFACE()
);
#3384=(
BOUNDED_SURFACE()
B_SPLINE_SURFACE(3,2,((#425457,#425458,#425459),(#425460,#425461,#425462),
(#425463,#425464,#425465),(#425466,#425467,#425468),(#425469,#425470,#425471),
(#425472,#425473,#425474)),.UNSPECIFIED.,.F.,.F.,.F.)
B_SPLINE_SURFACE_WITH_KNOTS((4,2,4),(3,3),(1.01643953670516E-19,1.66936432462293E-5,
3.33872864924585E-5),(0.,1.),.UNSPECIFIED.)
GEOMETRIC_REPRESENTATION_ITEM()
RATIONAL_B_SPLINE_SURFACE(((1.,0.796615278835177,1.),(1.,0.862310524418127,
1.),(1.,0.923774472010516,1.),(1.,0.923983993203427,1.),(1.,0.862574873720946,
1.),(1.,0.79661527883519,1.)))
REPRESENTATION_ITEM('')
SURFACE()
);
#3385=(
BOUNDED_SURFACE()
B_SPLINE_SURFACE(3,2,((#425511,#425512,#425513),(#425514,#425515,#425516),
(#425517,#425518,#425519),(#425520,#425521,#425522)),.UNSPECIFIED.,.F.,
 .F.,.F.)
B_SPLINE_SURFACE_WITH_KNOTS((4,4),(3,3),(-2.16840434497101E-19,0.000101244905251112),
(0.,1.),.UNSPECIFIED.)
GEOMETRIC_REPRESENTATION_ITEM()
RATIONAL_B_SPLINE_SURFACE(((1.,0.79661527883517,1.),(1.,0.795896146109793,
1.),(1.,0.795193565796498,1.),(1.,0.794506502889901,1.)))
REPRESENTATION_ITEM('')
SURFACE()
);
#3386=(
BOUNDED_SURFACE()
B_SPLINE_SURFACE(3,2,((#425558,#425559,#425560),(#425561,#425562,#425563),
(#425564,#425565,#425566),(#425567,#425568,#425569)),.UNSPECIFIED.,.F.,
 .F.,.F.)
B_SPLINE_SURFACE_WITH_KNOTS((4,4),(3,3),(2.85968127239939E-5,9.24681548475815E-5),
(-0.00167900678784821,1.01130827127814),.UNSPECIFIED.)
GEOMETRIC_REPRESENTATION_ITEM()
RATIONAL_B_SPLINE_SURFACE(((1.00059040895263,0.822187541868056,1.00401468696653),
(1.00036527718168,0.889990093671432,1.00248382673389),(1.00016469515026,
0.950399042257876,1.0011199008251),(1.00025604274012,0.922888044285984,
1.0017410499063)))
REPRESENTATION_ITEM('')
SURFACE()
);
#3387=(
BOUNDED_SURFACE()
B_SPLINE_SURFACE(3,2,((#425573,#425574,#425575),(#425576,#425577,#425578),
(#425579,#425580,#425581),(#425582,#425583,#425584)),.UNSPECIFIED.,.F.,
 .F.,.F.)
B_SPLINE_SURFACE_WITH_KNOTS((4,4),(3,3),(-5.22358356749054E-6,5.74594192424279E-5),
(-0.00127120052066195,1.),.UNSPECIFIED.)
GEOMETRIC_REPRESENTATION_ITEM()
RATIONAL_B_SPLINE_SURFACE(((1.0005444931318,0.785835073638738,1.),(1.00047707767479,
0.812351526358848,1.),(1.0004403178859,0.826810216506254,1.),(1.00044777653322,
0.823876514387246,1.)))
REPRESENTATION_ITEM('')
SURFACE()
);
#3388=(
BOUNDED_SURFACE()
B_SPLINE_SURFACE(3,2,((#425586,#425587,#425588),(#425589,#425590,#425591),
(#425592,#425593,#425594),(#425595,#425596,#425597)),.UNSPECIFIED.,.F.,
 .F.,.F.)
B_SPLINE_SURFACE_WITH_KNOTS((4,4),(3,3),(0.,4.88747512969883E-5),(-0.000215805215016013,
1.),.UNSPECIFIED.)
GEOMETRIC_REPRESENTATION_ITEM()
RATIONAL_B_SPLINE_SURFACE(((1.00008915600319,0.793434085499842,1.),(1.00008930224972,
0.793095246303386,1.),(1.00008944684594,0.79276023072066,1.),(1.00008958984373,
0.792428918540691,1.)))
REPRESENTATION_ITEM('')
SURFACE()
);
#3389=(
BOUNDED_SURFACE()
B_SPLINE_SURFACE(3,2,((#425599,#425600,#425601),(#425602,#425603,#425604),
(#425605,#425606,#425607),(#425608,#425609,#425610),(#425611,#425612,#425613),
(#425614,#425615,#425616)),.UNSPECIFIED.,.F.,.F.,.F.)
B_SPLINE_SURFACE_WITH_KNOTS((4,2,4),(3,3),(6.7762635780344E-21,7.62675010863196E-5,
0.000152535002172639),(0.,1.02152348203057),.UNSPECIFIED.)
GEOMETRIC_REPRESENTATION_ITEM()
RATIONAL_B_SPLINE_SURFACE(((1.,0.789033595401272,1.00908146323687),(1.,
0.857071781054866,1.00615262590425),(1.,0.92208726471072,1.0033539067159),
(1.,0.922394466502399,1.00334068261142),(1.,0.857224384599056,1.00614605678497),
(1.,0.789033595401673,1.00908146323685)))
REPRESENTATION_ITEM('')
SURFACE()
);
#3390=(
BOUNDED_SURFACE()
B_SPLINE_SURFACE(3,2,((#425618,#425619,#425620),(#425621,#425622,#425623),
(#425624,#425625,#425626),(#425627,#425628,#425629)),.UNSPECIFIED.,.F.,
 .F.,.F.)
B_SPLINE_SURFACE_WITH_KNOTS((4,4),(3,3),(3.25260651745651E-19,4.88747512969882E-5),
(-0.000215489857000909,1.),.UNSPECIFIED.)
GEOMETRIC_REPRESENTATION_ITEM()
RATIONAL_B_SPLINE_SURFACE(((1.00008945889712,0.792428983985751,1.),(1.00008931610833,
0.792760296061304,1.),(1.00008917172346,0.793095311538362,1.),(1.00008902569068,
0.793434150628,1.)))
REPRESENTATION_ITEM('')
SURFACE()
);
#3391=(
BOUNDED_SURFACE()
B_SPLINE_SURFACE(3,2,((#425631,#425632,#425633),(#425634,#425635,#425636),
(#425637,#425638,#425639),(#425640,#425641,#425642)),.UNSPECIFIED.,.F.,
 .F.,.F.)
B_SPLINE_SURFACE_WITH_KNOTS((4,4),(3,3),(-5.21974905013092E-6,5.74172395514399E-5),
(-0.00139822857802174,1.00051312364098),.UNSPECIFIED.)
GEOMETRIC_REPRESENTATION_ITEM()
RATIONAL_B_SPLINE_SURFACE(((1.00049256947267,0.823768952243878,1.0001806039786),
(1.00048448215737,0.826662424388162,1.00017763870893),(1.00052427784046,
0.812424361909232,1.00019223006933),(1.00059912365883,0.785646094632575,
1.00021967280244)))
REPRESENTATION_ITEM('')
SURFACE()
);
#3392=(
BOUNDED_SURFACE()
B_SPLINE_SURFACE(3,2,((#425646,#425647,#425648),(#425649,#425650,#425651),
(#425652,#425653,#425654),(#425655,#425656,#425657)),.UNSPECIFIED.,.F.,
 .F.,.F.)
B_SPLINE_SURFACE_WITH_KNOTS((4,4),(3,3),(3.22980774337782E-5,9.63764854872257E-5),
(-0.00154325936384171,1.01095292447529),.UNSPECIFIED.)
GEOMETRIC_REPRESENTATION_ITEM()
RATIONAL_B_SPLINE_SURFACE(((1.00023530983301,0.922925743796167,1.00168574728329),
(1.00015136166127,0.950422439594215,1.00108434699058),(1.00033574337401,
0.890029368953956,1.00240524789544),(1.00054260094225,0.822274473168344,
1.00388716464853)))
REPRESENTATION_ITEM('')
SURFACE()
);
#3393=(
BOUNDED_SURFACE()
B_SPLINE_SURFACE(3,2,((#425757,#425758,#425759),(#425760,#425761,#425762),
(#425763,#425764,#425765),(#425766,#425767,#425768)),.UNSPECIFIED.,.F.,
 .F.,.F.)
B_SPLINE_SURFACE_WITH_KNOTS((4,4),(3,3),(-4.33680868994202E-19,0.000101260117256738),
(0.,1.),.UNSPECIFIED.)
GEOMETRIC_REPRESENTATION_ITEM()
RATIONAL_B_SPLINE_SURFACE(((1.,0.796615278835172,1.),(1.,0.795896038055941,
1.),(1.,0.795193354661349,1.),(1.,0.794506193185546,1.)))
REPRESENTATION_ITEM('')
SURFACE()
);
#3394=(
BOUNDED_SURFACE()
B_SPLINE_SURFACE(3,2,((#425806,#425807,#425808),(#425809,#425810,#425811),
(#425812,#425813,#425814),(#425815,#425816,#425817),(#425818,#425819,#425820),
(#425821,#425822,#425823)),.UNSPECIFIED.,.F.,.F.,.F.)
B_SPLINE_SURFACE_WITH_KNOTS((4,2,4),(3,3),(8.97854924089558E-20,1.66936432462293E-5,
3.33872864924585E-5),(0.,1.),.UNSPECIFIED.)
GEOMETRIC_REPRESENTATION_ITEM()
RATIONAL_B_SPLINE_SURFACE(((1.,0.796615278835178,1.),(1.,0.862310524418125,
1.),(1.,0.923774472010522,1.),(1.,0.923983993203424,1.),(1.,0.862574873720937,
1.),(1.,0.796615278835187,1.)))
REPRESENTATION_ITEM('')
SURFACE()
);
#3395=(
BOUNDED_SURFACE()
B_SPLINE_SURFACE(3,2,((#425860,#425861,#425862),(#425863,#425864,#425865),
(#425866,#425867,#425868),(#425869,#425870,#425871)),.UNSPECIFIED.,.F.,
 .F.,.F.)
B_SPLINE_SURFACE_WITH_KNOTS((4,4),(3,3),(-2.16840434497101E-19,0.000101244905251112),
(0.,1.),.UNSPECIFIED.)
GEOMETRIC_REPRESENTATION_ITEM()
RATIONAL_B_SPLINE_SURFACE(((1.,0.796615278835171,1.),(1.,0.795896146109793,
1.),(1.,0.795193565796497,1.),(1.,0.794506502889901,1.)))
REPRESENTATION_ITEM('')
SURFACE()
);
#3396=(
BOUNDED_SURFACE()
B_SPLINE_SURFACE(3,2,((#425907,#425908,#425909),(#425910,#425911,#425912),
(#425913,#425914,#425915),(#425916,#425917,#425918)),.UNSPECIFIED.,.F.,
 .F.,.F.)
B_SPLINE_SURFACE_WITH_KNOTS((4,4),(3,3),(2.85968127239939E-5,9.24681548475819E-5),
(-0.00167900678704925,1.01130827127826),.UNSPECIFIED.)
GEOMETRIC_REPRESENTATION_ITEM()
RATIONAL_B_SPLINE_SURFACE(((1.00059040895235,0.822187541868178,1.00401468696658),
(1.00036527718151,0.889990093671508,1.00248382673392),(1.00016469515018,
0.950399042257906,1.00111990082511),(1.00025604274,0.922888044286039,1.00174104990632)))
REPRESENTATION_ITEM('')
SURFACE()
);
#3397=(
BOUNDED_SURFACE()
B_SPLINE_SURFACE(3,2,((#425922,#425923,#425924),(#425925,#425926,#425927),
(#425928,#425929,#425930),(#425931,#425932,#425933)),.UNSPECIFIED.,.F.,
 .F.,.F.)
B_SPLINE_SURFACE_WITH_KNOTS((4,4),(3,3),(-5.22358356749291E-6,5.74594192424279E-5),
(-0.00127120052059996,1.),.UNSPECIFIED.)
GEOMETRIC_REPRESENTATION_ITEM()
RATIONAL_B_SPLINE_SURFACE(((1.00054449313177,0.785835073638752,1.),(1.00047707767476,
0.812351526358855,1.),(1.00044031788588,0.826810216506264,1.),(1.0004477765332,
0.823876514387255,1.)))
REPRESENTATION_ITEM('')
SURFACE()
);
#3398=(
BOUNDED_SURFACE()
B_SPLINE_SURFACE(3,2,((#425935,#425936,#425937),(#425938,#425939,#425940),
(#425941,#425942,#425943),(#425944,#425945,#425946)),.UNSPECIFIED.,.F.,
 .F.,.F.)
B_SPLINE_SURFACE_WITH_KNOTS((4,4),(3,3),(-2.43945488809238E-19,4.88747512969882E-5),
(-0.000215805215941335,1.),.UNSPECIFIED.)
GEOMETRIC_REPRESENTATION_ITEM()
RATIONAL_B_SPLINE_SURFACE(((1.00008915600357,0.793434085499649,1.),(1.0000893022501,
0.793095246303205,1.),(1.00008944684632,0.792760230720455,1.),(1.00008958984411,
0.792428918540498,1.)))
REPRESENTATION_ITEM('')
SURFACE()
);
#3399=(
BOUNDED_SURFACE()
B_SPLINE_SURFACE(3,2,((#425948,#425949,#425950),(#425951,#425952,#425953),
(#425954,#425955,#425956),(#425957,#425958,#425959),(#425960,#425961,#425962),
(#425963,#425964,#425965)),.UNSPECIFIED.,.F.,.F.,.F.)
B_SPLINE_SURFACE_WITH_KNOTS((4,2,4),(3,3),(1.21972744404619E-19,7.62675010863195E-5,
0.000152535002172639),(0.,1.0215234820305),.UNSPECIFIED.)
GEOMETRIC_REPRESENTATION_ITEM()
RATIONAL_B_SPLINE_SURFACE(((1.,0.789033595401289,1.00908146323684),(1.,
0.85707178105485,1.00615262590423),(1.,0.922087264710762,1.00335390671589),
(1.,0.922394466502367,1.00334068261141),(1.,0.857224384599093,1.00614605678495),
(1.,0.789033595401684,1.00908146323682)))
REPRESENTATION_ITEM('')
SURFACE()
);
#3400=(
BOUNDED_SURFACE()
B_SPLINE_SURFACE(3,2,((#425967,#425968,#425969),(#425970,#425971,#425972),
(#425973,#425974,#425975),(#425976,#425977,#425978)),.UNSPECIFIED.,.F.,
 .F.,.F.)
B_SPLINE_SURFACE_WITH_KNOTS((4,4),(3,3),(3.52365706057789E-19,4.88747512969883E-5),
(-0.000215489857896713,1.),.UNSPECIFIED.)
GEOMETRIC_REPRESENTATION_ITEM()
RATIONAL_B_SPLINE_SURFACE(((1.00008945889749,0.792428983985566,1.),(1.0000893161087,
0.792760296061123,1.),(1.00008917172383,0.793095311538183,1.),(1.00008902569106,
0.793434150627818,1.)))
REPRESENTATION_ITEM('')
SURFACE()
);
#3401=(
BOUNDED_SURFACE()
B_SPLINE_SURFACE(3,2,((#425980,#425981,#425982),(#425983,#425984,#425985),
(#425986,#425987,#425988),(#425989,#425990,#425991)),.UNSPECIFIED.,.F.,
 .F.,.F.)
B_SPLINE_SURFACE_WITH_KNOTS((4,4),(3,3),(-5.21974905012879E-6,5.7417239551441E-5),
(-0.00139822857767231,1.00051312364052),.UNSPECIFIED.)
GEOMETRIC_REPRESENTATION_ITEM()
RATIONAL_B_SPLINE_SURFACE(((1.00049256947254,0.823768952244014,1.00018060397844),
(1.00048448215725,0.826662424388313,1.00017763870877),(1.00052427784033,
0.812424361909371,1.00019223006916),(1.00059912365868,0.785646094632754,
1.00021967280225)))
REPRESENTATION_ITEM('')
SURFACE()
);
#3402=(
BOUNDED_SURFACE()
B_SPLINE_SURFACE(3,2,((#425995,#425996,#425997),(#425998,#425999,#426000),
(#426001,#426002,#426003),(#426004,#426005,#426006)),.UNSPECIFIED.,.F.,
 .F.,.F.)
B_SPLINE_SURFACE_WITH_KNOTS((4,4),(3,3),(3.22980774337777E-5,9.63764854872253E-5),
(-0.00154325936391161,1.01095292447535),.UNSPECIFIED.)
GEOMETRIC_REPRESENTATION_ITEM()
RATIONAL_B_SPLINE_SURFACE(((1.00023530983302,0.922925743796154,1.0016857472833),
(1.00015136166127,0.950422439594211,1.00108434699059),(1.00033574337402,
0.890029368953947,1.00240524789546),(1.00054260094228,0.822274473168314,
1.00388716464855)))
REPRESENTATION_ITEM('')
SURFACE()
);
#3403=(
BOUNDED_SURFACE()
B_SPLINE_SURFACE(3,2,((#426106,#426107,#426108),(#426109,#426110,#426111),
(#426112,#426113,#426114),(#426115,#426116,#426117)),.UNSPECIFIED.,.F.,
 .F.,.F.)
B_SPLINE_SURFACE_WITH_KNOTS((4,4),(3,3),(-6.50521303491303E-19,0.000101260117256738),
(0.,1.),.UNSPECIFIED.)
GEOMETRIC_REPRESENTATION_ITEM()
RATIONAL_B_SPLINE_SURFACE(((1.,0.79661527883517,1.),(1.,0.795896038055941,
1.),(1.,0.795193354661336,1.),(1.,0.794506193185542,1.)))
REPRESENTATION_ITEM('')
SURFACE()
);
#3404=(
BOUNDED_SURFACE()
B_SPLINE_SURFACE(3,2,((#426155,#426156,#426157),(#426158,#426159,#426160),
(#426161,#426162,#426163),(#426164,#426165,#426166),(#426167,#426168,#426169),
(#426170,#426171,#426172)),.UNSPECIFIED.,.F.,.F.,.F.)
B_SPLINE_SURFACE_WITH_KNOTS((4,2,4),(3,3),(3.3881317890172E-20,1.66936432462296E-5,
3.33872864924592E-5),(0.,1.),.UNSPECIFIED.)
GEOMETRIC_REPRESENTATION_ITEM()
RATIONAL_B_SPLINE_SURFACE(((1.,0.796615278835172,1.),(1.,0.862310524418128,
1.),(1.,0.923774472010521,1.),(1.,0.923983993203426,1.),(1.,0.862574873720939,
1.),(1.,0.796615278835185,1.)))
REPRESENTATION_ITEM('')
SURFACE()
);
#3405=(
BOUNDED_SURFACE()
B_SPLINE_SURFACE(3,2,((#426209,#426210,#426211),(#426212,#426213,#426214),
(#426215,#426216,#426217),(#426218,#426219,#426220)),.UNSPECIFIED.,.F.,
 .F.,.F.)
B_SPLINE_SURFACE_WITH_KNOTS((4,4),(3,3),(-2.16840434497101E-19,0.000101244905251112),
(0.,1.),.UNSPECIFIED.)
GEOMETRIC_REPRESENTATION_ITEM()
RATIONAL_B_SPLINE_SURFACE(((1.,0.796615278835169,1.),(1.,0.795896146109794,
1.),(1.,0.795193565796498,1.),(1.,0.7945065028899,1.)))
REPRESENTATION_ITEM('')
SURFACE()
);
#3406=(
BOUNDED_SURFACE()
B_SPLINE_SURFACE(3,2,((#426256,#426257,#426258),(#426259,#426260,#426261),
(#426262,#426263,#426264),(#426265,#426266,#426267)),.UNSPECIFIED.,.F.,
 .F.,.F.)
B_SPLINE_SURFACE_WITH_KNOTS((4,4),(3,3),(2.85968127239939E-5,9.24681548475814E-5),
(-0.00167900678705586,1.01130827127826),.UNSPECIFIED.)
GEOMETRIC_REPRESENTATION_ITEM()
RATIONAL_B_SPLINE_SURFACE(((1.00059040895235,0.82218754186818,1.00401468696658),
(1.00036527718151,0.889990093671503,1.00248382673392),(1.00016469515018,
0.95039904225791,1.00111990082511),(1.00025604274,0.922888044286036,1.00174104990632)))
REPRESENTATION_ITEM('')
SURFACE()
);
#3407=(
BOUNDED_SURFACE()
B_SPLINE_SURFACE(3,2,((#426271,#426272,#426273),(#426274,#426275,#426276),
(#426277,#426278,#426279),(#426280,#426281,#426282)),.UNSPECIFIED.,.F.,
 .F.,.F.)
B_SPLINE_SURFACE_WITH_KNOTS((4,4),(3,3),(-5.22358356749331E-6,5.74594192424277E-5),
(-0.00127120052057017,1.),.UNSPECIFIED.)
GEOMETRIC_REPRESENTATION_ITEM()
RATIONAL_B_SPLINE_SURFACE(((1.00054449313176,0.785835073638767,1.),(1.00047707767475,
0.812351526358833,1.),(1.00044031788587,0.826810216506293,1.),(1.00044777653319,
0.82387651438725,1.)))
REPRESENTATION_ITEM('')
SURFACE()
);
#3408=(
BOUNDED_SURFACE()
B_SPLINE_SURFACE(3,2,((#426284,#426285,#426286),(#426287,#426288,#426289),
(#426290,#426291,#426292),(#426293,#426294,#426295)),.UNSPECIFIED.,.F.,
 .F.,.F.)
B_SPLINE_SURFACE_WITH_KNOTS((4,4),(3,3),(5.42101086242752E-20,4.88747512969877E-5),
(-0.000215805215420418,1.),.UNSPECIFIED.)
GEOMETRIC_REPRESENTATION_ITEM()
RATIONAL_B_SPLINE_SURFACE(((1.00008915600335,0.793434085499756,1.),(1.00008930224989,
0.793095246303299,1.),(1.00008944684611,0.79276023072057,1.),(1.0000895898439,
0.792428918540607,1.)))
REPRESENTATION_ITEM('')
SURFACE()
);
#3409=(
BOUNDED_SURFACE()
B_SPLINE_SURFACE(3,2,((#426297,#426298,#426299),(#426300,#426301,#426302),
(#426303,#426304,#426305),(#426306,#426307,#426308),(#426309,#426310,#426311),
(#426312,#426313,#426314)),.UNSPECIFIED.,.F.,.F.,.F.)
B_SPLINE_SURFACE_WITH_KNOTS((4,2,4),(3,3),(3.52365706057789E-19,7.626750108632E-5,
0.00015253500217264),(0.,1.02152348203043),.UNSPECIFIED.)
GEOMETRIC_REPRESENTATION_ITEM()
RATIONAL_B_SPLINE_SURFACE(((1.,0.7890335954013,1.00908146323681),(1.,0.857071781054874,
1.00615262590421),(1.,0.922087264710739,1.00335390671588),(1.,0.9223944665024,
1.0033406826114),(1.,0.857224384599083,1.00614605678493),(1.,0.789033595401701,
1.00908146323679)))
REPRESENTATION_ITEM('')
SURFACE()
);
#3410=(
BOUNDED_SURFACE()
B_SPLINE_SURFACE(3,2,((#426316,#426317,#426318),(#426319,#426320,#426321),
(#426322,#426323,#426324),(#426325,#426326,#426327)),.UNSPECIFIED.,.F.,
 .F.,.F.)
B_SPLINE_SURFACE_WITH_KNOTS((4,4),(3,3),(2.16840434497101E-19,4.88747512969884E-5),
(-0.000215489857091422,1.),.UNSPECIFIED.)
GEOMETRIC_REPRESENTATION_ITEM()
RATIONAL_B_SPLINE_SURFACE(((1.00008945889715,0.792428983985732,1.),(1.00008931610837,
0.792760296061273,1.),(1.0000891717235,0.793095311538358,1.),(1.00008902569072,
0.793434150627982,1.)))
REPRESENTATION_ITEM('')
SURFACE()
);
#3411=(
BOUNDED_SURFACE()
B_SPLINE_SURFACE(3,2,((#426329,#426330,#426331),(#426332,#426333,#426334),
(#426335,#426336,#426337),(#426338,#426339,#426340)),.UNSPECIFIED.,.F.,
 .F.,.F.)
B_SPLINE_SURFACE_WITH_KNOTS((4,4),(3,3),(-5.21974905013092E-6,5.74172395514398E-5),
(-0.00139822857739479,1.00051312364055),.UNSPECIFIED.)
GEOMETRIC_REPRESENTATION_ITEM()
RATIONAL_B_SPLINE_SURFACE(((1.00049256947244,0.823768952244062,1.00018060397845),
(1.00048448215715,0.826662424388343,1.00017763870878),(1.00052427784022,
0.812424361909432,1.00019223006917),(1.00059912365856,0.785646094632801,
1.00021967280226)))
REPRESENTATION_ITEM('')
SURFACE()
);
#3412=(
BOUNDED_SURFACE()
B_SPLINE_SURFACE(3,2,((#426344,#426345,#426346),(#426347,#426348,#426349),
(#426350,#426351,#426352),(#426353,#426354,#426355)),.UNSPECIFIED.,.F.,
 .F.,.F.)
B_SPLINE_SURFACE_WITH_KNOTS((4,4),(3,3),(3.22980774337781E-5,9.63764854872261E-5),
(-0.00154325936385449,1.01095292447525),.UNSPECIFIED.)
GEOMETRIC_REPRESENTATION_ITEM()
RATIONAL_B_SPLINE_SURFACE(((1.00023530983301,0.922925743796168,1.00168574728328),
(1.00015136166127,0.950422439594217,1.00108434699058),(1.00033574337401,
0.890029368953963,1.00240524789544),(1.00054260094226,0.822274473168349,
1.00388716464852)))
REPRESENTATION_ITEM('')
SURFACE()
);
#3413=(
BOUNDED_SURFACE()
B_SPLINE_SURFACE(3,2,((#426455,#426456,#426457),(#426458,#426459,#426460),
(#426461,#426462,#426463),(#426464,#426465,#426466)),.UNSPECIFIED.,.F.,
 .F.,.F.)
B_SPLINE_SURFACE_WITH_KNOTS((4,4),(3,3),(0.,0.000101260117256737),(0.,1.),
 .UNSPECIFIED.)
GEOMETRIC_REPRESENTATION_ITEM()
RATIONAL_B_SPLINE_SURFACE(((1.,0.79661527883517,1.),(1.,0.795896038055948,
1.),(1.,0.795193354661331,1.),(1.,0.794506193185546,1.)))
REPRESENTATION_ITEM('')
SURFACE()
);
#3414=(
BOUNDED_SURFACE()
B_SPLINE_SURFACE(3,2,((#426504,#426505,#426506),(#426507,#426508,#426509),
(#426510,#426511,#426512),(#426513,#426514,#426515),(#426516,#426517,#426518),
(#426519,#426520,#426521)),.UNSPECIFIED.,.F.,.F.,.F.)
B_SPLINE_SURFACE_WITH_KNOTS((4,2,4),(3,3),(7.45388993583784E-20,1.66936432462299E-5,
3.33872864924597E-5),(0.,1.),.UNSPECIFIED.)
GEOMETRIC_REPRESENTATION_ITEM()
RATIONAL_B_SPLINE_SURFACE(((1.,0.796615278835171,1.),(1.,0.862310524418139,
1.),(1.,0.92377447201052,1.),(1.,0.923983993203424,1.),(1.,0.862574873720947,
1.),(1.,0.79661527883518,1.)))
REPRESENTATION_ITEM('')
SURFACE()
);
#3415=(
BOUNDED_SURFACE()
B_SPLINE_SURFACE(3,2,((#426558,#426559,#426560),(#426561,#426562,#426563),
(#426564,#426565,#426566),(#426567,#426568,#426569)),.UNSPECIFIED.,.F.,
 .F.,.F.)
B_SPLINE_SURFACE_WITH_KNOTS((4,4),(3,3),(0.,0.000101244905251112),(0.,1.),
 .UNSPECIFIED.)
GEOMETRIC_REPRESENTATION_ITEM()
RATIONAL_B_SPLINE_SURFACE(((1.,0.796615278835171,1.),(1.,0.795896146109789,
1.),(1.,0.795193565796504,1.),(1.,0.794506502889899,1.)))
REPRESENTATION_ITEM('')
SURFACE()
);
#3416=(
BOUNDED_SURFACE()
B_SPLINE_SURFACE(3,2,((#426605,#426606,#426607),(#426608,#426609,#426610),
(#426611,#426612,#426613),(#426614,#426615,#426616)),.UNSPECIFIED.,.F.,
 .F.,.F.)
B_SPLINE_SURFACE_WITH_KNOTS((4,4),(3,3),(2.85968127239938E-5,9.24681548475817E-5),
(-0.00167900678654135,1.01130827127837),.UNSPECIFIED.)
GEOMETRIC_REPRESENTATION_ITEM()
RATIONAL_B_SPLINE_SURFACE(((1.00059040895217,0.822187541868246,1.00401468696662),
(1.0003652771814,0.889990093671551,1.00248382673394),(1.00016469515013,
0.950399042257927,1.00111990082512),(1.00025604273992,0.922888044286068,
1.00174104990633)))
REPRESENTATION_ITEM('')
SURFACE()
);
#3417=(
BOUNDED_SURFACE()
B_SPLINE_SURFACE(3,2,((#426620,#426621,#426622),(#426623,#426624,#426625),
(#426626,#426627,#426628),(#426629,#426630,#426631)),.UNSPECIFIED.,.F.,
 .F.,.F.)
B_SPLINE_SURFACE_WITH_KNOTS((4,4),(3,3),(-5.22358356749322E-6,5.74594192424276E-5),
(-0.00127120052062939,1.),.UNSPECIFIED.)
GEOMETRIC_REPRESENTATION_ITEM()
RATIONAL_B_SPLINE_SURFACE(((1.00054449313178,0.785835073638751,1.),(1.00047707767478,
0.812351526358826,1.),(1.00044031788589,0.826810216506275,1.),(1.00044777653321,
0.823876514387242,1.)))
REPRESENTATION_ITEM('')
SURFACE()
);
#3418=(
BOUNDED_SURFACE()
B_SPLINE_SURFACE(3,2,((#426633,#426634,#426635),(#426636,#426637,#426638),
(#426639,#426640,#426641),(#426642,#426643,#426644)),.UNSPECIFIED.,.F.,
 .F.,.F.)
B_SPLINE_SURFACE_WITH_KNOTS((4,4),(3,3),(-8.13151629364128E-20,4.8874751296988E-5),
(-0.000215805215034299,1.),.UNSPECIFIED.)
GEOMETRIC_REPRESENTATION_ITEM()
RATIONAL_B_SPLINE_SURFACE(((1.0000891560032,0.793434085499832,1.),(1.00008930224973,
0.793095246303387,1.),(1.00008944684595,0.79276023072065,1.),(1.00008958984374,
0.792428918540687,1.)))
REPRESENTATION_ITEM('')
SURFACE()
);
#3419=(
BOUNDED_SURFACE()
B_SPLINE_SURFACE(3,2,((#426646,#426647,#426648),(#426649,#426650,#426651),
(#426652,#426653,#426654),(#426655,#426656,#426657),(#426658,#426659,#426660),
(#426661,#426662,#426663)),.UNSPECIFIED.,.F.,.F.,.F.)
B_SPLINE_SURFACE_WITH_KNOTS((4,2,4),(3,3),(-2.03287907341032E-20,7.62675010863199E-5,
0.00015253500217264),(0.,1.02152348203051),.UNSPECIFIED.)
GEOMETRIC_REPRESENTATION_ITEM()
RATIONAL_B_SPLINE_SURFACE(((1.,0.789033595401288,1.00908146323684),(1.,
0.857071781054841,1.00615262590424),(1.,0.922087264710766,1.00335390671589),
(1.,0.922394466502363,1.00334068261141),(1.,0.857224384599088,1.00614605678495),
(1.,0.789033595401688,1.00908146323683)))
REPRESENTATION_ITEM('')
SURFACE()
);
#3420=(
BOUNDED_SURFACE()
B_SPLINE_SURFACE(3,2,((#426665,#426666,#426667),(#426668,#426669,#426670),
(#426671,#426672,#426673),(#426674,#426675,#426676)),.UNSPECIFIED.,.F.,
 .F.,.F.)
B_SPLINE_SURFACE_WITH_KNOTS((4,4),(3,3),(1.0842021724855E-19,4.88747512969883E-5),
(-0.000215489856815771,1.),.UNSPECIFIED.)
GEOMETRIC_REPRESENTATION_ITEM()
RATIONAL_B_SPLINE_SURFACE(((1.00008945889704,0.79242898398579,1.),(1.00008931610826,
0.792760296061347,1.),(1.00008917172338,0.793095311538396,1.),(1.00008902569061,
0.793434150628043,1.)))
REPRESENTATION_ITEM('')
SURFACE()
);
#3421=(
BOUNDED_SURFACE()
B_SPLINE_SURFACE(3,2,((#426678,#426679,#426680),(#426681,#426682,#426683),
(#426684,#426685,#426686),(#426687,#426688,#426689)),.UNSPECIFIED.,.F.,
 .F.,.F.)
B_SPLINE_SURFACE_WITH_KNOTS((4,4),(3,3),(-5.21974905012873E-6,5.74172395514394E-5),
(-0.00139822857773652,1.00051312364074),.UNSPECIFIED.)
GEOMETRIC_REPRESENTATION_ITEM()
RATIONAL_B_SPLINE_SURFACE(((1.00049256947257,0.82376895224397,1.00018060397852),
(1.00048448215727,0.826662424388236,1.00017763870885),(1.00052427784035,
0.812424361909349,1.00019223006924),(1.00059912365871,0.785646094632682,
1.00021967280234)))
REPRESENTATION_ITEM('')
SURFACE()
);
#3422=(
BOUNDED_SURFACE()
B_SPLINE_SURFACE(3,2,((#426693,#426694,#426695),(#426696,#426697,#426698),
(#426699,#426700,#426701),(#426702,#426703,#426704)),.UNSPECIFIED.,.F.,
 .F.,.F.)
B_SPLINE_SURFACE_WITH_KNOTS((4,4),(3,3),(3.22980774337783E-5,9.63764854872258E-5),
(-0.00154325936400768,1.01095292447557),.UNSPECIFIED.)
GEOMETRIC_REPRESENTATION_ITEM()
RATIONAL_B_SPLINE_SURFACE(((1.00023530983303,0.92292574379613,1.00168574728333),
(1.00015136166128,0.950422439594196,1.00108434699061),(1.00033574337404,
0.89002936895391,1.00240524789551),(1.00054260094231,0.82227447316826,1.00388716464863)))
REPRESENTATION_ITEM('')
SURFACE()
);
#3423=(
BOUNDED_SURFACE()
B_SPLINE_SURFACE(3,2,((#426804,#426805,#426806),(#426807,#426808,#426809),
(#426810,#426811,#426812),(#426813,#426814,#426815)),.UNSPECIFIED.,.F.,
 .F.,.F.)
B_SPLINE_SURFACE_WITH_KNOTS((4,4),(3,3),(0.,0.000101260117256738),(0.,1.),
 .UNSPECIFIED.)
GEOMETRIC_REPRESENTATION_ITEM()
RATIONAL_B_SPLINE_SURFACE(((1.,0.796615278835172,1.),(1.,0.795896038055938,
1.),(1.,0.795193354661348,1.),(1.,0.794506193185546,1.)))
REPRESENTATION_ITEM('')
SURFACE()
);
#3424=(
BOUNDED_SURFACE()
B_SPLINE_SURFACE(3,2,((#426853,#426854,#426855),(#426856,#426857,#426858),
(#426859,#426860,#426861),(#426862,#426863,#426864),(#426865,#426866,#426867),
(#426868,#426869,#426870)),.UNSPECIFIED.,.F.,.F.,.F.)
B_SPLINE_SURFACE_WITH_KNOTS((4,2,4),(3,3),(-1.94817577868489E-19,1.66936432462298E-5,
3.33872864924599E-5),(0.,1.),.UNSPECIFIED.)
GEOMETRIC_REPRESENTATION_ITEM()
RATIONAL_B_SPLINE_SURFACE(((1.,0.796615278835165,1.),(1.,0.862310524418136,
1.),(1.,0.923774472010517,1.),(1.,0.923983993203428,1.),(1.,0.862574873720953,
1.),(1.,0.796615278835182,1.)))
REPRESENTATION_ITEM('')
SURFACE()
);
#3425=(
BOUNDED_SURFACE()
B_SPLINE_SURFACE(3,2,((#426907,#426908,#426909),(#426910,#426911,#426912),
(#426913,#426914,#426915),(#426916,#426917,#426918)),.UNSPECIFIED.,.F.,
 .F.,.F.)
B_SPLINE_SURFACE_WITH_KNOTS((4,4),(3,3),(2.16840434497101E-19,0.000101244905251112),
(0.,1.),.UNSPECIFIED.)
GEOMETRIC_REPRESENTATION_ITEM()
RATIONAL_B_SPLINE_SURFACE(((1.,0.796615278835168,1.),(1.,0.795896146109795,
1.),(1.,0.795193565796498,1.),(1.,0.794506502889901,1.)))
REPRESENTATION_ITEM('')
SURFACE()
);
#3426=(
BOUNDED_SURFACE()
B_SPLINE_SURFACE(3,2,((#426954,#426955,#426956),(#426957,#426958,#426959),
(#426960,#426961,#426962),(#426963,#426964,#426965)),.UNSPECIFIED.,.F.,
 .F.,.F.)
B_SPLINE_SURFACE_WITH_KNOTS((4,4),(3,3),(2.85968127239939E-5,9.24681548475819E-5),
(-0.001679006786515,1.01130827127844),.UNSPECIFIED.)
GEOMETRIC_REPRESENTATION_ITEM()
RATIONAL_B_SPLINE_SURFACE(((1.00059040895216,0.822187541868239,1.00401468696665),
(1.00036527718139,0.889990093671552,1.00248382673396),(1.00016469515013,
0.950399042257921,1.00111990082513),(1.00025604273992,0.922888044286066,
1.00174104990634)))
REPRESENTATION_ITEM('')
SURFACE()
);
#3427=(
BOUNDED_SURFACE()
B_SPLINE_SURFACE(3,2,((#426969,#426970,#426971),(#426972,#426973,#426974),
(#426975,#426976,#426977),(#426978,#426979,#426980)),.UNSPECIFIED.,.F.,
 .F.,.F.)
B_SPLINE_SURFACE_WITH_KNOTS((4,4),(3,3),(-5.22358356749305E-6,5.74594192424275E-5),
(-0.0012712005206506,1.),.UNSPECIFIED.)
GEOMETRIC_REPRESENTATION_ITEM()
RATIONAL_B_SPLINE_SURFACE(((1.00054449313179,0.78583507363875,1.),(1.00047707767478,
0.812351526358819,1.),(1.0004403178859,0.826810216506276,1.),(1.00044777653322,
0.823876514387236,1.)))
REPRESENTATION_ITEM('')
SURFACE()
);
#3428=(
BOUNDED_SURFACE()
B_SPLINE_SURFACE(3,2,((#426982,#426983,#426984),(#426985,#426986,#426987),
(#426988,#426989,#426990),(#426991,#426992,#426993)),.UNSPECIFIED.,.F.,
 .F.,.F.)
B_SPLINE_SURFACE_WITH_KNOTS((4,4),(3,3),(2.71050543121376E-20,4.8874751296988E-5),
(-0.000215805214801446,1.),.UNSPECIFIED.)
GEOMETRIC_REPRESENTATION_ITEM()
RATIONAL_B_SPLINE_SURFACE(((1.0000891560031,0.793434085499885,1.),(1.00008930224963,
0.793095246303421,1.),(1.00008944684585,0.792760230720706,1.),(1.00008958984364,
0.792428918540732,1.)))
REPRESENTATION_ITEM('')
SURFACE()
);
#3429=(
BOUNDED_SURFACE()
B_SPLINE_SURFACE(3,2,((#426995,#426996,#426997),(#426998,#426999,#427000),
(#427001,#427002,#427003),(#427004,#427005,#427006),(#427007,#427008,#427009),
(#427010,#427011,#427012)),.UNSPECIFIED.,.F.,.F.,.F.)
B_SPLINE_SURFACE_WITH_KNOTS((4,2,4),(3,3),(1.55854062294791E-19,7.62675010863199E-5,
0.00015253500217264),(0.,1.02152348203048),.UNSPECIFIED.)
GEOMETRIC_REPRESENTATION_ITEM()
RATIONAL_B_SPLINE_SURFACE(((1.,0.789033595401297,1.00908146323683),(1.,
0.857071781054868,1.00615262590423),(1.,0.92208726471074,1.00335390671589),
(1.,0.922394466502395,1.0033406826114),(1.,0.857224384599078,1.00614605678494),
(1.,0.789033595401691,1.00908146323681)))
REPRESENTATION_ITEM('')
SURFACE()
);
#3430=(
BOUNDED_SURFACE()
B_SPLINE_SURFACE(3,2,((#427014,#427015,#427016),(#427017,#427018,#427019),
(#427020,#427021,#427022),(#427023,#427024,#427025)),.UNSPECIFIED.,.F.,
 .F.,.F.)
B_SPLINE_SURFACE_WITH_KNOTS((4,4),(3,3),(2.43945488809238E-19,4.88747512969886E-5),
(-0.000215489856871912,1.),.UNSPECIFIED.)
GEOMETRIC_REPRESENTATION_ITEM()
RATIONAL_B_SPLINE_SURFACE(((1.00008945889706,0.792428983985778,1.),(1.00008931610828,
0.792760296061328,1.),(1.00008917172341,0.793095311538385,1.),(1.00008902569063,
0.793434150628033,1.)))
REPRESENTATION_ITEM('')
SURFACE()
);
#3431=(
BOUNDED_SURFACE()
B_SPLINE_SURFACE(3,2,((#427027,#427028,#427029),(#427030,#427031,#427032),
(#427033,#427034,#427035),(#427036,#427037,#427038)),.UNSPECIFIED.,.F.,
 .F.,.F.)
B_SPLINE_SURFACE_WITH_KNOTS((4,4),(3,3),(-5.21974905013083E-6,5.74172395514396E-5),
(-0.00139822857794668,1.00051312364089),.UNSPECIFIED.)
GEOMETRIC_REPRESENTATION_ITEM()
RATIONAL_B_SPLINE_SURFACE(((1.00049256947264,0.823768952243904,1.00018060397857),
(1.00048448215734,0.826662424388192,1.0001776387089),(1.00052427784043,
0.812424361909265,1.00019223006929),(1.0005991236588,0.785646094632611,
1.0002196728024)))
REPRESENTATION_ITEM('')
SURFACE()
);
#3432=(
BOUNDED_SURFACE()
B_SPLINE_SURFACE(3,2,((#427042,#427043,#427044),(#427045,#427046,#427047),
(#427048,#427049,#427050),(#427051,#427052,#427053)),.UNSPECIFIED.,.F.,
 .F.,.F.)
B_SPLINE_SURFACE_WITH_KNOTS((4,4),(3,3),(3.22980774337778E-5,9.63764854872253E-5),
(-0.00154325936338914,1.01095292447536),.UNSPECIFIED.)
GEOMETRIC_REPRESENTATION_ITEM()
RATIONAL_B_SPLINE_SURFACE(((1.00023530983294,0.922925743796197,1.0016857472833),
(1.00015136166122,0.950422439594232,1.00108434699059),(1.00033574337391,
0.890029368954006,1.00240524789546),(1.00054260094209,0.822274473168407,
1.00388716464856)))
REPRESENTATION_ITEM('')
SURFACE()
);
#3433=(
BOUNDED_SURFACE()
B_SPLINE_SURFACE(3,2,((#427153,#427154,#427155),(#427156,#427157,#427158),
(#427159,#427160,#427161),(#427162,#427163,#427164)),.UNSPECIFIED.,.F.,
 .F.,.F.)
B_SPLINE_SURFACE_WITH_KNOTS((4,4),(3,3),(0.,0.000101260117256736),(0.,1.),
 .UNSPECIFIED.)
GEOMETRIC_REPRESENTATION_ITEM()
RATIONAL_B_SPLINE_SURFACE(((1.,0.796615278835173,1.),(1.,0.79589603805594,
1.),(1.,0.795193354661355,1.),(1.,0.794506193185536,1.)))
REPRESENTATION_ITEM('')
SURFACE()
);
#3434=(
BOUNDED_SURFACE()
B_SPLINE_SURFACE(3,2,((#427202,#427203,#427204),(#427205,#427206,#427207),
(#427208,#427209,#427210),(#427211,#427212,#427213),(#427214,#427215,#427216),
(#427217,#427218,#427219)),.UNSPECIFIED.,.F.,.F.,.F.)
B_SPLINE_SURFACE_WITH_KNOTS((4,2,4),(3,3),(-2.64274279543342E-19,1.66936432462293E-5,
3.33872864924589E-5),(0.,1.),.UNSPECIFIED.)
GEOMETRIC_REPRESENTATION_ITEM()
RATIONAL_B_SPLINE_SURFACE(((1.,0.79661527883517,1.),(1.,0.862310524418132,
1.),(1.,0.923774472010528,1.),(1.,0.923983993203422,1.),(1.,0.86257487372095,
1.),(1.,0.79661527883518,1.)))
REPRESENTATION_ITEM('')
SURFACE()
);
#3435=(
BOUNDED_SURFACE()
B_SPLINE_SURFACE(3,2,((#427256,#427257,#427258),(#427259,#427260,#427261),
(#427262,#427263,#427264),(#427265,#427266,#427267)),.UNSPECIFIED.,.F.,
 .F.,.F.)
B_SPLINE_SURFACE_WITH_KNOTS((4,4),(3,3),(0.,0.000101244905251112),(0.,1.),
 .UNSPECIFIED.)
GEOMETRIC_REPRESENTATION_ITEM()
RATIONAL_B_SPLINE_SURFACE(((1.,0.796615278835166,1.),(1.,0.795896146109796,
1.),(1.,0.795193565796497,1.),(1.,0.794506502889899,1.)))
REPRESENTATION_ITEM('')
SURFACE()
);
#3436=(
BOUNDED_SURFACE()
B_SPLINE_SURFACE(3,2,((#427303,#427304,#427305),(#427306,#427307,#427308),
(#427309,#427310,#427311),(#427312,#427313,#427314)),.UNSPECIFIED.,.F.,
 .F.,.F.)
B_SPLINE_SURFACE_WITH_KNOTS((4,4),(3,3),(2.85968127239939E-5,9.24681548475817E-5),
(-0.00167900678734404,1.01130827127821),.UNSPECIFIED.)
GEOMETRIC_REPRESENTATION_ITEM()
RATIONAL_B_SPLINE_SURFACE(((1.00059040895245,0.822187541868132,1.00401468696656),
(1.00036527718157,0.88999009367148,1.00248382673391),(1.00016469515021,
0.950399042257889,1.00111990082511),(1.00025604274005,0.922888044286016,
1.00174104990631)))
REPRESENTATION_ITEM('')
SURFACE()
);
#3437=(
BOUNDED_SURFACE()
B_SPLINE_SURFACE(3,2,((#427318,#427319,#427320),(#427321,#427322,#427323),
(#427324,#427325,#427326),(#427327,#427328,#427329)),.UNSPECIFIED.,.F.,
 .F.,.F.)
B_SPLINE_SURFACE_WITH_KNOTS((4,4),(3,3),(-5.22358356749204E-6,5.74594192424279E-5),
(-0.00127120052055143,1.),.UNSPECIFIED.)
GEOMETRIC_REPRESENTATION_ITEM()
RATIONAL_B_SPLINE_SURFACE(((1.00054449313175,0.785835073638762,1.),(1.00047707767475,
0.812351526358862,1.),(1.00044031788586,0.826810216506277,1.),(1.00044777653318,
0.823876514387263,1.)))
REPRESENTATION_ITEM('')
SURFACE()
);
#3438=(
BOUNDED_SURFACE()
B_SPLINE_SURFACE(3,2,((#427331,#427332,#427333),(#427334,#427335,#427336),
(#427337,#427338,#427339),(#427340,#427341,#427342)),.UNSPECIFIED.,.F.,
 .F.,.F.)
B_SPLINE_SURFACE_WITH_KNOTS((4,4),(3,3),(0.,4.88747512969878E-5),(-0.000215805215227164,
1.),.UNSPECIFIED.)
GEOMETRIC_REPRESENTATION_ITEM()
RATIONAL_B_SPLINE_SURFACE(((1.00008915600327,0.793434085499794,1.),(1.00008930224981,
0.793095246303354,1.),(1.00008944684603,0.792760230720619,1.),(1.00008958984382,
0.792428918540648,1.)))
REPRESENTATION_ITEM('')
SURFACE()
);
#3439=(
BOUNDED_SURFACE()
B_SPLINE_SURFACE(3,2,((#427344,#427345,#427346),(#427347,#427348,#427349),
(#427350,#427351,#427352),(#427353,#427354,#427355),(#427356,#427357,#427358),
(#427359,#427360,#427361)),.UNSPECIFIED.,.F.,.F.,.F.)
B_SPLINE_SURFACE_WITH_KNOTS((4,2,4),(3,3),(2.98155597433514E-19,7.62675010863198E-5,
0.000152535002172639),(0.,1.02152348203069),.UNSPECIFIED.)
GEOMETRIC_REPRESENTATION_ITEM()
RATIONAL_B_SPLINE_SURFACE(((1.,0.789033595401248,1.00908146323692),(1.,
0.857071781054857,1.00615262590429),(1.,0.922087264710701,1.00335390671592),
(1.,0.9223944665024,1.00334068261144),(1.,0.857224384599027,1.00614605678501),
(1.,0.789033595401649,1.0090814632369)))
REPRESENTATION_ITEM('')
SURFACE()
);
#3440=(
BOUNDED_SURFACE()
B_SPLINE_SURFACE(3,2,((#427363,#427364,#427365),(#427366,#427367,#427368),
(#427369,#427370,#427371),(#427372,#427373,#427374)),.UNSPECIFIED.,.F.,
 .F.,.F.)
B_SPLINE_SURFACE_WITH_KNOTS((4,4),(3,3),(6.50521303491303E-19,4.88747512969885E-5),
(-0.000215489857079631,1.),.UNSPECIFIED.)
GEOMETRIC_REPRESENTATION_ITEM()
RATIONAL_B_SPLINE_SURFACE(((1.00008945889715,0.792428983985734,1.),(1.00008931610837,
0.79276029606128,1.),(1.00008917172349,0.793095311538358,1.),(1.00008902569072,
0.793434150627986,1.)))
REPRESENTATION_ITEM('')
SURFACE()
);
#3441=(
BOUNDED_SURFACE()
B_SPLINE_SURFACE(3,2,((#427376,#427377,#427378),(#427379,#427380,#427381),
(#427382,#427383,#427384),(#427385,#427386,#427387)),.UNSPECIFIED.,.F.,
 .F.,.F.)
B_SPLINE_SURFACE_WITH_KNOTS((4,4),(3,3),(-5.21974905013096E-6,5.74172395514397E-5),
(-0.00139822857719932,1.00051312364059),.UNSPECIFIED.)
GEOMETRIC_REPRESENTATION_ITEM()
RATIONAL_B_SPLINE_SURFACE(((1.00049256947238,0.823768952244082,1.00018060397847),
(1.00048448215708,0.826662424388392,1.00017763870879),(1.00052427784015,
0.812424361909437,1.00019223006918),(1.00059912365847,0.78564609463284,
1.00021967280228)))
REPRESENTATION_ITEM('')
SURFACE()
);
#3442=(
BOUNDED_SURFACE()
B_SPLINE_SURFACE(3,2,((#427391,#427392,#427393),(#427394,#427395,#427396),
(#427397,#427398,#427399),(#427400,#427401,#427402)),.UNSPECIFIED.,.F.,
 .F.,.F.)
B_SPLINE_SURFACE_WITH_KNOTS((4,4),(3,3),(3.22980774337779E-5,9.63764854872255E-5),
(-0.00154325936518139,1.01095292447533),.UNSPECIFIED.)
GEOMETRIC_REPRESENTATION_ITEM()
RATIONAL_B_SPLINE_SURFACE(((1.00023530983321,0.922925743796062,1.00168574728329),
(1.0001513616614,0.95042243959415,1.00108434699059),(1.0003357433743,0.890029368953806,
1.00240524789545),(1.00054260094272,0.82227447316809,1.00388716464854)))
REPRESENTATION_ITEM('')
SURFACE()
);
#3443=(
BOUNDED_SURFACE()
B_SPLINE_SURFACE(3,2,((#427502,#427503,#427504),(#427505,#427506,#427507),
(#427508,#427509,#427510),(#427511,#427512,#427513)),.UNSPECIFIED.,.F.,
 .F.,.F.)
B_SPLINE_SURFACE_WITH_KNOTS((4,4),(3,3),(0.,0.000101260117256737),(0.,1.),
 .UNSPECIFIED.)
GEOMETRIC_REPRESENTATION_ITEM()
RATIONAL_B_SPLINE_SURFACE(((1.,0.79661527883517,1.),(1.,0.795896038055935,
1.),(1.,0.79519335466135,1.),(1.,0.794506193185543,1.)))
REPRESENTATION_ITEM('')
SURFACE()
);
#3444=(
BOUNDED_SURFACE()
B_SPLINE_SURFACE(3,2,((#427551,#427552,#427553),(#427554,#427555,#427556),
(#427557,#427558,#427559),(#427560,#427561,#427562),(#427563,#427564,#427565),
(#427566,#427567,#427568)),.UNSPECIFIED.,.F.,.F.,.F.)
B_SPLINE_SURFACE_WITH_KNOTS((4,2,4),(3,3),(-2.04981973235541E-19,1.66936432462293E-5,
3.33872864924587E-5),(0.,1.),.UNSPECIFIED.)
GEOMETRIC_REPRESENTATION_ITEM()
RATIONAL_B_SPLINE_SURFACE(((1.,0.796615278835175,1.),(1.,0.862310524418114,
1.),(1.,0.923774472010523,1.),(1.,0.923983993203425,1.),(1.,0.862574873720955,
1.),(1.,0.796615278835174,1.)))
REPRESENTATION_ITEM('')
SURFACE()
);
#3445=(
BOUNDED_SURFACE()
B_SPLINE_SURFACE(3,2,((#427605,#427606,#427607),(#427608,#427609,#427610),
(#427611,#427612,#427613),(#427614,#427615,#427616)),.UNSPECIFIED.,.F.,
 .F.,.F.)
B_SPLINE_SURFACE_WITH_KNOTS((4,4),(3,3),(0.,0.000101244905251112),(0.,1.),
 .UNSPECIFIED.)
GEOMETRIC_REPRESENTATION_ITEM()
RATIONAL_B_SPLINE_SURFACE(((1.,0.796615278835171,1.),(1.,0.795896146109795,
1.),(1.,0.795193565796493,1.),(1.,0.794506502889901,1.)))
REPRESENTATION_ITEM('')
SURFACE()
);
#3446=(
BOUNDED_SURFACE()
B_SPLINE_SURFACE(3,2,((#427652,#427653,#427654),(#427655,#427656,#427657),
(#427658,#427659,#427660),(#427661,#427662,#427663)),.UNSPECIFIED.,.F.,
 .F.,.F.)
B_SPLINE_SURFACE_WITH_KNOTS((4,4),(3,3),(2.85968127239939E-5,9.24681548475816E-5),
(-0.00167900678644083,1.01130827127813),.UNSPECIFIED.)
GEOMETRIC_REPRESENTATION_ITEM()
RATIONAL_B_SPLINE_SURFACE(((1.00059040895213,0.822187541868308,1.00401468696653),
(1.00036527718137,0.889990093671593,1.00248382673389),(1.00016469515012,
0.95039904225794,1.0011199008251),(1.00025604273991,0.922888044286096,1.0017410499063)))
REPRESENTATION_ITEM('')
SURFACE()
);
#3447=(
BOUNDED_SURFACE()
B_SPLINE_SURFACE(3,2,((#427667,#427668,#427669),(#427670,#427671,#427672),
(#427673,#427674,#427675),(#427676,#427677,#427678)),.UNSPECIFIED.,.F.,
 .F.,.F.)
B_SPLINE_SURFACE_WITH_KNOTS((4,4),(3,3),(-5.22358356749292E-6,5.74594192424277E-5),
(-0.00127120052058111,1.),.UNSPECIFIED.)
GEOMETRIC_REPRESENTATION_ITEM()
RATIONAL_B_SPLINE_SURFACE(((1.00054449313176,0.785835073638756,1.),(1.00047707767476,
0.812351526358861,1.),(1.00044031788587,0.826810216506268,1.),(1.00044777653319,
0.823876514387252,1.)))
REPRESENTATION_ITEM('')
SURFACE()
);
#3448=(
BOUNDED_SURFACE()
B_SPLINE_SURFACE(3,2,((#427680,#427681,#427682),(#427683,#427684,#427685),
(#427686,#427687,#427688),(#427689,#427690,#427691)),.UNSPECIFIED.,.F.,
 .F.,.F.)
B_SPLINE_SURFACE_WITH_KNOTS((4,4),(3,3),(-2.71050543121376E-20,4.88747512969881E-5),
(-0.0002158052151809,1.),.UNSPECIFIED.)
GEOMETRIC_REPRESENTATION_ITEM()
RATIONAL_B_SPLINE_SURFACE(((1.00008915600326,0.793434085499806,1.),(1.00008930224979,
0.793095246303342,1.),(1.00008944684601,0.792760230720625,1.),(1.0000895898438,
0.792428918540654,1.)))
REPRESENTATION_ITEM('')
SURFACE()
);
#3449=(
BOUNDED_SURFACE()
B_SPLINE_SURFACE(3,2,((#427693,#427694,#427695),(#427696,#427697,#427698),
(#427699,#427700,#427701),(#427702,#427703,#427704),(#427705,#427706,#427707),
(#427708,#427709,#427710)),.UNSPECIFIED.,.F.,.F.,.F.)
B_SPLINE_SURFACE_WITH_KNOTS((4,2,4),(3,3),(-9.48676900924816E-20,7.62675010863194E-5,
0.000152535002172639),(0.,1.02152348203078),.UNSPECIFIED.)
GEOMETRIC_REPRESENTATION_ITEM()
RATIONAL_B_SPLINE_SURFACE(((1.,0.789033595401232,1.00908146323696),(1.,
0.857071781054828,1.00615262590431),(1.,0.922087264710711,1.00335390671594),
(1.,0.922394466502375,1.00334068261145),(1.,0.857224384599031,1.00614605678503),
(1.,0.789033595401628,1.00908146323694)))
REPRESENTATION_ITEM('')
SURFACE()
);
#3450=(
BOUNDED_SURFACE()
B_SPLINE_SURFACE(3,2,((#427712,#427713,#427714),(#427715,#427716,#427717),
(#427718,#427719,#427720),(#427721,#427722,#427723)),.UNSPECIFIED.,.F.,
 .F.,.F.)
B_SPLINE_SURFACE_WITH_KNOTS((4,4),(3,3),(2.71050543121376E-19,4.88747512969886E-5),
(-0.000215489857605897,1.),.UNSPECIFIED.)
GEOMETRIC_REPRESENTATION_ITEM()
RATIONAL_B_SPLINE_SURFACE(((1.00008945889737,0.792428983985626,1.),(1.00008931610858,
0.792760296061186,1.),(1.00008917172371,0.79309531153825,1.),(1.00008902569093,
0.793434150627878,1.)))
REPRESENTATION_ITEM('')
SURFACE()
);
#3451=(
BOUNDED_SURFACE()
B_SPLINE_SURFACE(3,2,((#427725,#427726,#427727),(#427728,#427729,#427730),
(#427731,#427732,#427733),(#427734,#427735,#427736)),.UNSPECIFIED.,.F.,
 .F.,.F.)
B_SPLINE_SURFACE_WITH_KNOTS((4,4),(3,3),(-5.21974905013089E-6,5.74172395514395E-5),
(-0.00139822857804183,1.0005131236408),.UNSPECIFIED.)
GEOMETRIC_REPRESENTATION_ITEM()
RATIONAL_B_SPLINE_SURFACE(((1.00049256947267,0.823768952243908,1.00018060397854),
(1.00048448215738,0.826662424388174,1.00017763870887),(1.00052427784047,
0.812424361909285,1.00019223006926),(1.00059912365884,0.785646094632604,
1.00021967280237)))
REPRESENTATION_ITEM('')
SURFACE()
);
#3452=(
BOUNDED_SURFACE()
B_SPLINE_SURFACE(3,2,((#427740,#427741,#427742),(#427743,#427744,#427745),
(#427746,#427747,#427748),(#427749,#427750,#427751)),.UNSPECIFIED.,.F.,
 .F.,.F.)
B_SPLINE_SURFACE_WITH_KNOTS((4,4),(3,3),(3.22980774337779E-5,9.6376485487225E-5),
(-0.00154325936517141,1.01095292447531),.UNSPECIFIED.)
GEOMETRIC_REPRESENTATION_ITEM()
RATIONAL_B_SPLINE_SURFACE(((1.00023530983321,0.922925743796063,1.00168574728329),
(1.0001513616614,0.950422439594155,1.00108434699058),(1.0003357433743,0.890029368953809,
1.00240524789545),(1.00054260094272,0.822274473168098,1.00388716464854)))
REPRESENTATION_ITEM('')
SURFACE()
);
#3453=(
BOUNDED_SURFACE()
B_SPLINE_SURFACE(3,2,((#427851,#427852,#427853),(#427854,#427855,#427856),
(#427857,#427858,#427859),(#427860,#427861,#427862)),.UNSPECIFIED.,.F.,
 .F.,.F.)
B_SPLINE_SURFACE_WITH_KNOTS((4,4),(3,3),(2.16840434497101E-19,0.000101260117256738),
(0.,1.),.UNSPECIFIED.)
GEOMETRIC_REPRESENTATION_ITEM()
RATIONAL_B_SPLINE_SURFACE(((1.,0.796615278835173,1.),(1.,0.795896038055939,
1.),(1.,0.795193354661347,1.),(1.,0.794506193185548,1.)))
REPRESENTATION_ITEM('')
SURFACE()
);
#3454=(
BOUNDED_SURFACE()
B_SPLINE_SURFACE(3,2,((#427900,#427901,#427902),(#427903,#427904,#427905),
(#427906,#427907,#427908),(#427909,#427910,#427911),(#427912,#427913,#427914),
(#427915,#427916,#427917)),.UNSPECIFIED.,.F.,.F.,.F.)
B_SPLINE_SURFACE_WITH_KNOTS((4,2,4),(3,3),(-1.01643953670516E-19,1.66936432462293E-5,
3.33872864924587E-5),(0.,1.),.UNSPECIFIED.)
GEOMETRIC_REPRESENTATION_ITEM()
RATIONAL_B_SPLINE_SURFACE(((1.,0.796615278835177,1.),(1.,0.86231052441812,
1.),(1.,0.923774472010522,1.),(1.,0.923983993203425,1.),(1.,0.862574873720947,
1.),(1.,0.796615278835186,1.)))
REPRESENTATION_ITEM('')
SURFACE()
);
#3455=(
BOUNDED_SURFACE()
B_SPLINE_SURFACE(3,2,((#427954,#427955,#427956),(#427957,#427958,#427959),
(#427960,#427961,#427962),(#427963,#427964,#427965)),.UNSPECIFIED.,.F.,
 .F.,.F.)
B_SPLINE_SURFACE_WITH_KNOTS((4,4),(3,3),(0.,0.000101244905251112),(0.,1.),
 .UNSPECIFIED.)
GEOMETRIC_REPRESENTATION_ITEM()
RATIONAL_B_SPLINE_SURFACE(((1.,0.796615278835172,1.),(1.,0.795896146109793,
1.),(1.,0.795193565796498,1.),(1.,0.794506502889903,1.)))
REPRESENTATION_ITEM('')
SURFACE()
);
#3456=(
BOUNDED_SURFACE()
B_SPLINE_SURFACE(3,2,((#428001,#428002,#428003),(#428004,#428005,#428006),
(#428007,#428008,#428009),(#428010,#428011,#428012)),.UNSPECIFIED.,.F.,
 .F.,.F.)
B_SPLINE_SURFACE_WITH_KNOTS((4,4),(3,3),(2.85968127239939E-5,9.24681548475816E-5),
(-0.00167900679344736,1.0113082712782),.UNSPECIFIED.)
GEOMETRIC_REPRESENTATION_ITEM()
RATIONAL_B_SPLINE_SURFACE(((1.0005904089546,0.822187541867035,1.00401468696656),
(1.0003652771829,0.88999009367081,1.00248382673391),(1.00016469515081,0.950399042257587,
1.00111990082511),(1.00025604274098,0.922888044285544,1.00174104990631)))
REPRESENTATION_ITEM('')
SURFACE()
);
#3457=(
BOUNDED_SURFACE()
B_SPLINE_SURFACE(3,2,((#428016,#428017,#428018),(#428019,#428020,#428021),
(#428022,#428023,#428024),(#428025,#428026,#428027)),.UNSPECIFIED.,.F.,
 .F.,.F.)
B_SPLINE_SURFACE_WITH_KNOTS((4,4),(3,3),(-5.22358356749297E-6,5.7459419242428E-5),
(-0.00127120052059476,1.),.UNSPECIFIED.)
GEOMETRIC_REPRESENTATION_ITEM()
RATIONAL_B_SPLINE_SURFACE(((1.00054449313177,0.78583507363875,1.),(1.00047707767476,
0.812351526358855,1.),(1.00044031788588,0.826810216506272,1.),(1.0004477765332,
0.823876514387251,1.)))
REPRESENTATION_ITEM('')
SURFACE()
);
#3458=(
BOUNDED_SURFACE()
B_SPLINE_SURFACE(3,2,((#428029,#428030,#428031),(#428032,#428033,#428034),
(#428035,#428036,#428037),(#428038,#428039,#428040)),.UNSPECIFIED.,.F.,
 .F.,.F.)
B_SPLINE_SURFACE_WITH_KNOTS((4,4),(3,3),(-3.25260651745651E-19,4.88747512969879E-5),
(-0.00021580521588161,1.),.UNSPECIFIED.)
GEOMETRIC_REPRESENTATION_ITEM()
RATIONAL_B_SPLINE_SURFACE(((1.00008915600355,0.793434085499665,1.),(1.00008930225008,
0.793095246303214,1.),(1.0000894468463,0.792760230720471,1.),(1.00008958984409,
0.792428918540511,1.)))
REPRESENTATION_ITEM('')
SURFACE()
);
#3459=(
BOUNDED_SURFACE()
B_SPLINE_SURFACE(3,2,((#428042,#428043,#428044),(#428045,#428046,#428047),
(#428048,#428049,#428050),(#428051,#428052,#428053),(#428054,#428055,#428056),
(#428057,#428058,#428059)),.UNSPECIFIED.,.F.,.F.,.F.)
B_SPLINE_SURFACE_WITH_KNOTS((4,2,4),(3,3),(-1.76182853028894E-19,7.62675010863194E-5,
0.000152535002172639),(0.,1.02152348203075),.UNSPECIFIED.)
GEOMETRIC_REPRESENTATION_ITEM()
RATIONAL_B_SPLINE_SURFACE(((1.,0.789033595401239,1.00908146323695),(1.,
0.857071781054839,1.00615262590431),(1.,0.92208726471071,1.00335390671593),
(1.,0.922394466502382,1.00334068261144),(1.,0.857224384599031,1.00614605678502),
(1.,0.789033595401635,1.00908146323693)))
REPRESENTATION_ITEM('')
SURFACE()
);
#3460=(
BOUNDED_SURFACE()
B_SPLINE_SURFACE(3,2,((#428061,#428062,#428063),(#428064,#428065,#428066),
(#428067,#428068,#428069),(#428070,#428071,#428072)),.UNSPECIFIED.,.F.,
 .F.,.F.)
B_SPLINE_SURFACE_WITH_KNOTS((4,4),(3,3),(1.0842021724855E-19,4.88747512969882E-5),
(-0.000215489857601605,1.),.UNSPECIFIED.)
GEOMETRIC_REPRESENTATION_ITEM()
RATIONAL_B_SPLINE_SURFACE(((1.00008945889737,0.792428983985628,1.),(1.00008931610858,
0.792760296061173,1.),(1.00008917172371,0.793095311538253,1.),(1.00008902569093,
0.79343415062788,1.)))
REPRESENTATION_ITEM('')
SURFACE()
);
#3461=(
BOUNDED_SURFACE()
B_SPLINE_SURFACE(3,2,((#428074,#428075,#428076),(#428077,#428078,#428079),
(#428080,#428081,#428082),(#428083,#428084,#428085)),.UNSPECIFIED.,.F.,
 .F.,.F.)
B_SPLINE_SURFACE_WITH_KNOTS((4,4),(3,3),(-5.21974905013089E-6,5.74172395514397E-5),
(-0.00139822857724275,1.00051312364068),.UNSPECIFIED.)
GEOMETRIC_REPRESENTATION_ITEM()
RATIONAL_B_SPLINE_SURFACE(((1.00049256947239,0.823768952244066,1.0001806039785),
(1.0004844821571,0.826662424388356,1.00017763870883),(1.00052427784017,
0.812424361909431,1.00019223006922),(1.00059912365849,0.785646094632812,
1.00021967280231)))
REPRESENTATION_ITEM('')
SURFACE()
);
#3462=(
BOUNDED_SURFACE()
B_SPLINE_SURFACE(3,2,((#428089,#428090,#428091),(#428092,#428093,#428094),
(#428095,#428096,#428097),(#428098,#428099,#428100)),.UNSPECIFIED.,.F.,
 .F.,.F.)
B_SPLINE_SURFACE_WITH_KNOTS((4,4),(3,3),(3.22980774337781E-5,9.63764854872257E-5),
(-0.00154325936397012,1.01095292447533),.UNSPECIFIED.)
GEOMETRIC_REPRESENTATION_ITEM()
RATIONAL_B_SPLINE_SURFACE(((1.00023530983302,0.922925743796151,1.00168574728329),
(1.00015136166128,0.950422439594209,1.00108434699059),(1.00033574337403,
0.890029368953944,1.00240524789545),(1.0005426009423,0.822274473168309,
1.00388716464854)))
REPRESENTATION_ITEM('')
SURFACE()
);
#3463=(
BOUNDED_SURFACE()
B_SPLINE_SURFACE(3,2,((#428200,#428201,#428202),(#428203,#428204,#428205),
(#428206,#428207,#428208),(#428209,#428210,#428211)),.UNSPECIFIED.,.F.,
 .F.,.F.)
B_SPLINE_SURFACE_WITH_KNOTS((4,4),(3,3),(0.,0.000101260117256738),(0.,1.),
 .UNSPECIFIED.)
GEOMETRIC_REPRESENTATION_ITEM()
RATIONAL_B_SPLINE_SURFACE(((1.,0.796615278835171,1.),(1.,0.795896038055936,
1.),(1.,0.795193354661349,1.),(1.,0.794506193185544,1.)))
REPRESENTATION_ITEM('')
SURFACE()
);
#3464=(
BOUNDED_SURFACE()
B_SPLINE_SURFACE(3,2,((#428249,#428250,#428251),(#428252,#428253,#428254),
(#428255,#428256,#428257),(#428258,#428259,#428260),(#428261,#428262,#428263),
(#428264,#428265,#428266)),.UNSPECIFIED.,.F.,.F.,.F.)
B_SPLINE_SURFACE_WITH_KNOTS((4,2,4),(3,3),(1.32137139771671E-19,1.66936432462298E-5,
3.33872864924595E-5),(0.,1.),.UNSPECIFIED.)
GEOMETRIC_REPRESENTATION_ITEM()
RATIONAL_B_SPLINE_SURFACE(((1.,0.796615278835171,1.),(1.,0.862310524418131,
1.),(1.,0.923774472010519,1.),(1.,0.923983993203428,1.),(1.,0.862574873720954,
1.),(1.,0.79661527883518,1.)))
REPRESENTATION_ITEM('')
SURFACE()
);
#3465=(
BOUNDED_SURFACE()
B_SPLINE_SURFACE(3,2,((#428303,#428304,#428305),(#428306,#428307,#428308),
(#428309,#428310,#428311),(#428312,#428313,#428314)),.UNSPECIFIED.,.F.,
 .F.,.F.)
B_SPLINE_SURFACE_WITH_KNOTS((4,4),(3,3),(2.16840434497101E-19,0.000101244905251112),
(0.,1.),.UNSPECIFIED.)
GEOMETRIC_REPRESENTATION_ITEM()
RATIONAL_B_SPLINE_SURFACE(((1.,0.796615278835167,1.),(1.,0.79589614610979,
1.),(1.,0.7951935657965,1.),(1.,0.794506502889897,1.)))
REPRESENTATION_ITEM('')
SURFACE()
);
#3466=(
BOUNDED_SURFACE()
B_SPLINE_SURFACE(3,2,((#428350,#428351,#428352),(#428353,#428354,#428355),
(#428356,#428357,#428358),(#428359,#428360,#428361)),.UNSPECIFIED.,.F.,
 .F.,.F.)
B_SPLINE_SURFACE_WITH_KNOTS((4,4),(3,3),(2.85968127239939E-5,9.24681548475817E-5),
(-0.00167900678656574,1.0113082712785),.UNSPECIFIED.)
GEOMETRIC_REPRESENTATION_ITEM()
RATIONAL_B_SPLINE_SURFACE(((1.00059040895218,0.822187541868215,1.00401468696667),
(1.0003652771814,0.889990093671542,1.00248382673397),(1.00016469515013,
0.95039904225791,1.00111990082514),(1.00025604273993,0.922888044286058,
1.00174104990635)))
REPRESENTATION_ITEM('')
SURFACE()
);
#3467=(
BOUNDED_SURFACE()
B_SPLINE_SURFACE(3,2,((#428365,#428366,#428367),(#428368,#428369,#428370),
(#428371,#428372,#428373),(#428374,#428375,#428376)),.UNSPECIFIED.,.F.,
 .F.,.F.)
B_SPLINE_SURFACE_WITH_KNOTS((4,4),(3,3),(-5.22358356749274E-6,5.74594192424278E-5),
(-0.00127120052085918,1.),.UNSPECIFIED.)
GEOMETRIC_REPRESENTATION_ITEM()
RATIONAL_B_SPLINE_SURFACE(((1.00054449313188,0.785835073638707,1.),(1.00047707767486,
0.812351526358773,1.),(1.00044031788597,0.82681021650624,1.),(1.00044777653329,
0.823876514387199,1.)))
REPRESENTATION_ITEM('')
SURFACE()
);
#3468=(
BOUNDED_SURFACE()
B_SPLINE_SURFACE(3,2,((#428378,#428379,#428380),(#428381,#428382,#428383),
(#428384,#428385,#428386),(#428387,#428388,#428389)),.UNSPECIFIED.,.F.,
 .F.,.F.)
B_SPLINE_SURFACE_WITH_KNOTS((4,4),(3,3),(-1.0842021724855E-19,4.88747512969879E-5),
(-0.000215805215068792,1.),.UNSPECIFIED.)
GEOMETRIC_REPRESENTATION_ITEM()
RATIONAL_B_SPLINE_SURFACE(((1.00008915600321,0.793434085499829,1.),(1.00008930224974,
0.793095246303368,1.),(1.00008944684596,0.792760230720648,1.),(1.00008958984375,
0.792428918540678,1.)))
REPRESENTATION_ITEM('')
SURFACE()
);
#3469=(
BOUNDED_SURFACE()
B_SPLINE_SURFACE(3,2,((#428391,#428392,#428393),(#428394,#428395,#428396),
(#428397,#428398,#428399),(#428400,#428401,#428402),(#428403,#428404,#428405),
(#428406,#428407,#428408)),.UNSPECIFIED.,.F.,.F.,.F.)
B_SPLINE_SURFACE_WITH_KNOTS((4,2,4),(3,3),(-2.03287907341032E-20,7.62675010863198E-5,
0.00015253500217264),(0.,1.02152348203072),.UNSPECIFIED.)
GEOMETRIC_REPRESENTATION_ITEM()
RATIONAL_B_SPLINE_SURFACE(((1.,0.789033595401241,1.00908146323693),(1.,
0.857071781054893,1.0061526259043),(1.,0.922087264710644,1.00335390671593),
(1.,0.922394466502453,1.00334068261144),(1.,0.857224384598993,1.00614605678502),
(1.,0.789033595401637,1.00908146323692)))
REPRESENTATION_ITEM('')
SURFACE()
);
#3470=(
BOUNDED_SURFACE()
B_SPLINE_SURFACE(3,2,((#428410,#428411,#428412),(#428413,#428414,#428415),
(#428416,#428417,#428418),(#428419,#428420,#428421)),.UNSPECIFIED.,.F.,
 .F.,.F.)
B_SPLINE_SURFACE_WITH_KNOTS((4,4),(3,3),(3.25260651745651E-19,4.88747512969886E-5),
(-0.000215489856821933,1.),.UNSPECIFIED.)
GEOMETRIC_REPRESENTATION_ITEM()
RATIONAL_B_SPLINE_SURFACE(((1.00008945889704,0.792428983985787,1.),(1.00008931610826,
0.79276029606134,1.),(1.00008917172338,0.793095311538397,1.),(1.00008902569061,
0.793434150628038,1.)))
REPRESENTATION_ITEM('')
SURFACE()
);
#3471=(
BOUNDED_SURFACE()
B_SPLINE_SURFACE(3,2,((#428423,#428424,#428425),(#428426,#428427,#428428),
(#428429,#428430,#428431),(#428432,#428433,#428434)),.UNSPECIFIED.,.F.,
 .F.,.F.)
B_SPLINE_SURFACE_WITH_KNOTS((4,4),(3,3),(-5.21974905013084E-6,5.74172395514396E-5),
(-0.0013982285780412,1.00051312364079),.UNSPECIFIED.)
GEOMETRIC_REPRESENTATION_ITEM()
RATIONAL_B_SPLINE_SURFACE(((1.00049256947267,0.823768952243902,1.00018060397854),
(1.00048448215738,0.826662424388193,1.00017763870887),(1.00052427784047,
0.812424361909257,1.00019223006926),(1.00059912365884,0.785646094632611,
1.00021967280236)))
REPRESENTATION_ITEM('')
SURFACE()
);
#3472=(
BOUNDED_SURFACE()
B_SPLINE_SURFACE(3,2,((#428438,#428439,#428440),(#428441,#428442,#428443),
(#428444,#428445,#428446),(#428447,#428448,#428449)),.UNSPECIFIED.,.F.,
 .F.,.F.)
B_SPLINE_SURFACE_WITH_KNOTS((4,4),(3,3),(3.22980774337777E-5,9.63764854872247E-5),
(-0.00154325936325689,1.01095292447535),.UNSPECIFIED.)
GEOMETRIC_REPRESENTATION_ITEM()
RATIONAL_B_SPLINE_SURFACE(((1.00023530983292,0.92292574379621,1.0016857472833),
(1.00015136166121,0.950422439594245,1.00108434699059),(1.00033574337388,
0.890029368954018,1.00240524789546),(1.00054260094205,0.822274473168436,
1.00388716464855)))
REPRESENTATION_ITEM('')
SURFACE()
);
#3473=(
BOUNDED_SURFACE()
B_SPLINE_SURFACE(3,2,((#428549,#428550,#428551),(#428552,#428553,#428554),
(#428555,#428556,#428557),(#428558,#428559,#428560)),.UNSPECIFIED.,.F.,
 .F.,.F.)
B_SPLINE_SURFACE_WITH_KNOTS((4,4),(3,3),(0.,0.000101260117256738),(0.,1.),
 .UNSPECIFIED.)
GEOMETRIC_REPRESENTATION_ITEM()
RATIONAL_B_SPLINE_SURFACE(((1.,0.796615278835171,1.),(1.,0.795896038055939,
1.),(1.,0.795193354661346,1.),(1.,0.794506193185548,1.)))
REPRESENTATION_ITEM('')
SURFACE()
);
#3474=(
BOUNDED_SURFACE()
B_SPLINE_SURFACE(3,2,((#428598,#428599,#428600),(#428601,#428602,#428603),
(#428604,#428605,#428606),(#428607,#428608,#428609),(#428610,#428611,#428612),
(#428613,#428614,#428615)),.UNSPECIFIED.,.F.,.F.,.F.)
B_SPLINE_SURFACE_WITH_KNOTS((4,2,4),(3,3),(-1.82959116606929E-19,1.66936432462294E-5,
3.33872864924589E-5),(0.,1.),.UNSPECIFIED.)
GEOMETRIC_REPRESENTATION_ITEM()
RATIONAL_B_SPLINE_SURFACE(((1.,0.796615278835176,1.),(1.,0.862310524418125,
1.),(1.,0.923774472010523,1.),(1.,0.923983993203423,1.),(1.,0.862574873720947,
1.),(1.,0.796615278835187,1.)))
REPRESENTATION_ITEM('')
SURFACE()
);
#3475=(
BOUNDED_SURFACE()
B_SPLINE_SURFACE(3,2,((#428652,#428653,#428654),(#428655,#428656,#428657),
(#428658,#428659,#428660),(#428661,#428662,#428663)),.UNSPECIFIED.,.F.,
 .F.,.F.)
B_SPLINE_SURFACE_WITH_KNOTS((4,4),(3,3),(0.,0.000101244905251112),(0.,1.),
 .UNSPECIFIED.)
GEOMETRIC_REPRESENTATION_ITEM()
RATIONAL_B_SPLINE_SURFACE(((1.,0.796615278835172,1.),(1.,0.795896146109797,
1.),(1.,0.795193565796499,1.),(1.,0.794506502889901,1.)))
REPRESENTATION_ITEM('')
SURFACE()
);
#3476=(
BOUNDED_SURFACE()
B_SPLINE_SURFACE(3,2,((#428699,#428700,#428701),(#428702,#428703,#428704),
(#428705,#428706,#428707),(#428708,#428709,#428710)),.UNSPECIFIED.,.F.,
 .F.,.F.)
B_SPLINE_SURFACE_WITH_KNOTS((4,4),(3,3),(2.85968127239939E-5,9.24681548475817E-5),
(-0.00167900678552175,1.01130827127825),.UNSPECIFIED.)
GEOMETRIC_REPRESENTATION_ITEM()
RATIONAL_B_SPLINE_SURFACE(((1.00059040895181,0.822187541868451,1.00401468696657),
(1.00036527718117,0.889990093671682,1.00248382673392),(1.00016469515003,
0.950399042257977,1.00111990082511),(1.00025604273977,0.92288804428616,
1.00174104990631)))
REPRESENTATION_ITEM('')
SURFACE()
);
#3477=(
BOUNDED_SURFACE()
B_SPLINE_SURFACE(3,2,((#428714,#428715,#428716),(#428717,#428718,#428719),
(#428720,#428721,#428722),(#428723,#428724,#428725)),.UNSPECIFIED.,.F.,
 .F.,.F.)
B_SPLINE_SURFACE_WITH_KNOTS((4,4),(3,3),(-5.22358356749324E-6,5.74594192424276E-5),
(-0.0012712005205181,1.),.UNSPECIFIED.)
GEOMETRIC_REPRESENTATION_ITEM()
RATIONAL_B_SPLINE_SURFACE(((1.00054449313173,0.785835073638774,1.),(1.00047707767473,
0.812351526358856,1.),(1.00044031788585,0.826810216506294,1.),(1.00044777653317,
0.823876514387263,1.)))
REPRESENTATION_ITEM('')
SURFACE()
);
#3478=(
BOUNDED_SURFACE()
B_SPLINE_SURFACE(3,2,((#428727,#428728,#428729),(#428730,#428731,#428732),
(#428733,#428734,#428735),(#428736,#428737,#428738)),.UNSPECIFIED.,.F.,
 .F.,.F.)
B_SPLINE_SURFACE_WITH_KNOTS((4,4),(3,3),(-2.16840434497101E-19,4.88747512969878E-5),
(-0.000215805215532899,1.),.UNSPECIFIED.)
GEOMETRIC_REPRESENTATION_ITEM()
RATIONAL_B_SPLINE_SURFACE(((1.0000891560034,0.793434085499735,1.),(1.00008930224993,
0.793095246303274,1.),(1.00008944684615,0.792760230720554,1.),(1.00008958984395,
0.792428918540581,1.)))
REPRESENTATION_ITEM('')
SURFACE()
);
#3479=(
BOUNDED_SURFACE()
B_SPLINE_SURFACE(3,2,((#428740,#428741,#428742),(#428743,#428744,#428745),
(#428746,#428747,#428748),(#428749,#428750,#428751),(#428752,#428753,#428754),
(#428755,#428756,#428757)),.UNSPECIFIED.,.F.,.F.,.F.)
B_SPLINE_SURFACE_WITH_KNOTS((4,2,4),(3,3),(2.71050543121376E-19,7.62675010863199E-5,
0.00015253500217264),(0.,1.02152348203062),.UNSPECIFIED.)
GEOMETRIC_REPRESENTATION_ITEM()
RATIONAL_B_SPLINE_SURFACE(((1.,0.789033595401262,1.00908146323689),(1.,
0.857071781054858,1.00615262590427),(1.,0.922087264710723,1.00335390671591),
(1.,0.92239446650239,1.00334068261142),(1.,0.857224384599052,1.00614605678498),
(1.,0.78903359540166,1.00908146323687)))
REPRESENTATION_ITEM('')
SURFACE()
);
#3480=(
BOUNDED_SURFACE()
B_SPLINE_SURFACE(3,2,((#428759,#428760,#428761),(#428762,#428763,#428764),
(#428765,#428766,#428767),(#428768,#428769,#428770)),.UNSPECIFIED.,.F.,
 .F.,.F.)
B_SPLINE_SURFACE_WITH_KNOTS((4,4),(3,3),(2.43945488809238E-19,4.88747512969882E-5),
(-0.000215489856995972,1.),.UNSPECIFIED.)
GEOMETRIC_REPRESENTATION_ITEM()
RATIONAL_B_SPLINE_SURFACE(((1.00008945889711,0.792428983985754,1.),(1.00008931610833,
0.792760296061308,1.),(1.00008917172346,0.793095311538361,1.),(1.00008902569068,
0.793434150628005,1.)))
REPRESENTATION_ITEM('')
SURFACE()
);
#3481=(
BOUNDED_SURFACE()
B_SPLINE_SURFACE(3,2,((#428772,#428773,#428774),(#428775,#428776,#428777),
(#428778,#428779,#428780),(#428781,#428782,#428783)),.UNSPECIFIED.,.F.,
 .F.,.F.)
B_SPLINE_SURFACE_WITH_KNOTS((4,4),(3,3),(-5.21974905013083E-6,5.74172395514397E-5),
(-0.00139822857793678,1.00051312364077),.UNSPECIFIED.)
GEOMETRIC_REPRESENTATION_ITEM()
RATIONAL_B_SPLINE_SURFACE(((1.00049256947264,0.823768952243928,1.00018060397853),
(1.00048448215734,0.826662424388221,1.00017763870886),(1.00052427784043,
0.812424361909281,1.00019223006925),(1.00059912365879,0.785646094632644,
1.00021967280236)))
REPRESENTATION_ITEM('')
SURFACE()
);
#3482=(
BOUNDED_SURFACE()
B_SPLINE_SURFACE(3,2,((#428787,#428788,#428789),(#428790,#428791,#428792),
(#428793,#428794,#428795),(#428796,#428797,#428798)),.UNSPECIFIED.,.F.,
 .F.,.F.)
B_SPLINE_SURFACE_WITH_KNOTS((4,4),(3,3),(3.22980774337776E-5,9.63764854872256E-5),
(-0.00154325936406371,1.01095292447559),.UNSPECIFIED.)
GEOMETRIC_REPRESENTATION_ITEM()
RATIONAL_B_SPLINE_SURFACE(((1.00023530983304,0.922925743796126,1.00168574728333),
(1.00015136166129,0.950422439594194,1.00108434699061),(1.00033574337405,
0.890029368953907,1.00240524789551),(1.00054260094233,0.822274473168248,
1.00388716464864)))
REPRESENTATION_ITEM('')
SURFACE()
);
#3483=(
BOUNDED_SURFACE()
B_SPLINE_SURFACE(3,2,((#428898,#428899,#428900),(#428901,#428902,#428903),
(#428904,#428905,#428906),(#428907,#428908,#428909)),.UNSPECIFIED.,.F.,
 .F.,.F.)
B_SPLINE_SURFACE_WITH_KNOTS((4,4),(3,3),(0.,0.000101260117256737),(0.,1.),
 .UNSPECIFIED.)
GEOMETRIC_REPRESENTATION_ITEM()
RATIONAL_B_SPLINE_SURFACE(((1.,0.796615278835169,1.),(1.,0.79589603805594,
1.),(1.,0.795193354661342,1.),(1.,0.794506193185545,1.)))
REPRESENTATION_ITEM('')
SURFACE()
);
#3484=(
BOUNDED_SURFACE()
B_SPLINE_SURFACE(3,2,((#428947,#428948,#428949),(#428950,#428951,#428952),
(#428953,#428954,#428955),(#428956,#428957,#428958),(#428959,#428960,#428961),
(#428962,#428963,#428964)),.UNSPECIFIED.,.F.,.F.,.F.)
B_SPLINE_SURFACE_WITH_KNOTS((4,2,4),(3,3),(-1.99899775552015E-19,1.66936432462289E-5,
3.3387286492458E-5),(0.,1.),.UNSPECIFIED.)
GEOMETRIC_REPRESENTATION_ITEM()
RATIONAL_B_SPLINE_SURFACE(((1.,0.796615278835174,1.),(1.,0.862310524418136,
1.),(1.,0.923774472010518,1.),(1.,0.923983993203428,1.),(1.,0.862574873720939,
1.),(1.,0.796615278835189,1.)))
REPRESENTATION_ITEM('')
SURFACE()
);
#3485=(
BOUNDED_SURFACE()
B_SPLINE_SURFACE(3,2,((#429001,#429002,#429003),(#429004,#429005,#429006),
(#429007,#429008,#429009),(#429010,#429011,#429012)),.UNSPECIFIED.,.F.,
 .F.,.F.)
B_SPLINE_SURFACE_WITH_KNOTS((4,4),(3,3),(0.,0.000101244905251112),(0.,1.),
 .UNSPECIFIED.)
GEOMETRIC_REPRESENTATION_ITEM()
RATIONAL_B_SPLINE_SURFACE(((1.,0.796615278835169,1.),(1.,0.795896146109799,
1.),(1.,0.795193565796492,1.),(1.,0.7945065028899,1.)))
REPRESENTATION_ITEM('')
SURFACE()
);
#3486=(
BOUNDED_SURFACE()
B_SPLINE_SURFACE(3,2,((#429048,#429049,#429050),(#429051,#429052,#429053),
(#429054,#429055,#429056),(#429057,#429058,#429059)),.UNSPECIFIED.,.F.,
 .F.,.F.)
B_SPLINE_SURFACE_WITH_KNOTS((4,4),(3,3),(2.85968127239939E-5,9.24681548475814E-5),
(-0.0016790067864226,1.01130827127812),.UNSPECIFIED.)
GEOMETRIC_REPRESENTATION_ITEM()
RATIONAL_B_SPLINE_SURFACE(((1.00059040895212,0.822187541868312,1.00401468696653),
(1.00036527718137,0.889990093671596,1.00248382673389),(1.00016469515012,
0.950399042257943,1.0011199008251),(1.00025604273991,0.922888044286096,
1.00174104990629)))
REPRESENTATION_ITEM('')
SURFACE()
);
#3487=(
BOUNDED_SURFACE()
B_SPLINE_SURFACE(3,2,((#429063,#429064,#429065),(#429066,#429067,#429068),
(#429069,#429070,#429071),(#429072,#429073,#429074)),.UNSPECIFIED.,.F.,
 .F.,.F.)
B_SPLINE_SURFACE_WITH_KNOTS((4,4),(3,3),(-5.22358356749289E-6,5.74594192424278E-5),
(-0.00127120052075543,1.),.UNSPECIFIED.)
GEOMETRIC_REPRESENTATION_ITEM()
RATIONAL_B_SPLINE_SURFACE(((1.00054449313184,0.785835073638715,1.),(1.00047707767482,
0.81235152635882,1.),(1.00044031788593,0.826810216506243,1.),(1.00044777653326,
0.823876514387217,1.)))
REPRESENTATION_ITEM('')
SURFACE()
);
#3488=(
BOUNDED_SURFACE()
B_SPLINE_SURFACE(3,2,((#429076,#429077,#429078),(#429079,#429080,#429081),
(#429082,#429083,#429084),(#429085,#429086,#429087)),.UNSPECIFIED.,.F.,
 .F.,.F.)
B_SPLINE_SURFACE_WITH_KNOTS((4,4),(3,3),(0.,4.88747512969881E-5),(-0.000215805215095398,
1.),.UNSPECIFIED.)
GEOMETRIC_REPRESENTATION_ITEM()
RATIONAL_B_SPLINE_SURFACE(((1.00008915600322,0.793434085499822,1.),(1.00008930224975,
0.793095246303359,1.),(1.00008944684597,0.792760230720646,1.),(1.00008958984376,
0.79242891854067,1.)))
REPRESENTATION_ITEM('')
SURFACE()
);
#3489=(
BOUNDED_SURFACE()
B_SPLINE_SURFACE(3,2,((#429089,#429090,#429091),(#429092,#429093,#429094),
(#429095,#429096,#429097),(#429098,#429099,#429100),(#429101,#429102,#429103),
(#429104,#429105,#429106)),.UNSPECIFIED.,.F.,.F.,.F.)
B_SPLINE_SURFACE_WITH_KNOTS((4,2,4),(3,3),(-6.7762635780344E-20,7.62675010863195E-5,
0.000152535002172639),(0.,1.02152348203083),.UNSPECIFIED.)
GEOMETRIC_REPRESENTATION_ITEM()
RATIONAL_B_SPLINE_SURFACE(((1.,0.789033595401219,1.00908146323698),(1.,
0.857071781054809,1.00615262590433),(1.,0.922087264710727,1.00335390671594),
(1.,0.922394466502351,1.00334068261146),(1.,0.857224384599042,1.00614605678505),
(1.,0.789033595401617,1.00908146323697)))
REPRESENTATION_ITEM('')
SURFACE()
);
#3490=(
BOUNDED_SURFACE()
B_SPLINE_SURFACE(3,2,((#429108,#429109,#429110),(#429111,#429112,#429113),
(#429114,#429115,#429116),(#429117,#429118,#429119)),.UNSPECIFIED.,.F.,
 .F.,.F.)
B_SPLINE_SURFACE_WITH_KNOTS((4,4),(3,3),(1.89735380184963E-19,4.8874751296988E-5),
(-0.00021548985687891,1.),.UNSPECIFIED.)
GEOMETRIC_REPRESENTATION_ITEM()
RATIONAL_B_SPLINE_SURFACE(((1.00008945889707,0.792428983985783,1.),(1.00008931610828,
0.792760296061324,1.),(1.00008917172341,0.79309531153839,1.),(1.00008902569063,
0.793434150628027,1.)))
REPRESENTATION_ITEM('')
SURFACE()
);
#3491=(
BOUNDED_SURFACE()
B_SPLINE_SURFACE(3,2,((#429121,#429122,#429123),(#429124,#429125,#429126),
(#429127,#429128,#429129),(#429130,#429131,#429132)),.UNSPECIFIED.,.F.,
 .F.,.F.)
B_SPLINE_SURFACE_WITH_KNOTS((4,4),(3,3),(-5.21974905013083E-6,5.74172395514395E-5),
(-0.00139822857813303,1.00051312364079),.UNSPECIFIED.)
GEOMETRIC_REPRESENTATION_ITEM()
RATIONAL_B_SPLINE_SURFACE(((1.00049256947271,0.823768952243883,1.00018060397854),
(1.00048448215741,0.826662424388189,1.00017763870886),(1.0005242778405,
0.812424361909235,1.00019223006926),(1.00059912365888,0.7856460946326,1.00021967280236)))
REPRESENTATION_ITEM('')
SURFACE()
);
#3492=(
BOUNDED_SURFACE()
B_SPLINE_SURFACE(3,2,((#429136,#429137,#429138),(#429139,#429140,#429141),
(#429142,#429143,#429144),(#429145,#429146,#429147)),.UNSPECIFIED.,.F.,
 .F.,.F.)
B_SPLINE_SURFACE_WITH_KNOTS((4,4),(3,3),(3.22980774337778E-5,9.63764854872248E-5),
(-0.00154325936355796,1.01095292447537),.UNSPECIFIED.)
GEOMETRIC_REPRESENTATION_ITEM()
RATIONAL_B_SPLINE_SURFACE(((1.00023530983296,0.922925743796181,1.0016857472833),
(1.00015136166124,0.950422439594237,1.00108434699059),(1.00033574337394,
0.890029368953977,1.00240524789546),(1.00054260094215,0.822274473168379,
1.00388716464856)))
REPRESENTATION_ITEM('')
SURFACE()
);
#3493=(
BOUNDED_SURFACE()
B_SPLINE_SURFACE(3,2,((#429247,#429248,#429249),(#429250,#429251,#429252),
(#429253,#429254,#429255),(#429256,#429257,#429258)),.UNSPECIFIED.,.F.,
 .F.,.F.)
B_SPLINE_SURFACE_WITH_KNOTS((4,4),(3,3),(0.,0.000101260117256737),(0.,1.),
 .UNSPECIFIED.)
GEOMETRIC_REPRESENTATION_ITEM()
RATIONAL_B_SPLINE_SURFACE(((1.,0.796615278835173,1.),(1.,0.795896038055931,
1.),(1.,0.795193354661359,1.),(1.,0.794506193185536,1.)))
REPRESENTATION_ITEM('')
SURFACE()
);
#3494=(
BOUNDED_SURFACE()
B_SPLINE_SURFACE(3,2,((#429296,#429297,#429298),(#429299,#429300,#429301),
(#429302,#429303,#429304),(#429305,#429306,#429307),(#429308,#429309,#429310),
(#429311,#429312,#429313)),.UNSPECIFIED.,.F.,.F.,.F.)
B_SPLINE_SURFACE_WITH_KNOTS((4,2,4),(3,3),(-1.23666810299128E-19,1.66936432462298E-5,
3.33872864924597E-5),(0.,1.),.UNSPECIFIED.)
GEOMETRIC_REPRESENTATION_ITEM()
RATIONAL_B_SPLINE_SURFACE(((1.,0.796615278835171,1.),(1.,0.862310524418122,
1.),(1.,0.92377447201052,1.),(1.,0.92398399320343,1.),(1.,0.862574873720945,
1.),(1.,0.796615278835183,1.)))
REPRESENTATION_ITEM('')
SURFACE()
);
#3495=(
BOUNDED_SURFACE()
B_SPLINE_SURFACE(3,2,((#429350,#429351,#429352),(#429353,#429354,#429355),
(#429356,#429357,#429358),(#429359,#429360,#429361)),.UNSPECIFIED.,.F.,
 .F.,.F.)
B_SPLINE_SURFACE_WITH_KNOTS((4,4),(3,3),(0.,0.000101244905251112),(0.,1.),
 .UNSPECIFIED.)
GEOMETRIC_REPRESENTATION_ITEM()
RATIONAL_B_SPLINE_SURFACE(((1.,0.796615278835171,1.),(1.,0.795896146109787,
1.),(1.,0.795193565796502,1.),(1.,0.794506502889898,1.)))
REPRESENTATION_ITEM('')
SURFACE()
);
#3496=(
BOUNDED_SURFACE()
B_SPLINE_SURFACE(3,2,((#429397,#429398,#429399),(#429400,#429401,#429402),
(#429403,#429404,#429405),(#429406,#429407,#429408)),.UNSPECIFIED.,.F.,
 .F.,.F.)
B_SPLINE_SURFACE_WITH_KNOTS((4,4),(3,3),(2.85968127239939E-5,9.24681548475814E-5),
(-0.00167900678789534,1.01130827127821),.UNSPECIFIED.)
GEOMETRIC_REPRESENTATION_ITEM()
RATIONAL_B_SPLINE_SURFACE(((1.00059040895264,0.822187541868032,1.00401468696656),
(1.00036527718169,0.889990093671424,1.00248382673391),(1.00016469515026,
0.950399042257866,1.00111990082511),(1.00025604274013,0.922888044285976,
1.00174104990631)))
REPRESENTATION_ITEM('')
SURFACE()
);
#3497=(
BOUNDED_SURFACE()
B_SPLINE_SURFACE(3,2,((#429412,#429413,#429414),(#429415,#429416,#429417),
(#429418,#429419,#429420),(#429421,#429422,#429423)),.UNSPECIFIED.,.F.,
 .F.,.F.)
B_SPLINE_SURFACE_WITH_KNOTS((4,4),(3,3),(-5.22358356749297E-6,5.74594192424279E-5),
(-0.00127120052063385,1.),.UNSPECIFIED.)
GEOMETRIC_REPRESENTATION_ITEM()
RATIONAL_B_SPLINE_SURFACE(((1.00054449313178,0.785835073638746,1.),(1.00047707767478,
0.81235152635883,1.),(1.00044031788589,0.826810216506275,1.),(1.00044777653321,
0.823876514387243,1.)))
REPRESENTATION_ITEM('')
SURFACE()
);
#3498=(
BOUNDED_SURFACE()
B_SPLINE_SURFACE(3,2,((#429425,#429426,#429427),(#429428,#429429,#429430),
(#429431,#429432,#429433),(#429434,#429435,#429436)),.UNSPECIFIED.,.F.,
 .F.,.F.)
B_SPLINE_SURFACE_WITH_KNOTS((4,4),(3,3),(-2.71050543121376E-20,4.88747512969882E-5),
(-0.000215805215167394,1.),.UNSPECIFIED.)
GEOMETRIC_REPRESENTATION_ITEM()
RATIONAL_B_SPLINE_SURFACE(((1.00008915600325,0.793434085499807,1.),(1.00008930224978,
0.793095246303351,1.),(1.000089446846,0.792760230720625,1.),(1.00008958984379,
0.792428918540659,1.)))
REPRESENTATION_ITEM('')
SURFACE()
);
#3499=(
BOUNDED_SURFACE()
B_SPLINE_SURFACE(3,2,((#429438,#429439,#429440),(#429441,#429442,#429443),
(#429444,#429445,#429446),(#429447,#429448,#429449),(#429450,#429451,#429452),
(#429453,#429454,#429455)),.UNSPECIFIED.,.F.,.F.,.F.)
B_SPLINE_SURFACE_WITH_KNOTS((4,2,4),(3,3),(5.42101086242752E-20,7.62675010863199E-5,
0.00015253500217264),(0.,1.02152348203028),.UNSPECIFIED.)
GEOMETRIC_REPRESENTATION_ITEM()
RATIONAL_B_SPLINE_SURFACE(((1.,0.789033595401331,1.00908146323675),(1.,
0.857071781054903,1.00615262590417),(1.,0.922087264710748,1.00335390671586),
(1.,0.922394466502417,1.00334068261137),(1.,0.857224384599095,1.00614605678489),
(1.,0.789033595401731,1.00908146323673)))
REPRESENTATION_ITEM('')
SURFACE()
);
#3500=(
BOUNDED_SURFACE()
B_SPLINE_SURFACE(3,2,((#429457,#429458,#429459),(#429460,#429461,#429462),
(#429463,#429464,#429465),(#429466,#429467,#429468)),.UNSPECIFIED.,.F.,
 .F.,.F.)
B_SPLINE_SURFACE_WITH_KNOTS((4,4),(3,3),(5.42101086242752E-19,4.88747512969884E-5),
(-0.000215489857109308,1.),.UNSPECIFIED.)
GEOMETRIC_REPRESENTATION_ITEM()
RATIONAL_B_SPLINE_SURFACE(((1.00008945889716,0.792428983985732,1.),(1.00008931610838,
0.79276029606126,1.),(1.0000891717235,0.793095311538357,1.),(1.00008902569073,
0.793434150627978,1.)))
REPRESENTATION_ITEM('')
SURFACE()
);
#3501=(
BOUNDED_SURFACE()
B_SPLINE_SURFACE(3,2,((#429470,#429471,#429472),(#429473,#429474,#429475),
(#429476,#429477,#429478),(#429479,#429480,#429481)),.UNSPECIFIED.,.F.,
 .F.,.F.)
B_SPLINE_SURFACE_WITH_KNOTS((4,4),(3,3),(-5.21974905012879E-6,5.74172395514404E-5),
(-0.00139822857791635,1.00051312364079),.UNSPECIFIED.)
GEOMETRIC_REPRESENTATION_ITEM()
RATIONAL_B_SPLINE_SURFACE(((1.00049256947263,0.823768952243921,1.00018060397854),
(1.00048448215733,0.826662424388215,1.00017763870886),(1.00052427784042,
0.812424361909278,1.00019223006926),(1.00059912365878,0.785646094632641,
1.00021967280236)))
REPRESENTATION_ITEM('')
SURFACE()
);
#3502=(
BOUNDED_SURFACE()
B_SPLINE_SURFACE(3,2,((#429485,#429486,#429487),(#429488,#429489,#429490),
(#429491,#429492,#429493),(#429494,#429495,#429496)),.UNSPECIFIED.,.F.,
 .F.,.F.)
B_SPLINE_SURFACE_WITH_KNOTS((4,4),(3,3),(3.22980774337777E-5,9.63764854872246E-5),
(-0.00154325936392007,1.01095292447559),.UNSPECIFIED.)
GEOMETRIC_REPRESENTATION_ITEM()
RATIONAL_B_SPLINE_SURFACE(((1.00023530983302,0.922925743796137,1.00168574728333),
(1.00015136166127,0.950422439594199,1.00108434699061),(1.00033574337402,
0.890029368953927,1.00240524789551),(1.00054260094228,0.822274473168269,
1.00388716464864)))
REPRESENTATION_ITEM('')
SURFACE()
);
#3503=(
BOUNDED_SURFACE()
B_SPLINE_SURFACE(3,2,((#429596,#429597,#429598),(#429599,#429600,#429601),
(#429602,#429603,#429604),(#429605,#429606,#429607)),.UNSPECIFIED.,.F.,
 .F.,.F.)
B_SPLINE_SURFACE_WITH_KNOTS((4,4),(3,3),(-2.16840434497101E-19,0.000101260117256737),
(0.,1.),.UNSPECIFIED.)
GEOMETRIC_REPRESENTATION_ITEM()
RATIONAL_B_SPLINE_SURFACE(((1.,0.796615278835171,1.),(1.,0.795896038055954,
1.),(1.,0.795193354661325,1.),(1.,0.794506193185548,1.)))
REPRESENTATION_ITEM('')
SURFACE()
);
#3504=(
BOUNDED_SURFACE()
B_SPLINE_SURFACE(3,2,((#429645,#429646,#429647),(#429648,#429649,#429650),
(#429651,#429652,#429653),(#429654,#429655,#429656),(#429657,#429658,#429659),
(#429660,#429661,#429662)),.UNSPECIFIED.,.F.,.F.,.F.)
B_SPLINE_SURFACE_WITH_KNOTS((4,2,4),(3,3),(1.52465930505774E-20,1.66936432462301E-5,
3.33872864924601E-5),(0.,1.),.UNSPECIFIED.)
GEOMETRIC_REPRESENTATION_ITEM()
RATIONAL_B_SPLINE_SURFACE(((1.,0.796615278835175,1.),(1.,0.862310524418118,
1.),(1.,0.923774472010521,1.),(1.,0.923983993203426,1.),(1.,0.862574873720939,
1.),(1.,0.796615278835187,1.)))
REPRESENTATION_ITEM('')
SURFACE()
);
#3505=(
BOUNDED_SURFACE()
B_SPLINE_SURFACE(3,2,((#429699,#429700,#429701),(#429702,#429703,#429704),
(#429705,#429706,#429707),(#429708,#429709,#429710)),.UNSPECIFIED.,.F.,
 .F.,.F.)
B_SPLINE_SURFACE_WITH_KNOTS((4,4),(3,3),(0.,0.000101244905251112),(0.,1.),
 .UNSPECIFIED.)
GEOMETRIC_REPRESENTATION_ITEM()
RATIONAL_B_SPLINE_SURFACE(((1.,0.796615278835175,1.),(1.,0.795896146109783,
1.),(1.,0.795193565796506,1.),(1.,0.794506502889895,1.)))
REPRESENTATION_ITEM('')
SURFACE()
);
#3506=(
BOUNDED_SURFACE()
B_SPLINE_SURFACE(3,2,((#429746,#429747,#429748),(#429749,#429750,#429751),
(#429752,#429753,#429754),(#429755,#429756,#429757)),.UNSPECIFIED.,.F.,
 .F.,.F.)
B_SPLINE_SURFACE_WITH_KNOTS((4,4),(3,3),(2.85968127239939E-5,9.24681548475819E-5),
(-0.00167900679337037,1.01130827127828),.UNSPECIFIED.)
GEOMETRIC_REPRESENTATION_ITEM()
RATIONAL_B_SPLINE_SURFACE(((1.00059040895457,0.822187541867037,1.00401468696659),
(1.00036527718288,0.889990093670808,1.00248382673392),(1.0001646951508,
0.95039904225759,1.00111990082511),(1.00025604274097,0.922888044285542,
1.00174104990632)))
REPRESENTATION_ITEM('')
SURFACE()
);
#3507=(
BOUNDED_SURFACE()
B_SPLINE_SURFACE(3,2,((#429761,#429762,#429763),(#429764,#429765,#429766),
(#429767,#429768,#429769),(#429770,#429771,#429772)),.UNSPECIFIED.,.F.,
 .F.,.F.)
B_SPLINE_SURFACE_WITH_KNOTS((4,4),(3,3),(-5.22358356749127E-6,5.74594192424277E-5),
(-0.00127120052043637,1.),.UNSPECIFIED.)
GEOMETRIC_REPRESENTATION_ITEM()
RATIONAL_B_SPLINE_SURFACE(((1.0005444931317,0.785835073638799,1.),(1.0004770776747,
0.812351526358858,1.),(1.00044031788582,0.826810216506319,1.),(1.00044777653314,
0.823876514387272,0.999999999999999)))
REPRESENTATION_ITEM('')
SURFACE()
);
#3508=(
BOUNDED_SURFACE()
B_SPLINE_SURFACE(3,2,((#429774,#429775,#429776),(#429777,#429778,#429779),
(#429780,#429781,#429782),(#429783,#429784,#429785)),.UNSPECIFIED.,.F.,
 .F.,.F.)
B_SPLINE_SURFACE_WITH_KNOTS((4,4),(3,3),(-1.62630325872826E-19,4.8874751296988E-5),
(-0.000215805215728941,1.),.UNSPECIFIED.)
GEOMETRIC_REPRESENTATION_ITEM()
RATIONAL_B_SPLINE_SURFACE(((1.00008915600348,0.793434085499697,1.),(1.00008930225001,
0.79309524630324,1.),(1.00008944684623,0.792760230720509,1.),(1.00008958984403,
0.792428918540541,1.)))
REPRESENTATION_ITEM('')
SURFACE()
);
#3509=(
BOUNDED_SURFACE()
B_SPLINE_SURFACE(3,2,((#429787,#429788,#429789),(#429790,#429791,#429792),
(#429793,#429794,#429795),(#429796,#429797,#429798),(#429799,#429800,#429801),
(#429802,#429803,#429804)),.UNSPECIFIED.,.F.,.F.,.F.)
B_SPLINE_SURFACE_WITH_KNOTS((4,2,4),(3,3),(1.21972744404619E-19,7.626750108632E-5,
0.00015253500217264),(0.,1.02152348203059),.UNSPECIFIED.)
GEOMETRIC_REPRESENTATION_ITEM()
RATIONAL_B_SPLINE_SURFACE(((1.,0.789033595401271,1.00908146323688),(1.,
0.857071781054863,1.00615262590426),(1.,0.922087264710716,1.00335390671591),
(1.,0.922394466502397,1.00334068261142),(1.,0.857224384599058,1.00614605678498),
(1.,0.789033595401664,1.00908146323686)))
REPRESENTATION_ITEM('')
SURFACE()
);
#3510=(
BOUNDED_SURFACE()
B_SPLINE_SURFACE(3,2,((#429806,#429807,#429808),(#429809,#429810,#429811),
(#429812,#429813,#429814),(#429815,#429816,#429817)),.UNSPECIFIED.,.F.,
 .F.,.F.)
B_SPLINE_SURFACE_WITH_KNOTS((4,4),(3,3),(3.25260651745651E-19,4.88747512969883E-5),
(-0.000215489857120083,1.),.UNSPECIFIED.)
GEOMETRIC_REPRESENTATION_ITEM()
RATIONAL_B_SPLINE_SURFACE(((1.00008945889717,0.792428983985724,1.),(1.00008931610838,
0.792760296061273,1.),(1.00008917172351,0.793095311538346,1.),(1.00008902569073,
0.793434150627979,1.)))
REPRESENTATION_ITEM('')
SURFACE()
);
#3511=(
BOUNDED_SURFACE()
B_SPLINE_SURFACE(3,2,((#429819,#429820,#429821),(#429822,#429823,#429824),
(#429825,#429826,#429827),(#429828,#429829,#429830)),.UNSPECIFIED.,.F.,
 .F.,.F.)
B_SPLINE_SURFACE_WITH_KNOTS((4,4),(3,3),(-5.219749050131E-6,5.74172395514396E-5),
(-0.00139822857776702,1.00051312364072),.UNSPECIFIED.)
GEOMETRIC_REPRESENTATION_ITEM()
RATIONAL_B_SPLINE_SURFACE(((1.00049256947258,0.823768952243958,1.00018060397851),
(1.00048448215728,0.826662424388262,1.00017763870884),(1.00052427784036,
0.812424361909323,1.00019223006923),(1.00059912365872,0.78564609463269,
1.00021967280233)))
REPRESENTATION_ITEM('')
SURFACE()
);
#3512=(
BOUNDED_SURFACE()
B_SPLINE_SURFACE(3,2,((#429834,#429835,#429836),(#429837,#429838,#429839),
(#429840,#429841,#429842),(#429843,#429844,#429845)),.UNSPECIFIED.,.F.,
 .F.,.F.)
B_SPLINE_SURFACE_WITH_KNOTS((4,4),(3,3),(3.22980774337781E-5,9.63764854872258E-5),
(-0.00154325936368032,1.01095292447566),.UNSPECIFIED.)
GEOMETRIC_REPRESENTATION_ITEM()
RATIONAL_B_SPLINE_SURFACE(((1.00023530983298,0.922925743796149,1.00168574728335),
(1.00015136166125,0.950422439594211,1.00108434699062),(1.00033574337397,
0.890029368953936,1.00240524789553),(1.00054260094219,0.822274473168305,
1.00388716464866)))
REPRESENTATION_ITEM('')
SURFACE()
);
#3513=(
BOUNDED_SURFACE()
B_SPLINE_SURFACE(3,2,((#429945,#429946,#429947),(#429948,#429949,#429950),
(#429951,#429952,#429953),(#429954,#429955,#429956)),.UNSPECIFIED.,.F.,
 .F.,.F.)
B_SPLINE_SURFACE_WITH_KNOTS((4,4),(3,3),(2.16840434497101E-19,0.000101260117256738),
(0.,1.),.UNSPECIFIED.)
GEOMETRIC_REPRESENTATION_ITEM()
RATIONAL_B_SPLINE_SURFACE(((1.,0.796615278835173,1.),(1.,0.795896038055934,
1.),(1.,0.795193354661359,1.),(1.,0.794506193185544,1.)))
REPRESENTATION_ITEM('')
SURFACE()
);
#3514=(
BOUNDED_SURFACE()
B_SPLINE_SURFACE(3,2,((#429994,#429995,#429996),(#429997,#429998,#429999),
(#430000,#430001,#430002),(#430003,#430004,#430005),(#430006,#430007,#430008),
(#430009,#430010,#430011)),.UNSPECIFIED.,.F.,.F.,.F.)
B_SPLINE_SURFACE_WITH_KNOTS((4,2,4),(3,3),(6.09863722023096E-20,1.66936432462294E-5,
3.33872864924587E-5),(0.,1.),.UNSPECIFIED.)
GEOMETRIC_REPRESENTATION_ITEM()
RATIONAL_B_SPLINE_SURFACE(((1.,0.796615278835173,1.),(1.,0.862310524418131,
1.),(1.,0.92377447201052,1.),(1.,0.923983993203426,1.),(1.,0.862574873720942,
1.),(1.,0.796615278835181,1.)))
REPRESENTATION_ITEM('')
SURFACE()
);
#3515=(
BOUNDED_SURFACE()
B_SPLINE_SURFACE(3,2,((#430048,#430049,#430050),(#430051,#430052,#430053),
(#430054,#430055,#430056),(#430057,#430058,#430059)),.UNSPECIFIED.,.F.,
 .F.,.F.)
B_SPLINE_SURFACE_WITH_KNOTS((4,4),(3,3),(0.,0.000101244905251112),(0.,1.),
 .UNSPECIFIED.)
GEOMETRIC_REPRESENTATION_ITEM()
RATIONAL_B_SPLINE_SURFACE(((1.,0.796615278835172,1.),(1.,0.795896146109788,
1.),(1.,0.795193565796502,1.),(1.,0.794506502889901,1.)))
REPRESENTATION_ITEM('')
SURFACE()
);
#3516=(
BOUNDED_SURFACE()
B_SPLINE_SURFACE(3,2,((#430095,#430096,#430097),(#430098,#430099,#430100),
(#430101,#430102,#430103),(#430104,#430105,#430106)),.UNSPECIFIED.,.F.,
 .F.,.F.)
B_SPLINE_SURFACE_WITH_KNOTS((4,4),(3,3),(2.85968127239939E-5,9.24681548475816E-5),
(-0.00167900678720424,1.01130827127828),.UNSPECIFIED.)
GEOMETRIC_REPRESENTATION_ITEM()
RATIONAL_B_SPLINE_SURFACE(((1.0005904089524,0.822187541868145,1.00401468696659),
(1.00036527718154,0.889990093671497,1.00248382673392),(1.0001646951502,
0.950399042257892,1.00111990082511),(1.00025604274003,0.922888044286026,
1.00174104990632)))
REPRESENTATION_ITEM('')
SURFACE()
);
#3517=(
BOUNDED_SURFACE()
B_SPLINE_SURFACE(3,2,((#430110,#430111,#430112),(#430113,#430114,#430115),
(#430116,#430117,#430118),(#430119,#430120,#430121)),.UNSPECIFIED.,.F.,
 .F.,.F.)
B_SPLINE_SURFACE_WITH_KNOTS((4,4),(3,3),(-5.22358356749324E-6,5.74594192424276E-5),
(-0.00127120052082716,1.),.UNSPECIFIED.)
GEOMETRIC_REPRESENTATION_ITEM()
RATIONAL_B_SPLINE_SURFACE(((1.00054449313187,0.785835073638711,1.),(1.00047707767485,
0.812351526358801,1.),(1.00044031788596,0.826810216506234,1.),(1.00044777653328,
0.823876514387217,1.)))
REPRESENTATION_ITEM('')
SURFACE()
);
#3518=(
BOUNDED_SURFACE()
B_SPLINE_SURFACE(3,2,((#430123,#430124,#430125),(#430126,#430127,#430128),
(#430129,#430130,#430131),(#430132,#430133,#430134)),.UNSPECIFIED.,.F.,
 .F.,.F.)
B_SPLINE_SURFACE_WITH_KNOTS((4,4),(3,3),(-5.42101086242752E-20,4.88747512969881E-5),
(-0.000215805215198065,1.),.UNSPECIFIED.)
GEOMETRIC_REPRESENTATION_ITEM()
RATIONAL_B_SPLINE_SURFACE(((1.00008915600326,0.793434085499804,1.),(1.00008930224979,
0.793095246303347,1.),(1.00008944684601,0.792760230720621,1.),(1.00008958984381,
0.792428918540653,1.)))
REPRESENTATION_ITEM('')
SURFACE()
);
#3519=(
BOUNDED_SURFACE()
B_SPLINE_SURFACE(3,2,((#430136,#430137,#430138),(#430139,#430140,#430141),
(#430142,#430143,#430144),(#430145,#430146,#430147),(#430148,#430149,#430150),
(#430151,#430152,#430153)),.UNSPECIFIED.,.F.,.F.,.F.)
B_SPLINE_SURFACE_WITH_KNOTS((4,2,4),(3,3),(1.42301535138722E-19,7.62675010863197E-5,
0.000152535002172639),(0.,1.02152348203077),.UNSPECIFIED.)
GEOMETRIC_REPRESENTATION_ITEM()
RATIONAL_B_SPLINE_SURFACE(((1.,0.78903359540123,1.00908146323696),(1.,0.857071781054831,
1.00615262590431),(1.,0.922087264710718,1.00335390671593),(1.,0.922394466502371,
1.00334068261145),(1.,0.857224384599045,1.00614605678503),(1.,0.789033595401625,
1.00908146323694)))
REPRESENTATION_ITEM('')
SURFACE()
);
#3520=(
BOUNDED_SURFACE()
B_SPLINE_SURFACE(3,2,((#430155,#430156,#430157),(#430158,#430159,#430160),
(#430161,#430162,#430163),(#430164,#430165,#430166)),.UNSPECIFIED.,.F.,
 .F.,.F.)
B_SPLINE_SURFACE_WITH_KNOTS((4,4),(3,3),(3.79470760369927E-19,4.88747512969884E-5),
(-0.000215489856982675,1.),.UNSPECIFIED.)
GEOMETRIC_REPRESENTATION_ITEM()
RATIONAL_B_SPLINE_SURFACE(((1.00008945889711,0.792428983985755,1.),(1.00008931610833,
0.792760296061309,1.),(1.00008917172345,0.793095311538362,1.),(1.00008902569068,
0.793434150628006,1.)))
REPRESENTATION_ITEM('')
SURFACE()
);
#3521=(
BOUNDED_SURFACE()
B_SPLINE_SURFACE(3,2,((#430168,#430169,#430170),(#430171,#430172,#430173),
(#430174,#430175,#430176),(#430177,#430178,#430179)),.UNSPECIFIED.,.F.,
 .F.,.F.)
B_SPLINE_SURFACE_WITH_KNOTS((4,4),(3,3),(-5.21974905013088E-6,5.74172395514398E-5),
(-0.00139822857777732,1.00051312364092),.UNSPECIFIED.)
GEOMETRIC_REPRESENTATION_ITEM()
RATIONAL_B_SPLINE_SURFACE(((1.00049256947258,0.823768952243931,1.00018060397858),
(1.00048448215728,0.826662424388213,1.00017763870891),(1.00052427784037,
0.812424361909292,1.0001922300693),(1.00059912365872,0.785646094632641,
1.00021967280242)))
REPRESENTATION_ITEM('')
SURFACE()
);
#3522=(
BOUNDED_SURFACE()
B_SPLINE_SURFACE(3,2,((#430183,#430184,#430185),(#430186,#430187,#430188),
(#430189,#430190,#430191),(#430192,#430193,#430194)),.UNSPECIFIED.,.F.,
 .F.,.F.)
B_SPLINE_SURFACE_WITH_KNOTS((4,4),(3,3),(3.2298077433778E-5,9.63764854872248E-5),
(-0.00154325936368034,1.01095292447542),.UNSPECIFIED.)
GEOMETRIC_REPRESENTATION_ITEM()
RATIONAL_B_SPLINE_SURFACE(((1.00023530983298,0.922925743796171,1.00168574728331),
(1.00015136166125,0.950422439594218,1.0010843469906),(1.00033574337397,
0.89002936895396,1.00240524789547),(1.00054260094219,0.822274473168348,
1.00388716464858)))
REPRESENTATION_ITEM('')
SURFACE()
);
#3523=(
BOUNDED_SURFACE()
B_SPLINE_SURFACE(3,2,((#430294,#430295,#430296),(#430297,#430298,#430299),
(#430300,#430301,#430302),(#430303,#430304,#430305)),.UNSPECIFIED.,.F.,
 .F.,.F.)
B_SPLINE_SURFACE_WITH_KNOTS((4,4),(3,3),(2.16840434497101E-19,0.000101260117256738),
(0.,1.),.UNSPECIFIED.)
GEOMETRIC_REPRESENTATION_ITEM()
RATIONAL_B_SPLINE_SURFACE(((1.,0.79661527883517,1.),(1.,0.795896038055942,
1.),(1.,0.79519335466135,1.),(1.,0.794506193185549,1.)))
REPRESENTATION_ITEM('')
SURFACE()
);
#3524=(
BOUNDED_SURFACE()
B_SPLINE_SURFACE(3,2,((#430343,#430344,#430345),(#430346,#430347,#430348),
(#430349,#430350,#430351),(#430352,#430353,#430354),(#430355,#430356,#430357),
(#430358,#430359,#430360)),.UNSPECIFIED.,.F.,.F.,.F.)
B_SPLINE_SURFACE_WITH_KNOTS((4,2,4),(3,3),(4.57397791517322E-20,1.66936432462298E-5,
3.33872864924596E-5),(0.,1.),.UNSPECIFIED.)
GEOMETRIC_REPRESENTATION_ITEM()
RATIONAL_B_SPLINE_SURFACE(((1.,0.796615278835178,1.),(1.,0.862310524418128,
1.),(1.,0.923774472010521,1.),(1.,0.923983993203423,1.),(1.,0.862574873720944,
1.),(1.,0.796615278835188,1.)))
REPRESENTATION_ITEM('')
SURFACE()
);
#3525=(
BOUNDED_SURFACE()
B_SPLINE_SURFACE(3,2,((#430397,#430398,#430399),(#430400,#430401,#430402),
(#430403,#430404,#430405),(#430406,#430407,#430408)),.UNSPECIFIED.,.F.,
 .F.,.F.)
B_SPLINE_SURFACE_WITH_KNOTS((4,4),(3,3),(0.,0.000101244905251112),(0.,1.),
 .UNSPECIFIED.)
GEOMETRIC_REPRESENTATION_ITEM()
RATIONAL_B_SPLINE_SURFACE(((1.,0.796615278835173,1.),(1.,0.795896146109794,
1.),(1.,0.795193565796502,1.),(1.,0.794506502889902,1.)))
REPRESENTATION_ITEM('')
SURFACE()
);
#3526=(
BOUNDED_SURFACE()
B_SPLINE_SURFACE(3,2,((#430444,#430445,#430446),(#430447,#430448,#430449),
(#430450,#430451,#430452),(#430453,#430454,#430455)),.UNSPECIFIED.,.F.,
 .F.,.F.)
B_SPLINE_SURFACE_WITH_KNOTS((4,4),(3,3),(2.85968127239939E-5,9.24681548475819E-5),
(-0.00167900678745074,1.01130827127827),.UNSPECIFIED.)
GEOMETRIC_REPRESENTATION_ITEM()
RATIONAL_B_SPLINE_SURFACE(((1.00059040895249,0.822187541868105,1.00401468696658),
(1.00036527718159,0.889990093671465,1.00248382673392),(1.00016469515022,
0.950399042257882,1.00111990082511),(1.00025604274006,0.922888044286007,
1.00174104990632)))
REPRESENTATION_ITEM('')
SURFACE()
);
#3527=(
BOUNDED_SURFACE()
B_SPLINE_SURFACE(3,2,((#430459,#430460,#430461),(#430462,#430463,#430464),
(#430465,#430466,#430467),(#430468,#430469,#430470)),.UNSPECIFIED.,.F.,
 .F.,.F.)
B_SPLINE_SURFACE_WITH_KNOTS((4,4),(3,3),(-5.22358356749293E-6,5.74594192424277E-5),
(-0.00127120052034674,1.),.UNSPECIFIED.)
GEOMETRIC_REPRESENTATION_ITEM()
RATIONAL_B_SPLINE_SURFACE(((1.00054449313166,0.785835073638813,1.),(1.00047707767467,
0.812351526358894,1.),(1.00044031788579,0.826810216506316,1.),(1.00044777653311,
0.823876514387298,1.)))
REPRESENTATION_ITEM('')
SURFACE()
);
#3528=(
BOUNDED_SURFACE()
B_SPLINE_SURFACE(3,2,((#430472,#430473,#430474),(#430475,#430476,#430477),
(#430478,#430479,#430480),(#430481,#430482,#430483)),.UNSPECIFIED.,.F.,
 .F.,.F.)
B_SPLINE_SURFACE_WITH_KNOTS((4,4),(3,3),(1.62630325872826E-19,4.88747512969885E-5),
(-0.000215805215935403,1.),.UNSPECIFIED.)
GEOMETRIC_REPRESENTATION_ITEM()
RATIONAL_B_SPLINE_SURFACE(((1.00008915600357,0.79343408549965,1.),(1.0000893022501,
0.793095246303188,1.),(1.00008944684632,0.792760230720469,1.),(1.00008958984411,
0.792428918540496,1.)))
REPRESENTATION_ITEM('')
SURFACE()
);
#3529=(
BOUNDED_SURFACE()
B_SPLINE_SURFACE(3,2,((#430485,#430486,#430487),(#430488,#430489,#430490),
(#430491,#430492,#430493),(#430494,#430495,#430496),(#430497,#430498,#430499),
(#430500,#430501,#430502)),.UNSPECIFIED.,.F.,.F.,.F.)
B_SPLINE_SURFACE_WITH_KNOTS((4,2,4),(3,3),(1.76182853028894E-19,7.62675010863199E-5,
0.00015253500217264),(0.,1.0215234820306),.UNSPECIFIED.)
GEOMETRIC_REPRESENTATION_ITEM()
RATIONAL_B_SPLINE_SURFACE(((1.,0.789033595401265,1.00908146323688),(1.,
0.857071781054835,1.00615262590426),(1.,0.922087264710755,1.00335390671591),
(1.,0.922394466502361,1.00334068261142),(1.,0.857224384599075,1.00614605678498),
(1.,0.789033595401665,1.00908146323687)))
REPRESENTATION_ITEM('')
SURFACE()
);
#3530=(
BOUNDED_SURFACE()
B_SPLINE_SURFACE(3,2,((#430504,#430505,#430506),(#430507,#430508,#430509),
(#430510,#430511,#430512),(#430513,#430514,#430515)),.UNSPECIFIED.,.F.,
 .F.,.F.)
B_SPLINE_SURFACE_WITH_KNOTS((4,4),(3,3),(5.42101086242752E-20,4.88747512969881E-5),
(-0.000215489856972442,1.),.UNSPECIFIED.)
GEOMETRIC_REPRESENTATION_ITEM()
RATIONAL_B_SPLINE_SURFACE(((1.0000894588971,0.79242898398576,1.),(1.00008931610832,
0.792760296061302,1.),(1.00008917172345,0.793095311538378,1.),(1.00008902569067,
0.793434150628008,1.)))
REPRESENTATION_ITEM('')
SURFACE()
);
#3531=(
BOUNDED_SURFACE()
B_SPLINE_SURFACE(3,2,((#430517,#430518,#430519),(#430520,#430521,#430522),
(#430523,#430524,#430525),(#430526,#430527,#430528)),.UNSPECIFIED.,.F.,
 .F.,.F.)
B_SPLINE_SURFACE_WITH_KNOTS((4,4),(3,3),(-5.21974905013088E-6,5.74172395514395E-5),
(-0.00139822857773102,1.00051312364041),.UNSPECIFIED.)
GEOMETRIC_REPRESENTATION_ITEM()
RATIONAL_B_SPLINE_SURFACE(((1.00049256947256,0.823768952244029,1.0001806039784),
(1.00048448215727,0.826662424388317,1.00017763870873),(1.00052427784035,
0.812424361909394,1.00019223006911),(1.0005991236587,0.785646094632765,
1.0002196728022)))
REPRESENTATION_ITEM('')
SURFACE()
);
#3532=(
BOUNDED_SURFACE()
B_SPLINE_SURFACE(3,2,((#430532,#430533,#430534),(#430535,#430536,#430537),
(#430538,#430539,#430540),(#430541,#430542,#430543)),.UNSPECIFIED.,.F.,
 .F.,.F.)
B_SPLINE_SURFACE_WITH_KNOTS((4,4),(3,3),(3.22980774337783E-5,9.63764854872258E-5),
(-0.0015432593640314,1.01095292447538),.UNSPECIFIED.)
GEOMETRIC_REPRESENTATION_ITEM()
RATIONAL_B_SPLINE_SURFACE(((1.00023530983303,0.922925743796145,1.0016857472833),
(1.00015136166129,0.950422439594196,1.00108434699059),(1.00033574337405,
0.890029368953932,1.00240524789547),(1.00054260094232,0.822274473168291,
1.00388716464856)))
REPRESENTATION_ITEM('')
SURFACE()
);
#3533=(
BOUNDED_SURFACE()
B_SPLINE_SURFACE(3,2,((#430643,#430644,#430645),(#430646,#430647,#430648),
(#430649,#430650,#430651),(#430652,#430653,#430654)),.UNSPECIFIED.,.F.,
 .F.,.F.)
B_SPLINE_SURFACE_WITH_KNOTS((4,4),(3,3),(-2.16840434497101E-19,0.000101260117256738),
(0.,1.),.UNSPECIFIED.)
GEOMETRIC_REPRESENTATION_ITEM()
RATIONAL_B_SPLINE_SURFACE(((1.,0.796615278835167,1.),(1.,0.795896038055943,
1.),(1.,0.795193354661347,1.),(1.,0.794506193185542,1.)))
REPRESENTATION_ITEM('')
SURFACE()
);
#3534=(
BOUNDED_SURFACE()
B_SPLINE_SURFACE(3,2,((#430692,#430693,#430694),(#430695,#430696,#430697),
(#430698,#430699,#430700),(#430701,#430702,#430703),(#430704,#430705,#430706),
(#430707,#430708,#430709)),.UNSPECIFIED.,.F.,.F.,.F.)
B_SPLINE_SURFACE_WITH_KNOTS((4,2,4),(3,3),(5.0821976835258E-20,1.66936432462293E-5,
3.33872864924586E-5),(0.,1.),.UNSPECIFIED.)
GEOMETRIC_REPRESENTATION_ITEM()
RATIONAL_B_SPLINE_SURFACE(((1.,0.796615278835176,1.),(1.,0.86231052441813,
1.),(1.,0.923774472010521,1.),(1.,0.923983993203425,1.),(1.,0.86257487372094,
1.),(1.,0.796615278835182,1.)))
REPRESENTATION_ITEM('')
SURFACE()
);
#3535=(
BOUNDED_SURFACE()
B_SPLINE_SURFACE(3,2,((#430746,#430747,#430748),(#430749,#430750,#430751),
(#430752,#430753,#430754),(#430755,#430756,#430757)),.UNSPECIFIED.,.F.,
 .F.,.F.)
B_SPLINE_SURFACE_WITH_KNOTS((4,4),(3,3),(-2.16840434497101E-19,0.000101244905251112),
(0.,1.),.UNSPECIFIED.)
GEOMETRIC_REPRESENTATION_ITEM()
RATIONAL_B_SPLINE_SURFACE(((1.,0.796615278835169,1.),(1.,0.795896146109793,
1.),(1.,0.7951935657965,1.),(1.,0.794506502889899,1.)))
REPRESENTATION_ITEM('')
SURFACE()
);
#3536=(
BOUNDED_SURFACE()
B_SPLINE_SURFACE(3,2,((#430793,#430794,#430795),(#430796,#430797,#430798),
(#430799,#430800,#430801),(#430802,#430803,#430804)),.UNSPECIFIED.,.F.,
 .F.,.F.)
B_SPLINE_SURFACE_WITH_KNOTS((4,4),(3,3),(2.85968127239939E-5,9.24681548475816E-5),
(-0.00167900678819889,1.01130827127833),.UNSPECIFIED.)
GEOMETRIC_REPRESENTATION_ITEM()
RATIONAL_B_SPLINE_SURFACE(((1.00059040895275,0.822187541867959,1.00401468696661),
(1.00036527718176,0.889990093671379,1.00248382673393),(1.00016469515029,
0.950399042257845,1.00111990082512),(1.00025604274018,0.922888044285941,
1.00174104990633)))
REPRESENTATION_ITEM('')
SURFACE()
);
#3537=(
BOUNDED_SURFACE()
B_SPLINE_SURFACE(3,2,((#430808,#430809,#430810),(#430811,#430812,#430813),
(#430814,#430815,#430816),(#430817,#430818,#430819)),.UNSPECIFIED.,.F.,
 .F.,.F.)
B_SPLINE_SURFACE_WITH_KNOTS((4,4),(3,3),(-5.22358356749291E-6,5.74594192424256E-5),
(-0.00127120052061498,1.),.UNSPECIFIED.)
GEOMETRIC_REPRESENTATION_ITEM()
RATIONAL_B_SPLINE_SURFACE(((1.00054449313178,0.785835073638749,1.),(1.00047707767477,
0.812351526358845,1.),(1.00044031788588,0.826810216506264,1.),(1.00044777653321,
0.823876514387246,1.)))
REPRESENTATION_ITEM('')
SURFACE()
);
#3538=(
BOUNDED_SURFACE()
B_SPLINE_SURFACE(3,2,((#430821,#430822,#430823),(#430824,#430825,#430826),
(#430827,#430828,#430829),(#430830,#430831,#430832)),.UNSPECIFIED.,.F.,
 .F.,.F.)
B_SPLINE_SURFACE_WITH_KNOTS((4,4),(3,3),(-1.0842021724855E-19,4.88747512969882E-5),
(-0.000215805215860785,1.),.UNSPECIFIED.)
GEOMETRIC_REPRESENTATION_ITEM()
RATIONAL_B_SPLINE_SURFACE(((1.00008915600354,0.793434085499667,1.),(1.00008930225007,
0.793095246303216,1.),(1.00008944684629,0.792760230720475,1.),(1.00008958984408,
0.792428918540514,1.)))
REPRESENTATION_ITEM('')
SURFACE()
);
#3539=(
BOUNDED_SURFACE()
B_SPLINE_SURFACE(3,2,((#430834,#430835,#430836),(#430837,#430838,#430839),
(#430840,#430841,#430842),(#430843,#430844,#430845),(#430846,#430847,#430848),
(#430849,#430850,#430851)),.UNSPECIFIED.,.F.,.F.,.F.)
B_SPLINE_SURFACE_WITH_KNOTS((4,2,4),(3,3),(2.98155597433514E-19,7.62675010863196E-5,
0.000152535002172639),(0.,1.02152348203071),.UNSPECIFIED.)
GEOMETRIC_REPRESENTATION_ITEM()
RATIONAL_B_SPLINE_SURFACE(((1.,0.789033595401246,1.00908146323693),(1.,
0.857071781054844,1.00615262590429),(1.,0.922087264710711,1.00335390671592),
(1.,0.922394466502387,1.00334068261144),(1.,0.857224384599034,1.00614605678501),
(1.,0.789033595401642,1.00908146323691)))
REPRESENTATION_ITEM('')
SURFACE()
);
#3540=(
BOUNDED_SURFACE()
B_SPLINE_SURFACE(3,2,((#430853,#430854,#430855),(#430856,#430857,#430858),
(#430859,#430860,#430861),(#430862,#430863,#430864)),.UNSPECIFIED.,.F.,
 .F.,.F.)
B_SPLINE_SURFACE_WITH_KNOTS((4,4),(3,3),(-1.62630325872826E-19,4.88747512969882E-5),
(-0.000215489857814701,1.),.UNSPECIFIED.)
GEOMETRIC_REPRESENTATION_ITEM()
RATIONAL_B_SPLINE_SURFACE(((1.00008945889745,0.792428983985584,1.),(1.00008931610867,
0.79276029606113,1.),(1.0000891717238,0.793095311538205,1.),(1.00008902569102,
0.793434150627835,1.)))
REPRESENTATION_ITEM('')
SURFACE()
);
#3541=(
BOUNDED_SURFACE()
B_SPLINE_SURFACE(3,2,((#430866,#430867,#430868),(#430869,#430870,#430871),
(#430872,#430873,#430874),(#430875,#430876,#430877)),.UNSPECIFIED.,.F.,
 .F.,.F.)
B_SPLINE_SURFACE_WITH_KNOTS((4,4),(3,3),(-5.21974905013086E-6,5.74172395514373E-5),
(-0.00139822857748534,1.00051312364066),.UNSPECIFIED.)
GEOMETRIC_REPRESENTATION_ITEM()
RATIONAL_B_SPLINE_SURFACE(((1.00049256947248,0.823768952244017,1.00018060397849),
(1.00048448215718,0.826662424388332,1.00017763870882),(1.00052427784026,
0.812424361909375,1.00019223006921),(1.0005991236586,0.785646094632768,
1.00021967280231)))
REPRESENTATION_ITEM('')
SURFACE()
);
#3542=(
BOUNDED_SURFACE()
B_SPLINE_SURFACE(3,2,((#430881,#430882,#430883),(#430884,#430885,#430886),
(#430887,#430888,#430889),(#430890,#430891,#430892)),.UNSPECIFIED.,.F.,
 .F.,.F.)
B_SPLINE_SURFACE_WITH_KNOTS((4,4),(3,3),(3.22980774337778E-5,9.63764854872259E-5),
(-0.0015432593635687,1.01095292447554),.UNSPECIFIED.)
GEOMETRIC_REPRESENTATION_ITEM()
RATIONAL_B_SPLINE_SURFACE(((1.00023530983296,0.922925743796169,1.00168574728333),
(1.00015136166124,0.950422439594234,1.00108434699061),(1.00033574337395,
0.890029368953954,1.0024052478955),(1.00054260094215,0.822274473168349,
1.00388716464862)))
REPRESENTATION_ITEM('')
SURFACE()
);
#3543=(
BOUNDED_SURFACE()
B_SPLINE_SURFACE(3,2,((#430992,#430993,#430994),(#430995,#430996,#430997),
(#430998,#430999,#431000),(#431001,#431002,#431003)),.UNSPECIFIED.,.F.,
 .F.,.F.)
B_SPLINE_SURFACE_WITH_KNOTS((4,4),(3,3),(-2.16840434497101E-19,0.000101260117256738),
(0.,1.),.UNSPECIFIED.)
GEOMETRIC_REPRESENTATION_ITEM()
RATIONAL_B_SPLINE_SURFACE(((1.,0.796615278835174,1.),(1.,0.79589603805594,
1.),(1.,0.795193354661341,1.),(1.,0.794506193185547,1.)))
REPRESENTATION_ITEM('')
SURFACE()
);
#3544=(
BOUNDED_SURFACE()
B_SPLINE_SURFACE(3,2,((#431041,#431042,#431043),(#431044,#431045,#431046),
(#431047,#431048,#431049),(#431050,#431051,#431052),(#431053,#431054,#431055),
(#431056,#431057,#431058)),.UNSPECIFIED.,.F.,.F.,.F.)
B_SPLINE_SURFACE_WITH_KNOTS((4,2,4),(3,3),(6.7762635780344E-21,1.66936432462294E-5,
3.33872864924587E-5),(0.,1.),.UNSPECIFIED.)
GEOMETRIC_REPRESENTATION_ITEM()
RATIONAL_B_SPLINE_SURFACE(((1.,0.796615278835177,1.),(1.,0.862310524418125,
1.),(1.,0.923774472010521,1.),(1.,0.923983993203427,1.),(1.,0.86257487372095,
1.),(1.,0.796615278835183,1.)))
REPRESENTATION_ITEM('')
SURFACE()
);
#3545=(
BOUNDED_SURFACE()
B_SPLINE_SURFACE(3,2,((#431095,#431096,#431097),(#431098,#431099,#431100),
(#431101,#431102,#431103),(#431104,#431105,#431106)),.UNSPECIFIED.,.F.,
 .F.,.F.)
B_SPLINE_SURFACE_WITH_KNOTS((4,4),(3,3),(0.,0.000101244905251112),(0.,1.),
 .UNSPECIFIED.)
GEOMETRIC_REPRESENTATION_ITEM()
RATIONAL_B_SPLINE_SURFACE(((1.,0.79661527883517,1.),(1.,0.795896146109795,
1.),(1.,0.795193565796502,1.),(1.,0.794506502889901,1.)))
REPRESENTATION_ITEM('')
SURFACE()
);
#3546=(
BOUNDED_SURFACE()
B_SPLINE_SURFACE(3,2,((#431142,#431143,#431144),(#431145,#431146,#431147),
(#431148,#431149,#431150),(#431151,#431152,#431153)),.UNSPECIFIED.,.F.,
 .F.,.F.)
B_SPLINE_SURFACE_WITH_KNOTS((4,4),(3,3),(2.85968127239939E-5,9.24681548475818E-5),
(-0.00167900678659478,1.01130827127828),.UNSPECIFIED.)
GEOMETRIC_REPRESENTATION_ITEM()
RATIONAL_B_SPLINE_SURFACE(((1.00059040895219,0.822187541868253,1.00401468696659),
(1.00036527718141,0.88999009367156,1.00248382673392),(1.00016469515014,
0.95039904225793,1.00111990082511),(1.00025604273993,0.92288804428607,1.00174104990632)))
REPRESENTATION_ITEM('')
SURFACE()
);
#3547=(
BOUNDED_SURFACE()
B_SPLINE_SURFACE(3,2,((#431157,#431158,#431159),(#431160,#431161,#431162),
(#431163,#431164,#431165),(#431166,#431167,#431168)),.UNSPECIFIED.,.F.,
 .F.,.F.)
B_SPLINE_SURFACE_WITH_KNOTS((4,4),(3,3),(-5.22358356749329E-6,5.74594192424274E-5),
(-0.00127120052065071,1.),.UNSPECIFIED.)
GEOMETRIC_REPRESENTATION_ITEM()
RATIONAL_B_SPLINE_SURFACE(((1.00054449313179,0.785835073638744,1.),(1.00047707767478,
0.812351526358829,1.),(1.0004403178859,0.826810216506268,1.),(1.00044777653322,
0.823876514387243,1.)))
REPRESENTATION_ITEM('')
SURFACE()
);
#3548=(
BOUNDED_SURFACE()
B_SPLINE_SURFACE(3,2,((#431170,#431171,#431172),(#431173,#431174,#431175),
(#431176,#431177,#431178),(#431179,#431180,#431181)),.UNSPECIFIED.,.F.,
 .F.,.F.)
B_SPLINE_SURFACE_WITH_KNOTS((4,4),(3,3),(-4.33680868994202E-19,4.88747512969879E-5),
(-0.000215805215015582,1.),.UNSPECIFIED.)
GEOMETRIC_REPRESENTATION_ITEM()
RATIONAL_B_SPLINE_SURFACE(((1.00008915600319,0.793434085499841,1.),(1.00008930224972,
0.793095246303392,1.),(1.00008944684594,0.792760230720655,1.),(1.00008958984373,
0.79242891854069,1.)))
REPRESENTATION_ITEM('')
SURFACE()
);
#3549=(
BOUNDED_SURFACE()
B_SPLINE_SURFACE(3,2,((#431183,#431184,#431185),(#431186,#431187,#431188),
(#431189,#431190,#431191),(#431192,#431193,#431194),(#431195,#431196,#431197),
(#431198,#431199,#431200)),.UNSPECIFIED.,.F.,.F.,.F.)
B_SPLINE_SURFACE_WITH_KNOTS((4,2,4),(3,3),(2.91379333855479E-19,7.62675010863198E-5,
0.000152535002172639),(0.,1.02152348203076),.UNSPECIFIED.)
GEOMETRIC_REPRESENTATION_ITEM()
RATIONAL_B_SPLINE_SURFACE(((1.,0.789033595401233,1.00908146323695),(1.,
0.857071781054827,1.00615262590431),(1.,0.922087264710726,1.00335390671593),
(1.,0.922394466502363,1.00334068261145),(1.,0.857224384599045,1.00614605678503),
(1.,0.789033595401634,1.00908146323693)))
REPRESENTATION_ITEM('')
SURFACE()
);
#3550=(
BOUNDED_SURFACE()
B_SPLINE_SURFACE(3,2,((#431202,#431203,#431204),(#431205,#431206,#431207),
(#431208,#431209,#431210),(#431211,#431212,#431213)),.UNSPECIFIED.,.F.,
 .F.,.F.)
B_SPLINE_SURFACE_WITH_KNOTS((4,4),(3,3),(3.79470760369927E-19,4.88747512969882E-5),
(-0.000215489857114363,1.),.UNSPECIFIED.)
GEOMETRIC_REPRESENTATION_ITEM()
RATIONAL_B_SPLINE_SURFACE(((1.00008945889716,0.792428983985731,1.),(1.00008931610838,
0.792760296061279,1.),(1.00008917172351,0.793095311538343,1.),(1.00008902569073,
0.793434150627979,1.)))
REPRESENTATION_ITEM('')
SURFACE()
);
#3551=(
BOUNDED_SURFACE()
B_SPLINE_SURFACE(3,2,((#431215,#431216,#431217),(#431218,#431219,#431220),
(#431221,#431222,#431223),(#431224,#431225,#431226)),.UNSPECIFIED.,.F.,
 .F.,.F.)
B_SPLINE_SURFACE_WITH_KNOTS((4,4),(3,3),(-5.21974905013091E-6,5.741723955144E-5),
(-0.0013982285778192,1.0005131236406),.UNSPECIFIED.)
GEOMETRIC_REPRESENTATION_ITEM()
RATIONAL_B_SPLINE_SURFACE(((1.00049256947259,0.823768952243977,1.00018060397847),
(1.0004844821573,0.826662424388274,1.0001776387088),(1.00052427784038,0.812424361909338,
1.00019223006919),(1.00059912365874,0.785646094632704,1.00021967280228)))
REPRESENTATION_ITEM('')
SURFACE()
);
#3552=(
BOUNDED_SURFACE()
B_SPLINE_SURFACE(3,2,((#431230,#431231,#431232),(#431233,#431234,#431235),
(#431236,#431237,#431238),(#431239,#431240,#431241)),.UNSPECIFIED.,.F.,
 .F.,.F.)
B_SPLINE_SURFACE_WITH_KNOTS((4,4),(3,3),(3.22980774337778E-5,9.63764854872254E-5),
(-0.00154325936345388,1.01095292447556),.UNSPECIFIED.)
GEOMETRIC_REPRESENTATION_ITEM()
RATIONAL_B_SPLINE_SURFACE(((1.00023530983295,0.922925743796177,1.00168574728333),
(1.00015136166123,0.95042243959423,1.00108434699061),(1.00033574337392,
0.890029368953974,1.00240524789551),(1.00054260094211,0.82227447316836,
1.00388716464863)))
REPRESENTATION_ITEM('')
SURFACE()
);
#3553=(
BOUNDED_SURFACE()
B_SPLINE_SURFACE(3,2,((#431341,#431342,#431343),(#431344,#431345,#431346),
(#431347,#431348,#431349),(#431350,#431351,#431352)),.UNSPECIFIED.,.F.,
 .F.,.F.)
B_SPLINE_SURFACE_WITH_KNOTS((4,4),(3,3),(2.16840434497101E-19,0.000101260117256738),
(0.,1.),.UNSPECIFIED.)
GEOMETRIC_REPRESENTATION_ITEM()
RATIONAL_B_SPLINE_SURFACE(((1.,0.79661527883517,1.),(1.,0.79589603805594,
1.),(1.,0.795193354661347,1.),(1.,0.794506193185546,1.)))
REPRESENTATION_ITEM('')
SURFACE()
);
#3554=(
BOUNDED_SURFACE()
B_SPLINE_SURFACE(3,2,((#431390,#431391,#431392),(#431393,#431394,#431395),
(#431396,#431397,#431398),(#431399,#431400,#431401),(#431402,#431403,#431404),
(#431405,#431406,#431407)),.UNSPECIFIED.,.F.,.F.,.F.)
B_SPLINE_SURFACE_WITH_KNOTS((4,2,4),(3,3),(8.13151629364128E-20,1.66936432462295E-5,
3.33872864924589E-5),(0.,1.),.UNSPECIFIED.)
GEOMETRIC_REPRESENTATION_ITEM()
RATIONAL_B_SPLINE_SURFACE(((1.,0.796615278835172,1.),(1.,0.862310524418132,
1.),(1.,0.923774472010519,1.),(1.,0.923983993203429,1.),(1.,0.862574873720951,
1.),(1.,0.796615278835181,1.)))
REPRESENTATION_ITEM('')
SURFACE()
);
#3555=(
BOUNDED_SURFACE()
B_SPLINE_SURFACE(3,2,((#431444,#431445,#431446),(#431447,#431448,#431449),
(#431450,#431451,#431452),(#431453,#431454,#431455)),.UNSPECIFIED.,.F.,
 .F.,.F.)
B_SPLINE_SURFACE_WITH_KNOTS((4,4),(3,3),(0.,0.000101244905251112),(0.,1.),
 .UNSPECIFIED.)
GEOMETRIC_REPRESENTATION_ITEM()
RATIONAL_B_SPLINE_SURFACE(((1.,0.796615278835172,1.),(1.,0.795896146109797,
1.),(1.,0.7951935657965,1.),(1.,0.794506502889903,1.)))
REPRESENTATION_ITEM('')
SURFACE()
);
#3556=(
BOUNDED_SURFACE()
B_SPLINE_SURFACE(3,2,((#431491,#431492,#431493),(#431494,#431495,#431496),
(#431497,#431498,#431499),(#431500,#431501,#431502)),.UNSPECIFIED.,.F.,
 .F.,.F.)
B_SPLINE_SURFACE_WITH_KNOTS((4,4),(3,3),(2.85968127239938E-5,9.2468154847582E-5),
(-0.00167900678657004,1.01130827127851),.UNSPECIFIED.)
GEOMETRIC_REPRESENTATION_ITEM()
RATIONAL_B_SPLINE_SURFACE(((1.00059040895218,0.82218754186822,1.00401468696667),
(1.0003652771814,0.889990093671534,1.00248382673397),(1.00016469515013,
0.950399042257918,1.00111990082514),(1.00025604273993,0.922888044286056,
1.00174104990636)))
REPRESENTATION_ITEM('')
SURFACE()
);
#3557=(
BOUNDED_SURFACE()
B_SPLINE_SURFACE(3,2,((#431506,#431507,#431508),(#431509,#431510,#431511),
(#431512,#431513,#431514),(#431515,#431516,#431517)),.UNSPECIFIED.,.F.,
 .F.,.F.)
B_SPLINE_SURFACE_WITH_KNOTS((4,4),(3,3),(-5.22358356749114E-6,5.74594192424275E-5),
(-0.00127120052069131,1.),.UNSPECIFIED.)
GEOMETRIC_REPRESENTATION_ITEM()
RATIONAL_B_SPLINE_SURFACE(((1.00054449313181,0.78583507363874,1.),(1.0004770776748,
0.812351526358814,1.),(1.00044031788591,0.826810216506269,1.),(1.00044777653323,
0.823876514387229,1.)))
REPRESENTATION_ITEM('')
SURFACE()
);
#3558=(
BOUNDED_SURFACE()
B_SPLINE_SURFACE(3,2,((#431519,#431520,#431521),(#431522,#431523,#431524),
(#431525,#431526,#431527),(#431528,#431529,#431530)),.UNSPECIFIED.,.F.,
 .F.,.F.)
B_SPLINE_SURFACE_WITH_KNOTS((4,4),(3,3),(-2.71050543121376E-19,4.8874751296988E-5),
(-0.000215805215089049,1.),.UNSPECIFIED.)
GEOMETRIC_REPRESENTATION_ITEM()
RATIONAL_B_SPLINE_SURFACE(((1.00008915600322,0.793434085499826,1.),(1.00008930224975,
0.793095246303363,1.),(1.00008944684597,0.792760230720644,1.),(1.00008958984376,
0.792428918540672,1.)))
REPRESENTATION_ITEM('')
SURFACE()
);
#3559=(
BOUNDED_SURFACE()
B_SPLINE_SURFACE(3,2,((#431532,#431533,#431534),(#431535,#431536,#431537),
(#431538,#431539,#431540),(#431541,#431542,#431543),(#431544,#431545,#431546),
(#431547,#431548,#431549)),.UNSPECIFIED.,.F.,.F.,.F.)
B_SPLINE_SURFACE_WITH_KNOTS((4,2,4),(3,3),(1.15196480826585E-19,7.62675010863197E-5,
0.000152535002172639),(0.,1.02152348203072),.UNSPECIFIED.)
GEOMETRIC_REPRESENTATION_ITEM()
RATIONAL_B_SPLINE_SURFACE(((1.,0.789033595401238,1.00908146323694),(1.,
0.857071781054832,1.0061526259043),(1.,0.922087264710732,1.00335390671593),
(1.,0.922394466502364,1.00334068261144),(1.,0.857224384599056,1.00614605678502),
(1.,0.78903359540164,1.00908146323692)))
REPRESENTATION_ITEM('')
SURFACE()
);
#3560=(
BOUNDED_SURFACE()
B_SPLINE_SURFACE(3,2,((#431551,#431552,#431553),(#431554,#431555,#431556),
(#431557,#431558,#431559),(#431560,#431561,#431562)),.UNSPECIFIED.,.F.,
 .F.,.F.)
B_SPLINE_SURFACE_WITH_KNOTS((4,4),(3,3),(-8.13151629364128E-20,4.88747512969881E-5),
(-0.000215489856981559,1.),.UNSPECIFIED.)
GEOMETRIC_REPRESENTATION_ITEM()
RATIONAL_B_SPLINE_SURFACE(((1.00008945889711,0.792428983985759,1.),(1.00008931610833,
0.792760296061303,1.),(1.00008917172345,0.793095311538374,1.),(1.00008902569068,
0.793434150628007,1.)))
REPRESENTATION_ITEM('')
SURFACE()
);
#3561=(
BOUNDED_SURFACE()
B_SPLINE_SURFACE(3,2,((#431564,#431565,#431566),(#431567,#431568,#431569),
(#431570,#431571,#431572),(#431573,#431574,#431575)),.UNSPECIFIED.,.F.,
 .F.,.F.)
B_SPLINE_SURFACE_WITH_KNOTS((4,4),(3,3),(-5.2197490501287E-6,5.74172395514394E-5),
(-0.00139822857797119,1.00051312364064),.UNSPECIFIED.)
GEOMETRIC_REPRESENTATION_ITEM()
RATIONAL_B_SPLINE_SURFACE(((1.00049256947265,0.823768952243948,1.00018060397848),
(1.00048448215735,0.826662424388226,1.00017763870881),(1.00052427784044,
0.812424361909317,1.0001922300692),(1.00059912365881,0.785646094632657,
1.0002196728023)))
REPRESENTATION_ITEM('')
SURFACE()
);
#3562=(
BOUNDED_SURFACE()
B_SPLINE_SURFACE(3,2,((#431579,#431580,#431581),(#431582,#431583,#431584),
(#431585,#431586,#431587),(#431588,#431589,#431590)),.UNSPECIFIED.,.F.,
 .F.,.F.)
B_SPLINE_SURFACE_WITH_KNOTS((4,4),(3,3),(3.22980774337777E-5,9.63764854872246E-5),
(-0.00154325936298721,1.01095292447535),.UNSPECIFIED.)
GEOMETRIC_REPRESENTATION_ITEM()
RATIONAL_B_SPLINE_SURFACE(((1.00023530983287,0.922925743796231,1.0016857472833),
(1.00015136166118,0.95042243959425,1.00108434699059),(1.00033574337382,
0.890029368954052,1.00240524789546),(1.00054260094195,0.822274473168482,
1.00388716464855)))
REPRESENTATION_ITEM('')
SURFACE()
);
#3563=(
BOUNDED_SURFACE()
B_SPLINE_SURFACE(3,2,((#431690,#431691,#431692),(#431693,#431694,#431695),
(#431696,#431697,#431698),(#431699,#431700,#431701)),.UNSPECIFIED.,.F.,
 .F.,.F.)
B_SPLINE_SURFACE_WITH_KNOTS((4,4),(3,3),(2.16840434497101E-19,0.000101260117256738),
(0.,1.),.UNSPECIFIED.)
GEOMETRIC_REPRESENTATION_ITEM()
RATIONAL_B_SPLINE_SURFACE(((1.,0.79661527883517,1.),(1.,0.795896038055944,
1.),(1.,0.795193354661343,1.),(1.,0.794506193185549,1.)))
REPRESENTATION_ITEM('')
SURFACE()
);
#3564=(
BOUNDED_SURFACE()
B_SPLINE_SURFACE(3,2,((#431739,#431740,#431741),(#431742,#431743,#431744),
(#431745,#431746,#431747),(#431748,#431749,#431750),(#431751,#431752,#431753),
(#431754,#431755,#431756)),.UNSPECIFIED.,.F.,.F.,.F.)
B_SPLINE_SURFACE_WITH_KNOTS((4,2,4),(3,3),(6.43745039913268E-20,1.66936432462297E-5,
3.33872864924593E-5),(0.,1.),.UNSPECIFIED.)
GEOMETRIC_REPRESENTATION_ITEM()
RATIONAL_B_SPLINE_SURFACE(((1.,0.796615278835177,1.),(1.,0.862310524418133,
1.),(1.,0.92377447201052,1.),(1.,0.923983993203426,1.),(1.,0.862574873720953,
1.),(1.,0.796615278835183,1.)))
REPRESENTATION_ITEM('')
SURFACE()
);
#3565=(
BOUNDED_SURFACE()
B_SPLINE_SURFACE(3,2,((#431793,#431794,#431795),(#431796,#431797,#431798),
(#431799,#431800,#431801),(#431802,#431803,#431804)),.UNSPECIFIED.,.F.,
 .F.,.F.)
B_SPLINE_SURFACE_WITH_KNOTS((4,4),(3,3),(0.,0.000101244905251112),(0.,1.),
 .UNSPECIFIED.)
GEOMETRIC_REPRESENTATION_ITEM()
RATIONAL_B_SPLINE_SURFACE(((1.,0.796615278835172,1.),(1.,0.795896146109793,
1.),(1.,0.795193565796499,1.),(1.,0.7945065028899,1.)))
REPRESENTATION_ITEM('')
SURFACE()
);
#3566=(
BOUNDED_SURFACE()
B_SPLINE_SURFACE(3,2,((#431840,#431841,#431842),(#431843,#431844,#431845),
(#431846,#431847,#431848),(#431849,#431850,#431851)),.UNSPECIFIED.,.F.,
 .F.,.F.)
B_SPLINE_SURFACE_WITH_KNOTS((4,4),(3,3),(2.85968127239939E-5,9.24681548475818E-5),
(-0.0016790067864143,1.01130827127831),.UNSPECIFIED.)
GEOMETRIC_REPRESENTATION_ITEM()
RATIONAL_B_SPLINE_SURFACE(((1.00059040895212,0.822187541868281,1.0040146869666),
(1.00036527718137,0.889990093671572,1.00248382673393),(1.00016469515012,
0.950399042257936,1.00111990082512),(1.0002560427399,0.922888044286082,
1.00174104990632)))
REPRESENTATION_ITEM('')
SURFACE()
);
#3567=(
BOUNDED_SURFACE()
B_SPLINE_SURFACE(3,2,((#431855,#431856,#431857),(#431858,#431859,#431860),
(#431861,#431862,#431863),(#431864,#431865,#431866)),.UNSPECIFIED.,.F.,
 .F.,.F.)
B_SPLINE_SURFACE_WITH_KNOTS((4,4),(3,3),(-5.22358356749296E-6,5.74594192424277E-5),
(-0.00127120052094877,1.),.UNSPECIFIED.)
GEOMETRIC_REPRESENTATION_ITEM()
RATIONAL_B_SPLINE_SURFACE(((1.00054449313192,0.785835073638684,1.),(1.0004770776749,
0.812351526358764,1.),(1.000440317886,0.826810216506224,1.),(1.00044777653332,
0.823876514387182,1.)))
REPRESENTATION_ITEM('')
SURFACE()
);
#3568=(
BOUNDED_SURFACE()
B_SPLINE_SURFACE(3,2,((#431868,#431869,#431870),(#431871,#431872,#431873),
(#431874,#431875,#431876),(#431877,#431878,#431879)),.UNSPECIFIED.,.F.,
 .F.,.F.)
B_SPLINE_SURFACE_WITH_KNOTS((4,4),(3,3),(-2.71050543121376E-20,4.88747512969885E-5),
(-0.000215805215023358,1.),.UNSPECIFIED.)
GEOMETRIC_REPRESENTATION_ITEM()
RATIONAL_B_SPLINE_SURFACE(((1.00008915600319,0.79343408549984,1.),(1.00008930224972,
0.793095246303377,1.),(1.00008944684594,0.792760230720659,1.),(1.00008958984373,
0.792428918540687,1.)))
REPRESENTATION_ITEM('')
SURFACE()
);
#3569=(
BOUNDED_SURFACE()
B_SPLINE_SURFACE(3,2,((#431881,#431882,#431883),(#431884,#431885,#431886),
(#431887,#431888,#431889),(#431890,#431891,#431892),(#431893,#431894,#431895),
(#431896,#431897,#431898)),.UNSPECIFIED.,.F.,.F.,.F.)
B_SPLINE_SURFACE_WITH_KNOTS((4,2,4),(3,3),(8.13151629364128E-20,7.62675010863197E-5,
0.000152535002172639),(0.,1.02152348203076),.UNSPECIFIED.)
GEOMETRIC_REPRESENTATION_ITEM()
RATIONAL_B_SPLINE_SURFACE(((1.,0.789033595401234,1.00908146323695),(1.,
0.857071781054808,1.00615262590431),(1.,0.922087264710746,1.00335390671593),
(1.,0.922394466502346,1.00334068261145),(1.,0.857224384599065,1.00614605678503),
(1.,0.789033595401632,1.00908146323693)))
REPRESENTATION_ITEM('')
SURFACE()
);
#3570=(
BOUNDED_SURFACE()
B_SPLINE_SURFACE(3,2,((#431900,#431901,#431902),(#431903,#431904,#431905),
(#431906,#431907,#431908),(#431909,#431910,#431911)),.UNSPECIFIED.,.F.,
 .F.,.F.)
B_SPLINE_SURFACE_WITH_KNOTS((4,4),(3,3),(3.25260651745651E-19,4.88747512969883E-5),
(-0.000215489856881612,1.),.UNSPECIFIED.)
GEOMETRIC_REPRESENTATION_ITEM()
RATIONAL_B_SPLINE_SURFACE(((1.00008945889707,0.792428983985775,1.),(1.00008931610828,
0.792760296061327,1.),(1.00008917172341,0.793095311538389,1.),(1.00008902569064,
0.793434150628027,1.)))
REPRESENTATION_ITEM('')
SURFACE()
);
#3571=(
BOUNDED_SURFACE()
B_SPLINE_SURFACE(3,2,((#431913,#431914,#431915),(#431916,#431917,#431918),
(#431919,#431920,#431921),(#431922,#431923,#431924)),.UNSPECIFIED.,.F.,
 .F.,.F.)
B_SPLINE_SURFACE_WITH_KNOTS((4,4),(3,3),(-5.21974905013089E-6,5.74172395514398E-5),
(-0.00139822857799824,1.00051312364076),.UNSPECIFIED.)
GEOMETRIC_REPRESENTATION_ITEM()
RATIONAL_B_SPLINE_SURFACE(((1.00049256947266,0.823768952243919,1.00018060397852),
(1.00048448215736,0.826662424388207,1.00017763870885),(1.00052427784045,
0.812424361909281,1.00019223006925),(1.00059912365882,0.785646094632626,
1.00021967280235)))
REPRESENTATION_ITEM('')
SURFACE()
);
#3572=(
BOUNDED_SURFACE()
B_SPLINE_SURFACE(3,2,((#431928,#431929,#431930),(#431931,#431932,#431933),
(#431934,#431935,#431936),(#431937,#431938,#431939)),.UNSPECIFIED.,.F.,
 .F.,.F.)
B_SPLINE_SURFACE_WITH_KNOTS((4,4),(3,3),(3.22980774337781E-5,9.63764854872248E-5),
(-0.00154325936368443,1.01095292447551),.UNSPECIFIED.)
GEOMETRIC_REPRESENTATION_ITEM()
RATIONAL_B_SPLINE_SURFACE(((1.00023530983298,0.922925743796163,1.00168574728332),
(1.00015136166125,0.950422439594214,1.00108434699061),(1.00033574337397,
0.890029368953953,1.00240524789549),(1.0005426009422,0.82227447316833,1.00388716464861)))
REPRESENTATION_ITEM('')
SURFACE()
);
#3573=(
BOUNDED_SURFACE()
B_SPLINE_SURFACE(3,2,((#432039,#432040,#432041),(#432042,#432043,#432044),
(#432045,#432046,#432047),(#432048,#432049,#432050)),.UNSPECIFIED.,.F.,
 .F.,.F.)
B_SPLINE_SURFACE_WITH_KNOTS((4,4),(3,3),(-4.33680868994202E-19,0.000101260117256736),
(0.,1.),.UNSPECIFIED.)
GEOMETRIC_REPRESENTATION_ITEM()
RATIONAL_B_SPLINE_SURFACE(((1.,0.796615278835172,1.),(1.,0.79589603805593,
1.),(1.,0.79519335466136,1.),(1.,0.794506193185535,1.)))
REPRESENTATION_ITEM('')
SURFACE()
);
#3574=(
BOUNDED_SURFACE()
B_SPLINE_SURFACE(3,2,((#432088,#432089,#432090),(#432091,#432092,#432093),
(#432094,#432095,#432096),(#432097,#432098,#432099),(#432100,#432101,#432102),
(#432103,#432104,#432105)),.UNSPECIFIED.,.F.,.F.,.F.)
B_SPLINE_SURFACE_WITH_KNOTS((4,2,4),(3,3),(-1.18584612615602E-20,1.66936432462294E-5,
3.33872864924588E-5),(0.,1.),.UNSPECIFIED.)
GEOMETRIC_REPRESENTATION_ITEM()
RATIONAL_B_SPLINE_SURFACE(((1.,0.796615278835171,1.),(1.,0.862310524418129,
1.),(1.,0.923774472010521,1.),(1.,0.923983993203424,1.),(1.,0.862574873720939,
1.),(1.,0.796615278835184,1.)))
REPRESENTATION_ITEM('')
SURFACE()
);
#3575=(
BOUNDED_SURFACE()
B_SPLINE_SURFACE(3,2,((#432142,#432143,#432144),(#432145,#432146,#432147),
(#432148,#432149,#432150),(#432151,#432152,#432153)),.UNSPECIFIED.,.F.,
 .F.,.F.)
B_SPLINE_SURFACE_WITH_KNOTS((4,4),(3,3),(0.,0.000101244905251112),(0.,1.),
 .UNSPECIFIED.)
GEOMETRIC_REPRESENTATION_ITEM()
RATIONAL_B_SPLINE_SURFACE(((1.,0.796615278835171,1.),(1.,0.795896146109795,
1.),(1.,0.795193565796499,1.),(1.,0.794506502889906,1.)))
REPRESENTATION_ITEM('')
SURFACE()
);
#3576=(
BOUNDED_SURFACE()
B_SPLINE_SURFACE(3,2,((#432189,#432190,#432191),(#432192,#432193,#432194),
(#432195,#432196,#432197),(#432198,#432199,#432200)),.UNSPECIFIED.,.F.,
 .F.,.F.)
B_SPLINE_SURFACE_WITH_KNOTS((4,4),(3,3),(2.85968127239939E-5,9.24681548475815E-5),
(-0.00167900678654101,1.01130827127819),.UNSPECIFIED.)
GEOMETRIC_REPRESENTATION_ITEM()
RATIONAL_B_SPLINE_SURFACE(((1.00059040895217,0.822187541868279,1.00401468696655),
(1.0003652771814,0.889990093671582,1.0024838267339),(1.00016469515013,0.95039904225793,
1.00111990082511),(1.00025604273992,0.922888044286083,1.00174104990631)))
REPRESENTATION_ITEM('')
SURFACE()
);
#3577=(
BOUNDED_SURFACE()
B_SPLINE_SURFACE(3,2,((#432204,#432205,#432206),(#432207,#432208,#432209),
(#432210,#432211,#432212),(#432213,#432214,#432215)),.UNSPECIFIED.,.F.,
 .F.,.F.)
B_SPLINE_SURFACE_WITH_KNOTS((4,4),(3,3),(-5.22358356749296E-6,5.74594192424278E-5),
(-0.0012712005204959,1.),.UNSPECIFIED.)
GEOMETRIC_REPRESENTATION_ITEM()
RATIONAL_B_SPLINE_SURFACE(((1.00054449313172,0.785835073638773,1.),(1.00047707767473,
0.81235152635887,1.),(1.00044031788584,0.8268102165063,1.),(1.00044777653317,
0.823876514387263,1.)))
REPRESENTATION_ITEM('')
SURFACE()
);
#3578=(
BOUNDED_SURFACE()
B_SPLINE_SURFACE(3,2,((#432217,#432218,#432219),(#432220,#432221,#432222),
(#432223,#432224,#432225),(#432226,#432227,#432228)),.UNSPECIFIED.,.F.,
 .F.,.F.)
B_SPLINE_SURFACE_WITH_KNOTS((4,4),(3,3),(-3.52365706057789E-19,4.88747512969879E-5),
(-0.000215805215795982,1.),.UNSPECIFIED.)
GEOMETRIC_REPRESENTATION_ITEM()
RATIONAL_B_SPLINE_SURFACE(((1.00008915600351,0.793434085499681,1.),(1.00008930225004,
0.793095246303237,1.),(1.00008944684626,0.792760230720486,1.),(1.00008958984405,
0.792428918540534,1.)))
REPRESENTATION_ITEM('')
SURFACE()
);
#3579=(
BOUNDED_SURFACE()
B_SPLINE_SURFACE(3,2,((#432230,#432231,#432232),(#432233,#432234,#432235),
(#432236,#432237,#432238),(#432239,#432240,#432241),(#432242,#432243,#432244),
(#432245,#432246,#432247)),.UNSPECIFIED.,.F.,.F.,.F.)
B_SPLINE_SURFACE_WITH_KNOTS((4,2,4),(3,3),(5.48877349820787E-19,7.626750108632E-5,
0.000152535002172639),(0.,1.02152348203067),.UNSPECIFIED.)
GEOMETRIC_REPRESENTATION_ITEM()
RATIONAL_B_SPLINE_SURFACE(((1.,0.789033595401253,1.00908146323691),(1.,
0.857071781054832,1.00615262590428),(1.,0.922087264710739,1.00335390671592),
(1.,0.922394466502362,1.00334068261143),(1.,0.857224384599061,1.006146056785),
(1.,0.78903359540165,1.00908146323689)))
REPRESENTATION_ITEM('')
SURFACE()
);
#3580=(
BOUNDED_SURFACE()
B_SPLINE_SURFACE(3,2,((#432249,#432250,#432251),(#432252,#432253,#432254),
(#432255,#432256,#432257),(#432258,#432259,#432260)),.UNSPECIFIED.,.F.,
 .F.,.F.)
B_SPLINE_SURFACE_WITH_KNOTS((4,4),(3,3),(8.13151629364128E-20,4.88747512969884E-5),
(-0.000215489857882313,1.),.UNSPECIFIED.)
GEOMETRIC_REPRESENTATION_ITEM()
RATIONAL_B_SPLINE_SURFACE(((1.00008945889748,0.79242898398557,1.),(1.0000893161087,
0.79276029606112,1.),(1.00008917172382,0.793095311538191,1.),(1.00008902569105,
0.793434150627821,1.)))
REPRESENTATION_ITEM('')
SURFACE()
);
#3581=(
BOUNDED_SURFACE()
B_SPLINE_SURFACE(3,2,((#432262,#432263,#432264),(#432265,#432266,#432267),
(#432268,#432269,#432270),(#432271,#432272,#432273)),.UNSPECIFIED.,.F.,
 .F.,.F.)
B_SPLINE_SURFACE_WITH_KNOTS((4,4),(3,3),(-5.2197490501287E-6,5.7417239551439E-5),
(-0.00139822857770129,1.00051312364067),.UNSPECIFIED.)
GEOMETRIC_REPRESENTATION_ITEM()
RATIONAL_B_SPLINE_SURFACE(((1.00049256947255,0.823768952243992,1.00018060397849),
(1.00048448215726,0.826662424388284,1.00017763870882),(1.00052427784034,
0.812424361909331,1.00019223006921),(1.00059912365869,0.785646094632718,
1.00021967280231)))
REPRESENTATION_ITEM('')
SURFACE()
);
#3582=(
BOUNDED_SURFACE()
B_SPLINE_SURFACE(3,2,((#432277,#432278,#432279),(#432280,#432281,#432282),
(#432283,#432284,#432285),(#432286,#432287,#432288)),.UNSPECIFIED.,.F.,
 .F.,.F.)
B_SPLINE_SURFACE_WITH_KNOTS((4,4),(3,3),(3.22980774337779E-5,9.63764854872254E-5),
(-0.00154325936357871,1.01095292447542),.UNSPECIFIED.)
GEOMETRIC_REPRESENTATION_ITEM()
RATIONAL_B_SPLINE_SURFACE(((1.00023530983297,0.922925743796177,1.00168574728331),
(1.00015136166124,0.95042243959422,1.0010843469906),(1.00033574337395,0.890029368953977,
1.00240524789547),(1.00054260094216,0.822274473168365,1.00388716464858)))
REPRESENTATION_ITEM('')
SURFACE()
);
#3583=(
BOUNDED_SURFACE()
B_SPLINE_SURFACE(3,2,((#432388,#432389,#432390),(#432391,#432392,#432393),
(#432394,#432395,#432396),(#432397,#432398,#432399)),.UNSPECIFIED.,.F.,
 .F.,.F.)
B_SPLINE_SURFACE_WITH_KNOTS((4,4),(3,3),(0.,0.000101260117256738),(0.,1.),
 .UNSPECIFIED.)
GEOMETRIC_REPRESENTATION_ITEM()
RATIONAL_B_SPLINE_SURFACE(((1.,0.796615278835173,1.),(1.,0.795896038055939,
1.),(1.,0.795193354661356,1.),(1.,0.794506193185549,1.)))
REPRESENTATION_ITEM('')
SURFACE()
);
#3584=(
BOUNDED_SURFACE()
B_SPLINE_SURFACE(3,2,((#432437,#432438,#432439),(#432440,#432441,#432442),
(#432443,#432444,#432445),(#432446,#432447,#432448),(#432449,#432450,#432451),
(#432452,#432453,#432454)),.UNSPECIFIED.,.F.,.F.,.F.)
B_SPLINE_SURFACE_WITH_KNOTS((4,2,4),(3,3),(1.66018457661843E-19,1.66936432462296E-5,
3.3387286492459E-5),(0.,1.),.UNSPECIFIED.)
GEOMETRIC_REPRESENTATION_ITEM()
RATIONAL_B_SPLINE_SURFACE(((1.,0.796615278835173,1.),(1.,0.862310524418134,
1.),(1.,0.923774472010516,1.),(1.,0.923983993203428,1.),(1.,0.862574873720952,
1.),(1.,0.796615278835181,1.)))
REPRESENTATION_ITEM('')
SURFACE()
);
#3585=(
BOUNDED_SURFACE()
B_SPLINE_SURFACE(3,2,((#432491,#432492,#432493),(#432494,#432495,#432496),
(#432497,#432498,#432499),(#432500,#432501,#432502)),.UNSPECIFIED.,.F.,
 .F.,.F.)
B_SPLINE_SURFACE_WITH_KNOTS((4,4),(3,3),(0.,0.000101244905251112),(0.,1.),
 .UNSPECIFIED.)
GEOMETRIC_REPRESENTATION_ITEM()
RATIONAL_B_SPLINE_SURFACE(((1.,0.796615278835171,1.),(1.,0.795896146109787,
1.),(1.,0.795193565796506,1.),(1.,0.7945065028899,1.)))
REPRESENTATION_ITEM('')
SURFACE()
);
#3586=(
BOUNDED_SURFACE()
B_SPLINE_SURFACE(3,2,((#432538,#432539,#432540),(#432541,#432542,#432543),
(#432544,#432545,#432546),(#432547,#432548,#432549)),.UNSPECIFIED.,.F.,
 .F.,.F.)
B_SPLINE_SURFACE_WITH_KNOTS((4,4),(3,3),(2.85968127239939E-5,9.24681548475819E-5),
(-0.0016790067864535,1.01130827127836),.UNSPECIFIED.)
GEOMETRIC_REPRESENTATION_ITEM()
RATIONAL_B_SPLINE_SURFACE(((1.00059040895214,0.822187541868259,1.00401468696661),
(1.00036527718138,0.889990093671583,1.00248382673394),(1.00016469515012,
0.950399042257919,1.00111990082512),(1.00025604273991,0.922888044286074,
1.00174104990633)))
REPRESENTATION_ITEM('')
SURFACE()
);
#3587=(
BOUNDED_SURFACE()
B_SPLINE_SURFACE(3,2,((#432553,#432554,#432555),(#432556,#432557,#432558),
(#432559,#432560,#432561),(#432562,#432563,#432564)),.UNSPECIFIED.,.F.,
 .F.,.F.)
B_SPLINE_SURFACE_WITH_KNOTS((4,4),(3,3),(-5.22358356749225E-6,5.74594192424276E-5),
(-0.0012712005206289,1.),.UNSPECIFIED.)
GEOMETRIC_REPRESENTATION_ITEM()
RATIONAL_B_SPLINE_SURFACE(((1.00054449313178,0.785835073638762,1.),(1.00047707767478,
0.812351526358823,1.),(1.00044031788589,0.82681021650628,1.),(1.00044777653321,
0.82387651438725,1.)))
REPRESENTATION_ITEM('')
SURFACE()
);
#3588=(
BOUNDED_SURFACE()
B_SPLINE_SURFACE(3,2,((#432566,#432567,#432568),(#432569,#432570,#432571),
(#432572,#432573,#432574),(#432575,#432576,#432577)),.UNSPECIFIED.,.F.,
 .F.,.F.)
B_SPLINE_SURFACE_WITH_KNOTS((4,4),(3,3),(-4.87890977618477E-19,4.88747512969881E-5),
(-0.000215805215274508,1.),.UNSPECIFIED.)
GEOMETRIC_REPRESENTATION_ITEM()
RATIONAL_B_SPLINE_SURFACE(((1.00008915600329,0.793434085499789,1.),(1.00008930224983,
0.793095246303343,1.),(1.00008944684605,0.792760230720596,1.),(1.00008958984384,
0.792428918540638,1.)))
REPRESENTATION_ITEM('')
SURFACE()
);
#3589=(
BOUNDED_SURFACE()
B_SPLINE_SURFACE(3,2,((#432579,#432580,#432581),(#432582,#432583,#432584),
(#432585,#432586,#432587),(#432588,#432589,#432590),(#432591,#432592,#432593),
(#432594,#432595,#432596)),.UNSPECIFIED.,.F.,.F.,.F.)
B_SPLINE_SURFACE_WITH_KNOTS((4,2,4),(3,3),(1.01643953670516E-19,7.62675010863196E-5,
0.000152535002172639),(0.,1.02152348203063),.UNSPECIFIED.)
GEOMETRIC_REPRESENTATION_ITEM()
RATIONAL_B_SPLINE_SURFACE(((1.,0.789033595401257,1.0090814632369),(1.,0.857071781054861,
1.00615262590427),(1.,0.922087264710712,1.00335390671591),(1.,0.922394466502399,
1.00334068261143),(1.,0.857224384599035,1.00614605678499),(1.,0.789033595401663,
1.00908146323688)))
REPRESENTATION_ITEM('')
SURFACE()
);
#3590=(
BOUNDED_SURFACE()
B_SPLINE_SURFACE(3,2,((#432598,#432599,#432600),(#432601,#432602,#432603),
(#432604,#432605,#432606),(#432607,#432608,#432609)),.UNSPECIFIED.,.F.,
 .F.,.F.)
B_SPLINE_SURFACE_WITH_KNOTS((4,4),(3,3),(6.50521303491303E-19,4.88747512969886E-5),
(-0.000215489856880668,1.),.UNSPECIFIED.)
GEOMETRIC_REPRESENTATION_ITEM()
RATIONAL_B_SPLINE_SURFACE(((1.00008945889707,0.792428983985776,1.),(1.00008931610828,
0.792760296061328,1.),(1.00008917172341,0.79309531153839,1.),(1.00008902569064,
0.793434150628027,1.)))
REPRESENTATION_ITEM('')
SURFACE()
);
#3591=(
BOUNDED_SURFACE()
B_SPLINE_SURFACE(3,2,((#432611,#432612,#432613),(#432614,#432615,#432616),
(#432617,#432618,#432619),(#432620,#432621,#432622)),.UNSPECIFIED.,.F.,
 .F.,.F.)
B_SPLINE_SURFACE_WITH_KNOTS((4,4),(3,3),(-5.21974905013085E-6,5.74172395514398E-5),
(-0.00139822857786748,1.00051312364076),.UNSPECIFIED.)
GEOMETRIC_REPRESENTATION_ITEM()
RATIONAL_B_SPLINE_SURFACE(((1.00049256947261,0.823768952243938,1.00018060397853),
(1.00048448215732,0.826662424388239,1.00017763870885),(1.0005242778404,
0.812424361909295,1.00019223006925),(1.00059912365876,0.785646094632659,
1.00021967280235)))
REPRESENTATION_ITEM('')
SURFACE()
);
#3592=(
BOUNDED_SURFACE()
B_SPLINE_SURFACE(3,2,((#432626,#432627,#432628),(#432629,#432630,#432631),
(#432632,#432633,#432634),(#432635,#432636,#432637)),.UNSPECIFIED.,.F.,
 .F.,.F.)
B_SPLINE_SURFACE_WITH_KNOTS((4,4),(3,3),(3.22980774337778E-5,9.63764854872252E-5),
(-0.00154325936321,1.01095292447555),.UNSPECIFIED.)
GEOMETRIC_REPRESENTATION_ITEM()
RATIONAL_B_SPLINE_SURFACE(((1.00023530983291,0.922925743796198,1.00168574728333),
(1.0001513616612,0.950422439594237,1.00108434699061),(1.00033574337387,
0.890029368953991,1.0024052478955),(1.00054260094203,0.822274473168418,
1.00388716464862)))
REPRESENTATION_ITEM('')
SURFACE()
);
#3593=(
BOUNDED_SURFACE()
B_SPLINE_SURFACE(3,2,((#432737,#432738,#432739),(#432740,#432741,#432742),
(#432743,#432744,#432745),(#432746,#432747,#432748)),.UNSPECIFIED.,.F.,
 .F.,.F.)
B_SPLINE_SURFACE_WITH_KNOTS((4,4),(3,3),(0.,0.000101260117256737),(0.,1.),
 .UNSPECIFIED.)
GEOMETRIC_REPRESENTATION_ITEM()
RATIONAL_B_SPLINE_SURFACE(((1.,0.796615278835169,1.),(1.,0.795896038055939,
1.),(1.,0.795193354661348,1.),(1.,0.794506193185533,1.)))
REPRESENTATION_ITEM('')
SURFACE()
);
#3594=(
BOUNDED_SURFACE()
B_SPLINE_SURFACE(3,2,((#432786,#432787,#432788),(#432789,#432790,#432791),
(#432792,#432793,#432794),(#432795,#432796,#432797),(#432798,#432799,#432800),
(#432801,#432802,#432803)),.UNSPECIFIED.,.F.,.F.,.F.)
B_SPLINE_SURFACE_WITH_KNOTS((4,2,4),(3,3),(1.16890546721093E-19,1.66936432462296E-5,
3.33872864924591E-5),(0.,1.),.UNSPECIFIED.)
GEOMETRIC_REPRESENTATION_ITEM()
RATIONAL_B_SPLINE_SURFACE(((1.,0.796615278835178,1.),(1.,0.86231052441814,
1.),(1.,0.923774472010522,1.),(1.,0.923983993203428,1.),(1.,0.862574873720943,
1.),(1.,0.796615278835182,1.)))
REPRESENTATION_ITEM('')
SURFACE()
);
#3595=(
BOUNDED_SURFACE()
B_SPLINE_SURFACE(3,2,((#432840,#432841,#432842),(#432843,#432844,#432845),
(#432846,#432847,#432848),(#432849,#432850,#432851)),.UNSPECIFIED.,.F.,
 .F.,.F.)
B_SPLINE_SURFACE_WITH_KNOTS((4,4),(3,3),(0.,0.000101244905251112),(0.,1.),
 .UNSPECIFIED.)
GEOMETRIC_REPRESENTATION_ITEM()
RATIONAL_B_SPLINE_SURFACE(((1.,0.79661527883517,1.),(1.,0.795896146109795,
1.),(1.,0.795193565796498,1.),(1.,0.794506502889894,1.)))
REPRESENTATION_ITEM('')
SURFACE()
);
#3596=(
BOUNDED_SURFACE()
B_SPLINE_SURFACE(3,2,((#432887,#432888,#432889),(#432890,#432891,#432892),
(#432893,#432894,#432895),(#432896,#432897,#432898)),.UNSPECIFIED.,.F.,
 .F.,.F.)
B_SPLINE_SURFACE_WITH_KNOTS((4,4),(3,3),(2.85968127239939E-5,9.24681548475817E-5),
(-0.00167900678641286,1.0113082712782),.UNSPECIFIED.)
GEOMETRIC_REPRESENTATION_ITEM()
RATIONAL_B_SPLINE_SURFACE(((1.00059040895212,0.82218754186829,1.00401468696656),
(1.00036527718137,0.889990093671602,1.00248382673391),(1.00016469515012,
0.95039904225793,1.00111990082511),(1.0002560427399,0.922888044286091,1.00174104990631)))
REPRESENTATION_ITEM('')
SURFACE()
);
#3597=(
BOUNDED_SURFACE()
B_SPLINE_SURFACE(3,2,((#432902,#432903,#432904),(#432905,#432906,#432907),
(#432908,#432909,#432910),(#432911,#432912,#432913)),.UNSPECIFIED.,.F.,
 .F.,.F.)
B_SPLINE_SURFACE_WITH_KNOTS((4,4),(3,3),(-5.22358356749071E-6,5.74594192424274E-5),
(-0.00127120052062342,1.),.UNSPECIFIED.)
GEOMETRIC_REPRESENTATION_ITEM()
RATIONAL_B_SPLINE_SURFACE(((1.00054449313178,0.785835073638754,0.999999999999999),
(1.00047707767477,0.812351526358836,1.),(1.00044031788589,0.826810216506263,
1.),(1.00044777653321,0.823876514387245,1.)))
REPRESENTATION_ITEM('')
SURFACE()
);
#3598=(
BOUNDED_SURFACE()
B_SPLINE_SURFACE(3,2,((#432915,#432916,#432917),(#432918,#432919,#432920),
(#432921,#432922,#432923),(#432924,#432925,#432926)),.UNSPECIFIED.,.F.,
 .F.,.F.)
B_SPLINE_SURFACE_WITH_KNOTS((4,4),(3,3),(5.42101086242752E-20,4.88747512969879E-5),
(-0.000215805215510756,1.),.UNSPECIFIED.)
GEOMETRIC_REPRESENTATION_ITEM()
RATIONAL_B_SPLINE_SURFACE(((1.00008915600339,0.793434085499737,1.),(1.00008930224992,
0.793095246303276,1.),(1.00008944684614,0.792760230720552,1.),(1.00008958984394,
0.792428918540586,1.)))
REPRESENTATION_ITEM('')
SURFACE()
);
#3599=(
BOUNDED_SURFACE()
B_SPLINE_SURFACE(3,2,((#432928,#432929,#432930),(#432931,#432932,#432933),
(#432934,#432935,#432936),(#432937,#432938,#432939),(#432940,#432941,#432942),
(#432943,#432944,#432945)),.UNSPECIFIED.,.F.,.F.,.F.)
B_SPLINE_SURFACE_WITH_KNOTS((4,2,4),(3,3),(2.16840434497101E-19,7.62675010863198E-5,
0.000152535002172639),(0.,1.02152348203062),.UNSPECIFIED.)
GEOMETRIC_REPRESENTATION_ITEM()
RATIONAL_B_SPLINE_SURFACE(((1.,0.789033595401261,1.00908146323689),(1.,
0.857071781054845,1.00615262590427),(1.,0.922087264710742,1.00335390671591),
(1.,0.922394466502365,1.00334068261143),(1.,0.85722438459908,1.00614605678498),
(1.,0.789033595401654,1.00908146323687)))
REPRESENTATION_ITEM('')
SURFACE()
);
#3600=(
BOUNDED_SURFACE()
B_SPLINE_SURFACE(3,2,((#432947,#432948,#432949),(#432950,#432951,#432952),
(#432953,#432954,#432955),(#432956,#432957,#432958)),.UNSPECIFIED.,.F.,
 .F.,.F.)
B_SPLINE_SURFACE_WITH_KNOTS((4,4),(3,3),(5.14996031930615E-19,4.88747512969884E-5),
(-0.00021548985705842,1.),.UNSPECIFIED.)
GEOMETRIC_REPRESENTATION_ITEM()
RATIONAL_B_SPLINE_SURFACE(((1.00008945889714,0.792428983985738,1.),(1.00008931610836,
0.792760296061292,1.),(1.00008917172348,0.79309531153835,1.),(1.00008902569071,
0.793434150627988,1.)))
REPRESENTATION_ITEM('')
SURFACE()
);
#3601=(
BOUNDED_SURFACE()
B_SPLINE_SURFACE(3,2,((#432960,#432961,#432962),(#432963,#432964,#432965),
(#432966,#432967,#432968),(#432969,#432970,#432971)),.UNSPECIFIED.,.F.,
 .F.,.F.)
B_SPLINE_SURFACE_WITH_KNOTS((4,4),(3,3),(-5.21974905013084E-6,5.74172395514398E-5),
(-0.00139822857740927,1.00051312364064),.UNSPECIFIED.)
GEOMETRIC_REPRESENTATION_ITEM()
RATIONAL_B_SPLINE_SURFACE(((1.00049256947245,0.823768952244038,1.00018060397848),
(1.00048448215716,0.826662424388339,1.00017763870881),(1.00052427784023,
0.812424361909396,1.0001922300692),(1.00059912365856,0.78564609463279,1.0002196728023)))
REPRESENTATION_ITEM('')
SURFACE()
);
#3602=(
BOUNDED_SURFACE()
B_SPLINE_SURFACE(3,2,((#432975,#432976,#432977),(#432978,#432979,#432980),
(#432981,#432982,#432983),(#432984,#432985,#432986)),.UNSPECIFIED.,.F.,
 .F.,.F.)
B_SPLINE_SURFACE_WITH_KNOTS((4,4),(3,3),(3.2298077433778E-5,9.63764854872257E-5),
(-0.00154325936370795,1.01095292447541),.UNSPECIFIED.)
GEOMETRIC_REPRESENTATION_ITEM()
RATIONAL_B_SPLINE_SURFACE(((1.00023530983298,0.922925743796168,1.00168574728331),
(1.00015136166125,0.950422439594218,1.0010843469906),(1.00033574337398,
0.890029368953962,1.00240524789547),(1.0005426009422,0.822274473168342,
1.00388716464857)))
REPRESENTATION_ITEM('')
SURFACE()
);
#3603=(
BOUNDED_SURFACE()
B_SPLINE_SURFACE(3,2,((#433086,#433087,#433088),(#433089,#433090,#433091),
(#433092,#433093,#433094),(#433095,#433096,#433097)),.UNSPECIFIED.,.F.,
 .F.,.F.)
B_SPLINE_SURFACE_WITH_KNOTS((4,4),(3,3),(0.,0.000101260117256738),(0.,1.),
 .UNSPECIFIED.)
GEOMETRIC_REPRESENTATION_ITEM()
RATIONAL_B_SPLINE_SURFACE(((1.,0.79661527883517,1.),(1.,0.795896038055932,
1.),(1.,0.795193354661351,1.),(1.,0.794506193185546,1.)))
REPRESENTATION_ITEM('')
SURFACE()
);
#3604=(
BOUNDED_SURFACE()
B_SPLINE_SURFACE(3,2,((#433135,#433136,#433137),(#433138,#433139,#433140),
(#433141,#433142,#433143),(#433144,#433145,#433146),(#433147,#433148,#433149),
(#433150,#433151,#433152)),.UNSPECIFIED.,.F.,.F.,.F.)
B_SPLINE_SURFACE_WITH_KNOTS((4,2,4),(3,3),(-5.0821976835258E-20,1.66936432462296E-5,
3.33872864924593E-5),(0.,1.),.UNSPECIFIED.)
GEOMETRIC_REPRESENTATION_ITEM()
RATIONAL_B_SPLINE_SURFACE(((1.,0.796615278835167,1.),(1.,0.862310524418131,
1.),(1.,0.92377447201052,1.),(1.,0.923983993203425,1.),(1.,0.862574873720948,
1.),(1.,0.796615278835171,1.)))
REPRESENTATION_ITEM('')
SURFACE()
);
#3605=(
BOUNDED_SURFACE()
B_SPLINE_SURFACE(3,2,((#433189,#433190,#433191),(#433192,#433193,#433194),
(#433195,#433196,#433197),(#433198,#433199,#433200)),.UNSPECIFIED.,.F.,
 .F.,.F.)
B_SPLINE_SURFACE_WITH_KNOTS((4,4),(3,3),(0.,0.000101244905251112),(0.,1.),
 .UNSPECIFIED.)
GEOMETRIC_REPRESENTATION_ITEM()
RATIONAL_B_SPLINE_SURFACE(((1.,0.796615278835171,1.),(1.,0.795896146109791,
1.),(1.,0.7951935657965,1.),(1.,0.794506502889901,1.)))
REPRESENTATION_ITEM('')
SURFACE()
);
#3606=(
BOUNDED_SURFACE()
B_SPLINE_SURFACE(3,2,((#433236,#433237,#433238),(#433239,#433240,#433241),
(#433242,#433243,#433244),(#433245,#433246,#433247)),.UNSPECIFIED.,.F.,
 .F.,.F.)
B_SPLINE_SURFACE_WITH_KNOTS((4,4),(3,3),(2.85968127239939E-5,9.24681548475817E-5),
(-0.00167900678782365,1.01130827127822),.UNSPECIFIED.)
GEOMETRIC_REPRESENTATION_ITEM()
RATIONAL_B_SPLINE_SURFACE(((1.00059040895262,0.82218754186804,1.00401468696657),
(1.00036527718167,0.889990093671435,1.00248382673391),(1.00016469515026,
0.950399042257868,1.00111990082511),(1.00025604274012,0.92288804428598,
1.00174104990631)))
REPRESENTATION_ITEM('')
SURFACE()
);
#3607=(
BOUNDED_SURFACE()
B_SPLINE_SURFACE(3,2,((#433251,#433252,#433253),(#433254,#433255,#433256),
(#433257,#433258,#433259),(#433260,#433261,#433262)),.UNSPECIFIED.,.F.,
 .F.,.F.)
B_SPLINE_SURFACE_WITH_KNOTS((4,4),(3,3),(-5.22358356749241E-6,5.74594192424278E-5),
(-0.00127120052040753,1.),.UNSPECIFIED.)
GEOMETRIC_REPRESENTATION_ITEM()
RATIONAL_B_SPLINE_SURFACE(((1.00054449313169,0.785835073638789,1.),(1.00047707767469,
0.812351526358887,1.),(1.00044031788581,0.826810216506305,1.),(1.00044777653313,
0.823876514387289,1.)))
REPRESENTATION_ITEM('')
SURFACE()
);
#3608=(
BOUNDED_SURFACE()
B_SPLINE_SURFACE(3,2,((#433264,#433265,#433266),(#433267,#433268,#433269),
(#433270,#433271,#433272),(#433273,#433274,#433275)),.UNSPECIFIED.,.F.,
 .F.,.F.)
B_SPLINE_SURFACE_WITH_KNOTS((4,4),(3,3),(0.,4.88747512969878E-5),(-0.000215805215457177,
1.),.UNSPECIFIED.)
GEOMETRIC_REPRESENTATION_ITEM()
RATIONAL_B_SPLINE_SURFACE(((1.00008915600337,0.793434085499749,1.),(1.0000893022499,
0.793095246303283,1.),(1.00008944684612,0.792760230720569,1.),(1.00008958984391,
0.792428918540598,1.)))
REPRESENTATION_ITEM('')
SURFACE()
);
#3609=(
BOUNDED_SURFACE()
B_SPLINE_SURFACE(3,2,((#433277,#433278,#433279),(#433280,#433281,#433282),
(#433283,#433284,#433285),(#433286,#433287,#433288),(#433289,#433290,#433291),
(#433292,#433293,#433294)),.UNSPECIFIED.,.F.,.F.,.F.)
B_SPLINE_SURFACE_WITH_KNOTS((4,2,4),(3,3),(2.23616698075135E-19,7.62675010863198E-5,
0.000152535002172639),(0.,1.02152348203061),.UNSPECIFIED.)
GEOMETRIC_REPRESENTATION_ITEM()
RATIONAL_B_SPLINE_SURFACE(((1.,0.789033595401263,1.00908146323688),(1.,
0.857071781054884,1.00615262590426),(1.,0.922087264710692,1.00335390671591),
(1.,0.92239446650242,1.00334068261142),(1.,0.85722438459903,1.00614605678498),
(1.,0.789033595401661,1.00908146323687)))
REPRESENTATION_ITEM('')
SURFACE()
);
#3610=(
BOUNDED_SURFACE()
B_SPLINE_SURFACE(3,2,((#433296,#433297,#433298),(#433299,#433300,#433301),
(#433302,#433303,#433304),(#433305,#433306,#433307)),.UNSPECIFIED.,.F.,
 .F.,.F.)
B_SPLINE_SURFACE_WITH_KNOTS((4,4),(3,3),(3.79470760369927E-19,4.88747512969884E-5),
(-0.000215489857563226,1.),.UNSPECIFIED.)
GEOMETRIC_REPRESENTATION_ITEM()
RATIONAL_B_SPLINE_SURFACE(((1.00008945889735,0.792428983985636,1.),(1.00008931610857,
0.792760296061186,1.),(1.00008917172369,0.793095311538252,1.),(1.00008902569092,
0.793434150627887,1.)))
REPRESENTATION_ITEM('')
SURFACE()
);
#3611=(
BOUNDED_SURFACE()
B_SPLINE_SURFACE(3,2,((#433309,#433310,#433311),(#433312,#433313,#433314),
(#433315,#433316,#433317),(#433318,#433319,#433320)),.UNSPECIFIED.,.F.,
 .F.,.F.)
B_SPLINE_SURFACE_WITH_KNOTS((4,4),(3,3),(-5.2197490501308E-6,5.74172395514396E-5),
(-0.0013982285777185,1.00051312364079),.UNSPECIFIED.)
GEOMETRIC_REPRESENTATION_ITEM()
RATIONAL_B_SPLINE_SURFACE(((1.00049256947256,0.823768952243963,1.00018060397854),
(1.00048448215726,0.826662424388248,1.00017763870886),(1.00052427784034,
0.812424361909325,1.00019223006926),(1.0005991236587,0.785646094632683,
1.00021967280236)))
REPRESENTATION_ITEM('')
SURFACE()
);
#3612=(
BOUNDED_SURFACE()
B_SPLINE_SURFACE(3,2,((#433324,#433325,#433326),(#433327,#433328,#433329),
(#433330,#433331,#433332),(#433333,#433334,#433335)),.UNSPECIFIED.,.F.,
 .F.,.F.)
B_SPLINE_SURFACE_WITH_KNOTS((4,4),(3,3),(3.22980774337779E-5,9.63764854872253E-5),
(-0.00154325936394338,1.01095292447531),.UNSPECIFIED.)
GEOMETRIC_REPRESENTATION_ITEM()
RATIONAL_B_SPLINE_SURFACE(((1.00023530983302,0.922925743796155,1.00168574728329),
(1.00015136166128,0.950422439594212,1.00108434699059),(1.00033574337403,
0.890029368953942,1.00240524789545),(1.00054260094229,0.822274473168318,
1.00388716464854)))
REPRESENTATION_ITEM('')
SURFACE()
);
#3613=(
BOUNDED_SURFACE()
B_SPLINE_SURFACE(3,2,((#433435,#433436,#433437),(#433438,#433439,#433440),
(#433441,#433442,#433443),(#433444,#433445,#433446)),.UNSPECIFIED.,.F.,
 .F.,.F.)
B_SPLINE_SURFACE_WITH_KNOTS((4,4),(3,3),(-2.16840434497101E-19,0.000101260117256738),
(0.,1.),.UNSPECIFIED.)
GEOMETRIC_REPRESENTATION_ITEM()
RATIONAL_B_SPLINE_SURFACE(((1.,0.796615278835171,1.),(1.,0.795896038055945,
1.),(1.,0.795193354661344,1.),(1.,0.794506193185546,1.)))
REPRESENTATION_ITEM('')
SURFACE()
);
#3614=(
BOUNDED_SURFACE()
B_SPLINE_SURFACE(3,2,((#433484,#433485,#433486),(#433487,#433488,#433489),
(#433490,#433491,#433492),(#433493,#433494,#433495),(#433496,#433497,#433498),
(#433499,#433500,#433501)),.UNSPECIFIED.,.F.,.F.,.F.)
B_SPLINE_SURFACE_WITH_KNOTS((4,2,4),(3,3),(1.91429446079472E-19,1.66936432462294E-5,
3.33872864924587E-5),(0.,1.),.UNSPECIFIED.)
GEOMETRIC_REPRESENTATION_ITEM()
RATIONAL_B_SPLINE_SURFACE(((1.,0.79661527883518,1.),(1.,0.862310524418121,
1.),(1.,0.923774472010515,1.),(1.,0.92398399320343,1.),(1.,0.862574873720946,
1.),(1.,0.79661527883519,1.)))
REPRESENTATION_ITEM('')
SURFACE()
);
#3615=(
BOUNDED_SURFACE()
B_SPLINE_SURFACE(3,2,((#433538,#433539,#433540),(#433541,#433542,#433543),
(#433544,#433545,#433546),(#433547,#433548,#433549)),.UNSPECIFIED.,.F.,
 .F.,.F.)
B_SPLINE_SURFACE_WITH_KNOTS((4,4),(3,3),(0.,0.000101244905251112),(0.,1.),
 .UNSPECIFIED.)
GEOMETRIC_REPRESENTATION_ITEM()
RATIONAL_B_SPLINE_SURFACE(((1.,0.796615278835175,1.),(1.,0.795896146109785,
1.),(1.,0.795193565796504,1.),(1.,0.794506502889899,1.)))
REPRESENTATION_ITEM('')
SURFACE()
);
#3616=(
BOUNDED_SURFACE()
B_SPLINE_SURFACE(3,2,((#433585,#433586,#433587),(#433588,#433589,#433590),
(#433591,#433592,#433593),(#433594,#433595,#433596)),.UNSPECIFIED.,.F.,
 .F.,.F.)
B_SPLINE_SURFACE_WITH_KNOTS((4,4),(3,3),(2.85968127239939E-5,9.24681548475817E-5),
(-0.0016790067866049,1.01130827127825),.UNSPECIFIED.)
GEOMETRIC_REPRESENTATION_ITEM()
RATIONAL_B_SPLINE_SURFACE(((1.00059040895219,0.822187541868252,1.00401468696658),
(1.00036527718141,0.889990093671559,1.00248382673392),(1.00016469515014,
0.950399042257932,1.00111990082511),(1.00025604273993,0.922888044286072,
1.00174104990632)))
REPRESENTATION_ITEM('')
SURFACE()
);
#3617=(
BOUNDED_SURFACE()
B_SPLINE_SURFACE(3,2,((#433600,#433601,#433602),(#433603,#433604,#433605),
(#433606,#433607,#433608),(#433609,#433610,#433611)),.UNSPECIFIED.,.F.,
 .F.,.F.)
B_SPLINE_SURFACE_WITH_KNOTS((4,4),(3,3),(-5.22358356749298E-6,5.74594192424276E-5),
(-0.00127120052069362,1.),.UNSPECIFIED.)
GEOMETRIC_REPRESENTATION_ITEM()
RATIONAL_B_SPLINE_SURFACE(((1.00054449313181,0.785835073638747,1.),(1.0004770776748,
0.812351526358807,1.),(1.00044031788591,0.826810216506271,1.),(1.00044777653323,
0.823876514387229,1.)))
REPRESENTATION_ITEM('')
SURFACE()
);
#3618=(
BOUNDED_SURFACE()
B_SPLINE_SURFACE(3,2,((#433613,#433614,#433615),(#433616,#433617,#433618),
(#433619,#433620,#433621),(#433622,#433623,#433624)),.UNSPECIFIED.,.F.,
 .F.,.F.)
B_SPLINE_SURFACE_WITH_KNOTS((4,4),(3,3),(-5.42101086242752E-20,4.88747512969882E-5),
(-0.000215805215169258,1.),.UNSPECIFIED.)
GEOMETRIC_REPRESENTATION_ITEM()
RATIONAL_B_SPLINE_SURFACE(((1.00008915600325,0.793434085499808,1.),(1.00008930224978,
0.793095246303361,1.),(1.000089446846,0.792760230720617,1.),(1.00008958984379,
0.792428918540663,1.)))
REPRESENTATION_ITEM('')
SURFACE()
);
#3619=(
BOUNDED_SURFACE()
B_SPLINE_SURFACE(3,2,((#433626,#433627,#433628),(#433629,#433630,#433631),
(#433632,#433633,#433634),(#433635,#433636,#433637),(#433638,#433639,#433640),
(#433641,#433642,#433643)),.UNSPECIFIED.,.F.,.F.,.F.)
B_SPLINE_SURFACE_WITH_KNOTS((4,2,4),(3,3),(2.84603070277445E-19,7.62675010863197E-5,
0.000152535002172639),(0.,1.02152348203073),.UNSPECIFIED.)
GEOMETRIC_REPRESENTATION_ITEM()
RATIONAL_B_SPLINE_SURFACE(((1.,0.78903359540124,1.00908146323694),(1.,0.857071781054861,
1.0061526259043),(1.,0.922087264710688,1.00335390671593),(1.,0.922394466502408,
1.00334068261144),(1.,0.857224384599018,1.00614605678502),(1.,0.789033595401641,
1.00908146323692)))
REPRESENTATION_ITEM('')
SURFACE()
);
#3620=(
BOUNDED_SURFACE()
B_SPLINE_SURFACE(3,2,((#433645,#433646,#433647),(#433648,#433649,#433650),
(#433651,#433652,#433653),(#433654,#433655,#433656)),.UNSPECIFIED.,.F.,
 .F.,.F.)
B_SPLINE_SURFACE_WITH_KNOTS((4,4),(3,3),(4.87890977618477E-19,4.88747512969886E-5),
(-0.000215489857113495,1.),.UNSPECIFIED.)
GEOMETRIC_REPRESENTATION_ITEM()
RATIONAL_B_SPLINE_SURFACE(((1.00008945889716,0.792428983985728,1.),(1.00008931610838,
0.792760296061271,1.),(1.00008917172351,0.793095311538354,1.),(1.00008902569073,
0.793434150627978,1.)))
REPRESENTATION_ITEM('')
SURFACE()
);
#3621=(
BOUNDED_SURFACE()
B_SPLINE_SURFACE(3,2,((#433658,#433659,#433660),(#433661,#433662,#433663),
(#433664,#433665,#433666),(#433667,#433668,#433669)),.UNSPECIFIED.,.F.,
 .F.,.F.)
B_SPLINE_SURFACE_WITH_KNOTS((4,4),(3,3),(-5.2197490501309E-6,5.74172395514392E-5),
(-0.00139822857766469,1.0005131236408),.UNSPECIFIED.)
GEOMETRIC_REPRESENTATION_ITEM()
RATIONAL_B_SPLINE_SURFACE(((1.00049256947254,0.823768952243971,1.00018060397854),
(1.00048448215724,0.826662424388243,1.00017763870887),(1.00052427784032,
0.812424361909343,1.00019223006926),(1.00059912365867,0.785646094632688,
1.00021967280237)))
REPRESENTATION_ITEM('')
SURFACE()
);
#3622=(
BOUNDED_SURFACE()
B_SPLINE_SURFACE(3,2,((#433673,#433674,#433675),(#433676,#433677,#433678),
(#433679,#433680,#433681),(#433682,#433683,#433684)),.UNSPECIFIED.,.F.,
 .F.,.F.)
B_SPLINE_SURFACE_WITH_KNOTS((4,4),(3,3),(3.2298077433778E-5,9.63764854872256E-5),
(-0.00154325936361246,1.01095292447532),.UNSPECIFIED.)
GEOMETRIC_REPRESENTATION_ITEM()
RATIONAL_B_SPLINE_SURFACE(((1.00023530983297,0.922925743796182,1.00168574728329),
(1.00015136166124,0.95042243959422,1.00108434699059),(1.00033574337396,
0.890029368953983,1.00240524789545),(1.00054260094217,0.822274473168379,
1.00388716464854)))
REPRESENTATION_ITEM('')
SURFACE()
);
#3623=(
BOUNDED_SURFACE()
B_SPLINE_SURFACE(3,2,((#433784,#433785,#433786),(#433787,#433788,#433789),
(#433790,#433791,#433792),(#433793,#433794,#433795)),.UNSPECIFIED.,.F.,
 .F.,.F.)
B_SPLINE_SURFACE_WITH_KNOTS((4,4),(3,3),(-2.16840434497101E-19,0.000101260117256737),
(0.,1.),.UNSPECIFIED.)
GEOMETRIC_REPRESENTATION_ITEM()
RATIONAL_B_SPLINE_SURFACE(((1.,0.796615278835167,1.),(1.,0.795896038055936,
1.),(1.,0.79519335466135,1.),(1.,0.794506193185548,1.)))
REPRESENTATION_ITEM('')
SURFACE()
);
#3624=(
BOUNDED_SURFACE()
B_SPLINE_SURFACE(3,2,((#433833,#433834,#433835),(#433836,#433837,#433838),
(#433839,#433840,#433841),(#433842,#433843,#433844),(#433845,#433846,#433847),
(#433848,#433849,#433850)),.UNSPECIFIED.,.F.,.F.,.F.)
B_SPLINE_SURFACE_WITH_KNOTS((4,2,4),(3,3),(1.71100655345369E-19,1.66936432462295E-5,
3.33872864924587E-5),(0.,1.),.UNSPECIFIED.)
GEOMETRIC_REPRESENTATION_ITEM()
RATIONAL_B_SPLINE_SURFACE(((1.,0.79661527883518,1.),(1.,0.862310524418124,
1.),(1.,0.923774472010515,1.),(1.,0.92398399320343,1.),(1.,0.862574873720945,
1.),(1.,0.796615278835185,1.)))
REPRESENTATION_ITEM('')
SURFACE()
);
#3625=(
BOUNDED_SURFACE()
B_SPLINE_SURFACE(3,2,((#433887,#433888,#433889),(#433890,#433891,#433892),
(#433893,#433894,#433895),(#433896,#433897,#433898)),.UNSPECIFIED.,.F.,
 .F.,.F.)
B_SPLINE_SURFACE_WITH_KNOTS((4,4),(3,3),(-2.16840434497101E-19,0.000101244905251112),
(0.,1.),.UNSPECIFIED.)
GEOMETRIC_REPRESENTATION_ITEM()
RATIONAL_B_SPLINE_SURFACE(((1.,0.796615278835175,1.),(1.,0.795896146109793,
1.),(1.,0.795193565796495,1.),(1.,0.794506502889905,1.)))
REPRESENTATION_ITEM('')
SURFACE()
);
#3626=(
BOUNDED_SURFACE()
B_SPLINE_SURFACE(3,2,((#433934,#433935,#433936),(#433937,#433938,#433939),
(#433940,#433941,#433942),(#433943,#433944,#433945)),.UNSPECIFIED.,.F.,
 .F.,.F.)
B_SPLINE_SURFACE_WITH_KNOTS((4,4),(3,3),(2.85968127239939E-5,9.24681548475817E-5),
(-0.00167900678794363,1.01130827127821),.UNSPECIFIED.)
GEOMETRIC_REPRESENTATION_ITEM()
RATIONAL_B_SPLINE_SURFACE(((1.00059040895266,0.822187541868021,1.00401468696656),
(1.0003652771817,0.889990093671417,1.00248382673391),(1.00016469515027,
0.950399042257861,1.00111990082511),(1.00025604274014,0.922888044285972,
1.00174104990631)))
REPRESENTATION_ITEM('')
SURFACE()
);
#3627=(
BOUNDED_SURFACE()
B_SPLINE_SURFACE(3,2,((#433949,#433950,#433951),(#433952,#433953,#433954),
(#433955,#433956,#433957),(#433958,#433959,#433960)),.UNSPECIFIED.,.F.,
 .F.,.F.)
B_SPLINE_SURFACE_WITH_KNOTS((4,4),(3,3),(-5.22358356749302E-6,5.74594192424276E-5),
(-0.00127120052052642,1.),.UNSPECIFIED.)
GEOMETRIC_REPRESENTATION_ITEM()
RATIONAL_B_SPLINE_SURFACE(((1.00054449313174,0.785835073638765,1.),(1.00047707767474,
0.812351526358866,1.),(1.00044031788585,0.826810216506294,1.),(1.00044777653318,
0.823876514387261,1.)))
REPRESENTATION_ITEM('')
SURFACE()
);
#3628=(
BOUNDED_SURFACE()
B_SPLINE_SURFACE(3,2,((#433962,#433963,#433964),(#433965,#433966,#433967),
(#433968,#433969,#433970),(#433971,#433972,#433973)),.UNSPECIFIED.,.F.,
 .F.,.F.)
B_SPLINE_SURFACE_WITH_KNOTS((4,4),(3,3),(-8.13151629364128E-20,4.88747512969878E-5),
(-0.000215805215605584,1.),.UNSPECIFIED.)
GEOMETRIC_REPRESENTATION_ITEM()
RATIONAL_B_SPLINE_SURFACE(((1.00008915600343,0.793434085499714,1.),(1.00008930224996,
0.793095246303281,1.),(1.00008944684618,0.792760230720533,1.),(1.00008958984398,
0.792428918540569,1.)))
REPRESENTATION_ITEM('')
SURFACE()
);
#3629=(
BOUNDED_SURFACE()
B_SPLINE_SURFACE(3,2,((#433975,#433976,#433977),(#433978,#433979,#433980),
(#433981,#433982,#433983),(#433984,#433985,#433986),(#433987,#433988,#433989),
(#433990,#433991,#433992)),.UNSPECIFIED.,.F.,.F.,.F.)
B_SPLINE_SURFACE_WITH_KNOTS((4,2,4),(3,3),(6.7762635780344E-20,7.62675010863195E-5,
0.000152535002172639),(0.,1.02152348203066),.UNSPECIFIED.)
GEOMETRIC_REPRESENTATION_ITEM()
RATIONAL_B_SPLINE_SURFACE(((1.,0.789033595401255,1.00908146323691),(1.,
0.857071781054837,1.00615262590428),(1.,0.922087264710733,1.00335390671592),
(1.,0.92239446650238,1.00334068261143),(1.,0.857224384599051,1.006146056785),
(1.,0.789033595401652,1.00908146323689)))
REPRESENTATION_ITEM('')
SURFACE()
);
#3630=(
BOUNDED_SURFACE()
B_SPLINE_SURFACE(3,2,((#433994,#433995,#433996),(#433997,#433998,#433999),
(#434000,#434001,#434002),(#434003,#434004,#434005)),.UNSPECIFIED.,.F.,
 .F.,.F.)
B_SPLINE_SURFACE_WITH_KNOTS((4,4),(3,3),(6.50521303491303E-19,4.88747512969884E-5),
(-0.000215489857064291,1.),.UNSPECIFIED.)
GEOMETRIC_REPRESENTATION_ITEM()
RATIONAL_B_SPLINE_SURFACE(((1.00008945889714,0.792428983985734,1.),(1.00008931610836,
0.792760296061303,1.),(1.00008917172349,0.793095311538351,1.),(1.00008902569071,
0.79343415062799,1.)))
REPRESENTATION_ITEM('')
SURFACE()
);
#3631=(
BOUNDED_SURFACE()
B_SPLINE_SURFACE(3,2,((#434007,#434008,#434009),(#434010,#434011,#434012),
(#434013,#434014,#434015),(#434016,#434017,#434018)),.UNSPECIFIED.,.F.,
 .F.,.F.)
B_SPLINE_SURFACE_WITH_KNOTS((4,4),(3,3),(-5.21974905012868E-6,5.74172395514399E-5),
(-0.00139822857733951,1.00051312364071),.UNSPECIFIED.)
GEOMETRIC_REPRESENTATION_ITEM()
RATIONAL_B_SPLINE_SURFACE(((1.00049256947243,0.823768952244043,1.00018060397851),
(1.00048448215713,0.826662424388329,1.00017763870884),(1.0005242778402,
0.812424361909413,1.00019223006923),(1.00059912365854,0.78564609463278,
1.00021967280233)))
REPRESENTATION_ITEM('')
SURFACE()
);
#3632=(
BOUNDED_SURFACE()
B_SPLINE_SURFACE(3,2,((#434022,#434023,#434024),(#434025,#434026,#434027),
(#434028,#434029,#434030),(#434031,#434032,#434033)),.UNSPECIFIED.,.F.,
 .F.,.F.)
B_SPLINE_SURFACE_WITH_KNOTS((4,4),(3,3),(3.22980774337779E-5,9.63764854872252E-5),
(-0.00154325936260306,1.01095292447551),.UNSPECIFIED.)
GEOMETRIC_REPRESENTATION_ITEM()
RATIONAL_B_SPLINE_SURFACE(((1.00023530983282,0.922925743796246,1.00168574728332),
(1.00015136166114,0.950422439594261,1.00108434699061),(1.00033574337374,
0.89002936895408,1.00240524789549),(1.00054260094182,0.822274473168522,
1.00388716464861)))
REPRESENTATION_ITEM('')
SURFACE()
);
#3633=(
BOUNDED_SURFACE()
B_SPLINE_SURFACE(3,2,((#434133,#434134,#434135),(#434136,#434137,#434138),
(#434139,#434140,#434141),(#434142,#434143,#434144)),.UNSPECIFIED.,.F.,
 .F.,.F.)
B_SPLINE_SURFACE_WITH_KNOTS((4,4),(3,3),(0.,0.000101260117256737),(0.,1.),
 .UNSPECIFIED.)
GEOMETRIC_REPRESENTATION_ITEM()
RATIONAL_B_SPLINE_SURFACE(((1.,0.796615278835165,1.),(1.,0.795896038055936,
1.),(1.,0.795193354661363,1.),(1.,0.794506193185527,1.)))
REPRESENTATION_ITEM('')
SURFACE()
);
#3634=(
BOUNDED_SURFACE()
B_SPLINE_SURFACE(3,2,((#434182,#434183,#434184),(#434185,#434186,#434187),
(#434188,#434189,#434190),(#434191,#434192,#434193),(#434194,#434195,#434196),
(#434197,#434198,#434199)),.UNSPECIFIED.,.F.,.F.,.F.)
B_SPLINE_SURFACE_WITH_KNOTS((4,2,4),(3,3),(-1.88041314290455E-19,1.66936432462293E-5,
3.33872864924587E-5),(0.,1.),.UNSPECIFIED.)
GEOMETRIC_REPRESENTATION_ITEM()
RATIONAL_B_SPLINE_SURFACE(((1.,0.796615278835176,1.),(1.,0.862310524418128,
1.),(1.,0.923774472010522,1.),(1.,0.923983993203425,1.),(1.,0.862574873720946,
1.),(1.,0.796615278835188,1.)))
REPRESENTATION_ITEM('')
SURFACE()
);
#3635=(
BOUNDED_SURFACE()
B_SPLINE_SURFACE(3,2,((#434236,#434237,#434238),(#434239,#434240,#434241),
(#434242,#434243,#434244),(#434245,#434246,#434247)),.UNSPECIFIED.,.F.,
 .F.,.F.)
B_SPLINE_SURFACE_WITH_KNOTS((4,4),(3,3),(0.,0.000101244905251112),(0.,1.),
 .UNSPECIFIED.)
GEOMETRIC_REPRESENTATION_ITEM()
RATIONAL_B_SPLINE_SURFACE(((1.,0.796615278835171,1.),(1.,0.795896146109788,
1.),(1.,0.795193565796499,1.),(1.,0.7945065028899,1.)))
REPRESENTATION_ITEM('')
SURFACE()
);
#3636=(
BOUNDED_SURFACE()
B_SPLINE_SURFACE(3,2,((#434283,#434284,#434285),(#434286,#434287,#434288),
(#434289,#434290,#434291),(#434292,#434293,#434294)),.UNSPECIFIED.,.F.,
 .F.,.F.)
B_SPLINE_SURFACE_WITH_KNOTS((4,4),(3,3),(2.85968127239939E-5,9.24681548475816E-5),
(-0.00167900678752855,1.01130827127812),.UNSPECIFIED.)
GEOMETRIC_REPRESENTATION_ITEM()
RATIONAL_B_SPLINE_SURFACE(((1.00059040895251,0.822187541868116,1.00401468696653),
(1.00036527718161,0.889990093671472,1.00248382673389),(1.00016469515023,
0.950399042257892,1.0011199008251),(1.00025604274007,0.92288804428601,1.00174104990629)))
REPRESENTATION_ITEM('')
SURFACE()
);
#3637=(
BOUNDED_SURFACE()
B_SPLINE_SURFACE(3,2,((#434298,#434299,#434300),(#434301,#434302,#434303),
(#434304,#434305,#434306),(#434307,#434308,#434309)),.UNSPECIFIED.,.F.,
 .F.,.F.)
B_SPLINE_SURFACE_WITH_KNOTS((4,4),(3,3),(-5.2235835674927E-6,5.74594192424279E-5),
(-0.00127120052049952,1.),.UNSPECIFIED.)
GEOMETRIC_REPRESENTATION_ITEM()
RATIONAL_B_SPLINE_SURFACE(((1.00054449313173,0.785835073638772,1.),(1.00047707767473,
0.812351526358862,1.),(1.00044031788584,0.826810216506295,1.),(1.00044777653317,
0.823876514387265,1.)))
REPRESENTATION_ITEM('')
SURFACE()
);
#3638=(
BOUNDED_SURFACE()
B_SPLINE_SURFACE(3,2,((#434311,#434312,#434313),(#434314,#434315,#434316),
(#434317,#434318,#434319),(#434320,#434321,#434322)),.UNSPECIFIED.,.F.,
 .F.,.F.)
B_SPLINE_SURFACE_WITH_KNOTS((4,4),(3,3),(-3.52365706057789E-19,4.88747512969882E-5),
(-0.000215805215178045,1.),.UNSPECIFIED.)
GEOMETRIC_REPRESENTATION_ITEM()
RATIONAL_B_SPLINE_SURFACE(((1.00008915600325,0.793434085499806,1.),(1.00008930224979,
0.793095246303358,1.),(1.00008944684601,0.792760230720618,1.),(1.0000895898438,
0.792428918540656,1.)))
REPRESENTATION_ITEM('')
SURFACE()
);
#3639=(
BOUNDED_SURFACE()
B_SPLINE_SURFACE(3,2,((#434324,#434325,#434326),(#434327,#434328,#434329),
(#434330,#434331,#434332),(#434333,#434334,#434335),(#434336,#434337,#434338),
(#434339,#434340,#434341)),.UNSPECIFIED.,.F.,.F.,.F.)
B_SPLINE_SURFACE_WITH_KNOTS((4,2,4),(3,3),(1.35525271560688E-20,7.62675010863196E-5,
0.000152535002172639),(0.,1.02152348203061),.UNSPECIFIED.)
GEOMETRIC_REPRESENTATION_ITEM()
RATIONAL_B_SPLINE_SURFACE(((1.,0.789033595401266,1.00908146323688),(1.,
0.857071781054839,1.00615262590427),(1.,0.92208726471075,1.00335390671591),
(1.,0.922394466502367,1.00334068261142),(1.,0.857224384599071,1.00614605678498),
(1.,0.789033595401665,1.00908146323687)))
REPRESENTATION_ITEM('')
SURFACE()
);
#3640=(
BOUNDED_SURFACE()
B_SPLINE_SURFACE(3,2,((#434343,#434344,#434345),(#434346,#434347,#434348),
(#434349,#434350,#434351),(#434352,#434353,#434354)),.UNSPECIFIED.,.F.,
 .F.,.F.)
B_SPLINE_SURFACE_WITH_KNOTS((4,4),(3,3),(5.42101086242752E-20,4.88747512969884E-5),
(-0.000215489857847948,1.),.UNSPECIFIED.)
GEOMETRIC_REPRESENTATION_ITEM()
RATIONAL_B_SPLINE_SURFACE(((1.00008945889747,0.792428983985572,1.),(1.00008931610868,
0.792760296061129,1.),(1.00008917172381,0.793095311538201,1.),(1.00008902569103,
0.793434150627827,1.)))
REPRESENTATION_ITEM('')
SURFACE()
);
#3641=(
BOUNDED_SURFACE()
B_SPLINE_SURFACE(3,2,((#434356,#434357,#434358),(#434359,#434360,#434361),
(#434362,#434363,#434364),(#434365,#434366,#434367)),.UNSPECIFIED.,.F.,
 .F.,.F.)
B_SPLINE_SURFACE_WITH_KNOTS((4,4),(3,3),(-5.21974905013086E-6,5.74172395514392E-5),
(-0.00139822857736382,1.0005131236406),.UNSPECIFIED.)
GEOMETRIC_REPRESENTATION_ITEM()
RATIONAL_B_SPLINE_SURFACE(((1.00049256947243,0.823768952244056,1.00018060397847),
(1.00048448215714,0.826662424388351,1.0001776387088),(1.00052427784021,
0.812424361909417,1.00019223006919),(1.00059912365855,0.7856460946328,1.00021967280228)))
REPRESENTATION_ITEM('')
SURFACE()
);
#3642=(
BOUNDED_SURFACE()
B_SPLINE_SURFACE(3,2,((#434371,#434372,#434373),(#434374,#434375,#434376),
(#434377,#434378,#434379),(#434380,#434381,#434382)),.UNSPECIFIED.,.F.,
 .F.,.F.)
B_SPLINE_SURFACE_WITH_KNOTS((4,4),(3,3),(3.22980774337782E-5,9.63764854872257E-5),
(-0.0015432593638368,1.01095292447556),.UNSPECIFIED.)
GEOMETRIC_REPRESENTATION_ITEM()
RATIONAL_B_SPLINE_SURFACE(((1.000235309833,0.922925743796148,1.00168574728333),
(1.00015136166127,0.950422439594208,1.00108434699061),(1.000335743374,0.890029368953928,
1.00240524789551),(1.00054260094225,0.822274473168292,1.00388716464863)))
REPRESENTATION_ITEM('')
SURFACE()
);
#3643=(
BOUNDED_SURFACE()
B_SPLINE_SURFACE(3,2,((#434482,#434483,#434484),(#434485,#434486,#434487),
(#434488,#434489,#434490),(#434491,#434492,#434493)),.UNSPECIFIED.,.F.,
 .F.,.F.)
B_SPLINE_SURFACE_WITH_KNOTS((4,4),(3,3),(-2.16840434497101E-19,0.000101260117256738),
(0.,1.),.UNSPECIFIED.)
GEOMETRIC_REPRESENTATION_ITEM()
RATIONAL_B_SPLINE_SURFACE(((1.,0.796615278835173,1.),(1.,0.795896038055939,
1.),(1.,0.79519335466135,1.),(1.,0.794506193185547,1.)))
REPRESENTATION_ITEM('')
SURFACE()
);
#3644=(
BOUNDED_SURFACE()
B_SPLINE_SURFACE(3,2,((#434531,#434532,#434533),(#434534,#434535,#434536),
(#434537,#434538,#434539),(#434540,#434541,#434542),(#434543,#434544,#434545),
(#434546,#434547,#434548)),.UNSPECIFIED.,.F.,.F.,.F.)
B_SPLINE_SURFACE_WITH_KNOTS((4,2,4),(3,3),(-1.575481281893E-19,1.66936432462289E-5,
3.3387286492458E-5),(0.,1.),.UNSPECIFIED.)
GEOMETRIC_REPRESENTATION_ITEM()
RATIONAL_B_SPLINE_SURFACE(((1.,0.796615278835177,1.),(1.,0.862310524418138,
1.),(1.,0.923774472010511,1.),(1.,0.923983993203433,1.),(1.,0.862574873720957,
1.),(1.,0.796615278835182,1.)))
REPRESENTATION_ITEM('')
SURFACE()
);
#3645=(
BOUNDED_SURFACE()
B_SPLINE_SURFACE(3,2,((#434585,#434586,#434587),(#434588,#434589,#434590),
(#434591,#434592,#434593),(#434594,#434595,#434596)),.UNSPECIFIED.,.F.,
 .F.,.F.)
B_SPLINE_SURFACE_WITH_KNOTS((4,4),(3,3),(0.,0.000101244905251112),(0.,1.),
 .UNSPECIFIED.)
GEOMETRIC_REPRESENTATION_ITEM()
RATIONAL_B_SPLINE_SURFACE(((1.,0.796615278835173,1.),(1.,0.795896146109796,
1.),(1.,0.795193565796497,1.),(1.,0.794506502889903,1.)))
REPRESENTATION_ITEM('')
SURFACE()
);
#3646=(
BOUNDED_SURFACE()
B_SPLINE_SURFACE(3,2,((#434632,#434633,#434634),(#434635,#434636,#434637),
(#434638,#434639,#434640),(#434641,#434642,#434643)),.UNSPECIFIED.,.F.,
 .F.,.F.)
B_SPLINE_SURFACE_WITH_KNOTS((4,4),(3,3),(2.85968127239938E-5,9.24681548475818E-5),
(-0.00167900679475807,1.01130827127815),.UNSPECIFIED.)
GEOMETRIC_REPRESENTATION_ITEM()
RATIONAL_B_SPLINE_SURFACE(((1.00059040895506,0.82218754186681,1.00401468696654),
(1.00036527718319,0.88999009367067,1.00248382673389),(1.00016469515094,
0.950399042257525,1.0011199008251),(1.00025604274118,0.922888044285446,
1.0017410499063)))
REPRESENTATION_ITEM('')
SURFACE()
);
#3647=(
BOUNDED_SURFACE()
B_SPLINE_SURFACE(3,2,((#434647,#434648,#434649),(#434650,#434651,#434652),
(#434653,#434654,#434655),(#434656,#434657,#434658)),.UNSPECIFIED.,.F.,
 .F.,.F.)
B_SPLINE_SURFACE_WITH_KNOTS((4,4),(3,3),(-5.22358356749288E-6,5.74594192424277E-5),
(-0.00127120052068723,1.),.UNSPECIFIED.)
GEOMETRIC_REPRESENTATION_ITEM()
RATIONAL_B_SPLINE_SURFACE(((1.00054449313181,0.785835073638737,1.),(1.0004770776748,
0.81235152635883,1.),(1.00044031788591,0.82681021650626,1.),(1.00044777653323,
0.823876514387234,1.)))
REPRESENTATION_ITEM('')
SURFACE()
);
#3648=(
BOUNDED_SURFACE()
B_SPLINE_SURFACE(3,2,((#434660,#434661,#434662),(#434663,#434664,#434665),
(#434666,#434667,#434668),(#434669,#434670,#434671)),.UNSPECIFIED.,.F.,
 .F.,.F.)
B_SPLINE_SURFACE_WITH_KNOTS((4,4),(3,3),(-5.42101086242752E-19,4.8874751296988E-5),
(-0.000215805215632062,1.),.UNSPECIFIED.)
GEOMETRIC_REPRESENTATION_ITEM()
RATIONAL_B_SPLINE_SURFACE(((1.00008915600344,0.793434085499716,1.),(1.00008930224997,
0.793095246303267,1.),(1.00008944684619,0.792760230720526,1.),(1.00008958984399,
0.792428918540563,1.)))
REPRESENTATION_ITEM('')
SURFACE()
);
#3649=(
BOUNDED_SURFACE()
B_SPLINE_SURFACE(3,2,((#434673,#434674,#434675),(#434676,#434677,#434678),
(#434679,#434680,#434681),(#434682,#434683,#434684),(#434685,#434686,#434687),
(#434688,#434689,#434690)),.UNSPECIFIED.,.F.,.F.,.F.)
B_SPLINE_SURFACE_WITH_KNOTS((4,2,4),(3,3),(4.60785923306339E-19,7.62675010863196E-5,
0.000152535002172639),(0.,1.02152348203067),.UNSPECIFIED.)
GEOMETRIC_REPRESENTATION_ITEM()
RATIONAL_B_SPLINE_SURFACE(((1.,0.789033595401251,1.00908146323691),(1.,
0.85707178105489,1.00615262590428),(1.,0.922087264710668,1.00335390671592),
(1.,0.922394466502437,1.00334068261143),(1.,0.857224384599004,1.006146056785),
(1.,0.789033595401654,1.0090814632369)))
REPRESENTATION_ITEM('')
SURFACE()
);
#3650=(
BOUNDED_SURFACE()
B_SPLINE_SURFACE(3,2,((#434692,#434693,#434694),(#434695,#434696,#434697),
(#434698,#434699,#434700),(#434701,#434702,#434703)),.UNSPECIFIED.,.F.,
 .F.,.F.)
B_SPLINE_SURFACE_WITH_KNOTS((4,4),(3,3),(1.0842021724855E-19,4.88747512969884E-5),
(-0.000215489857023976,1.),.UNSPECIFIED.)
GEOMETRIC_REPRESENTATION_ITEM()
RATIONAL_B_SPLINE_SURFACE(((1.00008945889713,0.792428983985749,1.),(1.00008931610834,
0.792760296061302,1.),(1.00008917172347,0.793095311538355,1.),(1.00008902569069,
0.793434150627999,1.)))
REPRESENTATION_ITEM('')
SURFACE()
);
#3651=(
BOUNDED_SURFACE()
B_SPLINE_SURFACE(3,2,((#434705,#434706,#434707),(#434708,#434709,#434710),
(#434711,#434712,#434713),(#434714,#434715,#434716)),.UNSPECIFIED.,.F.,
 .F.,.F.)
B_SPLINE_SURFACE_WITH_KNOTS((4,4),(3,3),(-5.21974905013105E-6,5.74172395514412E-5),
(-0.001398228577509,1.00051312364061),.UNSPECIFIED.)
GEOMETRIC_REPRESENTATION_ITEM()
RATIONAL_B_SPLINE_SURFACE(((1.00049256947249,0.823768952244033,1.00018060397847),
(1.00048448215719,0.82666242438832,1.0001776387088),(1.00052427784027,0.812424361909404,
1.00019223006919),(1.00059912365861,0.785646094632767,1.00021967280229)))
REPRESENTATION_ITEM('')
SURFACE()
);
#3652=(
BOUNDED_SURFACE()
B_SPLINE_SURFACE(3,2,((#434720,#434721,#434722),(#434723,#434724,#434725),
(#434726,#434727,#434728),(#434729,#434730,#434731)),.UNSPECIFIED.,.F.,
 .F.,.F.)
B_SPLINE_SURFACE_WITH_KNOTS((4,4),(3,3),(3.22980774337781E-5,9.63764854872249E-5),
(-0.00154325936313331,1.01095292447533),.UNSPECIFIED.)
GEOMETRIC_REPRESENTATION_ITEM()
RATIONAL_B_SPLINE_SURFACE(((1.0002353098329,0.922925743796218,1.00168574728329),
(1.0001513616612,0.950422439594243,1.00108434699059),(1.00033574337385,
0.890029368954043,1.00240524789545),(1.000542600942,0.822274473168454,1.00388716464855)))
REPRESENTATION_ITEM('')
SURFACE()
);
#3653=(
BOUNDED_SURFACE()
B_SPLINE_SURFACE(3,2,((#434831,#434832,#434833),(#434834,#434835,#434836),
(#434837,#434838,#434839),(#434840,#434841,#434842)),.UNSPECIFIED.,.F.,
 .F.,.F.)
B_SPLINE_SURFACE_WITH_KNOTS((4,4),(3,3),(0.,0.000101260117256738),(0.,1.),
 .UNSPECIFIED.)
GEOMETRIC_REPRESENTATION_ITEM()
RATIONAL_B_SPLINE_SURFACE(((1.,0.796615278835171,1.),(1.,0.795896038055938,
1.),(1.,0.795193354661344,1.),(1.,0.794506193185546,1.)))
REPRESENTATION_ITEM('')
SURFACE()
);
#3654=(
BOUNDED_SURFACE()
B_SPLINE_SURFACE(3,2,((#434880,#434881,#434882),(#434883,#434884,#434885),
(#434886,#434887,#434888),(#434889,#434890,#434891),(#434892,#434893,#434894),
(#434895,#434896,#434897)),.UNSPECIFIED.,.F.,.F.,.F.)
B_SPLINE_SURFACE_WITH_KNOTS((4,2,4),(3,3),(-3.89635155736978E-20,1.66936432462297E-5,
3.33872864924594E-5),(0.,1.),.UNSPECIFIED.)
GEOMETRIC_REPRESENTATION_ITEM()
RATIONAL_B_SPLINE_SURFACE(((1.,0.796615278835171,1.),(1.,0.862310524418127,
1.),(1.,0.923774472010524,1.),(1.,0.923983993203424,1.),(1.,0.862574873720943,
1.),(1.,0.796615278835183,1.)))
REPRESENTATION_ITEM('')
SURFACE()
);
#3655=(
BOUNDED_SURFACE()
B_SPLINE_SURFACE(3,2,((#434934,#434935,#434936),(#434937,#434938,#434939),
(#434940,#434941,#434942),(#434943,#434944,#434945)),.UNSPECIFIED.,.F.,
 .F.,.F.)
B_SPLINE_SURFACE_WITH_KNOTS((4,4),(3,3),(0.,0.000101244905251112),(0.,1.),
 .UNSPECIFIED.)
GEOMETRIC_REPRESENTATION_ITEM()
RATIONAL_B_SPLINE_SURFACE(((1.,0.796615278835171,1.),(1.,0.795896146109796,
1.),(1.,0.795193565796499,1.),(1.,0.794506502889901,1.)))
REPRESENTATION_ITEM('')
SURFACE()
);
#3656=(
BOUNDED_SURFACE()
B_SPLINE_SURFACE(3,2,((#434981,#434982,#434983),(#434984,#434985,#434986),
(#434987,#434988,#434989),(#434990,#434991,#434992)),.UNSPECIFIED.,.F.,
 .F.,.F.)
B_SPLINE_SURFACE_WITH_KNOTS((4,4),(3,3),(2.85968127239939E-5,9.24681548475815E-5),
(-0.00167900678695995,1.01130827127814),.UNSPECIFIED.)
GEOMETRIC_REPRESENTATION_ITEM()
RATIONAL_B_SPLINE_SURFACE(((1.00059040895231,0.822187541868214,1.00401468696654),
(1.00036527718149,0.88999009367153,1.00248382673389),(1.00016469515017,
0.950399042257915,1.0011199008251),(1.00025604273999,0.922888044286055,
1.0017410499063)))
REPRESENTATION_ITEM('')
SURFACE()
);
#3657=(
BOUNDED_SURFACE()
B_SPLINE_SURFACE(3,2,((#434996,#434997,#434998),(#434999,#435000,#435001),
(#435002,#435003,#435004),(#435005,#435006,#435007)),.UNSPECIFIED.,.F.,
 .F.,.F.)
B_SPLINE_SURFACE_WITH_KNOTS((4,4),(3,3),(-5.2235835674929E-6,5.74594192424278E-5),
(-0.00127120052009694,1.),.UNSPECIFIED.)
GEOMETRIC_REPRESENTATION_ITEM()
RATIONAL_B_SPLINE_SURFACE(((1.00054449313155,0.785835073638853,1.),(1.00047707767458,
0.812351526358946,1.),(1.00044031788571,0.826810216506354,1.),(1.00044777653302,
0.823876514387337,1.)))
REPRESENTATION_ITEM('')
SURFACE()
);
#3658=(
BOUNDED_SURFACE()
B_SPLINE_SURFACE(3,2,((#435009,#435010,#435011),(#435012,#435013,#435014),
(#435015,#435016,#435017),(#435018,#435019,#435020)),.UNSPECIFIED.,.F.,
 .F.,.F.)
B_SPLINE_SURFACE_WITH_KNOTS((4,4),(3,3),(-3.79470760369927E-19,4.8874751296988E-5),
(-0.000215805215000492,1.),.UNSPECIFIED.)
GEOMETRIC_REPRESENTATION_ITEM()
RATIONAL_B_SPLINE_SURFACE(((1.00008915600318,0.793434085499843,1.),(1.00008930224971,
0.793095246303396,1.),(1.00008944684593,0.792760230720653,1.),(1.00008958984372,
0.792428918540692,1.)))
REPRESENTATION_ITEM('')
SURFACE()
);
#3659=(
BOUNDED_SURFACE()
B_SPLINE_SURFACE(3,2,((#435022,#435023,#435024),(#435025,#435026,#435027),
(#435028,#435029,#435030),(#435031,#435032,#435033),(#435034,#435035,#435036),
(#435037,#435038,#435039)),.UNSPECIFIED.,.F.,.F.,.F.)
B_SPLINE_SURFACE_WITH_KNOTS((4,2,4),(3,3),(4.26904605416167E-19,7.62675010863201E-5,
0.00015253500217264),(0.,1.0215234820307),.UNSPECIFIED.)
GEOMETRIC_REPRESENTATION_ITEM()
RATIONAL_B_SPLINE_SURFACE(((1.,0.789033595401245,1.00908146323693),(1.,
0.857071781054831,1.00615262590429),(1.,0.922087264710729,1.00335390671592),
(1.,0.92239446650237,1.00334068261144),(1.,0.857224384599049,1.00614605678501),
(1.,0.789033595401646,1.00908146323691)))
REPRESENTATION_ITEM('')
SURFACE()
);
#3660=(
BOUNDED_SURFACE()
B_SPLINE_SURFACE(3,2,((#435041,#435042,#435043),(#435044,#435045,#435046),
(#435047,#435048,#435049),(#435050,#435051,#435052)),.UNSPECIFIED.,.F.,
 .F.,.F.)
B_SPLINE_SURFACE_WITH_KNOTS((4,4),(3,3),(1.0842021724855E-19,4.88747512969882E-5),
(-0.000215489857076501,1.),.UNSPECIFIED.)
GEOMETRIC_REPRESENTATION_ITEM()
RATIONAL_B_SPLINE_SURFACE(((1.00008945889715,0.792428983985737,1.),(1.00008931610836,
0.792760296061283,1.),(1.00008917172349,0.793095311538362,1.),(1.00008902569072,
0.793434150627989,1.)))
REPRESENTATION_ITEM('')
SURFACE()
);
#3661=(
BOUNDED_SURFACE()
B_SPLINE_SURFACE(3,2,((#435054,#435055,#435056),(#435057,#435058,#435059),
(#435060,#435061,#435062),(#435063,#435064,#435065)),.UNSPECIFIED.,.F.,
 .F.,.F.)
B_SPLINE_SURFACE_WITH_KNOTS((4,4),(3,3),(-5.21974905013086E-6,5.74172395514395E-5),
(-0.00139822857795002,1.00051312364059),.UNSPECIFIED.)
GEOMETRIC_REPRESENTATION_ITEM()
RATIONAL_B_SPLINE_SURFACE(((1.00049256947264,0.823768952243958,1.00018060397847),
(1.00048448215734,0.826662424388247,1.0001776387088),(1.00052427784043,
0.812424361909319,1.00019223006918),(1.0005991236588,0.785646094632676,
1.00021967280228)))
REPRESENTATION_ITEM('')
SURFACE()
);
#3662=(
BOUNDED_SURFACE()
B_SPLINE_SURFACE(3,2,((#435069,#435070,#435071),(#435072,#435073,#435074),
(#435075,#435076,#435077),(#435078,#435079,#435080)),.UNSPECIFIED.,.F.,
 .F.,.F.)
B_SPLINE_SURFACE_WITH_KNOTS((4,4),(3,3),(3.22980774337779E-5,9.63764854872253E-5),
(-0.00154325936359312,1.01095292447535),.UNSPECIFIED.)
GEOMETRIC_REPRESENTATION_ITEM()
RATIONAL_B_SPLINE_SURFACE(((1.00023530983297,0.922925743796184,1.0016857472833),
(1.00015136166124,0.950422439594233,1.00108434699059),(1.00033574337395,
0.890029368953977,1.00240524789546),(1.00054260094216,0.82227447316838,
1.00388716464855)))
REPRESENTATION_ITEM('')
SURFACE()
);
#3663=(
BOUNDED_SURFACE()
B_SPLINE_SURFACE(3,2,((#435180,#435181,#435182),(#435183,#435184,#435185),
(#435186,#435187,#435188),(#435189,#435190,#435191)),.UNSPECIFIED.,.F.,
 .F.,.F.)
B_SPLINE_SURFACE_WITH_KNOTS((4,4),(3,3),(0.,0.000101260117256738),(0.,1.),
 .UNSPECIFIED.)
GEOMETRIC_REPRESENTATION_ITEM()
RATIONAL_B_SPLINE_SURFACE(((1.,0.796615278835172,1.),(1.,0.795896038055935,
1.),(1.,0.79519335466135,1.),(1.,0.794506193185544,1.)))
REPRESENTATION_ITEM('')
SURFACE()
);
#3664=(
BOUNDED_SURFACE()
B_SPLINE_SURFACE(3,2,((#435229,#435230,#435231),(#435232,#435233,#435234),
(#435235,#435236,#435237),(#435238,#435239,#435240),(#435241,#435242,#435243),
(#435244,#435245,#435246)),.UNSPECIFIED.,.F.,.F.,.F.)
B_SPLINE_SURFACE_WITH_KNOTS((4,2,4),(3,3),(1.06726151354042E-19,1.66936432462295E-5,
3.3387286492459E-5),(0.,1.),.UNSPECIFIED.)
GEOMETRIC_REPRESENTATION_ITEM()
RATIONAL_B_SPLINE_SURFACE(((1.,0.796615278835174,1.),(1.,0.86231052441814,
1.),(1.,0.92377447201052,1.),(1.,0.923983993203425,1.),(1.,0.862574873720945,
1.),(1.,0.79661527883518,1.)))
REPRESENTATION_ITEM('')
SURFACE()
);
#3665=(
BOUNDED_SURFACE()
B_SPLINE_SURFACE(3,2,((#435283,#435284,#435285),(#435286,#435287,#435288),
(#435289,#435290,#435291),(#435292,#435293,#435294)),.UNSPECIFIED.,.F.,
 .F.,.F.)
B_SPLINE_SURFACE_WITH_KNOTS((4,4),(3,3),(-2.16840434497101E-19,0.000101244905251112),
(0.,1.),.UNSPECIFIED.)
GEOMETRIC_REPRESENTATION_ITEM()
RATIONAL_B_SPLINE_SURFACE(((1.,0.79661527883517,1.),(1.,0.795896146109793,
1.),(1.,0.795193565796497,1.),(1.,0.794506502889899,1.)))
REPRESENTATION_ITEM('')
SURFACE()
);
#3666=(
BOUNDED_SURFACE()
B_SPLINE_SURFACE(3,2,((#435330,#435331,#435332),(#435333,#435334,#435335),
(#435336,#435337,#435338),(#435339,#435340,#435341)),.UNSPECIFIED.,.F.,
 .F.,.F.)
B_SPLINE_SURFACE_WITH_KNOTS((4,4),(3,3),(2.85968127239939E-5,9.24681548475817E-5),
(-0.00167900678672043,1.01130827127829),.UNSPECIFIED.)
GEOMETRIC_REPRESENTATION_ITEM()
RATIONAL_B_SPLINE_SURFACE(((1.00059040895223,0.82218754186823,1.00401468696659),
(1.00036527718143,0.889990093671546,1.00248382673392),(1.00016469515015,
0.950399042257917,1.00111990082511),(1.00025604273995,0.922888044286061,
1.00174104990632)))
REPRESENTATION_ITEM('')
SURFACE()
);
#3667=(
BOUNDED_SURFACE()
B_SPLINE_SURFACE(3,2,((#435345,#435346,#435347),(#435348,#435349,#435350),
(#435351,#435352,#435353),(#435354,#435355,#435356)),.UNSPECIFIED.,.F.,
 .F.,.F.)
B_SPLINE_SURFACE_WITH_KNOTS((4,4),(3,3),(-5.22358356749122E-6,5.74594192424277E-5),
(-0.00127120052070634,1.),.UNSPECIFIED.)
GEOMETRIC_REPRESENTATION_ITEM()
RATIONAL_B_SPLINE_SURFACE(((1.00054449313181,0.785835073638735,0.999999999999999),
(1.0004770776748,0.812351526358825,1.),(1.00044031788592,0.826810216506249,
1.),(1.00044777653324,0.82387651438723,1.)))
REPRESENTATION_ITEM('')
SURFACE()
);
#3668=(
BOUNDED_SURFACE()
B_SPLINE_SURFACE(3,2,((#435358,#435359,#435360),(#435361,#435362,#435363),
(#435364,#435365,#435366),(#435367,#435368,#435369)),.UNSPECIFIED.,.F.,
 .F.,.F.)
B_SPLINE_SURFACE_WITH_KNOTS((4,4),(3,3),(-2.16840434497101E-19,4.88747512969878E-5),
(-0.00021580521512041,1.),.UNSPECIFIED.)
GEOMETRIC_REPRESENTATION_ITEM()
RATIONAL_B_SPLINE_SURFACE(((1.00008915600323,0.793434085499819,1.),(1.00008930224976,
0.79309524630335,1.),(1.00008944684598,0.792760230720642,1.),(1.00008958984377,
0.792428918540667,1.)))
REPRESENTATION_ITEM('')
SURFACE()
);
#3669=(
BOUNDED_SURFACE()
B_SPLINE_SURFACE(3,2,((#435371,#435372,#435373),(#435374,#435375,#435376),
(#435377,#435378,#435379),(#435380,#435381,#435382),(#435383,#435384,#435385),
(#435386,#435387,#435388)),.UNSPECIFIED.,.F.,.F.,.F.)
B_SPLINE_SURFACE_WITH_KNOTS((4,2,4),(3,3),(-1.15196480826585E-19,7.62675010863196E-5,
0.000152535002172639),(0.,1.02152348203041),.UNSPECIFIED.)
GEOMETRIC_REPRESENTATION_ITEM()
RATIONAL_B_SPLINE_SURFACE(((1.,0.789033595401306,1.0090814632368),(1.,0.85707178105488,
1.00615262590421),(1.,0.922087264710749,1.00335390671588),(1.,0.922394466502395,
1.00334068261139),(1.,0.857224384599093,1.00614605678492),(1.,0.789033595401704,
1.00908146323678)))
REPRESENTATION_ITEM('')
SURFACE()
);
#3670=(
BOUNDED_SURFACE()
B_SPLINE_SURFACE(3,2,((#435390,#435391,#435392),(#435393,#435394,#435395),
(#435396,#435397,#435398),(#435399,#435400,#435401)),.UNSPECIFIED.,.F.,
 .F.,.F.)
B_SPLINE_SURFACE_WITH_KNOTS((4,4),(3,3),(2.98155597433514E-19,4.88747512969883E-5),
(-0.000215489856871959,1.),.UNSPECIFIED.)
GEOMETRIC_REPRESENTATION_ITEM()
RATIONAL_B_SPLINE_SURFACE(((1.00008945889706,0.792428983985777,1.),(1.00008931610828,
0.79276029606132,1.),(1.00008917172341,0.793095311538403,1.),(1.00008902569063,
0.793434150628028,1.)))
REPRESENTATION_ITEM('')
SURFACE()
);
#3671=(
BOUNDED_SURFACE()
B_SPLINE_SURFACE(3,2,((#435403,#435404,#435405),(#435406,#435407,#435408),
(#435409,#435410,#435411),(#435412,#435413,#435414)),.UNSPECIFIED.,.F.,
 .F.,.F.)
B_SPLINE_SURFACE_WITH_KNOTS((4,4),(3,3),(-5.21974905013095E-6,5.74172395514395E-5),
(-0.00139822857774113,1.00051312364093),.UNSPECIFIED.)
GEOMETRIC_REPRESENTATION_ITEM()
RATIONAL_B_SPLINE_SURFACE(((1.00049256947257,0.823768952243928,1.00018060397858),
(1.00048448215727,0.826662424388224,1.00017763870891),(1.00052427784035,
0.812424361909291,1.00019223006931),(1.00059912365871,0.785646094632647,
1.00021967280242)))
REPRESENTATION_ITEM('')
SURFACE()
);
#3672=(
BOUNDED_SURFACE()
B_SPLINE_SURFACE(3,2,((#435418,#435419,#435420),(#435421,#435422,#435423),
(#435424,#435425,#435426),(#435427,#435428,#435429)),.UNSPECIFIED.,.F.,
 .F.,.F.)
B_SPLINE_SURFACE_WITH_KNOTS((4,4),(3,3),(3.22980774337778E-5,9.63764854872251E-5),
(-0.00154325936392601,1.0109529244756),.UNSPECIFIED.)
GEOMETRIC_REPRESENTATION_ITEM()
RATIONAL_B_SPLINE_SURFACE(((1.00023530983302,0.922925743796135,1.00168574728334),
(1.00015136166127,0.950422439594195,1.00108434699061),(1.00033574337402,
0.890029368953922,1.00240524789552),(1.00054260094228,0.822274473168269,
1.00388716464864)))
REPRESENTATION_ITEM('')
SURFACE()
);
#3673=(
BOUNDED_SURFACE()
B_SPLINE_SURFACE(3,2,((#435529,#435530,#435531),(#435532,#435533,#435534),
(#435535,#435536,#435537),(#435538,#435539,#435540)),.UNSPECIFIED.,.F.,
 .F.,.F.)
B_SPLINE_SURFACE_WITH_KNOTS((4,4),(3,3),(-2.16840434497101E-19,0.000101260117256738),
(0.,1.),.UNSPECIFIED.)
GEOMETRIC_REPRESENTATION_ITEM()
RATIONAL_B_SPLINE_SURFACE(((1.,0.796615278835172,1.),(1.,0.795896038055936,
1.),(1.,0.795193354661352,1.),(1.,0.794506193185545,1.)))
REPRESENTATION_ITEM('')
SURFACE()
);
#3674=(
BOUNDED_SURFACE()
B_SPLINE_SURFACE(3,2,((#435578,#435579,#435580),(#435581,#435582,#435583),
(#435584,#435585,#435586),(#435587,#435588,#435589),(#435590,#435591,#435592),
(#435593,#435594,#435595)),.UNSPECIFIED.,.F.,.F.,.F.)
B_SPLINE_SURFACE_WITH_KNOTS((4,2,4),(3,3),(1.77876918923403E-19,1.66936432462295E-5,
3.33872864924589E-5),(0.,1.),.UNSPECIFIED.)
GEOMETRIC_REPRESENTATION_ITEM()
RATIONAL_B_SPLINE_SURFACE(((1.,0.796615278835179,1.),(1.,0.862310524418131,
1.),(1.,0.923774472010521,1.),(1.,0.923983993203423,1.),(1.,0.862574873720948,
1.),(1.,0.796615278835186,1.)))
REPRESENTATION_ITEM('')
SURFACE()
);
#3675=(
BOUNDED_SURFACE()
B_SPLINE_SURFACE(3,2,((#435632,#435633,#435634),(#435635,#435636,#435637),
(#435638,#435639,#435640),(#435641,#435642,#435643)),.UNSPECIFIED.,.F.,
 .F.,.F.)
B_SPLINE_SURFACE_WITH_KNOTS((4,4),(3,3),(-2.16840434497101E-19,0.000101244905251112),
(0.,1.),.UNSPECIFIED.)
GEOMETRIC_REPRESENTATION_ITEM()
RATIONAL_B_SPLINE_SURFACE(((1.,0.79661527883517,1.),(1.,0.795896146109795,
1.),(1.,0.795193565796499,1.),(1.,0.7945065028899,1.)))
REPRESENTATION_ITEM('')
SURFACE()
);
#3676=(
BOUNDED_SURFACE()
B_SPLINE_SURFACE(3,2,((#435679,#435680,#435681),(#435682,#435683,#435684),
(#435685,#435686,#435687),(#435688,#435689,#435690)),.UNSPECIFIED.,.F.,
 .F.,.F.)
B_SPLINE_SURFACE_WITH_KNOTS((4,4),(3,3),(2.85968127239938E-5,9.2468154847582E-5),
(-0.00167900678625328,1.01130827127842),.UNSPECIFIED.)
GEOMETRIC_REPRESENTATION_ITEM()
RATIONAL_B_SPLINE_SURFACE(((1.00059040895207,0.822187541868287,1.00401468696664),
(1.00036527718133,0.889990093671587,1.00248382673395),(1.0001646951501,
0.950399042257936,1.00111990082513),(1.00025604273988,0.922888044286088,
1.00174104990634)))
REPRESENTATION_ITEM('')
SURFACE()
);
#3677=(
BOUNDED_SURFACE()
B_SPLINE_SURFACE(3,2,((#435694,#435695,#435696),(#435697,#435698,#435699),
(#435700,#435701,#435702),(#435703,#435704,#435705)),.UNSPECIFIED.,.F.,
 .F.,.F.)
B_SPLINE_SURFACE_WITH_KNOTS((4,4),(3,3),(-5.22358356749338E-6,5.74594192424277E-5),
(-0.00127120052079804,1.),.UNSPECIFIED.)
GEOMETRIC_REPRESENTATION_ITEM()
RATIONAL_B_SPLINE_SURFACE(((1.00054449313185,0.785835073638721,1.),(1.00047707767484,
0.812351526358789,1.),(1.00044031788595,0.826810216506256,1.),(1.00044777653327,
0.823876514387212,1.)))
REPRESENTATION_ITEM('')
SURFACE()
);
#3678=(
BOUNDED_SURFACE()
B_SPLINE_SURFACE(3,2,((#435707,#435708,#435709),(#435710,#435711,#435712),
(#435713,#435714,#435715),(#435716,#435717,#435718)),.UNSPECIFIED.,.F.,
 .F.,.F.)
B_SPLINE_SURFACE_WITH_KNOTS((4,4),(3,3),(-5.42101086242752E-20,4.8874751296988E-5),
(-0.000215805214956234,1.),.UNSPECIFIED.)
GEOMETRIC_REPRESENTATION_ITEM()
RATIONAL_B_SPLINE_SURFACE(((1.00008915600316,0.793434085499853,1.),(1.00008930224969,
0.793095246303394,1.),(1.00008944684591,0.792760230720669,1.),(1.00008958984371,
0.792428918540704,1.)))
REPRESENTATION_ITEM('')
SURFACE()
);
#3679=(
BOUNDED_SURFACE()
B_SPLINE_SURFACE(3,2,((#435720,#435721,#435722),(#435723,#435724,#435725),
(#435726,#435727,#435728),(#435729,#435730,#435731),(#435732,#435733,#435734),
(#435735,#435736,#435737)),.UNSPECIFIED.,.F.,.F.,.F.)
B_SPLINE_SURFACE_WITH_KNOTS((4,2,4),(3,3),(1.28749007982654E-19,7.62675010863196E-5,
0.000152535002172639),(0.,1.02152348203102),.UNSPECIFIED.)
GEOMETRIC_REPRESENTATION_ITEM()
RATIONAL_B_SPLINE_SURFACE(((1.,0.789033595401182,1.00908146323706),(1.,
0.857071781054781,1.00615262590438),(1.,0.922087264710715,1.00335390671597),
(1.,0.922394466502335,1.00334068261149),(1.,0.857224384599015,1.0061460567851),
(1.,0.789033595401579,1.00908146323704)))
REPRESENTATION_ITEM('')
SURFACE()
);
#3680=(
BOUNDED_SURFACE()
B_SPLINE_SURFACE(3,2,((#435739,#435740,#435741),(#435742,#435743,#435744),
(#435745,#435746,#435747),(#435748,#435749,#435750)),.UNSPECIFIED.,.F.,
 .F.,.F.)
B_SPLINE_SURFACE_WITH_KNOTS((4,4),(3,3),(5.14996031930615E-19,4.88747512969886E-5),
(-0.000215489857762071,1.),.UNSPECIFIED.)
GEOMETRIC_REPRESENTATION_ITEM()
RATIONAL_B_SPLINE_SURFACE(((1.00008945889743,0.792428983985592,1.),(1.00008931610865,
0.792760296061145,1.),(1.00008917172377,0.793095311538216,1.),(1.000089025691,
0.793434150627846,1.)))
REPRESENTATION_ITEM('')
SURFACE()
);
#3681=(
BOUNDED_SURFACE()
B_SPLINE_SURFACE(3,2,((#435752,#435753,#435754),(#435755,#435756,#435757),
(#435758,#435759,#435760),(#435761,#435762,#435763)),.UNSPECIFIED.,.F.,
 .F.,.F.)
B_SPLINE_SURFACE_WITH_KNOTS((4,4),(3,3),(-5.21974905012869E-6,5.74172395514394E-5),
(-0.00139822857793504,1.00051312364104),.UNSPECIFIED.)
GEOMETRIC_REPRESENTATION_ITEM()
RATIONAL_B_SPLINE_SURFACE(((1.00049256947264,0.823768952243878,1.00018060397862),
(1.00048448215734,0.826662424388174,1.00017763870895),(1.00052427784043,
0.812424361909233,1.00019223006935),(1.00059912365879,0.785646094632582,
1.00021967280247)))
REPRESENTATION_ITEM('')
SURFACE()
);
#3682=(
BOUNDED_SURFACE()
B_SPLINE_SURFACE(3,2,((#435767,#435768,#435769),(#435770,#435771,#435772),
(#435773,#435774,#435775),(#435776,#435777,#435778)),.UNSPECIFIED.,.F.,
 .F.,.F.)
B_SPLINE_SURFACE_WITH_KNOTS((4,4),(3,3),(3.22980774337778E-5,9.63764854872257E-5),
(-0.00154325936384009,1.01095292447553),.UNSPECIFIED.)
GEOMETRIC_REPRESENTATION_ITEM()
RATIONAL_B_SPLINE_SURFACE(((1.000235309833,0.922925743796147,1.00168574728333),
(1.00015136166127,0.950422439594206,1.00108434699061),(1.00033574337401,
0.890029368953931,1.0024052478955),(1.00054260094225,0.822274473168301,
1.00388716464862)))
REPRESENTATION_ITEM('')
SURFACE()
);
#3683=(
BOUNDED_SURFACE()
B_SPLINE_SURFACE(3,2,((#435878,#435879,#435880),(#435881,#435882,#435883),
(#435884,#435885,#435886),(#435887,#435888,#435889)),.UNSPECIFIED.,.F.,
 .F.,.F.)
B_SPLINE_SURFACE_WITH_KNOTS((4,4),(3,3),(0.,0.000101260117256737),(0.,1.),
 .UNSPECIFIED.)
GEOMETRIC_REPRESENTATION_ITEM()
RATIONAL_B_SPLINE_SURFACE(((1.,0.796615278835173,1.),(1.,0.795896038055925,
1.),(1.,0.795193354661367,1.),(1.,0.794506193185532,1.)))
REPRESENTATION_ITEM('')
SURFACE()
);
#3684=(
BOUNDED_SURFACE()
B_SPLINE_SURFACE(3,2,((#435927,#435928,#435929),(#435930,#435931,#435932),
(#435933,#435934,#435935),(#435936,#435937,#435938),(#435939,#435940,#435941),
(#435942,#435943,#435944)),.UNSPECIFIED.,.F.,.F.,.F.)
B_SPLINE_SURFACE_WITH_KNOTS((4,2,4),(3,3),(-8.13151629364128E-20,1.66936432462297E-5,
3.33872864924594E-5),(0.,1.),.UNSPECIFIED.)
GEOMETRIC_REPRESENTATION_ITEM()
RATIONAL_B_SPLINE_SURFACE(((1.,0.79661527883517,1.),(1.,0.862310524418116,
1.),(1.,0.923774472010523,1.),(1.,0.923983993203425,1.),(1.,0.86257487372094,
1.),(1.,0.796615278835185,1.)))
REPRESENTATION_ITEM('')
SURFACE()
);
#3685=(
BOUNDED_SURFACE()
B_SPLINE_SURFACE(3,2,((#435981,#435982,#435983),(#435984,#435985,#435986),
(#435987,#435988,#435989),(#435990,#435991,#435992)),.UNSPECIFIED.,.F.,
 .F.,.F.)
B_SPLINE_SURFACE_WITH_KNOTS((4,4),(3,3),(0.,0.000101244905251112),(0.,1.),
 .UNSPECIFIED.)
GEOMETRIC_REPRESENTATION_ITEM()
RATIONAL_B_SPLINE_SURFACE(((1.,0.79661527883517,1.),(1.,0.79589614610979,
1.),(1.,0.795193565796501,1.),(1.,0.7945065028899,1.)))
REPRESENTATION_ITEM('')
SURFACE()
);
#3686=(
BOUNDED_SURFACE()
B_SPLINE_SURFACE(3,2,((#436028,#436029,#436030),(#436031,#436032,#436033),
(#436034,#436035,#436036),(#436037,#436038,#436039)),.UNSPECIFIED.,.F.,
 .F.,.F.)
B_SPLINE_SURFACE_WITH_KNOTS((4,4),(3,3),(2.85968127239939E-5,9.24681548475817E-5),
(-0.00167900678781028,1.01130827127812),.UNSPECIFIED.)
GEOMETRIC_REPRESENTATION_ITEM()
RATIONAL_B_SPLINE_SURFACE(((1.00059040895261,0.822187541868062,1.00401468696653),
(1.00036527718167,0.889990093671442,1.00248382673389),(1.00016469515025,
0.950399042257876,1.0011199008251),(1.00025604274012,0.92288804428599,1.00174104990629)))
REPRESENTATION_ITEM('')
SURFACE()
);
#3687=(
BOUNDED_SURFACE()
B_SPLINE_SURFACE(3,2,((#436043,#436044,#436045),(#436046,#436047,#436048),
(#436049,#436050,#436051),(#436052,#436053,#436054)),.UNSPECIFIED.,.F.,
 .F.,.F.)
B_SPLINE_SURFACE_WITH_KNOTS((4,4),(3,3),(-5.22358356749345E-6,5.74594192424276E-5),
(-0.00127120052056582,1.),.UNSPECIFIED.)
GEOMETRIC_REPRESENTATION_ITEM()
RATIONAL_B_SPLINE_SURFACE(((1.00054449313175,0.785835073638759,1.),(1.00047707767475,
0.812351526358855,1.),(1.00044031788587,0.826810216506281,1.),(1.00044777653319,
0.823876514387254,1.)))
REPRESENTATION_ITEM('')
SURFACE()
);
#3688=(
BOUNDED_SURFACE()
B_SPLINE_SURFACE(3,2,((#436056,#436057,#436058),(#436059,#436060,#436061),
(#436062,#436063,#436064),(#436065,#436066,#436067)),.UNSPECIFIED.,.F.,
 .F.,.F.)
B_SPLINE_SURFACE_WITH_KNOTS((4,4),(3,3),(-2.71050543121376E-19,4.88747512969877E-5),
(-0.000215805215438253,1.),.UNSPECIFIED.)
GEOMETRIC_REPRESENTATION_ITEM()
RATIONAL_B_SPLINE_SURFACE(((1.00008915600336,0.793434085499752,1.),(1.00008930224989,
0.793095246303316,1.),(1.00008944684611,0.792760230720558,1.),(1.00008958984391,
0.792428918540604,1.)))
REPRESENTATION_ITEM('')
SURFACE()
);
#3689=(
BOUNDED_SURFACE()
B_SPLINE_SURFACE(3,2,((#436069,#436070,#436071),(#436072,#436073,#436074),
(#436075,#436076,#436077),(#436078,#436079,#436080),(#436081,#436082,#436083),
(#436084,#436085,#436086)),.UNSPECIFIED.,.F.,.F.,.F.)
B_SPLINE_SURFACE_WITH_KNOTS((4,2,4),(3,3),(2.91379333855479E-19,7.62675010863199E-5,
0.000152535002172639),(0.,1.02152348203046),.UNSPECIFIED.)
GEOMETRIC_REPRESENTATION_ITEM()
RATIONAL_B_SPLINE_SURFACE(((1.,0.789033595401292,1.00908146323682),(1.,
0.857071781054872,1.00615262590422),(1.,0.922087264710747,1.00335390671588),
(1.,0.92239446650239,1.0033406826114),(1.,0.857224384599083,1.00614605678494),
(1.,0.789033595401694,1.0090814632368)))
REPRESENTATION_ITEM('')
SURFACE()
);
#3690=(
BOUNDED_SURFACE()
B_SPLINE_SURFACE(3,2,((#436088,#436089,#436090),(#436091,#436092,#436093),
(#436094,#436095,#436096),(#436097,#436098,#436099)),.UNSPECIFIED.,.F.,
 .F.,.F.)
B_SPLINE_SURFACE_WITH_KNOTS((4,4),(3,3),(3.25260651745651E-19,4.88747512969886E-5),
(-0.000215489857342165,1.),.UNSPECIFIED.)
GEOMETRIC_REPRESENTATION_ITEM()
RATIONAL_B_SPLINE_SURFACE(((1.00008945889726,0.792428983985683,1.),(1.00008931610847,
0.792760296061223,1.),(1.0000891717236,0.793095311538305,1.),(1.00008902569083,
0.793434150627931,1.)))
REPRESENTATION_ITEM('')
SURFACE()
);
#3691=(
BOUNDED_SURFACE()
B_SPLINE_SURFACE(3,2,((#436101,#436102,#436103),(#436104,#436105,#436106),
(#436107,#436108,#436109),(#436110,#436111,#436112)),.UNSPECIFIED.,.F.,
 .F.,.F.)
B_SPLINE_SURFACE_WITH_KNOTS((4,4),(3,3),(-5.21974905012869E-6,5.74172395514397E-5),
(-0.00139822857729007,1.00051312364051),.UNSPECIFIED.)
GEOMETRIC_REPRESENTATION_ITEM()
RATIONAL_B_SPLINE_SURFACE(((1.00049256947241,0.823768952244086,1.00018060397844),
(1.00048448215711,0.826662424388373,1.00017763870877),(1.00052427784018,
0.812424361909455,1.00019223006915),(1.00059912365851,0.785646094632833,
1.00021967280224)))
REPRESENTATION_ITEM('')
SURFACE()
);
#3692=(
BOUNDED_SURFACE()
B_SPLINE_SURFACE(3,2,((#436116,#436117,#436118),(#436119,#436120,#436121),
(#436122,#436123,#436124),(#436125,#436126,#436127)),.UNSPECIFIED.,.F.,
 .F.,.F.)
B_SPLINE_SURFACE_WITH_KNOTS((4,4),(3,3),(3.2298077433778E-5,9.63764854872252E-5),
(-0.00154325936375228,1.01095292447535),.UNSPECIFIED.)
GEOMETRIC_REPRESENTATION_ITEM()
RATIONAL_B_SPLINE_SURFACE(((1.00023530983299,0.922925743796169,1.0016857472833),
(1.00015136166126,0.95042243959422,1.00108434699059),(1.00033574337399,
0.890029368953975,1.00240524789546),(1.00054260094222,0.822274473168344,
1.00388716464855)))
REPRESENTATION_ITEM('')
SURFACE()
);
#3693=(
BOUNDED_SURFACE()
B_SPLINE_SURFACE(3,2,((#436227,#436228,#436229),(#436230,#436231,#436232),
(#436233,#436234,#436235),(#436236,#436237,#436238)),.UNSPECIFIED.,.F.,
 .F.,.F.)
B_SPLINE_SURFACE_WITH_KNOTS((4,4),(3,3),(0.,0.000101260117256738),(0.,1.),
 .UNSPECIFIED.)
GEOMETRIC_REPRESENTATION_ITEM()
RATIONAL_B_SPLINE_SURFACE(((1.,0.79661527883517,1.),(1.,0.795896038055943,
1.),(1.,0.795193354661343,1.),(1.,0.794506193185546,1.)))
REPRESENTATION_ITEM('')
SURFACE()
);
#3694=(
BOUNDED_SURFACE()
B_SPLINE_SURFACE(3,2,((#436276,#436277,#436278),(#436279,#436280,#436281),
(#436282,#436283,#436284),(#436285,#436286,#436287),(#436288,#436289,#436290),
(#436291,#436292,#436293)),.UNSPECIFIED.,.F.,.F.,.F.)
B_SPLINE_SURFACE_WITH_KNOTS((4,2,4),(3,3),(-1.10114283143059E-19,1.66936432462291E-5,
3.33872864924584E-5),(0.,1.),.UNSPECIFIED.)
GEOMETRIC_REPRESENTATION_ITEM()
RATIONAL_B_SPLINE_SURFACE(((1.,0.796615278835174,1.),(1.,0.86231052441814,
1.),(1.,0.92377447201052,1.),(1.,0.923983993203428,1.),(1.,0.862574873720945,
1.),(1.,0.796615278835184,1.)))
REPRESENTATION_ITEM('')
SURFACE()
);
#3695=(
BOUNDED_SURFACE()
B_SPLINE_SURFACE(3,2,((#436330,#436331,#436332),(#436333,#436334,#436335),
(#436336,#436337,#436338),(#436339,#436340,#436341)),.UNSPECIFIED.,.F.,
 .F.,.F.)
B_SPLINE_SURFACE_WITH_KNOTS((4,4),(3,3),(-2.16840434497101E-19,0.000101244905251112),
(0.,1.),.UNSPECIFIED.)
GEOMETRIC_REPRESENTATION_ITEM()
RATIONAL_B_SPLINE_SURFACE(((1.,0.796615278835169,1.),(1.,0.795896146109785,
1.),(1.,0.795193565796503,1.),(1.,0.794506502889899,1.)))
REPRESENTATION_ITEM('')
SURFACE()
);
#3696=(
BOUNDED_SURFACE()
B_SPLINE_SURFACE(3,2,((#436377,#436378,#436379),(#436380,#436381,#436382),
(#436383,#436384,#436385),(#436386,#436387,#436388)),.UNSPECIFIED.,.F.,
 .F.,.F.)
B_SPLINE_SURFACE_WITH_KNOTS((4,4),(3,3),(2.85968127239939E-5,9.24681548475814E-5),
(-0.00167900678689317,1.01130827127832),.UNSPECIFIED.)
GEOMETRIC_REPRESENTATION_ITEM()
RATIONAL_B_SPLINE_SURFACE(((1.00059040895229,0.822187541868193,1.0040146869666),
(1.00036527718147,0.889990093671525,1.00248382673393),(1.00016469515016,
0.950399042257908,1.00111990082512),(1.00025604273998,0.922888044286044,
1.00174104990633)))
REPRESENTATION_ITEM('')
SURFACE()
);
#3697=(
BOUNDED_SURFACE()
B_SPLINE_SURFACE(3,2,((#436392,#436393,#436394),(#436395,#436396,#436397),
(#436398,#436399,#436400),(#436401,#436402,#436403)),.UNSPECIFIED.,.F.,
 .F.,.F.)
B_SPLINE_SURFACE_WITH_KNOTS((4,4),(3,3),(-5.22358356749165E-6,5.74594192424277E-5),
(-0.00127120052054818,1.),.UNSPECIFIED.)
GEOMETRIC_REPRESENTATION_ITEM()
RATIONAL_B_SPLINE_SURFACE(((1.00054449313175,0.785835073638764,1.),(1.00047707767475,
0.812351526358859,1.),(1.00044031788586,0.826810216506276,1.),(1.00044777653318,
0.823876514387259,1.)))
REPRESENTATION_ITEM('')
SURFACE()
);
#3698=(
BOUNDED_SURFACE()
B_SPLINE_SURFACE(3,2,((#436405,#436406,#436407),(#436408,#436409,#436410),
(#436411,#436412,#436413),(#436414,#436415,#436416)),.UNSPECIFIED.,.F.,
 .F.,.F.)
B_SPLINE_SURFACE_WITH_KNOTS((4,4),(3,3),(-2.98155597433514E-19,4.88747512969879E-5),
(-0.00021580521504422,1.),.UNSPECIFIED.)
GEOMETRIC_REPRESENTATION_ITEM()
RATIONAL_B_SPLINE_SURFACE(((1.0000891560032,0.793434085499835,1.),(1.00008930224973,
0.793095246303373,1.),(1.00008944684595,0.792760230720652,1.),(1.00008958984374,
0.792428918540684,1.)))
REPRESENTATION_ITEM('')
SURFACE()
);
#3699=(
BOUNDED_SURFACE()
B_SPLINE_SURFACE(3,2,((#436418,#436419,#436420),(#436421,#436422,#436423),
(#436424,#436425,#436426),(#436427,#436428,#436429),(#436430,#436431,#436432),
(#436433,#436434,#436435)),.UNSPECIFIED.,.F.,.F.,.F.)
B_SPLINE_SURFACE_WITH_KNOTS((4,2,4),(3,3),(0.,7.62675010863195E-5,0.000152535002172639),
(0.,1.02152348203079),.UNSPECIFIED.)
GEOMETRIC_REPRESENTATION_ITEM()
RATIONAL_B_SPLINE_SURFACE(((1.,0.789033595401228,1.00908146323696),(1.,
0.857071781054826,1.00615262590432),(1.,0.922087264710717,1.00335390671594),
(1.,0.922394466502367,1.00334068261145),(1.,0.857224384599037,1.00614605678503),
(1.,0.789033595401621,1.00908146323695)))
REPRESENTATION_ITEM('')
SURFACE()
);
#3700=(
BOUNDED_SURFACE()
B_SPLINE_SURFACE(3,2,((#436437,#436438,#436439),(#436440,#436441,#436442),
(#436443,#436444,#436445),(#436446,#436447,#436448)),.UNSPECIFIED.,.F.,
 .F.,.F.)
B_SPLINE_SURFACE_WITH_KNOTS((4,4),(3,3),(1.0842021724855E-19,4.88747512969883E-5),
(-0.000215489857070327,1.),.UNSPECIFIED.)
GEOMETRIC_REPRESENTATION_ITEM()
RATIONAL_B_SPLINE_SURFACE(((1.00008945889715,0.792428983985738,1.),(1.00008931610836,
0.792760296061282,1.),(1.00008917172349,0.793095311538351,1.),(1.00008902569071,
0.793434150627988,1.)))
REPRESENTATION_ITEM('')
SURFACE()
);
#3701=(
BOUNDED_SURFACE()
B_SPLINE_SURFACE(3,2,((#436450,#436451,#436452),(#436453,#436454,#436455),
(#436456,#436457,#436458),(#436459,#436460,#436461)),.UNSPECIFIED.,.F.,
 .F.,.F.)
B_SPLINE_SURFACE_WITH_KNOTS((4,4),(3,3),(-5.21974905013086E-6,5.74172395514391E-5),
(-0.00139822857771562,1.00051312364077),.UNSPECIFIED.)
GEOMETRIC_REPRESENTATION_ITEM()
RATIONAL_B_SPLINE_SURFACE(((1.00049256947256,0.823768952243966,1.00018060397853),
(1.00048448215726,0.826662424388255,1.00017763870886),(1.00052427784034,
0.812424361909324,1.00019223006925),(1.0005991236587,0.78564609463269,1.00021967280235)))
REPRESENTATION_ITEM('')
SURFACE()
);
#3702=(
BOUNDED_SURFACE()
B_SPLINE_SURFACE(3,2,((#436465,#436466,#436467),(#436468,#436469,#436470),
(#436471,#436472,#436473),(#436474,#436475,#436476)),.UNSPECIFIED.,.F.,
 .F.,.F.)
B_SPLINE_SURFACE_WITH_KNOTS((4,4),(3,3),(3.22980774337782E-5,9.63764854872247E-5),
(-0.00154325936386019,1.0109529244756),.UNSPECIFIED.)
GEOMETRIC_REPRESENTATION_ITEM()
RATIONAL_B_SPLINE_SURFACE(((1.00023530983301,0.922925743796141,1.00168574728334),
(1.00015136166127,0.950422439594195,1.00108434699061),(1.00033574337401,
0.890029368953938,1.00240524789551),(1.00054260094226,0.822274473168278,
1.00388716464864)))
REPRESENTATION_ITEM('')
SURFACE()
);
#3703=(
BOUNDED_SURFACE()
B_SPLINE_SURFACE(3,2,((#436576,#436577,#436578),(#436579,#436580,#436581),
(#436582,#436583,#436584),(#436585,#436586,#436587)),.UNSPECIFIED.,.F.,
 .F.,.F.)
B_SPLINE_SURFACE_WITH_KNOTS((4,4),(3,3),(-2.16840434497101E-19,0.000101260117256737),
(0.,1.),.UNSPECIFIED.)
GEOMETRIC_REPRESENTATION_ITEM()
RATIONAL_B_SPLINE_SURFACE(((1.,0.796615278835171,1.),(1.,0.79589603805593,
1.),(1.,0.795193354661352,1.),(1.,0.794506193185539,1.)))
REPRESENTATION_ITEM('')
SURFACE()
);
#3704=(
BOUNDED_SURFACE()
B_SPLINE_SURFACE(3,2,((#436625,#436626,#436627),(#436628,#436629,#436630),
(#436631,#436632,#436633),(#436634,#436635,#436636),(#436637,#436638,#436639),
(#436640,#436641,#436642)),.UNSPECIFIED.,.F.,.F.,.F.)
B_SPLINE_SURFACE_WITH_KNOTS((4,2,4),(3,3),(7.28448334638698E-20,1.66936432462294E-5,
3.33872864924587E-5),(0.,1.),.UNSPECIFIED.)
GEOMETRIC_REPRESENTATION_ITEM()
RATIONAL_B_SPLINE_SURFACE(((1.,0.796615278835177,1.),(1.,0.862310524418129,
1.),(1.,0.923774472010524,1.),(1.,0.923983993203422,1.),(1.,0.862574873720948,
1.),(1.,0.796615278835187,1.)))
REPRESENTATION_ITEM('')
SURFACE()
);
#3705=(
BOUNDED_SURFACE()
B_SPLINE_SURFACE(3,2,((#436679,#436680,#436681),(#436682,#436683,#436684),
(#436685,#436686,#436687),(#436688,#436689,#436690)),.UNSPECIFIED.,.F.,
 .F.,.F.)
B_SPLINE_SURFACE_WITH_KNOTS((4,4),(3,3),(2.16840434497101E-19,0.000101244905251112),
(0.,1.),.UNSPECIFIED.)
GEOMETRIC_REPRESENTATION_ITEM()
RATIONAL_B_SPLINE_SURFACE(((1.,0.796615278835172,1.),(1.,0.79589614610979,
1.),(1.,0.795193565796502,1.),(1.,0.794506502889901,1.)))
REPRESENTATION_ITEM('')
SURFACE()
);
#3706=(
BOUNDED_SURFACE()
B_SPLINE_SURFACE(3,2,((#436726,#436727,#436728),(#436729,#436730,#436731),
(#436732,#436733,#436734),(#436735,#436736,#436737)),.UNSPECIFIED.,.F.,
 .F.,.F.)
B_SPLINE_SURFACE_WITH_KNOTS((4,4),(3,3),(2.85968127239939E-5,9.24681548475817E-5),
(-0.00167900678662011,1.01130827127831),.UNSPECIFIED.)
GEOMETRIC_REPRESENTATION_ITEM()
RATIONAL_B_SPLINE_SURFACE(((1.00059040895219,0.822187541868238,1.0040146869666),
(1.00036527718141,0.889990093671566,1.00248382673393),(1.00016469515014,
0.950399042257916,1.00111990082512),(1.00025604273994,0.922888044286067,
1.00174104990632)))
REPRESENTATION_ITEM('')
SURFACE()
);
#3707=(
BOUNDED_SURFACE()
B_SPLINE_SURFACE(3,2,((#436741,#436742,#436743),(#436744,#436745,#436746),
(#436747,#436748,#436749),(#436750,#436751,#436752)),.UNSPECIFIED.,.F.,
 .F.,.F.)
B_SPLINE_SURFACE_WITH_KNOTS((4,4),(3,3),(-5.22358356749333E-6,5.74594192424276E-5),
(-0.00127120052061989,1.),.UNSPECIFIED.)
GEOMETRIC_REPRESENTATION_ITEM()
RATIONAL_B_SPLINE_SURFACE(((1.00054449313178,0.785835073638753,1.),(1.00047707767477,
0.812351526358838,1.),(1.00044031788589,0.826810216506273,1.),(1.00044777653321,
0.823876514387244,1.)))
REPRESENTATION_ITEM('')
SURFACE()
);
#3708=(
BOUNDED_SURFACE()
B_SPLINE_SURFACE(3,2,((#436754,#436755,#436756),(#436757,#436758,#436759),
(#436760,#436761,#436762),(#436763,#436764,#436765)),.UNSPECIFIED.,.F.,
 .F.,.F.)
B_SPLINE_SURFACE_WITH_KNOTS((4,4),(3,3),(5.42101086242752E-20,4.88747512969881E-5),
(-0.000215805215480362,1.),.UNSPECIFIED.)
GEOMETRIC_REPRESENTATION_ITEM()
RATIONAL_B_SPLINE_SURFACE(((1.00008915600338,0.793434085499743,1.),(1.00008930224991,
0.793095246303286,1.),(1.00008944684613,0.792760230720563,1.),(1.00008958984392,
0.792428918540595,1.)))
REPRESENTATION_ITEM('')
SURFACE()
);
#3709=(
BOUNDED_SURFACE()
B_SPLINE_SURFACE(3,2,((#436767,#436768,#436769),(#436770,#436771,#436772),
(#436773,#436774,#436775),(#436776,#436777,#436778),(#436779,#436780,#436781),
(#436782,#436783,#436784)),.UNSPECIFIED.,.F.,.F.,.F.)
B_SPLINE_SURFACE_WITH_KNOTS((4,2,4),(3,3),(3.04931861011548E-19,7.62675010863197E-5,
0.000152535002172639),(0.,1.02152348203062),.UNSPECIFIED.)
GEOMETRIC_REPRESENTATION_ITEM()
RATIONAL_B_SPLINE_SURFACE(((1.,0.789033595401263,1.00908146323689),(1.,
0.857071781054836,1.00615262590427),(1.,0.922087264710742,1.00335390671591),
(1.,0.922394466502368,1.00334068261143),(1.,0.857224384599067,1.00614605678499),
(1.,0.789033595401662,1.00908146323687)))
REPRESENTATION_ITEM('')
SURFACE()
);
#3710=(
BOUNDED_SURFACE()
B_SPLINE_SURFACE(3,2,((#436786,#436787,#436788),(#436789,#436790,#436791),
(#436792,#436793,#436794),(#436795,#436796,#436797)),.UNSPECIFIED.,.F.,
 .F.,.F.)
B_SPLINE_SURFACE_WITH_KNOTS((4,4),(3,3),(-1.0842021724855E-19,4.8874751296988E-5),
(-0.000215489856966908,1.),.UNSPECIFIED.)
GEOMETRIC_REPRESENTATION_ITEM()
RATIONAL_B_SPLINE_SURFACE(((1.0000894588971,0.792428983985754,1.),(1.00008931610832,
0.792760296061314,1.),(1.00008917172344,0.793095311538369,1.),(1.00008902569067,
0.79343415062801,1.)))
REPRESENTATION_ITEM('')
SURFACE()
);
#3711=(
BOUNDED_SURFACE()
B_SPLINE_SURFACE(3,2,((#436799,#436800,#436801),(#436802,#436803,#436804),
(#436805,#436806,#436807),(#436808,#436809,#436810)),.UNSPECIFIED.,.F.,
 .F.,.F.)
B_SPLINE_SURFACE_WITH_KNOTS((4,4),(3,3),(-5.21974905013083E-6,5.74172395514388E-5),
(-0.00139822857789422,1.00051312364094),.UNSPECIFIED.)
GEOMETRIC_REPRESENTATION_ITEM()
RATIONAL_B_SPLINE_SURFACE(((1.00049256947262,0.823768952243901,1.00018060397859),
(1.00048448215732,0.826662424388206,1.00017763870891),(1.00052427784041,
0.812424361909259,1.00019223006931),(1.00059912365877,0.785646094632617,
1.00021967280243)))
REPRESENTATION_ITEM('')
SURFACE()
);
#3712=(
BOUNDED_SURFACE()
B_SPLINE_SURFACE(3,2,((#436814,#436815,#436816),(#436817,#436818,#436819),
(#436820,#436821,#436822),(#436823,#436824,#436825)),.UNSPECIFIED.,.F.,
 .F.,.F.)
B_SPLINE_SURFACE_WITH_KNOTS((4,4),(3,3),(3.22980774337778E-5,9.63764854872253E-5),
(-0.00154325936380046,1.01095292447544),.UNSPECIFIED.)
GEOMETRIC_REPRESENTATION_ITEM()
RATIONAL_B_SPLINE_SURFACE(((1.000235309833,0.922925743796158,1.00168574728331),
(1.00015136166126,0.950422439594206,1.0010843469906),(1.000335743374,0.890029368953957,
1.00240524789548),(1.00054260094224,0.822274473168322,1.00388716464858)))
REPRESENTATION_ITEM('')
SURFACE()
);
#3713=(
BOUNDED_SURFACE()
B_SPLINE_SURFACE(3,2,((#436925,#436926,#436927),(#436928,#436929,#436930),
(#436931,#436932,#436933),(#436934,#436935,#436936)),.UNSPECIFIED.,.F.,
 .F.,.F.)
B_SPLINE_SURFACE_WITH_KNOTS((4,4),(3,3),(-2.16840434497101E-19,0.000101260117256738),
(0.,1.),.UNSPECIFIED.)
GEOMETRIC_REPRESENTATION_ITEM()
RATIONAL_B_SPLINE_SURFACE(((1.,0.796615278835174,1.),(1.,0.79589603805594,
1.),(1.,0.795193354661349,1.),(1.,0.794506193185548,1.)))
REPRESENTATION_ITEM('')
SURFACE()
);
#3714=(
BOUNDED_SURFACE()
B_SPLINE_SURFACE(3,2,((#436974,#436975,#436976),(#436977,#436978,#436979),
(#436980,#436981,#436982),(#436983,#436984,#436985),(#436986,#436987,#436988),
(#436989,#436990,#436991)),.UNSPECIFIED.,.F.,.F.,.F.)
B_SPLINE_SURFACE_WITH_KNOTS((4,2,4),(3,3),(5.0821976835258E-21,1.66936432462294E-5,
3.33872864924587E-5),(0.,1.),.UNSPECIFIED.)
GEOMETRIC_REPRESENTATION_ITEM()
RATIONAL_B_SPLINE_SURFACE(((1.,0.79661527883518,1.),(1.,0.862310524418134,
1.),(1.,0.923774472010521,1.),(1.,0.923983993203426,1.),(1.,0.862574873720943,
1.),(1.,0.796615278835189,1.)))
REPRESENTATION_ITEM('')
SURFACE()
);
#3715=(
BOUNDED_SURFACE()
B_SPLINE_SURFACE(3,2,((#437028,#437029,#437030),(#437031,#437032,#437033),
(#437034,#437035,#437036),(#437037,#437038,#437039)),.UNSPECIFIED.,.F.,
 .F.,.F.)
B_SPLINE_SURFACE_WITH_KNOTS((4,4),(3,3),(0.,0.000101244905251112),(0.,1.),
 .UNSPECIFIED.)
GEOMETRIC_REPRESENTATION_ITEM()
RATIONAL_B_SPLINE_SURFACE(((1.,0.796615278835174,1.),(1.,0.795896146109795,
1.),(1.,0.795193565796497,1.),(1.,0.794506502889902,1.)))
REPRESENTATION_ITEM('')
SURFACE()
);
#3716=(
BOUNDED_SURFACE()
B_SPLINE_SURFACE(3,2,((#437075,#437076,#437077),(#437078,#437079,#437080),
(#437081,#437082,#437083),(#437084,#437085,#437086)),.UNSPECIFIED.,.F.,
 .F.,.F.)
B_SPLINE_SURFACE_WITH_KNOTS((4,4),(3,3),(2.85968127239939E-5,9.24681548475814E-5),
(-0.00167900678654074,1.0113082712781),.UNSPECIFIED.)
GEOMETRIC_REPRESENTATION_ITEM()
RATIONAL_B_SPLINE_SURFACE(((1.00059040895217,0.822187541868294,1.00401468696652),
(1.0003652771814,0.889990093671587,1.00248382673388),(1.00016469515013,
0.950399042257939,1.0011199008251),(1.00025604273992,0.922888044286088,
1.00174104990629)))
REPRESENTATION_ITEM('')
SURFACE()
);
#3717=(
BOUNDED_SURFACE()
B_SPLINE_SURFACE(3,2,((#437090,#437091,#437092),(#437093,#437094,#437095),
(#437096,#437097,#437098),(#437099,#437100,#437101)),.UNSPECIFIED.,.F.,
 .F.,.F.)
B_SPLINE_SURFACE_WITH_KNOTS((4,4),(3,3),(-5.22358356749296E-6,5.74594192424277E-5),
(-0.00127120052090352,1.),.UNSPECIFIED.)
GEOMETRIC_REPRESENTATION_ITEM()
RATIONAL_B_SPLINE_SURFACE(((1.0005444931319,0.785835073638689,1.),(1.00047707767488,
0.812351526358792,1.),(1.00044031788598,0.826810216506226,1.),(1.00044777653331,
0.823876514387197,1.)))
REPRESENTATION_ITEM('')
SURFACE()
);
#3718=(
BOUNDED_SURFACE()
B_SPLINE_SURFACE(3,2,((#437103,#437104,#437105),(#437106,#437107,#437108),
(#437109,#437110,#437111),(#437112,#437113,#437114)),.UNSPECIFIED.,.F.,
 .F.,.F.)
B_SPLINE_SURFACE_WITH_KNOTS((4,4),(3,3),(-2.71050543121376E-19,4.88747512969881E-5),
(-0.000215805215783492,1.),.UNSPECIFIED.)
GEOMETRIC_REPRESENTATION_ITEM()
RATIONAL_B_SPLINE_SURFACE(((1.0000891560035,0.793434085499686,1.),(1.00008930225004,
0.793095246303234,1.),(1.00008944684626,0.792760230720494,1.),(1.00008958984405,
0.792428918540536,1.)))
REPRESENTATION_ITEM('')
SURFACE()
);
#3719=(
BOUNDED_SURFACE()
B_SPLINE_SURFACE(3,2,((#437116,#437117,#437118),(#437119,#437120,#437121),
(#437122,#437123,#437124),(#437125,#437126,#437127),(#437128,#437129,#437130),
(#437131,#437132,#437133)),.UNSPECIFIED.,.F.,.F.,.F.)
B_SPLINE_SURFACE_WITH_KNOTS((4,2,4),(3,3),(2.91379333855479E-19,7.62675010863198E-5,
0.000152535002172639),(0.,1.02152348203046),.UNSPECIFIED.)
GEOMETRIC_REPRESENTATION_ITEM()
RATIONAL_B_SPLINE_SURFACE(((1.,0.789033595401294,1.00908146323682),(1.,
0.857071781054879,1.00615262590422),(1.,0.922087264710734,1.00335390671588),
(1.,0.9223944665024,1.0033406826114),(1.,0.857224384599077,1.00614605678494),
(1.,0.789033595401694,1.0090814632368)))
REPRESENTATION_ITEM('')
SURFACE()
);
#3720=(
BOUNDED_SURFACE()
B_SPLINE_SURFACE(3,2,((#437135,#437136,#437137),(#437138,#437139,#437140),
(#437141,#437142,#437143),(#437144,#437145,#437146)),.UNSPECIFIED.,.F.,
 .F.,.F.)
B_SPLINE_SURFACE_WITH_KNOTS((4,4),(3,3),(3.25260651745651E-19,4.88747512969884E-5),
(-0.000215489857083527,1.),.UNSPECIFIED.)
GEOMETRIC_REPRESENTATION_ITEM()
RATIONAL_B_SPLINE_SURFACE(((1.00008945889715,0.792428983985737,1.),(1.00008931610837,
0.792760296061273,1.),(1.00008917172349,0.793095311538366,1.),(1.00008902569072,
0.793434150627984,1.)))
REPRESENTATION_ITEM('')
SURFACE()
);
#3721=(
BOUNDED_SURFACE()
B_SPLINE_SURFACE(3,2,((#437148,#437149,#437150),(#437151,#437152,#437153),
(#437154,#437155,#437156),(#437157,#437158,#437159)),.UNSPECIFIED.,.F.,
 .F.,.F.)
B_SPLINE_SURFACE_WITH_KNOTS((4,4),(3,3),(-5.21974905013089E-6,5.74172395514386E-5),
(-0.00139822857702801,1.00051312364039),.UNSPECIFIED.)
GEOMETRIC_REPRESENTATION_ITEM()
RATIONAL_B_SPLINE_SURFACE(((1.00049256947232,0.823768952244153,1.0001806039784),
(1.00048448215702,0.826662424388442,1.00017763870873),(1.00052427784009,
0.81242436190953,1.00019223006911),(1.0005991236584,0.785646094632913,1.00021967280219)))
REPRESENTATION_ITEM('')
SURFACE()
);
#3722=(
BOUNDED_SURFACE()
B_SPLINE_SURFACE(3,2,((#437163,#437164,#437165),(#437166,#437167,#437168),
(#437169,#437170,#437171),(#437172,#437173,#437174)),.UNSPECIFIED.,.F.,
 .F.,.F.)
B_SPLINE_SURFACE_WITH_KNOTS((4,4),(3,3),(3.22980774337781E-5,9.63764854872258E-5),
(-0.00154325936375446,1.01095292447528),.UNSPECIFIED.)
GEOMETRIC_REPRESENTATION_ITEM()
RATIONAL_B_SPLINE_SURFACE(((1.00023530983299,0.922925743796172,1.00168574728329),
(1.00015136166126,0.950422439594222,1.00108434699058),(1.00033574337399,
0.89002936895397,1.00240524789544),(1.00054260094222,0.822274473168358,
1.00388716464853)))
REPRESENTATION_ITEM('')
SURFACE()
);
#3723=(
BOUNDED_SURFACE()
B_SPLINE_SURFACE(3,2,((#437274,#437275,#437276),(#437277,#437278,#437279),
(#437280,#437281,#437282),(#437283,#437284,#437285)),.UNSPECIFIED.,.F.,
 .F.,.F.)
B_SPLINE_SURFACE_WITH_KNOTS((4,4),(3,3),(0.,0.000101260117256736),(0.,1.),
 .UNSPECIFIED.)
GEOMETRIC_REPRESENTATION_ITEM()
RATIONAL_B_SPLINE_SURFACE(((1.,0.79661527883517,1.),(1.,0.795896038055932,
1.),(1.,0.795193354661359,1.),(1.,0.794506193185534,1.)))
REPRESENTATION_ITEM('')
SURFACE()
);
#3724=(
BOUNDED_SURFACE()
B_SPLINE_SURFACE(3,2,((#437323,#437324,#437325),(#437326,#437327,#437328),
(#437329,#437330,#437331),(#437332,#437333,#437334),(#437335,#437336,#437337),
(#437338,#437339,#437340)),.UNSPECIFIED.,.F.,.F.,.F.)
B_SPLINE_SURFACE_WITH_KNOTS((4,2,4),(3,3),(1.21972744404619E-19,1.66936432462291E-5,
3.33872864924582E-5),(0.,1.),.UNSPECIFIED.)
GEOMETRIC_REPRESENTATION_ITEM()
RATIONAL_B_SPLINE_SURFACE(((1.,0.796615278835175,1.),(1.,0.862310524418131,
1.),(1.,0.923774472010521,1.),(1.,0.923983993203428,1.),(1.,0.862574873720943,
1.),(1.,0.796615278835187,1.)))
REPRESENTATION_ITEM('')
SURFACE()
);
#3725=(
BOUNDED_SURFACE()
B_SPLINE_SURFACE(3,2,((#437377,#437378,#437379),(#437380,#437381,#437382),
(#437383,#437384,#437385),(#437386,#437387,#437388)),.UNSPECIFIED.,.F.,
 .F.,.F.)
B_SPLINE_SURFACE_WITH_KNOTS((4,4),(3,3),(0.,0.000101244905251112),(0.,1.),
 .UNSPECIFIED.)
GEOMETRIC_REPRESENTATION_ITEM()
RATIONAL_B_SPLINE_SURFACE(((1.,0.796615278835171,1.),(1.,0.795896146109793,
1.),(1.,0.7951935657965,1.),(1.,0.794506502889898,1.)))
REPRESENTATION_ITEM('')
SURFACE()
);
#3726=(
BOUNDED_SURFACE()
B_SPLINE_SURFACE(3,2,((#437424,#437425,#437426),(#437427,#437428,#437429),
(#437430,#437431,#437432),(#437433,#437434,#437435)),.UNSPECIFIED.,.F.,
 .F.,.F.)
B_SPLINE_SURFACE_WITH_KNOTS((4,4),(3,3),(2.85968127239939E-5,9.24681548475816E-5),
(-0.00167900678767833,1.01130827127821),.UNSPECIFIED.)
GEOMETRIC_REPRESENTATION_ITEM()
RATIONAL_B_SPLINE_SURFACE(((1.00059040895257,0.822187541868073,1.00401468696656),
(1.00036527718164,0.889990093671444,1.00248382673391),(1.00016469515024,
0.950399042257875,1.00111990082511),(1.0002560427401,0.922888044285992,
1.00174104990631)))
REPRESENTATION_ITEM('')
SURFACE()
);
#3727=(
BOUNDED_SURFACE()
B_SPLINE_SURFACE(3,2,((#437439,#437440,#437441),(#437442,#437443,#437444),
(#437445,#437446,#437447),(#437448,#437449,#437450)),.UNSPECIFIED.,.F.,
 .F.,.F.)
B_SPLINE_SURFACE_WITH_KNOTS((4,4),(3,3),(-5.22358356749301E-6,5.7459419242428E-5),
(-0.00127120052059091,1.),.UNSPECIFIED.)
GEOMETRIC_REPRESENTATION_ITEM()
RATIONAL_B_SPLINE_SURFACE(((1.00054449313177,0.785835073638755,1.),(1.00047707767476,
0.812351526358847,1.),(1.00044031788588,0.82681021650628,1.),(1.0004477765332,
0.823876514387243,1.)))
REPRESENTATION_ITEM('')
SURFACE()
);
#3728=(
BOUNDED_SURFACE()
B_SPLINE_SURFACE(3,2,((#437452,#437453,#437454),(#437455,#437456,#437457),
(#437458,#437459,#437460),(#437461,#437462,#437463)),.UNSPECIFIED.,.F.,
 .F.,.F.)
B_SPLINE_SURFACE_WITH_KNOTS((4,4),(3,3),(-1.35525271560688E-19,4.88747512969881E-5),
(-0.000215805216124583,1.),.UNSPECIFIED.)
GEOMETRIC_REPRESENTATION_ITEM()
RATIONAL_B_SPLINE_SURFACE(((1.00008915600365,0.793434085499612,1.),(1.00008930225018,
0.793095246303167,1.),(1.0000894468464,0.792760230720414,1.),(1.00008958984419,
0.792428918540462,1.)))
REPRESENTATION_ITEM('')
SURFACE()
);
#3729=(
BOUNDED_SURFACE()
B_SPLINE_SURFACE(3,2,((#437465,#437466,#437467),(#437468,#437469,#437470),
(#437471,#437472,#437473),(#437474,#437475,#437476),(#437477,#437478,#437479),
(#437480,#437481,#437482)),.UNSPECIFIED.,.F.,.F.,.F.)
B_SPLINE_SURFACE_WITH_KNOTS((4,2,4),(3,3),(-2.71050543121376E-20,7.62675010863192E-5,
0.000152535002172638),(0.,1.02152348203063),.UNSPECIFIED.)
GEOMETRIC_REPRESENTATION_ITEM()
RATIONAL_B_SPLINE_SURFACE(((1.,0.789033595401261,1.0090814632369),(1.,0.857071781054855,
1.00615262590427),(1.,0.922087264710718,1.00335390671591),(1.,0.922394466502388,
1.00334068261143),(1.,0.857224384599047,1.00614605678499),(1.,0.789033595401658,
1.00908146323688)))
REPRESENTATION_ITEM('')
SURFACE()
);
#3730=(
BOUNDED_SURFACE()
B_SPLINE_SURFACE(3,2,((#437484,#437485,#437486),(#437487,#437488,#437489),
(#437490,#437491,#437492),(#437493,#437494,#437495)),.UNSPECIFIED.,.F.,
 .F.,.F.)
B_SPLINE_SURFACE_WITH_KNOTS((4,4),(3,3),(3.79470760369927E-19,4.88747512969882E-5),
(-0.000215489857057505,1.),.UNSPECIFIED.)
GEOMETRIC_REPRESENTATION_ITEM()
RATIONAL_B_SPLINE_SURFACE(((1.00008945889714,0.792428983985739,1.),(1.00008931610836,
0.792760296061291,1.),(1.00008917172348,0.793095311538347,1.),(1.00008902569071,
0.793434150627992,1.)))
REPRESENTATION_ITEM('')
SURFACE()
);
#3731=(
BOUNDED_SURFACE()
B_SPLINE_SURFACE(3,2,((#437497,#437498,#437499),(#437500,#437501,#437502),
(#437503,#437504,#437505),(#437506,#437507,#437508)),.UNSPECIFIED.,.F.,
 .F.,.F.)
B_SPLINE_SURFACE_WITH_KNOTS((4,4),(3,3),(-5.21974905012869E-6,5.74172395514399E-5),
(-0.00139822857743797,1.00051312364057),.UNSPECIFIED.)
GEOMETRIC_REPRESENTATION_ITEM()
RATIONAL_B_SPLINE_SURFACE(((1.00049256947246,0.823768952244043,1.00018060397846),
(1.00048448215717,0.826662424388345,1.00017763870879),(1.00052427784024,
0.812424361909404,1.00019223006918),(1.00059912365858,0.785646094632793,
1.00021967280227)))
REPRESENTATION_ITEM('')
SURFACE()
);
#3732=(
BOUNDED_SURFACE()
B_SPLINE_SURFACE(3,2,((#437512,#437513,#437514),(#437515,#437516,#437517),
(#437518,#437519,#437520),(#437521,#437522,#437523)),.UNSPECIFIED.,.F.,
 .F.,.F.)
B_SPLINE_SURFACE_WITH_KNOTS((4,4),(3,3),(3.22980774337777E-5,9.6376485487225E-5),
(-0.00154325936378919,1.01095292447567),.UNSPECIFIED.)
GEOMETRIC_REPRESENTATION_ITEM()
RATIONAL_B_SPLINE_SURFACE(((1.000235309833,0.922925743796142,1.00168574728335),
(1.00015136166126,0.9504224395942,1.00108434699062),(1.000335743374,0.890029368953935,
1.00240524789553),(1.00054260094223,0.822274473168277,1.00388716464867)))
REPRESENTATION_ITEM('')
SURFACE()
);
#3733=(
BOUNDED_SURFACE()
B_SPLINE_SURFACE(3,2,((#437623,#437624,#437625),(#437626,#437627,#437628),
(#437629,#437630,#437631),(#437632,#437633,#437634)),.UNSPECIFIED.,.F.,
 .F.,.F.)
B_SPLINE_SURFACE_WITH_KNOTS((4,4),(3,3),(0.,0.000101260117256738),(0.,1.),
 .UNSPECIFIED.)
GEOMETRIC_REPRESENTATION_ITEM()
RATIONAL_B_SPLINE_SURFACE(((1.,0.796615278835171,1.),(1.,0.795896038055941,
1.),(1.,0.795193354661341,1.),(1.,0.794506193185546,1.)))
REPRESENTATION_ITEM('')
SURFACE()
);
#3734=(
BOUNDED_SURFACE()
B_SPLINE_SURFACE(3,2,((#437672,#437673,#437674),(#437675,#437676,#437677),
(#437678,#437679,#437680),(#437681,#437682,#437683),(#437684,#437685,#437686),
(#437687,#437688,#437689)),.UNSPECIFIED.,.F.,.F.,.F.)
B_SPLINE_SURFACE_WITH_KNOTS((4,2,4),(3,3),(4.45539330255762E-19,1.66936432462296E-5,
3.33872864924588E-5),(0.,1.),.UNSPECIFIED.)
GEOMETRIC_REPRESENTATION_ITEM()
RATIONAL_B_SPLINE_SURFACE(((1.,0.79661527883518,1.),(1.,0.862310524418132,
1.),(1.,0.923774472010522,1.),(1.,0.923983993203426,1.),(1.,0.862574873720932,
1.),(1.,0.796615278835189,1.)))
REPRESENTATION_ITEM('')
SURFACE()
);
#3735=(
BOUNDED_SURFACE()
B_SPLINE_SURFACE(3,2,((#437726,#437727,#437728),(#437729,#437730,#437731),
(#437732,#437733,#437734),(#437735,#437736,#437737)),.UNSPECIFIED.,.F.,
 .F.,.F.)
B_SPLINE_SURFACE_WITH_KNOTS((4,4),(3,3),(-2.16840434497101E-19,0.000101244905251112),
(0.,1.),.UNSPECIFIED.)
GEOMETRIC_REPRESENTATION_ITEM()
RATIONAL_B_SPLINE_SURFACE(((1.,0.796615278835168,1.),(1.,0.795896146109797,
1.),(1.,0.795193565796497,1.),(1.,0.794506502889899,1.)))
REPRESENTATION_ITEM('')
SURFACE()
);
#3736=(
BOUNDED_SURFACE()
B_SPLINE_SURFACE(3,2,((#437773,#437774,#437775),(#437776,#437777,#437778),
(#437779,#437780,#437781),(#437782,#437783,#437784)),.UNSPECIFIED.,.F.,
 .F.,.F.)
B_SPLINE_SURFACE_WITH_KNOTS((4,4),(3,3),(2.85968127239939E-5,9.24681548475815E-5),
(-0.00167900678606714,1.01130827127823),.UNSPECIFIED.)
GEOMETRIC_REPRESENTATION_ITEM()
RATIONAL_B_SPLINE_SURFACE(((1.000590408952,0.822187541868358,1.00401468696657),
(1.00036527718129,0.889990093671623,1.00248382673391),(1.00016469515008,
0.950399042257955,1.00111990082511),(1.00025604273985,0.922888044286117,
1.00174104990631)))
REPRESENTATION_ITEM('')
SURFACE()
);
#3737=(
BOUNDED_SURFACE()
B_SPLINE_SURFACE(3,2,((#437788,#437789,#437790),(#437791,#437792,#437793),
(#437794,#437795,#437796),(#437797,#437798,#437799)),.UNSPECIFIED.,.F.,
 .F.,.F.)
B_SPLINE_SURFACE_WITH_KNOTS((4,4),(3,3),(-5.22358356749019E-6,5.74594192424278E-5),
(-0.00127120052048488,1.),.UNSPECIFIED.)
GEOMETRIC_REPRESENTATION_ITEM()
RATIONAL_B_SPLINE_SURFACE(((1.00054449313172,0.785835073638779,0.999999999999999),
(1.00047707767472,0.812351526358877,1.),(1.00044031788584,0.826810216506281,
1.),(1.00044777653316,0.823876514387274,1.)))
REPRESENTATION_ITEM('')
SURFACE()
);
#3738=(
BOUNDED_SURFACE()
B_SPLINE_SURFACE(3,2,((#437801,#437802,#437803),(#437804,#437805,#437806),
(#437807,#437808,#437809),(#437810,#437811,#437812)),.UNSPECIFIED.,.F.,
 .F.,.F.)
B_SPLINE_SURFACE_WITH_KNOTS((4,4),(3,3),(-2.43945488809238E-19,4.88747512969881E-5),
(-0.000215805215277963,1.),.UNSPECIFIED.)
GEOMETRIC_REPRESENTATION_ITEM()
RATIONAL_B_SPLINE_SURFACE(((1.0000891560033,0.793434085499786,1.),(1.00008930224983,
0.793095246303339,1.),(1.00008944684605,0.792760230720593,1.),(1.00008958984384,
0.792428918540633,1.)))
REPRESENTATION_ITEM('')
SURFACE()
);
#3739=(
BOUNDED_SURFACE()
B_SPLINE_SURFACE(3,2,((#437814,#437815,#437816),(#437817,#437818,#437819),
(#437820,#437821,#437822),(#437823,#437824,#437825),(#437826,#437827,#437828),
(#437829,#437830,#437831)),.UNSPECIFIED.,.F.,.F.,.F.)
B_SPLINE_SURFACE_WITH_KNOTS((4,2,4),(3,3),(1.89735380184963E-19,7.62675010863193E-5,
0.000152535002172638),(0.,1.02152348203076),.UNSPECIFIED.)
GEOMETRIC_REPRESENTATION_ITEM()
RATIONAL_B_SPLINE_SURFACE(((1.,0.789033595401233,1.00908146323695),(1.,
0.85707178105484,1.00615262590431),(1.,0.922087264710706,1.00335390671593),
(1.,0.922394466502385,1.00334068261145),(1.,0.857224384599031,1.00614605678503),
(1.,0.789033595401629,1.00908146323694)))
REPRESENTATION_ITEM('')
SURFACE()
);
#3740=(
BOUNDED_SURFACE()
B_SPLINE_SURFACE(3,2,((#437833,#437834,#437835),(#437836,#437837,#437838),
(#437839,#437840,#437841),(#437842,#437843,#437844)),.UNSPECIFIED.,.F.,
 .F.,.F.)
B_SPLINE_SURFACE_WITH_KNOTS((4,4),(3,3),(1.0842021724855E-19,4.88747512969883E-5),
(-0.000215489856960214,1.),.UNSPECIFIED.)
GEOMETRIC_REPRESENTATION_ITEM()
RATIONAL_B_SPLINE_SURFACE(((1.0000894588971,0.79242898398576,1.),(1.00008931610832,
0.792760296061308,1.),(1.00008917172344,0.793095311538373,1.),(1.00008902569067,
0.79343415062801,1.)))
REPRESENTATION_ITEM('')
SURFACE()
);
#3741=(
BOUNDED_SURFACE()
B_SPLINE_SURFACE(3,2,((#437846,#437847,#437848),(#437849,#437850,#437851),
(#437852,#437853,#437854),(#437855,#437856,#437857)),.UNSPECIFIED.,.F.,
 .F.,.F.)
B_SPLINE_SURFACE_WITH_KNOTS((4,4),(3,3),(-5.21974905012869E-6,5.74172395514386E-5),
(-0.00139822857769568,1.00051312364042),.UNSPECIFIED.)
GEOMETRIC_REPRESENTATION_ITEM()
RATIONAL_B_SPLINE_SURFACE(((1.00049256947255,0.823768952244027,1.0001806039784),
(1.00048448215726,0.826662424388324,1.00017763870874),(1.00052427784034,
0.812424361909387,1.00019223006912),(1.00059912365869,0.785646094632771,
1.0002196728022)))
REPRESENTATION_ITEM('')
SURFACE()
);
#3742=(
BOUNDED_SURFACE()
B_SPLINE_SURFACE(3,2,((#437861,#437862,#437863),(#437864,#437865,#437866),
(#437867,#437868,#437869),(#437870,#437871,#437872)),.UNSPECIFIED.,.F.,
 .F.,.F.)
B_SPLINE_SURFACE_WITH_KNOTS((4,4),(3,3),(3.22980774337778E-5,9.63764854872255E-5),
(-0.00154325936389316,1.01095292447562),.UNSPECIFIED.)
GEOMETRIC_REPRESENTATION_ITEM()
RATIONAL_B_SPLINE_SURFACE(((1.00023530983301,0.922925743796137,1.00168574728334),
(1.00015136166127,0.950422439594205,1.00108434699062),(1.00033574337402,
0.890029368953915,1.00240524789552),(1.00054260094227,0.822274473168278,
1.00388716464865)))
REPRESENTATION_ITEM('')
SURFACE()
);
#3743=(
BOUNDED_SURFACE()
B_SPLINE_SURFACE(3,2,((#437972,#437973,#437974),(#437975,#437976,#437977),
(#437978,#437979,#437980),(#437981,#437982,#437983)),.UNSPECIFIED.,.F.,
 .F.,.F.)
B_SPLINE_SURFACE_WITH_KNOTS((4,4),(3,3),(2.16840434497101E-19,0.000101260117256738),
(0.,1.),.UNSPECIFIED.)
GEOMETRIC_REPRESENTATION_ITEM()
RATIONAL_B_SPLINE_SURFACE(((1.,0.796615278835169,1.),(1.,0.795896038055941,
1.),(1.,0.795193354661347,1.),(1.,0.794506193185546,1.)))
REPRESENTATION_ITEM('')
SURFACE()
);
#3744=(
BOUNDED_SURFACE()
B_SPLINE_SURFACE(3,2,((#438021,#438022,#438023),(#438024,#438025,#438026),
(#438027,#438028,#438029),(#438030,#438031,#438032),(#438033,#438034,#438035),
(#438036,#438037,#438038)),.UNSPECIFIED.,.F.,.F.,.F.)
B_SPLINE_SURFACE_WITH_KNOTS((4,2,4),(3,3),(1.77876918923403E-19,1.66936432462298E-5,
3.33872864924594E-5),(0.,1.),.UNSPECIFIED.)
GEOMETRIC_REPRESENTATION_ITEM()
RATIONAL_B_SPLINE_SURFACE(((1.,0.796615278835173,1.),(1.,0.862310524418123,
1.),(1.,0.923774472010521,1.),(1.,0.923983993203424,1.),(1.,0.862574873720951,
1.),(1.,0.796615278835182,1.)))
REPRESENTATION_ITEM('')
SURFACE()
);
#3745=(
BOUNDED_SURFACE()
B_SPLINE_SURFACE(3,2,((#438075,#438076,#438077),(#438078,#438079,#438080),
(#438081,#438082,#438083),(#438084,#438085,#438086)),.UNSPECIFIED.,.F.,
 .F.,.F.)
B_SPLINE_SURFACE_WITH_KNOTS((4,4),(3,3),(0.,0.000101244905251112),(0.,1.),
 .UNSPECIFIED.)
GEOMETRIC_REPRESENTATION_ITEM()
RATIONAL_B_SPLINE_SURFACE(((1.,0.796615278835169,1.),(1.,0.795896146109798,
1.),(1.,0.795193565796496,1.),(1.,0.794506502889901,1.)))
REPRESENTATION_ITEM('')
SURFACE()
);
#3746=(
BOUNDED_SURFACE()
B_SPLINE_SURFACE(3,2,((#438122,#438123,#438124),(#438125,#438126,#438127),
(#438128,#438129,#438130),(#438131,#438132,#438133)),.UNSPECIFIED.,.F.,
 .F.,.F.)
B_SPLINE_SURFACE_WITH_KNOTS((4,4),(3,3),(2.85968127239939E-5,9.24681548475816E-5),
(-0.00167900679302498,1.01130827127816),.UNSPECIFIED.)
GEOMETRIC_REPRESENTATION_ITEM()
RATIONAL_B_SPLINE_SURFACE(((1.00059040895445,0.822187541867124,1.00401468696654),
(1.00036527718281,0.889990093670864,1.0024838267339),(1.00016469515077,
0.950399042257607,1.0011199008251),(1.00025604274091,0.922888044285581,
1.0017410499063)))
REPRESENTATION_ITEM('')
SURFACE()
);
#3747=(
BOUNDED_SURFACE()
B_SPLINE_SURFACE(3,2,((#438137,#438138,#438139),(#438140,#438141,#438142),
(#438143,#438144,#438145),(#438146,#438147,#438148)),.UNSPECIFIED.,.F.,
 .F.,.F.)
B_SPLINE_SURFACE_WITH_KNOTS((4,4),(3,3),(-5.22358356749285E-6,5.74594192424277E-5),
(-0.00127120052057846,1.),.UNSPECIFIED.)
GEOMETRIC_REPRESENTATION_ITEM()
RATIONAL_B_SPLINE_SURFACE(((1.00054449313176,0.785835073638763,1.),(1.00047707767476,
0.812351526358834,1.),(1.00044031788587,0.826810216506288,1.),(1.00044777653319,
0.82387651438725,1.)))
REPRESENTATION_ITEM('')
SURFACE()
);
#3748=(
BOUNDED_SURFACE()
B_SPLINE_SURFACE(3,2,((#438150,#438151,#438152),(#438153,#438154,#438155),
(#438156,#438157,#438158),(#438159,#438160,#438161)),.UNSPECIFIED.,.F.,
 .F.,.F.)
B_SPLINE_SURFACE_WITH_KNOTS((4,4),(3,3),(-8.13151629364128E-20,4.8874751296988E-5),
(-0.000215805215388037,1.),.UNSPECIFIED.)
GEOMETRIC_REPRESENTATION_ITEM()
RATIONAL_B_SPLINE_SURFACE(((1.00008915600334,0.793434085499765,1.),(1.00008930224987,
0.793095246303302,1.),(1.00008944684609,0.792760230720584,1.),(1.00008958984389,
0.792428918540612,1.)))
REPRESENTATION_ITEM('')
SURFACE()
);
#3749=(
BOUNDED_SURFACE()
B_SPLINE_SURFACE(3,2,((#438163,#438164,#438165),(#438166,#438167,#438168),
(#438169,#438170,#438171),(#438172,#438173,#438174),(#438175,#438176,#438177),
(#438178,#438179,#438180)),.UNSPECIFIED.,.F.,.F.,.F.)
B_SPLINE_SURFACE_WITH_KNOTS((4,2,4),(3,3),(8.13151629364128E-20,7.62675010863197E-5,
0.000152535002172639),(0.,1.02152348203066),.UNSPECIFIED.)
GEOMETRIC_REPRESENTATION_ITEM()
RATIONAL_B_SPLINE_SURFACE(((1.,0.789033595401252,1.00908146323691),(1.,
0.857071781054831,1.00615262590428),(1.,0.922087264710747,1.00335390671592),
(1.,0.922394466502359,1.00334068261143),(1.,0.857224384599067,1.006146056785),
(1.,0.789033595401652,1.00908146323689)))
REPRESENTATION_ITEM('')
SURFACE()
);
#3750=(
BOUNDED_SURFACE()
B_SPLINE_SURFACE(3,2,((#438182,#438183,#438184),(#438185,#438186,#438187),
(#438188,#438189,#438190),(#438191,#438192,#438193)),.UNSPECIFIED.,.F.,
 .F.,.F.)
B_SPLINE_SURFACE_WITH_KNOTS((4,4),(3,3),(2.71050543121376E-19,4.88747512969882E-5),
(-0.00021548985699875,1.),.UNSPECIFIED.)
GEOMETRIC_REPRESENTATION_ITEM()
RATIONAL_B_SPLINE_SURFACE(((1.00008945889712,0.792428983985752,1.),(1.00008931610833,
0.792760296061301,1.),(1.00008917172346,0.793095311538365,1.),(1.00008902569068,
0.793434150628002,1.)))
REPRESENTATION_ITEM('')
SURFACE()
);
#3751=(
BOUNDED_SURFACE()
B_SPLINE_SURFACE(3,2,((#438195,#438196,#438197),(#438198,#438199,#438200),
(#438201,#438202,#438203),(#438204,#438205,#438206)),.UNSPECIFIED.,.F.,
 .F.,.F.)
B_SPLINE_SURFACE_WITH_KNOTS((4,4),(3,3),(-5.21974905013094E-6,5.74172395514392E-5),
(-0.00139822857772714,1.00051312364077),.UNSPECIFIED.)
GEOMETRIC_REPRESENTATION_ITEM()
RATIONAL_B_SPLINE_SURFACE(((1.00049256947256,0.823768952243963,1.00018060397853),
(1.00048448215727,0.826662424388249,1.00017763870886),(1.00052427784035,
0.812424361909331,1.00019223006925),(1.0005991236587,0.785646094632682,
1.00021967280235)))
REPRESENTATION_ITEM('')
SURFACE()
);
#3752=(
BOUNDED_SURFACE()
B_SPLINE_SURFACE(3,2,((#438210,#438211,#438212),(#438213,#438214,#438215),
(#438216,#438217,#438218),(#438219,#438220,#438221)),.UNSPECIFIED.,.F.,
 .F.,.F.)
B_SPLINE_SURFACE_WITH_KNOTS((4,4),(3,3),(3.22980774337784E-5,9.63764854872253E-5),
(-0.0015432593633078,1.01095292447534),.UNSPECIFIED.)
GEOMETRIC_REPRESENTATION_ITEM()
RATIONAL_B_SPLINE_SURFACE(((1.00023530983292,0.922925743796203,1.0016857472833),
(1.00015136166121,0.950422439594246,1.00108434699059),(1.00033574337389,
0.890029368954014,1.00240524789546),(1.00054260094206,0.822274473168425,
1.00388716464855)))
REPRESENTATION_ITEM('')
SURFACE()
);
#3753=(
BOUNDED_SURFACE()
B_SPLINE_SURFACE(3,2,((#438321,#438322,#438323),(#438324,#438325,#438326),
(#438327,#438328,#438329),(#438330,#438331,#438332)),.UNSPECIFIED.,.F.,
 .F.,.F.)
B_SPLINE_SURFACE_WITH_KNOTS((4,4),(3,3),(-2.16840434497101E-19,0.000101260117256738),
(0.,1.),.UNSPECIFIED.)
GEOMETRIC_REPRESENTATION_ITEM()
RATIONAL_B_SPLINE_SURFACE(((1.,0.796615278835171,1.),(1.,0.795896038055941,
1.),(1.,0.795193354661347,1.),(1.,0.794506193185546,1.)))
REPRESENTATION_ITEM('')
SURFACE()
);
#3754=(
BOUNDED_SURFACE()
B_SPLINE_SURFACE(3,2,((#438370,#438371,#438372),(#438373,#438374,#438375),
(#438376,#438377,#438378),(#438379,#438380,#438381),(#438382,#438383,#438384),
(#438385,#438386,#438387)),.UNSPECIFIED.,.F.,.F.,.F.)
B_SPLINE_SURFACE_WITH_KNOTS((4,2,4),(3,3),(8.30092288309214E-20,1.66936432462294E-5,
3.33872864924587E-5),(0.,1.),.UNSPECIFIED.)
GEOMETRIC_REPRESENTATION_ITEM()
RATIONAL_B_SPLINE_SURFACE(((1.,0.796615278835175,1.),(1.,0.862310524418132,
1.),(1.,0.92377447201052,1.),(1.,0.923983993203425,1.),(1.,0.862574873720945,
1.),(1.,0.796615278835182,1.)))
REPRESENTATION_ITEM('')
SURFACE()
);
#3755=(
BOUNDED_SURFACE()
B_SPLINE_SURFACE(3,2,((#438424,#438425,#438426),(#438427,#438428,#438429),
(#438430,#438431,#438432),(#438433,#438434,#438435)),.UNSPECIFIED.,.F.,
 .F.,.F.)
B_SPLINE_SURFACE_WITH_KNOTS((4,4),(3,3),(-2.16840434497101E-19,0.000101244905251112),
(0.,1.),.UNSPECIFIED.)
GEOMETRIC_REPRESENTATION_ITEM()
RATIONAL_B_SPLINE_SURFACE(((1.,0.796615278835169,1.),(1.,0.795896146109793,
1.),(1.,0.795193565796498,1.),(1.,0.794506502889898,1.)))
REPRESENTATION_ITEM('')
SURFACE()
);
#3756=(
BOUNDED_SURFACE()
B_SPLINE_SURFACE(3,2,((#438471,#438472,#438473),(#438474,#438475,#438476),
(#438477,#438478,#438479),(#438480,#438481,#438482)),.UNSPECIFIED.,.F.,
 .F.,.F.)
B_SPLINE_SURFACE_WITH_KNOTS((4,4),(3,3),(2.85968127239939E-5,9.24681548475819E-5),
(-0.0016790067865302,1.01130827127821),.UNSPECIFIED.)
GEOMETRIC_REPRESENTATION_ITEM()
RATIONAL_B_SPLINE_SURFACE(((1.00059040895216,0.822187541868273,1.00401468696656),
(1.00036527718139,0.889990093671574,1.00248382673391),(1.00016469515013,
0.950399042257933,1.00111990082511),(1.00025604273992,0.922888044286081,
1.00174104990631)))
REPRESENTATION_ITEM('')
SURFACE()
);
#3757=(
BOUNDED_SURFACE()
B_SPLINE_SURFACE(3,2,((#438486,#438487,#438488),(#438489,#438490,#438491),
(#438492,#438493,#438494),(#438495,#438496,#438497)),.UNSPECIFIED.,.F.,
 .F.,.F.)
B_SPLINE_SURFACE_WITH_KNOTS((4,4),(3,3),(-5.22358356749259E-6,5.7459419242428E-5),
(-0.00127120052070354,1.),.UNSPECIFIED.)
GEOMETRIC_REPRESENTATION_ITEM()
RATIONAL_B_SPLINE_SURFACE(((1.00054449313181,0.785835073638736,1.),(1.0004770776748,
0.812351526358819,1.),(1.00044031788592,0.826810216506259,1.),(1.00044777653324,
0.82387651438723,1.)))
REPRESENTATION_ITEM('')
SURFACE()
);
#3758=(
BOUNDED_SURFACE()
B_SPLINE_SURFACE(3,2,((#438499,#438500,#438501),(#438502,#438503,#438504),
(#438505,#438506,#438507),(#438508,#438509,#438510)),.UNSPECIFIED.,.F.,
 .F.,.F.)
B_SPLINE_SURFACE_WITH_KNOTS((4,4),(3,3),(-4.60785923306339E-19,4.88747512969879E-5),
(-0.000215805215175112,1.),.UNSPECIFIED.)
GEOMETRIC_REPRESENTATION_ITEM()
RATIONAL_B_SPLINE_SURFACE(((1.00008915600325,0.793434085499807,1.),(1.00008930224978,
0.793095246303347,1.),(1.000089446846,0.792760230720625,1.),(1.0000895898438,
0.792428918540656,1.)))
REPRESENTATION_ITEM('')
SURFACE()
);
#3759=(
BOUNDED_SURFACE()
B_SPLINE_SURFACE(3,2,((#438512,#438513,#438514),(#438515,#438516,#438517),
(#438518,#438519,#438520),(#438521,#438522,#438523),(#438524,#438525,#438526),
(#438527,#438528,#438529)),.UNSPECIFIED.,.F.,.F.,.F.)
B_SPLINE_SURFACE_WITH_KNOTS((4,2,4),(3,3),(4.26904605416167E-19,7.62675010863197E-5,
0.000152535002172639),(0.,1.02152348203057),.UNSPECIFIED.)
GEOMETRIC_REPRESENTATION_ITEM()
RATIONAL_B_SPLINE_SURFACE(((1.,0.789033595401272,1.00908146323687),(1.,
0.85707178105485,1.00615262590425),(1.,0.922087264710744,1.0033539067159),
(1.,0.922394466502376,1.00334068261142),(1.,0.857224384599074,1.00614605678497),
(1.,0.789033595401675,1.00908146323685)))
REPRESENTATION_ITEM('')
SURFACE()
);
#3760=(
BOUNDED_SURFACE()
B_SPLINE_SURFACE(3,2,((#438531,#438532,#438533),(#438534,#438535,#438536),
(#438537,#438538,#438539),(#438540,#438541,#438542)),.UNSPECIFIED.,.F.,
 .F.,.F.)
B_SPLINE_SURFACE_WITH_KNOTS((4,4),(3,3),(1.0842021724855E-19,4.88747512969884E-5),
(-0.00021548985702727,1.),.UNSPECIFIED.)
GEOMETRIC_REPRESENTATION_ITEM()
RATIONAL_B_SPLINE_SURFACE(((1.00008945889713,0.792428983985747,1.),(1.00008931610834,
0.792760296061294,1.),(1.00008917172347,0.793095311538357,1.),(1.0000890256907,
0.793434150627996,1.)))
REPRESENTATION_ITEM('')
SURFACE()
);
#3761=(
BOUNDED_SURFACE()
B_SPLINE_SURFACE(3,2,((#438544,#438545,#438546),(#438547,#438548,#438549),
(#438550,#438551,#438552),(#438553,#438554,#438555)),.UNSPECIFIED.,.F.,
 .F.,.F.)
B_SPLINE_SURFACE_WITH_KNOTS((4,4),(3,3),(-5.21974905013087E-6,5.74172395514396E-5),
(-0.00139822857741233,1.00051312364074),.UNSPECIFIED.)
GEOMETRIC_REPRESENTATION_ITEM()
RATIONAL_B_SPLINE_SURFACE(((1.00049256947245,0.823768952244018,1.00018060397852),
(1.00048448215716,0.826662424388315,1.00017763870885),(1.00052427784023,
0.812424361909384,1.00019223006924),(1.00059912365857,0.785646094632756,
1.00021967280234)))
REPRESENTATION_ITEM('')
SURFACE()
);
#3762=(
BOUNDED_SURFACE()
B_SPLINE_SURFACE(3,2,((#438559,#438560,#438561),(#438562,#438563,#438564),
(#438565,#438566,#438567),(#438568,#438569,#438570)),.UNSPECIFIED.,.F.,
 .F.,.F.)
B_SPLINE_SURFACE_WITH_KNOTS((4,4),(3,3),(3.22980774337782E-5,9.63764854872258E-5),
(-0.00154325936371964,1.01095292447535),.UNSPECIFIED.)
GEOMETRIC_REPRESENTATION_ITEM()
RATIONAL_B_SPLINE_SURFACE(((1.00023530983299,0.922925743796172,1.0016857472833),
(1.00015136166125,0.95042243959421,1.00108434699059),(1.00033574337398,
0.890029368953975,1.00240524789546),(1.00054260094221,0.82227447316835,
1.00388716464855)))
REPRESENTATION_ITEM('')
SURFACE()
);
#3763=(
BOUNDED_SURFACE()
B_SPLINE_SURFACE(3,2,((#438670,#438671,#438672),(#438673,#438674,#438675),
(#438676,#438677,#438678),(#438679,#438680,#438681)),.UNSPECIFIED.,.F.,
 .F.,.F.)
B_SPLINE_SURFACE_WITH_KNOTS((4,4),(3,3),(0.,0.000101260117256738),(0.,1.),
 .UNSPECIFIED.)
GEOMETRIC_REPRESENTATION_ITEM()
RATIONAL_B_SPLINE_SURFACE(((1.,0.796615278835171,1.),(1.,0.795896038055943,
1.),(1.,0.795193354661344,1.),(1.,0.794506193185545,1.)))
REPRESENTATION_ITEM('')
SURFACE()
);
#3764=(
BOUNDED_SURFACE()
B_SPLINE_SURFACE(3,2,((#438719,#438720,#438721),(#438722,#438723,#438724),
(#438725,#438726,#438727),(#438728,#438729,#438730),(#438731,#438732,#438733),
(#438734,#438735,#438736)),.UNSPECIFIED.,.F.,.F.,.F.)
B_SPLINE_SURFACE_WITH_KNOTS((4,2,4),(3,3),(6.60685698858354E-20,1.66936432462295E-5,
3.3387286492459E-5),(0.,1.),.UNSPECIFIED.)
GEOMETRIC_REPRESENTATION_ITEM()
RATIONAL_B_SPLINE_SURFACE(((1.,0.796615278835176,1.),(1.,0.862310524418131,
1.),(1.,0.923774472010521,1.),(1.,0.923983993203423,1.),(1.,0.862574873720945,
1.),(1.,0.796615278835188,1.)))
REPRESENTATION_ITEM('')
SURFACE()
);
#3765=(
BOUNDED_SURFACE()
B_SPLINE_SURFACE(3,2,((#438773,#438774,#438775),(#438776,#438777,#438778),
(#438779,#438780,#438781),(#438782,#438783,#438784)),.UNSPECIFIED.,.F.,
 .F.,.F.)
B_SPLINE_SURFACE_WITH_KNOTS((4,4),(3,3),(0.,0.000101244905251112),(0.,1.),
 .UNSPECIFIED.)
GEOMETRIC_REPRESENTATION_ITEM()
RATIONAL_B_SPLINE_SURFACE(((1.,0.796615278835171,1.),(1.,0.795896146109794,
1.),(1.,0.795193565796499,1.),(1.,0.794506502889906,1.)))
REPRESENTATION_ITEM('')
SURFACE()
);
#3766=(
BOUNDED_SURFACE()
B_SPLINE_SURFACE(3,2,((#438820,#438821,#438822),(#438823,#438824,#438825),
(#438826,#438827,#438828),(#438829,#438830,#438831)),.UNSPECIFIED.,.F.,
 .F.,.F.)
B_SPLINE_SURFACE_WITH_KNOTS((4,4),(3,3),(2.85968127239939E-5,9.24681548475817E-5),
(-0.00167900678770357,1.01130827127811),.UNSPECIFIED.)
GEOMETRIC_REPRESENTATION_ITEM()
RATIONAL_B_SPLINE_SURFACE(((1.00059040895258,0.822187541868087,1.00401468696653),
(1.00036527718165,0.889990093671452,1.00248382673389),(1.00016469515024,
0.950399042257882,1.0011199008251),(1.0002560427401,0.922888044285998,1.00174104990629)))
REPRESENTATION_ITEM('')
SURFACE()
);
#3767=(
BOUNDED_SURFACE()
B_SPLINE_SURFACE(3,2,((#438835,#438836,#438837),(#438838,#438839,#438840),
(#438841,#438842,#438843),(#438844,#438845,#438846)),.UNSPECIFIED.,.F.,
 .F.,.F.)
B_SPLINE_SURFACE_WITH_KNOTS((4,4),(3,3),(-5.22358356749358E-6,5.74594192424274E-5),
(-0.00127120052056364,1.),.UNSPECIFIED.)
GEOMETRIC_REPRESENTATION_ITEM()
RATIONAL_B_SPLINE_SURFACE(((1.00054449313175,0.785835073638748,1.),(1.00047707767475,
0.812351526358867,1.),(1.00044031788587,0.826810216506277,1.),(1.00044777653319,
0.823876514387257,1.)))
REPRESENTATION_ITEM('')
SURFACE()
);
#3768=(
BOUNDED_SURFACE()
B_SPLINE_SURFACE(3,2,((#438848,#438849,#438850),(#438851,#438852,#438853),
(#438854,#438855,#438856),(#438857,#438858,#438859)),.UNSPECIFIED.,.F.,
 .F.,.F.)
B_SPLINE_SURFACE_WITH_KNOTS((4,4),(3,3),(-4.60785923306339E-19,4.8874751296988E-5),
(-0.00021580521618408,1.),.UNSPECIFIED.)
GEOMETRIC_REPRESENTATION_ITEM()
RATIONAL_B_SPLINE_SURFACE(((1.00008915600367,0.793434085499599,1.),(1.0000893022502,
0.793095246303154,1.),(1.00008944684642,0.792760230720409,1.),(1.00008958984422,
0.792428918540447,1.)))
REPRESENTATION_ITEM('')
SURFACE()
);
#3769=(
BOUNDED_SURFACE()
B_SPLINE_SURFACE(3,2,((#438861,#438862,#438863),(#438864,#438865,#438866),
(#438867,#438868,#438869),(#438870,#438871,#438872),(#438873,#438874,#438875),
(#438876,#438877,#438878)),.UNSPECIFIED.,.F.,.F.,.F.)
B_SPLINE_SURFACE_WITH_KNOTS((4,2,4),(3,3),(4.26904605416167E-19,7.62675010863198E-5,
0.000152535002172639),(0.,1.02152348203057),.UNSPECIFIED.)
GEOMETRIC_REPRESENTATION_ITEM()
RATIONAL_B_SPLINE_SURFACE(((1.,0.789033595401273,1.00908146323687),(1.,
0.857071781054841,1.00615262590426),(1.,0.922087264710753,1.0033539067159),
(1.,0.922394466502368,1.00334068261142),(1.,0.857224384599077,1.00614605678497),
(1.,0.789033595401671,1.00908146323685)))
REPRESENTATION_ITEM('')
SURFACE()
);
#3770=(
BOUNDED_SURFACE()
B_SPLINE_SURFACE(3,2,((#438880,#438881,#438882),(#438883,#438884,#438885),
(#438886,#438887,#438888),(#438889,#438890,#438891)),.UNSPECIFIED.,.F.,
 .F.,.F.)
B_SPLINE_SURFACE_WITH_KNOTS((4,4),(3,3),(3.79470760369927E-19,4.88747512969885E-5),
(-0.000215489857867463,1.),.UNSPECIFIED.)
GEOMETRIC_REPRESENTATION_ITEM()
RATIONAL_B_SPLINE_SURFACE(((1.00008945889748,0.792428983985573,1.),(1.00008931610869,
0.792760296061128,1.),(1.00008917172382,0.793095311538193,1.),(1.00008902569104,
0.793434150627825,1.)))
REPRESENTATION_ITEM('')
SURFACE()
);
#3771=(
BOUNDED_SURFACE()
B_SPLINE_SURFACE(3,2,((#438893,#438894,#438895),(#438896,#438897,#438898),
(#438899,#438900,#438901),(#438902,#438903,#438904)),.UNSPECIFIED.,.F.,
 .F.,.F.)
B_SPLINE_SURFACE_WITH_KNOTS((4,4),(3,3),(-5.21974905012871E-6,5.74172395514387E-5),
(-0.00139822857711726,1.00051312364057),.UNSPECIFIED.)
GEOMETRIC_REPRESENTATION_ITEM()
RATIONAL_B_SPLINE_SURFACE(((1.00049256947235,0.823768952244105,1.00018060397846),
(1.00048448215706,0.826662424388402,1.00017763870879),(1.00052427784012,
0.812424361909468,1.00019223006917),(1.00059912365844,0.785646094632864,
1.00021967280227)))
REPRESENTATION_ITEM('')
SURFACE()
);
#3772=(
BOUNDED_SURFACE()
B_SPLINE_SURFACE(3,2,((#438908,#438909,#438910),(#438911,#438912,#438913),
(#438914,#438915,#438916),(#438917,#438918,#438919)),.UNSPECIFIED.,.F.,
 .F.,.F.)
B_SPLINE_SURFACE_WITH_KNOTS((4,4),(3,3),(3.2298077433778E-5,9.63764854872255E-5),
(-0.00154325936389459,1.01095292447531),.UNSPECIFIED.)
GEOMETRIC_REPRESENTATION_ITEM()
RATIONAL_B_SPLINE_SURFACE(((1.00023530983301,0.922925743796162,1.00168574728329),
(1.00015136166127,0.950422439594216,1.00108434699058),(1.00033574337402,
0.890029368953956,1.00240524789545),(1.00054260094227,0.822274473168327,
1.00388716464854)))
REPRESENTATION_ITEM('')
SURFACE()
);
#3773=(
BOUNDED_SURFACE()
B_SPLINE_SURFACE(3,2,((#439019,#439020,#439021),(#439022,#439023,#439024),
(#439025,#439026,#439027),(#439028,#439029,#439030)),.UNSPECIFIED.,.F.,
 .F.,.F.)
B_SPLINE_SURFACE_WITH_KNOTS((4,4),(3,3),(2.16840434497101E-19,0.000101260117256737),
(0.,1.),.UNSPECIFIED.)
GEOMETRIC_REPRESENTATION_ITEM()
RATIONAL_B_SPLINE_SURFACE(((1.,0.79661527883517,1.),(1.,0.795896038055935,
1.),(1.,0.795193354661354,1.),(1.,0.794506193185532,1.)))
REPRESENTATION_ITEM('')
SURFACE()
);
#3774=(
BOUNDED_SURFACE()
B_SPLINE_SURFACE(3,2,((#439068,#439069,#439070),(#439071,#439072,#439073),
(#439074,#439075,#439076),(#439077,#439078,#439079),(#439080,#439081,#439082),
(#439083,#439084,#439085)),.UNSPECIFIED.,.F.,.F.,.F.)
B_SPLINE_SURFACE_WITH_KNOTS((4,2,4),(3,3),(-6.09863722023096E-20,1.66936432462294E-5,
3.33872864924589E-5),(0.,1.),.UNSPECIFIED.)
GEOMETRIC_REPRESENTATION_ITEM()
RATIONAL_B_SPLINE_SURFACE(((1.,0.796615278835177,1.),(1.,0.862310524418133,
1.),(1.,0.923774472010523,1.),(1.,0.923983993203423,1.),(1.,0.862574873720948,
1.),(1.,0.79661527883519,1.)))
REPRESENTATION_ITEM('')
SURFACE()
);
#3775=(
BOUNDED_SURFACE()
B_SPLINE_SURFACE(3,2,((#439122,#439123,#439124),(#439125,#439126,#439127),
(#439128,#439129,#439130),(#439131,#439132,#439133)),.UNSPECIFIED.,.F.,
 .F.,.F.)
B_SPLINE_SURFACE_WITH_KNOTS((4,4),(3,3),(0.,0.000101244905251112),(0.,1.),
 .UNSPECIFIED.)
GEOMETRIC_REPRESENTATION_ITEM()
RATIONAL_B_SPLINE_SURFACE(((1.,0.796615278835172,1.),(1.,0.795896146109789,
1.),(1.,0.795193565796498,1.),(1.,0.794506502889901,1.)))
REPRESENTATION_ITEM('')
SURFACE()
);
#3776=(
BOUNDED_SURFACE()
B_SPLINE_SURFACE(3,2,((#439169,#439170,#439171),(#439172,#439173,#439174),
(#439175,#439176,#439177),(#439178,#439179,#439180)),.UNSPECIFIED.,.F.,
 .F.,.F.)
B_SPLINE_SURFACE_WITH_KNOTS((4,4),(3,3),(2.85968127239939E-5,9.24681548475817E-5),
(-0.00167900678778285,1.01130827127811),.UNSPECIFIED.)
GEOMETRIC_REPRESENTATION_ITEM()
RATIONAL_B_SPLINE_SURFACE(((1.0005904089526,0.822187541868067,1.00401468696652),
(1.00036527718167,0.889990093671455,1.00248382673388),(1.00016469515025,
0.950399042257867,1.0011199008251),(1.00025604274011,0.922888044285994,
1.00174104990629)))
REPRESENTATION_ITEM('')
SURFACE()
);
#3777=(
BOUNDED_SURFACE()
B_SPLINE_SURFACE(3,2,((#439184,#439185,#439186),(#439187,#439188,#439189),
(#439190,#439191,#439192),(#439193,#439194,#439195)),.UNSPECIFIED.,.F.,
 .F.,.F.)
B_SPLINE_SURFACE_WITH_KNOTS((4,4),(3,3),(-5.2235835674933E-6,5.74594192424276E-5),
(-0.00127120052052763,1.),.UNSPECIFIED.)
GEOMETRIC_REPRESENTATION_ITEM()
RATIONAL_B_SPLINE_SURFACE(((1.00054449313174,0.785835073638757,1.),(1.00047707767474,
0.812351526358864,1.),(1.00044031788585,0.826810216506289,1.),(1.00044777653318,
0.823876514387253,1.)))
REPRESENTATION_ITEM('')
SURFACE()
);
#3778=(
BOUNDED_SURFACE()
B_SPLINE_SURFACE(3,2,((#439197,#439198,#439199),(#439200,#439201,#439202),
(#439203,#439204,#439205),(#439206,#439207,#439208)),.UNSPECIFIED.,.F.,
 .F.,.F.)
B_SPLINE_SURFACE_WITH_KNOTS((4,4),(3,3),(-8.13151629364128E-20,4.88747512969877E-5),
(-0.00021580521555644,1.),.UNSPECIFIED.)
GEOMETRIC_REPRESENTATION_ITEM()
RATIONAL_B_SPLINE_SURFACE(((1.00008915600341,0.793434085499729,1.),(1.00008930224994,
0.793095246303277,1.),(1.00008944684616,0.792760230720541,1.),(1.00008958984396,
0.792428918540576,1.)))
REPRESENTATION_ITEM('')
SURFACE()
);
#3779=(
BOUNDED_SURFACE()
B_SPLINE_SURFACE(3,2,((#439210,#439211,#439212),(#439213,#439214,#439215),
(#439216,#439217,#439218),(#439219,#439220,#439221),(#439222,#439223,#439224),
(#439225,#439226,#439227)),.UNSPECIFIED.,.F.,.F.,.F.)
B_SPLINE_SURFACE_WITH_KNOTS((4,2,4),(3,3),(-1.28749007982654E-19,7.62675010863193E-5,
0.000152535002172639),(0.,1.02152348203056),.UNSPECIFIED.)
GEOMETRIC_REPRESENTATION_ITEM()
RATIONAL_B_SPLINE_SURFACE(((1.,0.789033595401272,1.00908146323686),(1.,
0.857071781054882,1.00615262590425),(1.,0.922087264710708,1.0033539067159),
(1.,0.92239446650241,1.00334068261141),(1.,0.857224384599053,1.00614605678497),
(1.,0.789033595401675,1.00908146323685)))
REPRESENTATION_ITEM('')
SURFACE()
);
#3780=(
BOUNDED_SURFACE()
B_SPLINE_SURFACE(3,2,((#439229,#439230,#439231),(#439232,#439233,#439234),
(#439235,#439236,#439237),(#439238,#439239,#439240)),.UNSPECIFIED.,.F.,
 .F.,.F.)
B_SPLINE_SURFACE_WITH_KNOTS((4,4),(3,3),(4.33680868994202E-19,4.88747512969882E-5),
(-0.00021548985691637,1.),.UNSPECIFIED.)
GEOMETRIC_REPRESENTATION_ITEM()
RATIONAL_B_SPLINE_SURFACE(((1.00008945889708,0.792428983985768,1.),(1.0000893161083,
0.792760296061316,1.),(1.00008917172342,0.793095311538391,1.),(1.00008902569065,
0.793434150628016,1.)))
REPRESENTATION_ITEM('')
SURFACE()
);
#3781=(
BOUNDED_SURFACE()
B_SPLINE_SURFACE(3,2,((#439242,#439243,#439244),(#439245,#439246,#439247),
(#439248,#439249,#439250),(#439251,#439252,#439253)),.UNSPECIFIED.,.F.,
 .F.,.F.)
B_SPLINE_SURFACE_WITH_KNOTS((4,4),(3,3),(-5.21974905012869E-6,5.74172395514398E-5),
(-0.00139822857789765,1.0005131236408),.UNSPECIFIED.)
GEOMETRIC_REPRESENTATION_ITEM()
RATIONAL_B_SPLINE_SURFACE(((1.00049256947262,0.82376895224393,1.00018060397854),
(1.00048448215733,0.826662424388206,1.00017763870887),(1.00052427784041,
0.812424361909297,1.00019223006926),(1.00059912365877,0.78564609463264,
1.00021967280237)))
REPRESENTATION_ITEM('')
SURFACE()
);
#3782=(
BOUNDED_SURFACE()
B_SPLINE_SURFACE(3,2,((#439257,#439258,#439259),(#439260,#439261,#439262),
(#439263,#439264,#439265),(#439266,#439267,#439268)),.UNSPECIFIED.,.F.,
 .F.,.F.)
B_SPLINE_SURFACE_WITH_KNOTS((4,4),(3,3),(3.22980774337777E-5,9.63764854872253E-5),
(-0.00154325936345656,1.01095292447531),.UNSPECIFIED.)
GEOMETRIC_REPRESENTATION_ITEM()
RATIONAL_B_SPLINE_SURFACE(((1.00023530983295,0.922925743796197,1.00168574728329),
(1.00015136166123,0.95042243959425,1.00108434699059),(1.00033574337392,
0.890029368953986,1.00240524789545),(1.00054260094212,0.82227447316841,
1.00388716464854)))
REPRESENTATION_ITEM('')
SURFACE()
);
#3783=(
BOUNDED_SURFACE()
B_SPLINE_SURFACE(3,2,((#439368,#439369,#439370),(#439371,#439372,#439373),
(#439374,#439375,#439376),(#439377,#439378,#439379)),.UNSPECIFIED.,.F.,
 .F.,.F.)
B_SPLINE_SURFACE_WITH_KNOTS((4,4),(3,3),(0.,0.000101260117256738),(0.,1.),
 .UNSPECIFIED.)
GEOMETRIC_REPRESENTATION_ITEM()
RATIONAL_B_SPLINE_SURFACE(((1.,0.796615278835172,1.),(1.,0.795896038055944,
1.),(1.,0.795193354661338,1.),(1.,0.794506193185553,1.)))
REPRESENTATION_ITEM('')
SURFACE()
);
#3784=(
BOUNDED_SURFACE()
B_SPLINE_SURFACE(3,2,((#439417,#439418,#439419),(#439420,#439421,#439422),
(#439423,#439424,#439425),(#439426,#439427,#439428),(#439429,#439430,#439431),
(#439432,#439433,#439434)),.UNSPECIFIED.,.F.,.F.,.F.)
B_SPLINE_SURFACE_WITH_KNOTS((4,2,4),(3,3),(-5.42101086242752E-20,1.66936432462296E-5,
3.33872864924593E-5),(0.,1.),.UNSPECIFIED.)
GEOMETRIC_REPRESENTATION_ITEM()
RATIONAL_B_SPLINE_SURFACE(((1.,0.796615278835171,1.),(1.,0.86231052441812,
1.),(1.,0.923774472010524,1.),(1.,0.923983993203427,1.),(1.,0.86257487372094,
1.),(1.,0.79661527883518,1.)))
REPRESENTATION_ITEM('')
SURFACE()
);
#3785=(
BOUNDED_SURFACE()
B_SPLINE_SURFACE(3,2,((#439471,#439472,#439473),(#439474,#439475,#439476),
(#439477,#439478,#439479),(#439480,#439481,#439482)),.UNSPECIFIED.,.F.,
 .F.,.F.)
B_SPLINE_SURFACE_WITH_KNOTS((4,4),(3,3),(0.,0.000101244905251112),(0.,1.),
 .UNSPECIFIED.)
GEOMETRIC_REPRESENTATION_ITEM()
RATIONAL_B_SPLINE_SURFACE(((1.,0.796615278835172,1.),(1.,0.795896146109793,
1.),(1.,0.795193565796501,1.),(1.,0.7945065028899,1.)))
REPRESENTATION_ITEM('')
SURFACE()
);
#3786=(
BOUNDED_SURFACE()
B_SPLINE_SURFACE(3,2,((#439518,#439519,#439520),(#439521,#439522,#439523),
(#439524,#439525,#439526),(#439527,#439528,#439529)),.UNSPECIFIED.,.F.,
 .F.,.F.)
B_SPLINE_SURFACE_WITH_KNOTS((4,4),(3,3),(2.85968127239939E-5,9.24681548475817E-5),
(-0.00167900678776883,1.01130827127819),.UNSPECIFIED.)
GEOMETRIC_REPRESENTATION_ITEM()
RATIONAL_B_SPLINE_SURFACE(((1.0005904089526,0.822187541868058,1.00401468696655),
(1.00036527718166,0.889990093671439,1.0024838267339),(1.00016469515025,
0.950399042257874,1.00111990082511),(1.00025604274011,0.922888044285987,
1.00174104990631)))
REPRESENTATION_ITEM('')
SURFACE()
);
#3787=(
BOUNDED_SURFACE()
B_SPLINE_SURFACE(3,2,((#439533,#439534,#439535),(#439536,#439537,#439538),
(#439539,#439540,#439541),(#439542,#439543,#439544)),.UNSPECIFIED.,.F.,
 .F.,.F.)
B_SPLINE_SURFACE_WITH_KNOTS((4,4),(3,3),(-5.22358356749338E-6,5.74594192424275E-5),
(-0.00127120052062783,1.),.UNSPECIFIED.)
GEOMETRIC_REPRESENTATION_ITEM()
RATIONAL_B_SPLINE_SURFACE(((1.00054449313178,0.785835073638751,1.),(1.00047707767478,
0.812351526358847,1.),(1.00044031788589,0.826810216506263,1.),(1.00044777653321,
0.823876514387255,1.)))
REPRESENTATION_ITEM('')
SURFACE()
);
#3788=(
BOUNDED_SURFACE()
B_SPLINE_SURFACE(3,2,((#439546,#439547,#439548),(#439549,#439550,#439551),
(#439552,#439553,#439554),(#439555,#439556,#439557)),.UNSPECIFIED.,.F.,
 .F.,.F.)
B_SPLINE_SURFACE_WITH_KNOTS((4,4),(3,3),(1.35525271560688E-19,4.88747512969878E-5),
(-0.000215805215419202,1.),.UNSPECIFIED.)
GEOMETRIC_REPRESENTATION_ITEM()
RATIONAL_B_SPLINE_SURFACE(((1.00008915600335,0.793434085499754,1.),(1.00008930224989,
0.793095246303315,1.),(1.00008944684611,0.792760230720557,1.),(1.0000895898439,
0.792428918540612,1.)))
REPRESENTATION_ITEM('')
SURFACE()
);
#3789=(
BOUNDED_SURFACE()
B_SPLINE_SURFACE(3,2,((#439559,#439560,#439561),(#439562,#439563,#439564),
(#439565,#439566,#439567),(#439568,#439569,#439570),(#439571,#439572,#439573),
(#439574,#439575,#439576)),.UNSPECIFIED.,.F.,.F.,.F.)
B_SPLINE_SURFACE_WITH_KNOTS((4,2,4),(3,3),(5.48877349820787E-19,7.62675010863201E-5,
0.00015253500217264),(0.,1.02152348203065),.UNSPECIFIED.)
GEOMETRIC_REPRESENTATION_ITEM()
RATIONAL_B_SPLINE_SURFACE(((1.,0.789033595401257,1.0090814632369),(1.,0.857071781054821,
1.00615262590428),(1.,0.922087264710762,1.00335390671591),(1.,0.922394466502347,
1.00334068261143),(1.,0.857224384599071,1.00614605678499),(1.,0.789033595401659,
1.00908146323689)))
REPRESENTATION_ITEM('')
SURFACE()
);
#3790=(
BOUNDED_SURFACE()
B_SPLINE_SURFACE(3,2,((#439578,#439579,#439580),(#439581,#439582,#439583),
(#439584,#439585,#439586),(#439587,#439588,#439589)),.UNSPECIFIED.,.F.,
 .F.,.F.)
B_SPLINE_SURFACE_WITH_KNOTS((4,4),(3,3),(2.98155597433514E-19,4.88747512969884E-5),
(-0.00021548985766335,1.),.UNSPECIFIED.)
GEOMETRIC_REPRESENTATION_ITEM()
RATIONAL_B_SPLINE_SURFACE(((1.00008945889739,0.792428983985614,1.),(1.00008931610861,
0.792760296061149,1.),(1.00008917172373,0.793095311538248,1.),(1.00008902569096,
0.793434150627866,1.)))
REPRESENTATION_ITEM('')
SURFACE()
);
#3791=(
BOUNDED_SURFACE()
B_SPLINE_SURFACE(3,2,((#439591,#439592,#439593),(#439594,#439595,#439596),
(#439597,#439598,#439599),(#439600,#439601,#439602)),.UNSPECIFIED.,.F.,
 .F.,.F.)
B_SPLINE_SURFACE_WITH_KNOTS((4,4),(3,3),(-5.21974905012878E-6,5.74172395514398E-5),
(-0.00139822857730411,1.00051312364056),.UNSPECIFIED.)
GEOMETRIC_REPRESENTATION_ITEM()
RATIONAL_B_SPLINE_SURFACE(((1.00049256947241,0.823768952244084,1.00018060397846),
(1.00048448215712,0.826662424388355,1.00017763870879),(1.00052427784019,
0.812424361909443,1.00019223006917),(1.00059912365852,0.78564609463282,
1.00021967280226)))
REPRESENTATION_ITEM('')
SURFACE()
);
#3792=(
BOUNDED_SURFACE()
B_SPLINE_SURFACE(3,2,((#439606,#439607,#439608),(#439609,#439610,#439611),
(#439612,#439613,#439614),(#439615,#439616,#439617)),.UNSPECIFIED.,.F.,
 .F.,.F.)
B_SPLINE_SURFACE_WITH_KNOTS((4,4),(3,3),(3.22980774337779E-5,9.63764854872255E-5),
(-0.00154325936375083,1.01095292447563),.UNSPECIFIED.)
GEOMETRIC_REPRESENTATION_ITEM()
RATIONAL_B_SPLINE_SURFACE(((1.00023530983299,0.92292574379615,1.00168574728334),
(1.00015136166126,0.950422439594203,1.00108434699062),(1.00033574337399,
0.890029368953946,1.00240524789552),(1.00054260094222,0.822274473168293,
1.00388716464865)))
REPRESENTATION_ITEM('')
SURFACE()
);
#3793=(
BOUNDED_SURFACE()
B_SPLINE_SURFACE(3,2,((#439717,#439718,#439719),(#439720,#439721,#439722),
(#439723,#439724,#439725),(#439726,#439727,#439728)),.UNSPECIFIED.,.F.,
 .F.,.F.)
B_SPLINE_SURFACE_WITH_KNOTS((4,4),(3,3),(0.,0.000101260117256737),(0.,1.),
 .UNSPECIFIED.)
GEOMETRIC_REPRESENTATION_ITEM()
RATIONAL_B_SPLINE_SURFACE(((1.,0.796615278835171,1.),(1.,0.795896038055945,
1.),(1.,0.795193354661351,1.),(1.,0.794506193185534,1.)))
REPRESENTATION_ITEM('')
SURFACE()
);
#3794=(
BOUNDED_SURFACE()
B_SPLINE_SURFACE(3,2,((#439766,#439767,#439768),(#439769,#439770,#439771),
(#439772,#439773,#439774),(#439775,#439776,#439777),(#439778,#439779,#439780),
(#439781,#439782,#439783)),.UNSPECIFIED.,.F.,.F.,.F.)
B_SPLINE_SURFACE_WITH_KNOTS((4,2,4),(3,3),(2.04981973235541E-19,1.66936432462297E-5,
3.33872864924591E-5),(0.,1.),.UNSPECIFIED.)
GEOMETRIC_REPRESENTATION_ITEM()
RATIONAL_B_SPLINE_SURFACE(((1.,0.796615278835174,1.),(1.,0.862310524418132,
1.),(1.,0.923774472010519,1.),(1.,0.923983993203426,1.),(1.,0.862574873720943,
1.),(1.,0.79661527883518,1.)))
REPRESENTATION_ITEM('')
SURFACE()
);
#3795=(
BOUNDED_SURFACE()
B_SPLINE_SURFACE(3,2,((#439820,#439821,#439822),(#439823,#439824,#439825),
(#439826,#439827,#439828),(#439829,#439830,#439831)),.UNSPECIFIED.,.F.,
 .F.,.F.)
B_SPLINE_SURFACE_WITH_KNOTS((4,4),(3,3),(-2.16840434497101E-19,0.000101244905251112),
(0.,1.),.UNSPECIFIED.)
GEOMETRIC_REPRESENTATION_ITEM()
RATIONAL_B_SPLINE_SURFACE(((1.,0.79661527883517,1.),(1.,0.795896146109799,
1.),(1.,0.795193565796492,1.),(1.,0.794506502889898,1.)))
REPRESENTATION_ITEM('')
SURFACE()
);
#3796=(
BOUNDED_SURFACE()
B_SPLINE_SURFACE(3,2,((#439867,#439868,#439869),(#439870,#439871,#439872),
(#439873,#439874,#439875),(#439876,#439877,#439878)),.UNSPECIFIED.,.F.,
 .F.,.F.)
B_SPLINE_SURFACE_WITH_KNOTS((4,4),(3,3),(2.85968127239939E-5,9.24681548475816E-5),
(-0.00167900678652977,1.01130827127818),.UNSPECIFIED.)
GEOMETRIC_REPRESENTATION_ITEM()
RATIONAL_B_SPLINE_SURFACE(((1.00059040895216,0.822187541868281,1.00401468696655),
(1.00036527718139,0.889990093671574,1.0024838267339),(1.00016469515013,
0.950399042257945,1.0011199008251),(1.00025604273992,0.922888044286082,
1.0017410499063)))
REPRESENTATION_ITEM('')
SURFACE()
);
#3797=(
BOUNDED_SURFACE()
B_SPLINE_SURFACE(3,2,((#439882,#439883,#439884),(#439885,#439886,#439887),
(#439888,#439889,#439890),(#439891,#439892,#439893)),.UNSPECIFIED.,.F.,
 .F.,.F.)
B_SPLINE_SURFACE_WITH_KNOTS((4,4),(3,3),(-5.22358356749313E-6,5.74594192424277E-5),
(-0.00127120052051313,1.),.UNSPECIFIED.)
GEOMETRIC_REPRESENTATION_ITEM()
RATIONAL_B_SPLINE_SURFACE(((1.00054449313173,0.785835073638764,1.),(1.00047707767473,
0.812351526358878,1.),(1.00044031788585,0.82681021650628,1.),(1.00044777653317,
0.823876514387266,1.)))
REPRESENTATION_ITEM('')
SURFACE()
);
#3798=(
BOUNDED_SURFACE()
B_SPLINE_SURFACE(3,2,((#439895,#439896,#439897),(#439898,#439899,#439900),
(#439901,#439902,#439903),(#439904,#439905,#439906)),.UNSPECIFIED.,.F.,
 .F.,.F.)
B_SPLINE_SURFACE_WITH_KNOTS((4,4),(3,3),(8.13151629364128E-20,4.88747512969883E-5),
(-0.000215805215948565,1.),.UNSPECIFIED.)
GEOMETRIC_REPRESENTATION_ITEM()
RATIONAL_B_SPLINE_SURFACE(((1.00008915600357,0.793434085499649,1.),(1.0000893022501,
0.793095246303197,1.),(1.00008944684633,0.792760230720471,1.),(1.00008958984412,
0.792428918540492,1.)))
REPRESENTATION_ITEM('')
SURFACE()
);
#3799=(
BOUNDED_SURFACE()
B_SPLINE_SURFACE(3,2,((#439908,#439909,#439910),(#439911,#439912,#439913),
(#439914,#439915,#439916),(#439917,#439918,#439919),(#439920,#439921,#439922),
(#439923,#439924,#439925)),.UNSPECIFIED.,.F.,.F.,.F.)
B_SPLINE_SURFACE_WITH_KNOTS((4,2,4),(3,3),(8.13151629364128E-20,7.62675010863196E-5,
0.000152535002172639),(0.,1.02152348203066),.UNSPECIFIED.)
GEOMETRIC_REPRESENTATION_ITEM()
RATIONAL_B_SPLINE_SURFACE(((1.,0.789033595401254,1.00908146323691),(1.,
0.857071781054843,1.00615262590428),(1.,0.922087264710728,1.00335390671592),
(1.,0.922394466502372,1.00334068261143),(1.,0.857224384599056,1.006146056785),
(1.,0.789033595401653,1.00908146323689)))
REPRESENTATION_ITEM('')
SURFACE()
);
#3800=(
BOUNDED_SURFACE()
B_SPLINE_SURFACE(3,2,((#439927,#439928,#439929),(#439930,#439931,#439932),
(#439933,#439934,#439935),(#439936,#439937,#439938)),.UNSPECIFIED.,.F.,
 .F.,.F.)
B_SPLINE_SURFACE_WITH_KNOTS((4,4),(3,3),(2.16840434497101E-19,4.88747512969884E-5),
(-0.000215489857764122,1.),.UNSPECIFIED.)
GEOMETRIC_REPRESENTATION_ITEM()
RATIONAL_B_SPLINE_SURFACE(((1.00008945889743,0.792428983985588,1.),(1.00008931610865,
0.792760296061136,1.),(1.00008917172377,0.793095311538216,1.),(1.000089025691,
0.793434150627844,1.)))
REPRESENTATION_ITEM('')
SURFACE()
);
#3801=(
BOUNDED_SURFACE()
B_SPLINE_SURFACE(3,2,((#439940,#439941,#439942),(#439943,#439944,#439945),
(#439946,#439947,#439948),(#439949,#439950,#439951)),.UNSPECIFIED.,.F.,
 .F.,.F.)
B_SPLINE_SURFACE_WITH_KNOTS((4,4),(3,3),(-5.21974905013083E-6,5.74172395514394E-5),
(-0.00139822857767231,1.00051312364078),.UNSPECIFIED.)
GEOMETRIC_REPRESENTATION_ITEM()
RATIONAL_B_SPLINE_SURFACE(((1.00049256947254,0.823768952243962,1.00018060397853),
(1.00048448215725,0.826662424388261,1.00017763870886),(1.00052427784033,
0.812424361909332,1.00019223006925),(1.00059912365868,0.785646094632691,
1.00021967280236)))
REPRESENTATION_ITEM('')
SURFACE()
);
#3802=(
BOUNDED_SURFACE()
B_SPLINE_SURFACE(3,2,((#439955,#439956,#439957),(#439958,#439959,#439960),
(#439961,#439962,#439963),(#439964,#439965,#439966)),.UNSPECIFIED.,.F.,
 .F.,.F.)
B_SPLINE_SURFACE_WITH_KNOTS((4,4),(3,3),(3.22980774337779E-5,9.63764854872257E-5),
(-0.00154325936399881,1.01095292447533),.UNSPECIFIED.)
GEOMETRIC_REPRESENTATION_ITEM()
RATIONAL_B_SPLINE_SURFACE(((1.00023530983303,0.922925743796152,1.00168574728329),
(1.00015136166128,0.950422439594205,1.00108434699059),(1.00033574337404,
0.890029368953934,1.00240524789545),(1.00054260094231,0.822274473168315,
1.00388716464855)))
REPRESENTATION_ITEM('')
SURFACE()
);
#3803=(
BOUNDED_SURFACE()
B_SPLINE_SURFACE(3,2,((#440066,#440067,#440068),(#440069,#440070,#440071),
(#440072,#440073,#440074),(#440075,#440076,#440077)),.UNSPECIFIED.,.F.,
 .F.,.F.)
B_SPLINE_SURFACE_WITH_KNOTS((4,4),(3,3),(0.,0.000101260117256738),(0.,1.),
 .UNSPECIFIED.)
GEOMETRIC_REPRESENTATION_ITEM()
RATIONAL_B_SPLINE_SURFACE(((1.,0.796615278835166,1.),(1.,0.795896038055944,
1.),(1.,0.795193354661345,1.),(1.,0.794506193185547,1.)))
REPRESENTATION_ITEM('')
SURFACE()
);
#3804=(
BOUNDED_SURFACE()
B_SPLINE_SURFACE(3,2,((#440115,#440116,#440117),(#440118,#440119,#440120),
(#440121,#440122,#440123),(#440124,#440125,#440126),(#440127,#440128,#440129),
(#440130,#440131,#440132)),.UNSPECIFIED.,.F.,.F.,.F.)
B_SPLINE_SURFACE_WITH_KNOTS((4,2,4),(3,3),(2.40557357020221E-19,1.66936432462298E-5,
3.33872864924593E-5),(0.,1.),.UNSPECIFIED.)
GEOMETRIC_REPRESENTATION_ITEM()
RATIONAL_B_SPLINE_SURFACE(((1.,0.796615278835179,1.),(1.,0.862310524418132,
1.),(1.,0.923774472010519,1.),(1.,0.923983993203427,1.),(1.,0.862574873720955,
1.),(1.,0.796615278835182,1.)))
REPRESENTATION_ITEM('')
SURFACE()
);
#3805=(
BOUNDED_SURFACE()
B_SPLINE_SURFACE(3,2,((#440169,#440170,#440171),(#440172,#440173,#440174),
(#440175,#440176,#440177),(#440178,#440179,#440180)),.UNSPECIFIED.,.F.,
 .F.,.F.)
B_SPLINE_SURFACE_WITH_KNOTS((4,4),(3,3),(0.,0.000101244905251112),(0.,1.),
 .UNSPECIFIED.)
GEOMETRIC_REPRESENTATION_ITEM()
RATIONAL_B_SPLINE_SURFACE(((1.,0.796615278835175,1.),(1.,0.795896146109791,
1.),(1.,0.795193565796496,1.),(1.,0.7945065028899,1.)))
REPRESENTATION_ITEM('')
SURFACE()
);
#3806=(
BOUNDED_SURFACE()
B_SPLINE_SURFACE(3,2,((#440216,#440217,#440218),(#440219,#440220,#440221),
(#440222,#440223,#440224),(#440225,#440226,#440227)),.UNSPECIFIED.,.F.,
 .F.,.F.)
B_SPLINE_SURFACE_WITH_KNOTS((4,4),(3,3),(2.85968127239939E-5,9.24681548475817E-5),
(-0.00167900678654135,1.01130827127829),.UNSPECIFIED.)
GEOMETRIC_REPRESENTATION_ITEM()
RATIONAL_B_SPLINE_SURFACE(((1.00059040895217,0.822187541868258,1.00401468696659),
(1.0003652771814,0.889990093671561,1.00248382673393),(1.00016469515013,
0.950399042257935,1.00111990082511),(1.00025604273992,0.922888044286072,
1.00174104990632)))
REPRESENTATION_ITEM('')
SURFACE()
);
#3807=(
BOUNDED_SURFACE()
B_SPLINE_SURFACE(3,2,((#440231,#440232,#440233),(#440234,#440235,#440236),
(#440237,#440238,#440239),(#440240,#440241,#440242)),.UNSPECIFIED.,.F.,
 .F.,.F.)
B_SPLINE_SURFACE_WITH_KNOTS((4,4),(3,3),(-5.22358356749291E-6,5.74594192424275E-5),
(-0.00127120052073408,1.),.UNSPECIFIED.)
GEOMETRIC_REPRESENTATION_ITEM()
RATIONAL_B_SPLINE_SURFACE(((1.00054449313183,0.785835073638734,1.),(1.00047707767482,
0.812351526358796,1.),(1.00044031788593,0.82681021650626,1.),(1.00044777653325,
0.823876514387224,1.)))
REPRESENTATION_ITEM('')
SURFACE()
);
#3808=(
BOUNDED_SURFACE()
B_SPLINE_SURFACE(3,2,((#440244,#440245,#440246),(#440247,#440248,#440249),
(#440250,#440251,#440252),(#440253,#440254,#440255)),.UNSPECIFIED.,.F.,
 .F.,.F.)
B_SPLINE_SURFACE_WITH_KNOTS((4,4),(3,3),(5.42101086242752E-20,4.88747512969882E-5),
(-0.000215805215285131,1.),.UNSPECIFIED.)
GEOMETRIC_REPRESENTATION_ITEM()
RATIONAL_B_SPLINE_SURFACE(((1.0000891560033,0.793434085499786,1.),(1.00008930224983,
0.793095246303321,1.),(1.00008944684605,0.79276023072061,1.),(1.00008958984384,
0.79242891854063,1.)))
REPRESENTATION_ITEM('')
SURFACE()
);
#3809=(
BOUNDED_SURFACE()
B_SPLINE_SURFACE(3,2,((#440257,#440258,#440259),(#440260,#440261,#440262),
(#440263,#440264,#440265),(#440266,#440267,#440268),(#440269,#440270,#440271),
(#440272,#440273,#440274)),.UNSPECIFIED.,.F.,.F.,.F.)
B_SPLINE_SURFACE_WITH_KNOTS((4,2,4),(3,3),(1.35525271560688E-19,7.62675010863197E-5,
0.000152535002172639),(0.,1.02152348203077),.UNSPECIFIED.)
GEOMETRIC_REPRESENTATION_ITEM()
RATIONAL_B_SPLINE_SURFACE(((1.,0.789033595401232,1.00908146323695),(1.,
0.857071781054877,1.00615262590431),(1.,0.922087264710654,1.00335390671594),
(1.,0.922394466502435,1.00334068261145),(1.,0.857224384598992,1.00614605678503),
(1.,0.78903359540163,1.00908146323694)))
REPRESENTATION_ITEM('')
SURFACE()
);
#3810=(
BOUNDED_SURFACE()
B_SPLINE_SURFACE(3,2,((#440276,#440277,#440278),(#440279,#440280,#440281),
(#440282,#440283,#440284),(#440285,#440286,#440287)),.UNSPECIFIED.,.F.,
 .F.,.F.)
B_SPLINE_SURFACE_WITH_KNOTS((4,4),(3,3),(3.79470760369927E-19,4.88747512969884E-5),
(-0.000215489856846097,1.),.UNSPECIFIED.)
GEOMETRIC_REPRESENTATION_ITEM()
RATIONAL_B_SPLINE_SURFACE(((1.00008945889705,0.792428983985783,1.),(1.00008931610827,
0.792760296061333,1.),(1.00008917172339,0.793095311538396,1.),(1.00008902569062,
0.793434150628034,1.)))
REPRESENTATION_ITEM('')
SURFACE()
);
#3811=(
BOUNDED_SURFACE()
B_SPLINE_SURFACE(3,2,((#440289,#440290,#440291),(#440292,#440293,#440294),
(#440295,#440296,#440297),(#440298,#440299,#440300)),.UNSPECIFIED.,.F.,
 .F.,.F.)
B_SPLINE_SURFACE_WITH_KNOTS((4,4),(3,3),(-5.21974905012864E-6,5.74172395514396E-5),
(-0.0013982285777479,1.00051312364095),.UNSPECIFIED.)
GEOMETRIC_REPRESENTATION_ITEM()
RATIONAL_B_SPLINE_SURFACE(((1.00049256947257,0.823768952243935,1.00018060397859),
(1.00048448215727,0.826662424388207,1.00017763870892),(1.00052427784036,
0.812424361909287,1.00019223006932),(1.00059912365871,0.785646094632647,
1.00021967280243)))
REPRESENTATION_ITEM('')
SURFACE()
);
#3812=(
BOUNDED_SURFACE()
B_SPLINE_SURFACE(3,2,((#440304,#440305,#440306),(#440307,#440308,#440309),
(#440310,#440311,#440312),(#440313,#440314,#440315)),.UNSPECIFIED.,.F.,
 .F.,.F.)
B_SPLINE_SURFACE_WITH_KNOTS((4,4),(3,3),(3.22980774337779E-5,9.6376485487225E-5),
(-0.00154325936373299,1.01095292447548),.UNSPECIFIED.)
GEOMETRIC_REPRESENTATION_ITEM()
RATIONAL_B_SPLINE_SURFACE(((1.00023530983299,0.922925743796163,1.00168574728332),
(1.00015136166126,0.950422439594215,1.0010843469906),(1.00033574337398,
0.89002936895396,1.00240524789549),(1.00054260094221,0.822274473168319,
1.0038871646486)))
REPRESENTATION_ITEM('')
SURFACE()
);
#3813=(
BOUNDED_SURFACE()
B_SPLINE_SURFACE(3,2,((#440415,#440416,#440417),(#440418,#440419,#440420),
(#440421,#440422,#440423),(#440424,#440425,#440426)),.UNSPECIFIED.,.F.,
 .F.,.F.)
B_SPLINE_SURFACE_WITH_KNOTS((4,4),(3,3),(-4.33680868994202E-19,0.000101260117256738),
(0.,1.),.UNSPECIFIED.)
GEOMETRIC_REPRESENTATION_ITEM()
RATIONAL_B_SPLINE_SURFACE(((1.,0.796615278835173,1.),(1.,0.795896038055942,
1.),(1.,0.795193354661347,1.),(1.,0.794506193185554,1.)))
REPRESENTATION_ITEM('')
SURFACE()
);
#3814=(
BOUNDED_SURFACE()
B_SPLINE_SURFACE(3,2,((#440464,#440465,#440466),(#440467,#440468,#440469),
(#440470,#440471,#440472),(#440473,#440474,#440475),(#440476,#440477,#440478),
(#440479,#440480,#440481)),.UNSPECIFIED.,.F.,.F.,.F.)
B_SPLINE_SURFACE_WITH_KNOTS((4,2,4),(3,3),(1.76182853028894E-19,1.66936432462295E-5,
3.33872864924588E-5),(0.,1.),.UNSPECIFIED.)
GEOMETRIC_REPRESENTATION_ITEM()
RATIONAL_B_SPLINE_SURFACE(((1.,0.796615278835175,1.),(1.,0.862310524418126,
1.),(1.,0.92377447201052,1.),(1.,0.923983993203426,1.),(1.,0.862574873720947,
1.),(1.,0.796615278835184,1.)))
REPRESENTATION_ITEM('')
SURFACE()
);
#3815=(
BOUNDED_SURFACE()
B_SPLINE_SURFACE(3,2,((#440518,#440519,#440520),(#440521,#440522,#440523),
(#440524,#440525,#440526),(#440527,#440528,#440529)),.UNSPECIFIED.,.F.,
 .F.,.F.)
B_SPLINE_SURFACE_WITH_KNOTS((4,4),(3,3),(0.,0.000101244905251112),(0.,1.),
 .UNSPECIFIED.)
GEOMETRIC_REPRESENTATION_ITEM()
RATIONAL_B_SPLINE_SURFACE(((1.,0.796615278835171,1.),(1.,0.795896146109794,
1.),(1.,0.795193565796501,1.),(1.,0.7945065028899,1.)))
REPRESENTATION_ITEM('')
SURFACE()
);
#3816=(
BOUNDED_SURFACE()
B_SPLINE_SURFACE(3,2,((#440565,#440566,#440567),(#440568,#440569,#440570),
(#440571,#440572,#440573),(#440574,#440575,#440576)),.UNSPECIFIED.,.F.,
 .F.,.F.)
B_SPLINE_SURFACE_WITH_KNOTS((4,4),(3,3),(2.85968127239939E-5,9.24681548475816E-5),
(-0.0016790067933083,1.01130827127841),.UNSPECIFIED.)
GEOMETRIC_REPRESENTATION_ITEM()
RATIONAL_B_SPLINE_SURFACE(((1.00059040895455,0.822187541867025,1.00401468696663),
(1.00036527718287,0.889990093670798,1.00248382673395),(1.00016469515079,
0.950399042257587,1.00111990082513),(1.00025604274096,0.922888044285538,
1.00174104990634)))
REPRESENTATION_ITEM('')
SURFACE()
);
#3817=(
BOUNDED_SURFACE()
B_SPLINE_SURFACE(3,2,((#440580,#440581,#440582),(#440583,#440584,#440585),
(#440586,#440587,#440588),(#440589,#440590,#440591)),.UNSPECIFIED.,.F.,
 .F.,.F.)
B_SPLINE_SURFACE_WITH_KNOTS((4,4),(3,3),(-5.22358356749145E-6,5.74594192424276E-5),
(-0.00127120052070219,1.),.UNSPECIFIED.)
GEOMETRIC_REPRESENTATION_ITEM()
RATIONAL_B_SPLINE_SURFACE(((1.00054449313181,0.785835073638729,1.),(1.0004770776748,
0.812351526358837,1.),(1.00044031788592,0.826810216506255,1.),(1.00044777653324,
0.823876514387233,1.)))
REPRESENTATION_ITEM('')
SURFACE()
);
#3818=(
BOUNDED_SURFACE()
B_SPLINE_SURFACE(3,2,((#440593,#440594,#440595),(#440596,#440597,#440598),
(#440599,#440600,#440601),(#440602,#440603,#440604)),.UNSPECIFIED.,.F.,
 .F.,.F.)
B_SPLINE_SURFACE_WITH_KNOTS((4,4),(3,3),(-1.35525271560688E-19,4.88747512969876E-5),
(-0.000215805215528143,1.),.UNSPECIFIED.)
GEOMETRIC_REPRESENTATION_ITEM()
RATIONAL_B_SPLINE_SURFACE(((1.0000891560034,0.793434085499736,1.),(1.00008930224993,
0.793095246303264,1.),(1.00008944684615,0.79276023072058,1.),(1.00008958984394,
0.79242891854058,1.)))
REPRESENTATION_ITEM('')
SURFACE()
);
#3819=(
BOUNDED_SURFACE()
B_SPLINE_SURFACE(3,2,((#440606,#440607,#440608),(#440609,#440610,#440611),
(#440612,#440613,#440614),(#440615,#440616,#440617),(#440618,#440619,#440620),
(#440621,#440622,#440623)),.UNSPECIFIED.,.F.,.F.,.F.)
B_SPLINE_SURFACE_WITH_KNOTS((4,2,4),(3,3),(3.72694496791892E-19,7.62675010863197E-5,
0.000152535002172639),(0.,1.02152348203055),.UNSPECIFIED.)
GEOMETRIC_REPRESENTATION_ITEM()
RATIONAL_B_SPLINE_SURFACE(((1.,0.789033595401277,1.00908146323686),(1.,
0.857071781054852,1.00615262590425),(1.,0.922087264710738,1.0033539067159),
(1.,0.922394466502381,1.00334068261141),(1.,0.857224384599074,1.00614605678497),
(1.,0.78903359540167,1.00908146323685)))
REPRESENTATION_ITEM('')
SURFACE()
);
#3820=(
BOUNDED_SURFACE()
B_SPLINE_SURFACE(3,2,((#440625,#440626,#440627),(#440628,#440629,#440630),
(#440631,#440632,#440633),(#440634,#440635,#440636)),.UNSPECIFIED.,.F.,
 .F.,.F.)
B_SPLINE_SURFACE_WITH_KNOTS((4,4),(3,3),(5.42101086242752E-19,4.88747512969886E-5),
(-0.000215489857798702,1.),.UNSPECIFIED.)
GEOMETRIC_REPRESENTATION_ITEM()
RATIONAL_B_SPLINE_SURFACE(((1.00008945889745,0.792428983985586,1.),(1.00008931610866,
0.792760296061132,1.),(1.00008917172379,0.79309531153821,1.),(1.00008902569101,
0.793434150627838,1.)))
REPRESENTATION_ITEM('')
SURFACE()
);
#3821=(
BOUNDED_SURFACE()
B_SPLINE_SURFACE(3,2,((#440638,#440639,#440640),(#440641,#440642,#440643),
(#440644,#440645,#440646),(#440647,#440648,#440649)),.UNSPECIFIED.,.F.,
 .F.,.F.)
B_SPLINE_SURFACE_WITH_KNOTS((4,4),(3,3),(-5.21974905013097E-6,5.74172395514412E-5),
(-0.00139822857775902,1.00051312364059),.UNSPECIFIED.)
GEOMETRIC_REPRESENTATION_ITEM()
RATIONAL_B_SPLINE_SURFACE(((1.00049256947257,0.823768952243987,1.00018060397847),
(1.00048448215728,0.826662424388286,1.0001776387088),(1.00052427784036,
0.812424361909344,1.00019223006918),(1.00059912365871,0.785646094632718,
1.00021967280228)))
REPRESENTATION_ITEM('')
SURFACE()
);
#3822=(
BOUNDED_SURFACE()
B_SPLINE_SURFACE(3,2,((#440653,#440654,#440655),(#440656,#440657,#440658),
(#440659,#440660,#440661),(#440662,#440663,#440664)),.UNSPECIFIED.,.F.,
 .F.,.F.)
B_SPLINE_SURFACE_WITH_KNOTS((4,4),(3,3),(3.22980774337779E-5,9.63764854872251E-5),
(-0.00154325936285191,1.01095292447548),.UNSPECIFIED.)
GEOMETRIC_REPRESENTATION_ITEM()
RATIONAL_B_SPLINE_SURFACE(((1.00023530983285,0.922925743796228,1.00168574728332),
(1.00015136166117,0.950422439594265,1.0010843469906),(1.00033574337379,
0.890029368954041,1.00240524789549),(1.0005426009419,0.822274473168488,
1.0038871646486)))
REPRESENTATION_ITEM('')
SURFACE()
);
#3823=(
BOUNDED_SURFACE()
B_SPLINE_SURFACE(3,2,((#440764,#440765,#440766),(#440767,#440768,#440769),
(#440770,#440771,#440772),(#440773,#440774,#440775)),.UNSPECIFIED.,.F.,
 .F.,.F.)
B_SPLINE_SURFACE_WITH_KNOTS((4,4),(3,3),(0.,0.000101260117256737),(0.,1.),
 .UNSPECIFIED.)
GEOMETRIC_REPRESENTATION_ITEM()
RATIONAL_B_SPLINE_SURFACE(((1.,0.796615278835173,1.),(1.,0.795896038055929,
1.),(1.,0.795193354661366,1.),(1.,0.794506193185535,1.)))
REPRESENTATION_ITEM('')
SURFACE()
);
#3824=(
BOUNDED_SURFACE()
B_SPLINE_SURFACE(3,2,((#440813,#440814,#440815),(#440816,#440817,#440818),
(#440819,#440820,#440821),(#440822,#440823,#440824),(#440825,#440826,#440827),
(#440828,#440829,#440830)),.UNSPECIFIED.,.F.,.F.,.F.)
B_SPLINE_SURFACE_WITH_KNOTS((4,2,4),(3,3),(-1.575481281893E-19,1.66936432462296E-5,
3.33872864924593E-5),(0.,1.),.UNSPECIFIED.)
GEOMETRIC_REPRESENTATION_ITEM()
RATIONAL_B_SPLINE_SURFACE(((1.,0.796615278835169,1.),(1.,0.862310524418131,
1.),(1.,0.923774472010519,1.),(1.,0.923983993203425,1.),(1.,0.862574873720939,
1.),(1.,0.796615278835181,1.)))
REPRESENTATION_ITEM('')
SURFACE()
);
#3825=(
BOUNDED_SURFACE()
B_SPLINE_SURFACE(3,2,((#440867,#440868,#440869),(#440870,#440871,#440872),
(#440873,#440874,#440875),(#440876,#440877,#440878)),.UNSPECIFIED.,.F.,
 .F.,.F.)
B_SPLINE_SURFACE_WITH_KNOTS((4,4),(3,3),(2.16840434497101E-19,0.000101244905251112),
(0.,1.),.UNSPECIFIED.)
GEOMETRIC_REPRESENTATION_ITEM()
RATIONAL_B_SPLINE_SURFACE(((1.,0.796615278835173,1.),(1.,0.795896146109799,
1.),(1.,0.795193565796499,1.),(1.,0.794506502889902,1.)))
REPRESENTATION_ITEM('')
SURFACE()
);
#3826=(
BOUNDED_SURFACE()
B_SPLINE_SURFACE(3,2,((#440914,#440915,#440916),(#440917,#440918,#440919),
(#440920,#440921,#440922),(#440923,#440924,#440925)),.UNSPECIFIED.,.F.,
 .F.,.F.)
B_SPLINE_SURFACE_WITH_KNOTS((4,4),(3,3),(2.85968127239939E-5,9.24681548475817E-5),
(-0.00167900678819985,1.01130827127813),.UNSPECIFIED.)
GEOMETRIC_REPRESENTATION_ITEM()
RATIONAL_B_SPLINE_SURFACE(((1.00059040895275,0.82218754186799,1.00401468696653),
(1.00036527718176,0.889990093671399,1.00248382673389),(1.00016469515029,
0.950399042257849,1.0011199008251),(1.00025604274018,0.922888044285957,
1.0017410499063)))
REPRESENTATION_ITEM('')
SURFACE()
);
#3827=(
BOUNDED_SURFACE()
B_SPLINE_SURFACE(3,2,((#440929,#440930,#440931),(#440932,#440933,#440934),
(#440935,#440936,#440937),(#440938,#440939,#440940)),.UNSPECIFIED.,.F.,
 .F.,.F.)
B_SPLINE_SURFACE_WITH_KNOTS((4,4),(3,3),(-5.22358356749294E-6,5.74594192424276E-5),
(-0.00127120052064046,1.),.UNSPECIFIED.)
GEOMETRIC_REPRESENTATION_ITEM()
RATIONAL_B_SPLINE_SURFACE(((1.00054449313179,0.785835073638756,1.),(1.00047707767478,
0.812351526358813,1.),(1.00044031788589,0.826810216506291,1.),(1.00044777653322,
0.823876514387238,1.)))
REPRESENTATION_ITEM('')
SURFACE()
);
#3828=(
BOUNDED_SURFACE()
B_SPLINE_SURFACE(3,2,((#440942,#440943,#440944),(#440945,#440946,#440947),
(#440948,#440949,#440950),(#440951,#440952,#440953)),.UNSPECIFIED.,.F.,
 .F.,.F.)
B_SPLINE_SURFACE_WITH_KNOTS((4,4),(3,3),(-8.13151629364128E-20,4.88747512969884E-5),
(-0.000215805215829361,1.),.UNSPECIFIED.)
GEOMETRIC_REPRESENTATION_ITEM()
RATIONAL_B_SPLINE_SURFACE(((1.00008915600352,0.793434085499674,1.),(1.00008930225006,
0.793095246303229,1.),(1.00008944684628,0.792760230720482,1.),(1.00008958984407,
0.792428918540523,1.)))
REPRESENTATION_ITEM('')
SURFACE()
);
#3829=(
BOUNDED_SURFACE()
B_SPLINE_SURFACE(3,2,((#440955,#440956,#440957),(#440958,#440959,#440960),
(#440961,#440962,#440963),(#440964,#440965,#440966),(#440967,#440968,#440969),
(#440970,#440971,#440972)),.UNSPECIFIED.,.F.,.F.,.F.)
B_SPLINE_SURFACE_WITH_KNOTS((4,2,4),(3,3),(2.10064170919066E-19,7.62675010863199E-5,
0.00015253500217264),(0.,1.02152348203051),.UNSPECIFIED.)
GEOMETRIC_REPRESENTATION_ITEM()
RATIONAL_B_SPLINE_SURFACE(((1.,0.789033595401284,1.00908146323684),(1.,
0.857071781054853,1.00615262590424),(1.,0.922087264710752,1.00335390671589),
(1.,0.922394466502378,1.00334068261141),(1.,0.857224384599074,1.00614605678495),
(1.,0.78903359540169,1.00908146323683)))
REPRESENTATION_ITEM('')
SURFACE()
);
#3830=(
BOUNDED_SURFACE()
B_SPLINE_SURFACE(3,2,((#440974,#440975,#440976),(#440977,#440978,#440979),
(#440980,#440981,#440982),(#440983,#440984,#440985)),.UNSPECIFIED.,.F.,
 .F.,.F.)
B_SPLINE_SURFACE_WITH_KNOTS((4,4),(3,3),(2.98155597433514E-19,4.88747512969883E-5),
(-0.000215489857094047,1.),.UNSPECIFIED.)
GEOMETRIC_REPRESENTATION_ITEM()
RATIONAL_B_SPLINE_SURFACE(((1.00008945889716,0.792428983985731,1.),(1.00008931610837,
0.792760296061287,1.),(1.0000891717235,0.793095311538365,1.),(1.00008902569072,
0.793434150627986,1.)))
REPRESENTATION_ITEM('')
SURFACE()
);
#3831=(
BOUNDED_SURFACE()
B_SPLINE_SURFACE(3,2,((#440987,#440988,#440989),(#440990,#440991,#440992),
(#440993,#440994,#440995),(#440996,#440997,#440998)),.UNSPECIFIED.,.F.,
 .F.,.F.)
B_SPLINE_SURFACE_WITH_KNOTS((4,4),(3,3),(-5.2197490501308E-6,5.74172395514384E-5),
(-0.00139822857742788,1.00051312364056),.UNSPECIFIED.)
GEOMETRIC_REPRESENTATION_ITEM()
RATIONAL_B_SPLINE_SURFACE(((1.00049256947246,0.823768952244055,1.00018060397845),
(1.00048448215716,0.826662424388338,1.00017763870878),(1.00052427784024,
0.81242436190943,1.00019223006917),(1.00059912365857,0.785646094632794,
1.00021967280226)))
REPRESENTATION_ITEM('')
SURFACE()
);
#3832=(
BOUNDED_SURFACE()
B_SPLINE_SURFACE(3,2,((#441002,#441003,#441004),(#441005,#441006,#441007),
(#441008,#441009,#441010),(#441011,#441012,#441013)),.UNSPECIFIED.,.F.,
 .F.,.F.)
B_SPLINE_SURFACE_WITH_KNOTS((4,4),(3,3),(3.2298077433778E-5,9.6376485487225E-5),
(-0.00154325936375615,1.01095292447547),.UNSPECIFIED.)
GEOMETRIC_REPRESENTATION_ITEM()
RATIONAL_B_SPLINE_SURFACE(((1.00023530983299,0.922925743796159,1.00168574728332),
(1.00015136166126,0.950422439594215,1.0010843469906),(1.00033574337399,
0.890029368953947,1.00240524789549),(1.00054260094222,0.822274473168324,
1.00388716464859)))
REPRESENTATION_ITEM('')
SURFACE()
);
#3833=(
BOUNDED_SURFACE()
B_SPLINE_SURFACE(3,2,((#441113,#441114,#441115),(#441116,#441117,#441118),
(#441119,#441120,#441121),(#441122,#441123,#441124)),.UNSPECIFIED.,.F.,
 .F.,.F.)
B_SPLINE_SURFACE_WITH_KNOTS((4,4),(3,3),(0.,0.000101260117256738),(0.,1.),
 .UNSPECIFIED.)
GEOMETRIC_REPRESENTATION_ITEM()
RATIONAL_B_SPLINE_SURFACE(((1.,0.796615278835173,1.),(1.,0.795896038055945,
1.),(1.,0.795193354661346,1.),(1.,0.794506193185549,1.)))
REPRESENTATION_ITEM('')
SURFACE()
);
#3834=(
BOUNDED_SURFACE()
B_SPLINE_SURFACE(3,2,((#441162,#441163,#441164),(#441165,#441166,#441167),
(#441168,#441169,#441170),(#441171,#441172,#441173),(#441174,#441175,#441176),
(#441177,#441178,#441179)),.UNSPECIFIED.,.F.,.F.,.F.)
B_SPLINE_SURFACE_WITH_KNOTS((4,2,4),(3,3),(-1.9312351197398E-19,1.66936432462293E-5,
3.33872864924588E-5),(0.,1.),.UNSPECIFIED.)
GEOMETRIC_REPRESENTATION_ITEM()
RATIONAL_B_SPLINE_SURFACE(((1.,0.796615278835169,1.),(1.,0.862310524418132,
1.),(1.,0.92377447201052,1.),(1.,0.923983993203426,1.),(1.,0.86257487372095,
1.),(1.,0.796615278835187,1.)))
REPRESENTATION_ITEM('')
SURFACE()
);
#3835=(
BOUNDED_SURFACE()
B_SPLINE_SURFACE(3,2,((#441216,#441217,#441218),(#441219,#441220,#441221),
(#441222,#441223,#441224),(#441225,#441226,#441227)),.UNSPECIFIED.,.F.,
 .F.,.F.)
B_SPLINE_SURFACE_WITH_KNOTS((4,4),(3,3),(2.16840434497101E-19,0.000101244905251112),
(0.,1.),.UNSPECIFIED.)
GEOMETRIC_REPRESENTATION_ITEM()
RATIONAL_B_SPLINE_SURFACE(((1.,0.796615278835169,1.),(1.,0.795896146109799,
1.),(1.,0.795193565796484,1.),(1.,0.794506502889905,1.)))
REPRESENTATION_ITEM('')
SURFACE()
);
#3836=(
BOUNDED_SURFACE()
B_SPLINE_SURFACE(3,2,((#441263,#441264,#441265),(#441266,#441267,#441268),
(#441269,#441270,#441271),(#441272,#441273,#441274)),.UNSPECIFIED.,.F.,
 .F.,.F.)
B_SPLINE_SURFACE_WITH_KNOTS((4,4),(3,3),(2.85968127239939E-5,9.24681548475816E-5),
(-0.00167900678719404,1.01130827127821),.UNSPECIFIED.)
GEOMETRIC_REPRESENTATION_ITEM()
RATIONAL_B_SPLINE_SURFACE(((1.0005904089524,0.822187541868157,1.00401468696656),
(1.00036527718154,0.889990093671496,1.00248382673391),(1.00016469515019,
0.950399042257903,1.00111990082511),(1.00025604274002,0.922888044286031,
1.00174104990631)))
REPRESENTATION_ITEM('')
SURFACE()
);
#3837=(
BOUNDED_SURFACE()
B_SPLINE_SURFACE(3,2,((#441278,#441279,#441280),(#441281,#441282,#441283),
(#441284,#441285,#441286),(#441287,#441288,#441289)),.UNSPECIFIED.,.F.,
 .F.,.F.)
B_SPLINE_SURFACE_WITH_KNOTS((4,4),(3,3),(-5.22358356749284E-6,5.74594192424277E-5),
(-0.00127120052058705,1.),.UNSPECIFIED.)
GEOMETRIC_REPRESENTATION_ITEM()
RATIONAL_B_SPLINE_SURFACE(((1.00054449313176,0.785835073638765,1.),(1.00047707767476,
0.812351526358836,1.),(1.00044031788588,0.826810216506289,1.),(1.0004477765332,
0.82387651438725,1.)))
REPRESENTATION_ITEM('')
SURFACE()
);
#3838=(
BOUNDED_SURFACE()
B_SPLINE_SURFACE(3,2,((#441291,#441292,#441293),(#441294,#441295,#441296),
(#441297,#441298,#441299),(#441300,#441301,#441302)),.UNSPECIFIED.,.F.,
 .F.,.F.)
B_SPLINE_SURFACE_WITH_KNOTS((4,4),(3,3),(-4.60785923306339E-19,4.88747512969882E-5),
(-0.00021580521588719,1.),.UNSPECIFIED.)
GEOMETRIC_REPRESENTATION_ITEM()
RATIONAL_B_SPLINE_SURFACE(((1.00008915600355,0.793434085499662,1.),(1.00008930225008,
0.793095246303215,1.),(1.0000894468463,0.792760230720473,1.),(1.00008958984409,
0.792428918540512,1.)))
REPRESENTATION_ITEM('')
SURFACE()
);
#3839=(
BOUNDED_SURFACE()
B_SPLINE_SURFACE(3,2,((#441304,#441305,#441306),(#441307,#441308,#441309),
(#441310,#441311,#441312),(#441313,#441314,#441315),(#441316,#441317,#441318),
(#441319,#441320,#441321)),.UNSPECIFIED.,.F.,.F.,.F.)
B_SPLINE_SURFACE_WITH_KNOTS((4,2,4),(3,3),(2.71050543121376E-19,7.62675010863194E-5,
0.000152535002172639),(0.,1.02152348203075),.UNSPECIFIED.)
GEOMETRIC_REPRESENTATION_ITEM()
RATIONAL_B_SPLINE_SURFACE(((1.,0.789033595401236,1.00908146323695),(1.,
0.857071781054828,1.00615262590431),(1.,0.922087264710721,1.00335390671593),
(1.,0.922394466502373,1.00334068261145),(1.,0.857224384599039,1.00614605678502),
(1.,0.789033595401634,1.00908146323693)))
REPRESENTATION_ITEM('')
SURFACE()
);
#3840=(
BOUNDED_SURFACE()
B_SPLINE_SURFACE(3,2,((#441323,#441324,#441325),(#441326,#441327,#441328),
(#441329,#441330,#441331),(#441332,#441333,#441334)),.UNSPECIFIED.,.F.,
 .F.,.F.)
B_SPLINE_SURFACE_WITH_KNOTS((4,4),(3,3),(3.52365706057789E-19,4.88747512969884E-5),
(-0.000215489857661774,1.),.UNSPECIFIED.)
GEOMETRIC_REPRESENTATION_ITEM()
RATIONAL_B_SPLINE_SURFACE(((1.00008945889739,0.792428983985612,1.),(1.00008931610861,
0.792760296061157,1.),(1.00008917172373,0.79309531153824,1.),(1.00008902569096,
0.793434150627865,1.)))
REPRESENTATION_ITEM('')
SURFACE()
);
#3841=(
BOUNDED_SURFACE()
B_SPLINE_SURFACE(3,2,((#441336,#441337,#441338),(#441339,#441340,#441341),
(#441342,#441343,#441344),(#441345,#441346,#441347)),.UNSPECIFIED.,.F.,
 .F.,.F.)
B_SPLINE_SURFACE_WITH_KNOTS((4,4),(3,3),(-5.21974905013096E-6,5.74172395514412E-5),
(-0.00139822857786666,1.00051312364074),.UNSPECIFIED.)
GEOMETRIC_REPRESENTATION_ITEM()
RATIONAL_B_SPLINE_SURFACE(((1.00049256947261,0.823768952243954,1.00018060397852),
(1.00048448215732,0.826662424388216,1.00017763870884),(1.0005242778404,
0.812424361909314,1.00019223006924),(1.00059912365876,0.785646094632656,
1.00021967280234)))
REPRESENTATION_ITEM('')
SURFACE()
);
#3842=(
BOUNDED_SURFACE()
B_SPLINE_SURFACE(3,2,((#441351,#441352,#441353),(#441354,#441355,#441356),
(#441357,#441358,#441359),(#441360,#441361,#441362)),.UNSPECIFIED.,.F.,
 .F.,.F.)
B_SPLINE_SURFACE_WITH_KNOTS((4,4),(3,3),(3.22980774337779E-5,9.63764854872255E-5),
(-0.00154325936374115,1.01095292447532),.UNSPECIFIED.)
GEOMETRIC_REPRESENTATION_ITEM()
RATIONAL_B_SPLINE_SURFACE(((1.00023530983299,0.92292574379617,1.00168574728329),
(1.00015136166126,0.950422439594228,1.00108434699059),(1.00033574337398,
0.890029368953965,1.00240524789545),(1.00054260094222,0.822274473168348,
1.00388716464854)))
REPRESENTATION_ITEM('')
SURFACE()
);
#3843=(
BOUNDED_SURFACE()
B_SPLINE_SURFACE(3,2,((#441462,#441463,#441464),(#441465,#441466,#441467),
(#441468,#441469,#441470),(#441471,#441472,#441473)),.UNSPECIFIED.,.F.,
 .F.,.F.)
B_SPLINE_SURFACE_WITH_KNOTS((4,4),(3,3),(0.,0.000101260117256738),(0.,1.),
 .UNSPECIFIED.)
GEOMETRIC_REPRESENTATION_ITEM()
RATIONAL_B_SPLINE_SURFACE(((1.,0.796615278835171,1.),(1.,0.795896038055941,
1.),(1.,0.795193354661349,1.),(1.,0.794506193185546,1.)))
REPRESENTATION_ITEM('')
SURFACE()
);
#3844=(
BOUNDED_SURFACE()
B_SPLINE_SURFACE(3,2,((#441511,#441512,#441513),(#441514,#441515,#441516),
(#441517,#441518,#441519),(#441520,#441521,#441522),(#441523,#441524,#441525),
(#441526,#441527,#441528)),.UNSPECIFIED.,.F.,.F.,.F.)
B_SPLINE_SURFACE_WITH_KNOTS((4,2,4),(3,3),(-5.0821976835258E-20,1.66936432462292E-5,
3.33872864924585E-5),(0.,1.),.UNSPECIFIED.)
GEOMETRIC_REPRESENTATION_ITEM()
RATIONAL_B_SPLINE_SURFACE(((1.,0.796615278835176,1.),(1.,0.86231052441814,
1.),(1.,0.923774472010514,1.),(1.,0.923983993203431,1.),(1.,0.862574873720946,
1.),(1.,0.79661527883519,1.)))
REPRESENTATION_ITEM('')
SURFACE()
);
#3845=(
BOUNDED_SURFACE()
B_SPLINE_SURFACE(3,2,((#441565,#441566,#441567),(#441568,#441569,#441570),
(#441571,#441572,#441573),(#441574,#441575,#441576)),.UNSPECIFIED.,.F.,
 .F.,.F.)
B_SPLINE_SURFACE_WITH_KNOTS((4,4),(3,3),(0.,0.000101244905251112),(0.,1.),
 .UNSPECIFIED.)
GEOMETRIC_REPRESENTATION_ITEM()
RATIONAL_B_SPLINE_SURFACE(((1.,0.796615278835168,1.),(1.,0.795896146109792,
1.),(1.,0.795193565796498,1.),(1.,0.794506502889897,1.)))
REPRESENTATION_ITEM('')
SURFACE()
);
#3846=(
BOUNDED_SURFACE()
B_SPLINE_SURFACE(3,2,((#441612,#441613,#441614),(#441615,#441616,#441617),
(#441618,#441619,#441620),(#441621,#441622,#441623)),.UNSPECIFIED.,.F.,
 .F.,.F.)
B_SPLINE_SURFACE_WITH_KNOTS((4,4),(3,3),(2.85968127239939E-5,9.24681548475815E-5),
(-0.00167900678670198,1.01130827127827),.UNSPECIFIED.)
GEOMETRIC_REPRESENTATION_ITEM()
RATIONAL_B_SPLINE_SURFACE(((1.00059040895222,0.822187541868232,1.00401468696659),
(1.00036527718143,0.889990093671556,1.00248382673392),(1.00016469515015,
0.950399042257909,1.00111990082511),(1.00025604273995,0.922888044286064,
1.00174104990632)))
REPRESENTATION_ITEM('')
SURFACE()
);
#3847=(
BOUNDED_SURFACE()
B_SPLINE_SURFACE(3,2,((#441627,#441628,#441629),(#441630,#441631,#441632),
(#441633,#441634,#441635),(#441636,#441637,#441638)),.UNSPECIFIED.,.F.,
 .F.,.F.)
B_SPLINE_SURFACE_WITH_KNOTS((4,4),(3,3),(-5.22358356749263E-6,5.74594192424276E-5),
(-0.00127120052053174,1.),.UNSPECIFIED.)
GEOMETRIC_REPRESENTATION_ITEM()
RATIONAL_B_SPLINE_SURFACE(((1.00054449313174,0.785835073638776,1.),(1.00047707767474,
0.812351526358855,1.),(1.00044031788586,0.826810216506291,1.),(1.00044777653318,
0.823876514387259,1.)))
REPRESENTATION_ITEM('')
SURFACE()
);
#3848=(
BOUNDED_SURFACE()
B_SPLINE_SURFACE(3,2,((#441640,#441641,#441642),(#441643,#441644,#441645),
(#441646,#441647,#441648),(#441649,#441650,#441651)),.UNSPECIFIED.,.F.,
 .F.,.F.)
B_SPLINE_SURFACE_WITH_KNOTS((4,4),(3,3),(-3.25260651745651E-19,4.88747512969878E-5),
(-0.000215805214925867,1.),.UNSPECIFIED.)
GEOMETRIC_REPRESENTATION_ITEM()
RATIONAL_B_SPLINE_SURFACE(((1.00008915600315,0.793434085499861,1.),(1.00008930224968,
0.793095246303394,1.),(1.0000894468459,0.79276023072068,1.),(1.00008958984369,
0.79242891854071,1.)))
REPRESENTATION_ITEM('')
SURFACE()
);
#3849=(
BOUNDED_SURFACE()
B_SPLINE_SURFACE(3,2,((#441653,#441654,#441655),(#441656,#441657,#441658),
(#441659,#441660,#441661),(#441662,#441663,#441664),(#441665,#441666,#441667),
(#441668,#441669,#441670)),.UNSPECIFIED.,.F.,.F.,.F.)
B_SPLINE_SURFACE_WITH_KNOTS((4,2,4),(3,3),(1.0842021724855E-19,7.62675010863196E-5,
0.000152535002172639),(0.,1.02152348203107),.UNSPECIFIED.)
GEOMETRIC_REPRESENTATION_ITEM()
RATIONAL_B_SPLINE_SURFACE(((1.,0.789033595401171,1.00908146323708),(1.,
0.857071781054833,1.0061526259044),(1.,0.922087264710633,1.00335390671598),
(1.,0.922394466502411,1.00334068261149),(1.,0.857224384598956,1.00614605678512),
(1.,0.789033595401567,1.00908146323707)))
REPRESENTATION_ITEM('')
SURFACE()
);
#3850=(
BOUNDED_SURFACE()
B_SPLINE_SURFACE(3,2,((#441672,#441673,#441674),(#441675,#441676,#441677),
(#441678,#441679,#441680),(#441681,#441682,#441683)),.UNSPECIFIED.,.F.,
 .F.,.F.)
B_SPLINE_SURFACE_WITH_KNOTS((4,4),(3,3),(4.87890977618477E-19,4.88747512969882E-5),
(-0.000215489856788559,1.),.UNSPECIFIED.)
GEOMETRIC_REPRESENTATION_ITEM()
RATIONAL_B_SPLINE_SURFACE(((1.00008945889703,0.792428983985793,1.),(1.00008931610825,
0.792760296061348,1.),(1.00008917172337,0.793095311538401,1.),(1.0000890256906,
0.793434150628046,1.)))
REPRESENTATION_ITEM('')
SURFACE()
);
#3851=(
BOUNDED_SURFACE()
B_SPLINE_SURFACE(3,2,((#441685,#441686,#441687),(#441688,#441689,#441690),
(#441691,#441692,#441693),(#441694,#441695,#441696)),.UNSPECIFIED.,.F.,
 .F.,.F.)
B_SPLINE_SURFACE_WITH_KNOTS((4,4),(3,3),(-5.21974905012872E-6,5.74172395514387E-5),
(-0.00139822857731876,1.00051312364056),.UNSPECIFIED.)
GEOMETRIC_REPRESENTATION_ITEM()
RATIONAL_B_SPLINE_SURFACE(((1.00049256947242,0.82376895224407,1.00018060397845),
(1.00048448215713,0.826662424388353,1.00017763870878),(1.00052427784019,
0.812424361909445,1.00019223006917),(1.00059912365853,0.785646094632814,
1.00021967280226)))
REPRESENTATION_ITEM('')
SURFACE()
);
#3852=(
BOUNDED_SURFACE()
B_SPLINE_SURFACE(3,2,((#441700,#441701,#441702),(#441703,#441704,#441705),
(#441706,#441707,#441708),(#441709,#441710,#441711)),.UNSPECIFIED.,.F.,
 .F.,.F.)
B_SPLINE_SURFACE_WITH_KNOTS((4,4),(3,3),(3.22980774337779E-5,9.63764854872246E-5),
(-0.00154325936327203,1.01095292447554),.UNSPECIFIED.)
GEOMETRIC_REPRESENTATION_ITEM()
RATIONAL_B_SPLINE_SURFACE(((1.00023530983292,0.922925743796195,1.00168574728333),
(1.00015136166121,0.950422439594221,1.00108434699061),(1.00033574337388,
0.890029368954008,1.0024052478955),(1.00054260094205,0.822274473168397,
1.00388716464862)))
REPRESENTATION_ITEM('')
SURFACE()
);
#3853=(
BOUNDED_SURFACE()
B_SPLINE_SURFACE(3,2,((#441811,#441812,#441813),(#441814,#441815,#441816),
(#441817,#441818,#441819),(#441820,#441821,#441822)),.UNSPECIFIED.,.F.,
 .F.,.F.)
B_SPLINE_SURFACE_WITH_KNOTS((4,4),(3,3),(0.,0.000101260117256738),(0.,1.),
 .UNSPECIFIED.)
GEOMETRIC_REPRESENTATION_ITEM()
RATIONAL_B_SPLINE_SURFACE(((1.,0.796615278835171,1.),(1.,0.795896038055938,
1.),(1.,0.795193354661346,1.),(1.,0.79450619318555,1.)))
REPRESENTATION_ITEM('')
SURFACE()
);
#3854=(
BOUNDED_SURFACE()
B_SPLINE_SURFACE(3,2,((#441860,#441861,#441862),(#441863,#441864,#441865),
(#441866,#441867,#441868),(#441869,#441870,#441871),(#441872,#441873,#441874),
(#441875,#441876,#441877)),.UNSPECIFIED.,.F.,.F.,.F.)
B_SPLINE_SURFACE_WITH_KNOTS((4,2,4),(3,3),(1.55854062294791E-19,1.66936432462295E-5,
3.33872864924588E-5),(0.,1.),.UNSPECIFIED.)
GEOMETRIC_REPRESENTATION_ITEM()
RATIONAL_B_SPLINE_SURFACE(((1.,0.796615278835172,1.),(1.,0.862310524418129,
1.),(1.,0.92377447201052,1.),(1.,0.923983993203427,1.),(1.,0.862574873720937,
1.),(1.,0.796615278835187,1.)))
REPRESENTATION_ITEM('')
SURFACE()
);
#3855=(
BOUNDED_SURFACE()
B_SPLINE_SURFACE(3,2,((#441914,#441915,#441916),(#441917,#441918,#441919),
(#441920,#441921,#441922),(#441923,#441924,#441925)),.UNSPECIFIED.,.F.,
 .F.,.F.)
B_SPLINE_SURFACE_WITH_KNOTS((4,4),(3,3),(0.,0.000101244905251113),(0.,1.),
 .UNSPECIFIED.)
GEOMETRIC_REPRESENTATION_ITEM()
RATIONAL_B_SPLINE_SURFACE(((1.,0.796615278835168,1.),(1.,0.795896146109794,
1.),(1.,0.795193565796498,1.),(1.,0.794506502889898,1.)))
REPRESENTATION_ITEM('')
SURFACE()
);
#3856=(
BOUNDED_SURFACE()
B_SPLINE_SURFACE(3,2,((#441961,#441962,#441963),(#441964,#441965,#441966),
(#441967,#441968,#441969),(#441970,#441971,#441972)),.UNSPECIFIED.,.F.,
 .F.,.F.)
B_SPLINE_SURFACE_WITH_KNOTS((4,4),(3,3),(2.85968127239939E-5,9.24681548475813E-5),
(-0.00167900678669566,1.01130827127813),.UNSPECIFIED.)
GEOMETRIC_REPRESENTATION_ITEM()
RATIONAL_B_SPLINE_SURFACE(((1.00059040895222,0.822187541868261,1.00401468696653),
(1.00036527718143,0.88999009367157,1.00248382673389),(1.00016469515015,
0.950399042257926,1.0011199008251),(1.00025604273995,0.922888044286076,
1.0017410499063)))
REPRESENTATION_ITEM('')
SURFACE()
);
#3857=(
BOUNDED_SURFACE()
B_SPLINE_SURFACE(3,2,((#441976,#441977,#441978),(#441979,#441980,#441981),
(#441982,#441983,#441984),(#441985,#441986,#441987)),.UNSPECIFIED.,.F.,
 .F.,.F.)
B_SPLINE_SURFACE_WITH_KNOTS((4,4),(3,3),(-5.22358356749252E-6,5.74594192424278E-5),
(-0.00127120052064908,1.),.UNSPECIFIED.)
GEOMETRIC_REPRESENTATION_ITEM()
RATIONAL_B_SPLINE_SURFACE(((1.00054449313179,0.785835073638743,1.),(1.00047707767478,
0.812351526358841,1.),(1.0004403178859,0.82681021650626,1.),(1.00044777653322,
0.823876514387243,1.)))
REPRESENTATION_ITEM('')
SURFACE()
);
#3858=(
BOUNDED_SURFACE()
B_SPLINE_SURFACE(3,2,((#441989,#441990,#441991),(#441992,#441993,#441994),
(#441995,#441996,#441997),(#441998,#441999,#442000)),.UNSPECIFIED.,.F.,
 .F.,.F.)
B_SPLINE_SURFACE_WITH_KNOTS((4,4),(3,3),(5.42101086242752E-20,4.88747512969879E-5),
(-0.000215805215441692,1.),.UNSPECIFIED.)
GEOMETRIC_REPRESENTATION_ITEM()
RATIONAL_B_SPLINE_SURFACE(((1.00008915600336,0.793434085499753,1.),(1.00008930224989,
0.793095246303307,1.),(1.00008944684611,0.792760230720563,1.),(1.00008958984391,
0.792428918540602,1.)))
REPRESENTATION_ITEM('')
SURFACE()
);
#3859=(
BOUNDED_SURFACE()
B_SPLINE_SURFACE(3,2,((#442002,#442003,#442004),(#442005,#442006,#442007),
(#442008,#442009,#442010),(#442011,#442012,#442013),(#442014,#442015,#442016),
(#442017,#442018,#442019)),.UNSPECIFIED.,.F.,.F.,.F.)
B_SPLINE_SURFACE_WITH_KNOTS((4,2,4),(3,3),(3.25260651745651E-19,7.62675010863198E-5,
0.000152535002172639),(0.,1.02152348203058),.UNSPECIFIED.)
GEOMETRIC_REPRESENTATION_ITEM()
RATIONAL_B_SPLINE_SURFACE(((1.,0.789033595401269,1.00908146323687),(1.,
0.857071781054852,1.00615262590426),(1.,0.922087264710738,1.0033539067159),
(1.,0.922394466502381,1.00334068261142),(1.,0.85722438459907,1.00614605678497),
(1.,0.789033595401667,1.00908146323686)))
REPRESENTATION_ITEM('')
SURFACE()
);
#3860=(
BOUNDED_SURFACE()
B_SPLINE_SURFACE(3,2,((#442021,#442022,#442023),(#442024,#442025,#442026),
(#442027,#442028,#442029),(#442030,#442031,#442032)),.UNSPECIFIED.,.F.,
 .F.,.F.)
B_SPLINE_SURFACE_WITH_KNOTS((4,4),(3,3),(3.79470760369927E-19,4.88747512969882E-5),
(-0.000215489857128971,1.),.UNSPECIFIED.)
GEOMETRIC_REPRESENTATION_ITEM()
RATIONAL_B_SPLINE_SURFACE(((1.00008945889717,0.792428983985724,1.),(1.00008931610839,
0.792760296061274,1.),(1.00008917172351,0.793095311538338,1.),(1.00008902569074,
0.793434150627974,1.)))
REPRESENTATION_ITEM('')
SURFACE()
);
#3861=(
BOUNDED_SURFACE()
B_SPLINE_SURFACE(3,2,((#442034,#442035,#442036),(#442037,#442038,#442039),
(#442040,#442041,#442042),(#442043,#442044,#442045)),.UNSPECIFIED.,.F.,
 .F.,.F.)
B_SPLINE_SURFACE_WITH_KNOTS((4,4),(3,3),(-5.21974905013103E-6,5.74172395514409E-5),
(-0.00139822857735267,1.00051312364046),.UNSPECIFIED.)
GEOMETRIC_REPRESENTATION_ITEM()
RATIONAL_B_SPLINE_SURFACE(((1.00049256947243,0.82376895224408,1.00018060397842),
(1.00048448215714,0.826662424388374,1.00017763870875),(1.00052427784021,
0.812424361909455,1.00019223006913),(1.00059912365854,0.78564609463283,
1.00021967280222)))
REPRESENTATION_ITEM('')
SURFACE()
);
#3862=(
BOUNDED_SURFACE()
B_SPLINE_SURFACE(3,2,((#442049,#442050,#442051),(#442052,#442053,#442054),
(#442055,#442056,#442057),(#442058,#442059,#442060)),.UNSPECIFIED.,.F.,
 .F.,.F.)
B_SPLINE_SURFACE_WITH_KNOTS((4,4),(3,3),(3.22980774337778E-5,9.63764854872252E-5),
(-0.00154325936387336,1.01095292447545),.UNSPECIFIED.)
GEOMETRIC_REPRESENTATION_ITEM()
RATIONAL_B_SPLINE_SURFACE(((1.00023530983301,0.922925743796151,1.00168574728331),
(1.00015136166127,0.95042243959421,1.0010843469906),(1.00033574337401,0.890029368953935,
1.00240524789548),(1.00054260094226,0.822274473168311,1.00388716464859)))
REPRESENTATION_ITEM('')
SURFACE()
);
#3863=(
BOUNDED_SURFACE()
B_SPLINE_SURFACE(3,2,((#442160,#442161,#442162),(#442163,#442164,#442165),
(#442166,#442167,#442168),(#442169,#442170,#442171)),.UNSPECIFIED.,.F.,
 .F.,.F.)
B_SPLINE_SURFACE_WITH_KNOTS((4,4),(3,3),(0.,0.000101260117256738),(0.,1.),
 .UNSPECIFIED.)
GEOMETRIC_REPRESENTATION_ITEM()
RATIONAL_B_SPLINE_SURFACE(((1.,0.79661527883517,1.),(1.,0.795896038055938,
1.),(1.,0.795193354661352,1.),(1.,0.794506193185546,1.)))
REPRESENTATION_ITEM('')
SURFACE()
);
#3864=(
BOUNDED_SURFACE()
B_SPLINE_SURFACE(3,2,((#442209,#442210,#442211),(#442212,#442213,#442214),
(#442215,#442216,#442217),(#442218,#442219,#442220),(#442221,#442222,#442223),
(#442224,#442225,#442226)),.UNSPECIFIED.,.F.,.F.,.F.)
B_SPLINE_SURFACE_WITH_KNOTS((4,2,4),(3,3),(1.18584612615602E-19,1.66936432462296E-5,
3.33872864924591E-5),(0.,1.),.UNSPECIFIED.)
GEOMETRIC_REPRESENTATION_ITEM()
RATIONAL_B_SPLINE_SURFACE(((1.,0.796615278835173,1.),(1.,0.862310524418132,
1.),(1.,0.923774472010519,1.),(1.,0.923983993203429,1.),(1.,0.862574873720937,
1.),(1.,0.796615278835185,1.)))
REPRESENTATION_ITEM('')
SURFACE()
);
#3865=(
BOUNDED_SURFACE()
B_SPLINE_SURFACE(3,2,((#442263,#442264,#442265),(#442266,#442267,#442268),
(#442269,#442270,#442271),(#442272,#442273,#442274)),.UNSPECIFIED.,.F.,
 .F.,.F.)
B_SPLINE_SURFACE_WITH_KNOTS((4,4),(3,3),(0.,0.000101244905251112),(0.,1.),
 .UNSPECIFIED.)
GEOMETRIC_REPRESENTATION_ITEM()
RATIONAL_B_SPLINE_SURFACE(((1.,0.796615278835173,1.),(1.,0.795896146109791,
1.),(1.,0.795193565796504,1.),(1.,0.794506502889902,1.)))
REPRESENTATION_ITEM('')
SURFACE()
);
#3866=(
BOUNDED_SURFACE()
B_SPLINE_SURFACE(3,2,((#442310,#442311,#442312),(#442313,#442314,#442315),
(#442316,#442317,#442318),(#442319,#442320,#442321)),.UNSPECIFIED.,.F.,
 .F.,.F.)
B_SPLINE_SURFACE_WITH_KNOTS((4,4),(3,3),(2.85968127239939E-5,9.24681548475818E-5),
(-0.00167900678658251,1.01130827127826),.UNSPECIFIED.)
GEOMETRIC_REPRESENTATION_ITEM()
RATIONAL_B_SPLINE_SURFACE(((1.00059040895218,0.822187541868258,1.00401468696658),
(1.0003652771814,0.889990093671564,1.00248382673392),(1.00016469515013,
0.950399042257928,1.00111990082511),(1.00025604273993,0.922888044286075,
1.00174104990632)))
REPRESENTATION_ITEM('')
SURFACE()
);
#3867=(
BOUNDED_SURFACE()
B_SPLINE_SURFACE(3,2,((#442325,#442326,#442327),(#442328,#442329,#442330),
(#442331,#442332,#442333),(#442334,#442335,#442336)),.UNSPECIFIED.,.F.,
 .F.,.F.)
B_SPLINE_SURFACE_WITH_KNOTS((4,4),(3,3),(-5.22358356749274E-6,5.74594192424278E-5),
(-0.0012712005206484,1.),.UNSPECIFIED.)
GEOMETRIC_REPRESENTATION_ITEM()
RATIONAL_B_SPLINE_SURFACE(((1.00054449313179,0.78583507363874,1.),(1.00047707767478,
0.812351526358843,1.),(1.0004403178859,0.826810216506262,1.),(1.00044777653322,
0.823876514387242,0.999999999999999)))
REPRESENTATION_ITEM('')
SURFACE()
);
#3868=(
BOUNDED_SURFACE()
B_SPLINE_SURFACE(3,2,((#442338,#442339,#442340),(#442341,#442342,#442343),
(#442344,#442345,#442346),(#442347,#442348,#442349)),.UNSPECIFIED.,.F.,
 .F.,.F.)
B_SPLINE_SURFACE_WITH_KNOTS((4,4),(3,3),(-5.42101086242752E-20,4.88747512969881E-5),
(-0.000215805215096801,1.),.UNSPECIFIED.)
GEOMETRIC_REPRESENTATION_ITEM()
RATIONAL_B_SPLINE_SURFACE(((1.00008915600322,0.793434085499825,1.),(1.00008930224975,
0.793095246303367,1.),(1.00008944684597,0.792760230720641,1.),(1.00008958984376,
0.792428918540674,1.)))
REPRESENTATION_ITEM('')
SURFACE()
);
#3869=(
BOUNDED_SURFACE()
B_SPLINE_SURFACE(3,2,((#442351,#442352,#442353),(#442354,#442355,#442356),
(#442357,#442358,#442359),(#442360,#442361,#442362),(#442363,#442364,#442365),
(#442366,#442367,#442368)),.UNSPECIFIED.,.F.,.F.,.F.)
B_SPLINE_SURFACE_WITH_KNOTS((4,2,4),(3,3),(6.09863722023096E-20,7.62675010863195E-5,
0.000152535002172639),(0.,1.02152348203069),.UNSPECIFIED.)
GEOMETRIC_REPRESENTATION_ITEM()
RATIONAL_B_SPLINE_SURFACE(((1.,0.789033595401248,1.00908146323692),(1.,
0.857071781054843,1.00615262590429),(1.,0.92208726471072,1.00335390671592),
(1.,0.922394466502381,1.00334068261144),(1.,0.857224384599051,1.00614605678501),
(1.,0.789033595401646,1.0090814632369)))
REPRESENTATION_ITEM('')
SURFACE()
);
#3870=(
BOUNDED_SURFACE()
B_SPLINE_SURFACE(3,2,((#442370,#442371,#442372),(#442373,#442374,#442375),
(#442376,#442377,#442378),(#442379,#442380,#442381)),.UNSPECIFIED.,.F.,
 .F.,.F.)
B_SPLINE_SURFACE_WITH_KNOTS((4,4),(3,3),(8.13151629364128E-20,4.88747512969882E-5),
(-0.000215489857699746,1.),.UNSPECIFIED.)
GEOMETRIC_REPRESENTATION_ITEM()
RATIONAL_B_SPLINE_SURFACE(((1.00008945889741,0.792428983985608,1.),(1.00008931610862,
0.792760296061175,1.),(1.00008917172375,0.793095311538219,1.),(1.00008902569097,
0.793434150627864,1.)))
REPRESENTATION_ITEM('')
SURFACE()
);
#3871=(
BOUNDED_SURFACE()
B_SPLINE_SURFACE(3,2,((#442383,#442384,#442385),(#442386,#442387,#442388),
(#442389,#442390,#442391),(#442392,#442393,#442394)),.UNSPECIFIED.,.F.,
 .F.,.F.)
B_SPLINE_SURFACE_WITH_KNOTS((4,4),(3,3),(-5.21974905013091E-6,5.74172395514411E-5),
(-0.00139822857775922,1.00051312364068),.UNSPECIFIED.)
GEOMETRIC_REPRESENTATION_ITEM()
RATIONAL_B_SPLINE_SURFACE(((1.00049256947257,0.823768952243979,1.00018060397849),
(1.00048448215728,0.826662424388264,1.00017763870882),(1.00052427784036,
0.812424361909345,1.00019223006921),(1.00059912365872,0.785646094632693,
1.00021967280231)))
REPRESENTATION_ITEM('')
SURFACE()
);
#3872=(
BOUNDED_SURFACE()
B_SPLINE_SURFACE(3,2,((#442398,#442399,#442400),(#442401,#442402,#442403),
(#442404,#442405,#442406),(#442407,#442408,#442409)),.UNSPECIFIED.,.F.,
 .F.,.F.)
B_SPLINE_SURFACE_WITH_KNOTS((4,4),(3,3),(3.2298077433778E-5,9.63764854872256E-5),
(-0.00154325936351672,1.01095292447559),.UNSPECIFIED.)
GEOMETRIC_REPRESENTATION_ITEM()
RATIONAL_B_SPLINE_SURFACE(((1.00023530983296,0.922925743796168,1.00168574728333),
(1.00015136166123,0.950422439594232,1.00108434699061),(1.00033574337394,
0.890029368953954,1.00240524789551),(1.00054260094214,0.822274473168349,
1.00388716464864)))
REPRESENTATION_ITEM('')
SURFACE()
);
#3873=(
BOUNDED_SURFACE()
B_SPLINE_SURFACE(3,2,((#442509,#442510,#442511),(#442512,#442513,#442514),
(#442515,#442516,#442517),(#442518,#442519,#442520)),.UNSPECIFIED.,.F.,
 .F.,.F.)
B_SPLINE_SURFACE_WITH_KNOTS((4,4),(3,3),(0.,0.000101260117256738),(0.,1.),
 .UNSPECIFIED.)
GEOMETRIC_REPRESENTATION_ITEM()
RATIONAL_B_SPLINE_SURFACE(((1.,0.796615278835173,1.),(1.,0.79589603805594,
1.),(1.,0.795193354661347,1.),(1.,0.794506193185548,1.)))
REPRESENTATION_ITEM('')
SURFACE()
);
#3874=(
BOUNDED_SURFACE()
B_SPLINE_SURFACE(3,2,((#442558,#442559,#442560),(#442561,#442562,#442563),
(#442564,#442565,#442566),(#442567,#442568,#442569),(#442570,#442571,#442572),
(#442573,#442574,#442575)),.UNSPECIFIED.,.F.,.F.,.F.)
B_SPLINE_SURFACE_WITH_KNOTS((4,2,4),(3,3),(2.28698895758661E-19,1.66936432462294E-5,
3.33872864924585E-5),(0.,1.),.UNSPECIFIED.)
GEOMETRIC_REPRESENTATION_ITEM()
RATIONAL_B_SPLINE_SURFACE(((1.,0.796615278835184,1.),(1.,0.862310524418132,
1.),(1.,0.923774472010521,1.),(1.,0.923983993203422,1.),(1.,0.862574873720953,
1.),(1.,0.796615278835186,1.)))
REPRESENTATION_ITEM('')
SURFACE()
);
#3875=(
BOUNDED_SURFACE()
B_SPLINE_SURFACE(3,2,((#442612,#442613,#442614),(#442615,#442616,#442617),
(#442618,#442619,#442620),(#442621,#442622,#442623)),.UNSPECIFIED.,.F.,
 .F.,.F.)
B_SPLINE_SURFACE_WITH_KNOTS((4,4),(3,3),(-2.16840434497101E-19,0.000101244905251112),
(0.,1.),.UNSPECIFIED.)
GEOMETRIC_REPRESENTATION_ITEM()
RATIONAL_B_SPLINE_SURFACE(((1.,0.796615278835171,1.),(1.,0.795896146109791,
1.),(1.,0.795193565796496,1.),(1.,0.794506502889899,1.)))
REPRESENTATION_ITEM('')
SURFACE()
);
#3876=(
BOUNDED_SURFACE()
B_SPLINE_SURFACE(3,2,((#442659,#442660,#442661),(#442662,#442663,#442664),
(#442665,#442666,#442667),(#442668,#442669,#442670)),.UNSPECIFIED.,.F.,
 .F.,.F.)
B_SPLINE_SURFACE_WITH_KNOTS((4,4),(3,3),(2.85968127239939E-5,9.24681548475819E-5),
(-0.0016790067946991,1.01130827127835),.UNSPECIFIED.)
GEOMETRIC_REPRESENTATION_ITEM()
RATIONAL_B_SPLINE_SURFACE(((1.00059040895504,0.822187541866784,1.00401468696661),
(1.00036527718317,0.889990093670652,1.00248382673394),(1.00016469515093,
0.950399042257517,1.00111990082512),(1.00025604274117,0.922888044285435,
1.00174104990633)))
REPRESENTATION_ITEM('')
SURFACE()
);
#3877=(
BOUNDED_SURFACE()
B_SPLINE_SURFACE(3,2,((#442674,#442675,#442676),(#442677,#442678,#442679),
(#442680,#442681,#442682),(#442683,#442684,#442685)),.UNSPECIFIED.,.F.,
 .F.,.F.)
B_SPLINE_SURFACE_WITH_KNOTS((4,4),(3,3),(-5.22358356749143E-6,5.74594192424279E-5),
(-0.00127120052051176,1.),.UNSPECIFIED.)
GEOMETRIC_REPRESENTATION_ITEM()
RATIONAL_B_SPLINE_SURFACE(((1.00054449313173,0.78583507363877,1.),(1.00047707767473,
0.812351526358871,1.),(1.00044031788585,0.826810216506278,1.),(1.00044777653317,
0.823876514387267,0.999999999999999)))
REPRESENTATION_ITEM('')
SURFACE()
);
#3878=(
BOUNDED_SURFACE()
B_SPLINE_SURFACE(3,2,((#442687,#442688,#442689),(#442690,#442691,#442692),
(#442693,#442694,#442695),(#442696,#442697,#442698)),.UNSPECIFIED.,.F.,
 .F.,.F.)
B_SPLINE_SURFACE_WITH_KNOTS((4,4),(3,3),(2.71050543121376E-20,4.8874751296988E-5),
(-0.000215805215085956,1.),.UNSPECIFIED.)
GEOMETRIC_REPRESENTATION_ITEM()
RATIONAL_B_SPLINE_SURFACE(((1.00008915600322,0.793434085499825,1.),(1.00008930224975,
0.793095246303369,1.),(1.00008944684597,0.792760230720644,1.),(1.00008958984376,
0.792428918540674,1.)))
REPRESENTATION_ITEM('')
SURFACE()
);
#3879=(
BOUNDED_SURFACE()
B_SPLINE_SURFACE(3,2,((#442700,#442701,#442702),(#442703,#442704,#442705),
(#442706,#442707,#442708),(#442709,#442710,#442711),(#442712,#442713,#442714),
(#442715,#442716,#442717)),.UNSPECIFIED.,.F.,.F.,.F.)
B_SPLINE_SURFACE_WITH_KNOTS((4,2,4),(3,3),(2.03287907341032E-20,7.62675010863199E-5,
0.00015253500217264),(0.,1.02152348203066),.UNSPECIFIED.)
GEOMETRIC_REPRESENTATION_ITEM()
RATIONAL_B_SPLINE_SURFACE(((1.,0.789033595401254,1.00908146323691),(1.,
0.857071781054841,1.00615262590428),(1.,0.922087264710727,1.00335390671592),
(1.,0.922394466502377,1.00334068261143),(1.,0.857224384599056,1.006146056785),
(1.,0.789033595401652,1.00908146323689)))
REPRESENTATION_ITEM('')
SURFACE()
);
#3880=(
BOUNDED_SURFACE()
B_SPLINE_SURFACE(3,2,((#442719,#442720,#442721),(#442722,#442723,#442724),
(#442725,#442726,#442727),(#442728,#442729,#442730)),.UNSPECIFIED.,.F.,
 .F.,.F.)
B_SPLINE_SURFACE_WITH_KNOTS((4,4),(3,3),(4.33680868994202E-19,4.88747512969881E-5),
(-0.000215489856948962,1.),.UNSPECIFIED.)
GEOMETRIC_REPRESENTATION_ITEM()
RATIONAL_B_SPLINE_SURFACE(((1.00008945889709,0.792428983985764,1.),(1.00008931610831,
0.792760296061302,1.),(1.00008917172344,0.793095311538389,1.),(1.00008902569066,
0.793434150628012,1.)))
REPRESENTATION_ITEM('')
SURFACE()
);
#3881=(
BOUNDED_SURFACE()
B_SPLINE_SURFACE(3,2,((#442732,#442733,#442734),(#442735,#442736,#442737),
(#442738,#442739,#442740),(#442741,#442742,#442743)),.UNSPECIFIED.,.F.,
 .F.,.F.)
B_SPLINE_SURFACE_WITH_KNOTS((4,4),(3,3),(-5.21974905012881E-6,5.74172395514414E-5),
(-0.00139822857773428,1.0005131236407),.UNSPECIFIED.)
GEOMETRIC_REPRESENTATION_ITEM()
RATIONAL_B_SPLINE_SURFACE(((1.00049256947256,0.823768952243969,1.0001806039785),
(1.00048448215727,0.826662424388272,1.00017763870883),(1.00052427784035,
0.812424361909323,1.00019223006923),(1.0005991236587,0.785646094632698,
1.00021967280233)))
REPRESENTATION_ITEM('')
SURFACE()
);
#3882=(
BOUNDED_SURFACE()
B_SPLINE_SURFACE(3,2,((#442747,#442748,#442749),(#442750,#442751,#442752),
(#442753,#442754,#442755),(#442756,#442757,#442758)),.UNSPECIFIED.,.F.,
 .F.,.F.)
B_SPLINE_SURFACE_WITH_KNOTS((4,4),(3,3),(3.22980774337778E-5,9.63764854872253E-5),
(-0.00154325936372609,1.01095292447536),.UNSPECIFIED.)
GEOMETRIC_REPRESENTATION_ITEM()
RATIONAL_B_SPLINE_SURFACE(((1.00023530983299,0.922925743796169,1.0016857472833),
(1.00015136166125,0.950422439594221,1.00108434699059),(1.00033574337398,
0.890029368953967,1.00240524789546),(1.00054260094221,0.822274473168345,
1.00388716464856)))
REPRESENTATION_ITEM('')
SURFACE()
);
#3883=(
BOUNDED_SURFACE()
B_SPLINE_SURFACE(3,2,((#442858,#442859,#442860),(#442861,#442862,#442863),
(#442864,#442865,#442866),(#442867,#442868,#442869)),.UNSPECIFIED.,.F.,
 .F.,.F.)
B_SPLINE_SURFACE_WITH_KNOTS((4,4),(3,3),(0.,0.000101260117256738),(0.,1.),
 .UNSPECIFIED.)
GEOMETRIC_REPRESENTATION_ITEM()
RATIONAL_B_SPLINE_SURFACE(((1.,0.79661527883517,1.),(1.,0.795896038055939,
1.),(1.,0.79519335466135,1.),(1.,0.794506193185545,1.)))
REPRESENTATION_ITEM('')
SURFACE()
);
#3884=(
BOUNDED_SURFACE()
B_SPLINE_SURFACE(3,2,((#442907,#442908,#442909),(#442910,#442911,#442912),
(#442913,#442914,#442915),(#442916,#442917,#442918),(#442919,#442920,#442921),
(#442922,#442923,#442924)),.UNSPECIFIED.,.F.,.F.,.F.)
B_SPLINE_SURFACE_WITH_KNOTS((4,2,4),(3,3),(-1.06726151354042E-19,1.66936432462298E-5,
3.33872864924597E-5),(0.,1.),.UNSPECIFIED.)
GEOMETRIC_REPRESENTATION_ITEM()
RATIONAL_B_SPLINE_SURFACE(((1.,0.796615278835171,1.),(1.,0.862310524418125,
1.),(1.,0.923774472010519,1.),(1.,0.923983993203426,1.),(1.,0.862574873720946,
1.),(1.,0.796615278835184,1.)))
REPRESENTATION_ITEM('')
SURFACE()
);
#3885=(
BOUNDED_SURFACE()
B_SPLINE_SURFACE(3,2,((#442961,#442962,#442963),(#442964,#442965,#442966),
(#442967,#442968,#442969),(#442970,#442971,#442972)),.UNSPECIFIED.,.F.,
 .F.,.F.)
B_SPLINE_SURFACE_WITH_KNOTS((4,4),(3,3),(0.,0.000101244905251112),(0.,1.),
 .UNSPECIFIED.)
GEOMETRIC_REPRESENTATION_ITEM()
RATIONAL_B_SPLINE_SURFACE(((1.,0.79661527883517,1.),(1.,0.795896146109796,
1.),(1.,0.7951935657965,1.),(1.,0.794506502889897,1.)))
REPRESENTATION_ITEM('')
SURFACE()
);
#3886=(
BOUNDED_SURFACE()
B_SPLINE_SURFACE(3,2,((#443008,#443009,#443010),(#443011,#443012,#443013),
(#443014,#443015,#443016),(#443017,#443018,#443019)),.UNSPECIFIED.,.F.,
 .F.,.F.)
B_SPLINE_SURFACE_WITH_KNOTS((4,4),(3,3),(2.85968127239938E-5,9.24681548475817E-5),
(-0.00167900678627269,1.01130827127815),.UNSPECIFIED.)
GEOMETRIC_REPRESENTATION_ITEM()
RATIONAL_B_SPLINE_SURFACE(((1.00059040895207,0.822187541868334,1.00401468696654),
(1.00036527718134,0.889990093671605,1.00248382673389),(1.0001646951501,
0.950399042257946,1.0011199008251),(1.00025604273988,0.922888044286107,
1.0017410499063)))
REPRESENTATION_ITEM('')
SURFACE()
);
#3887=(
BOUNDED_SURFACE()
B_SPLINE_SURFACE(3,2,((#443023,#443024,#443025),(#443026,#443027,#443028),
(#443029,#443030,#443031),(#443032,#443033,#443034)),.UNSPECIFIED.,.F.,
 .F.,.F.)
B_SPLINE_SURFACE_WITH_KNOTS((4,4),(3,3),(-5.22358356749279E-6,5.74594192424277E-5),
(-0.00127120052061258,1.),.UNSPECIFIED.)
GEOMETRIC_REPRESENTATION_ITEM()
RATIONAL_B_SPLINE_SURFACE(((1.00054449313177,0.785835073638748,1.),(1.00047707767477,
0.812351526358847,1.),(1.00044031788588,0.826810216506265,1.),(1.00044777653321,
0.82387651438725,1.)))
REPRESENTATION_ITEM('')
SURFACE()
);
#3888=(
BOUNDED_SURFACE()
B_SPLINE_SURFACE(3,2,((#443036,#443037,#443038),(#443039,#443040,#443041),
(#443042,#443043,#443044),(#443045,#443046,#443047)),.UNSPECIFIED.,.F.,
 .F.,.F.)
B_SPLINE_SURFACE_WITH_KNOTS((4,4),(3,3),(-1.62630325872826E-19,4.88747512969879E-5),
(-0.000215805215084324,1.),.UNSPECIFIED.)
GEOMETRIC_REPRESENTATION_ITEM()
RATIONAL_B_SPLINE_SURFACE(((1.00008915600322,0.793434085499825,1.),(1.00008930224975,
0.793095246303363,1.),(1.00008944684597,0.792760230720643,1.),(1.00008958984376,
0.792428918540676,1.)))
REPRESENTATION_ITEM('')
SURFACE()
);
#3889=(
BOUNDED_SURFACE()
B_SPLINE_SURFACE(3,2,((#443049,#443050,#443051),(#443052,#443053,#443054),
(#443055,#443056,#443057),(#443058,#443059,#443060),(#443061,#443062,#443063),
(#443064,#443065,#443066)),.UNSPECIFIED.,.F.,.F.,.F.)
B_SPLINE_SURFACE_WITH_KNOTS((4,2,4),(3,3),(1.89735380184963E-19,7.62675010863201E-5,
0.00015253500217264),(0.,1.02152348203042),.UNSPECIFIED.)
GEOMETRIC_REPRESENTATION_ITEM()
RATIONAL_B_SPLINE_SURFACE(((1.,0.789033595401301,1.0090814632368),(1.,0.857071781054865,
1.00615262590421),(1.,0.922087264710765,1.00335390671588),(1.,0.922394466502376,
1.00334068261139),(1.,0.857224384599105,1.00614605678493),(1.,0.7890335954017,
1.00908146323679)))
REPRESENTATION_ITEM('')
SURFACE()
);
#3890=(
BOUNDED_SURFACE()
B_SPLINE_SURFACE(3,2,((#443068,#443069,#443070),(#443071,#443072,#443073),
(#443074,#443075,#443076),(#443077,#443078,#443079)),.UNSPECIFIED.,.F.,
 .F.,.F.)
B_SPLINE_SURFACE_WITH_KNOTS((4,4),(3,3),(1.62630325872826E-19,4.88747512969885E-5),
(-0.000215489856958563,1.),.UNSPECIFIED.)
GEOMETRIC_REPRESENTATION_ITEM()
RATIONAL_B_SPLINE_SURFACE(((1.0000894588971,0.792428983985762,1.),(1.00008931610832,
0.792760296061314,1.),(1.00008917172344,0.793095311538372,1.),(1.00008902569067,
0.793434150628011,1.)))
REPRESENTATION_ITEM('')
SURFACE()
);
#3891=(
BOUNDED_SURFACE()
B_SPLINE_SURFACE(3,2,((#443081,#443082,#443083),(#443084,#443085,#443086),
(#443087,#443088,#443089),(#443090,#443091,#443092)),.UNSPECIFIED.,.F.,
 .F.,.F.)
B_SPLINE_SURFACE_WITH_KNOTS((4,4),(3,3),(-5.21974905013081E-6,5.74172395514397E-5),
(-0.00139822857806521,1.00051312364087),.UNSPECIFIED.)
GEOMETRIC_REPRESENTATION_ITEM()
RATIONAL_B_SPLINE_SURFACE(((1.00049256947268,0.823768952243879,1.00018060397856),
(1.00048448215738,0.826662424388185,1.00017763870889),(1.00052427784047,
0.81242436190924,1.00019223006929),(1.00059912365885,0.785646094632593,
1.0002196728024)))
REPRESENTATION_ITEM('')
SURFACE()
);
#3892=(
BOUNDED_SURFACE()
B_SPLINE_SURFACE(3,2,((#443096,#443097,#443098),(#443099,#443100,#443101),
(#443102,#443103,#443104),(#443105,#443106,#443107)),.UNSPECIFIED.,.F.,
 .F.,.F.)
B_SPLINE_SURFACE_WITH_KNOTS((4,4),(3,3),(3.22980774337778E-5,9.63764854872243E-5),
(-0.0015432593634407,1.0109529244754),.UNSPECIFIED.)
GEOMETRIC_REPRESENTATION_ITEM()
RATIONAL_B_SPLINE_SURFACE(((1.00023530983294,0.922925743796191,1.0016857472833),
(1.00015136166123,0.950422439594233,1.00108434699059),(1.00033574337392,
0.89002936895399,1.00240524789547),(1.00054260094211,0.822274473168393,
1.00388716464857)))
REPRESENTATION_ITEM('')
SURFACE()
);
#3893=(
BOUNDED_SURFACE()
B_SPLINE_SURFACE(3,2,((#443207,#443208,#443209),(#443210,#443211,#443212),
(#443213,#443214,#443215),(#443216,#443217,#443218)),.UNSPECIFIED.,.F.,
 .F.,.F.)
B_SPLINE_SURFACE_WITH_KNOTS((4,4),(3,3),(-2.16840434497101E-19,0.000101260117256737),
(0.,1.),.UNSPECIFIED.)
GEOMETRIC_REPRESENTATION_ITEM()
RATIONAL_B_SPLINE_SURFACE(((1.,0.796615278835171,1.),(1.,0.795896038055952,
1.),(1.,0.795193354661332,1.),(1.,0.794506193185545,1.)))
REPRESENTATION_ITEM('')
SURFACE()
);
#3894=(
BOUNDED_SURFACE()
B_SPLINE_SURFACE(3,2,((#443256,#443257,#443258),(#443259,#443260,#443261),
(#443262,#443263,#443264),(#443265,#443266,#443267),(#443268,#443269,#443270),
(#443271,#443272,#443273)),.UNSPECIFIED.,.F.,.F.,.F.)
B_SPLINE_SURFACE_WITH_KNOTS((4,2,4),(3,3),(-2.03287907341032E-20,1.66936432462293E-5,
3.33872864924587E-5),(0.,1.),.UNSPECIFIED.)
GEOMETRIC_REPRESENTATION_ITEM()
RATIONAL_B_SPLINE_SURFACE(((1.,0.796615278835177,1.),(1.,0.862310524418135,
1.),(1.,0.92377447201052,1.),(1.,0.923983993203427,1.),(1.,0.862574873720944,
1.),(1.,0.796615278835187,1.)))
REPRESENTATION_ITEM('')
SURFACE()
);
#3895=(
BOUNDED_SURFACE()
B_SPLINE_SURFACE(3,2,((#443310,#443311,#443312),(#443313,#443314,#443315),
(#443316,#443317,#443318),(#443319,#443320,#443321)),.UNSPECIFIED.,.F.,
 .F.,.F.)
B_SPLINE_SURFACE_WITH_KNOTS((4,4),(3,3),(0.,0.000101244905251112),(0.,1.),
 .UNSPECIFIED.)
GEOMETRIC_REPRESENTATION_ITEM()
RATIONAL_B_SPLINE_SURFACE(((1.,0.79661527883517,1.),(1.,0.795896146109793,
1.),(1.,0.795193565796498,1.),(1.,0.794506502889899,1.)))
REPRESENTATION_ITEM('')
SURFACE()
);
#3896=(
BOUNDED_SURFACE()
B_SPLINE_SURFACE(3,2,((#443357,#443358,#443359),(#443360,#443361,#443362),
(#443363,#443364,#443365),(#443366,#443367,#443368)),.UNSPECIFIED.,.F.,
 .F.,.F.)
B_SPLINE_SURFACE_WITH_KNOTS((4,4),(3,3),(2.85968127239939E-5,9.24681548475817E-5),
(-0.00167900678708718,1.01130827127833),.UNSPECIFIED.)
GEOMETRIC_REPRESENTATION_ITEM()
RATIONAL_B_SPLINE_SURFACE(((1.00059040895236,0.82218754186816,1.00401468696661),
(1.00036527718151,0.889990093671499,1.00248382673393),(1.00016469515018,
0.950399042257896,1.00111990082512),(1.00025604274001,0.922888044286031,
1.00174104990633)))
REPRESENTATION_ITEM('')
SURFACE()
);
#3897=(
BOUNDED_SURFACE()
B_SPLINE_SURFACE(3,2,((#443372,#443373,#443374),(#443375,#443376,#443377),
(#443378,#443379,#443380),(#443381,#443382,#443383)),.UNSPECIFIED.,.F.,
 .F.,.F.)
B_SPLINE_SURFACE_WITH_KNOTS((4,4),(3,3),(-5.22358356749297E-6,5.74594192424277E-5),
(-0.00127120052032446,1.),.UNSPECIFIED.)
GEOMETRIC_REPRESENTATION_ITEM()
RATIONAL_B_SPLINE_SURFACE(((1.00054449313165,0.785835073638822,1.),(1.00047707767466,
0.812351526358885,1.),(1.00044031788578,0.826810216506333,1.),(1.0004477765331,
0.823876514387295,1.)))
REPRESENTATION_ITEM('')
SURFACE()
);
#3898=(
BOUNDED_SURFACE()
B_SPLINE_SURFACE(3,2,((#443385,#443386,#443387),(#443388,#443389,#443390),
(#443391,#443392,#443393),(#443394,#443395,#443396)),.UNSPECIFIED.,.F.,
 .F.,.F.)
B_SPLINE_SURFACE_WITH_KNOTS((4,4),(3,3),(-1.35525271560688E-19,4.8874751296988E-5),
(-0.000215805215246867,1.),.UNSPECIFIED.)
GEOMETRIC_REPRESENTATION_ITEM()
RATIONAL_B_SPLINE_SURFACE(((1.00008915600328,0.793434085499793,1.),(1.00008930224981,
0.79309524630333,1.),(1.00008944684603,0.792760230720615,1.),(1.00008958984383,
0.792428918540643,1.)))
REPRESENTATION_ITEM('')
SURFACE()
);
#3899=(
BOUNDED_SURFACE()
B_SPLINE_SURFACE(3,2,((#443398,#443399,#443400),(#443401,#443402,#443403),
(#443404,#443405,#443406),(#443407,#443408,#443409),(#443410,#443411,#443412),
(#443413,#443414,#443415)),.UNSPECIFIED.,.F.,.F.,.F.)
B_SPLINE_SURFACE_WITH_KNOTS((4,2,4),(3,3),(2.57498015965307E-19,7.62675010863198E-5,
0.000152535002172639),(0.,1.02152348203072),.UNSPECIFIED.)
GEOMETRIC_REPRESENTATION_ITEM()
RATIONAL_B_SPLINE_SURFACE(((1.,0.78903359540124,1.00908146323694),(1.,0.857071781054825,
1.0061526259043),(1.,0.922087264710737,1.00335390671593),(1.,0.922394466502358,
1.00334068261144),(1.,0.857224384599055,1.00614605678502),(1.,0.789033595401639,
1.00908146323692)))
REPRESENTATION_ITEM('')
SURFACE()
);
#3900=(
BOUNDED_SURFACE()
B_SPLINE_SURFACE(3,2,((#443417,#443418,#443419),(#443420,#443421,#443422),
(#443423,#443424,#443425),(#443426,#443427,#443428)),.UNSPECIFIED.,.F.,
 .F.,.F.)
B_SPLINE_SURFACE_WITH_KNOTS((4,4),(3,3),(2.43945488809238E-19,4.88747512969884E-5),
(-0.000215489857031757,1.),.UNSPECIFIED.)
GEOMETRIC_REPRESENTATION_ITEM()
RATIONAL_B_SPLINE_SURFACE(((1.00008945889713,0.792428983985742,1.),(1.00008931610835,
0.792760296061288,1.),(1.00008917172347,0.793095311538377,1.),(1.0000890256907,
0.793434150627996,1.)))
REPRESENTATION_ITEM('')
SURFACE()
);
#3901=(
BOUNDED_SURFACE()
B_SPLINE_SURFACE(3,2,((#443430,#443431,#443432),(#443433,#443434,#443435),
(#443436,#443437,#443438),(#443439,#443440,#443441)),.UNSPECIFIED.,.F.,
 .F.,.F.)
B_SPLINE_SURFACE_WITH_KNOTS((4,4),(3,3),(-5.21974905013094E-6,5.74172395514396E-5),
(-0.00139822857774065,1.00051312364089),.UNSPECIFIED.)
GEOMETRIC_REPRESENTATION_ITEM()
RATIONAL_B_SPLINE_SURFACE(((1.00049256947257,0.823768952243939,1.00018060397857),
(1.00048448215727,0.826662424388233,1.0001776387089),(1.00052427784035,
0.812424361909294,1.00019223006929),(1.00059912365871,0.785646094632658,
1.0002196728024)))
REPRESENTATION_ITEM('')
SURFACE()
);
#3902=(
BOUNDED_SURFACE()
B_SPLINE_SURFACE(3,2,((#443445,#443446,#443447),(#443448,#443449,#443450),
(#443451,#443452,#443453),(#443454,#443455,#443456)),.UNSPECIFIED.,.F.,
 .F.,.F.)
B_SPLINE_SURFACE_WITH_KNOTS((4,4),(3,3),(3.22980774337778E-5,9.63764854872255E-5),
(-0.0015432593638328,1.01095292447545),.UNSPECIFIED.)
GEOMETRIC_REPRESENTATION_ITEM()
RATIONAL_B_SPLINE_SURFACE(((1.000235309833,0.922925743796155,1.00168574728331),
(1.00015136166127,0.950422439594211,1.0010843469906),(1.000335743374,0.890029368953947,
1.00240524789548),(1.00054260094225,0.822274473168314,1.00388716464859)))
REPRESENTATION_ITEM('')
SURFACE()
);
#3903=(
BOUNDED_SURFACE()
B_SPLINE_SURFACE(3,2,((#443556,#443557,#443558),(#443559,#443560,#443561),
(#443562,#443563,#443564),(#443565,#443566,#443567)),.UNSPECIFIED.,.F.,
 .F.,.F.)
B_SPLINE_SURFACE_WITH_KNOTS((4,4),(3,3),(-2.16840434497101E-19,0.000101260117256738),
(0.,1.),.UNSPECIFIED.)
GEOMETRIC_REPRESENTATION_ITEM()
RATIONAL_B_SPLINE_SURFACE(((1.,0.796615278835171,1.),(1.,0.795896038055942,
1.),(1.,0.795193354661349,1.),(1.,0.794506193185546,1.)))
REPRESENTATION_ITEM('')
SURFACE()
);
#3904=(
BOUNDED_SURFACE()
B_SPLINE_SURFACE(3,2,((#443605,#443606,#443607),(#443608,#443609,#443610),
(#443611,#443612,#443613),(#443614,#443615,#443616),(#443617,#443618,#443619),
(#443620,#443621,#443622)),.UNSPECIFIED.,.F.,.F.,.F.)
B_SPLINE_SURFACE_WITH_KNOTS((4,2,4),(3,3),(1.25360876193636E-19,1.66936432462297E-5,
3.33872864924592E-5),(0.,1.),.UNSPECIFIED.)
GEOMETRIC_REPRESENTATION_ITEM()
RATIONAL_B_SPLINE_SURFACE(((1.,0.796615278835178,1.),(1.,0.862310524418135,
1.),(1.,0.923774472010519,1.),(1.,0.923983993203426,1.),(1.,0.862574873720954,
1.),(1.,0.796615278835182,1.)))
REPRESENTATION_ITEM('')
SURFACE()
);
#3905=(
BOUNDED_SURFACE()
B_SPLINE_SURFACE(3,2,((#443659,#443660,#443661),(#443662,#443663,#443664),
(#443665,#443666,#443667),(#443668,#443669,#443670)),.UNSPECIFIED.,.F.,
 .F.,.F.)
B_SPLINE_SURFACE_WITH_KNOTS((4,4),(3,3),(-2.16840434497101E-19,0.000101244905251112),
(0.,1.),.UNSPECIFIED.)
GEOMETRIC_REPRESENTATION_ITEM()
RATIONAL_B_SPLINE_SURFACE(((1.,0.79661527883517,1.),(1.,0.795896146109798,
1.),(1.,0.795193565796495,1.),(1.,0.794506502889903,1.)))
REPRESENTATION_ITEM('')
SURFACE()
);
#3906=(
BOUNDED_SURFACE()
B_SPLINE_SURFACE(3,2,((#443706,#443707,#443708),(#443709,#443710,#443711),
(#443712,#443713,#443714),(#443715,#443716,#443717)),.UNSPECIFIED.,.F.,
 .F.,.F.)
B_SPLINE_SURFACE_WITH_KNOTS((4,4),(3,3),(2.85968127239938E-5,9.24681548475816E-5),
(-0.0016790067878167,1.01130827127815),.UNSPECIFIED.)
GEOMETRIC_REPRESENTATION_ITEM()
RATIONAL_B_SPLINE_SURFACE(((1.00059040895262,0.82218754186806,1.00401468696654),
(1.00036527718167,0.889990093671433,1.00248382673389),(1.00016469515026,
0.950399042257871,1.0011199008251),(1.00025604274012,0.922888044285985,
1.0017410499063)))
REPRESENTATION_ITEM('')
SURFACE()
);
#3907=(
BOUNDED_SURFACE()
B_SPLINE_SURFACE(3,2,((#443721,#443722,#443723),(#443724,#443725,#443726),
(#443727,#443728,#443729),(#443730,#443731,#443732)),.UNSPECIFIED.,.F.,
 .F.,.F.)
B_SPLINE_SURFACE_WITH_KNOTS((4,4),(3,3),(-5.22358356749278E-6,5.74594192424278E-5),
(-0.0012712005204861,1.),.UNSPECIFIED.)
GEOMETRIC_REPRESENTATION_ITEM()
RATIONAL_B_SPLINE_SURFACE(((1.00054449313172,0.785835073638772,1.),(1.00047707767472,
0.812351526358881,1.),(1.00044031788584,0.826810216506285,1.),(1.00044777653316,
0.823876514387271,1.)))
REPRESENTATION_ITEM('')
SURFACE()
);
#3908=(
BOUNDED_SURFACE()
B_SPLINE_SURFACE(3,2,((#443734,#443735,#443736),(#443737,#443738,#443739),
(#443740,#443741,#443742),(#443743,#443744,#443745)),.UNSPECIFIED.,.F.,
 .F.,.F.)
B_SPLINE_SURFACE_WITH_KNOTS((4,4),(3,3),(-3.25260651745651E-19,4.8874751296988E-5),
(-0.000215805215234466,1.),.UNSPECIFIED.)
GEOMETRIC_REPRESENTATION_ITEM()
RATIONAL_B_SPLINE_SURFACE(((1.00008915600328,0.793434085499797,1.),(1.00008930224981,
0.793095246303335,1.),(1.00008944684603,0.792760230720615,1.),(1.00008958984382,
0.792428918540643,1.)))
REPRESENTATION_ITEM('')
SURFACE()
);
#3909=(
BOUNDED_SURFACE()
B_SPLINE_SURFACE(3,2,((#443747,#443748,#443749),(#443750,#443751,#443752),
(#443753,#443754,#443755),(#443756,#443757,#443758),(#443759,#443760,#443761),
(#443762,#443763,#443764)),.UNSPECIFIED.,.F.,.F.,.F.)
B_SPLINE_SURFACE_WITH_KNOTS((4,2,4),(3,3),(1.62630325872826E-19,7.626750108632E-5,
0.00015253500217264),(0.,1.02152348203049),.UNSPECIFIED.)
GEOMETRIC_REPRESENTATION_ITEM()
RATIONAL_B_SPLINE_SURFACE(((1.,0.789033595401288,1.00908146323684),(1.,
0.857071781054874,1.00615262590423),(1.,0.922087264710735,1.00335390671589),
(1.,0.922394466502399,1.0033406826114),(1.,0.857224384599066,1.00614605678495),
(1.,0.78903359540169,1.00908146323682)))
REPRESENTATION_ITEM('')
SURFACE()
);
#3910=(
BOUNDED_SURFACE()
B_SPLINE_SURFACE(3,2,((#443766,#443767,#443768),(#443769,#443770,#443771),
(#443772,#443773,#443774),(#443775,#443776,#443777)),.UNSPECIFIED.,.F.,
 .F.,.F.)
B_SPLINE_SURFACE_WITH_KNOTS((4,4),(3,3),(1.89735380184963E-19,4.88747512969881E-5),
(-0.000215489857082434,1.),.UNSPECIFIED.)
GEOMETRIC_REPRESENTATION_ITEM()
RATIONAL_B_SPLINE_SURFACE(((1.00008945889715,0.792428983985737,1.),(1.00008931610837,
0.792760296061274,1.),(1.00008917172349,0.793095311538363,1.),(1.00008902569072,
0.793434150627986,1.)))
REPRESENTATION_ITEM('')
SURFACE()
);
#3911=(
BOUNDED_SURFACE()
B_SPLINE_SURFACE(3,2,((#443779,#443780,#443781),(#443782,#443783,#443784),
(#443785,#443786,#443787),(#443788,#443789,#443790)),.UNSPECIFIED.,.F.,
 .F.,.F.)
B_SPLINE_SURFACE_WITH_KNOTS((4,4),(3,3),(-5.219749050131E-6,5.74172395514409E-5),
(-0.00139822857753858,1.00051312364028),.UNSPECIFIED.)
GEOMETRIC_REPRESENTATION_ITEM()
RATIONAL_B_SPLINE_SURFACE(((1.0004925694725,0.823768952244087,1.00018060397836),
(1.0004844821572,0.826662424388369,1.00017763870869),(1.00052427784028,
0.81242436190945,1.00019223006907),(1.00059912365862,0.785646094632834,
1.00021967280214)))
REPRESENTATION_ITEM('')
SURFACE()
);
#3912=(
BOUNDED_SURFACE()
B_SPLINE_SURFACE(3,2,((#443794,#443795,#443796),(#443797,#443798,#443799),
(#443800,#443801,#443802),(#443803,#443804,#443805)),.UNSPECIFIED.,.F.,
 .F.,.F.)
B_SPLINE_SURFACE_WITH_KNOTS((4,4),(3,3),(3.22980774337778E-5,9.63764854872256E-5),
(-0.00154325936393493,1.01095292447551),.UNSPECIFIED.)
GEOMETRIC_REPRESENTATION_ITEM()
RATIONAL_B_SPLINE_SURFACE(((1.00023530983302,0.92292574379614,1.00168574728332),
(1.00015136166128,0.950422439594204,1.00108434699061),(1.00033574337403,
0.890029368953927,1.00240524789549),(1.00054260094228,0.822274473168288,
1.00388716464861)))
REPRESENTATION_ITEM('')
SURFACE()
);
#3913=(
BOUNDED_SURFACE()
B_SPLINE_SURFACE(3,2,((#443905,#443906,#443907),(#443908,#443909,#443910),
(#443911,#443912,#443913),(#443914,#443915,#443916)),.UNSPECIFIED.,.F.,
 .F.,.F.)
B_SPLINE_SURFACE_WITH_KNOTS((4,4),(3,3),(-2.16840434497101E-19,0.000101260117256738),
(0.,1.),.UNSPECIFIED.)
GEOMETRIC_REPRESENTATION_ITEM()
RATIONAL_B_SPLINE_SURFACE(((1.,0.796615278835172,1.),(1.,0.795896038055946,
1.),(1.,0.795193354661346,1.),(1.,0.794506193185549,1.)))
REPRESENTATION_ITEM('')
SURFACE()
);
#3914=(
BOUNDED_SURFACE()
B_SPLINE_SURFACE(3,2,((#443954,#443955,#443956),(#443957,#443958,#443959),
(#443960,#443961,#443962),(#443963,#443964,#443965),(#443966,#443967,#443968),
(#443969,#443970,#443971)),.UNSPECIFIED.,.F.,.F.,.F.)
B_SPLINE_SURFACE_WITH_KNOTS((4,2,4),(3,3),(-1.67712523556351E-19,1.66936432462289E-5,
3.3387286492458E-5),(0.,1.),.UNSPECIFIED.)
GEOMETRIC_REPRESENTATION_ITEM()
RATIONAL_B_SPLINE_SURFACE(((1.,0.796615278835171,1.),(1.,0.862310524418131,
1.),(1.,0.923774472010519,1.),(1.,0.923983993203428,1.),(1.,0.862574873720941,
1.),(1.,0.796615278835185,1.)))
REPRESENTATION_ITEM('')
SURFACE()
);
#3915=(
BOUNDED_SURFACE()
B_SPLINE_SURFACE(3,2,((#444008,#444009,#444010),(#444011,#444012,#444013),
(#444014,#444015,#444016),(#444017,#444018,#444019)),.UNSPECIFIED.,.F.,
 .F.,.F.)
B_SPLINE_SURFACE_WITH_KNOTS((4,4),(3,3),(0.,0.000101244905251112),(0.,1.),
 .UNSPECIFIED.)
GEOMETRIC_REPRESENTATION_ITEM()
RATIONAL_B_SPLINE_SURFACE(((1.,0.796615278835171,1.),(1.,0.7958961461098,
1.),(1.,0.795193565796498,1.),(1.,0.794506502889905,1.)))
REPRESENTATION_ITEM('')
SURFACE()
);
#3916=(
BOUNDED_SURFACE()
B_SPLINE_SURFACE(3,2,((#444055,#444056,#444057),(#444058,#444059,#444060),
(#444061,#444062,#444063),(#444064,#444065,#444066)),.UNSPECIFIED.,.F.,
 .F.,.F.)
B_SPLINE_SURFACE_WITH_KNOTS((4,4),(3,3),(2.85968127239939E-5,9.24681548475817E-5),
(-0.00167900678787809,1.01130827127808),.UNSPECIFIED.)
GEOMETRIC_REPRESENTATION_ITEM()
RATIONAL_B_SPLINE_SURFACE(((1.00059040895264,0.822187541868059,1.00401468696652),
(1.00036527718169,0.88999009367143,1.00248382673388),(1.00016469515026,
0.950399042257877,1.00111990082509),(1.00025604274013,0.922888044285986,
1.00174104990629)))
REPRESENTATION_ITEM('')
SURFACE()
);
#3917=(
BOUNDED_SURFACE()
B_SPLINE_SURFACE(3,2,((#444070,#444071,#444072),(#444073,#444074,#444075),
(#444076,#444077,#444078),(#444079,#444080,#444081)),.UNSPECIFIED.,.F.,
 .F.,.F.)
B_SPLINE_SURFACE_WITH_KNOTS((4,4),(3,3),(-5.22358356749313E-6,5.74594192424276E-5),
(-0.00127120052068568,1.),.UNSPECIFIED.)
GEOMETRIC_REPRESENTATION_ITEM()
RATIONAL_B_SPLINE_SURFACE(((1.00054449313181,0.785835073638733,1.),(1.0004770776748,
0.812351526358834,1.),(1.00044031788591,0.826810216506262,1.),(1.00044777653323,
0.823876514387234,1.)))
REPRESENTATION_ITEM('')
SURFACE()
);
#3918=(
BOUNDED_SURFACE()
B_SPLINE_SURFACE(3,2,((#444083,#444084,#444085),(#444086,#444087,#444088),
(#444089,#444090,#444091),(#444092,#444093,#444094)),.UNSPECIFIED.,.F.,
 .F.,.F.)
B_SPLINE_SURFACE_WITH_KNOTS((4,4),(3,3),(-4.60785923306339E-19,4.8874751296988E-5),
(-0.000215805216141731,1.),.UNSPECIFIED.)
GEOMETRIC_REPRESENTATION_ITEM()
RATIONAL_B_SPLINE_SURFACE(((1.00008915600365,0.793434085499609,1.),(1.00008930225018,
0.793095246303164,1.),(1.00008944684641,0.792760230720417,1.),(1.0000895898442,
0.792428918540459,1.)))
REPRESENTATION_ITEM('')
SURFACE()
);
#3919=(
BOUNDED_SURFACE()
B_SPLINE_SURFACE(3,2,((#444096,#444097,#444098),(#444099,#444100,#444101),
(#444102,#444103,#444104),(#444105,#444106,#444107),(#444108,#444109,#444110),
(#444111,#444112,#444113)),.UNSPECIFIED.,.F.,.F.,.F.)
B_SPLINE_SURFACE_WITH_KNOTS((4,2,4),(3,3),(1.35525271560688E-19,7.62675010863194E-5,
0.000152535002172639),(0.,1.02152348203065),.UNSPECIFIED.)
GEOMETRIC_REPRESENTATION_ITEM()
RATIONAL_B_SPLINE_SURFACE(((1.,0.789033595401256,1.00908146323691),(1.,
0.857071781054846,1.00615262590428),(1.,0.922087264710725,1.00335390671592),
(1.,0.922394466502383,1.00334068261143),(1.,0.857224384599043,1.006146056785),
(1.,0.789033595401655,1.00908146323689)))
REPRESENTATION_ITEM('')
SURFACE()
);
#3920=(
BOUNDED_SURFACE()
B_SPLINE_SURFACE(3,2,((#444115,#444116,#444117),(#444118,#444119,#444120),
(#444121,#444122,#444123),(#444124,#444125,#444126)),.UNSPECIFIED.,.F.,
 .F.,.F.)
B_SPLINE_SURFACE_WITH_KNOTS((4,4),(3,3),(3.52365706057789E-19,4.88747512969884E-5),
(-0.000215489857101505,1.),.UNSPECIFIED.)
GEOMETRIC_REPRESENTATION_ITEM()
RATIONAL_B_SPLINE_SURFACE(((1.00008945889716,0.792428983985735,1.),(1.00008931610838,
0.792760296061276,1.),(1.0000891717235,0.793095311538357,1.),(1.00008902569073,
0.793434150627985,1.)))
REPRESENTATION_ITEM('')
SURFACE()
);
#3921=(
BOUNDED_SURFACE()
B_SPLINE_SURFACE(3,2,((#444128,#444129,#444130),(#444131,#444132,#444133),
(#444134,#444135,#444136),(#444137,#444138,#444139)),.UNSPECIFIED.,.F.,
 .F.,.F.)
B_SPLINE_SURFACE_WITH_KNOTS((4,4),(3,3),(-5.21974905013088E-6,5.74172395514369E-5),
(-0.00139822857783258,1.0005131236407),.UNSPECIFIED.)
GEOMETRIC_REPRESENTATION_ITEM()
RATIONAL_B_SPLINE_SURFACE(((1.0004925694726,0.823768952243959,1.00018060397851),
(1.0004844821573,0.826662424388252,1.00017763870883),(1.00052427784039,
0.812424361909319,1.00019223006923),(1.00059912365875,0.785646094632685,
1.00021967280233)))
REPRESENTATION_ITEM('')
SURFACE()
);
#3922=(
BOUNDED_SURFACE()
B_SPLINE_SURFACE(3,2,((#444143,#444144,#444145),(#444146,#444147,#444148),
(#444149,#444150,#444151),(#444152,#444153,#444154)),.UNSPECIFIED.,.F.,
 .F.,.F.)
B_SPLINE_SURFACE_WITH_KNOTS((4,4),(3,3),(3.22980774337779E-5,9.63764854872245E-5),
(-0.00154325936379329,1.01095292447549),.UNSPECIFIED.)
GEOMETRIC_REPRESENTATION_ITEM()
RATIONAL_B_SPLINE_SURFACE(((1.000235309833,0.922925743796154,1.00168574728332),
(1.00015136166126,0.950422439594211,1.0010843469906),(1.000335743374,0.890029368953942,
1.00240524789549),(1.00054260094223,0.822274473168313,1.0038871646486)))
REPRESENTATION_ITEM('')
SURFACE()
);
#3923=(
BOUNDED_SURFACE()
B_SPLINE_SURFACE(3,2,((#444254,#444255,#444256),(#444257,#444258,#444259),
(#444260,#444261,#444262),(#444263,#444264,#444265)),.UNSPECIFIED.,.F.,
 .F.,.F.)
B_SPLINE_SURFACE_WITH_KNOTS((4,4),(3,3),(0.,0.000101260117256738),(0.,1.),
 .UNSPECIFIED.)
GEOMETRIC_REPRESENTATION_ITEM()
RATIONAL_B_SPLINE_SURFACE(((1.,0.796615278835172,1.),(1.,0.795896038055945,
1.),(1.,0.795193354661348,1.),(1.,0.794506193185548,1.)))
REPRESENTATION_ITEM('')
SURFACE()
);
#3924=(
BOUNDED_SURFACE()
B_SPLINE_SURFACE(3,2,((#444303,#444304,#444305),(#444306,#444307,#444308),
(#444309,#444310,#444311),(#444312,#444313,#444314),(#444315,#444316,#444317),
(#444318,#444319,#444320)),.UNSPECIFIED.,.F.,.F.,.F.)
B_SPLINE_SURFACE_WITH_KNOTS((4,2,4),(3,3),(-2.37169225231204E-20,1.66936432462295E-5,
3.33872864924591E-5),(0.,1.),.UNSPECIFIED.)
GEOMETRIC_REPRESENTATION_ITEM()
RATIONAL_B_SPLINE_SURFACE(((1.,0.796615278835175,1.),(1.,0.862310524418127,
1.),(1.,0.92377447201052,1.),(1.,0.923983993203425,1.),(1.,0.86257487372095,
1.),(1.,0.796615278835181,1.)))
REPRESENTATION_ITEM('')
SURFACE()
);
#3925=(
BOUNDED_SURFACE()
B_SPLINE_SURFACE(3,2,((#444357,#444358,#444359),(#444360,#444361,#444362),
(#444363,#444364,#444365),(#444366,#444367,#444368)),.UNSPECIFIED.,.F.,
 .F.,.F.)
B_SPLINE_SURFACE_WITH_KNOTS((4,4),(3,3),(0.,0.000101244905251112),(0.,1.),
 .UNSPECIFIED.)
GEOMETRIC_REPRESENTATION_ITEM()
RATIONAL_B_SPLINE_SURFACE(((1.,0.79661527883517,1.),(1.,0.795896146109792,
1.),(1.,0.7951935657965,1.),(1.,0.794506502889901,1.)))
REPRESENTATION_ITEM('')
SURFACE()
);
#3926=(
BOUNDED_SURFACE()
B_SPLINE_SURFACE(3,2,((#444404,#444405,#444406),(#444407,#444408,#444409),
(#444410,#444411,#444412),(#444413,#444414,#444415)),.UNSPECIFIED.,.F.,
 .F.,.F.)
B_SPLINE_SURFACE_WITH_KNOTS((4,4),(3,3),(2.85968127239938E-5,9.24681548475814E-5),
(-0.00167900678701706,1.0113082712782),.UNSPECIFIED.)
GEOMETRIC_REPRESENTATION_ITEM()
RATIONAL_B_SPLINE_SURFACE(((1.00059040895233,0.82218754186819,1.00401468696656),
(1.0003652771815,0.889990093671522,1.00248382673391),(1.00016469515018,
0.950399042257911,1.00111990082511),(1.00025604274,0.922888044286047,1.00174104990631)))
REPRESENTATION_ITEM('')
SURFACE()
);
#3927=(
BOUNDED_SURFACE()
B_SPLINE_SURFACE(3,2,((#444419,#444420,#444421),(#444422,#444423,#444424),
(#444425,#444426,#444427),(#444428,#444429,#444430)),.UNSPECIFIED.,.F.,
 .F.,.F.)
B_SPLINE_SURFACE_WITH_KNOTS((4,4),(3,3),(-5.2235835674934E-6,5.74594192424275E-5),
(-0.00127120052040424,1.),.UNSPECIFIED.)
GEOMETRIC_REPRESENTATION_ITEM()
RATIONAL_B_SPLINE_SURFACE(((1.00054449313169,0.785835073638797,1.),(1.00047707767469,
0.812351526358888,1.),(1.00044031788581,0.826810216506311,1.),(1.00044777653313,
0.823876514387279,1.)))
REPRESENTATION_ITEM('')
SURFACE()
);
#3928=(
BOUNDED_SURFACE()
B_SPLINE_SURFACE(3,2,((#444432,#444433,#444434),(#444435,#444436,#444437),
(#444438,#444439,#444440),(#444441,#444442,#444443)),.UNSPECIFIED.,.F.,
 .F.,.F.)
B_SPLINE_SURFACE_WITH_KNOTS((4,4),(3,3),(-2.71050543121376E-19,4.88747512969877E-5),
(-0.000215805216116114,1.),.UNSPECIFIED.)
GEOMETRIC_REPRESENTATION_ITEM()
RATIONAL_B_SPLINE_SURFACE(((1.00008915600364,0.793434085499616,1.),(1.00008930225017,
0.793095246303171,1.),(1.00008944684639,0.792760230720422,1.),(1.00008958984419,
0.792428918540464,1.)))
REPRESENTATION_ITEM('')
SURFACE()
);
#3929=(
BOUNDED_SURFACE()
B_SPLINE_SURFACE(3,2,((#444445,#444446,#444447),(#444448,#444449,#444450),
(#444451,#444452,#444453),(#444454,#444455,#444456),(#444457,#444458,#444459),
(#444460,#444461,#444462)),.UNSPECIFIED.,.F.,.F.,.F.)
B_SPLINE_SURFACE_WITH_KNOTS((4,2,4),(3,3),(3.93023287525995E-19,7.626750108632E-5,
0.00015253500217264),(0.,1.02152348203056),.UNSPECIFIED.)
GEOMETRIC_REPRESENTATION_ITEM()
RATIONAL_B_SPLINE_SURFACE(((1.,0.789033595401277,1.00908146323686),(1.,
0.857071781054839,1.00615262590425),(1.,0.922087264710758,1.0033539067159),
(1.,0.92239446650236,1.00334068261142),(1.,0.857224384599083,1.00614605678497),
(1.,0.789033595401673,1.00908146323685)))
REPRESENTATION_ITEM('')
SURFACE()
);
#3930=(
BOUNDED_SURFACE()
B_SPLINE_SURFACE(3,2,((#444464,#444465,#444466),(#444467,#444468,#444469),
(#444470,#444471,#444472),(#444473,#444474,#444475)),.UNSPECIFIED.,.F.,
 .F.,.F.)
B_SPLINE_SURFACE_WITH_KNOTS((4,4),(3,3),(2.16840434497101E-19,4.88747512969882E-5),
(-0.000215489857183668,1.),.UNSPECIFIED.)
GEOMETRIC_REPRESENTATION_ITEM()
RATIONAL_B_SPLINE_SURFACE(((1.00008945889719,0.792428983985715,1.),(1.00008931610841,
0.792760296061256,1.),(1.00008917172353,0.793095311538336,1.),(1.00008902569076,
0.793434150627967,1.)))
REPRESENTATION_ITEM('')
SURFACE()
);
#3931=(
BOUNDED_SURFACE()
B_SPLINE_SURFACE(3,2,((#444477,#444478,#444479),(#444480,#444481,#444482),
(#444483,#444484,#444485),(#444486,#444487,#444488)),.UNSPECIFIED.,.F.,
 .F.,.F.)
B_SPLINE_SURFACE_WITH_KNOTS((4,4),(3,3),(-5.2197490501309E-6,5.74172395514396E-5),
(-0.00139822857793751,1.0005131236405),.UNSPECIFIED.)
GEOMETRIC_REPRESENTATION_ITEM()
RATIONAL_B_SPLINE_SURFACE(((1.00049256947264,0.823768952243972,1.00018060397843),
(1.00048448215734,0.826662424388268,1.00017763870876),(1.00052427784043,
0.812424361909329,1.00019223006915),(1.00059912365879,0.785646094632703,
1.00021967280224)))
REPRESENTATION_ITEM('')
SURFACE()
);
#3932=(
BOUNDED_SURFACE()
B_SPLINE_SURFACE(3,2,((#444492,#444493,#444494),(#444495,#444496,#444497),
(#444498,#444499,#444500),(#444501,#444502,#444503)),.UNSPECIFIED.,.F.,
 .F.,.F.)
B_SPLINE_SURFACE_WITH_KNOTS((4,4),(3,3),(3.2298077433778E-5,9.63764854872254E-5),
(-0.00154325936349561,1.01095292447536),.UNSPECIFIED.)
GEOMETRIC_REPRESENTATION_ITEM()
RATIONAL_B_SPLINE_SURFACE(((1.00023530983295,0.922925743796188,1.0016857472833),
(1.00015136166123,0.950422439594238,1.00108434699059),(1.00033574337393,
0.890029368953987,1.00240524789546),(1.00054260094213,0.822274473168394,
1.00388716464855)))
REPRESENTATION_ITEM('')
SURFACE()
);
#3933=(
BOUNDED_SURFACE()
B_SPLINE_SURFACE(3,2,((#444603,#444604,#444605),(#444606,#444607,#444608),
(#444609,#444610,#444611),(#444612,#444613,#444614)),.UNSPECIFIED.,.F.,
 .F.,.F.)
B_SPLINE_SURFACE_WITH_KNOTS((4,4),(3,3),(0.,0.000101260117256737),(0.,1.),
 .UNSPECIFIED.)
GEOMETRIC_REPRESENTATION_ITEM()
RATIONAL_B_SPLINE_SURFACE(((1.,0.796615278835171,1.),(1.,0.795896038055939,
1.),(1.,0.795193354661347,1.),(1.,0.794506193185534,1.)))
REPRESENTATION_ITEM('')
SURFACE()
);
#3934=(
BOUNDED_SURFACE()
B_SPLINE_SURFACE(3,2,((#444652,#444653,#444654),(#444655,#444656,#444657),
(#444658,#444659,#444660),(#444661,#444662,#444663),(#444664,#444665,#444666),
(#444667,#444668,#444669)),.UNSPECIFIED.,.F.,.F.,.F.)
B_SPLINE_SURFACE_WITH_KNOTS((4,2,4),(3,3),(2.3039296165317E-19,1.66936432462298E-5,
3.33872864924594E-5),(0.,1.),.UNSPECIFIED.)
GEOMETRIC_REPRESENTATION_ITEM()
RATIONAL_B_SPLINE_SURFACE(((1.,0.796615278835177,1.),(1.,0.862310524418133,
1.),(1.,0.923774472010522,1.),(1.,0.923983993203425,1.),(1.,0.862574873720947,
1.),(1.,0.796615278835184,1.)))
REPRESENTATION_ITEM('')
SURFACE()
);
#3935=(
BOUNDED_SURFACE()
B_SPLINE_SURFACE(3,2,((#444706,#444707,#444708),(#444709,#444710,#444711),
(#444712,#444713,#444714),(#444715,#444716,#444717)),.UNSPECIFIED.,.F.,
 .F.,.F.)
B_SPLINE_SURFACE_WITH_KNOTS((4,4),(3,3),(-2.16840434497101E-19,0.000101244905251112),
(0.,1.),.UNSPECIFIED.)
GEOMETRIC_REPRESENTATION_ITEM()
RATIONAL_B_SPLINE_SURFACE(((1.,0.796615278835171,1.),(1.,0.795896146109795,
1.),(1.,0.795193565796498,1.),(1.,0.794506502889903,1.)))
REPRESENTATION_ITEM('')
SURFACE()
);
#3936=(
BOUNDED_SURFACE()
B_SPLINE_SURFACE(3,2,((#444753,#444754,#444755),(#444756,#444757,#444758),
(#444759,#444760,#444761),(#444762,#444763,#444764)),.UNSPECIFIED.,.F.,
 .F.,.F.)
B_SPLINE_SURFACE_WITH_KNOTS((4,4),(3,3),(2.85968127239939E-5,9.24681548475817E-5),
(-0.00167900678690871,1.01130827127831),.UNSPECIFIED.)
GEOMETRIC_REPRESENTATION_ITEM()
RATIONAL_B_SPLINE_SURFACE(((1.0005904089523,0.822187541868189,1.0040146869666),
(1.00036527718148,0.889990093671519,1.00248382673393),(1.00016469515017,
0.950399042257909,1.00111990082512),(1.00025604273998,0.922888044286045,
1.00174104990632)))
REPRESENTATION_ITEM('')
SURFACE()
);
#3937=(
BOUNDED_SURFACE()
B_SPLINE_SURFACE(3,2,((#444768,#444769,#444770),(#444771,#444772,#444773),
(#444774,#444775,#444776),(#444777,#444778,#444779)),.UNSPECIFIED.,.F.,
 .F.,.F.)
B_SPLINE_SURFACE_WITH_KNOTS((4,4),(3,3),(-5.22358356749282E-6,5.74594192424277E-5),
(-0.00127120052078626,1.),.UNSPECIFIED.)
GEOMETRIC_REPRESENTATION_ITEM()
RATIONAL_B_SPLINE_SURFACE(((1.00054449313185,0.785835073638714,1.),(1.00047707767483,
0.812351526358813,1.),(1.00044031788594,0.826810216506242,1.),(1.00044777653327,
0.823876514387215,1.)))
REPRESENTATION_ITEM('')
SURFACE()
);
#3938=(
BOUNDED_SURFACE()
B_SPLINE_SURFACE(3,2,((#444781,#444782,#444783),(#444784,#444785,#444786),
(#444787,#444788,#444789),(#444790,#444791,#444792)),.UNSPECIFIED.,.F.,
 .F.,.F.)
B_SPLINE_SURFACE_WITH_KNOTS((4,4),(3,3),(-2.71050543121376E-19,4.88747512969883E-5),
(-0.000215805215133611,1.),.UNSPECIFIED.)
GEOMETRIC_REPRESENTATION_ITEM()
RATIONAL_B_SPLINE_SURFACE(((1.00008915600324,0.793434085499815,1.),(1.00008930224977,
0.793095246303358,1.),(1.00008944684599,0.792760230720632,1.),(1.00008958984378,
0.792428918540665,1.)))
REPRESENTATION_ITEM('')
SURFACE()
);
#3939=(
BOUNDED_SURFACE()
B_SPLINE_SURFACE(3,2,((#444794,#444795,#444796),(#444797,#444798,#444799),
(#444800,#444801,#444802),(#444803,#444804,#444805),(#444806,#444807,#444808),
(#444809,#444810,#444811)),.UNSPECIFIED.,.F.,.F.,.F.)
B_SPLINE_SURFACE_WITH_KNOTS((4,2,4),(3,3),(2.03287907341032E-19,7.62675010863199E-5,
0.00015253500217264),(0.,1.02152348203091),.UNSPECIFIED.)
GEOMETRIC_REPRESENTATION_ITEM()
RATIONAL_B_SPLINE_SURFACE(((1.,0.789033595401203,1.00908146323702),(1.,
0.857071781054809,1.00615262590435),(1.,0.922087264710707,1.00335390671596),
(1.,0.922394466502357,1.00334068261147),(1.,0.857224384599022,1.00614605678507),
(1.,0.789033595401601,1.009081463237)))
REPRESENTATION_ITEM('')
SURFACE()
);
#3940=(
BOUNDED_SURFACE()
B_SPLINE_SURFACE(3,2,((#444813,#444814,#444815),(#444816,#444817,#444818),
(#444819,#444820,#444821),(#444822,#444823,#444824)),.UNSPECIFIED.,.F.,
 .F.,.F.)
B_SPLINE_SURFACE_WITH_KNOTS((4,4),(3,3),(1.35525271560688E-19,4.88747512969882E-5),
(-0.000215489856921436,1.),.UNSPECIFIED.)
GEOMETRIC_REPRESENTATION_ITEM()
RATIONAL_B_SPLINE_SURFACE(((1.00008945889708,0.792428983985769,1.),(1.0000893161083,
0.792760296061308,1.),(1.00008917172343,0.793095311538394,1.),(1.00008902569065,
0.79343415062802,1.)))
REPRESENTATION_ITEM('')
SURFACE()
);
#3941=(
BOUNDED_SURFACE()
B_SPLINE_SURFACE(3,2,((#444826,#444827,#444828),(#444829,#444830,#444831),
(#444832,#444833,#444834),(#444835,#444836,#444837)),.UNSPECIFIED.,.F.,
 .F.,.F.)
B_SPLINE_SURFACE_WITH_KNOTS((4,4),(3,3),(-5.21974905012869E-6,5.74172395514383E-5),
(-0.0013982285776812,1.00051312364052),.UNSPECIFIED.)
GEOMETRIC_REPRESENTATION_ITEM()
RATIONAL_B_SPLINE_SURFACE(((1.00049256947255,0.823768952244018,1.00018060397844),
(1.00048448215725,0.826662424388302,1.00017763870877),(1.00052427784033,
0.812424361909381,1.00019223006916),(1.00059912365868,0.78564609463275,
1.00021967280225)))
REPRESENTATION_ITEM('')
SURFACE()
);
#3942=(
BOUNDED_SURFACE()
B_SPLINE_SURFACE(3,2,((#444841,#444842,#444843),(#444844,#444845,#444846),
(#444847,#444848,#444849),(#444850,#444851,#444852)),.UNSPECIFIED.,.F.,
 .F.,.F.)
B_SPLINE_SURFACE_WITH_KNOTS((4,4),(3,3),(3.22980774337779E-5,9.63764854872253E-5),
(-0.00154325936290737,1.01095292447553),.UNSPECIFIED.)
GEOMETRIC_REPRESENTATION_ITEM()
RATIONAL_B_SPLINE_SURFACE(((1.00023530983286,0.92292574379622,1.00168574728332),
(1.00015136166117,0.950422439594252,1.00108434699061),(1.0003357433738,
0.890029368954036,1.0024052478955),(1.00054260094192,0.822274473168471,
1.00388716464861)))
REPRESENTATION_ITEM('')
SURFACE()
);
#3943=(
BOUNDED_SURFACE()
B_SPLINE_SURFACE(3,2,((#444952,#444953,#444954),(#444955,#444956,#444957),
(#444958,#444959,#444960),(#444961,#444962,#444963)),.UNSPECIFIED.,.F.,
 .F.,.F.)
B_SPLINE_SURFACE_WITH_KNOTS((4,4),(3,3),(0.,0.000101260117256737),(0.,1.),
 .UNSPECIFIED.)
GEOMETRIC_REPRESENTATION_ITEM()
RATIONAL_B_SPLINE_SURFACE(((1.,0.796615278835171,1.),(1.,0.79589603805594,
1.),(1.,0.795193354661346,1.),(1.,0.794506193185533,1.)))
REPRESENTATION_ITEM('')
SURFACE()
);
#3944=(
BOUNDED_SURFACE()
B_SPLINE_SURFACE(3,2,((#445001,#445002,#445003),(#445004,#445005,#445006),
(#445007,#445008,#445009),(#445010,#445011,#445012),(#445013,#445014,#445015),
(#445016,#445017,#445018)),.UNSPECIFIED.,.F.,.F.,.F.)
B_SPLINE_SURFACE_WITH_KNOTS((4,2,4),(3,3),(-2.11758236813575E-19,1.66936432462294E-5,
3.3387286492459E-5),(0.,1.),.UNSPECIFIED.)
GEOMETRIC_REPRESENTATION_ITEM()
RATIONAL_B_SPLINE_SURFACE(((1.,0.796615278835173,1.),(1.,0.862310524418121,
1.),(1.,0.923774472010524,1.),(1.,0.923983993203421,1.),(1.,0.862574873720939,
1.),(1.,0.796615278835189,1.)))
REPRESENTATION_ITEM('')
SURFACE()
);
#3945=(
BOUNDED_SURFACE()
B_SPLINE_SURFACE(3,2,((#445055,#445056,#445057),(#445058,#445059,#445060),
(#445061,#445062,#445063),(#445064,#445065,#445066)),.UNSPECIFIED.,.F.,
 .F.,.F.)
B_SPLINE_SURFACE_WITH_KNOTS((4,4),(3,3),(0.,0.000101244905251112),(0.,1.),
 .UNSPECIFIED.)
GEOMETRIC_REPRESENTATION_ITEM()
RATIONAL_B_SPLINE_SURFACE(((1.,0.796615278835172,1.),(1.,0.795896146109794,
1.),(1.,0.795193565796497,1.),(1.,0.7945065028899,1.)))
REPRESENTATION_ITEM('')
SURFACE()
);
#3946=(
BOUNDED_SURFACE()
B_SPLINE_SURFACE(3,2,((#445102,#445103,#445104),(#445105,#445106,#445107),
(#445108,#445109,#445110),(#445111,#445112,#445113)),.UNSPECIFIED.,.F.,
 .F.,.F.)
B_SPLINE_SURFACE_WITH_KNOTS((4,4),(3,3),(2.85968127239939E-5,9.24681548475818E-5),
(-0.00167900678679091,1.01130827127834),.UNSPECIFIED.)
GEOMETRIC_REPRESENTATION_ITEM()
RATIONAL_B_SPLINE_SURFACE(((1.00059040895225,0.822187541868203,1.00401468696661),
(1.00036527718145,0.889990093671535,1.00248382673394),(1.00016469515015,
0.950399042257911,1.00111990082512),(1.00025604273996,0.922888044286052,
1.00174104990633)))
REPRESENTATION_ITEM('')
SURFACE()
);
#3947=(
BOUNDED_SURFACE()
B_SPLINE_SURFACE(3,2,((#445117,#445118,#445119),(#445120,#445121,#445122),
(#445123,#445124,#445125),(#445126,#445127,#445128)),.UNSPECIFIED.,.F.,
 .F.,.F.)
B_SPLINE_SURFACE_WITH_KNOTS((4,4),(3,3),(-5.22358356749289E-6,5.74594192424278E-5),
(-0.00127120052035666,1.),.UNSPECIFIED.)
GEOMETRIC_REPRESENTATION_ITEM()
RATIONAL_B_SPLINE_SURFACE(((1.00054449313166,0.785835073638806,1.),(1.00047707767467,
0.812351526358888,1.),(1.0004403178858,0.826810216506318,1.),(1.00044777653312,
0.823876514387286,1.)))
REPRESENTATION_ITEM('')
SURFACE()
);
#3948=(
BOUNDED_SURFACE()
B_SPLINE_SURFACE(3,2,((#445130,#445131,#445132),(#445133,#445134,#445135),
(#445136,#445137,#445138),(#445139,#445140,#445141)),.UNSPECIFIED.,.F.,
 .F.,.F.)
B_SPLINE_SURFACE_WITH_KNOTS((4,4),(3,3),(-1.0842021724855E-19,4.8874751296988E-5),
(-0.000215805215040772,1.),.UNSPECIFIED.)
GEOMETRIC_REPRESENTATION_ITEM()
RATIONAL_B_SPLINE_SURFACE(((1.0000891560032,0.793434085499837,1.),(1.00008930224973,
0.793095246303369,1.),(1.00008944684595,0.792760230720652,1.),(1.00008958984374,
0.792428918540683,1.)))
REPRESENTATION_ITEM('')
SURFACE()
);
#3949=(
BOUNDED_SURFACE()
B_SPLINE_SURFACE(3,2,((#445143,#445144,#445145),(#445146,#445147,#445148),
(#445149,#445150,#445151),(#445152,#445153,#445154),(#445155,#445156,#445157),
(#445158,#445159,#445160)),.UNSPECIFIED.,.F.,.F.,.F.)
B_SPLINE_SURFACE_WITH_KNOTS((4,2,4),(3,3),(6.7762635780344E-20,7.62675010863195E-5,
0.000152535002172639),(0.,1.0215234820307),.UNSPECIFIED.)
GEOMETRIC_REPRESENTATION_ITEM()
RATIONAL_B_SPLINE_SURFACE(((1.,0.789033595401244,1.00908146323692),(1.,
0.85707178105484,1.00615262590429),(1.,0.922087264710726,1.00335390671592),
(1.,0.922394466502372,1.00334068261144),(1.,0.857224384599049,1.00614605678501),
(1.,0.789033595401646,1.00908146323691)))
REPRESENTATION_ITEM('')
SURFACE()
);
#3950=(
BOUNDED_SURFACE()
B_SPLINE_SURFACE(3,2,((#445162,#445163,#445164),(#445165,#445166,#445167),
(#445168,#445169,#445170),(#445171,#445172,#445173)),.UNSPECIFIED.,.F.,
 .F.,.F.)
B_SPLINE_SURFACE_WITH_KNOTS((4,4),(3,3),(2.16840434497101E-19,4.8874751296988E-5),
(-0.000215489856918745,1.),.UNSPECIFIED.)
GEOMETRIC_REPRESENTATION_ITEM()
RATIONAL_B_SPLINE_SURFACE(((1.00008945889708,0.79242898398577,1.),(1.0000893161083,
0.792760296061318,1.),(1.00008917172342,0.793095311538385,1.),(1.00008902569065,
0.793434150628019,1.)))
REPRESENTATION_ITEM('')
SURFACE()
);
#3951=(
BOUNDED_SURFACE()
B_SPLINE_SURFACE(3,2,((#445175,#445176,#445177),(#445178,#445179,#445180),
(#445181,#445182,#445183),(#445184,#445185,#445186)),.UNSPECIFIED.,.F.,
 .F.,.F.)
B_SPLINE_SURFACE_WITH_KNOTS((4,4),(3,3),(-5.21974905013088E-6,5.7417239551438E-5),
(-0.00139822857722359,1.00051312364048),.UNSPECIFIED.)
GEOMETRIC_REPRESENTATION_ITEM()
RATIONAL_B_SPLINE_SURFACE(((1.00049256947238,0.823768952244102,1.00018060397842),
(1.00048448215709,0.826662424388395,1.00017763870876),(1.00052427784016,
0.812424361909474,1.00019223006914),(1.00059912365849,0.78564609463286,
1.00021967280223)))
REPRESENTATION_ITEM('')
SURFACE()
);
#3952=(
BOUNDED_SURFACE()
B_SPLINE_SURFACE(3,2,((#445190,#445191,#445192),(#445193,#445194,#445195),
(#445196,#445197,#445198),(#445199,#445200,#445201)),.UNSPECIFIED.,.F.,
 .F.,.F.)
B_SPLINE_SURFACE_WITH_KNOTS((4,4),(3,3),(3.2298077433778E-5,9.63764854872249E-5),
(-0.00154325936386665,1.01095292447556),.UNSPECIFIED.)
GEOMETRIC_REPRESENTATION_ITEM()
RATIONAL_B_SPLINE_SURFACE(((1.00023530983301,0.922925743796142,1.00168574728333),
(1.00015136166127,0.95042243959421,1.00108434699061),(1.00033574337401,
0.890029368953932,1.0024052478955),(1.00054260094226,0.822274473168286,
1.00388716464863)))
REPRESENTATION_ITEM('')
SURFACE()
);
#3953=(
BOUNDED_SURFACE()
B_SPLINE_SURFACE(3,2,((#445301,#445302,#445303),(#445304,#445305,#445306),
(#445307,#445308,#445309),(#445310,#445311,#445312)),.UNSPECIFIED.,.F.,
 .F.,.F.)
B_SPLINE_SURFACE_WITH_KNOTS((4,4),(3,3),(-4.33680868994202E-19,0.000101260117256737),
(0.,1.),.UNSPECIFIED.)
GEOMETRIC_REPRESENTATION_ITEM()
RATIONAL_B_SPLINE_SURFACE(((1.,0.796615278835171,1.),(1.,0.795896038055937,
1.),(1.,0.795193354661347,1.),(1.,0.794506193185543,1.)))
REPRESENTATION_ITEM('')
SURFACE()
);
#3954=(
BOUNDED_SURFACE()
B_SPLINE_SURFACE(3,2,((#445350,#445351,#445352),(#445353,#445354,#445355),
(#445356,#445357,#445358),(#445359,#445360,#445361),(#445362,#445363,#445364),
(#445365,#445366,#445367)),.UNSPECIFIED.,.F.,.F.,.F.)
B_SPLINE_SURFACE_WITH_KNOTS((4,2,4),(3,3),(1.35525271560688E-20,1.66936432462295E-5,
3.33872864924589E-5),(0.,1.),.UNSPECIFIED.)
GEOMETRIC_REPRESENTATION_ITEM()
RATIONAL_B_SPLINE_SURFACE(((1.,0.796615278835177,1.),(1.,0.862310524418129,
1.),(1.,0.92377447201052,1.),(1.,0.923983993203425,1.),(1.,0.862574873720951,
1.),(1.,0.796615278835181,1.)))
REPRESENTATION_ITEM('')
SURFACE()
);
#3955=(
BOUNDED_SURFACE()
B_SPLINE_SURFACE(3,2,((#445404,#445405,#445406),(#445407,#445408,#445409),
(#445410,#445411,#445412),(#445413,#445414,#445415)),.UNSPECIFIED.,.F.,
 .F.,.F.)
B_SPLINE_SURFACE_WITH_KNOTS((4,4),(3,3),(-2.16840434497101E-19,0.000101244905251112),
(0.,1.),.UNSPECIFIED.)
GEOMETRIC_REPRESENTATION_ITEM()
RATIONAL_B_SPLINE_SURFACE(((1.,0.796615278835172,1.),(1.,0.795896146109783,
1.),(1.,0.795193565796517,1.),(1.,0.794506502889896,1.)))
REPRESENTATION_ITEM('')
SURFACE()
);
#3956=(
BOUNDED_SURFACE()
B_SPLINE_SURFACE(3,2,((#445451,#445452,#445453),(#445454,#445455,#445456),
(#445457,#445458,#445459),(#445460,#445461,#445462)),.UNSPECIFIED.,.F.,
 .F.,.F.)
B_SPLINE_SURFACE_WITH_KNOTS((4,4),(3,3),(2.85968127239939E-5,9.24681548475817E-5),
(-0.00167900678782723,1.01130827127812),.UNSPECIFIED.)
GEOMETRIC_REPRESENTATION_ITEM()
RATIONAL_B_SPLINE_SURFACE(((1.00059040895262,0.822187541868066,1.00401468696653),
(1.00036527718168,0.88999009367143,1.00248382673389),(1.00016469515026,
0.950399042257876,1.0011199008251),(1.00025604274012,0.922888044285988,
1.0017410499063)))
REPRESENTATION_ITEM('')
SURFACE()
);
#3957=(
BOUNDED_SURFACE()
B_SPLINE_SURFACE(3,2,((#445466,#445467,#445468),(#445469,#445470,#445471),
(#445472,#445473,#445474),(#445475,#445476,#445477)),.UNSPECIFIED.,.F.,
 .F.,.F.)
B_SPLINE_SURFACE_WITH_KNOTS((4,4),(3,3),(-5.22358356749287E-6,5.74594192424278E-5),
(-0.00127120052040456,1.),.UNSPECIFIED.)
GEOMETRIC_REPRESENTATION_ITEM()
RATIONAL_B_SPLINE_SURFACE(((1.00054449313169,0.785835073638795,1.),(1.00047707767469,
0.812351526358882,1.),(1.00044031788581,0.826810216506303,1.),(1.00044777653313,
0.823876514387282,1.)))
REPRESENTATION_ITEM('')
SURFACE()
);
#3958=(
BOUNDED_SURFACE()
B_SPLINE_SURFACE(3,2,((#445479,#445480,#445481),(#445482,#445483,#445484),
(#445485,#445486,#445487),(#445488,#445489,#445490)),.UNSPECIFIED.,.F.,
 .F.,.F.)
B_SPLINE_SURFACE_WITH_KNOTS((4,4),(3,3),(-4.06575814682064E-19,4.88747512969879E-5),
(-0.000215805216148118,1.),.UNSPECIFIED.)
GEOMETRIC_REPRESENTATION_ITEM()
RATIONAL_B_SPLINE_SURFACE(((1.00008915600365,0.793434085499607,1.),(1.00008930225019,
0.793095246303155,1.),(1.00008944684641,0.792760230720426,1.),(1.0000895898442,
0.792428918540454,1.)))
REPRESENTATION_ITEM('')
SURFACE()
);
#3959=(
BOUNDED_SURFACE()
B_SPLINE_SURFACE(3,2,((#445492,#445493,#445494),(#445495,#445496,#445497),
(#445498,#445499,#445500),(#445501,#445502,#445503),(#445504,#445505,#445506),
(#445507,#445508,#445509)),.UNSPECIFIED.,.F.,.F.,.F.)
B_SPLINE_SURFACE_WITH_KNOTS((4,2,4),(3,3),(4.94667241196511E-19,7.626750108632E-5,
0.000152535002172639),(0.,1.0215234820307),.UNSPECIFIED.)
GEOMETRIC_REPRESENTATION_ITEM()
RATIONAL_B_SPLINE_SURFACE(((1.,0.789033595401248,1.00908146323693),(1.,
0.857071781054843,1.00615262590429),(1.,0.922087264710718,1.00335390671592),
(1.,0.922394466502379,1.00334068261144),(1.,0.857224384599044,1.00614605678501),
(1.,0.789033595401645,1.00908146323691)))
REPRESENTATION_ITEM('')
SURFACE()
);
#3960=(
BOUNDED_SURFACE()
B_SPLINE_SURFACE(3,2,((#445511,#445512,#445513),(#445514,#445515,#445516),
(#445517,#445518,#445519),(#445520,#445521,#445522)),.UNSPECIFIED.,.F.,
 .F.,.F.)
B_SPLINE_SURFACE_WITH_KNOTS((4,4),(3,3),(3.52365706057789E-19,4.88747512969884E-5),
(-0.000215489857968907,1.),.UNSPECIFIED.)
GEOMETRIC_REPRESENTATION_ITEM()
RATIONAL_B_SPLINE_SURFACE(((1.00008945889752,0.792428983985552,1.),(1.00008931610873,
0.792760296061093,1.),(1.00008917172386,0.793095311538178,1.),(1.00008902569108,
0.793434150627804,1.)))
REPRESENTATION_ITEM('')
SURFACE()
);
#3961=(
BOUNDED_SURFACE()
B_SPLINE_SURFACE(3,2,((#445524,#445525,#445526),(#445527,#445528,#445529),
(#445530,#445531,#445532),(#445533,#445534,#445535)),.UNSPECIFIED.,.F.,
 .F.,.F.)
B_SPLINE_SURFACE_WITH_KNOTS((4,4),(3,3),(-5.21974905012869E-6,5.74172395514398E-5),
(-0.00139822857721556,1.00051312364053),.UNSPECIFIED.)
GEOMETRIC_REPRESENTATION_ITEM()
RATIONAL_B_SPLINE_SURFACE(((1.00049256947238,0.823768952244095,1.00018060397845),
(1.00048448215709,0.826662424388383,1.00017763870878),(1.00052427784016,
0.812424361909465,1.00019223006916),(1.00059912365848,0.785646094632845,
1.00021967280225)))
REPRESENTATION_ITEM('')
SURFACE()
);
#3962=(
BOUNDED_SURFACE()
B_SPLINE_SURFACE(3,2,((#445539,#445540,#445541),(#445542,#445543,#445544),
(#445545,#445546,#445547),(#445548,#445549,#445550)),.UNSPECIFIED.,.F.,
 .F.,.F.)
B_SPLINE_SURFACE_WITH_KNOTS((4,4),(3,3),(3.22980774337778E-5,9.63764854872256E-5),
(-0.0015432593639103,1.01095292447531),.UNSPECIFIED.)
GEOMETRIC_REPRESENTATION_ITEM()
RATIONAL_B_SPLINE_SURFACE(((1.00023530983302,0.922925743796159,1.00168574728329),
(1.00015136166127,0.950422439594222,1.00108434699058),(1.00033574337402,
0.890029368953943,1.00240524789545),(1.00054260094228,0.822274473168331,
1.00388716464854)))
REPRESENTATION_ITEM('')
SURFACE()
);
#3963=(
BOUNDED_SURFACE()
B_SPLINE_SURFACE(3,2,((#445650,#445651,#445652),(#445653,#445654,#445655),
(#445656,#445657,#445658),(#445659,#445660,#445661)),.UNSPECIFIED.,.F.,
 .F.,.F.)
B_SPLINE_SURFACE_WITH_KNOTS((4,4),(3,3),(-4.33680868994202E-19,0.000101260117256737),
(0.,1.),.UNSPECIFIED.)
GEOMETRIC_REPRESENTATION_ITEM()
RATIONAL_B_SPLINE_SURFACE(((1.,0.796615278835173,1.),(1.,0.795896038055939,
1.),(1.,0.79519335466135,1.),(1.,0.794506193185544,1.)))
REPRESENTATION_ITEM('')
SURFACE()
);
#3964=(
BOUNDED_SURFACE()
B_SPLINE_SURFACE(3,2,((#445699,#445700,#445701),(#445702,#445703,#445704),
(#445705,#445706,#445707),(#445708,#445709,#445710),(#445711,#445712,#445713),
(#445714,#445715,#445716)),.UNSPECIFIED.,.F.,.F.,.F.)
B_SPLINE_SURFACE_WITH_KNOTS((4,2,4),(3,3),(5.75982404132924E-20,1.66936432462296E-5,
3.33872864924592E-5),(0.,1.),.UNSPECIFIED.)
GEOMETRIC_REPRESENTATION_ITEM()
RATIONAL_B_SPLINE_SURFACE(((1.,0.796615278835172,1.),(1.,0.862310524418126,
1.),(1.,0.923774472010521,1.),(1.,0.923983993203426,1.),(1.,0.862574873720941,
1.),(1.,0.796615278835176,1.)))
REPRESENTATION_ITEM('')
SURFACE()
);
#3965=(
BOUNDED_SURFACE()
B_SPLINE_SURFACE(3,2,((#445753,#445754,#445755),(#445756,#445757,#445758),
(#445759,#445760,#445761),(#445762,#445763,#445764)),.UNSPECIFIED.,.F.,
 .F.,.F.)
B_SPLINE_SURFACE_WITH_KNOTS((4,4),(3,3),(0.,0.000101244905251112),(0.,1.),
 .UNSPECIFIED.)
GEOMETRIC_REPRESENTATION_ITEM()
RATIONAL_B_SPLINE_SURFACE(((1.,0.796615278835172,1.),(1.,0.795896146109795,
1.),(1.,0.79519356579651,1.),(1.,0.794506502889903,1.)))
REPRESENTATION_ITEM('')
SURFACE()
);
#3966=(
BOUNDED_SURFACE()
B_SPLINE_SURFACE(3,2,((#445800,#445801,#445802),(#445803,#445804,#445805),
(#445806,#445807,#445808),(#445809,#445810,#445811)),.UNSPECIFIED.,.F.,
 .F.,.F.)
B_SPLINE_SURFACE_WITH_KNOTS((4,4),(3,3),(2.85968127239939E-5,9.24681548475815E-5),
(-0.00167900678670585,1.01130827127827),.UNSPECIFIED.)
GEOMETRIC_REPRESENTATION_ITEM()
RATIONAL_B_SPLINE_SURFACE(((1.00059040895222,0.822187541868234,1.00401468696658),
(1.00036527718143,0.889990093671548,1.00248382673392),(1.00016469515015,
0.950399042257928,1.00111990082511),(1.00025604273995,0.922888044286062,
1.00174104990632)))
REPRESENTATION_ITEM('')
SURFACE()
);
#3967=(
BOUNDED_SURFACE()
B_SPLINE_SURFACE(3,2,((#445815,#445816,#445817),(#445818,#445819,#445820),
(#445821,#445822,#445823),(#445824,#445825,#445826)),.UNSPECIFIED.,.F.,
 .F.,.F.)
B_SPLINE_SURFACE_WITH_KNOTS((4,4),(3,3),(-5.22358356749319E-6,5.74594192424276E-5),
(-0.00127120052051403,1.),.UNSPECIFIED.)
GEOMETRIC_REPRESENTATION_ITEM()
RATIONAL_B_SPLINE_SURFACE(((1.00054449313173,0.78583507363877,1.),(1.00047707767473,
0.812351526358864,1.),(1.00044031788585,0.82681021650629,1.),(1.00044777653317,
0.823876514387265,1.)))
REPRESENTATION_ITEM('')
SURFACE()
);
#3968=(
BOUNDED_SURFACE()
B_SPLINE_SURFACE(3,2,((#445828,#445829,#445830),(#445831,#445832,#445833),
(#445834,#445835,#445836),(#445837,#445838,#445839)),.UNSPECIFIED.,.F.,
 .F.,.F.)
B_SPLINE_SURFACE_WITH_KNOTS((4,4),(3,3),(2.71050543121376E-20,4.88747512969881E-5),
(-0.00021580521507922,1.),.UNSPECIFIED.)
GEOMETRIC_REPRESENTATION_ITEM()
RATIONAL_B_SPLINE_SURFACE(((1.00008915600321,0.793434085499829,1.),(1.00008930224974,
0.79309524630337,1.),(1.00008944684596,0.792760230720645,1.),(1.00008958984376,
0.792428918540678,1.)))
REPRESENTATION_ITEM('')
SURFACE()
);
#3969=(
BOUNDED_SURFACE()
B_SPLINE_SURFACE(3,2,((#445841,#445842,#445843),(#445844,#445845,#445846),
(#445847,#445848,#445849),(#445850,#445851,#445852),(#445853,#445854,#445855),
(#445856,#445857,#445858)),.UNSPECIFIED.,.F.,.F.,.F.)
B_SPLINE_SURFACE_WITH_KNOTS((4,2,4),(3,3),(-1.76182853028894E-19,7.62675010863195E-5,
0.000152535002172639),(0.,1.02152348203063),.UNSPECIFIED.)
GEOMETRIC_REPRESENTATION_ITEM()
RATIONAL_B_SPLINE_SURFACE(((1.,0.78903359540126,1.00908146323689),(1.,0.857071781054843,
1.00615262590427),(1.,0.922087264710726,1.00335390671591),(1.,0.922394466502384,
1.00334068261143),(1.,0.857224384599053,1.00614605678499),(1.,0.78903359540166,
1.00908146323688)))
REPRESENTATION_ITEM('')
SURFACE()
);
#3970=(
BOUNDED_SURFACE()
B_SPLINE_SURFACE(3,2,((#445860,#445861,#445862),(#445863,#445864,#445865),
(#445866,#445867,#445868),(#445869,#445870,#445871)),.UNSPECIFIED.,.F.,
 .F.,.F.)
B_SPLINE_SURFACE_WITH_KNOTS((4,4),(3,3),(6.23416249179165E-19,4.88747512969881E-5),
(-0.000215489857056772,1.),.UNSPECIFIED.)
GEOMETRIC_REPRESENTATION_ITEM()
RATIONAL_B_SPLINE_SURFACE(((1.00008945889714,0.792428983985737,1.),(1.00008931610836,
0.792760296061305,1.),(1.00008917172348,0.793095311538342,1.),(1.00008902569071,
0.793434150627993,1.)))
REPRESENTATION_ITEM('')
SURFACE()
);
#3971=(
BOUNDED_SURFACE()
B_SPLINE_SURFACE(3,2,((#445873,#445874,#445875),(#445876,#445877,#445878),
(#445879,#445880,#445881),(#445882,#445883,#445884)),.UNSPECIFIED.,.F.,
 .F.,.F.)
B_SPLINE_SURFACE_WITH_KNOTS((4,4),(3,3),(-5.21974905012868E-6,5.74172395514396E-5),
(-0.00139822857796667,1.00051312364096),.UNSPECIFIED.)
GEOMETRIC_REPRESENTATION_ITEM()
RATIONAL_B_SPLINE_SURFACE(((1.00049256947265,0.823768952243889,1.00018060397859),
(1.00048448215735,0.82666242438818,1.00017763870892),(1.00052427784044,
0.812424361909243,1.00019223006932),(1.0005991236588,0.785646094632596,
1.00021967280243)))
REPRESENTATION_ITEM('')
SURFACE()
);
#3972=(
BOUNDED_SURFACE()
B_SPLINE_SURFACE(3,2,((#445888,#445889,#445890),(#445891,#445892,#445893),
(#445894,#445895,#445896),(#445897,#445898,#445899)),.UNSPECIFIED.,.F.,
 .F.,.F.)
B_SPLINE_SURFACE_WITH_KNOTS((4,4),(3,3),(3.22980774337781E-5,9.63764854872251E-5),
(-0.00154325936385716,1.01095292447533),.UNSPECIFIED.)
GEOMETRIC_REPRESENTATION_ITEM()
RATIONAL_B_SPLINE_SURFACE(((1.00023530983301,0.922925743796162,1.00168574728329),
(1.00015136166127,0.950422439594222,1.00108434699059),(1.00033574337401,
0.890029368953952,1.00240524789545),(1.00054260094226,0.822274473168332,
1.00388716464854)))
REPRESENTATION_ITEM('')
SURFACE()
);
#3973=(
BOUNDED_SURFACE()
B_SPLINE_SURFACE(3,2,((#445999,#446000,#446001),(#446002,#446003,#446004),
(#446005,#446006,#446007),(#446008,#446009,#446010)),.UNSPECIFIED.,.F.,
 .F.,.F.)
B_SPLINE_SURFACE_WITH_KNOTS((4,4),(3,3),(0.,0.000101260117256738),(0.,1.),
 .UNSPECIFIED.)
GEOMETRIC_REPRESENTATION_ITEM()
RATIONAL_B_SPLINE_SURFACE(((1.,0.796615278835168,1.),(1.,0.795896038055949,
1.),(1.,0.795193354661346,1.),(1.,0.794506193185548,1.)))
REPRESENTATION_ITEM('')
SURFACE()
);
#3974=(
BOUNDED_SURFACE()
B_SPLINE_SURFACE(3,2,((#446048,#446049,#446050),(#446051,#446052,#446053),
(#446054,#446055,#446056),(#446057,#446058,#446059),(#446060,#446061,#446062),
(#446063,#446064,#446065)),.UNSPECIFIED.,.F.,.F.,.F.)
B_SPLINE_SURFACE_WITH_KNOTS((4,2,4),(3,3),(-2.4225142291473E-19,1.6693643246229E-5,
3.33872864924583E-5),(0.,1.),.UNSPECIFIED.)
GEOMETRIC_REPRESENTATION_ITEM()
RATIONAL_B_SPLINE_SURFACE(((1.,0.796615278835185,1.),(1.,0.862310524418132,
1.),(1.,0.92377447201052,1.),(1.,0.923983993203428,1.),(1.,0.862574873720944,
1.),(1.,0.796615278835193,1.)))
REPRESENTATION_ITEM('')
SURFACE()
);
#3975=(
BOUNDED_SURFACE()
B_SPLINE_SURFACE(3,2,((#446102,#446103,#446104),(#446105,#446106,#446107),
(#446108,#446109,#446110),(#446111,#446112,#446113)),.UNSPECIFIED.,.F.,
 .F.,.F.)
B_SPLINE_SURFACE_WITH_KNOTS((4,4),(3,3),(0.,0.000101244905251112),(0.,1.),
 .UNSPECIFIED.)
GEOMETRIC_REPRESENTATION_ITEM()
RATIONAL_B_SPLINE_SURFACE(((1.,0.796615278835176,1.),(1.,0.795896146109792,
1.),(1.,0.795193565796492,1.),(1.,0.794506502889906,1.)))
REPRESENTATION_ITEM('')
SURFACE()
);
#3976=(
BOUNDED_SURFACE()
B_SPLINE_SURFACE(3,2,((#446149,#446150,#446151),(#446152,#446153,#446154),
(#446155,#446156,#446157),(#446158,#446159,#446160)),.UNSPECIFIED.,.F.,
 .F.,.F.)
B_SPLINE_SURFACE_WITH_KNOTS((4,4),(3,3),(2.85968127239939E-5,9.24681548475817E-5),
(-0.00167900678634675,1.01130827127812),.UNSPECIFIED.)
GEOMETRIC_REPRESENTATION_ITEM()
RATIONAL_B_SPLINE_SURFACE(((1.0005904089521,0.822187541868325,1.00401468696653),
(1.00036527718135,0.889990093671606,1.00248382673389),(1.00016469515011,
0.950399042257947,1.0011199008251),(1.00025604273989,0.922888044286103,
1.0017410499063)))
REPRESENTATION_ITEM('')
SURFACE()
);
#3977=(
BOUNDED_SURFACE()
B_SPLINE_SURFACE(3,2,((#446164,#446165,#446166),(#446167,#446168,#446169),
(#446170,#446171,#446172),(#446173,#446174,#446175)),.UNSPECIFIED.,.F.,
 .F.,.F.)
B_SPLINE_SURFACE_WITH_KNOTS((4,4),(3,3),(-5.22358356749342E-6,5.74594192424275E-5),
(-0.00127120052036188,1.),.UNSPECIFIED.)
GEOMETRIC_REPRESENTATION_ITEM()
RATIONAL_B_SPLINE_SURFACE(((1.00054449313167,0.785835073638801,1.),(1.00047707767468,
0.812351526358897,1.),(1.0004403178858,0.826810216506308,1.),(1.00044777653312,
0.823876514387295,1.)))
REPRESENTATION_ITEM('')
SURFACE()
);
#3978=(
BOUNDED_SURFACE()
B_SPLINE_SURFACE(3,2,((#446177,#446178,#446179),(#446180,#446181,#446182),
(#446183,#446184,#446185),(#446186,#446187,#446188)),.UNSPECIFIED.,.F.,
 .F.,.F.)
B_SPLINE_SURFACE_WITH_KNOTS((4,4),(3,3),(-4.06575814682064E-19,4.88747512969881E-5),
(-0.000215805216127666,1.),.UNSPECIFIED.)
GEOMETRIC_REPRESENTATION_ITEM()
RATIONAL_B_SPLINE_SURFACE(((1.00008915600365,0.793434085499612,1.),(1.00008930225018,
0.793095246303167,1.),(1.0000894468464,0.792760230720418,1.),(1.00008958984419,
0.792428918540461,1.)))
REPRESENTATION_ITEM('')
SURFACE()
);
#3979=(
BOUNDED_SURFACE()
B_SPLINE_SURFACE(3,2,((#446190,#446191,#446192),(#446193,#446194,#446195),
(#446196,#446197,#446198),(#446199,#446200,#446201),(#446202,#446203,#446204),
(#446205,#446206,#446207)),.UNSPECIFIED.,.F.,.F.,.F.)
B_SPLINE_SURFACE_WITH_KNOTS((4,2,4),(3,3),(2.57498015965307E-19,7.62675010863196E-5,
0.000152535002172639),(0.,1.02152348203073),.UNSPECIFIED.)
GEOMETRIC_REPRESENTATION_ITEM()
RATIONAL_B_SPLINE_SURFACE(((1.,0.78903359540124,1.00908146323694),(1.,0.857071781054815,
1.0061526259043),(1.,0.922087264710745,1.00335390671593),(1.,0.922394466502351,
1.00334068261144),(1.,0.857224384599061,1.00614605678502),(1.,0.789033595401638,
1.00908146323692)))
REPRESENTATION_ITEM('')
SURFACE()
);
#3980=(
BOUNDED_SURFACE()
B_SPLINE_SURFACE(3,2,((#446209,#446210,#446211),(#446212,#446213,#446214),
(#446215,#446216,#446217),(#446218,#446219,#446220)),.UNSPECIFIED.,.F.,
 .F.,.F.)
B_SPLINE_SURFACE_WITH_KNOTS((4,4),(3,3),(2.71050543121376E-19,4.88747512969884E-5),
(-0.000215489857776657,1.),.UNSPECIFIED.)
GEOMETRIC_REPRESENTATION_ITEM()
RATIONAL_B_SPLINE_SURFACE(((1.00008945889744,0.792428983985584,1.),(1.00008931610865,
0.792760296061136,1.),(1.00008917172378,0.793095311538218,1.),(1.00008902569101,
0.793434150627841,1.)))
REPRESENTATION_ITEM('')
SURFACE()
);
#3981=(
BOUNDED_SURFACE()
B_SPLINE_SURFACE(3,2,((#446222,#446223,#446224),(#446225,#446226,#446227),
(#446228,#446229,#446230),(#446231,#446232,#446233)),.UNSPECIFIED.,.F.,
 .F.,.F.)
B_SPLINE_SURFACE_WITH_KNOTS((4,4),(3,3),(-5.21974905013089E-6,5.74172395514396E-5),
(-0.00139822857761498,1.00051312364071),.UNSPECIFIED.)
GEOMETRIC_REPRESENTATION_ITEM()
RATIONAL_B_SPLINE_SURFACE(((1.00049256947252,0.823768952243994,1.00018060397851),
(1.00048448215723,0.826662424388281,1.00017763870884),(1.00052427784031,
0.812424361909353,1.00019223006923),(1.00059912365865,0.785646094632723,
1.00021967280233)))
REPRESENTATION_ITEM('')
SURFACE()
);
#3982=(
BOUNDED_SURFACE()
B_SPLINE_SURFACE(3,2,((#446237,#446238,#446239),(#446240,#446241,#446242),
(#446243,#446244,#446245),(#446246,#446247,#446248)),.UNSPECIFIED.,.F.,
 .F.,.F.)
B_SPLINE_SURFACE_WITH_KNOTS((4,4),(3,3),(3.22980774337779E-5,9.6376485487225E-5),
(-0.00154325936391278,1.01095292447534),.UNSPECIFIED.)
GEOMETRIC_REPRESENTATION_ITEM()
RATIONAL_B_SPLINE_SURFACE(((1.00023530983302,0.922925743796155,1.0016857472833),
(1.00015136166127,0.95042243959421,1.00108434699059),(1.00033574337402,
0.890029368953955,1.00240524789546),(1.00054260094228,0.822274473168319,
1.00388716464855)))
REPRESENTATION_ITEM('')
SURFACE()
);
#3983=(
BOUNDED_SURFACE()
B_SPLINE_SURFACE(3,2,((#446348,#446349,#446350),(#446351,#446352,#446353),
(#446354,#446355,#446356),(#446357,#446358,#446359)),.UNSPECIFIED.,.F.,
 .F.,.F.)
B_SPLINE_SURFACE_WITH_KNOTS((4,4),(3,3),(-2.16840434497101E-19,0.000101260117256737),
(0.,1.),.UNSPECIFIED.)
GEOMETRIC_REPRESENTATION_ITEM()
RATIONAL_B_SPLINE_SURFACE(((1.,0.796615278835167,1.),(1.,0.795896038055957,
1.),(1.,0.795193354661325,1.),(1.,0.794506193185552,1.)))
REPRESENTATION_ITEM('')
SURFACE()
);
#3984=(
BOUNDED_SURFACE()
B_SPLINE_SURFACE(3,2,((#446397,#446398,#446399),(#446400,#446401,#446402),
(#446403,#446404,#446405),(#446406,#446407,#446408),(#446409,#446410,#446411),
(#446412,#446413,#446414)),.UNSPECIFIED.,.F.,.F.,.F.)
B_SPLINE_SURFACE_WITH_KNOTS((4,2,4),(3,3),(-9.65617559869902E-20,1.66936432462292E-5,
3.33872864924584E-5),(0.,1.),.UNSPECIFIED.)
GEOMETRIC_REPRESENTATION_ITEM()
RATIONAL_B_SPLINE_SURFACE(((1.,0.796615278835172,1.),(1.,0.862310524418138,
1.),(1.,0.923774472010516,1.),(1.,0.923983993203424,1.),(1.,0.862574873720945,
1.),(1.,0.796615278835193,1.)))
REPRESENTATION_ITEM('')
SURFACE()
);
#3985=(
BOUNDED_SURFACE()
B_SPLINE_SURFACE(3,2,((#446451,#446452,#446453),(#446454,#446455,#446456),
(#446457,#446458,#446459),(#446460,#446461,#446462)),.UNSPECIFIED.,.F.,
 .F.,.F.)
B_SPLINE_SURFACE_WITH_KNOTS((4,4),(3,3),(0.,0.000101244905251112),(0.,1.),
 .UNSPECIFIED.)
GEOMETRIC_REPRESENTATION_ITEM()
RATIONAL_B_SPLINE_SURFACE(((1.,0.796615278835168,1.),(1.,0.795896146109815,
1.),(1.,0.795193565796487,1.),(1.,0.794506502889903,1.)))
REPRESENTATION_ITEM('')
SURFACE()
);
#3986=(
BOUNDED_SURFACE()
B_SPLINE_SURFACE(3,2,((#446498,#446499,#446500),(#446501,#446502,#446503),
(#446504,#446505,#446506),(#446507,#446508,#446509)),.UNSPECIFIED.,.F.,
 .F.,.F.)
B_SPLINE_SURFACE_WITH_KNOTS((4,4),(3,3),(2.85968127239939E-5,9.24681548475817E-5),
(-0.00167900678566562,1.0113082712783),.UNSPECIFIED.)
GEOMETRIC_REPRESENTATION_ITEM()
RATIONAL_B_SPLINE_SURFACE(((1.00059040895186,0.822187541868416,1.00401468696659),
(1.0003652771812,0.889990093671664,1.00248382673393),(1.00016469515004,
0.950399042257967,1.00111990082512),(1.00025604273979,0.922888044286144,
1.00174104990632)))
REPRESENTATION_ITEM('')
SURFACE()
);
#3987=(
BOUNDED_SURFACE()
B_SPLINE_SURFACE(3,2,((#446513,#446514,#446515),(#446516,#446517,#446518),
(#446519,#446520,#446521),(#446522,#446523,#446524)),.UNSPECIFIED.,.F.,
 .F.,.F.)
B_SPLINE_SURFACE_WITH_KNOTS((4,4),(3,3),(-5.2235835674927E-6,5.74594192424276E-5),
(-0.00127120052072291,1.),.UNSPECIFIED.)
GEOMETRIC_REPRESENTATION_ITEM()
RATIONAL_B_SPLINE_SURFACE(((1.00054449313182,0.785835073638727,1.),(1.00047707767481,
0.812351526358816,1.),(1.00044031788592,0.826810216506266,1.),(1.00044777653324,
0.823876514387224,0.999999999999999)))
REPRESENTATION_ITEM('')
SURFACE()
);
#3988=(
BOUNDED_SURFACE()
B_SPLINE_SURFACE(3,2,((#446526,#446527,#446528),(#446529,#446530,#446531),
(#446532,#446533,#446534),(#446535,#446536,#446537)),.UNSPECIFIED.,.F.,
 .F.,.F.)
B_SPLINE_SURFACE_WITH_KNOTS((4,4),(3,3),(8.13151629364128E-20,4.88747512969881E-5),
(-0.000215805215461378,1.),.UNSPECIFIED.)
GEOMETRIC_REPRESENTATION_ITEM()
RATIONAL_B_SPLINE_SURFACE(((1.00008915600337,0.793434085499749,1.),(1.0000893022499,
0.793095246303298,1.),(1.00008944684612,0.792760230720561,1.),(1.00008958984392,
0.792428918540598,1.)))
REPRESENTATION_ITEM('')
SURFACE()
);
#3989=(
BOUNDED_SURFACE()
B_SPLINE_SURFACE(3,2,((#446539,#446540,#446541),(#446542,#446543,#446544),
(#446545,#446546,#446547),(#446548,#446549,#446550),(#446551,#446552,#446553),
(#446554,#446555,#446556)),.UNSPECIFIED.,.F.,.F.,.F.)
B_SPLINE_SURFACE_WITH_KNOTS((4,2,4),(3,3),(3.3881317890172E-19,7.62675010863196E-5,
0.000152535002172639),(0.,1.02152348203084),.UNSPECIFIED.)
GEOMETRIC_REPRESENTATION_ITEM()
RATIONAL_B_SPLINE_SURFACE(((1.,0.789033595401216,1.00908146323698),(1.,
0.857071781054838,1.00615262590433),(1.,0.922087264710683,1.00335390671595),
(1.,0.922394466502394,1.00334068261146),(1.,0.857224384599003,1.00614605678505),
(1.,0.789033595401619,1.00908146323697)))
REPRESENTATION_ITEM('')
SURFACE()
);
#3990=(
BOUNDED_SURFACE()
B_SPLINE_SURFACE(3,2,((#446558,#446559,#446560),(#446561,#446562,#446563),
(#446564,#446565,#446566),(#446567,#446568,#446569)),.UNSPECIFIED.,.F.,
 .F.,.F.)
B_SPLINE_SURFACE_WITH_KNOTS((4,4),(3,3),(3.79470760369927E-19,4.88747512969887E-5),
(-0.000215489857685973,1.),.UNSPECIFIED.)
GEOMETRIC_REPRESENTATION_ITEM()
RATIONAL_B_SPLINE_SURFACE(((1.0000894588974,0.792428983985612,1.),(1.00008931610862,
0.792760296061168,1.),(1.00008917172374,0.793095311538222,1.),(1.00008902569097,
0.793434150627863,1.)))
REPRESENTATION_ITEM('')
SURFACE()
);
#3991=(
BOUNDED_SURFACE()
B_SPLINE_SURFACE(3,2,((#446571,#446572,#446573),(#446574,#446575,#446576),
(#446577,#446578,#446579),(#446580,#446581,#446582)),.UNSPECIFIED.,.F.,
 .F.,.F.)
B_SPLINE_SURFACE_WITH_KNOTS((4,4),(3,3),(-5.21974905012865E-6,5.74172395514394E-5),
(-0.00139822857779505,1.00051312364059),.UNSPECIFIED.)
GEOMETRIC_REPRESENTATION_ITEM()
RATIONAL_B_SPLINE_SURFACE(((1.00049256947259,0.823768952243974,1.00018060397847),
(1.00048448215729,0.82666242438829,1.00017763870879),(1.00052427784037,
0.812424361909337,1.00019223006918),(1.00059912365873,0.785646094632719,
1.00021967280228)))
REPRESENTATION_ITEM('')
SURFACE()
);
#3992=(
BOUNDED_SURFACE()
B_SPLINE_SURFACE(3,2,((#446586,#446587,#446588),(#446589,#446590,#446591),
(#446592,#446593,#446594),(#446595,#446596,#446597)),.UNSPECIFIED.,.F.,
 .F.,.F.)
B_SPLINE_SURFACE_WITH_KNOTS((4,4),(3,3),(3.22980774337779E-5,9.63764854872255E-5),
(-0.00154325936373564,1.01095292447558),.UNSPECIFIED.)
GEOMETRIC_REPRESENTATION_ITEM()
RATIONAL_B_SPLINE_SURFACE(((1.00023530983299,0.922925743796153,1.00168574728333),
(1.00015136166126,0.950422439594224,1.00108434699061),(1.00033574337398,
0.890029368953923,1.00240524789551),(1.00054260094221,0.822274473168319,
1.00388716464863)))
REPRESENTATION_ITEM('')
SURFACE()
);
#3993=(
BOUNDED_SURFACE()
B_SPLINE_SURFACE(3,2,((#446697,#446698,#446699),(#446700,#446701,#446702),
(#446703,#446704,#446705),(#446706,#446707,#446708)),.UNSPECIFIED.,.F.,
 .F.,.F.)
B_SPLINE_SURFACE_WITH_KNOTS((4,4),(3,3),(0.,0.000101260117256737),(0.,1.),
 .UNSPECIFIED.)
GEOMETRIC_REPRESENTATION_ITEM()
RATIONAL_B_SPLINE_SURFACE(((1.,0.796615278835172,1.),(1.,0.795896038055943,
1.),(1.,0.795193354661353,1.),(1.,0.794506193185535,1.)))
REPRESENTATION_ITEM('')
SURFACE()
);
#3994=(
BOUNDED_SURFACE()
B_SPLINE_SURFACE(3,2,((#446746,#446747,#446748),(#446749,#446750,#446751),
(#446752,#446753,#446754),(#446755,#446756,#446757),(#446758,#446759,#446760),
(#446761,#446762,#446763)),.UNSPECIFIED.,.F.,.F.,.F.)
B_SPLINE_SURFACE_WITH_KNOTS((4,2,4),(3,3),(6.7762635780344E-21,1.66936432462296E-5,
3.33872864924592E-5),(0.,1.),.UNSPECIFIED.)
GEOMETRIC_REPRESENTATION_ITEM()
RATIONAL_B_SPLINE_SURFACE(((1.,0.796615278835168,1.),(1.,0.862310524418132,
1.),(1.,0.923774472010516,1.),(1.,0.92398399320343,1.),(1.,0.862574873720948,
1.),(1.,0.796615278835173,1.)))
REPRESENTATION_ITEM('')
SURFACE()
);
#3995=(
BOUNDED_SURFACE()
B_SPLINE_SURFACE(3,2,((#446800,#446801,#446802),(#446803,#446804,#446805),
(#446806,#446807,#446808),(#446809,#446810,#446811)),.UNSPECIFIED.,.F.,
 .F.,.F.)
B_SPLINE_SURFACE_WITH_KNOTS((4,4),(3,3),(0.,0.000101244905251112),(0.,1.),
 .UNSPECIFIED.)
GEOMETRIC_REPRESENTATION_ITEM()
RATIONAL_B_SPLINE_SURFACE(((1.,0.796615278835173,1.),(1.,0.795896146109806,
1.),(1.,0.795193565796486,1.),(1.,0.794506502889902,1.)))
REPRESENTATION_ITEM('')
SURFACE()
);
#3996=(
BOUNDED_SURFACE()
B_SPLINE_SURFACE(3,2,((#446847,#446848,#446849),(#446850,#446851,#446852),
(#446853,#446854,#446855),(#446856,#446857,#446858)),.UNSPECIFIED.,.F.,
 .F.,.F.)
B_SPLINE_SURFACE_WITH_KNOTS((4,4),(3,3),(2.85968127239939E-5,9.24681548475817E-5),
(-0.00167900678653656,1.01130827127818),.UNSPECIFIED.)
GEOMETRIC_REPRESENTATION_ITEM()
RATIONAL_B_SPLINE_SURFACE(((1.00059040895217,0.822187541868281,1.00401468696655),
(1.00036527718139,0.889990093671577,1.0024838267339),(1.00016469515013,
0.950399042257933,1.0011199008251),(1.00025604273992,0.922888044286085,
1.0017410499063)))
REPRESENTATION_ITEM('')
SURFACE()
);
#3997=(
BOUNDED_SURFACE()
B_SPLINE_SURFACE(3,2,((#446862,#446863,#446864),(#446865,#446866,#446867),
(#446868,#446869,#446870),(#446871,#446872,#446873)),.UNSPECIFIED.,.F.,
 .F.,.F.)
B_SPLINE_SURFACE_WITH_KNOTS((4,4),(3,3),(-5.22358356749152E-6,5.74594192424278E-5),
(-0.00127120052060224,1.),.UNSPECIFIED.)
GEOMETRIC_REPRESENTATION_ITEM()
RATIONAL_B_SPLINE_SURFACE(((1.00054449313177,0.785835073638743,1.),(1.00047707767477,
0.812351526358862,1.),(1.00044031788588,0.826810216506264,1.),(1.0004477765332,
0.82387651438726,1.)))
REPRESENTATION_ITEM('')
SURFACE()
);
#3998=(
BOUNDED_SURFACE()
B_SPLINE_SURFACE(3,2,((#446875,#446876,#446877),(#446878,#446879,#446880),
(#446881,#446882,#446883),(#446884,#446885,#446886)),.UNSPECIFIED.,.F.,
 .F.,.F.)
B_SPLINE_SURFACE_WITH_KNOTS((4,4),(3,3),(5.42101086242752E-20,4.88747512969882E-5),
(-0.000215805215310359,1.),.UNSPECIFIED.)
GEOMETRIC_REPRESENTATION_ITEM()
RATIONAL_B_SPLINE_SURFACE(((1.00008915600331,0.793434085499782,1.),(1.00008930224984,
0.793095246303326,1.),(1.00008944684606,0.792760230720599,1.),(1.00008958984385,
0.792428918540626,1.)))
REPRESENTATION_ITEM('')
SURFACE()
);
#3999=(
BOUNDED_SURFACE()
B_SPLINE_SURFACE(3,2,((#446888,#446889,#446890),(#446891,#446892,#446893),
(#446894,#446895,#446896),(#446897,#446898,#446899),(#446900,#446901,#446902),
(#446903,#446904,#446905)),.UNSPECIFIED.,.F.,.F.,.F.)
B_SPLINE_SURFACE_WITH_KNOTS((4,2,4),(3,3),(5.42101086242752E-20,7.62675010863198E-5,
0.00015253500217264),(0.,1.02152348203056),.UNSPECIFIED.)
GEOMETRIC_REPRESENTATION_ITEM()
RATIONAL_B_SPLINE_SURFACE(((1.,0.789033595401273,1.00908146323687),(1.,
0.857071781054834,1.00615262590425),(1.,0.922087264710764,1.0033539067159),
(1.,0.922394466502349,1.00334068261142),(1.,0.857224384599092,1.00614605678497),
(1.,0.789033595401673,1.00908146323685)))
REPRESENTATION_ITEM('')
SURFACE()
);
#4000=(
BOUNDED_SURFACE()
B_SPLINE_SURFACE(3,2,((#446907,#446908,#446909),(#446910,#446911,#446912),
(#446913,#446914,#446915),(#446916,#446917,#446918)),.UNSPECIFIED.,.F.,
 .F.,.F.)
B_SPLINE_SURFACE_WITH_KNOTS((4,4),(3,3),(2.16840434497101E-19,4.88747512969882E-5),
(-0.00021548985710036,1.),.UNSPECIFIED.)
GEOMETRIC_REPRESENTATION_ITEM()
RATIONAL_B_SPLINE_SURFACE(((1.00008945889716,0.792428983985733,1.),(1.00008931610837,
0.792760296061284,1.),(1.0000891717235,0.79309531153835,1.),(1.00008902569073,
0.793434150627984,1.)))
REPRESENTATION_ITEM('')
SURFACE()
);
#4001=(
BOUNDED_SURFACE()
B_SPLINE_SURFACE(3,2,((#446920,#446921,#446922),(#446923,#446924,#446925),
(#446926,#446927,#446928),(#446929,#446930,#446931)),.UNSPECIFIED.,.F.,
 .F.,.F.)
B_SPLINE_SURFACE_WITH_KNOTS((4,4),(3,3),(-5.21974905013085E-6,5.74172395514395E-5),
(-0.00139822857727288,1.00051312364058),.UNSPECIFIED.)
GEOMETRIC_REPRESENTATION_ITEM()
RATIONAL_B_SPLINE_SURFACE(((1.0004925694724,0.823768952244077,1.00018060397846),
(1.00048448215711,0.826662424388372,1.00017763870879),(1.00052427784018,
0.812424361909439,1.00019223006918),(1.00059912365851,0.785646094632826,
1.00021967280227)))
REPRESENTATION_ITEM('')
SURFACE()
);
#4002=(
BOUNDED_SURFACE()
B_SPLINE_SURFACE(3,2,((#446935,#446936,#446937),(#446938,#446939,#446940),
(#446941,#446942,#446943),(#446944,#446945,#446946)),.UNSPECIFIED.,.F.,
 .F.,.F.)
B_SPLINE_SURFACE_WITH_KNOTS((4,4),(3,3),(3.22980774337779E-5,9.63764854872249E-5),
(-0.00154325936381161,1.01095292447546),.UNSPECIFIED.)
GEOMETRIC_REPRESENTATION_ITEM()
RATIONAL_B_SPLINE_SURFACE(((1.000235309833,0.922925743796154,1.00168574728331),
(1.00015136166126,0.950422439594223,1.0010843469906),(1.000335743374,0.890029368953939,
1.00240524789548),(1.00054260094224,0.822274473168318,1.00388716464859)))
REPRESENTATION_ITEM('')
SURFACE()
);
#4003=(
BOUNDED_SURFACE()
B_SPLINE_SURFACE(3,2,((#447046,#447047,#447048),(#447049,#447050,#447051),
(#447052,#447053,#447054),(#447055,#447056,#447057)),.UNSPECIFIED.,.F.,
 .F.,.F.)
B_SPLINE_SURFACE_WITH_KNOTS((4,4),(3,3),(0.,0.000101260117256738),(0.,1.),
 .UNSPECIFIED.)
GEOMETRIC_REPRESENTATION_ITEM()
RATIONAL_B_SPLINE_SURFACE(((1.,0.796615278835172,1.),(1.,0.795896038055937,
1.),(1.,0.795193354661345,1.),(1.,0.794506193185552,1.)))
REPRESENTATION_ITEM('')
SURFACE()
);
#4004=(
BOUNDED_SURFACE()
B_SPLINE_SURFACE(3,2,((#447095,#447096,#447097),(#447098,#447099,#447100),
(#447101,#447102,#447103),(#447104,#447105,#447106),(#447107,#447108,#447109),
(#447110,#447111,#447112)),.UNSPECIFIED.,.F.,.F.,.F.)
B_SPLINE_SURFACE_WITH_KNOTS((4,2,4),(3,3),(-2.3039296165317E-19,1.66936432462291E-5,
3.33872864924584E-5),(0.,1.),.UNSPECIFIED.)
GEOMETRIC_REPRESENTATION_ITEM()
RATIONAL_B_SPLINE_SURFACE(((1.,0.796615278835176,1.),(1.,0.862310524418132,
1.),(1.,0.923774472010524,1.),(1.,0.923983993203423,1.),(1.,0.862574873720957,
1.),(1.,0.796615278835182,1.)))
REPRESENTATION_ITEM('')
SURFACE()
);
#4005=(
BOUNDED_SURFACE()
B_SPLINE_SURFACE(3,2,((#447149,#447150,#447151),(#447152,#447153,#447154),
(#447155,#447156,#447157),(#447158,#447159,#447160)),.UNSPECIFIED.,.F.,
 .F.,.F.)
B_SPLINE_SURFACE_WITH_KNOTS((4,4),(3,3),(0.,0.000101244905251112),(0.,1.),
 .UNSPECIFIED.)
GEOMETRIC_REPRESENTATION_ITEM()
RATIONAL_B_SPLINE_SURFACE(((1.,0.796615278835172,1.),(1.,0.795896146109801,
1.),(1.,0.795193565796489,1.),(1.,0.794506502889901,1.)))
REPRESENTATION_ITEM('')
SURFACE()
);
#4006=(
BOUNDED_SURFACE()
B_SPLINE_SURFACE(3,2,((#447196,#447197,#447198),(#447199,#447200,#447201),
(#447202,#447203,#447204),(#447205,#447206,#447207)),.UNSPECIFIED.,.F.,
 .F.,.F.)
B_SPLINE_SURFACE_WITH_KNOTS((4,4),(3,3),(2.85968127239939E-5,9.24681548475818E-5),
(-0.00167900678649614,1.01130827127826),.UNSPECIFIED.)
GEOMETRIC_REPRESENTATION_ITEM()
RATIONAL_B_SPLINE_SURFACE(((1.00059040895215,0.822187541868272,1.00401468696658),
(1.00036527718139,0.889990093671571,1.00248382673392),(1.00016469515013,
0.950399042257931,1.00111990082511),(1.00025604273992,0.92288804428608,
1.00174104990632)))
REPRESENTATION_ITEM('')
SURFACE()
);
#4007=(
BOUNDED_SURFACE()
B_SPLINE_SURFACE(3,2,((#447211,#447212,#447213),(#447214,#447215,#447216),
(#447217,#447218,#447219),(#447220,#447221,#447222)),.UNSPECIFIED.,.F.,
 .F.,.F.)
B_SPLINE_SURFACE_WITH_KNOTS((4,4),(3,3),(-5.22358356749255E-6,5.74594192424278E-5),
(-0.00127120052063573,1.),.UNSPECIFIED.)
GEOMETRIC_REPRESENTATION_ITEM()
RATIONAL_B_SPLINE_SURFACE(((1.00054449313178,0.785835073638738,1.),(1.00047707767478,
0.812351526358855,1.),(1.00044031788589,0.826810216506258,1.),(1.00044777653321,
0.823876514387244,1.)))
REPRESENTATION_ITEM('')
SURFACE()
);
#4008=(
BOUNDED_SURFACE()
B_SPLINE_SURFACE(3,2,((#447224,#447225,#447226),(#447227,#447228,#447229),
(#447230,#447231,#447232),(#447233,#447234,#447235)),.UNSPECIFIED.,.F.,
 .F.,.F.)
B_SPLINE_SURFACE_WITH_KNOTS((4,4),(3,3),(2.71050543121376E-20,4.88747512969881E-5),
(-0.000215805215194671,1.),.UNSPECIFIED.)
GEOMETRIC_REPRESENTATION_ITEM()
RATIONAL_B_SPLINE_SURFACE(((1.00008915600326,0.793434085499798,1.),(1.00008930224979,
0.793095246303346,1.),(1.00008944684601,0.792760230720619,1.),(1.0000895898438,
0.792428918540652,1.)))
REPRESENTATION_ITEM('')
SURFACE()
);
#4009=(
BOUNDED_SURFACE()
B_SPLINE_SURFACE(3,2,((#447237,#447238,#447239),(#447240,#447241,#447242),
(#447243,#447244,#447245),(#447246,#447247,#447248),(#447249,#447250,#447251),
(#447252,#447253,#447254)),.UNSPECIFIED.,.F.,.F.,.F.)
B_SPLINE_SURFACE_WITH_KNOTS((4,2,4),(3,3),(5.21772295508649E-19,7.62675010863198E-5,
0.000152535002172639),(0.,1.02152348203077),.UNSPECIFIED.)
GEOMETRIC_REPRESENTATION_ITEM()
RATIONAL_B_SPLINE_SURFACE(((1.,0.789033595401235,1.00908146323695),(1.,
0.857071781054861,1.00615262590431),(1.,0.92208726471068,1.00335390671594),
(1.,0.922394466502408,1.00334068261145),(1.,0.85722438459901,1.00614605678503),
(1.,0.789033595401628,1.00908146323694)))
REPRESENTATION_ITEM('')
SURFACE()
);
#4010=(
BOUNDED_SURFACE()
B_SPLINE_SURFACE(3,2,((#447256,#447257,#447258),(#447259,#447260,#447261),
(#447262,#447263,#447264),(#447265,#447266,#447267)),.UNSPECIFIED.,.F.,
 .F.,.F.)
B_SPLINE_SURFACE_WITH_KNOTS((4,4),(3,3),(2.16840434497101E-19,4.88747512969882E-5),
(-0.000215489857075741,1.),.UNSPECIFIED.)
GEOMETRIC_REPRESENTATION_ITEM()
RATIONAL_B_SPLINE_SURFACE(((1.00008945889715,0.792428983985742,1.),(1.00008931610836,
0.792760296061281,1.),(1.00008917172349,0.793095311538358,1.),(1.00008902569072,
0.793434150627989,1.)))
REPRESENTATION_ITEM('')
SURFACE()
);
#4011=(
BOUNDED_SURFACE()
B_SPLINE_SURFACE(3,2,((#447269,#447270,#447271),(#447272,#447273,#447274),
(#447275,#447276,#447277),(#447278,#447279,#447280)),.UNSPECIFIED.,.F.,
 .F.,.F.)
B_SPLINE_SURFACE_WITH_KNOTS((4,4),(3,3),(-5.2197490501309E-6,5.74172395514397E-5),
(-0.00139822857767823,1.00051312364072),.UNSPECIFIED.)
GEOMETRIC_REPRESENTATION_ITEM()
RATIONAL_B_SPLINE_SURFACE(((1.00049256947254,0.823768952243982,1.00018060397851),
(1.00048448215725,0.826662424388278,1.00017763870884),(1.00052427784033,
0.812424361909341,1.00019223006923),(1.00059912365868,0.785646094632709,
1.00021967280233)))
REPRESENTATION_ITEM('')
SURFACE()
);
#4012=(
BOUNDED_SURFACE()
B_SPLINE_SURFACE(3,2,((#447284,#447285,#447286),(#447287,#447288,#447289),
(#447290,#447291,#447292),(#447293,#447294,#447295)),.UNSPECIFIED.,.F.,
 .F.,.F.)
B_SPLINE_SURFACE_WITH_KNOTS((4,4),(3,3),(3.22980774337779E-5,9.63764854872255E-5),
(-0.00154325936377236,1.01095292447541),.UNSPECIFIED.)
GEOMETRIC_REPRESENTATION_ITEM()
RATIONAL_B_SPLINE_SURFACE(((1.00023530983299,0.922925743796161,1.00168574728331),
(1.00015136166126,0.950422439594217,1.0010843469906),(1.00033574337399,
0.890029368953947,1.00240524789547),(1.00054260094223,0.822274473168337,
1.00388716464857)))
REPRESENTATION_ITEM('')
SURFACE()
);
#4013=(
BOUNDED_SURFACE()
B_SPLINE_SURFACE(3,2,((#447395,#447396,#447397),(#447398,#447399,#447400),
(#447401,#447402,#447403),(#447404,#447405,#447406)),.UNSPECIFIED.,.F.,
 .F.,.F.)
B_SPLINE_SURFACE_WITH_KNOTS((4,4),(3,3),(0.,0.000101260117256738),(0.,1.),
 .UNSPECIFIED.)
GEOMETRIC_REPRESENTATION_ITEM()
RATIONAL_B_SPLINE_SURFACE(((1.,0.796615278835173,1.),(1.,0.795896038055938,
1.),(1.,0.795193354661348,1.),(1.,0.794506193185554,1.)))
REPRESENTATION_ITEM('')
SURFACE()
);
#4014=(
BOUNDED_SURFACE()
B_SPLINE_SURFACE(3,2,((#447444,#447445,#447446),(#447447,#447448,#447449),
(#447450,#447451,#447452),(#447453,#447454,#447455),(#447456,#447457,#447458),
(#447459,#447460,#447461)),.UNSPECIFIED.,.F.,.F.,.F.)
B_SPLINE_SURFACE_WITH_KNOTS((4,2,4),(3,3),(1.18584612615602E-20,1.66936432462294E-5,
3.33872864924588E-5),(0.,1.),.UNSPECIFIED.)
GEOMETRIC_REPRESENTATION_ITEM()
RATIONAL_B_SPLINE_SURFACE(((1.,0.796615278835176,1.),(1.,0.862310524418132,
1.),(1.,0.923774472010525,1.),(1.,0.923983993203423,1.),(1.,0.862574873720945,
1.),(1.,0.796615278835186,1.)))
REPRESENTATION_ITEM('')
SURFACE()
);
#4015=(
BOUNDED_SURFACE()
B_SPLINE_SURFACE(3,2,((#447498,#447499,#447500),(#447501,#447502,#447503),
(#447504,#447505,#447506),(#447507,#447508,#447509)),.UNSPECIFIED.,.F.,
 .F.,.F.)
B_SPLINE_SURFACE_WITH_KNOTS((4,4),(3,3),(-2.16840434497101E-19,0.000101244905251112),
(0.,1.),.UNSPECIFIED.)
GEOMETRIC_REPRESENTATION_ITEM()
RATIONAL_B_SPLINE_SURFACE(((1.,0.796615278835172,1.),(1.,0.795896146109798,
1.),(1.,0.795193565796494,1.),(1.,0.794506502889905,1.)))
REPRESENTATION_ITEM('')
SURFACE()
);
#4016=(
BOUNDED_SURFACE()
B_SPLINE_SURFACE(3,2,((#447545,#447546,#447547),(#447548,#447549,#447550),
(#447551,#447552,#447553),(#447554,#447555,#447556)),.UNSPECIFIED.,.F.,
 .F.,.F.)
B_SPLINE_SURFACE_WITH_KNOTS((4,4),(3,3),(2.85968127239939E-5,9.24681548475818E-5),
(-0.00167900678790481,1.01130827127829),.UNSPECIFIED.)
GEOMETRIC_REPRESENTATION_ITEM()
RATIONAL_B_SPLINE_SURFACE(((1.00059040895265,0.822187541868015,1.00401468696659),
(1.00036527718169,0.889990093671412,1.00248382673393),(1.00016469515026,
0.950399042257863,1.00111990082512),(1.00025604274013,0.922888044285965,
1.00174104990632)))
REPRESENTATION_ITEM('')
SURFACE()
);
#4017=(
BOUNDED_SURFACE()
B_SPLINE_SURFACE(3,2,((#447560,#447561,#447562),(#447563,#447564,#447565),
(#447566,#447567,#447568),(#447569,#447570,#447571)),.UNSPECIFIED.,.F.,
 .F.,.F.)
B_SPLINE_SURFACE_WITH_KNOTS((4,4),(3,3),(-5.22358356749333E-6,5.74594192424277E-5),
(-0.00127120052062949,1.),.UNSPECIFIED.)
GEOMETRIC_REPRESENTATION_ITEM()
RATIONAL_B_SPLINE_SURFACE(((1.00054449313178,0.785835073638757,1.),(1.00047707767478,
0.812351526358823,1.),(1.00044031788589,0.826810216506297,1.),(1.00044777653321,
0.823876514387231,1.)))
REPRESENTATION_ITEM('')
SURFACE()
);
#4018=(
BOUNDED_SURFACE()
B_SPLINE_SURFACE(3,2,((#447573,#447574,#447575),(#447576,#447577,#447578),
(#447579,#447580,#447581),(#447582,#447583,#447584)),.UNSPECIFIED.,.F.,
 .F.,.F.)
B_SPLINE_SURFACE_WITH_KNOTS((4,4),(3,3),(-2.98155597433514E-19,4.88747512969879E-5),
(-0.000215805215320105,1.),.UNSPECIFIED.)
GEOMETRIC_REPRESENTATION_ITEM()
RATIONAL_B_SPLINE_SURFACE(((1.00008915600331,0.793434085499779,1.),(1.00008930224984,
0.79309524630333,1.),(1.00008944684606,0.792760230720593,1.),(1.00008958984386,
0.792428918540629,1.)))
REPRESENTATION_ITEM('')
SURFACE()
);
#4019=(
BOUNDED_SURFACE()
B_SPLINE_SURFACE(3,2,((#447586,#447587,#447588),(#447589,#447590,#447591),
(#447592,#447593,#447594),(#447595,#447596,#447597),(#447598,#447599,#447600),
(#447601,#447602,#447603)),.UNSPECIFIED.,.F.,.F.,.F.)
B_SPLINE_SURFACE_WITH_KNOTS((4,2,4),(3,3),(2.91379333855479E-19,7.62675010863198E-5,
0.000152535002172639),(0.,1.02152348203072),.UNSPECIFIED.)
GEOMETRIC_REPRESENTATION_ITEM()
RATIONAL_B_SPLINE_SURFACE(((1.,0.789033595401243,1.00908146323693),(1.,
0.857071781054836,1.0061526259043),(1.,0.922087264710717,1.00335390671593),
(1.,0.922394466502379,1.00334068261144),(1.,0.857224384599041,1.00614605678501),
(1.,0.78903359540164,1.00908146323692)))
REPRESENTATION_ITEM('')
SURFACE()
);
#4020=(
BOUNDED_SURFACE()
B_SPLINE_SURFACE(3,2,((#447605,#447606,#447607),(#447608,#447609,#447610),
(#447611,#447612,#447613),(#447614,#447615,#447616)),.UNSPECIFIED.,.F.,
 .F.,.F.)
B_SPLINE_SURFACE_WITH_KNOTS((4,4),(3,3),(3.79470760369927E-19,4.88747512969886E-5),
(-0.000215489857667756,1.),.UNSPECIFIED.)
GEOMETRIC_REPRESENTATION_ITEM()
RATIONAL_B_SPLINE_SURFACE(((1.00008945889739,0.792428983985614,1.),(1.00008931610861,
0.79276029606116,1.),(1.00008917172374,0.793095311538243,1.),(1.00008902569096,
0.793434150627865,1.)))
REPRESENTATION_ITEM('')
SURFACE()
);
#4021=(
BOUNDED_SURFACE()
B_SPLINE_SURFACE(3,2,((#447618,#447619,#447620),(#447621,#447622,#447623),
(#447624,#447625,#447626),(#447627,#447628,#447629)),.UNSPECIFIED.,.F.,
 .F.,.F.)
B_SPLINE_SURFACE_WITH_KNOTS((4,4),(3,3),(-5.21974905013081E-6,5.74172395514399E-5),
(-0.00139822857725879,1.00051312364054),.UNSPECIFIED.)
GEOMETRIC_REPRESENTATION_ITEM()
RATIONAL_B_SPLINE_SURFACE(((1.0004925694724,0.823768952244095,1.00018060397845),
(1.0004844821571,0.826662424388373,1.00017763870878),(1.00052427784017,
0.812424361909455,1.00019223006916),(1.0005991236585,0.785646094632837,
1.00021967280225)))
REPRESENTATION_ITEM('')
SURFACE()
);
#4022=(
BOUNDED_SURFACE()
B_SPLINE_SURFACE(3,2,((#447633,#447634,#447635),(#447636,#447637,#447638),
(#447639,#447640,#447641),(#447642,#447643,#447644)),.UNSPECIFIED.,.F.,
 .F.,.F.)
B_SPLINE_SURFACE_WITH_KNOTS((4,4),(3,3),(3.22980774337778E-5,9.63764854872249E-5),
(-0.0015432593637765,1.01095292447533),.UNSPECIFIED.)
GEOMETRIC_REPRESENTATION_ITEM()
RATIONAL_B_SPLINE_SURFACE(((1.000235309833,0.922925743796168,1.00168574728329),
(1.00015136166126,0.950422439594216,1.00108434699059),(1.00033574337399,
0.890029368953968,1.00240524789545),(1.00054260094223,0.822274473168339,
1.00388716464855)))
REPRESENTATION_ITEM('')
SURFACE()
);
#4023=(
BOUNDED_SURFACE()
B_SPLINE_SURFACE(3,2,((#447744,#447745,#447746),(#447747,#447748,#447749),
(#447750,#447751,#447752),(#447753,#447754,#447755)),.UNSPECIFIED.,.F.,
 .F.,.F.)
B_SPLINE_SURFACE_WITH_KNOTS((4,4),(3,3),(-2.16840434497101E-19,0.000101260117256738),
(0.,1.),.UNSPECIFIED.)
GEOMETRIC_REPRESENTATION_ITEM()
RATIONAL_B_SPLINE_SURFACE(((1.,0.79661527883517,1.),(1.,0.795896038055935,
1.),(1.,0.795193354661348,1.),(1.,0.794506193185538,1.)))
REPRESENTATION_ITEM('')
SURFACE()
);
#4024=(
BOUNDED_SURFACE()
B_SPLINE_SURFACE(3,2,((#447793,#447794,#447795),(#447796,#447797,#447798),
(#447799,#447800,#447801),(#447802,#447803,#447804),(#447805,#447806,#447807),
(#447808,#447809,#447810)),.UNSPECIFIED.,.F.,.F.,.F.)
B_SPLINE_SURFACE_WITH_KNOTS((4,2,4),(3,3),(-2.3039296165317E-19,1.66936432462292E-5,
3.33872864924587E-5),(0.,1.),.UNSPECIFIED.)
GEOMETRIC_REPRESENTATION_ITEM()
RATIONAL_B_SPLINE_SURFACE(((1.,0.79661527883517,1.),(1.,0.862310524418134,
1.),(1.,0.923774472010517,1.),(1.,0.923983993203428,1.),(1.,0.862574873720944,
1.),(1.,0.796615278835184,1.)))
REPRESENTATION_ITEM('')
SURFACE()
);
#4025=(
BOUNDED_SURFACE()
B_SPLINE_SURFACE(3,2,((#447847,#447848,#447849),(#447850,#447851,#447852),
(#447853,#447854,#447855),(#447856,#447857,#447858)),.UNSPECIFIED.,.F.,
 .F.,.F.)
B_SPLINE_SURFACE_WITH_KNOTS((4,4),(3,3),(0.,0.000101244905251112),(0.,1.),
 .UNSPECIFIED.)
GEOMETRIC_REPRESENTATION_ITEM()
RATIONAL_B_SPLINE_SURFACE(((1.,0.79661527883517,1.),(1.,0.795896146109801,
1.),(1.,0.795193565796499,1.),(1.,0.794506502889901,1.)))
REPRESENTATION_ITEM('')
SURFACE()
);
#4026=(
BOUNDED_SURFACE()
B_SPLINE_SURFACE(3,2,((#447894,#447895,#447896),(#447897,#447898,#447899),
(#447900,#447901,#447902),(#447903,#447904,#447905)),.UNSPECIFIED.,.F.,
 .F.,.F.)
B_SPLINE_SURFACE_WITH_KNOTS((4,4),(3,3),(2.85968127239939E-5,9.24681548475816E-5),
(-0.0016790067878601,1.01130827127821),.UNSPECIFIED.)
GEOMETRIC_REPRESENTATION_ITEM()
RATIONAL_B_SPLINE_SURFACE(((1.00059040895263,0.822187541868038,1.00401468696656),
(1.00036527718168,0.889990093671423,1.00248382673391),(1.00016469515026,
0.950399042257866,1.00111990082511),(1.00025604274013,0.922888044285977,
1.00174104990631)))
REPRESENTATION_ITEM('')
SURFACE()
);
#4027=(
BOUNDED_SURFACE()
B_SPLINE_SURFACE(3,2,((#447909,#447910,#447911),(#447912,#447913,#447914),
(#447915,#447916,#447917),(#447918,#447919,#447920)),.UNSPECIFIED.,.F.,
 .F.,.F.)
B_SPLINE_SURFACE_WITH_KNOTS((4,4),(3,3),(-5.22358356749301E-6,5.74594192424277E-5),
(-0.00127120052063902,1.),.UNSPECIFIED.)
GEOMETRIC_REPRESENTATION_ITEM()
RATIONAL_B_SPLINE_SURFACE(((1.00054449313179,0.785835073638746,1.),(1.00047707767478,
0.812351526358838,1.),(1.00044031788589,0.826810216506265,1.),(1.00044777653322,
0.823876514387241,1.)))
REPRESENTATION_ITEM('')
SURFACE()
);
#4028=(
BOUNDED_SURFACE()
B_SPLINE_SURFACE(3,2,((#447922,#447923,#447924),(#447925,#447926,#447927),
(#447928,#447929,#447930),(#447931,#447932,#447933)),.UNSPECIFIED.,.F.,
 .F.,.F.)
B_SPLINE_SURFACE_WITH_KNOTS((4,4),(3,3),(-2.71050543121376E-20,4.88747512969879E-5),
(-0.000215805215354959,1.),.UNSPECIFIED.)
GEOMETRIC_REPRESENTATION_ITEM()
RATIONAL_B_SPLINE_SURFACE(((1.00008915600333,0.793434085499769,1.),(1.00008930224986,
0.793095246303308,1.),(1.00008944684608,0.792760230720586,1.),(1.00008958984387,
0.792428918540619,1.)))
REPRESENTATION_ITEM('')
SURFACE()
);
#4029=(
BOUNDED_SURFACE()
B_SPLINE_SURFACE(3,2,((#447935,#447936,#447937),(#447938,#447939,#447940),
(#447941,#447942,#447943),(#447944,#447945,#447946),(#447947,#447948,#447949),
(#447950,#447951,#447952)),.UNSPECIFIED.,.F.,.F.,.F.)
B_SPLINE_SURFACE_WITH_KNOTS((4,2,4),(3,3),(4.74338450462408E-20,7.62675010863196E-5,
0.000152535002172639),(0.,1.02152348203074),.UNSPECIFIED.)
GEOMETRIC_REPRESENTATION_ITEM()
RATIONAL_B_SPLINE_SURFACE(((1.,0.78903359540124,1.00908146323694),(1.,0.857071781054833,
1.0061526259043),(1.,0.922087264710719,1.00335390671593),(1.,0.922394466502377,
1.00334068261144),(1.,0.857224384599036,1.00614605678502),(1.,0.789033595401636,
1.00908146323692)))
REPRESENTATION_ITEM('')
SURFACE()
);
#4030=(
BOUNDED_SURFACE()
B_SPLINE_SURFACE(3,2,((#447954,#447955,#447956),(#447957,#447958,#447959),
(#447960,#447961,#447962),(#447963,#447964,#447965)),.UNSPECIFIED.,.F.,
 .F.,.F.)
B_SPLINE_SURFACE_WITH_KNOTS((4,4),(3,3),(-1.0842021724855E-19,4.88747512969881E-5),
(-0.000215489857626116,1.),.UNSPECIFIED.)
GEOMETRIC_REPRESENTATION_ITEM()
RATIONAL_B_SPLINE_SURFACE(((1.00008945889738,0.792428983985623,1.),(1.00008931610859,
0.792760296061174,1.),(1.00008917172372,0.793095311538236,1.),(1.00008902569094,
0.793434150627873,1.)))
REPRESENTATION_ITEM('')
SURFACE()
);
#4031=(
BOUNDED_SURFACE()
B_SPLINE_SURFACE(3,2,((#447967,#447968,#447969),(#447970,#447971,#447972),
(#447973,#447974,#447975),(#447976,#447977,#447978)),.UNSPECIFIED.,.F.,
 .F.,.F.)
B_SPLINE_SURFACE_WITH_KNOTS((4,4),(3,3),(-5.21974905012888E-6,5.7417239551441E-5),
(-0.00139822857724751,1.00051312364062),.UNSPECIFIED.)
GEOMETRIC_REPRESENTATION_ITEM()
RATIONAL_B_SPLINE_SURFACE(((1.00049256947239,0.823768952244076,1.00018060397848),
(1.0004844821571,0.82666242438836,1.0001776387088),(1.00052427784017,0.812424361909453,
1.00019223006919),(1.0005991236585,0.785646094632817,1.00021967280229)))
REPRESENTATION_ITEM('')
SURFACE()
);
#4032=(
BOUNDED_SURFACE()
B_SPLINE_SURFACE(3,2,((#447982,#447983,#447984),(#447985,#447986,#447987),
(#447988,#447989,#447990),(#447991,#447992,#447993)),.UNSPECIFIED.,.F.,
 .F.,.F.)
B_SPLINE_SURFACE_WITH_KNOTS((4,4),(3,3),(3.22980774337779E-5,9.63764854872253E-5),
(-0.00154325936389752,1.01095292447534),.UNSPECIFIED.)
GEOMETRIC_REPRESENTATION_ITEM()
RATIONAL_B_SPLINE_SURFACE(((1.00023530983301,0.922925743796159,1.0016857472833),
(1.00015136166127,0.950422439594206,1.00108434699059),(1.00033574337402,
0.890029368953955,1.00240524789546),(1.00054260094227,0.822274473168315,
1.00388716464855)))
REPRESENTATION_ITEM('')
SURFACE()
);
#4033=(
BOUNDED_SURFACE()
B_SPLINE_SURFACE(3,2,((#448093,#448094,#448095),(#448096,#448097,#448098),
(#448099,#448100,#448101),(#448102,#448103,#448104)),.UNSPECIFIED.,.F.,
 .F.,.F.)
B_SPLINE_SURFACE_WITH_KNOTS((4,4),(3,3),(-2.16840434497101E-19,0.000101260117256738),
(0.,1.),.UNSPECIFIED.)
GEOMETRIC_REPRESENTATION_ITEM()
RATIONAL_B_SPLINE_SURFACE(((1.,0.796615278835172,1.),(1.,0.79589603805594,
1.),(1.,0.79519335466135,1.),(1.,0.794506193185548,1.)))
REPRESENTATION_ITEM('')
SURFACE()
);
#4034=(
BOUNDED_SURFACE()
B_SPLINE_SURFACE(3,2,((#448142,#448143,#448144),(#448145,#448146,#448147),
(#448148,#448149,#448150),(#448151,#448152,#448153),(#448154,#448155,#448156),
(#448157,#448158,#448159)),.UNSPECIFIED.,.F.,.F.,.F.)
B_SPLINE_SURFACE_WITH_KNOTS((4,2,4),(3,3),(-8.63973606199386E-20,1.66936432462294E-5,
3.33872864924588E-5),(0.,1.),.UNSPECIFIED.)
GEOMETRIC_REPRESENTATION_ITEM()
RATIONAL_B_SPLINE_SURFACE(((1.,0.796615278835177,1.),(1.,0.862310524418125,
1.),(1.,0.923774472010521,1.),(1.,0.923983993203424,1.),(1.,0.86257487372095,
1.),(1.,0.796615278835179,1.)))
REPRESENTATION_ITEM('')
SURFACE()
);
#4035=(
BOUNDED_SURFACE()
B_SPLINE_SURFACE(3,2,((#448196,#448197,#448198),(#448199,#448200,#448201),
(#448202,#448203,#448204),(#448205,#448206,#448207)),.UNSPECIFIED.,.F.,
 .F.,.F.)
B_SPLINE_SURFACE_WITH_KNOTS((4,4),(3,3),(-2.16840434497101E-19,0.000101244905251112),
(0.,1.),.UNSPECIFIED.)
GEOMETRIC_REPRESENTATION_ITEM()
RATIONAL_B_SPLINE_SURFACE(((1.,0.796615278835169,1.),(1.,0.795896146109794,
1.),(1.,0.795193565796499,1.),(1.,0.794506502889899,1.)))
REPRESENTATION_ITEM('')
SURFACE()
);
#4036=(
BOUNDED_SURFACE()
B_SPLINE_SURFACE(3,2,((#448243,#448244,#448245),(#448246,#448247,#448248),
(#448249,#448250,#448251),(#448252,#448253,#448254)),.UNSPECIFIED.,.F.,
 .F.,.F.)
B_SPLINE_SURFACE_WITH_KNOTS((4,4),(3,3),(2.85968127239939E-5,9.24681548475818E-5),
(-0.00167900678733353,1.01130827127828),.UNSPECIFIED.)
GEOMETRIC_REPRESENTATION_ITEM()
RATIONAL_B_SPLINE_SURFACE(((1.00059040895245,0.82218754186812,1.00401468696659),
(1.00036527718157,0.889990093671481,1.00248382673392),(1.00016469515021,
0.950399042257883,1.00111990082511),(1.00025604274004,0.922888044286016,
1.00174104990632)))
REPRESENTATION_ITEM('')
SURFACE()
);
#4037=(
BOUNDED_SURFACE()
B_SPLINE_SURFACE(3,2,((#448258,#448259,#448260),(#448261,#448262,#448263),
(#448264,#448265,#448266),(#448267,#448268,#448269)),.UNSPECIFIED.,.F.,
 .F.,.F.)
B_SPLINE_SURFACE_WITH_KNOTS((4,4),(3,3),(-5.22358356749328E-6,5.74594192424278E-5),
(-0.00127120052054192,1.),.UNSPECIFIED.)
GEOMETRIC_REPRESENTATION_ITEM()
RATIONAL_B_SPLINE_SURFACE(((1.00054449313174,0.785835073638759,1.),(1.00047707767474,
0.812351526358873,1.),(1.00044031788586,0.826810216506272,1.),(1.00044777653318,
0.823876514387262,1.)))
REPRESENTATION_ITEM('')
SURFACE()
);
#4038=(
BOUNDED_SURFACE()
B_SPLINE_SURFACE(3,2,((#448271,#448272,#448273),(#448274,#448275,#448276),
(#448277,#448278,#448279),(#448280,#448281,#448282)),.UNSPECIFIED.,.F.,
 .F.,.F.)
B_SPLINE_SURFACE_WITH_KNOTS((4,4),(3,3),(1.89735380184963E-19,4.88747512969881E-5),
(-0.000215805215098437,1.),.UNSPECIFIED.)
GEOMETRIC_REPRESENTATION_ITEM()
RATIONAL_B_SPLINE_SURFACE(((1.00008915600322,0.793434085499826,1.),(1.00008930224975,
0.793095246303361,1.),(1.00008944684597,0.792760230720644,1.),(1.00008958984376,
0.792428918540672,1.)))
REPRESENTATION_ITEM('')
SURFACE()
);
#4039=(
BOUNDED_SURFACE()
B_SPLINE_SURFACE(3,2,((#448284,#448285,#448286),(#448287,#448288,#448289),
(#448290,#448291,#448292),(#448293,#448294,#448295),(#448296,#448297,#448298),
(#448299,#448300,#448301)),.UNSPECIFIED.,.F.,.F.,.F.)
B_SPLINE_SURFACE_WITH_KNOTS((4,2,4),(3,3),(3.65918233213858E-19,7.626750108632E-5,
0.00015253500217264),(0.,1.0215234820306),.UNSPECIFIED.)
GEOMETRIC_REPRESENTATION_ITEM()
RATIONAL_B_SPLINE_SURFACE(((1.,0.789033595401266,1.00908146323688),(1.,
0.857071781054849,1.00615262590426),(1.,0.922087264710724,1.00335390671591),
(1.,0.922394466502391,1.00334068261142),(1.,0.857224384599052,1.00614605678498),
(1.,0.789033595401665,1.00908146323687)))
REPRESENTATION_ITEM('')
SURFACE()
);
#4040=(
BOUNDED_SURFACE()
B_SPLINE_SURFACE(3,2,((#448303,#448304,#448305),(#448306,#448307,#448308),
(#448309,#448310,#448311),(#448312,#448313,#448314)),.UNSPECIFIED.,.F.,
 .F.,.F.)
B_SPLINE_SURFACE_WITH_KNOTS((4,4),(3,3),(3.52365706057789E-19,4.88747512969885E-5),
(-0.000215489857907747,1.),.UNSPECIFIED.)
GEOMETRIC_REPRESENTATION_ITEM()
RATIONAL_B_SPLINE_SURFACE(((1.00008945889749,0.792428983985561,1.),(1.00008931610871,
0.792760296061118,1.),(1.00008917172383,0.793095311538185,1.),(1.00008902569106,
0.793434150627815,1.)))
REPRESENTATION_ITEM('')
SURFACE()
);
#4041=(
BOUNDED_SURFACE()
B_SPLINE_SURFACE(3,2,((#448316,#448317,#448318),(#448319,#448320,#448321),
(#448322,#448323,#448324),(#448325,#448326,#448327)),.UNSPECIFIED.,.F.,
 .F.,.F.)
B_SPLINE_SURFACE_WITH_KNOTS((4,4),(3,3),(-5.219749050131E-6,5.74172395514409E-5),
(-0.00139822857747908,1.00051312364054),.UNSPECIFIED.)
GEOMETRIC_REPRESENTATION_ITEM()
RATIONAL_B_SPLINE_SURFACE(((1.00049256947247,0.823768952244047,1.00018060397845),
(1.00048448215718,0.826662424388334,1.00017763870878),(1.00052427784026,
0.812424361909417,1.00019223006916),(1.0005991236586,0.785646094632787,
1.00021967280225)))
REPRESENTATION_ITEM('')
SURFACE()
);
#4042=(
BOUNDED_SURFACE()
B_SPLINE_SURFACE(3,2,((#448331,#448332,#448333),(#448334,#448335,#448336),
(#448337,#448338,#448339),(#448340,#448341,#448342)),.UNSPECIFIED.,.F.,
 .F.,.F.)
B_SPLINE_SURFACE_WITH_KNOTS((4,4),(3,3),(3.22980774337781E-5,9.63764854872256E-5),
(-0.00154325936487747,1.01095292447528),.UNSPECIFIED.)
GEOMETRIC_REPRESENTATION_ITEM()
RATIONAL_B_SPLINE_SURFACE(((1.00023530983316,0.92292574379609,1.00168574728329),
(1.00015136166137,0.950422439594164,1.00108434699058),(1.00033574337423,
0.890029368953841,1.00240524789544),(1.00054260094262,0.822274473168158,
1.00388716464853)))
REPRESENTATION_ITEM('')
SURFACE()
);
#4043=(
BOUNDED_SURFACE()
B_SPLINE_SURFACE(3,2,((#448442,#448443,#448444),(#448445,#448446,#448447),
(#448448,#448449,#448450),(#448451,#448452,#448453)),.UNSPECIFIED.,.F.,
 .F.,.F.)
B_SPLINE_SURFACE_WITH_KNOTS((4,4),(3,3),(0.,0.000101260117256738),(0.,1.),
 .UNSPECIFIED.)
GEOMETRIC_REPRESENTATION_ITEM()
RATIONAL_B_SPLINE_SURFACE(((1.,0.796615278835173,1.),(1.,0.795896038055939,
1.),(1.,0.795193354661348,1.),(1.,0.794506193185548,1.)))
REPRESENTATION_ITEM('')
SURFACE()
);
#4044=(
BOUNDED_SURFACE()
B_SPLINE_SURFACE(3,2,((#448491,#448492,#448493),(#448494,#448495,#448496),
(#448497,#448498,#448499),(#448500,#448501,#448502),(#448503,#448504,#448505),
(#448506,#448507,#448508)),.UNSPECIFIED.,.F.,.F.,.F.)
B_SPLINE_SURFACE_WITH_KNOTS((4,2,4),(3,3),(-1.10114283143059E-19,1.66936432462296E-5,
3.33872864924593E-5),(0.,1.),.UNSPECIFIED.)
GEOMETRIC_REPRESENTATION_ITEM()
RATIONAL_B_SPLINE_SURFACE(((1.,0.796615278835173,1.),(1.,0.862310524418128,
1.),(1.,0.923774472010522,1.),(1.,0.923983993203426,1.),(1.,0.862574873720947,
1.),(1.,0.796615278835177,1.)))
REPRESENTATION_ITEM('')
SURFACE()
);
#4045=(
BOUNDED_SURFACE()
B_SPLINE_SURFACE(3,2,((#448545,#448546,#448547),(#448548,#448549,#448550),
(#448551,#448552,#448553),(#448554,#448555,#448556)),.UNSPECIFIED.,.F.,
 .F.,.F.)
B_SPLINE_SURFACE_WITH_KNOTS((4,4),(3,3),(0.,0.000101244905251112),(0.,1.),
 .UNSPECIFIED.)
GEOMETRIC_REPRESENTATION_ITEM()
RATIONAL_B_SPLINE_SURFACE(((1.,0.796615278835173,1.),(1.,0.795896146109793,
1.),(1.,0.795193565796502,1.),(1.,0.794506502889902,1.)))
REPRESENTATION_ITEM('')
SURFACE()
);
#4046=(
BOUNDED_SURFACE()
B_SPLINE_SURFACE(3,2,((#448592,#448593,#448594),(#448595,#448596,#448597),
(#448598,#448599,#448600),(#448601,#448602,#448603)),.UNSPECIFIED.,.F.,
 .F.,.F.)
B_SPLINE_SURFACE_WITH_KNOTS((4,4),(3,3),(2.85968127239938E-5,9.24681548475818E-5),
(-0.00167900678711253,1.01130827127809),.UNSPECIFIED.)
GEOMETRIC_REPRESENTATION_ITEM()
RATIONAL_B_SPLINE_SURFACE(((1.00059040895237,0.822187541868192,1.00401468696652),
(1.00036527718152,0.889990093671527,1.00248382673388),(1.00016469515019,
0.950399042257907,1.00111990082509),(1.00025604274001,0.922888044286047,
1.00174104990629)))
REPRESENTATION_ITEM('')
SURFACE()
);
#4047=(
BOUNDED_SURFACE()
B_SPLINE_SURFACE(3,2,((#448607,#448608,#448609),(#448610,#448611,#448612),
(#448613,#448614,#448615),(#448616,#448617,#448618)),.UNSPECIFIED.,.F.,
 .F.,.F.)
B_SPLINE_SURFACE_WITH_KNOTS((4,4),(3,3),(-5.22358356749311E-6,5.74594192424278E-5),
(-0.00127120052062198,1.),.UNSPECIFIED.)
GEOMETRIC_REPRESENTATION_ITEM()
RATIONAL_B_SPLINE_SURFACE(((1.00054449313178,0.785835073638755,1.),(1.00047707767477,
0.812351526358825,1.),(1.00044031788589,0.826810216506286,1.),(1.00044777653321,
0.82387651438724,1.)))
REPRESENTATION_ITEM('')
SURFACE()
);
#4048=(
BOUNDED_SURFACE()
B_SPLINE_SURFACE(3,2,((#448620,#448621,#448622),(#448623,#448624,#448625),
(#448626,#448627,#448628),(#448629,#448630,#448631)),.UNSPECIFIED.,.F.,
 .F.,.F.)
B_SPLINE_SURFACE_WITH_KNOTS((4,4),(3,3),(-1.89735380184963E-19,4.88747512969879E-5),
(-0.000215805215091942,1.),.UNSPECIFIED.)
GEOMETRIC_REPRESENTATION_ITEM()
RATIONAL_B_SPLINE_SURFACE(((1.00008915600322,0.793434085499825,1.),(1.00008930224975,
0.793095246303367,1.),(1.00008944684597,0.79276023072064,1.),(1.00008958984376,
0.792428918540676,1.)))
REPRESENTATION_ITEM('')
SURFACE()
);
#4049=(
BOUNDED_SURFACE()
B_SPLINE_SURFACE(3,2,((#448633,#448634,#448635),(#448636,#448637,#448638),
(#448639,#448640,#448641),(#448642,#448643,#448644),(#448645,#448646,#448647),
(#448648,#448649,#448650)),.UNSPECIFIED.,.F.,.F.,.F.)
B_SPLINE_SURFACE_WITH_KNOTS((4,2,4),(3,3),(3.3881317890172E-20,7.62675010863199E-5,
0.00015253500217264),(0.,1.02152348203045),.UNSPECIFIED.)
GEOMETRIC_REPRESENTATION_ITEM()
RATIONAL_B_SPLINE_SURFACE(((1.,0.789033595401298,1.00908146323682),(1.,
0.857071781054873,1.00615262590422),(1.,0.922087264710742,1.00335390671588),
(1.,0.922394466502397,1.0033406826114),(1.,0.857224384599075,1.00614605678494),
(1.,0.789033595401696,1.0090814632368)))
REPRESENTATION_ITEM('')
SURFACE()
);
#4050=(
BOUNDED_SURFACE()
B_SPLINE_SURFACE(3,2,((#448652,#448653,#448654),(#448655,#448656,#448657),
(#448658,#448659,#448660),(#448661,#448662,#448663)),.UNSPECIFIED.,.F.,
 .F.,.F.)
B_SPLINE_SURFACE_WITH_KNOTS((4,4),(3,3),(3.79470760369927E-19,4.88747512969883E-5),
(-0.000215489857081522,1.),.UNSPECIFIED.)
GEOMETRIC_REPRESENTATION_ITEM()
RATIONAL_B_SPLINE_SURFACE(((1.00008945889715,0.792428983985735,1.),(1.00008931610837,
0.792760296061283,1.),(1.00008917172349,0.793095311538361,1.),(1.00008902569072,
0.793434150627989,1.)))
REPRESENTATION_ITEM('')
SURFACE()
);
#4051=(
BOUNDED_SURFACE()
B_SPLINE_SURFACE(3,2,((#448665,#448666,#448667),(#448668,#448669,#448670),
(#448671,#448672,#448673),(#448674,#448675,#448676)),.UNSPECIFIED.,.F.,
 .F.,.F.)
B_SPLINE_SURFACE_WITH_KNOTS((4,4),(3,3),(-5.21974905013089E-6,5.74172395514398E-5),
(-0.00139822857803481,1.00051312364081),.UNSPECIFIED.)
GEOMETRIC_REPRESENTATION_ITEM()
RATIONAL_B_SPLINE_SURFACE(((1.00049256947267,0.823768952243903,1.00018060397854),
(1.00048448215737,0.826662424388194,1.00017763870887),(1.00052427784046,
0.812424361909265,1.00019223006927),(1.00059912365883,0.785646094632609,
1.00021967280237)))
REPRESENTATION_ITEM('')
SURFACE()
);
#4052=(
BOUNDED_SURFACE()
B_SPLINE_SURFACE(3,2,((#448680,#448681,#448682),(#448683,#448684,#448685),
(#448686,#448687,#448688),(#448689,#448690,#448691)),.UNSPECIFIED.,.F.,
 .F.,.F.)
B_SPLINE_SURFACE_WITH_KNOTS((4,4),(3,3),(3.22980774337777E-5,9.6376485487225E-5),
(-0.00154325936392724,1.01095292447545),.UNSPECIFIED.)
GEOMETRIC_REPRESENTATION_ITEM()
RATIONAL_B_SPLINE_SURFACE(((1.00023530983302,0.922925743796147,1.00168574728331),
(1.00015136166127,0.950422439594206,1.0010843469906),(1.00033574337403,
0.890029368953936,1.00240524789548),(1.00054260094228,0.822274473168295,
1.00388716464859)))
REPRESENTATION_ITEM('')
SURFACE()
);
#4053=(
BOUNDED_SURFACE()
B_SPLINE_SURFACE(3,2,((#448791,#448792,#448793),(#448794,#448795,#448796),
(#448797,#448798,#448799),(#448800,#448801,#448802)),.UNSPECIFIED.,.F.,
 .F.,.F.)
B_SPLINE_SURFACE_WITH_KNOTS((4,4),(3,3),(0.,0.000101260117256738),(0.,1.),
 .UNSPECIFIED.)
GEOMETRIC_REPRESENTATION_ITEM()
RATIONAL_B_SPLINE_SURFACE(((1.,0.79661527883517,1.),(1.,0.795896038055943,
1.),(1.,0.795193354661348,1.),(1.,0.794506193185545,1.)))
REPRESENTATION_ITEM('')
SURFACE()
);
#4054=(
BOUNDED_SURFACE()
B_SPLINE_SURFACE(3,2,((#448840,#448841,#448842),(#448843,#448844,#448845),
(#448846,#448847,#448848),(#448849,#448850,#448851),(#448852,#448853,#448854),
(#448855,#448856,#448857)),.UNSPECIFIED.,.F.,.F.,.F.)
B_SPLINE_SURFACE_WITH_KNOTS((4,2,4),(3,3),(1.42301535138722E-19,1.66936432462299E-5,
3.33872864924596E-5),(0.,1.),.UNSPECIFIED.)
GEOMETRIC_REPRESENTATION_ITEM()
RATIONAL_B_SPLINE_SURFACE(((1.,0.796615278835174,1.),(1.,0.862310524418123,
1.),(1.,0.923774472010524,1.),(1.,0.923983993203422,1.),(1.,0.86257487372094,
1.),(1.,0.796615278835185,1.)))
REPRESENTATION_ITEM('')
SURFACE()
);
#4055=(
BOUNDED_SURFACE()
B_SPLINE_SURFACE(3,2,((#448894,#448895,#448896),(#448897,#448898,#448899),
(#448900,#448901,#448902),(#448903,#448904,#448905)),.UNSPECIFIED.,.F.,
 .F.,.F.)
B_SPLINE_SURFACE_WITH_KNOTS((4,4),(3,3),(-2.16840434497101E-19,0.000101244905251112),
(0.,1.),.UNSPECIFIED.)
GEOMETRIC_REPRESENTATION_ITEM()
RATIONAL_B_SPLINE_SURFACE(((1.,0.79661527883517,1.),(1.,0.795896146109792,
1.),(1.,0.795193565796506,1.),(1.,0.794506502889899,1.)))
REPRESENTATION_ITEM('')
SURFACE()
);
#4056=(
BOUNDED_SURFACE()
B_SPLINE_SURFACE(3,2,((#448941,#448942,#448943),(#448944,#448945,#448946),
(#448947,#448948,#448949),(#448950,#448951,#448952)),.UNSPECIFIED.,.F.,
 .F.,.F.)
B_SPLINE_SURFACE_WITH_KNOTS((4,4),(3,3),(2.85968127239939E-5,9.24681548475821E-5),
(-0.00167900678649206,1.01130827127841),.UNSPECIFIED.)
GEOMETRIC_REPRESENTATION_ITEM()
RATIONAL_B_SPLINE_SURFACE(((1.00059040895215,0.822187541868248,1.00401468696663),
(1.00036527718138,0.889990093671552,1.00248382673395),(1.00016469515012,
0.950399042257925,1.00111990082513),(1.00025604273992,0.922888044286069,
1.00174104990634)))
REPRESENTATION_ITEM('')
SURFACE()
);
#4057=(
BOUNDED_SURFACE()
B_SPLINE_SURFACE(3,2,((#448956,#448957,#448958),(#448959,#448960,#448961),
(#448962,#448963,#448964),(#448965,#448966,#448967)),.UNSPECIFIED.,.F.,
 .F.,.F.)
B_SPLINE_SURFACE_WITH_KNOTS((4,4),(3,3),(-5.22358356749231E-6,5.74594192424277E-5),
(-0.00127120052066043,1.),.UNSPECIFIED.)
GEOMETRIC_REPRESENTATION_ITEM()
RATIONAL_B_SPLINE_SURFACE(((1.0005444931318,0.785835073638737,1.),(1.00047707767479,
0.812351526358842,1.),(1.0004403178859,0.82681021650626,1.),(1.00044777653322,
0.82387651438724,1.)))
REPRESENTATION_ITEM('')
SURFACE()
);
#4058=(
BOUNDED_SURFACE()
B_SPLINE_SURFACE(3,2,((#448969,#448970,#448971),(#448972,#448973,#448974),
(#448975,#448976,#448977),(#448978,#448979,#448980)),.UNSPECIFIED.,.F.,
 .F.,.F.)
B_SPLINE_SURFACE_WITH_KNOTS((4,4),(3,3),(-1.0842021724855E-19,4.88747512969881E-5),
(-0.000215805215184123,1.),.UNSPECIFIED.)
GEOMETRIC_REPRESENTATION_ITEM()
RATIONAL_B_SPLINE_SURFACE(((1.00008915600326,0.793434085499805,1.),(1.00008930224979,
0.79309524630336,1.),(1.00008944684601,0.792760230720614,1.),(1.0000895898438,
0.792428918540653,1.)))
REPRESENTATION_ITEM('')
SURFACE()
);
#4059=(
BOUNDED_SURFACE()
B_SPLINE_SURFACE(3,2,((#448982,#448983,#448984),(#448985,#448986,#448987),
(#448988,#448989,#448990),(#448991,#448992,#448993),(#448994,#448995,#448996),
(#448997,#448998,#448999)),.UNSPECIFIED.,.F.,.F.,.F.)
B_SPLINE_SURFACE_WITH_KNOTS((4,2,4),(3,3),(6.09863722023096E-20,7.62675010863199E-5,
0.00015253500217264),(0.,1.02152348203022),.UNSPECIFIED.)
GEOMETRIC_REPRESENTATION_ITEM()
RATIONAL_B_SPLINE_SURFACE(((1.,0.789033595401343,1.00908146323672),(1.,
0.857071781054904,1.00615262590415),(1.,0.922087264710765,1.00335390671585),
(1.,0.922394466502406,1.00334068261136),(1.,0.857224384599113,1.00614605678487),
(1.,0.789033595401744,1.0090814632367)))
REPRESENTATION_ITEM('')
SURFACE()
);
#4060=(
BOUNDED_SURFACE()
B_SPLINE_SURFACE(3,2,((#449001,#449002,#449003),(#449004,#449005,#449006),
(#449007,#449008,#449009),(#449010,#449011,#449012)),.UNSPECIFIED.,.F.,
 .F.,.F.)
B_SPLINE_SURFACE_WITH_KNOTS((4,4),(3,3),(1.0842021724855E-19,4.88747512969882E-5),
(-0.0002154898570242,1.),.UNSPECIFIED.)
GEOMETRIC_REPRESENTATION_ITEM()
RATIONAL_B_SPLINE_SURFACE(((1.00008945889713,0.792428983985745,1.),(1.00008931610834,
0.792760296061291,1.),(1.00008917172347,0.793095311538371,1.),(1.00008902569069,
0.793434150627998,1.)))
REPRESENTATION_ITEM('')
SURFACE()
);
#4061=(
BOUNDED_SURFACE()
B_SPLINE_SURFACE(3,2,((#449014,#449015,#449016),(#449017,#449018,#449019),
(#449020,#449021,#449022),(#449023,#449024,#449025)),.UNSPECIFIED.,.F.,
 .F.,.F.)
B_SPLINE_SURFACE_WITH_KNOTS((4,4),(3,3),(-5.21974905013085E-6,5.74172395514398E-5),
(-0.00139822857777821,1.00051312364075),.UNSPECIFIED.)
GEOMETRIC_REPRESENTATION_ITEM()
RATIONAL_B_SPLINE_SURFACE(((1.00049256947258,0.823768952243957,1.00018060397852),
(1.00048448215728,0.826662424388249,1.00017763870885),(1.00052427784037,
0.812424361909315,1.00019223006924),(1.00059912365872,0.785646094632677,
1.00021967280235)))
REPRESENTATION_ITEM('')
SURFACE()
);
#4062=(
BOUNDED_SURFACE()
B_SPLINE_SURFACE(3,2,((#449029,#449030,#449031),(#449032,#449033,#449034),
(#449035,#449036,#449037),(#449038,#449039,#449040)),.UNSPECIFIED.,.F.,
 .F.,.F.)
B_SPLINE_SURFACE_WITH_KNOTS((4,4),(3,3),(3.22980774337779E-5,9.63764854872257E-5),
(-0.00154325936360782,1.01095292447527),.UNSPECIFIED.)
GEOMETRIC_REPRESENTATION_ITEM()
RATIONAL_B_SPLINE_SURFACE(((1.00023530983297,0.922925743796185,1.00168574728329),
(1.00015136166124,0.950422439594226,1.00108434699058),(1.00033574337396,
0.890029368953995,1.00240524789544),(1.00054260094217,0.822274473168382,
1.00388716464852)))
REPRESENTATION_ITEM('')
SURFACE()
);
#4063=(
BOUNDED_SURFACE()
B_SPLINE_SURFACE(3,2,((#449140,#449141,#449142),(#449143,#449144,#449145),
(#449146,#449147,#449148),(#449149,#449150,#449151)),.UNSPECIFIED.,.F.,
 .F.,.F.)
B_SPLINE_SURFACE_WITH_KNOTS((4,4),(3,3),(0.,0.000101260117256737),(0.,1.),
 .UNSPECIFIED.)
GEOMETRIC_REPRESENTATION_ITEM()
RATIONAL_B_SPLINE_SURFACE(((1.,0.79661527883517,1.),(1.,0.795896038055935,
1.),(1.,0.79519335466136,1.),(1.,0.794506193185533,1.)))
REPRESENTATION_ITEM('')
SURFACE()
);
#4064=(
BOUNDED_SURFACE()
B_SPLINE_SURFACE(3,2,((#449189,#449190,#449191),(#449192,#449193,#449194),
(#449195,#449196,#449197),(#449198,#449199,#449200),(#449201,#449202,#449203),
(#449204,#449205,#449206)),.UNSPECIFIED.,.F.,.F.,.F.)
B_SPLINE_SURFACE_WITH_KNOTS((4,2,4),(3,3),(1.55854062294791E-19,1.66936432462294E-5,
3.33872864924587E-5),(0.,1.),.UNSPECIFIED.)
GEOMETRIC_REPRESENTATION_ITEM()
RATIONAL_B_SPLINE_SURFACE(((1.,0.796615278835177,1.),(1.,0.862310524418132,
1.),(1.,0.923774472010521,1.),(1.,0.923983993203426,1.),(1.,0.862574873720942,
1.),(1.,0.796615278835183,1.)))
REPRESENTATION_ITEM('')
SURFACE()
);
#4065=(
BOUNDED_SURFACE()
B_SPLINE_SURFACE(3,2,((#449243,#449244,#449245),(#449246,#449247,#449248),
(#449249,#449250,#449251),(#449252,#449253,#449254)),.UNSPECIFIED.,.F.,
 .F.,.F.)
B_SPLINE_SURFACE_WITH_KNOTS((4,4),(3,3),(0.,0.000101244905251112),(0.,1.),
 .UNSPECIFIED.)
GEOMETRIC_REPRESENTATION_ITEM()
RATIONAL_B_SPLINE_SURFACE(((1.,0.796615278835169,1.),(1.,0.795896146109794,
1.),(1.,0.795193565796497,1.),(1.,0.794506502889899,1.)))
REPRESENTATION_ITEM('')
SURFACE()
);
#4066=(
BOUNDED_SURFACE()
B_SPLINE_SURFACE(3,2,((#449290,#449291,#449292),(#449293,#449294,#449295),
(#449296,#449297,#449298),(#449299,#449300,#449301)),.UNSPECIFIED.,.F.,
 .F.,.F.)
B_SPLINE_SURFACE_WITH_KNOTS((4,4),(3,3),(2.85968127239938E-5,9.24681548475816E-5),
(-0.00167900678746727,1.01130827127807),.UNSPECIFIED.)
GEOMETRIC_REPRESENTATION_ITEM()
RATIONAL_B_SPLINE_SURFACE(((1.00059040895249,0.822187541868134,1.00401468696651),
(1.0003652771816,0.889990093671489,1.00248382673388),(1.00016469515022,
0.950399042257892,1.00111990082509),(1.00025604274006,0.92288804428602,
1.00174104990629)))
REPRESENTATION_ITEM('')
SURFACE()
);
#4067=(
BOUNDED_SURFACE()
B_SPLINE_SURFACE(3,2,((#449305,#449306,#449307),(#449308,#449309,#449310),
(#449311,#449312,#449313),(#449314,#449315,#449316)),.UNSPECIFIED.,.F.,
 .F.,.F.)
B_SPLINE_SURFACE_WITH_KNOTS((4,4),(3,3),(-5.22358356749317E-6,5.74594192424277E-5),
(-0.00127120052063584,1.),.UNSPECIFIED.)
GEOMETRIC_REPRESENTATION_ITEM()
RATIONAL_B_SPLINE_SURFACE(((1.00054449313178,0.785835073638741,1.),(1.00047707767478,
0.812351526358851,1.),(1.00044031788589,0.826810216506262,1.),(1.00044777653321,
0.823876514387244,1.)))
REPRESENTATION_ITEM('')
SURFACE()
);
#4068=(
BOUNDED_SURFACE()
B_SPLINE_SURFACE(3,2,((#449318,#449319,#449320),(#449321,#449322,#449323),
(#449324,#449325,#449326),(#449327,#449328,#449329)),.UNSPECIFIED.,.F.,
 .F.,.F.)
B_SPLINE_SURFACE_WITH_KNOTS((4,4),(3,3),(-8.13151629364128E-20,4.8874751296988E-5),
(-0.00021580521548104,1.),.UNSPECIFIED.)
GEOMETRIC_REPRESENTATION_ITEM()
RATIONAL_B_SPLINE_SURFACE(((1.00008915600338,0.793434085499746,1.),(1.00008930224991,
0.793095246303297,1.),(1.00008944684613,0.792760230720554,1.),(1.00008958984392,
0.792428918540594,1.)))
REPRESENTATION_ITEM('')
SURFACE()
);
#4069=(
BOUNDED_SURFACE()
B_SPLINE_SURFACE(3,2,((#449331,#449332,#449333),(#449334,#449335,#449336),
(#449337,#449338,#449339),(#449340,#449341,#449342),(#449343,#449344,#449345),
(#449346,#449347,#449348)),.UNSPECIFIED.,.F.,.F.,.F.)
B_SPLINE_SURFACE_WITH_KNOTS((4,2,4),(3,3),(-1.0842021724855E-19,7.62675010863192E-5,
0.000152535002172638),(0.,1.02152348203042),.UNSPECIFIED.)
GEOMETRIC_REPRESENTATION_ITEM()
RATIONAL_B_SPLINE_SURFACE(((1.,0.789033595401302,1.0090814632368),(1.,0.857071781054877,
1.00615262590421),(1.,0.922087264710747,1.00335390671588),(1.,0.922394466502397,
1.00334068261139),(1.,0.857224384599085,1.00614605678493),(1.,0.789033595401703,
1.00908146323679)))
REPRESENTATION_ITEM('')
SURFACE()
);
#4070=(
BOUNDED_SURFACE()
B_SPLINE_SURFACE(3,2,((#449350,#449351,#449352),(#449353,#449354,#449355),
(#449356,#449357,#449358),(#449359,#449360,#449361)),.UNSPECIFIED.,.F.,
 .F.,.F.)
B_SPLINE_SURFACE_WITH_KNOTS((4,4),(3,3),(1.62630325872826E-19,4.88747512969882E-5),
(-0.000215489857674331,1.),.UNSPECIFIED.)
GEOMETRIC_REPRESENTATION_ITEM()
RATIONAL_B_SPLINE_SURFACE(((1.0000894588974,0.792428983985611,1.),(1.00008931610861,
0.792760296061153,1.),(1.00008917172374,0.793095311538236,1.),(1.00008902569096,
0.793434150627863,1.)))
REPRESENTATION_ITEM('')
SURFACE()
);
#4071=(
BOUNDED_SURFACE()
B_SPLINE_SURFACE(3,2,((#449363,#449364,#449365),(#449366,#449367,#449368),
(#449369,#449370,#449371),(#449372,#449373,#449374)),.UNSPECIFIED.,.F.,
 .F.,.F.)
B_SPLINE_SURFACE_WITH_KNOTS((4,4),(3,3),(-5.21974905013085E-6,5.74172395514395E-5),
(-0.00139822857732513,1.00051312364061),.UNSPECIFIED.)
GEOMETRIC_REPRESENTATION_ITEM()
RATIONAL_B_SPLINE_SURFACE(((1.00049256947242,0.82376895224406,1.00018060397847),
(1.00048448215713,0.82666242438835,1.0001776387088),(1.0005242778402,0.812424361909424,
1.00019223006919),(1.00059912365853,0.785646094632805,1.00021967280229)))
REPRESENTATION_ITEM('')
SURFACE()
);
#4072=(
BOUNDED_SURFACE()
B_SPLINE_SURFACE(3,2,((#449378,#449379,#449380),(#449381,#449382,#449383),
(#449384,#449385,#449386),(#449387,#449388,#449389)),.UNSPECIFIED.,.F.,
 .F.,.F.)
B_SPLINE_SURFACE_WITH_KNOTS((4,4),(3,3),(3.22980774337778E-5,9.6376485487225E-5),
(-0.00154325936394921,1.01095292447551),.UNSPECIFIED.)
GEOMETRIC_REPRESENTATION_ITEM()
RATIONAL_B_SPLINE_SURFACE(((1.00023530983302,0.92292574379614,1.00168574728332),
(1.00015136166128,0.950422439594194,1.00108434699061),(1.00033574337403,
0.890029368953931,1.00240524789549),(1.00054260094229,0.822274473168285,
1.00388716464861)))
REPRESENTATION_ITEM('')
SURFACE()
);
#4073=(
BOUNDED_CURVE()
B_SPLINE_CURVE(2,(#138438,#138439,#138440),.UNSPECIFIED.,.F.,.F.)
B_SPLINE_CURVE_WITH_KNOTS((3,3),(0.530296992815185,0.716353725522381),
 .UNSPECIFIED.)
CURVE()
GEOMETRIC_REPRESENTATION_ITEM()
RATIONAL_B_SPLINE_CURVE((1.02304101018598,1.02047479091633,1.01327152413875))
REPRESENTATION_ITEM('')
);
#4074=(
BOUNDED_CURVE()
B_SPLINE_CURVE(2,(#138443,#138444,#138445),.UNSPECIFIED.,.F.,.F.)
B_SPLINE_CURVE_WITH_KNOTS((3,3),(0.13830647491131,0.324363207617007),
 .UNSPECIFIED.)
CURVE()
GEOMETRIC_REPRESENTATION_ITEM()
RATIONAL_B_SPLINE_CURVE((1.01327152413597,1.02047479091208,1.02304101018125))
REPRESENTATION_ITEM('')
);
#4075=(
BOUNDED_CURVE()
B_SPLINE_CURVE(2,(#138448,#138449,#138450),.UNSPECIFIED.,.F.,.F.)
B_SPLINE_CURVE_WITH_KNOTS((3,3),(0.138306474911315,0.324363207616966),
 .UNSPECIFIED.)
CURVE()
GEOMETRIC_REPRESENTATION_ITEM()
RATIONAL_B_SPLINE_CURVE((1.01327152413589,1.02047479091195,1.02304101018111))
REPRESENTATION_ITEM('')
);
#4076=(
BOUNDED_CURVE()
B_SPLINE_CURVE(2,(#138452,#138453,#138454),.UNSPECIFIED.,.F.,.F.)
B_SPLINE_CURVE_WITH_KNOTS((3,3),(0.530296992818036,0.716353725523729),
 .UNSPECIFIED.)
CURVE()
GEOMETRIC_REPRESENTATION_ITEM()
RATIONAL_B_SPLINE_CURVE((1.02304101018115,1.02047479091198,1.01327152413591))
REPRESENTATION_ITEM('')
);
#4077=(
BOUNDED_CURVE()
B_SPLINE_CURVE(2,(#138458,#138459,#138460),.UNSPECIFIED.,.F.,.F.)
B_SPLINE_CURVE_WITH_KNOTS((3,3),(0.138306474911272,0.324363207616997),
 .UNSPECIFIED.)
CURVE()
GEOMETRIC_REPRESENTATION_ITEM()
RATIONAL_B_SPLINE_CURVE((1.01327152413612,1.02047479091231,1.02304101018152))
REPRESENTATION_ITEM('')
);
#4078=(
BOUNDED_CURVE()
B_SPLINE_CURVE(2,(#138462,#138463,#138464),.UNSPECIFIED.,.F.,.F.)
B_SPLINE_CURVE_WITH_KNOTS((3,3),(0.530296992818049,0.716353725523754),
 .UNSPECIFIED.)
CURVE()
GEOMETRIC_REPRESENTATION_ITEM()
RATIONAL_B_SPLINE_CURVE((1.0230410101813,1.02047479091212,1.013271524136))
REPRESENTATION_ITEM('')
);
#4079=(
BOUNDED_CURVE()
B_SPLINE_CURVE(2,(#138468,#138469,#138470),.UNSPECIFIED.,.F.,.F.)
B_SPLINE_CURVE_WITH_KNOTS((3,3),(1.87444128059995,1.89461071071013),
 .UNSPECIFIED.)
CURVE()
GEOMETRIC_REPRESENTATION_ITEM()
RATIONAL_B_SPLINE_CURVE((1.50304878048778,1.4222597775933,1.33967391292897))
REPRESENTATION_ITEM('')
);
#4080=(
BOUNDED_CURVE()
B_SPLINE_CURVE(2,(#138473,#138474,#138475),.UNSPECIFIED.,.F.,.F.)
B_SPLINE_CURVE_WITH_KNOTS((3,3),(0.0405896019330352,0.0607590320292299),
 .UNSPECIFIED.)
CURVE()
GEOMETRIC_REPRESENTATION_ITEM()
RATIONAL_B_SPLINE_CURVE((1.3396739130435,1.42225977764934,1.50304878048783))
REPRESENTATION_ITEM('')
);
#4081=(
BOUNDED_CURVE()
B_SPLINE_CURVE(2,(#138478,#138479,#138480),.UNSPECIFIED.,.F.,.F.)
B_SPLINE_CURVE_WITH_KNOTS((3,3),(0.0405896019330352,0.0607590320292299),
 .UNSPECIFIED.)
CURVE()
GEOMETRIC_REPRESENTATION_ITEM()
RATIONAL_B_SPLINE_CURVE((1.3396739130435,1.42225977764934,1.50304878048783))
REPRESENTATION_ITEM('')
);
#4082=(
BOUNDED_CURVE()
B_SPLINE_CURVE(2,(#138482,#138483,#138484),.UNSPECIFIED.,.F.,.F.)
B_SPLINE_CURVE_WITH_KNOTS((3,3),(1.87444128059996,1.89461071071012),
 .UNSPECIFIED.)
CURVE()
GEOMETRIC_REPRESENTATION_ITEM()
RATIONAL_B_SPLINE_CURVE((1.50304878048772,1.42225977759326,1.33967391292897))
REPRESENTATION_ITEM('')
);
#4083=(
BOUNDED_CURVE()
B_SPLINE_CURVE(2,(#138488,#138489,#138490),.UNSPECIFIED.,.F.,.F.)
B_SPLINE_CURVE_WITH_KNOTS((3,3),(0.0405896019330354,0.0607590320292301),
 .UNSPECIFIED.)
CURVE()
GEOMETRIC_REPRESENTATION_ITEM()
RATIONAL_B_SPLINE_CURVE((1.3396739130435,1.42225977764934,1.50304878048783))
REPRESENTATION_ITEM('')
);
#4084=(
BOUNDED_CURVE()
B_SPLINE_CURVE(2,(#138492,#138493,#138494),.UNSPECIFIED.,.F.,.F.)
B_SPLINE_CURVE_WITH_KNOTS((3,3),(1.87444128059996,1.89461071071014),
 .UNSPECIFIED.)
CURVE()
GEOMETRIC_REPRESENTATION_ITEM()
RATIONAL_B_SPLINE_CURVE((1.50304878048772,1.42225977759322,1.33967391292888))
REPRESENTATION_ITEM('')
);
#4085=(
BOUNDED_CURVE()
B_SPLINE_CURVE(2,(#138551,#138552,#138553),.UNSPECIFIED.,.F.,.F.)
B_SPLINE_CURVE_WITH_KNOTS((3,3),(0.530296992815185,0.716353725522381),
 .UNSPECIFIED.)
CURVE()
GEOMETRIC_REPRESENTATION_ITEM()
RATIONAL_B_SPLINE_CURVE((1.02304101018598,1.02047479091633,1.01327152413875))
REPRESENTATION_ITEM('')
);
#4086=(
BOUNDED_CURVE()
B_SPLINE_CURVE(2,(#138556,#138557,#138558),.UNSPECIFIED.,.F.,.F.)
B_SPLINE_CURVE_WITH_KNOTS((3,3),(0.13830647491131,0.324363207617007),
 .UNSPECIFIED.)
CURVE()
GEOMETRIC_REPRESENTATION_ITEM()
RATIONAL_B_SPLINE_CURVE((1.01327152413597,1.02047479091208,1.02304101018125))
REPRESENTATION_ITEM('')
);
#4087=(
BOUNDED_CURVE()
B_SPLINE_CURVE(2,(#138561,#138562,#138563),.UNSPECIFIED.,.F.,.F.)
B_SPLINE_CURVE_WITH_KNOTS((3,3),(1.87444128059995,1.89461071071013),
 .UNSPECIFIED.)
CURVE()
GEOMETRIC_REPRESENTATION_ITEM()
RATIONAL_B_SPLINE_CURVE((1.50304878048776,1.42225977759327,1.33967391292894))
REPRESENTATION_ITEM('')
);
#4088=(
BOUNDED_CURVE()
B_SPLINE_CURVE(2,(#138566,#138567,#138568),.UNSPECIFIED.,.F.,.F.)
B_SPLINE_CURVE_WITH_KNOTS((3,3),(0.0405896019330352,0.0607590320292299),
 .UNSPECIFIED.)
CURVE()
GEOMETRIC_REPRESENTATION_ITEM()
RATIONAL_B_SPLINE_CURVE((1.3396739130435,1.42225977764934,1.50304878048783))
REPRESENTATION_ITEM('')
);
#4089=(
BOUNDED_CURVE()
B_SPLINE_CURVE(2,(#140599,#140600,#140601),.UNSPECIFIED.,.F.,.F.)
B_SPLINE_CURVE_WITH_KNOTS((3,3),(0.,0.128077890591623),.UNSPECIFIED.)
CURVE()
GEOMETRIC_REPRESENTATION_ITEM()
RATIONAL_B_SPLINE_CURVE((1.,1.00129982111734,1.))
REPRESENTATION_ITEM('')
);
#4090=(
BOUNDED_CURVE()
B_SPLINE_CURVE(2,(#140616,#140617,#140618),.UNSPECIFIED.,.F.,.F.)
B_SPLINE_CURVE_WITH_KNOTS((3,3),(0.000362946931860339,0.146205519527569),
 .UNSPECIFIED.)
CURVE()
GEOMETRIC_REPRESENTATION_ITEM()
RATIONAL_B_SPLINE_CURVE((1.00000258096586,1.0005198467923,1.00000237765636))
REPRESENTATION_ITEM('')
);
#4091=(
BOUNDED_CURVE()
B_SPLINE_CURVE(2,(#141526,#141527,#141528),.UNSPECIFIED.,.F.,.F.)
B_SPLINE_CURVE_WITH_KNOTS((3,3),(0.00319674958924355,0.00384559926899821),
 .UNSPECIFIED.)
CURVE()
GEOMETRIC_REPRESENTATION_ITEM()
RATIONAL_B_SPLINE_CURVE((1.00001174504467,1.00001239664656,1.00001282889535))
REPRESENTATION_ITEM('')
);
#4092=(
BOUNDED_CURVE()
B_SPLINE_CURVE(2,(#141532,#141533,#141534),.UNSPECIFIED.,.F.,.F.)
B_SPLINE_CURVE_WITH_KNOTS((3,3),(0.235117374689744,0.605037926847431),
 .UNSPECIFIED.)
CURVE()
GEOMETRIC_REPRESENTATION_ITEM()
RATIONAL_B_SPLINE_CURVE((1.05233383959897,1.08689092491703,1.10064057896449))
REPRESENTATION_ITEM('')
);
#4093=(
BOUNDED_CURVE()
B_SPLINE_CURVE(2,(#141570,#141571,#141572),.UNSPECIFIED.,.F.,.F.)
B_SPLINE_CURVE_WITH_KNOTS((3,3),(1.57192299052648,2.14887151832575),
 .UNSPECIFIED.)
CURVE()
GEOMETRIC_REPRESENTATION_ITEM()
RATIONAL_B_SPLINE_CURVE((6.65976698144355,7.49223785412377,8.17335038631666))
REPRESENTATION_ITEM('')
);
#4094=(
BOUNDED_CURVE()
B_SPLINE_CURVE(2,(#141613,#141614,#141615),.UNSPECIFIED.,.F.,.F.)
B_SPLINE_CURVE_WITH_KNOTS((3,3),(0.270860367343992,0.325892472320335),
 .UNSPECIFIED.)
CURVE()
GEOMETRIC_REPRESENTATION_ITEM()
RATIONAL_B_SPLINE_CURVE((1.54730126785002,1.59219194080314,1.63273127384522))
REPRESENTATION_ITEM('')
);
#4095=(
BOUNDED_CURVE()
B_SPLINE_CURVE(2,(#141631,#141632,#141633),.UNSPECIFIED.,.F.,.F.)
B_SPLINE_CURVE_WITH_KNOTS((3,3),(0.,0.29854563440631),.UNSPECIFIED.)
CURVE()
GEOMETRIC_REPRESENTATION_ITEM()
RATIONAL_B_SPLINE_CURVE((1.,1.04264499839507,1.))
REPRESENTATION_ITEM('')
);
#4096=(
BOUNDED_CURVE()
B_SPLINE_CURVE(2,(#141725,#141726,#141727,#141728),.UNSPECIFIED.,.F.,.F.)
B_SPLINE_CURVE_WITH_KNOTS((3,1,3),(1.66167847180388,2.26230069355391,2.27651444205068),
 .UNSPECIFIED.)
CURVE()
GEOMETRIC_REPRESENTATION_ITEM()
RATIONAL_B_SPLINE_CURVE((6.5568621272732,7.34757944538262,7.99897023989561,
8.01394260001255))
REPRESENTATION_ITEM('')
);
#4097=(
BOUNDED_CURVE()
B_SPLINE_CURVE(2,(#143650,#143651,#143652),.UNSPECIFIED.,.F.,.F.)
B_SPLINE_CURVE_WITH_KNOTS((3,3),(0.,0.28311686851659),.UNSPECIFIED.)
CURVE()
GEOMETRIC_REPRESENTATION_ITEM()
RATIONAL_B_SPLINE_CURVE((1.,1.06870093790198,1.))
REPRESENTATION_ITEM('')
);
#4098=(
BOUNDED_CURVE()
B_SPLINE_CURVE(2,(#143653,#143654,#143655),.UNSPECIFIED.,.F.,.F.)
B_SPLINE_CURVE_WITH_KNOTS((3,3),(0.,0.283116868518929),.UNSPECIFIED.)
CURVE()
GEOMETRIC_REPRESENTATION_ITEM()
RATIONAL_B_SPLINE_CURVE((1.,1.0687009379036,1.))
REPRESENTATION_ITEM('')
);
#4099=(
BOUNDED_CURVE()
B_SPLINE_CURVE(2,(#143729,#143730,#143731),.UNSPECIFIED.,.F.,.F.)
B_SPLINE_CURVE_WITH_KNOTS((3,3),(0.185737456128969,0.362789547470562),
 .UNSPECIFIED.)
CURVE()
GEOMETRIC_REPRESENTATION_ITEM()
RATIONAL_B_SPLINE_CURVE((1.,1.13683142662591,1.01279688953851))
REPRESENTATION_ITEM('')
);
#4100=(
BOUNDED_CURVE()
B_SPLINE_CURVE(2,(#143745,#143746,#143747),.UNSPECIFIED.,.F.,.F.)
B_SPLINE_CURVE_WITH_KNOTS((3,3),(0.00868536478737642,0.185737456128969),
 .UNSPECIFIED.)
CURVE()
GEOMETRIC_REPRESENTATION_ITEM()
RATIONAL_B_SPLINE_CURVE((1.01279688953851,1.13683142662591,1.))
REPRESENTATION_ITEM('')
);
#4101=(
BOUNDED_CURVE()
B_SPLINE_CURVE(2,(#143752,#143753,#143754),.UNSPECIFIED.,.F.,.F.)
B_SPLINE_CURVE_WITH_KNOTS((3,3),(0.,0.0101246152898397),.UNSPECIFIED.)
CURVE()
GEOMETRIC_REPRESENTATION_ITEM()
RATIONAL_B_SPLINE_CURVE((1.,1.01194504282515,1.023099278064))
REPRESENTATION_ITEM('')
);
#4102=(
BOUNDED_CURVE()
B_SPLINE_CURVE(2,(#143755,#143756,#143757),.UNSPECIFIED.,.F.,.F.)
B_SPLINE_CURVE_WITH_KNOTS((3,3),(0.29573730439733,0.30586191968717),
 .UNSPECIFIED.)
CURVE()
GEOMETRIC_REPRESENTATION_ITEM()
RATIONAL_B_SPLINE_CURVE((1.02309927806399,1.01194504282515,1.))
REPRESENTATION_ITEM('')
);
#4103=(
BOUNDED_CURVE()
B_SPLINE_CURVE(2,(#143761,#143762,#143763),.UNSPECIFIED.,.F.,.F.)
B_SPLINE_CURVE_WITH_KNOTS((3,3),(0.185737456128969,0.362789547470561),
 .UNSPECIFIED.)
CURVE()
GEOMETRIC_REPRESENTATION_ITEM()
RATIONAL_B_SPLINE_CURVE((1.,1.13683142662589,1.01279688953851))
REPRESENTATION_ITEM('')
);
#4104=(
BOUNDED_CURVE()
B_SPLINE_CURVE(2,(#143777,#143778,#143779),.UNSPECIFIED.,.F.,.F.)
B_SPLINE_CURVE_WITH_KNOTS((3,3),(0.00868536478737701,0.18573745612897),
 .UNSPECIFIED.)
CURVE()
GEOMETRIC_REPRESENTATION_ITEM()
RATIONAL_B_SPLINE_CURVE((1.01279688953851,1.13683142662591,1.))
REPRESENTATION_ITEM('')
);
#4105=(
BOUNDED_CURVE()
B_SPLINE_CURVE(2,(#143784,#143785,#143786),.UNSPECIFIED.,.F.,.F.)
B_SPLINE_CURVE_WITH_KNOTS((3,3),(0.,0.0101246152898398),.UNSPECIFIED.)
CURVE()
GEOMETRIC_REPRESENTATION_ITEM()
RATIONAL_B_SPLINE_CURVE((1.,1.01194504282515,1.023099278064))
REPRESENTATION_ITEM('')
);
#4106=(
BOUNDED_CURVE()
B_SPLINE_CURVE(2,(#143787,#143788,#143789),.UNSPECIFIED.,.F.,.F.)
B_SPLINE_CURVE_WITH_KNOTS((3,3),(0.29573730439733,0.30586191968717),
 .UNSPECIFIED.)
CURVE()
GEOMETRIC_REPRESENTATION_ITEM()
RATIONAL_B_SPLINE_CURVE((1.023099278064,1.01194504282515,1.))
REPRESENTATION_ITEM('')
);
#4107=(
BOUNDED_CURVE()
B_SPLINE_CURVE(2,(#143926,#143927,#143928),.UNSPECIFIED.,.F.,.F.)
B_SPLINE_CURVE_WITH_KNOTS((3,3),(0.281942572226475,0.665668068688164),
 .UNSPECIFIED.)
CURVE()
GEOMETRIC_REPRESENTATION_ITEM()
RATIONAL_B_SPLINE_CURVE((1.10320422134355,1.12183288632099,1.))
REPRESENTATION_ITEM('')
);
#4108=(
BOUNDED_CURVE()
B_SPLINE_CURVE(2,(#143930,#143931,#143932),.UNSPECIFIED.,.F.,.F.)
B_SPLINE_CURVE_WITH_KNOTS((3,3),(0.,0.283207139377398),.UNSPECIFIED.)
CURVE()
GEOMETRIC_REPRESENTATION_ITEM()
RATIONAL_B_SPLINE_CURVE((1.,1.06875639213164,1.00010378144267))
REPRESENTATION_ITEM('')
);
#4109=(
BOUNDED_CURVE()
B_SPLINE_CURVE(2,(#144536,#144537,#144538),.UNSPECIFIED.,.F.,.F.)
B_SPLINE_CURVE_WITH_KNOTS((3,3),(0.,0.128077890592173),.UNSPECIFIED.)
CURVE()
GEOMETRIC_REPRESENTATION_ITEM()
RATIONAL_B_SPLINE_CURVE((1.,1.001299821138,1.))
REPRESENTATION_ITEM('')
);
#4110=(
BOUNDED_CURVE()
B_SPLINE_CURVE(2,(#144636,#144637,#144638),.UNSPECIFIED.,.F.,.F.)
B_SPLINE_CURVE_WITH_KNOTS((3,3),(0.,0.0065572501027407),.UNSPECIFIED.)
CURVE()
GEOMETRIC_REPRESENTATION_ITEM()
RATIONAL_B_SPLINE_CURVE((1.,1.00078068132504,1.00149559186922))
REPRESENTATION_ITEM('')
);
#4111=(
BOUNDED_CURVE()
B_SPLINE_CURVE(2,(#144967,#144968,#144969),.UNSPECIFIED.,.F.,.F.)
B_SPLINE_CURVE_WITH_KNOTS((3,3),(0.000566681709996598,0.146427783245033),
 .UNSPECIFIED.)
CURVE()
GEOMETRIC_REPRESENTATION_ITEM()
RATIONAL_B_SPLINE_CURVE((1.00000402002378,1.00051937724566,1.))
REPRESENTATION_ITEM('')
);
#4112=(
BOUNDED_CURVE()
B_SPLINE_CURVE(2,(#358532,#358533,#358534,#358535,#358536,#358537,#358538,
#358539,#358540,#358541,#358542,#358543,#358544),.UNSPECIFIED.,.F.,.F.)
B_SPLINE_CURVE_WITH_KNOTS((3,2,2,2,2,2,3),(0.954545454545455,0.95959595959596,
0.964646464646465,0.96969696969697,0.974747474747475,0.97979797979798,0.984848484848485),
 .UNSPECIFIED.)
CURVE()
GEOMETRIC_REPRESENTATION_ITEM()
RATIONAL_B_SPLINE_CURVE((1.,0.866025403784439,1.,0.866025403784439,1.,0.866025403784439,
1.,0.866025403784439,1.,0.866025403784439,1.,0.866025403784439,1.))
REPRESENTATION_ITEM('')
);
#4113=(
BOUNDED_CURVE()
B_SPLINE_CURVE(2,(#358547,#358548,#358549,#358550,#358551,#358552,#358553,
#358554,#358555,#358556,#358557,#358558,#358559),.UNSPECIFIED.,.F.,.F.)
B_SPLINE_CURVE_WITH_KNOTS((3,2,2,2,2,2,3),(0.954545454545455,0.95959595959596,
0.964646464646465,0.96969696969697,0.974747474747475,0.97979797979798,0.981126180289492),
 .UNSPECIFIED.)
CURVE()
GEOMETRIC_REPRESENTATION_ITEM()
RATIONAL_B_SPLINE_CURVE((1.,0.866025403784439,1.,0.866025403784439,1.,0.866025403784439,
1.,0.866025403784439,1.,0.866025403784439,1.,0.964766865340363,0.948065210722611))
REPRESENTATION_ITEM('')
);
#4114=(
BOUNDED_CURVE()
B_SPLINE_CURVE(2,(#358564,#358565,#358566,#358567,#358568,#358569,#358570,
#358571,#358572,#358573,#358574,#358575,#358576),.UNSPECIFIED.,.F.,.F.)
B_SPLINE_CURVE_WITH_KNOTS((3,2,2,2,2,2,3),(0.924242424242424,0.929292929292929,
0.934343434343434,0.939393939393939,0.944444444444444,0.94949494949495,
0.954545454545455),.UNSPECIFIED.)
CURVE()
GEOMETRIC_REPRESENTATION_ITEM()
RATIONAL_B_SPLINE_CURVE((1.,0.866025403784439,1.,0.866025403784439,1.,0.866025403784439,
1.,0.866025403784439,1.,0.866025403784439,1.,0.866025403784439,1.))
REPRESENTATION_ITEM('')
);
#4115=(
BOUNDED_CURVE()
B_SPLINE_CURVE(2,(#358577,#358578,#358579,#358580,#358581,#358582,#358583,
#358584,#358585,#358586,#358587,#358588,#358589),.UNSPECIFIED.,.F.,.F.)
B_SPLINE_CURVE_WITH_KNOTS((3,2,2,2,2,2,3),(0.924242424242424,0.929292929292929,
0.934343434343434,0.939393939393939,0.944444444444444,0.94949494949495,
0.954545454545455),.UNSPECIFIED.)
CURVE()
GEOMETRIC_REPRESENTATION_ITEM()
RATIONAL_B_SPLINE_CURVE((1.,0.866025403784439,1.,0.866025403784439,1.,0.866025403784439,
1.,0.866025403784439,1.,0.866025403784439,1.,0.866025403784439,1.))
REPRESENTATION_ITEM('')
);
#4116=(
BOUNDED_CURVE()
B_SPLINE_CURVE(2,(#358594,#358595,#358596,#358597,#358598,#358599,#358600,
#358601,#358602,#358603,#358604,#358605,#358606),.UNSPECIFIED.,.F.,.F.)
B_SPLINE_CURVE_WITH_KNOTS((3,2,2,2,2,2,3),(0.893939393939394,0.898989898989899,
0.904040404040404,0.909090909090909,0.914141414141414,0.919191919191919,
0.924242424242424),.UNSPECIFIED.)
CURVE()
GEOMETRIC_REPRESENTATION_ITEM()
RATIONAL_B_SPLINE_CURVE((1.,0.866025403784439,1.,0.866025403784439,1.,0.866025403784439,
1.,0.866025403784439,1.,0.866025403784439,1.,0.866025403784439,1.))
REPRESENTATION_ITEM('')
);
#4117=(
BOUNDED_CURVE()
B_SPLINE_CURVE(2,(#358607,#358608,#358609,#358610,#358611,#358612,#358613,
#358614,#358615,#358616,#358617,#358618,#358619),.UNSPECIFIED.,.F.,.F.)
B_SPLINE_CURVE_WITH_KNOTS((3,2,2,2,2,2,3),(0.893939393939394,0.898989898989899,
0.904040404040404,0.909090909090909,0.914141414141414,0.919191919191919,
0.924242424242424),.UNSPECIFIED.)
CURVE()
GEOMETRIC_REPRESENTATION_ITEM()
RATIONAL_B_SPLINE_CURVE((1.,0.866025403784439,1.,0.866025403784439,1.,0.866025403784439,
1.,0.866025403784439,1.,0.866025403784439,1.,0.866025403784439,1.))
REPRESENTATION_ITEM('')
);
#4118=(
BOUNDED_CURVE()
B_SPLINE_CURVE(2,(#358624,#358625,#358626,#358627,#358628,#358629,#358630,
#358631,#358632,#358633,#358634,#358635,#358636),.UNSPECIFIED.,.F.,.F.)
B_SPLINE_CURVE_WITH_KNOTS((3,2,2,2,2,2,3),(0.863636363636364,0.868686868686869,
0.873737373737374,0.878787878787879,0.883838383838384,0.888888888888889,
0.893939393939394),.UNSPECIFIED.)
CURVE()
GEOMETRIC_REPRESENTATION_ITEM()
RATIONAL_B_SPLINE_CURVE((1.,0.866025403784439,1.,0.866025403784439,1.,0.866025403784439,
1.,0.866025403784439,1.,0.866025403784439,1.,0.866025403784439,1.))
REPRESENTATION_ITEM('')
);
#4119=(
BOUNDED_CURVE()
B_SPLINE_CURVE(2,(#358637,#358638,#358639,#358640,#358641,#358642,#358643,
#358644,#358645,#358646,#358647,#358648,#358649),.UNSPECIFIED.,.F.,.F.)
B_SPLINE_CURVE_WITH_KNOTS((3,2,2,2,2,2,3),(0.863636363636364,0.868686868686869,
0.873737373737374,0.878787878787879,0.883838383838384,0.888888888888889,
0.893939393939394),.UNSPECIFIED.)
CURVE()
GEOMETRIC_REPRESENTATION_ITEM()
RATIONAL_B_SPLINE_CURVE((1.,0.866025403784439,1.,0.866025403784439,1.,0.866025403784439,
1.,0.866025403784439,1.,0.866025403784439,1.,0.866025403784439,1.))
REPRESENTATION_ITEM('')
);
#4120=(
BOUNDED_CURVE()
B_SPLINE_CURVE(2,(#358654,#358655,#358656,#358657,#358658,#358659,#358660,
#358661,#358662,#358663,#358664,#358665,#358666),.UNSPECIFIED.,.F.,.F.)
B_SPLINE_CURVE_WITH_KNOTS((3,2,2,2,2,2,3),(0.833333333333333,0.838383838383838,
0.843434343434343,0.848484848484849,0.853535353535353,0.858585858585859,
0.863636363636364),.UNSPECIFIED.)
CURVE()
GEOMETRIC_REPRESENTATION_ITEM()
RATIONAL_B_SPLINE_CURVE((1.,0.866025403784439,1.,0.866025403784439,1.,0.866025403784439,
1.,0.866025403784439,1.,0.866025403784439,1.,0.866025403784439,1.))
REPRESENTATION_ITEM('')
);
#4121=(
BOUNDED_CURVE()
B_SPLINE_CURVE(2,(#358667,#358668,#358669,#358670,#358671,#358672,#358673,
#358674,#358675,#358676,#358677,#358678,#358679),.UNSPECIFIED.,.F.,.F.)
B_SPLINE_CURVE_WITH_KNOTS((3,2,2,2,2,2,3),(0.833333333333333,0.838383838383838,
0.843434343434343,0.848484848484849,0.853535353535353,0.858585858585859,
0.863636363636364),.UNSPECIFIED.)
CURVE()
GEOMETRIC_REPRESENTATION_ITEM()
RATIONAL_B_SPLINE_CURVE((1.,0.866025403784439,1.,0.866025403784439,1.,0.866025403784439,
1.,0.866025403784439,1.,0.866025403784439,1.,0.866025403784439,1.))
REPRESENTATION_ITEM('')
);
#4122=(
BOUNDED_CURVE()
B_SPLINE_CURVE(2,(#358684,#358685,#358686,#358687,#358688,#358689,#358690,
#358691,#358692,#358693,#358694,#358695,#358696),.UNSPECIFIED.,.F.,.F.)
B_SPLINE_CURVE_WITH_KNOTS((3,2,2,2,2,2,3),(0.803030303030303,0.808080808080808,
0.813131313131313,0.818181818181818,0.823232323232323,0.828282828282828,
0.833333333333333),.UNSPECIFIED.)
CURVE()
GEOMETRIC_REPRESENTATION_ITEM()
RATIONAL_B_SPLINE_CURVE((1.,0.866025403784439,1.,0.866025403784439,1.,0.866025403784439,
1.,0.866025403784439,1.,0.866025403784439,1.,0.866025403784439,1.))
REPRESENTATION_ITEM('')
);
#4123=(
BOUNDED_CURVE()
B_SPLINE_CURVE(2,(#358697,#358698,#358699,#358700,#358701,#358702,#358703,
#358704,#358705,#358706,#358707,#358708,#358709),.UNSPECIFIED.,.F.,.F.)
B_SPLINE_CURVE_WITH_KNOTS((3,2,2,2,2,2,3),(0.803030303030303,0.808080808080808,
0.813131313131313,0.818181818181818,0.823232323232323,0.828282828282828,
0.833333333333333),.UNSPECIFIED.)
CURVE()
GEOMETRIC_REPRESENTATION_ITEM()
RATIONAL_B_SPLINE_CURVE((1.,0.866025403784439,1.,0.866025403784439,1.,0.866025403784439,
1.,0.866025403784439,1.,0.866025403784439,1.,0.866025403784439,1.))
REPRESENTATION_ITEM('')
);
#4124=(
BOUNDED_CURVE()
B_SPLINE_CURVE(2,(#358714,#358715,#358716,#358717,#358718,#358719,#358720,
#358721,#358722,#358723,#358724,#358725,#358726),.UNSPECIFIED.,.F.,.F.)
B_SPLINE_CURVE_WITH_KNOTS((3,2,2,2,2,2,3),(0.772727272727273,0.777777777777778,
0.782828282828283,0.787878787878788,0.792929292929293,0.797979797979798,
0.803030303030303),.UNSPECIFIED.)
CURVE()
GEOMETRIC_REPRESENTATION_ITEM()
RATIONAL_B_SPLINE_CURVE((1.,0.866025403784439,1.,0.866025403784439,1.,0.866025403784439,
1.,0.866025403784439,1.,0.866025403784439,1.,0.866025403784439,1.))
REPRESENTATION_ITEM('')
);
#4125=(
BOUNDED_CURVE()
B_SPLINE_CURVE(2,(#358727,#358728,#358729,#358730,#358731,#358732,#358733,
#358734,#358735,#358736,#358737,#358738,#358739),.UNSPECIFIED.,.F.,.F.)
B_SPLINE_CURVE_WITH_KNOTS((3,2,2,2,2,2,3),(0.772727272727273,0.777777777777778,
0.782828282828283,0.787878787878788,0.792929292929293,0.797979797979798,
0.803030303030303),.UNSPECIFIED.)
CURVE()
GEOMETRIC_REPRESENTATION_ITEM()
RATIONAL_B_SPLINE_CURVE((1.,0.866025403784439,1.,0.866025403784439,1.,0.866025403784439,
1.,0.866025403784439,1.,0.866025403784439,1.,0.866025403784439,1.))
REPRESENTATION_ITEM('')
);
#4126=(
BOUNDED_CURVE()
B_SPLINE_CURVE(2,(#358744,#358745,#358746,#358747,#358748,#358749,#358750,
#358751,#358752,#358753,#358754,#358755,#358756),.UNSPECIFIED.,.F.,.F.)
B_SPLINE_CURVE_WITH_KNOTS((3,2,2,2,2,2,3),(0.742424242424242,0.747474747474748,
0.752525252525252,0.757575757575758,0.762626262626263,0.767676767676768,
0.772727272727273),.UNSPECIFIED.)
CURVE()
GEOMETRIC_REPRESENTATION_ITEM()
RATIONAL_B_SPLINE_CURVE((1.,0.866025403784439,1.,0.866025403784439,1.,0.866025403784439,
1.,0.866025403784439,1.,0.866025403784439,1.,0.866025403784439,1.))
REPRESENTATION_ITEM('')
);
#4127=(
BOUNDED_CURVE()
B_SPLINE_CURVE(2,(#358757,#358758,#358759,#358760,#358761,#358762,#358763,
#358764,#358765,#358766,#358767,#358768,#358769),.UNSPECIFIED.,.F.,.F.)
B_SPLINE_CURVE_WITH_KNOTS((3,2,2,2,2,2,3),(0.742424242424242,0.747474747474748,
0.752525252525252,0.757575757575758,0.762626262626263,0.767676767676768,
0.772727272727273),.UNSPECIFIED.)
CURVE()
GEOMETRIC_REPRESENTATION_ITEM()
RATIONAL_B_SPLINE_CURVE((1.,0.866025403784439,1.,0.866025403784439,1.,0.866025403784439,
1.,0.866025403784439,1.,0.866025403784439,1.,0.866025403784439,1.))
REPRESENTATION_ITEM('')
);
#4128=(
BOUNDED_CURVE()
B_SPLINE_CURVE(2,(#358774,#358775,#358776,#358777,#358778,#358779,#358780,
#358781,#358782,#358783,#358784,#358785,#358786),.UNSPECIFIED.,.F.,.F.)
B_SPLINE_CURVE_WITH_KNOTS((3,2,2,2,2,2,3),(0.712121212121212,0.717171717171717,
0.722222222222222,0.727272727272727,0.732323232323232,0.737373737373737,
0.742424242424242),.UNSPECIFIED.)
CURVE()
GEOMETRIC_REPRESENTATION_ITEM()
RATIONAL_B_SPLINE_CURVE((1.,0.866025403784439,1.,0.866025403784439,1.,0.866025403784439,
1.,0.866025403784439,1.,0.866025403784439,1.,0.866025403784439,1.))
REPRESENTATION_ITEM('')
);
#4129=(
BOUNDED_CURVE()
B_SPLINE_CURVE(2,(#358787,#358788,#358789,#358790,#358791,#358792,#358793,
#358794,#358795,#358796,#358797,#358798,#358799),.UNSPECIFIED.,.F.,.F.)
B_SPLINE_CURVE_WITH_KNOTS((3,2,2,2,2,2,3),(0.712121212121212,0.717171717171717,
0.722222222222222,0.727272727272727,0.732323232323232,0.737373737373737,
0.742424242424242),.UNSPECIFIED.)
CURVE()
GEOMETRIC_REPRESENTATION_ITEM()
RATIONAL_B_SPLINE_CURVE((1.,0.866025403784439,1.,0.866025403784439,1.,0.866025403784439,
1.,0.866025403784439,1.,0.866025403784439,1.,0.866025403784439,1.))
REPRESENTATION_ITEM('')
);
#4130=(
BOUNDED_CURVE()
B_SPLINE_CURVE(2,(#358804,#358805,#358806,#358807,#358808,#358809,#358810,
#358811,#358812,#358813,#358814,#358815,#358816),.UNSPECIFIED.,.F.,.F.)
B_SPLINE_CURVE_WITH_KNOTS((3,2,2,2,2,2,3),(0.681818181818182,0.686868686868687,
0.691919191919192,0.696969696969697,0.702020202020202,0.707070707070707,
0.712121212121212),.UNSPECIFIED.)
CURVE()
GEOMETRIC_REPRESENTATION_ITEM()
RATIONAL_B_SPLINE_CURVE((1.,0.866025403784439,1.,0.866025403784439,1.,0.866025403784439,
1.,0.866025403784439,1.,0.866025403784439,1.,0.866025403784439,1.))
REPRESENTATION_ITEM('')
);
#4131=(
BOUNDED_CURVE()
B_SPLINE_CURVE(2,(#358817,#358818,#358819,#358820,#358821,#358822,#358823,
#358824,#358825,#358826,#358827,#358828,#358829),.UNSPECIFIED.,.F.,.F.)
B_SPLINE_CURVE_WITH_KNOTS((3,2,2,2,2,2,3),(0.681818181818182,0.686868686868687,
0.691919191919192,0.696969696969697,0.702020202020202,0.707070707070707,
0.712121212121212),.UNSPECIFIED.)
CURVE()
GEOMETRIC_REPRESENTATION_ITEM()
RATIONAL_B_SPLINE_CURVE((1.,0.866025403784439,1.,0.866025403784439,1.,0.866025403784439,
1.,0.866025403784439,1.,0.866025403784439,1.,0.866025403784439,1.))
REPRESENTATION_ITEM('')
);
#4132=(
BOUNDED_CURVE()
B_SPLINE_CURVE(2,(#358834,#358835,#358836,#358837,#358838,#358839,#358840,
#358841,#358842,#358843,#358844,#358845,#358846),.UNSPECIFIED.,.F.,.F.)
B_SPLINE_CURVE_WITH_KNOTS((3,2,2,2,2,2,3),(0.651515151515151,0.656565656565657,
0.661616161616162,0.666666666666667,0.671717171717172,0.676767676767677,
0.681818181818182),.UNSPECIFIED.)
CURVE()
GEOMETRIC_REPRESENTATION_ITEM()
RATIONAL_B_SPLINE_CURVE((1.,0.866025403784439,1.,0.866025403784439,1.,0.866025403784439,
1.,0.866025403784439,1.,0.866025403784439,1.,0.866025403784439,1.))
REPRESENTATION_ITEM('')
);
#4133=(
BOUNDED_CURVE()
B_SPLINE_CURVE(2,(#358847,#358848,#358849,#358850,#358851,#358852,#358853,
#358854,#358855,#358856,#358857,#358858,#358859),.UNSPECIFIED.,.F.,.F.)
B_SPLINE_CURVE_WITH_KNOTS((3,2,2,2,2,2,3),(0.651515151515151,0.656565656565656,
0.661616161616162,0.666666666666667,0.671717171717172,0.676767676767677,
0.681818181818182),.UNSPECIFIED.)
CURVE()
GEOMETRIC_REPRESENTATION_ITEM()
RATIONAL_B_SPLINE_CURVE((1.,0.866025403784439,1.,0.866025403784439,1.,0.866025403784439,
1.,0.866025403784439,1.,0.866025403784439,1.,0.866025403784439,1.))
REPRESENTATION_ITEM('')
);
#4134=(
BOUNDED_CURVE()
B_SPLINE_CURVE(2,(#358864,#358865,#358866,#358867,#358868,#358869,#358870,
#358871,#358872,#358873,#358874,#358875,#358876),.UNSPECIFIED.,.F.,.F.)
B_SPLINE_CURVE_WITH_KNOTS((3,2,2,2,2,2,3),(0.621212121212121,0.626262626262626,
0.631313131313131,0.636363636363636,0.641414141414141,0.646464646464647,
0.651515151515151),.UNSPECIFIED.)
CURVE()
GEOMETRIC_REPRESENTATION_ITEM()
RATIONAL_B_SPLINE_CURVE((1.,0.866025403784439,1.,0.866025403784439,1.,0.866025403784439,
1.,0.866025403784439,1.,0.866025403784439,1.,0.866025403784439,1.))
REPRESENTATION_ITEM('')
);
#4135=(
BOUNDED_CURVE()
B_SPLINE_CURVE(2,(#358877,#358878,#358879,#358880,#358881,#358882,#358883,
#358884,#358885,#358886,#358887,#358888,#358889),.UNSPECIFIED.,.F.,.F.)
B_SPLINE_CURVE_WITH_KNOTS((3,2,2,2,2,2,3),(0.621212121212121,0.626262626262626,
0.631313131313131,0.636363636363636,0.641414141414141,0.646464646464647,
0.651515151515151),.UNSPECIFIED.)
CURVE()
GEOMETRIC_REPRESENTATION_ITEM()
RATIONAL_B_SPLINE_CURVE((1.,0.866025403784439,1.,0.866025403784439,1.,0.866025403784439,
1.,0.866025403784439,1.,0.866025403784439,1.,0.866025403784439,1.))
REPRESENTATION_ITEM('')
);
#4136=(
BOUNDED_CURVE()
B_SPLINE_CURVE(2,(#358894,#358895,#358896,#358897,#358898,#358899,#358900,
#358901,#358902,#358903,#358904,#358905,#358906),.UNSPECIFIED.,.F.,.F.)
B_SPLINE_CURVE_WITH_KNOTS((3,2,2,2,2,2,3),(0.590909090909091,0.595959595959596,
0.601010101010101,0.606060606060606,0.611111111111111,0.616161616161616,
0.621212121212121),.UNSPECIFIED.)
CURVE()
GEOMETRIC_REPRESENTATION_ITEM()
RATIONAL_B_SPLINE_CURVE((1.,0.866025403784439,1.,0.866025403784439,1.,0.866025403784439,
1.,0.866025403784439,1.,0.866025403784439,1.,0.866025403784439,1.))
REPRESENTATION_ITEM('')
);
#4137=(
BOUNDED_CURVE()
B_SPLINE_CURVE(2,(#358907,#358908,#358909,#358910,#358911,#358912,#358913,
#358914,#358915,#358916,#358917,#358918,#358919),.UNSPECIFIED.,.F.,.F.)
B_SPLINE_CURVE_WITH_KNOTS((3,2,2,2,2,2,3),(0.590909090909091,0.595959595959596,
0.601010101010101,0.606060606060606,0.611111111111111,0.616161616161616,
0.621212121212121),.UNSPECIFIED.)
CURVE()
GEOMETRIC_REPRESENTATION_ITEM()
RATIONAL_B_SPLINE_CURVE((1.,0.866025403784439,1.,0.866025403784439,1.,0.866025403784439,
1.,0.866025403784439,1.,0.866025403784439,1.,0.866025403784439,1.))
REPRESENTATION_ITEM('')
);
#4138=(
BOUNDED_CURVE()
B_SPLINE_CURVE(2,(#358924,#358925,#358926,#358927,#358928,#358929,#358930,
#358931,#358932,#358933,#358934,#358935,#358936),.UNSPECIFIED.,.F.,.F.)
B_SPLINE_CURVE_WITH_KNOTS((3,2,2,2,2,2,3),(0.560606060606061,0.565656565656566,
0.570707070707071,0.575757575757576,0.580808080808081,0.585858585858586,
0.590909090909091),.UNSPECIFIED.)
CURVE()
GEOMETRIC_REPRESENTATION_ITEM()
RATIONAL_B_SPLINE_CURVE((1.,0.866025403784439,1.,0.866025403784439,1.,0.866025403784439,
1.,0.866025403784439,1.,0.866025403784439,1.,0.866025403784439,1.))
REPRESENTATION_ITEM('')
);
#4139=(
BOUNDED_CURVE()
B_SPLINE_CURVE(2,(#358937,#358938,#358939,#358940,#358941,#358942,#358943,
#358944,#358945,#358946,#358947,#358948,#358949),.UNSPECIFIED.,.F.,.F.)
B_SPLINE_CURVE_WITH_KNOTS((3,2,2,2,2,2,3),(0.560606060606061,0.565656565656566,
0.570707070707071,0.575757575757576,0.580808080808081,0.585858585858586,
0.590909090909091),.UNSPECIFIED.)
CURVE()
GEOMETRIC_REPRESENTATION_ITEM()
RATIONAL_B_SPLINE_CURVE((1.,0.866025403784439,1.,0.866025403784439,1.,0.866025403784439,
1.,0.866025403784439,1.,0.866025403784439,1.,0.866025403784439,1.))
REPRESENTATION_ITEM('')
);
#4140=(
BOUNDED_CURVE()
B_SPLINE_CURVE(2,(#358954,#358955,#358956,#358957,#358958,#358959,#358960,
#358961,#358962,#358963,#358964,#358965,#358966),.UNSPECIFIED.,.F.,.F.)
B_SPLINE_CURVE_WITH_KNOTS((3,2,2,2,2,2,3),(0.53030303030303,0.535353535353535,
0.54040404040404,0.545454545454545,0.55050505050505,0.555555555555556,0.560606060606061),
 .UNSPECIFIED.)
CURVE()
GEOMETRIC_REPRESENTATION_ITEM()
RATIONAL_B_SPLINE_CURVE((1.,0.866025403784439,1.,0.866025403784439,1.,0.866025403784439,
1.,0.866025403784439,1.,0.866025403784439,1.,0.866025403784439,1.))
REPRESENTATION_ITEM('')
);
#4141=(
BOUNDED_CURVE()
B_SPLINE_CURVE(2,(#358967,#358968,#358969,#358970,#358971,#358972,#358973,
#358974,#358975,#358976,#358977,#358978,#358979),.UNSPECIFIED.,.F.,.F.)
B_SPLINE_CURVE_WITH_KNOTS((3,2,2,2,2,2,3),(0.53030303030303,0.535353535353535,
0.54040404040404,0.545454545454545,0.550505050505051,0.555555555555556,
0.560606060606061),.UNSPECIFIED.)
CURVE()
GEOMETRIC_REPRESENTATION_ITEM()
RATIONAL_B_SPLINE_CURVE((1.,0.866025403784439,1.,0.866025403784439,1.,0.866025403784439,
1.,0.866025403784439,1.,0.866025403784439,1.,0.866025403784439,1.))
REPRESENTATION_ITEM('')
);
#4142=(
BOUNDED_CURVE()
B_SPLINE_CURVE(2,(#358984,#358985,#358986,#358987,#358988,#358989,#358990,
#358991,#358992,#358993,#358994,#358995,#358996),.UNSPECIFIED.,.F.,.F.)
B_SPLINE_CURVE_WITH_KNOTS((3,2,2,2,2,2,3),(0.5,0.505050505050505,0.51010101010101,
0.515151515151515,0.52020202020202,0.525252525252525,0.53030303030303),
 .UNSPECIFIED.)
CURVE()
GEOMETRIC_REPRESENTATION_ITEM()
RATIONAL_B_SPLINE_CURVE((1.,0.866025403784439,1.,0.866025403784439,1.,0.866025403784439,
1.,0.866025403784439,1.,0.866025403784439,1.,0.866025403784439,1.))
REPRESENTATION_ITEM('')
);
#4143=(
BOUNDED_CURVE()
B_SPLINE_CURVE(2,(#358997,#358998,#358999,#359000,#359001,#359002,#359003,
#359004,#359005,#359006,#359007,#359008,#359009),.UNSPECIFIED.,.F.,.F.)
B_SPLINE_CURVE_WITH_KNOTS((3,2,2,2,2,2,3),(0.5,0.505050505050505,0.51010101010101,
0.515151515151515,0.52020202020202,0.525252525252525,0.53030303030303),
 .UNSPECIFIED.)
CURVE()
GEOMETRIC_REPRESENTATION_ITEM()
RATIONAL_B_SPLINE_CURVE((1.,0.866025403784439,1.,0.866025403784439,1.,0.866025403784439,
1.,0.866025403784439,1.,0.866025403784439,1.,0.866025403784439,1.))
REPRESENTATION_ITEM('')
);
#4144=(
BOUNDED_CURVE()
B_SPLINE_CURVE(2,(#359014,#359015,#359016,#359017,#359018,#359019,#359020,
#359021,#359022,#359023,#359024,#359025,#359026),.UNSPECIFIED.,.F.,.F.)
B_SPLINE_CURVE_WITH_KNOTS((3,2,2,2,2,2,3),(0.46969696969697,0.474747474747475,
0.47979797979798,0.484848484848485,0.48989898989899,0.494949494949495,0.5),
 .UNSPECIFIED.)
CURVE()
GEOMETRIC_REPRESENTATION_ITEM()
RATIONAL_B_SPLINE_CURVE((1.,0.866025403784439,1.,0.866025403784439,1.,0.866025403784439,
1.,0.866025403784439,1.,0.866025403784439,1.,0.866025403784439,1.))
REPRESENTATION_ITEM('')
);
#4145=(
BOUNDED_CURVE()
B_SPLINE_CURVE(2,(#359027,#359028,#359029,#359030,#359031,#359032,#359033,
#359034,#359035,#359036,#359037,#359038,#359039),.UNSPECIFIED.,.F.,.F.)
B_SPLINE_CURVE_WITH_KNOTS((3,2,2,2,2,2,3),(0.46969696969697,0.474747474747475,
0.47979797979798,0.484848484848485,0.48989898989899,0.494949494949495,0.5),
 .UNSPECIFIED.)
CURVE()
GEOMETRIC_REPRESENTATION_ITEM()
RATIONAL_B_SPLINE_CURVE((1.,0.866025403784439,1.,0.866025403784439,1.,0.866025403784439,
1.,0.866025403784439,1.,0.866025403784439,1.,0.866025403784439,1.))
REPRESENTATION_ITEM('')
);
#4146=(
BOUNDED_CURVE()
B_SPLINE_CURVE(2,(#359044,#359045,#359046,#359047,#359048,#359049,#359050,
#359051,#359052,#359053,#359054,#359055,#359056),.UNSPECIFIED.,.F.,.F.)
B_SPLINE_CURVE_WITH_KNOTS((3,2,2,2,2,2,3),(0.439393939393939,0.444444444444444,
0.44949494949495,0.454545454545455,0.45959595959596,0.464646464646465,0.46969696969697),
 .UNSPECIFIED.)
CURVE()
GEOMETRIC_REPRESENTATION_ITEM()
RATIONAL_B_SPLINE_CURVE((1.,0.866025403784439,1.,0.866025403784439,1.,0.866025403784439,
1.,0.866025403784439,1.,0.866025403784439,1.,0.866025403784439,1.))
REPRESENTATION_ITEM('')
);
#4147=(
BOUNDED_CURVE()
B_SPLINE_CURVE(2,(#359057,#359058,#359059,#359060,#359061,#359062,#359063,
#359064,#359065,#359066,#359067,#359068,#359069),.UNSPECIFIED.,.F.,.F.)
B_SPLINE_CURVE_WITH_KNOTS((3,2,2,2,2,2,3),(0.439393939393939,0.444444444444444,
0.44949494949495,0.454545454545455,0.45959595959596,0.464646464646465,0.46969696969697),
 .UNSPECIFIED.)
CURVE()
GEOMETRIC_REPRESENTATION_ITEM()
RATIONAL_B_SPLINE_CURVE((1.,0.866025403784439,1.,0.866025403784439,1.,0.866025403784439,
1.,0.866025403784439,1.,0.866025403784439,1.,0.866025403784439,1.))
REPRESENTATION_ITEM('')
);
#4148=(
BOUNDED_CURVE()
B_SPLINE_CURVE(2,(#359074,#359075,#359076,#359077,#359078,#359079,#359080,
#359081,#359082,#359083,#359084,#359085,#359086),.UNSPECIFIED.,.F.,.F.)
B_SPLINE_CURVE_WITH_KNOTS((3,2,2,2,2,2,3),(0.409090909090909,0.414141414141414,
0.419191919191919,0.424242424242424,0.429292929292929,0.434343434343434,
0.439393939393939),.UNSPECIFIED.)
CURVE()
GEOMETRIC_REPRESENTATION_ITEM()
RATIONAL_B_SPLINE_CURVE((1.,0.866025403784439,1.,0.866025403784439,1.,0.866025403784439,
1.,0.866025403784439,1.,0.866025403784439,1.,0.866025403784439,1.))
REPRESENTATION_ITEM('')
);
#4149=(
BOUNDED_CURVE()
B_SPLINE_CURVE(2,(#359087,#359088,#359089,#359090,#359091,#359092,#359093,
#359094,#359095,#359096,#359097,#359098,#359099),.UNSPECIFIED.,.F.,.F.)
B_SPLINE_CURVE_WITH_KNOTS((3,2,2,2,2,2,3),(0.409090909090909,0.414141414141414,
0.419191919191919,0.424242424242424,0.429292929292929,0.434343434343434,
0.439393939393939),.UNSPECIFIED.)
CURVE()
GEOMETRIC_REPRESENTATION_ITEM()
RATIONAL_B_SPLINE_CURVE((1.,0.866025403784439,1.,0.866025403784439,1.,0.866025403784439,
1.,0.866025403784439,1.,0.866025403784439,1.,0.866025403784439,1.))
REPRESENTATION_ITEM('')
);
#4150=(
BOUNDED_CURVE()
B_SPLINE_CURVE(2,(#359104,#359105,#359106,#359107,#359108,#359109,#359110,
#359111,#359112,#359113,#359114,#359115,#359116),.UNSPECIFIED.,.F.,.F.)
B_SPLINE_CURVE_WITH_KNOTS((3,2,2,2,2,2,3),(0.378787878787879,0.383838383838384,
0.388888888888889,0.393939393939394,0.398989898989899,0.404040404040404,
0.409090909090909),.UNSPECIFIED.)
CURVE()
GEOMETRIC_REPRESENTATION_ITEM()
RATIONAL_B_SPLINE_CURVE((1.,0.866025403784439,1.,0.866025403784439,1.,0.866025403784439,
1.,0.866025403784439,1.,0.866025403784439,1.,0.866025403784439,1.))
REPRESENTATION_ITEM('')
);
#4151=(
BOUNDED_CURVE()
B_SPLINE_CURVE(2,(#359117,#359118,#359119,#359120,#359121,#359122,#359123,
#359124,#359125,#359126,#359127,#359128,#359129),.UNSPECIFIED.,.F.,.F.)
B_SPLINE_CURVE_WITH_KNOTS((3,2,2,2,2,2,3),(0.378787878787879,0.383838383838384,
0.388888888888889,0.393939393939394,0.398989898989899,0.404040404040404,
0.409090909090909),.UNSPECIFIED.)
CURVE()
GEOMETRIC_REPRESENTATION_ITEM()
RATIONAL_B_SPLINE_CURVE((1.,0.866025403784439,1.,0.866025403784439,1.,0.866025403784439,
1.,0.866025403784439,1.,0.866025403784439,1.,0.866025403784439,1.))
REPRESENTATION_ITEM('')
);
#4152=(
BOUNDED_CURVE()
B_SPLINE_CURVE(2,(#359134,#359135,#359136,#359137,#359138,#359139,#359140,
#359141,#359142,#359143,#359144,#359145,#359146),.UNSPECIFIED.,.F.,.F.)
B_SPLINE_CURVE_WITH_KNOTS((3,2,2,2,2,2,3),(0.348484848484849,0.353535353535354,
0.358585858585859,0.363636363636364,0.368686868686869,0.373737373737374,
0.378787878787879),.UNSPECIFIED.)
CURVE()
GEOMETRIC_REPRESENTATION_ITEM()
RATIONAL_B_SPLINE_CURVE((1.,0.866025403784439,1.,0.866025403784439,1.,0.866025403784439,
1.,0.866025403784439,1.,0.866025403784439,1.,0.866025403784439,1.))
REPRESENTATION_ITEM('')
);
#4153=(
BOUNDED_CURVE()
B_SPLINE_CURVE(2,(#359147,#359148,#359149,#359150,#359151,#359152,#359153,
#359154,#359155,#359156,#359157,#359158,#359159),.UNSPECIFIED.,.F.,.F.)
B_SPLINE_CURVE_WITH_KNOTS((3,2,2,2,2,2,3),(0.348484848484849,0.353535353535354,
0.358585858585859,0.363636363636364,0.368686868686869,0.373737373737374,
0.378787878787879),.UNSPECIFIED.)
CURVE()
GEOMETRIC_REPRESENTATION_ITEM()
RATIONAL_B_SPLINE_CURVE((1.,0.866025403784439,1.,0.866025403784439,1.,0.866025403784439,
1.,0.866025403784439,1.,0.866025403784439,1.,0.866025403784439,1.))
REPRESENTATION_ITEM('')
);
#4154=(
BOUNDED_CURVE()
B_SPLINE_CURVE(2,(#359164,#359165,#359166,#359167,#359168,#359169,#359170,
#359171,#359172,#359173,#359174,#359175,#359176),.UNSPECIFIED.,.F.,.F.)
B_SPLINE_CURVE_WITH_KNOTS((3,2,2,2,2,2,3),(0.318181818181818,0.323232323232323,
0.328282828282828,0.333333333333333,0.338383838383838,0.343434343434343,
0.348484848484849),.UNSPECIFIED.)
CURVE()
GEOMETRIC_REPRESENTATION_ITEM()
RATIONAL_B_SPLINE_CURVE((1.,0.866025403784439,1.,0.866025403784439,1.,0.866025403784439,
1.,0.866025403784439,1.,0.866025403784439,1.,0.866025403784439,1.))
REPRESENTATION_ITEM('')
);
#4155=(
BOUNDED_CURVE()
B_SPLINE_CURVE(2,(#359177,#359178,#359179,#359180,#359181,#359182,#359183,
#359184,#359185,#359186,#359187,#359188,#359189),.UNSPECIFIED.,.F.,.F.)
B_SPLINE_CURVE_WITH_KNOTS((3,2,2,2,2,2,3),(0.318181818181818,0.323232323232323,
0.328282828282828,0.333333333333333,0.338383838383838,0.343434343434343,
0.348484848484849),.UNSPECIFIED.)
CURVE()
GEOMETRIC_REPRESENTATION_ITEM()
RATIONAL_B_SPLINE_CURVE((1.,0.866025403784439,1.,0.866025403784439,1.,0.866025403784439,
1.,0.866025403784439,1.,0.866025403784439,1.,0.866025403784439,1.))
REPRESENTATION_ITEM('')
);
#4156=(
BOUNDED_CURVE()
B_SPLINE_CURVE(2,(#359194,#359195,#359196,#359197,#359198,#359199,#359200,
#359201,#359202,#359203,#359204,#359205,#359206),.UNSPECIFIED.,.F.,.F.)
B_SPLINE_CURVE_WITH_KNOTS((3,2,2,2,2,2,3),(0.287878787878788,0.292929292929293,
0.297979797979798,0.303030303030303,0.308080808080808,0.313131313131313,
0.318181818181818),.UNSPECIFIED.)
CURVE()
GEOMETRIC_REPRESENTATION_ITEM()
RATIONAL_B_SPLINE_CURVE((1.,0.866025403784439,1.,0.866025403784439,1.,0.866025403784439,
1.,0.866025403784439,1.,0.866025403784439,1.,0.866025403784439,1.))
REPRESENTATION_ITEM('')
);
#4157=(
BOUNDED_CURVE()
B_SPLINE_CURVE(2,(#359207,#359208,#359209,#359210,#359211,#359212,#359213,
#359214,#359215,#359216,#359217,#359218,#359219),.UNSPECIFIED.,.F.,.F.)
B_SPLINE_CURVE_WITH_KNOTS((3,2,2,2,2,2,3),(0.287878787878788,0.292929292929293,
0.297979797979798,0.303030303030303,0.308080808080808,0.313131313131313,
0.318181818181818),.UNSPECIFIED.)
CURVE()
GEOMETRIC_REPRESENTATION_ITEM()
RATIONAL_B_SPLINE_CURVE((1.,0.866025403784439,1.,0.866025403784439,1.,0.866025403784439,
1.,0.866025403784439,1.,0.866025403784439,1.,0.866025403784439,1.))
REPRESENTATION_ITEM('')
);
#4158=(
BOUNDED_CURVE()
B_SPLINE_CURVE(2,(#359224,#359225,#359226,#359227,#359228,#359229,#359230,
#359231,#359232,#359233,#359234,#359235,#359236),.UNSPECIFIED.,.F.,.F.)
B_SPLINE_CURVE_WITH_KNOTS((3,2,2,2,2,2,3),(0.257575757575758,0.262626262626263,
0.267676767676768,0.272727272727273,0.277777777777778,0.282828282828283,
0.287878787878788),.UNSPECIFIED.)
CURVE()
GEOMETRIC_REPRESENTATION_ITEM()
RATIONAL_B_SPLINE_CURVE((1.,0.866025403784439,1.,0.866025403784439,1.,0.866025403784439,
1.,0.866025403784439,1.,0.866025403784439,1.,0.866025403784439,1.))
REPRESENTATION_ITEM('')
);
#4159=(
BOUNDED_CURVE()
B_SPLINE_CURVE(2,(#359237,#359238,#359239,#359240,#359241,#359242,#359243,
#359244,#359245,#359246,#359247,#359248,#359249),.UNSPECIFIED.,.F.,.F.)
B_SPLINE_CURVE_WITH_KNOTS((3,2,2,2,2,2,3),(0.257575757575758,0.262626262626263,
0.267676767676768,0.272727272727273,0.277777777777778,0.282828282828283,
0.287878787878788),.UNSPECIFIED.)
CURVE()
GEOMETRIC_REPRESENTATION_ITEM()
RATIONAL_B_SPLINE_CURVE((1.,0.866025403784439,1.,0.866025403784439,1.,0.866025403784439,
1.,0.866025403784439,1.,0.866025403784439,1.,0.866025403784439,1.))
REPRESENTATION_ITEM('')
);
#4160=(
BOUNDED_CURVE()
B_SPLINE_CURVE(2,(#359254,#359255,#359256,#359257,#359258,#359259,#359260,
#359261,#359262,#359263,#359264,#359265,#359266),.UNSPECIFIED.,.F.,.F.)
B_SPLINE_CURVE_WITH_KNOTS((3,2,2,2,2,2,3),(0.227272727272727,0.232323232323232,
0.237373737373737,0.242424242424242,0.247474747474747,0.252525252525253,
0.257575757575758),.UNSPECIFIED.)
CURVE()
GEOMETRIC_REPRESENTATION_ITEM()
RATIONAL_B_SPLINE_CURVE((1.,0.866025403784439,1.,0.866025403784439,1.,0.866025403784439,
1.,0.866025403784439,1.,0.866025403784439,1.,0.866025403784439,1.))
REPRESENTATION_ITEM('')
);
#4161=(
BOUNDED_CURVE()
B_SPLINE_CURVE(2,(#359267,#359268,#359269,#359270,#359271,#359272,#359273,
#359274,#359275,#359276,#359277,#359278,#359279),.UNSPECIFIED.,.F.,.F.)
B_SPLINE_CURVE_WITH_KNOTS((3,2,2,2,2,2,3),(0.227272727272727,0.232323232323232,
0.237373737373737,0.242424242424242,0.247474747474747,0.252525252525253,
0.257575757575758),.UNSPECIFIED.)
CURVE()
GEOMETRIC_REPRESENTATION_ITEM()
RATIONAL_B_SPLINE_CURVE((1.,0.866025403784439,1.,0.866025403784439,1.,0.866025403784439,
1.,0.866025403784439,1.,0.866025403784439,1.,0.866025403784439,1.))
REPRESENTATION_ITEM('')
);
#4162=(
BOUNDED_CURVE()
B_SPLINE_CURVE(2,(#359284,#359285,#359286,#359287,#359288,#359289,#359290,
#359291,#359292,#359293,#359294,#359295,#359296),.UNSPECIFIED.,.F.,.F.)
B_SPLINE_CURVE_WITH_KNOTS((3,2,2,2,2,2,3),(0.196969696969697,0.202020202020202,
0.207070707070707,0.212121212121212,0.217171717171717,0.222222222222222,
0.227272727272727),.UNSPECIFIED.)
CURVE()
GEOMETRIC_REPRESENTATION_ITEM()
RATIONAL_B_SPLINE_CURVE((1.,0.866025403784439,1.,0.866025403784439,1.,0.866025403784439,
1.,0.866025403784439,1.,0.866025403784439,1.,0.866025403784439,1.))
REPRESENTATION_ITEM('')
);
#4163=(
BOUNDED_CURVE()
B_SPLINE_CURVE(2,(#359297,#359298,#359299,#359300,#359301,#359302,#359303,
#359304,#359305,#359306,#359307,#359308,#359309),.UNSPECIFIED.,.F.,.F.)
B_SPLINE_CURVE_WITH_KNOTS((3,2,2,2,2,2,3),(0.196969696969697,0.202020202020202,
0.207070707070707,0.212121212121212,0.217171717171717,0.222222222222222,
0.227272727272727),.UNSPECIFIED.)
CURVE()
GEOMETRIC_REPRESENTATION_ITEM()
RATIONAL_B_SPLINE_CURVE((1.,0.866025403784439,1.,0.866025403784439,1.,0.866025403784439,
1.,0.866025403784439,1.,0.866025403784439,1.,0.866025403784439,1.))
REPRESENTATION_ITEM('')
);
#4164=(
BOUNDED_CURVE()
B_SPLINE_CURVE(2,(#359314,#359315,#359316,#359317,#359318,#359319,#359320,
#359321,#359322,#359323,#359324,#359325,#359326),.UNSPECIFIED.,.F.,.F.)
B_SPLINE_CURVE_WITH_KNOTS((3,2,2,2,2,2,3),(0.166666666666667,0.171717171717172,
0.176767676767677,0.181818181818182,0.186868686868687,0.191919191919192,
0.196969696969697),.UNSPECIFIED.)
CURVE()
GEOMETRIC_REPRESENTATION_ITEM()
RATIONAL_B_SPLINE_CURVE((1.,0.866025403784439,1.,0.866025403784439,1.,0.866025403784439,
1.,0.866025403784439,1.,0.866025403784439,1.,0.866025403784439,1.))
REPRESENTATION_ITEM('')
);
#4165=(
BOUNDED_CURVE()
B_SPLINE_CURVE(2,(#359327,#359328,#359329,#359330,#359331,#359332,#359333,
#359334,#359335,#359336,#359337,#359338,#359339),.UNSPECIFIED.,.F.,.F.)
B_SPLINE_CURVE_WITH_KNOTS((3,2,2,2,2,2,3),(0.166666666666667,0.171717171717172,
0.176767676767677,0.181818181818182,0.186868686868687,0.191919191919192,
0.196969696969697),.UNSPECIFIED.)
CURVE()
GEOMETRIC_REPRESENTATION_ITEM()
RATIONAL_B_SPLINE_CURVE((1.,0.866025403784439,1.,0.866025403784439,1.,0.866025403784439,
1.,0.866025403784439,1.,0.866025403784439,1.,0.866025403784439,1.))
REPRESENTATION_ITEM('')
);
#4166=(
BOUNDED_CURVE()
B_SPLINE_CURVE(2,(#359344,#359345,#359346,#359347,#359348,#359349,#359350,
#359351,#359352,#359353,#359354,#359355,#359356),.UNSPECIFIED.,.F.,.F.)
B_SPLINE_CURVE_WITH_KNOTS((3,2,2,2,2,2,3),(0.136363636363636,0.141414141414141,
0.146464646464646,0.151515151515151,0.156565656565657,0.161616161616162,
0.166666666666667),.UNSPECIFIED.)
CURVE()
GEOMETRIC_REPRESENTATION_ITEM()
RATIONAL_B_SPLINE_CURVE((1.,0.866025403784439,1.,0.866025403784439,1.,0.866025403784439,
1.,0.866025403784439,1.,0.866025403784439,1.,0.866025403784439,1.))
REPRESENTATION_ITEM('')
);
#4167=(
BOUNDED_CURVE()
B_SPLINE_CURVE(2,(#359357,#359358,#359359,#359360,#359361,#359362,#359363,
#359364,#359365,#359366,#359367,#359368,#359369),.UNSPECIFIED.,.F.,.F.)
B_SPLINE_CURVE_WITH_KNOTS((3,2,2,2,2,2,3),(0.136363636363636,0.141414141414141,
0.146464646464646,0.151515151515152,0.156565656565657,0.161616161616162,
0.166666666666667),.UNSPECIFIED.)
CURVE()
GEOMETRIC_REPRESENTATION_ITEM()
RATIONAL_B_SPLINE_CURVE((1.,0.866025403784439,1.,0.866025403784439,1.,0.866025403784439,
1.,0.866025403784439,1.,0.866025403784439,1.,0.866025403784439,1.))
REPRESENTATION_ITEM('')
);
#4168=(
BOUNDED_CURVE()
B_SPLINE_CURVE(2,(#359374,#359375,#359376,#359377,#359378,#359379,#359380,
#359381,#359382,#359383,#359384,#359385,#359386),.UNSPECIFIED.,.F.,.F.)
B_SPLINE_CURVE_WITH_KNOTS((3,2,2,2,2,2,3),(0.106060606060606,0.111111111111111,
0.116161616161616,0.121212121212121,0.126262626262626,0.131313131313131,
0.136363636363636),.UNSPECIFIED.)
CURVE()
GEOMETRIC_REPRESENTATION_ITEM()
RATIONAL_B_SPLINE_CURVE((1.,0.866025403784439,1.,0.866025403784439,1.,0.866025403784439,
1.,0.866025403784439,1.,0.866025403784439,1.,0.866025403784439,1.))
REPRESENTATION_ITEM('')
);
#4169=(
BOUNDED_CURVE()
B_SPLINE_CURVE(2,(#359387,#359388,#359389,#359390,#359391,#359392,#359393,
#359394,#359395,#359396,#359397,#359398,#359399),.UNSPECIFIED.,.F.,.F.)
B_SPLINE_CURVE_WITH_KNOTS((3,2,2,2,2,2,3),(0.106060606060606,0.111111111111111,
0.116161616161616,0.121212121212121,0.126262626262626,0.131313131313131,
0.136363636363636),.UNSPECIFIED.)
CURVE()
GEOMETRIC_REPRESENTATION_ITEM()
RATIONAL_B_SPLINE_CURVE((1.,0.866025403784439,1.,0.866025403784439,1.,0.866025403784439,
1.,0.866025403784439,1.,0.866025403784439,1.,0.866025403784439,1.))
REPRESENTATION_ITEM('')
);
#4170=(
BOUNDED_CURVE()
B_SPLINE_CURVE(2,(#359404,#359405,#359406,#359407,#359408,#359409,#359410,
#359411,#359412,#359413,#359414,#359415,#359416),.UNSPECIFIED.,.F.,.F.)
B_SPLINE_CURVE_WITH_KNOTS((3,2,2,2,2,2,3),(0.0757575757575758,0.0808080808080808,
0.0858585858585859,0.0909090909090909,0.095959595959596,0.101010101010101,
0.106060606060606),.UNSPECIFIED.)
CURVE()
GEOMETRIC_REPRESENTATION_ITEM()
RATIONAL_B_SPLINE_CURVE((1.,0.866025403784439,1.,0.866025403784439,1.,0.866025403784439,
1.,0.866025403784439,1.,0.866025403784439,1.,0.866025403784439,1.))
REPRESENTATION_ITEM('')
);
#4171=(
BOUNDED_CURVE()
B_SPLINE_CURVE(2,(#359417,#359418,#359419,#359420,#359421,#359422,#359423,
#359424,#359425,#359426,#359427,#359428,#359429),.UNSPECIFIED.,.F.,.F.)
B_SPLINE_CURVE_WITH_KNOTS((3,2,2,2,2,2,3),(0.0757575757575758,0.0808080808080808,
0.0858585858585859,0.0909090909090909,0.095959595959596,0.101010101010101,
0.106060606060606),.UNSPECIFIED.)
CURVE()
GEOMETRIC_REPRESENTATION_ITEM()
RATIONAL_B_SPLINE_CURVE((1.,0.866025403784439,1.,0.866025403784439,1.,0.866025403784439,
1.,0.866025403784439,1.,0.866025403784439,1.,0.866025403784439,1.))
REPRESENTATION_ITEM('')
);
#4172=(
BOUNDED_CURVE()
B_SPLINE_CURVE(2,(#359434,#359435,#359436,#359437,#359438,#359439,#359440,
#359441,#359442,#359443,#359444,#359445,#359446),.UNSPECIFIED.,.F.,.F.)
B_SPLINE_CURVE_WITH_KNOTS((3,2,2,2,2,2,3),(0.0454545454545455,0.0505050505050505,
0.0555555555555556,0.0606060606060606,0.0656565656565657,0.0707070707070707,
0.0757575757575758),.UNSPECIFIED.)
CURVE()
GEOMETRIC_REPRESENTATION_ITEM()
RATIONAL_B_SPLINE_CURVE((1.,0.866025403784439,1.,0.866025403784439,1.,0.866025403784439,
1.,0.866025403784439,1.,0.866025403784439,1.,0.866025403784439,1.))
REPRESENTATION_ITEM('')
);
#4173=(
BOUNDED_CURVE()
B_SPLINE_CURVE(2,(#359447,#359448,#359449,#359450,#359451,#359452,#359453,
#359454,#359455,#359456,#359457,#359458,#359459),.UNSPECIFIED.,.F.,.F.)
B_SPLINE_CURVE_WITH_KNOTS((3,2,2,2,2,2,3),(0.0454545454545455,0.0505050505050505,
0.0555555555555556,0.0606060606060606,0.0656565656565657,0.0707070707070707,
0.0757575757575758),.UNSPECIFIED.)
CURVE()
GEOMETRIC_REPRESENTATION_ITEM()
RATIONAL_B_SPLINE_CURVE((1.,0.866025403784439,1.,0.866025403784439,1.,0.866025403784439,
1.,0.866025403784439,1.,0.866025403784439,1.,0.866025403784439,1.))
REPRESENTATION_ITEM('')
);
#4174=(
BOUNDED_CURVE()
B_SPLINE_CURVE(2,(#359466,#359467,#359468,#359469,#359470,#359471,#359472,
#359473,#359474,#359475,#359476,#359477,#359478),.UNSPECIFIED.,.F.,.F.)
B_SPLINE_CURVE_WITH_KNOTS((3,2,2,2,2,2,3),(0.0181628739236012,0.0202020202020202,
0.0252525252525253,0.0303030303030303,0.0353535353535354,0.0404040404040404,
0.0454545454545455),.UNSPECIFIED.)
CURVE()
GEOMETRIC_REPRESENTATION_ITEM()
RATIONAL_B_SPLINE_CURVE((0.935494950279675,0.945907627743422,1.,0.866025403784439,
1.,0.866025403784439,1.,0.866025403784439,1.,0.866025403784439,1.,0.866025403784439,
1.))
REPRESENTATION_ITEM('')
);
#4175=(
BOUNDED_CURVE()
B_SPLINE_CURVE(2,(#359479,#359480,#359481,#359482,#359483,#359484,#359485,
#359486,#359487,#359488,#359489,#359490,#359491),.UNSPECIFIED.,.F.,.F.)
B_SPLINE_CURVE_WITH_KNOTS((3,2,2,2,2,2,3),(0.0151515151515152,0.0202020202020202,
0.0252525252525253,0.0303030303030303,0.0353535353535354,0.0404040404040404,
0.0454545454545455),.UNSPECIFIED.)
CURVE()
GEOMETRIC_REPRESENTATION_ITEM()
RATIONAL_B_SPLINE_CURVE((1.,0.866025403784439,1.,0.866025403784439,1.,0.866025403784439,
1.,0.866025403784439,1.,0.866025403784439,1.,0.866025403784439,1.))
REPRESENTATION_ITEM('')
);
#4176=(
BOUNDED_CURVE()
B_SPLINE_CURVE(2,(#359497,#359498,#359499,#359500,#359501,#359502,#359503),
 .UNSPECIFIED.,.F.,.F.)
B_SPLINE_CURVE_WITH_KNOTS((3,2,2,3),(0.954545454545455,0.95959595959596,
0.964646464646465,0.96969696969697),.UNSPECIFIED.)
CURVE()
GEOMETRIC_REPRESENTATION_ITEM()
RATIONAL_B_SPLINE_CURVE((1.,0.866025403784439,1.,0.866025403784439,1.,0.866025403784439,
1.))
REPRESENTATION_ITEM('')
);
#4177=(
BOUNDED_CURVE()
B_SPLINE_CURVE(2,(#361825,#361826,#361827),.UNSPECIFIED.,.F.,.F.)
B_SPLINE_CURVE_WITH_KNOTS((3,3),(0.124274873543865,0.321867155116299),
 .UNSPECIFIED.)
CURVE()
GEOMETRIC_REPRESENTATION_ITEM()
RATIONAL_B_SPLINE_CURVE((1.46410161513778,1.69059892324148,1.46410161513778))
REPRESENTATION_ITEM('')
);
#4178=(
BOUNDED_CURVE()
B_SPLINE_CURVE(2,(#361924,#361925,#361926,#361927,#361928,#361929,#361930),
 .UNSPECIFIED.,.F.,.F.)
B_SPLINE_CURVE_WITH_KNOTS((3,2,2,3),(0.0491768500135387,0.0505050505050505,
0.0555555555555556,0.0606060606060607),.UNSPECIFIED.)
CURVE()
GEOMETRIC_REPRESENTATION_ITEM()
RATIONAL_B_SPLINE_CURVE((0.948065210722613,0.964766865340365,1.,0.866025403784439,
1.,0.866025403784437,1.))
REPRESENTATION_ITEM('')
);
#4179=(
BOUNDED_CURVE()
B_SPLINE_CURVE(2,(#362007,#362008,#362009),.UNSPECIFIED.,.F.,.F.)
B_SPLINE_CURVE_WITH_KNOTS((3,3),(-0.3218671551163,-0.124274873543866),
 .UNSPECIFIED.)
CURVE()
GEOMETRIC_REPRESENTATION_ITEM()
RATIONAL_B_SPLINE_CURVE((1.46410161513778,1.69059892324148,1.46410161513778))
REPRESENTATION_ITEM('')
);
#4180=(
BOUNDED_CURVE()
B_SPLINE_CURVE(2,(#362011,#362012,#362013),.UNSPECIFIED.,.F.,.F.)
B_SPLINE_CURVE_WITH_KNOTS((3,3),(-0.321867155116299,-0.124274873543865),
 .UNSPECIFIED.)
CURVE()
GEOMETRIC_REPRESENTATION_ITEM()
RATIONAL_B_SPLINE_CURVE((1.46410161513778,1.69059892324148,1.46410161513778))
REPRESENTATION_ITEM('')
);
#4181=(
BOUNDED_CURVE()
B_SPLINE_CURVE(2,(#362015,#362016,#362017),.UNSPECIFIED.,.F.,.F.)
B_SPLINE_CURVE_WITH_KNOTS((3,3),(-0.321867155116299,-0.124274873543865),
 .UNSPECIFIED.)
CURVE()
GEOMETRIC_REPRESENTATION_ITEM()
RATIONAL_B_SPLINE_CURVE((1.46410161513778,1.69059892324148,1.46410161513778))
REPRESENTATION_ITEM('')
);
#4182=(
BOUNDED_CURVE()
B_SPLINE_CURVE(2,(#362019,#362020,#362021),.UNSPECIFIED.,.F.,.F.)
B_SPLINE_CURVE_WITH_KNOTS((3,3),(-0.321867155116299,-0.124274873543865),
 .UNSPECIFIED.)
CURVE()
GEOMETRIC_REPRESENTATION_ITEM()
RATIONAL_B_SPLINE_CURVE((1.46410161513778,1.69059892324148,1.46410161513778))
REPRESENTATION_ITEM('')
);
#4183=(
BOUNDED_CURVE()
B_SPLINE_CURVE(2,(#362023,#362024,#362025),.UNSPECIFIED.,.F.,.F.)
B_SPLINE_CURVE_WITH_KNOTS((3,3),(-0.321867155116299,-0.124274873543865),
 .UNSPECIFIED.)
CURVE()
GEOMETRIC_REPRESENTATION_ITEM()
RATIONAL_B_SPLINE_CURVE((1.46410161513778,1.69059892324148,1.46410161513778))
REPRESENTATION_ITEM('')
);
#4184=(
BOUNDED_CURVE()
B_SPLINE_CURVE(2,(#362846,#362847,#362848),.UNSPECIFIED.,.F.,.F.)
B_SPLINE_CURVE_WITH_KNOTS((3,3),(0.0143443920644589,0.0151515151515152),
 .UNSPECIFIED.)
CURVE()
GEOMETRIC_REPRESENTATION_ITEM()
RATIONAL_B_SPLINE_CURVE((0.964022189566691,0.978589470042445,1.))
REPRESENTATION_ITEM('')
);
#4185=(
BOUNDED_CURVE()
B_SPLINE_CURVE(2,(#366331,#366332,#366333),.UNSPECIFIED.,.F.,.F.)
B_SPLINE_CURVE_WITH_KNOTS((3,3),(0.0278449963604202,0.0294117647058824),
 .UNSPECIFIED.)
CURVE()
GEOMETRIC_REPRESENTATION_ITEM()
RATIONAL_B_SPLINE_CURVE((0.964022189566693,0.978589470042446,1.))
REPRESENTATION_ITEM('')
);
#4186=(
BOUNDED_CURVE()
B_SPLINE_CURVE(2,(#366339,#366340,#366341,#366342,#366343,#366344,#366345,
#366346,#366347,#366348,#366349,#366350,#366351),.UNSPECIFIED.,.F.,.F.)
B_SPLINE_CURVE_WITH_KNOTS((3,2,2,2,2,2,3),(0.0294117647058824,0.0392156862745098,
0.0490196078431373,0.0588235294117647,0.0686274509803922,0.0784313725490196,
0.0882352941176471),.UNSPECIFIED.)
CURVE()
GEOMETRIC_REPRESENTATION_ITEM()
RATIONAL_B_SPLINE_CURVE((1.,0.866025403784439,1.,0.866025403784439,1.,0.866025403784439,
1.,0.866025403784439,1.,0.866025403784439,1.,0.866025403784439,1.))
REPRESENTATION_ITEM('')
);
#4187=(
BOUNDED_CURVE()
B_SPLINE_CURVE(2,(#366354,#366355,#366356,#366357,#366358,#366359,#366360,
#366361,#366362,#366363,#366364,#366365,#366366),.UNSPECIFIED.,.F.,.F.)
B_SPLINE_CURVE_WITH_KNOTS((3,2,2,2,2,2,3),(0.035257343498756,0.0392156862745098,
0.0490196078431373,0.0588235294117647,0.0686274509803922,0.0784313725490196,
0.0882352941176471),.UNSPECIFIED.)
CURVE()
GEOMETRIC_REPRESENTATION_ITEM()
RATIONAL_B_SPLINE_CURVE((0.935494950279678,0.945907627743432,1.,0.866025403784439,
1.,0.866025403784439,1.,0.866025403784439,1.,0.866025403784439,1.,0.866025403784439,
1.))
REPRESENTATION_ITEM('')
);
#4188=(
BOUNDED_CURVE()
B_SPLINE_CURVE(2,(#366371,#366372,#366373,#366374,#366375,#366376,#366377,
#366378,#366379,#366380,#366381,#366382,#366383),.UNSPECIFIED.,.F.,.F.)
B_SPLINE_CURVE_WITH_KNOTS((3,2,2,2,2,2,3),(0.0882352941176471,0.0980392156862745,
0.107843137254902,0.117647058823529,0.127450980392157,0.137254901960784,
0.147058823529412),.UNSPECIFIED.)
CURVE()
GEOMETRIC_REPRESENTATION_ITEM()
RATIONAL_B_SPLINE_CURVE((1.,0.866025403784439,1.,0.866025403784439,1.,0.866025403784439,
1.,0.866025403784439,1.,0.866025403784439,1.,0.866025403784439,1.))
REPRESENTATION_ITEM('')
);
#4189=(
BOUNDED_CURVE()
B_SPLINE_CURVE(2,(#366384,#366385,#366386,#366387,#366388,#366389,#366390,
#366391,#366392,#366393,#366394,#366395,#366396),.UNSPECIFIED.,.F.,.F.)
B_SPLINE_CURVE_WITH_KNOTS((3,2,2,2,2,2,3),(0.0882352941176471,0.0980392156862745,
0.107843137254902,0.117647058823529,0.127450980392157,0.137254901960784,
0.147058823529412),.UNSPECIFIED.)
CURVE()
GEOMETRIC_REPRESENTATION_ITEM()
RATIONAL_B_SPLINE_CURVE((1.,0.866025403784439,1.,0.866025403784439,1.,0.866025403784439,
1.,0.866025403784439,1.,0.866025403784439,1.,0.866025403784439,1.))
REPRESENTATION_ITEM('')
);
#4190=(
BOUNDED_CURVE()
B_SPLINE_CURVE(2,(#366401,#366402,#366403,#366404,#366405,#366406,#366407,
#366408,#366409,#366410,#366411,#366412,#366413),.UNSPECIFIED.,.F.,.F.)
B_SPLINE_CURVE_WITH_KNOTS((3,2,2,2,2,2,3),(0.147058823529412,0.156862745098039,
0.166666666666667,0.176470588235294,0.186274509803922,0.196078431372549,
0.205882352941176),.UNSPECIFIED.)
CURVE()
GEOMETRIC_REPRESENTATION_ITEM()
RATIONAL_B_SPLINE_CURVE((1.,0.866025403784439,1.,0.866025403784439,1.,0.866025403784439,
1.,0.866025403784439,1.,0.866025403784439,1.,0.866025403784439,1.))
REPRESENTATION_ITEM('')
);
#4191=(
BOUNDED_CURVE()
B_SPLINE_CURVE(2,(#366414,#366415,#366416,#366417,#366418,#366419,#366420,
#366421,#366422,#366423,#366424,#366425,#366426),.UNSPECIFIED.,.F.,.F.)
B_SPLINE_CURVE_WITH_KNOTS((3,2,2,2,2,2,3),(0.147058823529412,0.156862745098039,
0.166666666666667,0.176470588235294,0.186274509803922,0.196078431372549,
0.205882352941177),.UNSPECIFIED.)
CURVE()
GEOMETRIC_REPRESENTATION_ITEM()
RATIONAL_B_SPLINE_CURVE((1.,0.866025403784439,1.,0.866025403784439,1.,0.866025403784439,
1.,0.866025403784439,1.,0.866025403784439,1.,0.866025403784439,1.))
REPRESENTATION_ITEM('')
);
#4192=(
BOUNDED_CURVE()
B_SPLINE_CURVE(2,(#366431,#366432,#366433,#366434,#366435,#366436,#366437,
#366438,#366439,#366440,#366441,#366442,#366443),.UNSPECIFIED.,.F.,.F.)
B_SPLINE_CURVE_WITH_KNOTS((3,2,2,2,2,2,3),(0.205882352941176,0.215686274509804,
0.225490196078431,0.235294117647059,0.245098039215686,0.254901960784314,
0.264705882352941),.UNSPECIFIED.)
CURVE()
GEOMETRIC_REPRESENTATION_ITEM()
RATIONAL_B_SPLINE_CURVE((1.,0.866025403784439,1.,0.866025403784439,1.,0.866025403784439,
1.,0.866025403784439,1.,0.866025403784439,1.,0.866025403784439,1.))
REPRESENTATION_ITEM('')
);
#4193=(
BOUNDED_CURVE()
B_SPLINE_CURVE(2,(#366444,#366445,#366446,#366447,#366448,#366449,#366450,
#366451,#366452,#366453,#366454,#366455,#366456),.UNSPECIFIED.,.F.,.F.)
B_SPLINE_CURVE_WITH_KNOTS((3,2,2,2,2,2,3),(0.205882352941177,0.215686274509804,
0.225490196078431,0.235294117647059,0.245098039215686,0.254901960784314,
0.264705882352941),.UNSPECIFIED.)
CURVE()
GEOMETRIC_REPRESENTATION_ITEM()
RATIONAL_B_SPLINE_CURVE((1.,0.866025403784439,1.,0.866025403784439,1.,0.866025403784439,
1.,0.866025403784439,1.,0.866025403784439,1.,0.866025403784439,1.))
REPRESENTATION_ITEM('')
);
#4194=(
BOUNDED_CURVE()
B_SPLINE_CURVE(2,(#366461,#366462,#366463,#366464,#366465,#366466,#366467,
#366468,#366469,#366470,#366471,#366472,#366473),.UNSPECIFIED.,.F.,.F.)
B_SPLINE_CURVE_WITH_KNOTS((3,2,2,2,2,2,3),(0.264705882352941,0.274509803921569,
0.284313725490196,0.294117647058824,0.303921568627451,0.313725490196078,
0.323529411764706),.UNSPECIFIED.)
CURVE()
GEOMETRIC_REPRESENTATION_ITEM()
RATIONAL_B_SPLINE_CURVE((1.,0.866025403784439,1.,0.866025403784439,1.,0.866025403784439,
1.,0.866025403784439,1.,0.866025403784439,1.,0.866025403784439,1.))
REPRESENTATION_ITEM('')
);
#4195=(
BOUNDED_CURVE()
B_SPLINE_CURVE(2,(#366474,#366475,#366476,#366477,#366478,#366479,#366480,
#366481,#366482,#366483,#366484,#366485,#366486),.UNSPECIFIED.,.F.,.F.)
B_SPLINE_CURVE_WITH_KNOTS((3,2,2,2,2,2,3),(0.264705882352941,0.274509803921569,
0.284313725490196,0.294117647058824,0.303921568627451,0.313725490196078,
0.323529411764706),.UNSPECIFIED.)
CURVE()
GEOMETRIC_REPRESENTATION_ITEM()
RATIONAL_B_SPLINE_CURVE((1.,0.866025403784439,1.,0.866025403784439,1.,0.866025403784439,
1.,0.866025403784439,1.,0.866025403784439,1.,0.866025403784439,1.))
REPRESENTATION_ITEM('')
);
#4196=(
BOUNDED_CURVE()
B_SPLINE_CURVE(2,(#366491,#366492,#366493,#366494,#366495,#366496,#366497,
#366498,#366499,#366500,#366501,#366502,#366503),.UNSPECIFIED.,.F.,.F.)
B_SPLINE_CURVE_WITH_KNOTS((3,2,2,2,2,2,3),(0.323529411764706,0.333333333333333,
0.343137254901961,0.352941176470588,0.362745098039216,0.372549019607843,
0.382352941176471),.UNSPECIFIED.)
CURVE()
GEOMETRIC_REPRESENTATION_ITEM()
RATIONAL_B_SPLINE_CURVE((1.,0.866025403784439,1.,0.866025403784439,1.,0.866025403784439,
1.,0.866025403784439,1.,0.866025403784439,1.,0.866025403784439,1.))
REPRESENTATION_ITEM('')
);
#4197=(
BOUNDED_CURVE()
B_SPLINE_CURVE(2,(#366504,#366505,#366506,#366507,#366508,#366509,#366510,
#366511,#366512,#366513,#366514,#366515,#366516),.UNSPECIFIED.,.F.,.F.)
B_SPLINE_CURVE_WITH_KNOTS((3,2,2,2,2,2,3),(0.323529411764706,0.333333333333333,
0.343137254901961,0.352941176470588,0.362745098039216,0.372549019607843,
0.382352941176471),.UNSPECIFIED.)
CURVE()
GEOMETRIC_REPRESENTATION_ITEM()
RATIONAL_B_SPLINE_CURVE((1.,0.866025403784439,1.,0.866025403784439,1.,0.866025403784439,
1.,0.866025403784439,1.,0.866025403784439,1.,0.866025403784439,1.))
REPRESENTATION_ITEM('')
);
#4198=(
BOUNDED_CURVE()
B_SPLINE_CURVE(2,(#366521,#366522,#366523,#366524,#366525,#366526,#366527,
#366528,#366529,#366530,#366531,#366532,#366533),.UNSPECIFIED.,.F.,.F.)
B_SPLINE_CURVE_WITH_KNOTS((3,2,2,2,2,2,3),(0.382352941176471,0.392156862745098,
0.401960784313726,0.411764705882353,0.42156862745098,0.431372549019608,
0.441176470588235),.UNSPECIFIED.)
CURVE()
GEOMETRIC_REPRESENTATION_ITEM()
RATIONAL_B_SPLINE_CURVE((1.,0.866025403784439,1.,0.866025403784439,1.,0.866025403784439,
1.,0.866025403784439,1.,0.866025403784439,1.,0.866025403784439,1.))
REPRESENTATION_ITEM('')
);
#4199=(
BOUNDED_CURVE()
B_SPLINE_CURVE(2,(#366534,#366535,#366536,#366537,#366538,#366539,#366540,
#366541,#366542,#366543,#366544,#366545,#366546),.UNSPECIFIED.,.F.,.F.)
B_SPLINE_CURVE_WITH_KNOTS((3,2,2,2,2,2,3),(0.382352941176471,0.392156862745098,
0.401960784313726,0.411764705882353,0.421568627450981,0.431372549019608,
0.441176470588235),.UNSPECIFIED.)
CURVE()
GEOMETRIC_REPRESENTATION_ITEM()
RATIONAL_B_SPLINE_CURVE((1.,0.866025403784439,1.,0.866025403784439,1.,0.866025403784439,
1.,0.866025403784439,1.,0.866025403784439,1.,0.866025403784439,1.))
REPRESENTATION_ITEM('')
);
#4200=(
BOUNDED_CURVE()
B_SPLINE_CURVE(2,(#366551,#366552,#366553,#366554,#366555,#366556,#366557,
#366558,#366559,#366560,#366561,#366562,#366563),.UNSPECIFIED.,.F.,.F.)
B_SPLINE_CURVE_WITH_KNOTS((3,2,2,2,2,2,3),(0.441176470588235,0.450980392156863,
0.46078431372549,0.470588235294118,0.480392156862745,0.490196078431373,
0.5),.UNSPECIFIED.)
CURVE()
GEOMETRIC_REPRESENTATION_ITEM()
RATIONAL_B_SPLINE_CURVE((1.,0.866025403784439,1.,0.866025403784439,1.,0.866025403784439,
1.,0.866025403784439,1.,0.866025403784439,1.,0.866025403784439,1.))
REPRESENTATION_ITEM('')
);
#4201=(
BOUNDED_CURVE()
B_SPLINE_CURVE(2,(#366564,#366565,#366566,#366567,#366568,#366569,#366570,
#366571,#366572,#366573,#366574,#366575,#366576),.UNSPECIFIED.,.F.,.F.)
B_SPLINE_CURVE_WITH_KNOTS((3,2,2,2,2,2,3),(0.441176470588235,0.450980392156863,
0.46078431372549,0.470588235294118,0.480392156862745,0.490196078431373,
0.5),.UNSPECIFIED.)
CURVE()
GEOMETRIC_REPRESENTATION_ITEM()
RATIONAL_B_SPLINE_CURVE((1.,0.866025403784439,1.,0.866025403784439,1.,0.866025403784439,
1.,0.866025403784439,1.,0.866025403784439,1.,0.866025403784439,1.))
REPRESENTATION_ITEM('')
);
#4202=(
BOUNDED_CURVE()
B_SPLINE_CURVE(2,(#366581,#366582,#366583,#366584,#366585,#366586,#366587,
#366588,#366589,#366590,#366591,#366592,#366593),.UNSPECIFIED.,.F.,.F.)
B_SPLINE_CURVE_WITH_KNOTS((3,2,2,2,2,2,3),(0.5,0.509803921568627,0.519607843137255,
0.529411764705882,0.53921568627451,0.549019607843137,0.558823529411765),
 .UNSPECIFIED.)
CURVE()
GEOMETRIC_REPRESENTATION_ITEM()
RATIONAL_B_SPLINE_CURVE((1.,0.866025403784439,1.,0.866025403784439,1.,0.866025403784439,
1.,0.866025403784439,1.,0.866025403784439,1.,0.866025403784439,1.))
REPRESENTATION_ITEM('')
);
#4203=(
BOUNDED_CURVE()
B_SPLINE_CURVE(2,(#366594,#366595,#366596,#366597,#366598,#366599,#366600,
#366601,#366602,#366603,#366604,#366605,#366606),.UNSPECIFIED.,.F.,.F.)
B_SPLINE_CURVE_WITH_KNOTS((3,2,2,2,2,2,3),(0.5,0.509803921568628,0.519607843137255,
0.529411764705882,0.53921568627451,0.549019607843137,0.558823529411765),
 .UNSPECIFIED.)
CURVE()
GEOMETRIC_REPRESENTATION_ITEM()
RATIONAL_B_SPLINE_CURVE((1.,0.866025403784439,1.,0.866025403784439,1.,0.866025403784439,
1.,0.866025403784439,1.,0.866025403784439,1.,0.866025403784439,1.))
REPRESENTATION_ITEM('')
);
#4204=(
BOUNDED_CURVE()
B_SPLINE_CURVE(2,(#366611,#366612,#366613,#366614,#366615,#366616,#366617,
#366618,#366619,#366620,#366621,#366622,#366623),.UNSPECIFIED.,.F.,.F.)
B_SPLINE_CURVE_WITH_KNOTS((3,2,2,2,2,2,3),(0.558823529411765,0.568627450980392,
0.57843137254902,0.588235294117647,0.598039215686274,0.607843137254902,
0.617647058823529),.UNSPECIFIED.)
CURVE()
GEOMETRIC_REPRESENTATION_ITEM()
RATIONAL_B_SPLINE_CURVE((1.,0.866025403784439,1.,0.866025403784439,1.,0.866025403784439,
1.,0.866025403784439,1.,0.866025403784439,1.,0.866025403784439,1.))
REPRESENTATION_ITEM('')
);
#4205=(
BOUNDED_CURVE()
B_SPLINE_CURVE(2,(#366624,#366625,#366626,#366627,#366628,#366629,#366630,
#366631,#366632,#366633,#366634,#366635,#366636),.UNSPECIFIED.,.F.,.F.)
B_SPLINE_CURVE_WITH_KNOTS((3,2,2,2,2,2,3),(0.558823529411765,0.568627450980392,
0.57843137254902,0.588235294117647,0.598039215686275,0.607843137254902,
0.61764705882353),.UNSPECIFIED.)
CURVE()
GEOMETRIC_REPRESENTATION_ITEM()
RATIONAL_B_SPLINE_CURVE((1.,0.866025403784439,1.,0.866025403784439,1.,0.866025403784439,
1.,0.866025403784439,1.,0.866025403784439,1.,0.866025403784439,1.))
REPRESENTATION_ITEM('')
);
#4206=(
BOUNDED_CURVE()
B_SPLINE_CURVE(2,(#366641,#366642,#366643,#366644,#366645,#366646,#366647,
#366648,#366649,#366650,#366651,#366652,#366653),.UNSPECIFIED.,.F.,.F.)
B_SPLINE_CURVE_WITH_KNOTS((3,2,2,2,2,2,3),(0.617647058823529,0.627450980392157,
0.637254901960784,0.647058823529412,0.656862745098039,0.666666666666667,
0.676470588235294),.UNSPECIFIED.)
CURVE()
GEOMETRIC_REPRESENTATION_ITEM()
RATIONAL_B_SPLINE_CURVE((1.,0.866025403784439,1.,0.866025403784439,1.,0.866025403784439,
1.,0.866025403784439,1.,0.866025403784439,1.,0.866025403784439,1.))
REPRESENTATION_ITEM('')
);
#4207=(
BOUNDED_CURVE()
B_SPLINE_CURVE(2,(#366654,#366655,#366656,#366657,#366658,#366659,#366660,
#366661,#366662,#366663,#366664,#366665,#366666),.UNSPECIFIED.,.F.,.F.)
B_SPLINE_CURVE_WITH_KNOTS((3,2,2,2,2,2,3),(0.61764705882353,0.627450980392157,
0.637254901960784,0.647058823529412,0.656862745098039,0.666666666666667,
0.676470588235294),.UNSPECIFIED.)
CURVE()
GEOMETRIC_REPRESENTATION_ITEM()
RATIONAL_B_SPLINE_CURVE((1.,0.866025403784439,1.,0.866025403784439,1.,0.866025403784439,
1.,0.866025403784439,1.,0.866025403784439,1.,0.866025403784439,1.))
REPRESENTATION_ITEM('')
);
#4208=(
BOUNDED_CURVE()
B_SPLINE_CURVE(2,(#366671,#366672,#366673,#366674,#366675,#366676,#366677,
#366678,#366679,#366680,#366681,#366682,#366683),.UNSPECIFIED.,.F.,.F.)
B_SPLINE_CURVE_WITH_KNOTS((3,2,2,2,2,2,3),(0.676470588235294,0.686274509803922,
0.696078431372549,0.705882352941177,0.715686274509804,0.725490196078431,
0.735294117647059),.UNSPECIFIED.)
CURVE()
GEOMETRIC_REPRESENTATION_ITEM()
RATIONAL_B_SPLINE_CURVE((1.,0.866025403784439,1.,0.866025403784439,1.,0.866025403784439,
1.,0.866025403784439,1.,0.866025403784439,1.,0.866025403784439,1.))
REPRESENTATION_ITEM('')
);
#4209=(
BOUNDED_CURVE()
B_SPLINE_CURVE(2,(#366684,#366685,#366686,#366687,#366688,#366689,#366690,
#366691,#366692,#366693,#366694,#366695,#366696),.UNSPECIFIED.,.F.,.F.)
B_SPLINE_CURVE_WITH_KNOTS((3,2,2,2,2,2,3),(0.676470588235294,0.686274509803922,
0.696078431372549,0.705882352941177,0.715686274509804,0.725490196078431,
0.735294117647059),.UNSPECIFIED.)
CURVE()
GEOMETRIC_REPRESENTATION_ITEM()
RATIONAL_B_SPLINE_CURVE((1.,0.866025403784439,1.,0.866025403784439,1.,0.866025403784439,
1.,0.866025403784439,1.,0.866025403784439,1.,0.866025403784439,1.))
REPRESENTATION_ITEM('')
);
#4210=(
BOUNDED_CURVE()
B_SPLINE_CURVE(2,(#366701,#366702,#366703,#366704,#366705,#366706,#366707,
#366708,#366709,#366710,#366711,#366712,#366713),.UNSPECIFIED.,.F.,.F.)
B_SPLINE_CURVE_WITH_KNOTS((3,2,2,2,2,2,3),(0.735294117647059,0.745098039215686,
0.754901960784314,0.764705882352941,0.774509803921569,0.784313725490196,
0.794117647058823),.UNSPECIFIED.)
CURVE()
GEOMETRIC_REPRESENTATION_ITEM()
RATIONAL_B_SPLINE_CURVE((1.,0.866025403784439,1.,0.866025403784439,1.,0.866025403784439,
1.,0.866025403784439,1.,0.866025403784439,1.,0.866025403784439,1.))
REPRESENTATION_ITEM('')
);
#4211=(
BOUNDED_CURVE()
B_SPLINE_CURVE(2,(#366714,#366715,#366716,#366717,#366718,#366719,#366720,
#366721,#366722,#366723,#366724,#366725,#366726),.UNSPECIFIED.,.F.,.F.)
B_SPLINE_CURVE_WITH_KNOTS((3,2,2,2,2,2,3),(0.735294117647059,0.745098039215686,
0.754901960784314,0.764705882352941,0.774509803921569,0.784313725490196,
0.794117647058824),.UNSPECIFIED.)
CURVE()
GEOMETRIC_REPRESENTATION_ITEM()
RATIONAL_B_SPLINE_CURVE((1.,0.866025403784439,1.,0.866025403784439,1.,0.866025403784439,
1.,0.866025403784439,1.,0.866025403784439,1.,0.866025403784439,1.))
REPRESENTATION_ITEM('')
);
#4212=(
BOUNDED_CURVE()
B_SPLINE_CURVE(2,(#366731,#366732,#366733,#366734,#366735,#366736,#366737,
#366738,#366739,#366740,#366741,#366742,#366743),.UNSPECIFIED.,.F.,.F.)
B_SPLINE_CURVE_WITH_KNOTS((3,2,2,2,2,2,3),(0.794117647058823,0.803921568627451,
0.813725490196078,0.823529411764706,0.833333333333333,0.843137254901961,
0.852941176470588),.UNSPECIFIED.)
CURVE()
GEOMETRIC_REPRESENTATION_ITEM()
RATIONAL_B_SPLINE_CURVE((1.,0.866025403784439,1.,0.866025403784439,1.,0.866025403784439,
1.,0.866025403784439,1.,0.866025403784439,1.,0.866025403784439,1.))
REPRESENTATION_ITEM('')
);
#4213=(
BOUNDED_CURVE()
B_SPLINE_CURVE(2,(#366744,#366745,#366746,#366747,#366748,#366749,#366750,
#366751,#366752,#366753,#366754,#366755,#366756),.UNSPECIFIED.,.F.,.F.)
B_SPLINE_CURVE_WITH_KNOTS((3,2,2,2,2,2,3),(0.794117647058824,0.803921568627451,
0.813725490196079,0.823529411764706,0.833333333333333,0.843137254901961,
0.852941176470588),.UNSPECIFIED.)
CURVE()
GEOMETRIC_REPRESENTATION_ITEM()
RATIONAL_B_SPLINE_CURVE((1.,0.866025403784439,1.,0.866025403784439,1.,0.866025403784439,
1.,0.866025403784439,1.,0.866025403784439,1.,0.866025403784439,1.))
REPRESENTATION_ITEM('')
);
#4214=(
BOUNDED_CURVE()
B_SPLINE_CURVE(2,(#366761,#366762,#366763,#366764,#366765,#366766,#366767,
#366768,#366769,#366770,#366771,#366772,#366773),.UNSPECIFIED.,.F.,.F.)
B_SPLINE_CURVE_WITH_KNOTS((3,2,2,2,2,2,3),(0.852941176470588,0.862745098039216,
0.872549019607843,0.882352941176471,0.892156862745098,0.901960784313726,
0.911764705882353),.UNSPECIFIED.)
CURVE()
GEOMETRIC_REPRESENTATION_ITEM()
RATIONAL_B_SPLINE_CURVE((1.,0.866025403784439,1.,0.866025403784439,1.,0.866025403784439,
1.,0.866025403784439,1.,0.866025403784439,1.,0.866025403784439,1.))
REPRESENTATION_ITEM('')
);
#4215=(
BOUNDED_CURVE()
B_SPLINE_CURVE(2,(#366774,#366775,#366776,#366777,#366778,#366779,#366780,
#366781,#366782,#366783,#366784,#366785,#366786),.UNSPECIFIED.,.F.,.F.)
B_SPLINE_CURVE_WITH_KNOTS((3,2,2,2,2,2,3),(0.852941176470588,0.862745098039216,
0.872549019607843,0.882352941176471,0.892156862745098,0.901960784313726,
0.911764705882353),.UNSPECIFIED.)
CURVE()
GEOMETRIC_REPRESENTATION_ITEM()
RATIONAL_B_SPLINE_CURVE((1.,0.866025403784439,1.,0.866025403784439,1.,0.866025403784439,
1.,0.866025403784439,1.,0.866025403784439,1.,0.866025403784439,1.))
REPRESENTATION_ITEM('')
);
#4216=(
BOUNDED_CURVE()
B_SPLINE_CURVE(2,(#367905,#367906,#367907),.UNSPECIFIED.,.F.,.F.)
B_SPLINE_CURVE_WITH_KNOTS((3,3),(0.124274873543865,0.321867155116299),
 .UNSPECIFIED.)
CURVE()
GEOMETRIC_REPRESENTATION_ITEM()
RATIONAL_B_SPLINE_CURVE((1.46410161513778,1.69059892324148,1.46410161513778))
REPRESENTATION_ITEM('')
);
#4217=(
BOUNDED_CURVE()
B_SPLINE_CURVE(2,(#368096,#368097,#368098),.UNSPECIFIED.,.F.,.F.)
B_SPLINE_CURVE_WITH_KNOTS((3,3),(-0.3218671551163,-0.124274873543866),
 .UNSPECIFIED.)
CURVE()
GEOMETRIC_REPRESENTATION_ITEM()
RATIONAL_B_SPLINE_CURVE((1.46410161513778,1.69059892324148,1.46410161513778))
REPRESENTATION_ITEM('')
);
#4218=(
BOUNDED_CURVE()
B_SPLINE_CURVE(2,(#368100,#368101,#368102),.UNSPECIFIED.,.F.,.F.)
B_SPLINE_CURVE_WITH_KNOTS((3,3),(-0.321867155116299,-0.124274873543865),
 .UNSPECIFIED.)
CURVE()
GEOMETRIC_REPRESENTATION_ITEM()
RATIONAL_B_SPLINE_CURVE((1.46410161513778,1.69059892324148,1.46410161513778))
REPRESENTATION_ITEM('')
);
#4219=(
BOUNDED_CURVE()
B_SPLINE_CURVE(2,(#368104,#368105,#368106),.UNSPECIFIED.,.F.,.F.)
B_SPLINE_CURVE_WITH_KNOTS((3,3),(-0.321867155116299,-0.124274873543865),
 .UNSPECIFIED.)
CURVE()
GEOMETRIC_REPRESENTATION_ITEM()
RATIONAL_B_SPLINE_CURVE((1.46410161513778,1.69059892324148,1.46410161513778))
REPRESENTATION_ITEM('')
);
#4220=(
BOUNDED_CURVE()
B_SPLINE_CURVE(2,(#368108,#368109,#368110),.UNSPECIFIED.,.F.,.F.)
B_SPLINE_CURVE_WITH_KNOTS((3,3),(-0.321867155116299,-0.124274873543865),
 .UNSPECIFIED.)
CURVE()
GEOMETRIC_REPRESENTATION_ITEM()
RATIONAL_B_SPLINE_CURVE((1.46410161513778,1.69059892324148,1.46410161513778))
REPRESENTATION_ITEM('')
);
#4221=(
BOUNDED_CURVE()
B_SPLINE_CURVE(2,(#368112,#368113,#368114),.UNSPECIFIED.,.F.,.F.)
B_SPLINE_CURVE_WITH_KNOTS((3,3),(-0.321867155116299,-0.124274873543865),
 .UNSPECIFIED.)
CURVE()
GEOMETRIC_REPRESENTATION_ITEM()
RATIONAL_B_SPLINE_CURVE((1.46410161513778,1.69059892324148,1.46410161513778))
REPRESENTATION_ITEM('')
);
#4222=(
BOUNDED_CURVE()
B_SPLINE_CURVE(2,(#368550,#368551,#368552,#368553,#368554,#368555,#368556,
#368557,#368558,#368559,#368560,#368561,#368562),.UNSPECIFIED.,.F.,.F.)
B_SPLINE_CURVE_WITH_KNOTS((3,2,2,2,2,2,3),(0.911764705882353,0.921568627450981,
0.931372549019608,0.941176470588236,0.950980392156863,0.96078431372549,
0.970588235294118),.UNSPECIFIED.)
CURVE()
GEOMETRIC_REPRESENTATION_ITEM()
RATIONAL_B_SPLINE_CURVE((1.,0.866025403784439,1.,0.866025403784439,1.,0.866025403784439,
1.,0.866025403784439,1.,0.866025403784439,1.,0.866025403784436,1.))
REPRESENTATION_ITEM('')
);
#4223=(
BOUNDED_CURVE()
B_SPLINE_CURVE(2,(#368564,#368565,#368566,#368567,#368568,#368569,#368570,
#368571,#368572,#368573,#368574,#368575,#368576),.UNSPECIFIED.,.F.,.F.)
B_SPLINE_CURVE_WITH_KNOTS((3,2,2,2,2,2,3),(0.911764705882353,0.92156862745098,
0.931372549019608,0.941176470588235,0.950980392156863,0.96078431372549,
0.963362585267837),.UNSPECIFIED.)
CURVE()
GEOMETRIC_REPRESENTATION_ITEM()
RATIONAL_B_SPLINE_CURVE((1.,0.866025403784439,1.,0.866025403784439,1.,0.866025403784439,
1.,0.866025403784439,1.,0.866025403784439,1.,0.964766865340364,0.948065210722612))
REPRESENTATION_ITEM('')
);
#4224=(
BOUNDED_CURVE()
B_SPLINE_CURVE(2,(#368993,#368994,#368995,#368996,#368997,#368998,#368999),
 .UNSPECIFIED.,.F.,.F.)
B_SPLINE_CURVE_WITH_KNOTS((3,2,2,3),(0.815651079918082,0.825026379687255,
0.834401679456429,0.840557475565081),.UNSPECIFIED.)
CURVE()
GEOMETRIC_REPRESENTATION_ITEM()
RATIONAL_B_SPLINE_CURVE((1.,0.866025403784439,1.,0.866025403784439,1.,0.912032647664899,
0.939583539764693))
REPRESENTATION_ITEM('')
);
#4225=(
BOUNDED_CURVE()
B_SPLINE_CURVE(2,(#369002,#369003,#369004,#369005,#369006),
 .UNSPECIFIED.,.F.,.F.)
B_SPLINE_CURVE_WITH_KNOTS((3,2,3),(0.815651208026079,0.825026509267758,
0.833532478045858),.UNSPECIFIED.)
CURVE()
GEOMETRIC_REPRESENTATION_ITEM()
RATIONAL_B_SPLINE_CURVE((1.,0.866025403784439,1.,0.878448307623234,0.977458040128596))
REPRESENTATION_ITEM('')
);
#4226=(
BOUNDED_CURVE()
B_SPLINE_CURVE(2,(#369011,#369012,#369013,#369014,#369015,#369016,#369017,
#369018,#369019,#369020,#369021,#369022,#369023),.UNSPECIFIED.,.F.,.F.)
B_SPLINE_CURVE_WITH_KNOTS((3,2,2,2,2,2,3),(0.759399281303043,0.768774581072216,
0.778149880841389,0.787525180610563,0.796900480379736,0.806275780148909,
0.815651079918082),.UNSPECIFIED.)
CURVE()
GEOMETRIC_REPRESENTATION_ITEM()
RATIONAL_B_SPLINE_CURVE((1.,0.866025403784439,1.,0.866025403784439,1.,0.866025403784439,
1.,0.866025403784439,1.,0.866025403784439,1.,0.866025403784439,1.))
REPRESENTATION_ITEM('')
);
#4227=(
BOUNDED_CURVE()
B_SPLINE_CURVE(2,(#369024,#369025,#369026,#369027,#369028,#369029,#369030,
#369031,#369032,#369033,#369034,#369035,#369036),.UNSPECIFIED.,.F.,.F.)
B_SPLINE_CURVE_WITH_KNOTS((3,2,2,2,2,2,3),(0.759399400576005,0.768774701817684,
0.778150003059363,0.787525304301042,0.796900605542721,0.8062759067844,0.815651208026079),
 .UNSPECIFIED.)
CURVE()
GEOMETRIC_REPRESENTATION_ITEM()
RATIONAL_B_SPLINE_CURVE((1.,0.866025403784439,1.,0.866025403784439,1.,0.866025403784439,
1.,0.866025403784439,1.,0.866025403784439,1.,0.866025403784439,1.))
REPRESENTATION_ITEM('')
);
#4228=(
BOUNDED_CURVE()
B_SPLINE_CURVE(2,(#369041,#369042,#369043,#369044,#369045,#369046,#369047,
#369048,#369049,#369050,#369051,#369052,#369053),.UNSPECIFIED.,.F.,.F.)
B_SPLINE_CURVE_WITH_KNOTS((3,2,2,2,2,2,3),(0.703147482688004,0.712522782457177,
0.72189808222635,0.731273381995523,0.740648681764697,0.75002398153387,0.759399281303043),
 .UNSPECIFIED.)
CURVE()
GEOMETRIC_REPRESENTATION_ITEM()
RATIONAL_B_SPLINE_CURVE((1.,0.866025403784439,1.,0.866025403784439,1.,0.866025403784439,
1.,0.866025403784439,1.,0.866025403784439,1.,0.866025403784439,1.))
REPRESENTATION_ITEM('')
);
#4229=(
BOUNDED_CURVE()
B_SPLINE_CURVE(2,(#369054,#369055,#369056,#369057,#369058,#369059,#369060,
#369061,#369062,#369063,#369064,#369065,#369066),.UNSPECIFIED.,.F.,.F.)
B_SPLINE_CURVE_WITH_KNOTS((3,2,2,2,2,2,3),(0.70314759312593,0.712522894367609,
0.721898195609288,0.731273496850967,0.740648798092646,0.750024099334325,
0.759399400576005),.UNSPECIFIED.)
CURVE()
GEOMETRIC_REPRESENTATION_ITEM()
RATIONAL_B_SPLINE_CURVE((1.,0.866025403784439,1.,0.866025403784439,1.,0.866025403784439,
1.,0.866025403784439,1.,0.866025403784439,1.,0.866025403784439,1.))
REPRESENTATION_ITEM('')
);
#4230=(
BOUNDED_CURVE()
B_SPLINE_CURVE(2,(#369071,#369072,#369073,#369074,#369075,#369076,#369077,
#369078,#369079,#369080,#369081,#369082,#369083),.UNSPECIFIED.,.F.,.F.)
B_SPLINE_CURVE_WITH_KNOTS((3,2,2,2,2,2,3),(0.646895684072964,0.656270983842138,
0.665646283611311,0.675021583380484,0.684396883149657,0.693772182918831,
0.703147482688004),.UNSPECIFIED.)
CURVE()
GEOMETRIC_REPRESENTATION_ITEM()
RATIONAL_B_SPLINE_CURVE((1.,0.866025403784439,1.,0.866025403784439,1.,0.866025403784439,
1.,0.866025403784439,1.,0.866025403784439,1.,0.866025403784439,1.))
REPRESENTATION_ITEM('')
);
#4231=(
BOUNDED_CURVE()
B_SPLINE_CURVE(2,(#369084,#369085,#369086,#369087,#369088,#369089,#369090,
#369091,#369092,#369093,#369094,#369095,#369096),.UNSPECIFIED.,.F.,.F.)
B_SPLINE_CURVE_WITH_KNOTS((3,2,2,2,2,2,3),(0.646895785675856,0.656271086917535,
0.665646388159214,0.675021689400893,0.684396990642572,0.693772291884251,
0.70314759312593),.UNSPECIFIED.)
CURVE()
GEOMETRIC_REPRESENTATION_ITEM()
RATIONAL_B_SPLINE_CURVE((1.,0.866025403784439,1.,0.866025403784439,1.,0.866025403784439,
1.,0.866025403784439,1.,0.866025403784439,1.,0.866025403784439,1.))
REPRESENTATION_ITEM('')
);
#4232=(
BOUNDED_CURVE()
B_SPLINE_CURVE(2,(#369101,#369102,#369103,#369104,#369105,#369106,#369107,
#369108,#369109,#369110,#369111,#369112,#369113),.UNSPECIFIED.,.F.,.F.)
B_SPLINE_CURVE_WITH_KNOTS((3,2,2,2,2,2,3),(0.590643885457925,0.600019185227099,
0.609394484996272,0.618769784765445,0.628145084534618,0.637520384303791,
0.646895684072964),.UNSPECIFIED.)
CURVE()
GEOMETRIC_REPRESENTATION_ITEM()
RATIONAL_B_SPLINE_CURVE((1.,0.866025403784439,1.,0.866025403784439,1.,0.866025403784439,
1.,0.866025403784439,1.,0.866025403784439,1.,0.866025403784439,1.))
REPRESENTATION_ITEM('')
);
#4233=(
BOUNDED_CURVE()
B_SPLINE_CURVE(2,(#369114,#369115,#369116,#369117,#369118,#369119,#369120,
#369121,#369122,#369123,#369124,#369125,#369126),.UNSPECIFIED.,.F.,.F.)
B_SPLINE_CURVE_WITH_KNOTS((3,2,2,2,2,2,3),(0.590643978225781,0.60001927946746,
0.60939458070914,0.618769881950819,0.628145183192497,0.637520484434177,
0.646895785675856),.UNSPECIFIED.)
CURVE()
GEOMETRIC_REPRESENTATION_ITEM()
RATIONAL_B_SPLINE_CURVE((1.,0.866025403784439,1.,0.866025403784439,1.,0.866025403784439,
1.,0.866025403784439,1.,0.866025403784439,1.,0.866025403784439,1.))
REPRESENTATION_ITEM('')
);
#4234=(
BOUNDED_CURVE()
B_SPLINE_CURVE(2,(#369131,#369132,#369133,#369134,#369135,#369136,#369137,
#369138,#369139,#369140,#369141,#369142,#369143),.UNSPECIFIED.,.F.,.F.)
B_SPLINE_CURVE_WITH_KNOTS((3,2,2,2,2,2,3),(0.534392086842886,0.543767386612059,
0.553142686381232,0.562517986150406,0.571893285919579,0.581268585688752,
0.590643885457925),.UNSPECIFIED.)
CURVE()
GEOMETRIC_REPRESENTATION_ITEM()
RATIONAL_B_SPLINE_CURVE((1.,0.866025403784439,1.,0.866025403784439,1.,0.866025403784439,
1.,0.866025403784439,1.,0.866025403784439,1.,0.866025403784439,1.))
REPRESENTATION_ITEM('')
);
#4235=(
BOUNDED_CURVE()
B_SPLINE_CURVE(2,(#369144,#369145,#369146,#369147,#369148,#369149,#369150,
#369151,#369152,#369153,#369154,#369155,#369156),.UNSPECIFIED.,.F.,.F.)
B_SPLINE_CURVE_WITH_KNOTS((3,2,2,2,2,2,3),(0.534392170775707,0.543767472017386,
0.553142773259065,0.562518074500744,0.571893375742423,0.581268676984102,
0.590643978225781),.UNSPECIFIED.)
CURVE()
GEOMETRIC_REPRESENTATION_ITEM()
RATIONAL_B_SPLINE_CURVE((1.,0.866025403784439,1.,0.866025403784439,1.,0.866025403784439,
1.,0.866025403784439,1.,0.866025403784439,1.,0.866025403784439,1.))
REPRESENTATION_ITEM('')
);
#4236=(
BOUNDED_CURVE()
B_SPLINE_CURVE(2,(#369161,#369162,#369163,#369164,#369165,#369166,#369167,
#369168,#369169,#369170,#369171,#369172,#369173),.UNSPECIFIED.,.F.,.F.)
B_SPLINE_CURVE_WITH_KNOTS((3,2,2,2,2,2,3),(0.478140288227847,0.48751558799702,
0.496890887766193,0.506266187535366,0.51564148730454,0.525016787073713,
0.534392086842886),.UNSPECIFIED.)
CURVE()
GEOMETRIC_REPRESENTATION_ITEM()
RATIONAL_B_SPLINE_CURVE((1.,0.866025403784439,1.,0.866025403784439,1.,0.866025403784439,
1.,0.866025403784439,1.,0.866025403784439,1.,0.866025403784439,1.))
REPRESENTATION_ITEM('')
);
#4237=(
BOUNDED_CURVE()
B_SPLINE_CURVE(2,(#369174,#369175,#369176,#369177,#369178,#369179,#369180,
#369181,#369182,#369183,#369184,#369185,#369186),.UNSPECIFIED.,.F.,.F.)
B_SPLINE_CURVE_WITH_KNOTS((3,2,2,2,2,2,3),(0.478140363325633,0.487515664567311,
0.496890965808991,0.50626626705067,0.515641568292349,0.525016869534028,
0.534392170775707),.UNSPECIFIED.)
CURVE()
GEOMETRIC_REPRESENTATION_ITEM()
RATIONAL_B_SPLINE_CURVE((1.,0.866025403784439,1.,0.866025403784439,1.,0.866025403784439,
1.,0.866025403784439,1.,0.866025403784439,1.,0.866025403784439,1.))
REPRESENTATION_ITEM('')
);
#4238=(
BOUNDED_CURVE()
B_SPLINE_CURVE(2,(#369191,#369192,#369193,#369194,#369195,#369196,#369197,
#369198,#369199,#369200,#369201,#369202,#369203),.UNSPECIFIED.,.F.,.F.)
B_SPLINE_CURVE_WITH_KNOTS((3,2,2,2,2,2,3),(0.421888489612808,0.431263789381981,
0.440639089151154,0.450014388920327,0.4593896886895,0.468764988458674,0.478140288227847),
 .UNSPECIFIED.)
CURVE()
GEOMETRIC_REPRESENTATION_ITEM()
RATIONAL_B_SPLINE_CURVE((1.,0.866025403784439,1.,0.866025403784439,1.,0.866025403784439,
1.,0.866025403784439,1.,0.866025403784439,1.,0.866025403784439,1.))
REPRESENTATION_ITEM('')
);
#4239=(
BOUNDED_CURVE()
B_SPLINE_CURVE(2,(#369204,#369205,#369206,#369207,#369208,#369209,#369210,
#369211,#369212,#369213,#369214,#369215,#369216),.UNSPECIFIED.,.F.,.F.)
B_SPLINE_CURVE_WITH_KNOTS((3,2,2,2,2,2,3),(0.421888555875558,0.431263857117237,
0.440639158358916,0.450014459600595,0.459389760842274,0.468765062083953,
0.478140363325633),.UNSPECIFIED.)
CURVE()
GEOMETRIC_REPRESENTATION_ITEM()
RATIONAL_B_SPLINE_CURVE((1.,0.866025403784439,1.,0.866025403784439,1.,0.866025403784439,
1.,0.866025403784439,1.,0.866025403784439,1.,0.866025403784439,1.))
REPRESENTATION_ITEM('')
);
#4240=(
BOUNDED_CURVE()
B_SPLINE_CURVE(2,(#369221,#369222,#369223,#369224,#369225,#369226,#369227,
#369228,#369229,#369230,#369231,#369232,#369233),.UNSPECIFIED.,.F.,.F.)
B_SPLINE_CURVE_WITH_KNOTS((3,2,2,2,2,2,3),(0.365636690997768,0.375011990766941,
0.384387290536115,0.393762590305288,0.403137890074461,0.412513189843634,
0.421888489612808),.UNSPECIFIED.)
CURVE()
GEOMETRIC_REPRESENTATION_ITEM()
RATIONAL_B_SPLINE_CURVE((1.,0.866025403784439,1.,0.866025403784439,1.,0.866025403784439,
1.,0.866025403784439,1.,0.866025403784439,1.,0.866025403784439,1.))
REPRESENTATION_ITEM('')
);
#4241=(
BOUNDED_CURVE()
B_SPLINE_CURVE(2,(#369234,#369235,#369236,#369237,#369238,#369239,#369240,
#369241,#369242,#369243,#369244,#369245,#369246),.UNSPECIFIED.,.F.,.F.)
B_SPLINE_CURVE_WITH_KNOTS((3,2,2,2,2,2,3),(0.365636748425484,0.375012049667163,
0.384387350908842,0.393762652150521,0.4031379533922,0.412513254633879,0.421888555875558),
 .UNSPECIFIED.)
CURVE()
GEOMETRIC_REPRESENTATION_ITEM()
RATIONAL_B_SPLINE_CURVE((1.,0.866025403784439,1.,0.866025403784439,1.,0.866025403784439,
1.,0.866025403784439,1.,0.866025403784439,1.,0.866025403784439,1.))
REPRESENTATION_ITEM('')
);
#4242=(
BOUNDED_CURVE()
B_SPLINE_CURVE(2,(#369251,#369252,#369253,#369254,#369255,#369256,#369257,
#369258,#369259,#369260,#369261,#369262,#369263),.UNSPECIFIED.,.F.,.F.)
B_SPLINE_CURVE_WITH_KNOTS((3,2,2,2,2,2,3),(0.309384892382729,0.318760192151902,
0.328135491921075,0.337510791690249,0.346886091459422,0.356261391228595,
0.365636690997768),.UNSPECIFIED.)
CURVE()
GEOMETRIC_REPRESENTATION_ITEM()
RATIONAL_B_SPLINE_CURVE((1.,0.866025403784439,1.,0.866025403784439,1.,0.866025403784439,
1.,0.866025403784439,1.,0.866025403784439,1.,0.866025403784439,1.))
REPRESENTATION_ITEM('')
);
#4243=(
BOUNDED_CURVE()
B_SPLINE_CURVE(2,(#369264,#369265,#369266,#369267,#369268,#369269,#369270,
#369271,#369272,#369273,#369274,#369275,#369276),.UNSPECIFIED.,.F.,.F.)
B_SPLINE_CURVE_WITH_KNOTS((3,2,2,2,2,2,3),(0.309384940975409,0.318760242217088,
0.328135543458767,0.337510844700446,0.346886145942126,0.356261447183805,
0.365636748425484),.UNSPECIFIED.)
CURVE()
GEOMETRIC_REPRESENTATION_ITEM()
RATIONAL_B_SPLINE_CURVE((1.,0.866025403784439,1.,0.866025403784439,1.,0.866025403784439,
1.,0.866025403784439,1.,0.866025403784439,1.,0.866025403784439,1.))
REPRESENTATION_ITEM('')
);
#4244=(
BOUNDED_CURVE()
B_SPLINE_CURVE(2,(#369281,#369282,#369283,#369284,#369285,#369286,#369287,
#369288,#369289,#369290,#369291,#369292,#369293),.UNSPECIFIED.,.F.,.F.)
B_SPLINE_CURVE_WITH_KNOTS((3,2,2,2,2,2,3),(0.25313309376769,0.262508393536863,
0.271883693306036,0.28125899307521,0.290634292844383,0.300009592613556,
0.309384892382729),.UNSPECIFIED.)
CURVE()
GEOMETRIC_REPRESENTATION_ITEM()
RATIONAL_B_SPLINE_CURVE((1.,0.866025403784439,1.,0.866025403784439,1.,0.866025403784439,
1.,0.866025403784439,1.,0.866025403784439,1.,0.866025403784439,1.))
REPRESENTATION_ITEM('')
);
#4245=(
BOUNDED_CURVE()
B_SPLINE_CURVE(2,(#369294,#369295,#369296,#369297,#369298,#369299,#369300,
#369301,#369302,#369303,#369304,#369305,#369306),.UNSPECIFIED.,.F.,.F.)
B_SPLINE_CURVE_WITH_KNOTS((3,2,2,2,2,2,3),(0.253133133525335,0.262508434767014,
0.271883736008693,0.281259037250372,0.290634338492051,0.30000963973373,
0.309384940975409),.UNSPECIFIED.)
CURVE()
GEOMETRIC_REPRESENTATION_ITEM()
RATIONAL_B_SPLINE_CURVE((1.,0.866025403784439,1.,0.866025403784439,1.,0.866025403784439,
1.,0.866025403784439,1.,0.866025403784439,1.,0.866025403784439,1.))
REPRESENTATION_ITEM('')
);
#4246=(
BOUNDED_CURVE()
B_SPLINE_CURVE(2,(#369311,#369312,#369313,#369314,#369315,#369316,#369317,
#369318,#369319,#369320,#369321,#369322,#369323),.UNSPECIFIED.,.F.,.F.)
B_SPLINE_CURVE_WITH_KNOTS((3,2,2,2,2,2,3),(0.196881295152651,0.206256594921824,
0.215631894690997,0.22500719446017,0.234382494229343,0.243757793998517,
0.25313309376769),.UNSPECIFIED.)
CURVE()
GEOMETRIC_REPRESENTATION_ITEM()
RATIONAL_B_SPLINE_CURVE((1.,0.866025403784439,1.,0.866025403784439,1.,0.866025403784439,
1.,0.866025403784439,1.,0.866025403784439,1.,0.866025403784439,1.))
REPRESENTATION_ITEM('')
);
#4247=(
BOUNDED_CURVE()
B_SPLINE_CURVE(2,(#369324,#369325,#369326,#369327,#369328,#369329,#369330,
#369331,#369332,#369333,#369334,#369335,#369336),.UNSPECIFIED.,.F.,.F.)
B_SPLINE_CURVE_WITH_KNOTS((3,2,2,2,2,2,3),(0.19688132607526,0.20625662731694,
0.215631928558619,0.225007229800298,0.234382531041977,0.243757832283656,
0.253133133525335),.UNSPECIFIED.)
CURVE()
GEOMETRIC_REPRESENTATION_ITEM()
RATIONAL_B_SPLINE_CURVE((1.,0.866025403784439,1.,0.866025403784439,1.,0.866025403784439,
1.,0.866025403784439,1.,0.866025403784439,1.,0.866025403784439,1.))
REPRESENTATION_ITEM('')
);
#4248=(
BOUNDED_CURVE()
B_SPLINE_CURVE(2,(#369341,#369342,#369343,#369344,#369345,#369346,#369347,
#369348,#369349,#369350,#369351,#369352,#369353),.UNSPECIFIED.,.F.,.F.)
B_SPLINE_CURVE_WITH_KNOTS((3,2,2,2,2,2,3),(0.140629496537611,0.150004796306785,
0.159380096075958,0.168755395845131,0.178130695614304,0.187505995383477,
0.196881295152651),.UNSPECIFIED.)
CURVE()
GEOMETRIC_REPRESENTATION_ITEM()
RATIONAL_B_SPLINE_CURVE((1.,0.866025403784439,1.,0.866025403784439,1.,0.866025403784439,
1.,0.866025403784439,1.,0.866025403784439,1.,0.866025403784439,1.))
REPRESENTATION_ITEM('')
);
#4249=(
BOUNDED_CURVE()
B_SPLINE_CURVE(2,(#369354,#369355,#369356,#369357,#369358,#369359,#369360,
#369361,#369362,#369363,#369364,#369365,#369366),.UNSPECIFIED.,.F.,.F.)
B_SPLINE_CURVE_WITH_KNOTS((3,2,2,2,2,2,3),(0.140629518625186,0.150004819866865,
0.159380121108544,0.168755422350223,0.178130723591902,0.187506024833581,
0.19688132607526),.UNSPECIFIED.)
CURVE()
GEOMETRIC_REPRESENTATION_ITEM()
RATIONAL_B_SPLINE_CURVE((1.,0.866025403784439,1.,0.866025403784439,1.,0.866025403784439,
1.,0.866025403784439,1.,0.866025403784439,1.,0.866025403784439,1.))
REPRESENTATION_ITEM('')
);
#4250=(
BOUNDED_CURVE()
B_SPLINE_CURVE(2,(#369371,#369372,#369373,#369374,#369375,#369376,#369377,
#369378,#369379,#369380,#369381,#369382,#369383),.UNSPECIFIED.,.F.,.F.)
B_SPLINE_CURVE_WITH_KNOTS((3,2,2,2,2,2,3),(0.0843776979225721,0.0937529976917453,
0.103128297460919,0.112503597230092,0.121878896999265,0.131254196768438,
0.140629496537611),.UNSPECIFIED.)
CURVE()
GEOMETRIC_REPRESENTATION_ITEM()
RATIONAL_B_SPLINE_CURVE((1.,0.866025403784439,1.,0.866025403784439,1.,0.866025403784439,
1.,0.866025403784439,1.,0.866025403784439,1.,0.866025403784439,1.))
REPRESENTATION_ITEM('')
);
#4251=(
BOUNDED_CURVE()
B_SPLINE_CURVE(2,(#369384,#369385,#369386,#369387,#369388,#369389,#369390,
#369391,#369392,#369393,#369394,#369395,#369396),.UNSPECIFIED.,.F.,.F.)
B_SPLINE_CURVE_WITH_KNOTS((3,2,2,2,2,2,3),(0.0843777111751116,0.0937530124167907,
0.10312831365847,0.112503614900149,0.121878916141828,0.131254217383507,
0.140629518625186),.UNSPECIFIED.)
CURVE()
GEOMETRIC_REPRESENTATION_ITEM()
RATIONAL_B_SPLINE_CURVE((1.,0.866025403784439,1.,0.866025403784439,1.,0.866025403784439,
1.,0.866025403784439,1.,0.866025403784439,1.,0.866025403784439,1.))
REPRESENTATION_ITEM('')
);
#4252=(
BOUNDED_CURVE()
B_SPLINE_CURVE(2,(#369403,#369404,#369405,#369406,#369407,#369408,#369409,
#369410,#369411,#369412,#369413,#369414,#369415),.UNSPECIFIED.,.F.,.F.)
B_SPLINE_CURVE_WITH_KNOTS((3,2,2,2,2,2,3),(0.033715912765314,0.0375011990767061,
0.0468764988458793,0.0562517986150525,0.0656270983842257,0.0750023981533989,
0.0843776979225721),.UNSPECIFIED.)
CURVE()
GEOMETRIC_REPRESENTATION_ITEM()
RATIONAL_B_SPLINE_CURVE((0.93549495027976,0.945907627743645,1.,0.866025403784439,
1.,0.866025403784439,1.,0.866025403784439,1.,0.866025403784439,1.,0.866025403784439,
1.))
REPRESENTATION_ITEM('')
);
#4253=(
BOUNDED_CURVE()
B_SPLINE_CURVE(2,(#369416,#369417,#369418,#369419,#369420,#369421,#369422,
#369423,#369424,#369425,#369426,#369427,#369428),.UNSPECIFIED.,.F.,.F.)
B_SPLINE_CURVE_WITH_KNOTS((3,2,2,2,2,2,3),(0.0281259037250372,0.0375012049667163,
0.0468765062083953,0.0562518074500744,0.0656271086917535,0.0750024099334325,
0.0843777111751116),.UNSPECIFIED.)
CURVE()
GEOMETRIC_REPRESENTATION_ITEM()
RATIONAL_B_SPLINE_CURVE((1.,0.866025403784439,1.,0.866025403784439,1.,0.866025403784439,
1.,0.866025403784439,1.,0.866025403784439,1.,0.866025403784439,1.))
REPRESENTATION_ITEM('')
);
#4254=(
BOUNDED_CURVE()
B_SPLINE_CURVE(2,(#370584,#370585,#370586),.UNSPECIFIED.,.F.,.F.)
B_SPLINE_CURVE_WITH_KNOTS((3,3),(0.120361405182823,0.287808339382405),
 .UNSPECIFIED.)
CURVE()
GEOMETRIC_REPRESENTATION_ITEM()
RATIONAL_B_SPLINE_CURVE((1.61880215351743,1.86923171819516,1.61880215351743))
REPRESENTATION_ITEM('')
);
#4255=(
BOUNDED_CURVE()
B_SPLINE_CURVE(2,(#370694,#370695,#370696),.UNSPECIFIED.,.F.,.F.)
B_SPLINE_CURVE_WITH_KNOTS((3,3),(0.120361405182824,0.287808339382406),
 .UNSPECIFIED.)
CURVE()
GEOMETRIC_REPRESENTATION_ITEM()
RATIONAL_B_SPLINE_CURVE((1.61880215351743,1.86923171819516,1.61880215351743))
REPRESENTATION_ITEM('')
);
#4256=(
BOUNDED_CURVE()
B_SPLINE_CURVE(2,(#370698,#370699,#370700),.UNSPECIFIED.,.F.,.F.)
B_SPLINE_CURVE_WITH_KNOTS((3,3),(0.120361405182823,0.287808339382407),
 .UNSPECIFIED.)
CURVE()
GEOMETRIC_REPRESENTATION_ITEM()
RATIONAL_B_SPLINE_CURVE((1.61880215351743,1.86923171819516,1.61880215351743))
REPRESENTATION_ITEM('')
);
#4257=(
BOUNDED_CURVE()
B_SPLINE_CURVE(2,(#370702,#370703,#370704),.UNSPECIFIED.,.F.,.F.)
B_SPLINE_CURVE_WITH_KNOTS((3,3),(0.120361405182823,0.287808339382406),
 .UNSPECIFIED.)
CURVE()
GEOMETRIC_REPRESENTATION_ITEM()
RATIONAL_B_SPLINE_CURVE((1.61880215351743,1.86923171819516,1.61880215351743))
REPRESENTATION_ITEM('')
);
#4258=(
BOUNDED_CURVE()
B_SPLINE_CURVE(2,(#370706,#370707,#370708),.UNSPECIFIED.,.F.,.F.)
B_SPLINE_CURVE_WITH_KNOTS((3,3),(0.120361405182824,0.287808339382405),
 .UNSPECIFIED.)
CURVE()
GEOMETRIC_REPRESENTATION_ITEM()
RATIONAL_B_SPLINE_CURVE((1.61880215351743,1.86923171819515,1.61880215351743))
REPRESENTATION_ITEM('')
);
#4259=(
BOUNDED_CURVE()
B_SPLINE_CURVE(2,(#370710,#370711,#370712),.UNSPECIFIED.,.F.,.F.)
B_SPLINE_CURVE_WITH_KNOTS((3,3),(0.120361405182823,0.287808339382406),
 .UNSPECIFIED.)
CURVE()
GEOMETRIC_REPRESENTATION_ITEM()
RATIONAL_B_SPLINE_CURVE((1.61880215351743,1.86923171819516,1.61880215351743))
REPRESENTATION_ITEM('')
);
#4260=(
BOUNDED_CURVE()
B_SPLINE_CURVE(2,(#371174,#371175,#371176),.UNSPECIFIED.,.F.,.F.)
B_SPLINE_CURVE_WITH_KNOTS((3,3),(0.0266276333531501,0.0281259037250372),
 .UNSPECIFIED.)
CURVE()
GEOMETRIC_REPRESENTATION_ITEM()
RATIONAL_B_SPLINE_CURVE((0.964022189566802,0.978589470042526,1.))
REPRESENTATION_ITEM('')
);
#4261=(
BOUNDED_CURVE()
B_SPLINE_CURVE(2,(#371613,#371614,#371615),.UNSPECIFIED.,.F.,.F.)
B_SPLINE_CURVE_WITH_KNOTS((3,3),(0.0121665790178462,0.0161290322580645),
 .UNSPECIFIED.)
CURVE()
GEOMETRIC_REPRESENTATION_ITEM()
RATIONAL_B_SPLINE_CURVE((0.948065210722606,0.901258538444081,1.))
REPRESENTATION_ITEM('')
);
#4262=(
BOUNDED_CURVE()
B_SPLINE_CURVE(2,(#371621,#371622,#371623,#371624,#371625,#371626,#371627,
#371628,#371629,#371630,#371631,#371632,#371633),.UNSPECIFIED.,.F.,.F.)
B_SPLINE_CURVE_WITH_KNOTS((3,2,2,2,2,2,3),(0.0161290322580645,0.021505376344086,
0.0268817204301075,0.032258064516129,0.0376344086021505,0.043010752688172,
0.0483870967741935),.UNSPECIFIED.)
CURVE()
GEOMETRIC_REPRESENTATION_ITEM()
RATIONAL_B_SPLINE_CURVE((1.,0.866025403784439,1.,0.866025403784439,1.,0.866025403784439,
1.,0.866025403784439,1.,0.866025403784439,1.,0.866025403784439,1.))
REPRESENTATION_ITEM('')
);
#4263=(
BOUNDED_CURVE()
B_SPLINE_CURVE(2,(#371634,#371635,#371636,#371637,#371638,#371639,#371640,
#371641,#371642,#371643,#371644,#371645,#371646),.UNSPECIFIED.,.F.,.F.)
B_SPLINE_CURVE_WITH_KNOTS((3,2,2,2,2,2,3),(0.0161290322580645,0.021505376344086,
0.0268817204301075,0.032258064516129,0.0376344086021506,0.0430107526881721,
0.0483870967741936),.UNSPECIFIED.)
CURVE()
GEOMETRIC_REPRESENTATION_ITEM()
RATIONAL_B_SPLINE_CURVE((1.,0.866025403784439,1.,0.866025403784439,1.,0.866025403784439,
1.,0.866025403784439,1.,0.866025403784439,1.,0.866025403784439,1.))
REPRESENTATION_ITEM('')
);
#4264=(
BOUNDED_CURVE()
B_SPLINE_CURVE(2,(#371651,#371652,#371653,#371654,#371655,#371656,#371657,
#371658,#371659,#371660,#371661,#371662,#371663),.UNSPECIFIED.,.F.,.F.)
B_SPLINE_CURVE_WITH_KNOTS((3,2,2,2,2,2,3),(0.0483870967741935,0.0537634408602151,
0.0591397849462366,0.0645161290322581,0.0698924731182796,0.0752688172043011,
0.0806451612903226),.UNSPECIFIED.)
CURVE()
GEOMETRIC_REPRESENTATION_ITEM()
RATIONAL_B_SPLINE_CURVE((1.,0.866025403784439,1.,0.866025403784439,1.,0.866025403784439,
1.,0.866025403784439,1.,0.866025403784439,1.,0.866025403784439,1.))
REPRESENTATION_ITEM('')
);
#4265=(
BOUNDED_CURVE()
B_SPLINE_CURVE(2,(#371664,#371665,#371666,#371667,#371668,#371669,#371670,
#371671,#371672,#371673,#371674,#371675,#371676),.UNSPECIFIED.,.F.,.F.)
B_SPLINE_CURVE_WITH_KNOTS((3,2,2,2,2,2,3),(0.0483870967741936,0.0537634408602151,
0.0591397849462366,0.0645161290322581,0.0698924731182796,0.0752688172043011,
0.0806451612903226),.UNSPECIFIED.)
CURVE()
GEOMETRIC_REPRESENTATION_ITEM()
RATIONAL_B_SPLINE_CURVE((1.,0.866025403784439,1.,0.866025403784439,1.,0.866025403784439,
1.,0.866025403784439,1.,0.866025403784439,1.,0.866025403784439,1.))
REPRESENTATION_ITEM('')
);
#4266=(
BOUNDED_CURVE()
B_SPLINE_CURVE(2,(#371681,#371682,#371683,#371684,#371685,#371686,#371687,
#371688,#371689,#371690,#371691,#371692,#371693),.UNSPECIFIED.,.F.,.F.)
B_SPLINE_CURVE_WITH_KNOTS((3,2,2,2,2,2,3),(0.0806451612903226,0.0860215053763441,
0.0913978494623656,0.0967741935483871,0.102150537634409,0.10752688172043,
0.112903225806452),.UNSPECIFIED.)
CURVE()
GEOMETRIC_REPRESENTATION_ITEM()
RATIONAL_B_SPLINE_CURVE((1.,0.866025403784439,1.,0.866025403784439,1.,0.866025403784439,
1.,0.866025403784439,1.,0.866025403784439,1.,0.866025403784439,1.))
REPRESENTATION_ITEM('')
);
#4267=(
BOUNDED_CURVE()
B_SPLINE_CURVE(2,(#371694,#371695,#371696,#371697,#371698,#371699,#371700,
#371701,#371702,#371703,#371704,#371705,#371706),.UNSPECIFIED.,.F.,.F.)
B_SPLINE_CURVE_WITH_KNOTS((3,2,2,2,2,2,3),(0.0806451612903226,0.0860215053763441,
0.0913978494623656,0.0967741935483871,0.102150537634409,0.10752688172043,
0.112903225806452),.UNSPECIFIED.)
CURVE()
GEOMETRIC_REPRESENTATION_ITEM()
RATIONAL_B_SPLINE_CURVE((1.,0.866025403784439,1.,0.866025403784439,1.,0.866025403784439,
1.,0.866025403784439,1.,0.866025403784439,1.,0.866025403784439,1.))
REPRESENTATION_ITEM('')
);
#4268=(
BOUNDED_CURVE()
B_SPLINE_CURVE(2,(#371711,#371712,#371713,#371714,#371715,#371716,#371717,
#371718,#371719,#371720,#371721,#371722,#371723),.UNSPECIFIED.,.F.,.F.)
B_SPLINE_CURVE_WITH_KNOTS((3,2,2,2,2,2,3),(0.112903225806452,0.118279569892473,
0.123655913978495,0.129032258064516,0.134408602150538,0.139784946236559,
0.145161290322581),.UNSPECIFIED.)
CURVE()
GEOMETRIC_REPRESENTATION_ITEM()
RATIONAL_B_SPLINE_CURVE((1.,0.866025403784439,1.,0.866025403784439,1.,0.866025403784439,
1.,0.866025403784439,1.,0.866025403784439,1.,0.866025403784439,1.))
REPRESENTATION_ITEM('')
);
#4269=(
BOUNDED_CURVE()
B_SPLINE_CURVE(2,(#371724,#371725,#371726,#371727,#371728,#371729,#371730,
#371731,#371732,#371733,#371734,#371735,#371736),.UNSPECIFIED.,.F.,.F.)
B_SPLINE_CURVE_WITH_KNOTS((3,2,2,2,2,2,3),(0.112903225806452,0.118279569892473,
0.123655913978495,0.129032258064516,0.134408602150538,0.139784946236559,
0.145161290322581),.UNSPECIFIED.)
CURVE()
GEOMETRIC_REPRESENTATION_ITEM()
RATIONAL_B_SPLINE_CURVE((1.,0.866025403784439,1.,0.866025403784439,1.,0.866025403784439,
1.,0.866025403784439,1.,0.866025403784439,1.,0.866025403784439,1.))
REPRESENTATION_ITEM('')
);
#4270=(
BOUNDED_CURVE()
B_SPLINE_CURVE(2,(#371741,#371742,#371743,#371744,#371745,#371746,#371747,
#371748,#371749,#371750,#371751,#371752,#371753),.UNSPECIFIED.,.F.,.F.)
B_SPLINE_CURVE_WITH_KNOTS((3,2,2,2,2,2,3),(0.145161290322581,0.150537634408602,
0.155913978494624,0.161290322580645,0.166666666666667,0.172043010752688,
0.17741935483871),.UNSPECIFIED.)
CURVE()
GEOMETRIC_REPRESENTATION_ITEM()
RATIONAL_B_SPLINE_CURVE((1.,0.866025403784439,1.,0.866025403784439,1.,0.866025403784439,
1.,0.866025403784439,1.,0.866025403784439,1.,0.866025403784439,1.))
REPRESENTATION_ITEM('')
);
#4271=(
BOUNDED_CURVE()
B_SPLINE_CURVE(2,(#371754,#371755,#371756,#371757,#371758,#371759,#371760,
#371761,#371762,#371763,#371764,#371765,#371766),.UNSPECIFIED.,.F.,.F.)
B_SPLINE_CURVE_WITH_KNOTS((3,2,2,2,2,2,3),(0.145161290322581,0.150537634408602,
0.155913978494624,0.161290322580645,0.166666666666667,0.172043010752688,
0.17741935483871),.UNSPECIFIED.)
CURVE()
GEOMETRIC_REPRESENTATION_ITEM()
RATIONAL_B_SPLINE_CURVE((1.,0.866025403784439,1.,0.866025403784439,1.,0.866025403784439,
1.,0.866025403784439,1.,0.866025403784439,1.,0.866025403784439,1.))
REPRESENTATION_ITEM('')
);
#4272=(
BOUNDED_CURVE()
B_SPLINE_CURVE(2,(#371771,#371772,#371773,#371774,#371775,#371776,#371777,
#371778,#371779,#371780,#371781,#371782,#371783),.UNSPECIFIED.,.F.,.F.)
B_SPLINE_CURVE_WITH_KNOTS((3,2,2,2,2,2,3),(0.17741935483871,0.182795698924731,
0.188172043010753,0.193548387096774,0.198924731182796,0.204301075268817,
0.209677419354839),.UNSPECIFIED.)
CURVE()
GEOMETRIC_REPRESENTATION_ITEM()
RATIONAL_B_SPLINE_CURVE((1.,0.866025403784439,1.,0.866025403784439,1.,0.866025403784439,
1.,0.866025403784439,1.,0.866025403784439,1.,0.866025403784439,1.))
REPRESENTATION_ITEM('')
);
#4273=(
BOUNDED_CURVE()
B_SPLINE_CURVE(2,(#371784,#371785,#371786,#371787,#371788,#371789,#371790,
#371791,#371792,#371793,#371794,#371795,#371796),.UNSPECIFIED.,.F.,.F.)
B_SPLINE_CURVE_WITH_KNOTS((3,2,2,2,2,2,3),(0.17741935483871,0.182795698924731,
0.188172043010753,0.193548387096774,0.198924731182796,0.204301075268817,
0.209677419354839),.UNSPECIFIED.)
CURVE()
GEOMETRIC_REPRESENTATION_ITEM()
RATIONAL_B_SPLINE_CURVE((1.,0.866025403784439,1.,0.866025403784439,1.,0.866025403784439,
1.,0.866025403784439,1.,0.866025403784439,1.,0.866025403784439,1.))
REPRESENTATION_ITEM('')
);
#4274=(
BOUNDED_CURVE()
B_SPLINE_CURVE(2,(#371801,#371802,#371803,#371804,#371805,#371806,#371807,
#371808,#371809,#371810,#371811,#371812,#371813),.UNSPECIFIED.,.F.,.F.)
B_SPLINE_CURVE_WITH_KNOTS((3,2,2,2,2,2,3),(0.209677419354839,0.21505376344086,
0.220430107526882,0.225806451612903,0.231182795698925,0.236559139784946,
0.241935483870968),.UNSPECIFIED.)
CURVE()
GEOMETRIC_REPRESENTATION_ITEM()
RATIONAL_B_SPLINE_CURVE((1.,0.866025403784439,1.,0.866025403784439,1.,0.866025403784439,
1.,0.866025403784439,1.,0.866025403784439,1.,0.866025403784439,1.))
REPRESENTATION_ITEM('')
);
#4275=(
BOUNDED_CURVE()
B_SPLINE_CURVE(2,(#371814,#371815,#371816,#371817,#371818,#371819,#371820,
#371821,#371822,#371823,#371824,#371825,#371826),.UNSPECIFIED.,.F.,.F.)
B_SPLINE_CURVE_WITH_KNOTS((3,2,2,2,2,2,3),(0.209677419354839,0.21505376344086,
0.220430107526882,0.225806451612903,0.231182795698925,0.236559139784946,
0.241935483870968),.UNSPECIFIED.)
CURVE()
GEOMETRIC_REPRESENTATION_ITEM()
RATIONAL_B_SPLINE_CURVE((1.,0.866025403784439,1.,0.866025403784439,1.,0.866025403784439,
1.,0.866025403784439,1.,0.866025403784439,1.,0.866025403784439,1.))
REPRESENTATION_ITEM('')
);
#4276=(
BOUNDED_CURVE()
B_SPLINE_CURVE(2,(#371831,#371832,#371833,#371834,#371835,#371836,#371837,
#371838,#371839,#371840,#371841,#371842,#371843),.UNSPECIFIED.,.F.,.F.)
B_SPLINE_CURVE_WITH_KNOTS((3,2,2,2,2,2,3),(0.241935483870968,0.247311827956989,
0.252688172043011,0.258064516129032,0.263440860215054,0.268817204301075,
0.274193548387097),.UNSPECIFIED.)
CURVE()
GEOMETRIC_REPRESENTATION_ITEM()
RATIONAL_B_SPLINE_CURVE((1.,0.866025403784439,1.,0.866025403784439,1.,0.866025403784439,
1.,0.866025403784439,1.,0.866025403784439,1.,0.866025403784439,1.))
REPRESENTATION_ITEM('')
);
#4277=(
BOUNDED_CURVE()
B_SPLINE_CURVE(2,(#371844,#371845,#371846,#371847,#371848,#371849,#371850,
#371851,#371852,#371853,#371854,#371855,#371856),.UNSPECIFIED.,.F.,.F.)
B_SPLINE_CURVE_WITH_KNOTS((3,2,2,2,2,2,3),(0.241935483870968,0.247311827956989,
0.252688172043011,0.258064516129032,0.263440860215054,0.268817204301075,
0.274193548387097),.UNSPECIFIED.)
CURVE()
GEOMETRIC_REPRESENTATION_ITEM()
RATIONAL_B_SPLINE_CURVE((1.,0.866025403784439,1.,0.866025403784439,1.,0.866025403784439,
1.,0.866025403784439,1.,0.866025403784439,1.,0.866025403784439,1.))
REPRESENTATION_ITEM('')
);
#4278=(
BOUNDED_CURVE()
B_SPLINE_CURVE(2,(#371861,#371862,#371863,#371864,#371865,#371866,#371867,
#371868,#371869,#371870,#371871,#371872,#371873),.UNSPECIFIED.,.F.,.F.)
B_SPLINE_CURVE_WITH_KNOTS((3,2,2,2,2,2,3),(0.274193548387097,0.279569892473118,
0.28494623655914,0.290322580645161,0.295698924731183,0.301075268817204,
0.306451612903226),.UNSPECIFIED.)
CURVE()
GEOMETRIC_REPRESENTATION_ITEM()
RATIONAL_B_SPLINE_CURVE((1.,0.866025403784439,1.,0.866025403784439,1.,0.866025403784439,
1.,0.866025403784439,1.,0.866025403784439,1.,0.866025403784439,1.))
REPRESENTATION_ITEM('')
);
#4279=(
BOUNDED_CURVE()
B_SPLINE_CURVE(2,(#371874,#371875,#371876,#371877,#371878,#371879,#371880,
#371881,#371882,#371883,#371884,#371885,#371886),.UNSPECIFIED.,.F.,.F.)
B_SPLINE_CURVE_WITH_KNOTS((3,2,2,2,2,2,3),(0.274193548387097,0.279569892473118,
0.28494623655914,0.290322580645161,0.295698924731183,0.301075268817204,
0.306451612903226),.UNSPECIFIED.)
CURVE()
GEOMETRIC_REPRESENTATION_ITEM()
RATIONAL_B_SPLINE_CURVE((1.,0.866025403784439,1.,0.866025403784439,1.,0.866025403784439,
1.,0.866025403784439,1.,0.866025403784439,1.,0.866025403784439,1.))
REPRESENTATION_ITEM('')
);
#4280=(
BOUNDED_CURVE()
B_SPLINE_CURVE(2,(#371891,#371892,#371893,#371894,#371895,#371896,#371897,
#371898,#371899,#371900,#371901,#371902,#371903),.UNSPECIFIED.,.F.,.F.)
B_SPLINE_CURVE_WITH_KNOTS((3,2,2,2,2,2,3),(0.306451612903226,0.311827956989247,
0.317204301075269,0.32258064516129,0.327956989247312,0.333333333333333,
0.338709677419355),.UNSPECIFIED.)
CURVE()
GEOMETRIC_REPRESENTATION_ITEM()
RATIONAL_B_SPLINE_CURVE((1.,0.866025403784439,1.,0.866025403784439,1.,0.866025403784439,
1.,0.866025403784439,1.,0.866025403784439,1.,0.866025403784439,1.))
REPRESENTATION_ITEM('')
);
#4281=(
BOUNDED_CURVE()
B_SPLINE_CURVE(2,(#371904,#371905,#371906,#371907,#371908,#371909,#371910,
#371911,#371912,#371913,#371914,#371915,#371916),.UNSPECIFIED.,.F.,.F.)
B_SPLINE_CURVE_WITH_KNOTS((3,2,2,2,2,2,3),(0.306451612903226,0.311827956989247,
0.317204301075269,0.32258064516129,0.327956989247312,0.333333333333333,
0.338709677419355),.UNSPECIFIED.)
CURVE()
GEOMETRIC_REPRESENTATION_ITEM()
RATIONAL_B_SPLINE_CURVE((1.,0.866025403784439,1.,0.866025403784439,1.,0.866025403784439,
1.,0.866025403784439,1.,0.866025403784439,1.,0.866025403784439,1.))
REPRESENTATION_ITEM('')
);
#4282=(
BOUNDED_CURVE()
B_SPLINE_CURVE(2,(#371921,#371922,#371923,#371924,#371925,#371926,#371927,
#371928,#371929,#371930,#371931,#371932,#371933),.UNSPECIFIED.,.F.,.F.)
B_SPLINE_CURVE_WITH_KNOTS((3,2,2,2,2,2,3),(0.338709677419355,0.344086021505376,
0.349462365591398,0.354838709677419,0.360215053763441,0.365591397849462,
0.370967741935484),.UNSPECIFIED.)
CURVE()
GEOMETRIC_REPRESENTATION_ITEM()
RATIONAL_B_SPLINE_CURVE((1.,0.866025403784439,1.,0.866025403784439,1.,0.866025403784439,
1.,0.866025403784439,1.,0.866025403784439,1.,0.866025403784439,1.))
REPRESENTATION_ITEM('')
);
#4283=(
BOUNDED_CURVE()
B_SPLINE_CURVE(2,(#371934,#371935,#371936,#371937,#371938,#371939,#371940,
#371941,#371942,#371943,#371944,#371945,#371946),.UNSPECIFIED.,.F.,.F.)
B_SPLINE_CURVE_WITH_KNOTS((3,2,2,2,2,2,3),(0.338709677419355,0.344086021505376,
0.349462365591398,0.354838709677419,0.360215053763441,0.365591397849462,
0.370967741935484),.UNSPECIFIED.)
CURVE()
GEOMETRIC_REPRESENTATION_ITEM()
RATIONAL_B_SPLINE_CURVE((1.,0.866025403784439,1.,0.866025403784439,1.,0.866025403784439,
1.,0.866025403784439,1.,0.866025403784439,1.,0.866025403784439,1.))
REPRESENTATION_ITEM('')
);
#4284=(
BOUNDED_CURVE()
B_SPLINE_CURVE(2,(#371951,#371952,#371953,#371954,#371955,#371956,#371957,
#371958,#371959,#371960,#371961,#371962,#371963),.UNSPECIFIED.,.F.,.F.)
B_SPLINE_CURVE_WITH_KNOTS((3,2,2,2,2,2,3),(0.370967741935484,0.376344086021505,
0.381720430107527,0.387096774193548,0.39247311827957,0.397849462365591,
0.403225806451613),.UNSPECIFIED.)
CURVE()
GEOMETRIC_REPRESENTATION_ITEM()
RATIONAL_B_SPLINE_CURVE((1.,0.866025403784439,1.,0.866025403784439,1.,0.866025403784439,
1.,0.866025403784439,1.,0.866025403784439,1.,0.866025403784439,1.))
REPRESENTATION_ITEM('')
);
#4285=(
BOUNDED_CURVE()
B_SPLINE_CURVE(2,(#371964,#371965,#371966,#371967,#371968,#371969,#371970,
#371971,#371972,#371973,#371974,#371975,#371976),.UNSPECIFIED.,.F.,.F.)
B_SPLINE_CURVE_WITH_KNOTS((3,2,2,2,2,2,3),(0.370967741935484,0.376344086021505,
0.381720430107527,0.387096774193548,0.39247311827957,0.397849462365591,
0.403225806451613),.UNSPECIFIED.)
CURVE()
GEOMETRIC_REPRESENTATION_ITEM()
RATIONAL_B_SPLINE_CURVE((1.,0.866025403784439,1.,0.866025403784439,1.,0.866025403784439,
1.,0.866025403784439,1.,0.866025403784439,1.,0.866025403784439,1.))
REPRESENTATION_ITEM('')
);
#4286=(
BOUNDED_CURVE()
B_SPLINE_CURVE(2,(#371981,#371982,#371983,#371984,#371985,#371986,#371987,
#371988,#371989,#371990,#371991,#371992,#371993),.UNSPECIFIED.,.F.,.F.)
B_SPLINE_CURVE_WITH_KNOTS((3,2,2,2,2,2,3),(0.403225806451613,0.408602150537634,
0.413978494623656,0.419354838709677,0.424731182795699,0.43010752688172,
0.435483870967742),.UNSPECIFIED.)
CURVE()
GEOMETRIC_REPRESENTATION_ITEM()
RATIONAL_B_SPLINE_CURVE((1.,0.866025403784439,1.,0.866025403784439,1.,0.866025403784439,
1.,0.866025403784439,1.,0.866025403784439,1.,0.866025403784439,1.))
REPRESENTATION_ITEM('')
);
#4287=(
BOUNDED_CURVE()
B_SPLINE_CURVE(2,(#371994,#371995,#371996,#371997,#371998,#371999,#372000,
#372001,#372002,#372003,#372004,#372005,#372006),.UNSPECIFIED.,.F.,.F.)
B_SPLINE_CURVE_WITH_KNOTS((3,2,2,2,2,2,3),(0.403225806451613,0.408602150537634,
0.413978494623656,0.419354838709677,0.424731182795699,0.43010752688172,
0.435483870967742),.UNSPECIFIED.)
CURVE()
GEOMETRIC_REPRESENTATION_ITEM()
RATIONAL_B_SPLINE_CURVE((1.,0.866025403784439,1.,0.866025403784439,1.,0.866025403784439,
1.,0.866025403784439,1.,0.866025403784439,1.,0.866025403784439,1.))
REPRESENTATION_ITEM('')
);
#4288=(
BOUNDED_CURVE()
B_SPLINE_CURVE(2,(#372011,#372012,#372013,#372014,#372015,#372016,#372017,
#372018,#372019,#372020,#372021,#372022,#372023),.UNSPECIFIED.,.F.,.F.)
B_SPLINE_CURVE_WITH_KNOTS((3,2,2,2,2,2,3),(0.435483870967742,0.440860215053763,
0.446236559139785,0.451612903225806,0.456989247311828,0.462365591397849,
0.467741935483871),.UNSPECIFIED.)
CURVE()
GEOMETRIC_REPRESENTATION_ITEM()
RATIONAL_B_SPLINE_CURVE((1.,0.866025403784439,1.,0.866025403784439,1.,0.866025403784439,
1.,0.866025403784439,1.,0.866025403784439,1.,0.866025403784439,1.))
REPRESENTATION_ITEM('')
);
#4289=(
BOUNDED_CURVE()
B_SPLINE_CURVE(2,(#372024,#372025,#372026,#372027,#372028,#372029,#372030,
#372031,#372032,#372033,#372034,#372035,#372036),.UNSPECIFIED.,.F.,.F.)
B_SPLINE_CURVE_WITH_KNOTS((3,2,2,2,2,2,3),(0.435483870967742,0.440860215053763,
0.446236559139785,0.451612903225806,0.456989247311828,0.462365591397849,
0.467741935483871),.UNSPECIFIED.)
CURVE()
GEOMETRIC_REPRESENTATION_ITEM()
RATIONAL_B_SPLINE_CURVE((1.,0.866025403784439,1.,0.866025403784439,1.,0.866025403784439,
1.,0.866025403784439,1.,0.866025403784439,1.,0.866025403784439,1.))
REPRESENTATION_ITEM('')
);
#4290=(
BOUNDED_CURVE()
B_SPLINE_CURVE(2,(#372041,#372042,#372043,#372044,#372045,#372046,#372047,
#372048,#372049,#372050,#372051,#372052,#372053),.UNSPECIFIED.,.F.,.F.)
B_SPLINE_CURVE_WITH_KNOTS((3,2,2,2,2,2,3),(0.467741935483871,0.473118279569892,
0.478494623655914,0.483870967741935,0.489247311827957,0.494623655913979,
0.5),.UNSPECIFIED.)
CURVE()
GEOMETRIC_REPRESENTATION_ITEM()
RATIONAL_B_SPLINE_CURVE((1.,0.866025403784439,1.,0.866025403784439,1.,0.866025403784439,
1.,0.866025403784439,1.,0.866025403784439,1.,0.866025403784439,1.))
REPRESENTATION_ITEM('')
);
#4291=(
BOUNDED_CURVE()
B_SPLINE_CURVE(2,(#372054,#372055,#372056,#372057,#372058,#372059,#372060,
#372061,#372062,#372063,#372064,#372065,#372066),.UNSPECIFIED.,.F.,.F.)
B_SPLINE_CURVE_WITH_KNOTS((3,2,2,2,2,2,3),(0.467741935483871,0.473118279569892,
0.478494623655914,0.483870967741935,0.489247311827957,0.494623655913978,
0.5),.UNSPECIFIED.)
CURVE()
GEOMETRIC_REPRESENTATION_ITEM()
RATIONAL_B_SPLINE_CURVE((1.,0.866025403784439,1.,0.866025403784439,1.,0.866025403784439,
1.,0.866025403784439,1.,0.866025403784439,1.,0.866025403784439,1.))
REPRESENTATION_ITEM('')
);
#4292=(
BOUNDED_CURVE()
B_SPLINE_CURVE(2,(#372071,#372072,#372073,#372074,#372075,#372076,#372077,
#372078,#372079,#372080,#372081,#372082,#372083),.UNSPECIFIED.,.F.,.F.)
B_SPLINE_CURVE_WITH_KNOTS((3,2,2,2,2,2,3),(0.5,0.505376344086022,0.510752688172043,
0.516129032258065,0.521505376344086,0.526881720430108,0.532258064516129),
 .UNSPECIFIED.)
CURVE()
GEOMETRIC_REPRESENTATION_ITEM()
RATIONAL_B_SPLINE_CURVE((1.,0.866025403784439,1.,0.866025403784439,1.,0.866025403784439,
1.,0.866025403784439,1.,0.866025403784439,1.,0.866025403784439,1.))
REPRESENTATION_ITEM('')
);
#4293=(
BOUNDED_CURVE()
B_SPLINE_CURVE(2,(#372084,#372085,#372086,#372087,#372088,#372089,#372090,
#372091,#372092,#372093,#372094,#372095,#372096),.UNSPECIFIED.,.F.,.F.)
B_SPLINE_CURVE_WITH_KNOTS((3,2,2,2,2,2,3),(0.5,0.505376344086022,0.510752688172043,
0.516129032258065,0.521505376344086,0.526881720430108,0.532258064516129),
 .UNSPECIFIED.)
CURVE()
GEOMETRIC_REPRESENTATION_ITEM()
RATIONAL_B_SPLINE_CURVE((1.,0.866025403784439,1.,0.866025403784439,1.,0.866025403784439,
1.,0.866025403784439,1.,0.866025403784439,1.,0.866025403784439,1.))
REPRESENTATION_ITEM('')
);
#4294=(
BOUNDED_CURVE()
B_SPLINE_CURVE(2,(#372101,#372102,#372103,#372104,#372105,#372106,#372107,
#372108,#372109,#372110,#372111,#372112,#372113),.UNSPECIFIED.,.F.,.F.)
B_SPLINE_CURVE_WITH_KNOTS((3,2,2,2,2,2,3),(0.532258064516129,0.537634408602151,
0.543010752688172,0.548387096774194,0.553763440860215,0.559139784946237,
0.564516129032258),.UNSPECIFIED.)
CURVE()
GEOMETRIC_REPRESENTATION_ITEM()
RATIONAL_B_SPLINE_CURVE((1.,0.866025403784439,1.,0.866025403784439,1.,0.866025403784439,
1.,0.866025403784439,1.,0.866025403784439,1.,0.866025403784439,1.))
REPRESENTATION_ITEM('')
);
#4295=(
BOUNDED_CURVE()
B_SPLINE_CURVE(2,(#372114,#372115,#372116,#372117,#372118,#372119,#372120,
#372121,#372122,#372123,#372124,#372125,#372126),.UNSPECIFIED.,.F.,.F.)
B_SPLINE_CURVE_WITH_KNOTS((3,2,2,2,2,2,3),(0.532258064516129,0.537634408602151,
0.543010752688172,0.548387096774194,0.553763440860215,0.559139784946237,
0.564516129032258),.UNSPECIFIED.)
CURVE()
GEOMETRIC_REPRESENTATION_ITEM()
RATIONAL_B_SPLINE_CURVE((1.,0.866025403784439,1.,0.866025403784439,1.,0.866025403784439,
1.,0.866025403784439,1.,0.866025403784439,1.,0.866025403784439,1.))
REPRESENTATION_ITEM('')
);
#4296=(
BOUNDED_CURVE()
B_SPLINE_CURVE(2,(#372131,#372132,#372133,#372134,#372135,#372136,#372137,
#372138,#372139,#372140,#372141,#372142,#372143),.UNSPECIFIED.,.F.,.F.)
B_SPLINE_CURVE_WITH_KNOTS((3,2,2,2,2,2,3),(0.564516129032258,0.56989247311828,
0.575268817204301,0.580645161290323,0.586021505376344,0.591397849462366,
0.596774193548387),.UNSPECIFIED.)
CURVE()
GEOMETRIC_REPRESENTATION_ITEM()
RATIONAL_B_SPLINE_CURVE((1.,0.866025403784439,1.,0.866025403784439,1.,0.866025403784439,
1.,0.866025403784439,1.,0.866025403784439,1.,0.866025403784439,1.))
REPRESENTATION_ITEM('')
);
#4297=(
BOUNDED_CURVE()
B_SPLINE_CURVE(2,(#372144,#372145,#372146,#372147,#372148,#372149,#372150,
#372151,#372152,#372153,#372154,#372155,#372156),.UNSPECIFIED.,.F.,.F.)
B_SPLINE_CURVE_WITH_KNOTS((3,2,2,2,2,2,3),(0.564516129032258,0.56989247311828,
0.575268817204301,0.580645161290323,0.586021505376344,0.591397849462366,
0.596774193548387),.UNSPECIFIED.)
CURVE()
GEOMETRIC_REPRESENTATION_ITEM()
RATIONAL_B_SPLINE_CURVE((1.,0.866025403784439,1.,0.866025403784439,1.,0.866025403784439,
1.,0.866025403784439,1.,0.866025403784439,1.,0.866025403784439,1.))
REPRESENTATION_ITEM('')
);
#4298=(
BOUNDED_CURVE()
B_SPLINE_CURVE(2,(#372161,#372162,#372163,#372164,#372165,#372166,#372167,
#372168,#372169,#372170,#372171,#372172,#372173),.UNSPECIFIED.,.F.,.F.)
B_SPLINE_CURVE_WITH_KNOTS((3,2,2,2,2,2,3),(0.596774193548387,0.602150537634409,
0.60752688172043,0.612903225806452,0.618279569892473,0.623655913978495,
0.629032258064516),.UNSPECIFIED.)
CURVE()
GEOMETRIC_REPRESENTATION_ITEM()
RATIONAL_B_SPLINE_CURVE((1.,0.866025403784439,1.,0.866025403784439,1.,0.866025403784439,
1.,0.866025403784439,1.,0.866025403784439,1.,0.866025403784439,1.))
REPRESENTATION_ITEM('')
);
#4299=(
BOUNDED_CURVE()
B_SPLINE_CURVE(2,(#372174,#372175,#372176,#372177,#372178,#372179,#372180,
#372181,#372182,#372183,#372184,#372185,#372186),.UNSPECIFIED.,.F.,.F.)
B_SPLINE_CURVE_WITH_KNOTS((3,2,2,2,2,2,3),(0.596774193548387,0.602150537634409,
0.60752688172043,0.612903225806452,0.618279569892473,0.623655913978495,
0.629032258064516),.UNSPECIFIED.)
CURVE()
GEOMETRIC_REPRESENTATION_ITEM()
RATIONAL_B_SPLINE_CURVE((1.,0.866025403784439,1.,0.866025403784439,1.,0.866025403784439,
1.,0.866025403784439,1.,0.866025403784439,1.,0.866025403784439,1.))
REPRESENTATION_ITEM('')
);
#4300=(
BOUNDED_CURVE()
B_SPLINE_CURVE(2,(#372191,#372192,#372193,#372194,#372195,#372196,#372197,
#372198,#372199,#372200,#372201,#372202,#372203),.UNSPECIFIED.,.F.,.F.)
B_SPLINE_CURVE_WITH_KNOTS((3,2,2,2,2,2,3),(0.629032258064516,0.634408602150538,
0.639784946236559,0.645161290322581,0.650537634408602,0.655913978494624,
0.661290322580645),.UNSPECIFIED.)
CURVE()
GEOMETRIC_REPRESENTATION_ITEM()
RATIONAL_B_SPLINE_CURVE((1.,0.866025403784439,1.,0.866025403784439,1.,0.866025403784439,
1.,0.866025403784439,1.,0.866025403784439,1.,0.866025403784439,1.))
REPRESENTATION_ITEM('')
);
#4301=(
BOUNDED_CURVE()
B_SPLINE_CURVE(2,(#372204,#372205,#372206,#372207,#372208,#372209,#372210,
#372211,#372212,#372213,#372214,#372215,#372216),.UNSPECIFIED.,.F.,.F.)
B_SPLINE_CURVE_WITH_KNOTS((3,2,2,2,2,2,3),(0.629032258064516,0.634408602150538,
0.639784946236559,0.645161290322581,0.650537634408602,0.655913978494624,
0.661290322580645),.UNSPECIFIED.)
CURVE()
GEOMETRIC_REPRESENTATION_ITEM()
RATIONAL_B_SPLINE_CURVE((1.,0.866025403784439,1.,0.866025403784439,1.,0.866025403784439,
1.,0.866025403784439,1.,0.866025403784439,1.,0.866025403784439,1.))
REPRESENTATION_ITEM('')
);
#4302=(
BOUNDED_CURVE()
B_SPLINE_CURVE(2,(#372221,#372222,#372223,#372224,#372225,#372226,#372227,
#372228,#372229,#372230,#372231,#372232,#372233),.UNSPECIFIED.,.F.,.F.)
B_SPLINE_CURVE_WITH_KNOTS((3,2,2,2,2,2,3),(0.661290322580645,0.666666666666667,
0.672043010752688,0.67741935483871,0.682795698924731,0.688172043010753,
0.693548387096774),.UNSPECIFIED.)
CURVE()
GEOMETRIC_REPRESENTATION_ITEM()
RATIONAL_B_SPLINE_CURVE((1.,0.866025403784439,1.,0.866025403784439,1.,0.866025403784439,
1.,0.866025403784439,1.,0.866025403784439,1.,0.866025403784439,1.))
REPRESENTATION_ITEM('')
);
#4303=(
BOUNDED_CURVE()
B_SPLINE_CURVE(2,(#372234,#372235,#372236,#372237,#372238,#372239,#372240,
#372241,#372242,#372243,#372244,#372245,#372246),.UNSPECIFIED.,.F.,.F.)
B_SPLINE_CURVE_WITH_KNOTS((3,2,2,2,2,2,3),(0.661290322580645,0.666666666666667,
0.672043010752688,0.67741935483871,0.682795698924731,0.688172043010753,
0.693548387096774),.UNSPECIFIED.)
CURVE()
GEOMETRIC_REPRESENTATION_ITEM()
RATIONAL_B_SPLINE_CURVE((1.,0.866025403784439,1.,0.866025403784439,1.,0.866025403784439,
1.,0.866025403784439,1.,0.866025403784439,1.,0.866025403784439,1.))
REPRESENTATION_ITEM('')
);
#4304=(
BOUNDED_CURVE()
B_SPLINE_CURVE(2,(#372251,#372252,#372253,#372254,#372255,#372256,#372257,
#372258,#372259,#372260,#372261,#372262,#372263),.UNSPECIFIED.,.F.,.F.)
B_SPLINE_CURVE_WITH_KNOTS((3,2,2,2,2,2,3),(0.693548387096774,0.698924731182796,
0.704301075268817,0.709677419354839,0.71505376344086,0.720430107526882,
0.725806451612903),.UNSPECIFIED.)
CURVE()
GEOMETRIC_REPRESENTATION_ITEM()
RATIONAL_B_SPLINE_CURVE((1.,0.866025403784439,1.,0.866025403784439,1.,0.866025403784439,
1.,0.866025403784439,1.,0.866025403784439,1.,0.866025403784439,1.))
REPRESENTATION_ITEM('')
);
#4305=(
BOUNDED_CURVE()
B_SPLINE_CURVE(2,(#372264,#372265,#372266,#372267,#372268,#372269,#372270,
#372271,#372272,#372273,#372274,#372275,#372276),.UNSPECIFIED.,.F.,.F.)
B_SPLINE_CURVE_WITH_KNOTS((3,2,2,2,2,2,3),(0.693548387096774,0.698924731182796,
0.704301075268817,0.709677419354839,0.71505376344086,0.720430107526882,
0.725806451612903),.UNSPECIFIED.)
CURVE()
GEOMETRIC_REPRESENTATION_ITEM()
RATIONAL_B_SPLINE_CURVE((1.,0.866025403784439,1.,0.866025403784439,1.,0.866025403784439,
1.,0.866025403784439,1.,0.866025403784439,1.,0.866025403784439,1.))
REPRESENTATION_ITEM('')
);
#4306=(
BOUNDED_CURVE()
B_SPLINE_CURVE(2,(#372281,#372282,#372283,#372284,#372285,#372286,#372287,
#372288,#372289,#372290,#372291,#372292,#372293),.UNSPECIFIED.,.F.,.F.)
B_SPLINE_CURVE_WITH_KNOTS((3,2,2,2,2,2,3),(0.725806451612903,0.731182795698925,
0.736559139784946,0.741935483870968,0.747311827956989,0.752688172043011,
0.758064516129032),.UNSPECIFIED.)
CURVE()
GEOMETRIC_REPRESENTATION_ITEM()
RATIONAL_B_SPLINE_CURVE((1.,0.866025403784439,1.,0.866025403784439,1.,0.866025403784439,
1.,0.866025403784439,1.,0.866025403784439,1.,0.866025403784439,1.))
REPRESENTATION_ITEM('')
);
#4307=(
BOUNDED_CURVE()
B_SPLINE_CURVE(2,(#372294,#372295,#372296,#372297,#372298,#372299,#372300,
#372301,#372302,#372303,#372304,#372305,#372306),.UNSPECIFIED.,.F.,.F.)
B_SPLINE_CURVE_WITH_KNOTS((3,2,2,2,2,2,3),(0.725806451612903,0.731182795698925,
0.736559139784946,0.741935483870968,0.747311827956989,0.752688172043011,
0.758064516129032),.UNSPECIFIED.)
CURVE()
GEOMETRIC_REPRESENTATION_ITEM()
RATIONAL_B_SPLINE_CURVE((1.,0.866025403784439,1.,0.866025403784439,1.,0.866025403784439,
1.,0.866025403784439,1.,0.866025403784439,1.,0.866025403784439,1.))
REPRESENTATION_ITEM('')
);
#4308=(
BOUNDED_CURVE()
B_SPLINE_CURVE(2,(#372311,#372312,#372313,#372314,#372315,#372316,#372317,
#372318,#372319,#372320,#372321,#372322,#372323),.UNSPECIFIED.,.F.,.F.)
B_SPLINE_CURVE_WITH_KNOTS((3,2,2,2,2,2,3),(0.758064516129032,0.763440860215054,
0.768817204301075,0.774193548387097,0.779569892473118,0.78494623655914,
0.790322580645161),.UNSPECIFIED.)
CURVE()
GEOMETRIC_REPRESENTATION_ITEM()
RATIONAL_B_SPLINE_CURVE((1.,0.866025403784439,1.,0.866025403784439,1.,0.866025403784439,
1.,0.866025403784439,1.,0.866025403784439,1.,0.866025403784439,1.))
REPRESENTATION_ITEM('')
);
#4309=(
BOUNDED_CURVE()
B_SPLINE_CURVE(2,(#372324,#372325,#372326,#372327,#372328,#372329,#372330,
#372331,#372332,#372333,#372334,#372335,#372336),.UNSPECIFIED.,.F.,.F.)
B_SPLINE_CURVE_WITH_KNOTS((3,2,2,2,2,2,3),(0.758064516129032,0.763440860215054,
0.768817204301075,0.774193548387097,0.779569892473118,0.78494623655914,
0.790322580645161),.UNSPECIFIED.)
CURVE()
GEOMETRIC_REPRESENTATION_ITEM()
RATIONAL_B_SPLINE_CURVE((1.,0.866025403784439,1.,0.866025403784439,1.,0.866025403784439,
1.,0.866025403784439,1.,0.866025403784439,1.,0.866025403784439,1.))
REPRESENTATION_ITEM('')
);
#4310=(
BOUNDED_CURVE()
B_SPLINE_CURVE(2,(#372341,#372342,#372343,#372344,#372345,#372346,#372347,
#372348,#372349,#372350,#372351,#372352,#372353),.UNSPECIFIED.,.F.,.F.)
B_SPLINE_CURVE_WITH_KNOTS((3,2,2,2,2,2,3),(0.790322580645161,0.795698924731183,
0.801075268817204,0.806451612903226,0.811827956989247,0.817204301075269,
0.82258064516129),.UNSPECIFIED.)
CURVE()
GEOMETRIC_REPRESENTATION_ITEM()
RATIONAL_B_SPLINE_CURVE((1.,0.866025403784439,1.,0.866025403784439,1.,0.866025403784439,
1.,0.866025403784439,1.,0.866025403784439,1.,0.866025403784439,1.))
REPRESENTATION_ITEM('')
);
#4311=(
BOUNDED_CURVE()
B_SPLINE_CURVE(2,(#372354,#372355,#372356,#372357,#372358,#372359,#372360,
#372361,#372362,#372363,#372364,#372365,#372366),.UNSPECIFIED.,.F.,.F.)
B_SPLINE_CURVE_WITH_KNOTS((3,2,2,2,2,2,3),(0.790322580645161,0.795698924731183,
0.801075268817204,0.806451612903226,0.811827956989247,0.817204301075269,
0.82258064516129),.UNSPECIFIED.)
CURVE()
GEOMETRIC_REPRESENTATION_ITEM()
RATIONAL_B_SPLINE_CURVE((1.,0.866025403784439,1.,0.866025403784439,1.,0.866025403784439,
1.,0.866025403784439,1.,0.866025403784439,1.,0.866025403784439,1.))
REPRESENTATION_ITEM('')
);
#4312=(
BOUNDED_CURVE()
B_SPLINE_CURVE(2,(#372371,#372372,#372373,#372374,#372375,#372376,#372377,
#372378,#372379,#372380,#372381,#372382,#372383),.UNSPECIFIED.,.F.,.F.)
B_SPLINE_CURVE_WITH_KNOTS((3,2,2,2,2,2,3),(0.82258064516129,0.827956989247312,
0.833333333333333,0.838709677419355,0.844086021505376,0.849462365591398,
0.854838709677419),.UNSPECIFIED.)
CURVE()
GEOMETRIC_REPRESENTATION_ITEM()
RATIONAL_B_SPLINE_CURVE((1.,0.866025403784439,1.,0.866025403784439,1.,0.866025403784439,
1.,0.866025403784439,1.,0.866025403784439,1.,0.866025403784439,1.))
REPRESENTATION_ITEM('')
);
#4313=(
BOUNDED_CURVE()
B_SPLINE_CURVE(2,(#372384,#372385,#372386,#372387,#372388,#372389,#372390,
#372391,#372392,#372393,#372394,#372395,#372396),.UNSPECIFIED.,.F.,.F.)
B_SPLINE_CURVE_WITH_KNOTS((3,2,2,2,2,2,3),(0.82258064516129,0.827956989247312,
0.833333333333333,0.838709677419355,0.844086021505376,0.849462365591398,
0.854838709677419),.UNSPECIFIED.)
CURVE()
GEOMETRIC_REPRESENTATION_ITEM()
RATIONAL_B_SPLINE_CURVE((1.,0.866025403784439,1.,0.866025403784439,1.,0.866025403784439,
1.,0.866025403784439,1.,0.866025403784439,1.,0.866025403784439,1.))
REPRESENTATION_ITEM('')
);
#4314=(
BOUNDED_CURVE()
B_SPLINE_CURVE(2,(#372401,#372402,#372403,#372404,#372405,#372406,#372407,
#372408,#372409,#372410,#372411,#372412,#372413),.UNSPECIFIED.,.F.,.F.)
B_SPLINE_CURVE_WITH_KNOTS((3,2,2,2,2,2,3),(0.854838709677419,0.860215053763441,
0.865591397849462,0.870967741935484,0.876344086021505,0.881720430107527,
0.887096774193548),.UNSPECIFIED.)
CURVE()
GEOMETRIC_REPRESENTATION_ITEM()
RATIONAL_B_SPLINE_CURVE((1.,0.866025403784439,1.,0.866025403784439,1.,0.866025403784439,
1.,0.866025403784439,1.,0.866025403784439,1.,0.866025403784439,1.))
REPRESENTATION_ITEM('')
);
#4315=(
BOUNDED_CURVE()
B_SPLINE_CURVE(2,(#372414,#372415,#372416,#372417,#372418,#372419,#372420,
#372421,#372422,#372423,#372424,#372425,#372426),.UNSPECIFIED.,.F.,.F.)
B_SPLINE_CURVE_WITH_KNOTS((3,2,2,2,2,2,3),(0.854838709677419,0.860215053763441,
0.865591397849462,0.870967741935484,0.876344086021505,0.881720430107527,
0.887096774193548),.UNSPECIFIED.)
CURVE()
GEOMETRIC_REPRESENTATION_ITEM()
RATIONAL_B_SPLINE_CURVE((1.,0.866025403784439,1.,0.866025403784439,1.,0.866025403784439,
1.,0.866025403784439,1.,0.866025403784439,1.,0.866025403784439,1.))
REPRESENTATION_ITEM('')
);
#4316=(
BOUNDED_CURVE()
B_SPLINE_CURVE(2,(#372431,#372432,#372433,#372434,#372435,#372436,#372437,
#372438,#372439,#372440,#372441,#372442,#372443),.UNSPECIFIED.,.F.,.F.)
B_SPLINE_CURVE_WITH_KNOTS((3,2,2,2,2,2,3),(0.887096774193548,0.89247311827957,
0.897849462365591,0.903225806451613,0.908602150537634,0.913978494623656,
0.919354838709677),.UNSPECIFIED.)
CURVE()
GEOMETRIC_REPRESENTATION_ITEM()
RATIONAL_B_SPLINE_CURVE((1.,0.866025403784439,1.,0.866025403784439,1.,0.866025403784439,
1.,0.866025403784439,1.,0.866025403784439,1.,0.866025403784439,1.))
REPRESENTATION_ITEM('')
);
#4317=(
BOUNDED_CURVE()
B_SPLINE_CURVE(2,(#372444,#372445,#372446,#372447,#372448,#372449,#372450,
#372451,#372452,#372453,#372454,#372455,#372456),.UNSPECIFIED.,.F.,.F.)
B_SPLINE_CURVE_WITH_KNOTS((3,2,2,2,2,2,3),(0.887096774193548,0.89247311827957,
0.897849462365591,0.903225806451613,0.908602150537634,0.913978494623656,
0.919354838709677),.UNSPECIFIED.)
CURVE()
GEOMETRIC_REPRESENTATION_ITEM()
RATIONAL_B_SPLINE_CURVE((1.,0.866025403784439,1.,0.866025403784439,1.,0.866025403784439,
1.,0.866025403784439,1.,0.866025403784439,1.,0.866025403784439,1.))
REPRESENTATION_ITEM('')
);
#4318=(
BOUNDED_CURVE()
B_SPLINE_CURVE(2,(#374793,#374794,#374795),.UNSPECIFIED.,.F.,.F.)
B_SPLINE_CURVE_WITH_KNOTS((3,3),(0.127655147271297,0.35532436269275),
 .UNSPECIFIED.)
CURVE()
GEOMETRIC_REPRESENTATION_ITEM()
RATIONAL_B_SPLINE_CURVE((1.3712812921102,1.58341924626904,1.3712812921102))
REPRESENTATION_ITEM('')
);
#4319=(
BOUNDED_CURVE()
B_SPLINE_CURVE(2,(#378380,#378381,#378382),.UNSPECIFIED.,.F.,.F.)
B_SPLINE_CURVE_WITH_KNOTS((3,3),(-0.355324362692751,-0.127655147271297),
 .UNSPECIFIED.)
CURVE()
GEOMETRIC_REPRESENTATION_ITEM()
RATIONAL_B_SPLINE_CURVE((1.3712812921102,1.58341924626904,1.3712812921102))
REPRESENTATION_ITEM('')
);
#4320=(
BOUNDED_CURVE()
B_SPLINE_CURVE(2,(#378388,#378389,#378390),.UNSPECIFIED.,.F.,.F.)
B_SPLINE_CURVE_WITH_KNOTS((3,3),(-0.355324362692751,-0.127655147271297),
 .UNSPECIFIED.)
CURVE()
GEOMETRIC_REPRESENTATION_ITEM()
RATIONAL_B_SPLINE_CURVE((1.3712812921102,1.58341924626905,1.37128129211021))
REPRESENTATION_ITEM('')
);
#4321=(
BOUNDED_CURVE()
B_SPLINE_CURVE(2,(#378394,#378395,#378396),.UNSPECIFIED.,.F.,.F.)
B_SPLINE_CURVE_WITH_KNOTS((3,3),(-0.35532436269275,-0.127655147271297),
 .UNSPECIFIED.)
CURVE()
GEOMETRIC_REPRESENTATION_ITEM()
RATIONAL_B_SPLINE_CURVE((1.37128129211021,1.58341924626905,1.37128129211021))
REPRESENTATION_ITEM('')
);
#4322=(
BOUNDED_CURVE()
B_SPLINE_CURVE(2,(#378400,#378401,#378402),.UNSPECIFIED.,.F.,.F.)
B_SPLINE_CURVE_WITH_KNOTS((3,3),(-0.355324362692751,-0.127655147271297),
 .UNSPECIFIED.)
CURVE()
GEOMETRIC_REPRESENTATION_ITEM()
RATIONAL_B_SPLINE_CURVE((1.37128129211021,1.58341924626905,1.37128129211021))
REPRESENTATION_ITEM('')
);
#4323=(
BOUNDED_CURVE()
B_SPLINE_CURVE(2,(#378405,#378406,#378407),.UNSPECIFIED.,.F.,.F.)
B_SPLINE_CURVE_WITH_KNOTS((3,3),(-0.35532436269275,-0.127655147271297),
 .UNSPECIFIED.)
CURVE()
GEOMETRIC_REPRESENTATION_ITEM()
RATIONAL_B_SPLINE_CURVE((1.37128129211021,1.58341924626905,1.37128129211021))
REPRESENTATION_ITEM('')
);
#4324=(
BOUNDED_CURVE()
B_SPLINE_CURVE(2,(#378417,#378418,#378419,#378420,#378421,#378422,#378423),
 .UNSPECIFIED.,.F.,.F.)
B_SPLINE_CURVE_WITH_KNOTS((3,2,2,3),(0.919354838709677,0.924731182795699,
0.93010752688172,0.930718281243958),.UNSPECIFIED.)
CURVE()
GEOMETRIC_REPRESENTATION_ITEM()
RATIONAL_B_SPLINE_CURVE((1.,0.866025403784439,1.,0.866025403784439,1.,0.984780444153422,
0.973018780873198))
REPRESENTATION_ITEM('')
);
#4325=(
BOUNDED_CURVE()
B_SPLINE_CURVE(2,(#378424,#378425,#378426,#378427,#378428),
 .UNSPECIFIED.,.F.,.F.)
B_SPLINE_CURVE_WITH_KNOTS((3,2,3),(0.919354838709677,0.924731182795699,
0.926677363777307),.UNSPECIFIED.)
CURVE()
GEOMETRIC_REPRESENTATION_ITEM()
RATIONAL_B_SPLINE_CURVE((1.,0.866025403784439,1.,0.951502581121761,0.938116290834902))
REPRESENTATION_ITEM('')
);
#4326=(
BOUNDED_CURVE()
B_SPLINE_CURVE(2,(#409628,#409629,#409630),.UNSPECIFIED.,.F.,.F.)
B_SPLINE_CURVE_WITH_KNOTS((3,3),(0.00739537155986661,0.00980392156862745),
 .UNSPECIFIED.)
CURVE()
GEOMETRIC_REPRESENTATION_ITEM()
RATIONAL_B_SPLINE_CURVE((0.948065210722634,0.901258538444052,1.))
REPRESENTATION_ITEM('')
);
#4327=(
BOUNDED_CURVE()
B_SPLINE_CURVE(2,(#409636,#409637,#409638,#409639,#409640,#409641,#409642,
#409643,#409644,#409645,#409646,#409647,#409648),.UNSPECIFIED.,.F.,.F.)
B_SPLINE_CURVE_WITH_KNOTS((3,2,2,2,2,2,3),(0.00980392156862745,0.0130718954248366,
0.0163398692810458,0.0196078431372549,0.0228758169934641,0.0261437908496732,
0.0294117647058824),.UNSPECIFIED.)
CURVE()
GEOMETRIC_REPRESENTATION_ITEM()
RATIONAL_B_SPLINE_CURVE((1.,0.866025403784439,1.,0.866025403784439,1.,0.866025403784439,
1.,0.866025403784439,1.,0.866025403784439,1.,0.866025403784439,1.))
REPRESENTATION_ITEM('')
);
#4328=(
BOUNDED_CURVE()
B_SPLINE_CURVE(2,(#409649,#409650,#409651,#409652,#409653,#409654,#409655,
#409656,#409657,#409658,#409659,#409660,#409661),.UNSPECIFIED.,.F.,.F.)
B_SPLINE_CURVE_WITH_KNOTS((3,2,2,2,2,2,3),(0.00980392156862746,0.0130718954248366,
0.0163398692810458,0.0196078431372549,0.0228758169934641,0.0261437908496732,
0.0294117647058824),.UNSPECIFIED.)
CURVE()
GEOMETRIC_REPRESENTATION_ITEM()
RATIONAL_B_SPLINE_CURVE((1.,0.866025403784439,1.,0.866025403784439,1.,0.866025403784439,
1.,0.866025403784439,1.,0.866025403784439,1.,0.866025403784439,1.))
REPRESENTATION_ITEM('')
);
#4329=(
BOUNDED_CURVE()
B_SPLINE_CURVE(2,(#409666,#409667,#409668,#409669,#409670,#409671,#409672,
#409673,#409674,#409675,#409676,#409677,#409678),.UNSPECIFIED.,.F.,.F.)
B_SPLINE_CURVE_WITH_KNOTS((3,2,2,2,2,2,3),(0.0294117647058824,0.0326797385620915,
0.0359477124183007,0.0392156862745098,0.042483660130719,0.0457516339869281,
0.0490196078431373),.UNSPECIFIED.)
CURVE()
GEOMETRIC_REPRESENTATION_ITEM()
RATIONAL_B_SPLINE_CURVE((1.,0.866025403784439,1.,0.866025403784439,1.,0.866025403784439,
1.,0.866025403784439,1.,0.866025403784439,1.,0.866025403784439,1.))
REPRESENTATION_ITEM('')
);
#4330=(
BOUNDED_CURVE()
B_SPLINE_CURVE(2,(#409679,#409680,#409681,#409682,#409683,#409684,#409685,
#409686,#409687,#409688,#409689,#409690,#409691),.UNSPECIFIED.,.F.,.F.)
B_SPLINE_CURVE_WITH_KNOTS((3,2,2,2,2,2,3),(0.0294117647058824,0.0326797385620915,
0.0359477124183007,0.0392156862745098,0.042483660130719,0.0457516339869281,
0.0490196078431373),.UNSPECIFIED.)
CURVE()
GEOMETRIC_REPRESENTATION_ITEM()
RATIONAL_B_SPLINE_CURVE((1.,0.866025403784439,1.,0.866025403784439,1.,0.866025403784439,
1.,0.866025403784439,1.,0.866025403784439,1.,0.866025403784439,1.))
REPRESENTATION_ITEM('')
);
#4331=(
BOUNDED_CURVE()
B_SPLINE_CURVE(2,(#409696,#409697,#409698,#409699,#409700,#409701,#409702,
#409703,#409704,#409705,#409706,#409707,#409708),.UNSPECIFIED.,.F.,.F.)
B_SPLINE_CURVE_WITH_KNOTS((3,2,2,2,2,2,3),(0.0490196078431373,0.0522875816993464,
0.0555555555555556,0.0588235294117647,0.0620915032679739,0.065359477124183,
0.0686274509803922),.UNSPECIFIED.)
CURVE()
GEOMETRIC_REPRESENTATION_ITEM()
RATIONAL_B_SPLINE_CURVE((1.,0.866025403784439,1.,0.866025403784439,1.,0.866025403784439,
1.,0.866025403784439,1.,0.866025403784439,1.,0.866025403784439,1.))
REPRESENTATION_ITEM('')
);
#4332=(
BOUNDED_CURVE()
B_SPLINE_CURVE(2,(#409709,#409710,#409711,#409712,#409713,#409714,#409715,
#409716,#409717,#409718,#409719,#409720,#409721),.UNSPECIFIED.,.F.,.F.)
B_SPLINE_CURVE_WITH_KNOTS((3,2,2,2,2,2,3),(0.0490196078431373,0.0522875816993464,
0.0555555555555556,0.0588235294117647,0.0620915032679739,0.065359477124183,
0.0686274509803922),.UNSPECIFIED.)
CURVE()
GEOMETRIC_REPRESENTATION_ITEM()
RATIONAL_B_SPLINE_CURVE((1.,0.866025403784439,1.,0.866025403784439,1.,0.866025403784439,
1.,0.866025403784439,1.,0.866025403784439,1.,0.866025403784439,1.))
REPRESENTATION_ITEM('')
);
#4333=(
BOUNDED_CURVE()
B_SPLINE_CURVE(2,(#409726,#409727,#409728,#409729,#409730,#409731,#409732,
#409733,#409734,#409735,#409736,#409737,#409738),.UNSPECIFIED.,.F.,.F.)
B_SPLINE_CURVE_WITH_KNOTS((3,2,2,2,2,2,3),(0.0686274509803922,0.0718954248366013,
0.0751633986928105,0.0784313725490196,0.0816993464052288,0.0849673202614379,
0.0882352941176471),.UNSPECIFIED.)
CURVE()
GEOMETRIC_REPRESENTATION_ITEM()
RATIONAL_B_SPLINE_CURVE((1.,0.866025403784439,1.,0.866025403784439,1.,0.866025403784439,
1.,0.866025403784439,1.,0.866025403784439,1.,0.866025403784439,1.))
REPRESENTATION_ITEM('')
);
#4334=(
BOUNDED_CURVE()
B_SPLINE_CURVE(2,(#409739,#409740,#409741,#409742,#409743,#409744,#409745,
#409746,#409747,#409748,#409749,#409750,#409751),.UNSPECIFIED.,.F.,.F.)
B_SPLINE_CURVE_WITH_KNOTS((3,2,2,2,2,2,3),(0.0686274509803922,0.0718954248366013,
0.0751633986928105,0.0784313725490196,0.0816993464052288,0.0849673202614379,
0.0882352941176471),.UNSPECIFIED.)
CURVE()
GEOMETRIC_REPRESENTATION_ITEM()
RATIONAL_B_SPLINE_CURVE((1.,0.866025403784439,1.,0.866025403784439,1.,0.866025403784439,
1.,0.866025403784439,1.,0.866025403784439,1.,0.866025403784439,1.))
REPRESENTATION_ITEM('')
);
#4335=(
BOUNDED_CURVE()
B_SPLINE_CURVE(2,(#409756,#409757,#409758,#409759,#409760,#409761,#409762,
#409763,#409764,#409765,#409766,#409767,#409768),.UNSPECIFIED.,.F.,.F.)
B_SPLINE_CURVE_WITH_KNOTS((3,2,2,2,2,2,3),(0.0882352941176471,0.0915032679738562,
0.0947712418300654,0.0980392156862745,0.101307189542484,0.104575163398693,
0.107843137254902),.UNSPECIFIED.)
CURVE()
GEOMETRIC_REPRESENTATION_ITEM()
RATIONAL_B_SPLINE_CURVE((1.,0.866025403784439,1.,0.866025403784439,1.,0.866025403784439,
1.,0.866025403784439,1.,0.866025403784439,1.,0.866025403784439,1.))
REPRESENTATION_ITEM('')
);
#4336=(
BOUNDED_CURVE()
B_SPLINE_CURVE(2,(#409769,#409770,#409771,#409772,#409773,#409774,#409775,
#409776,#409777,#409778,#409779,#409780,#409781),.UNSPECIFIED.,.F.,.F.)
B_SPLINE_CURVE_WITH_KNOTS((3,2,2,2,2,2,3),(0.0882352941176471,0.0915032679738562,
0.0947712418300654,0.0980392156862745,0.101307189542484,0.104575163398693,
0.107843137254902),.UNSPECIFIED.)
CURVE()
GEOMETRIC_REPRESENTATION_ITEM()
RATIONAL_B_SPLINE_CURVE((1.,0.866025403784439,1.,0.866025403784439,1.,0.866025403784439,
1.,0.866025403784439,1.,0.866025403784439,1.,0.866025403784439,1.))
REPRESENTATION_ITEM('')
);
#4337=(
BOUNDED_CURVE()
B_SPLINE_CURVE(2,(#409786,#409787,#409788,#409789,#409790,#409791,#409792,
#409793,#409794,#409795,#409796,#409797,#409798),.UNSPECIFIED.,.F.,.F.)
B_SPLINE_CURVE_WITH_KNOTS((3,2,2,2,2,2,3),(0.107843137254902,0.111111111111111,
0.11437908496732,0.117647058823529,0.120915032679739,0.124183006535948,
0.127450980392157),.UNSPECIFIED.)
CURVE()
GEOMETRIC_REPRESENTATION_ITEM()
RATIONAL_B_SPLINE_CURVE((1.,0.866025403784439,1.,0.866025403784439,1.,0.866025403784439,
1.,0.866025403784439,1.,0.866025403784439,1.,0.866025403784439,1.))
REPRESENTATION_ITEM('')
);
#4338=(
BOUNDED_CURVE()
B_SPLINE_CURVE(2,(#409799,#409800,#409801,#409802,#409803,#409804,#409805,
#409806,#409807,#409808,#409809,#409810,#409811),.UNSPECIFIED.,.F.,.F.)
B_SPLINE_CURVE_WITH_KNOTS((3,2,2,2,2,2,3),(0.107843137254902,0.111111111111111,
0.11437908496732,0.117647058823529,0.120915032679739,0.124183006535948,
0.127450980392157),.UNSPECIFIED.)
CURVE()
GEOMETRIC_REPRESENTATION_ITEM()
RATIONAL_B_SPLINE_CURVE((1.,0.866025403784439,1.,0.866025403784439,1.,0.866025403784439,
1.,0.866025403784439,1.,0.866025403784439,1.,0.866025403784439,1.))
REPRESENTATION_ITEM('')
);
#4339=(
BOUNDED_CURVE()
B_SPLINE_CURVE(2,(#409816,#409817,#409818,#409819,#409820,#409821,#409822,
#409823,#409824,#409825,#409826,#409827,#409828),.UNSPECIFIED.,.F.,.F.)
B_SPLINE_CURVE_WITH_KNOTS((3,2,2,2,2,2,3),(0.127450980392157,0.130718954248366,
0.133986928104575,0.137254901960784,0.140522875816993,0.143790849673203,
0.147058823529412),.UNSPECIFIED.)
CURVE()
GEOMETRIC_REPRESENTATION_ITEM()
RATIONAL_B_SPLINE_CURVE((1.,0.866025403784439,1.,0.866025403784439,1.,0.866025403784439,
1.,0.866025403784439,1.,0.866025403784439,1.,0.866025403784439,1.))
REPRESENTATION_ITEM('')
);
#4340=(
BOUNDED_CURVE()
B_SPLINE_CURVE(2,(#409829,#409830,#409831,#409832,#409833,#409834,#409835,
#409836,#409837,#409838,#409839,#409840,#409841),.UNSPECIFIED.,.F.,.F.)
B_SPLINE_CURVE_WITH_KNOTS((3,2,2,2,2,2,3),(0.127450980392157,0.130718954248366,
0.133986928104575,0.137254901960784,0.140522875816993,0.143790849673203,
0.147058823529412),.UNSPECIFIED.)
CURVE()
GEOMETRIC_REPRESENTATION_ITEM()
RATIONAL_B_SPLINE_CURVE((1.,0.866025403784439,1.,0.866025403784439,1.,0.866025403784439,
1.,0.866025403784439,1.,0.866025403784439,1.,0.866025403784439,1.))
REPRESENTATION_ITEM('')
);
#4341=(
BOUNDED_CURVE()
B_SPLINE_CURVE(2,(#409846,#409847,#409848,#409849,#409850,#409851,#409852,
#409853,#409854,#409855,#409856,#409857,#409858),.UNSPECIFIED.,.F.,.F.)
B_SPLINE_CURVE_WITH_KNOTS((3,2,2,2,2,2,3),(0.147058823529412,0.150326797385621,
0.15359477124183,0.156862745098039,0.160130718954248,0.163398692810458,
0.166666666666667),.UNSPECIFIED.)
CURVE()
GEOMETRIC_REPRESENTATION_ITEM()
RATIONAL_B_SPLINE_CURVE((1.,0.866025403784439,1.,0.866025403784439,1.,0.866025403784439,
1.,0.866025403784439,1.,0.866025403784439,1.,0.866025403784439,1.))
REPRESENTATION_ITEM('')
);
#4342=(
BOUNDED_CURVE()
B_SPLINE_CURVE(2,(#409859,#409860,#409861,#409862,#409863,#409864,#409865,
#409866,#409867,#409868,#409869,#409870,#409871),.UNSPECIFIED.,.F.,.F.)
B_SPLINE_CURVE_WITH_KNOTS((3,2,2,2,2,2,3),(0.147058823529412,0.150326797385621,
0.15359477124183,0.156862745098039,0.160130718954248,0.163398692810458,
0.166666666666667),.UNSPECIFIED.)
CURVE()
GEOMETRIC_REPRESENTATION_ITEM()
RATIONAL_B_SPLINE_CURVE((1.,0.866025403784439,1.,0.866025403784439,1.,0.866025403784439,
1.,0.866025403784439,1.,0.866025403784439,1.,0.866025403784439,1.))
REPRESENTATION_ITEM('')
);
#4343=(
BOUNDED_CURVE()
B_SPLINE_CURVE(2,(#409876,#409877,#409878,#409879,#409880,#409881,#409882,
#409883,#409884,#409885,#409886,#409887,#409888),.UNSPECIFIED.,.F.,.F.)
B_SPLINE_CURVE_WITH_KNOTS((3,2,2,2,2,2,3),(0.166666666666667,0.169934640522876,
0.173202614379085,0.176470588235294,0.179738562091503,0.183006535947712,
0.186274509803922),.UNSPECIFIED.)
CURVE()
GEOMETRIC_REPRESENTATION_ITEM()
RATIONAL_B_SPLINE_CURVE((1.,0.866025403784439,1.,0.866025403784439,1.,0.866025403784439,
1.,0.866025403784439,1.,0.866025403784439,1.,0.866025403784439,1.))
REPRESENTATION_ITEM('')
);
#4344=(
BOUNDED_CURVE()
B_SPLINE_CURVE(2,(#409889,#409890,#409891,#409892,#409893,#409894,#409895,
#409896,#409897,#409898,#409899,#409900,#409901),.UNSPECIFIED.,.F.,.F.)
B_SPLINE_CURVE_WITH_KNOTS((3,2,2,2,2,2,3),(0.166666666666667,0.169934640522876,
0.173202614379085,0.176470588235294,0.179738562091503,0.183006535947712,
0.186274509803922),.UNSPECIFIED.)
CURVE()
GEOMETRIC_REPRESENTATION_ITEM()
RATIONAL_B_SPLINE_CURVE((1.,0.866025403784439,1.,0.866025403784439,1.,0.866025403784439,
1.,0.866025403784439,1.,0.866025403784439,1.,0.866025403784439,1.))
REPRESENTATION_ITEM('')
);
#4345=(
BOUNDED_CURVE()
B_SPLINE_CURVE(2,(#409906,#409907,#409908,#409909,#409910,#409911,#409912,
#409913,#409914,#409915,#409916,#409917,#409918),.UNSPECIFIED.,.F.,.F.)
B_SPLINE_CURVE_WITH_KNOTS((3,2,2,2,2,2,3),(0.186274509803922,0.189542483660131,
0.19281045751634,0.196078431372549,0.199346405228758,0.202614379084967,
0.205882352941176),.UNSPECIFIED.)
CURVE()
GEOMETRIC_REPRESENTATION_ITEM()
RATIONAL_B_SPLINE_CURVE((1.,0.866025403784439,1.,0.866025403784439,1.,0.866025403784439,
1.,0.866025403784439,1.,0.866025403784439,1.,0.866025403784439,1.))
REPRESENTATION_ITEM('')
);
#4346=(
BOUNDED_CURVE()
B_SPLINE_CURVE(2,(#409919,#409920,#409921,#409922,#409923,#409924,#409925,
#409926,#409927,#409928,#409929,#409930,#409931),.UNSPECIFIED.,.F.,.F.)
B_SPLINE_CURVE_WITH_KNOTS((3,2,2,2,2,2,3),(0.186274509803922,0.189542483660131,
0.19281045751634,0.196078431372549,0.199346405228758,0.202614379084967,
0.205882352941177),.UNSPECIFIED.)
CURVE()
GEOMETRIC_REPRESENTATION_ITEM()
RATIONAL_B_SPLINE_CURVE((1.,0.866025403784439,1.,0.866025403784439,1.,0.866025403784439,
1.,0.866025403784439,1.,0.866025403784439,1.,0.866025403784439,1.))
REPRESENTATION_ITEM('')
);
#4347=(
BOUNDED_CURVE()
B_SPLINE_CURVE(2,(#409936,#409937,#409938,#409939,#409940,#409941,#409942,
#409943,#409944,#409945,#409946,#409947,#409948),.UNSPECIFIED.,.F.,.F.)
B_SPLINE_CURVE_WITH_KNOTS((3,2,2,2,2,2,3),(0.205882352941176,0.209150326797386,
0.212418300653595,0.215686274509804,0.218954248366013,0.222222222222222,
0.225490196078431),.UNSPECIFIED.)
CURVE()
GEOMETRIC_REPRESENTATION_ITEM()
RATIONAL_B_SPLINE_CURVE((1.,0.866025403784439,1.,0.866025403784439,1.,0.866025403784439,
1.,0.866025403784439,1.,0.866025403784439,1.,0.866025403784439,1.))
REPRESENTATION_ITEM('')
);
#4348=(
BOUNDED_CURVE()
B_SPLINE_CURVE(2,(#409949,#409950,#409951,#409952,#409953,#409954,#409955,
#409956,#409957,#409958,#409959,#409960,#409961),.UNSPECIFIED.,.F.,.F.)
B_SPLINE_CURVE_WITH_KNOTS((3,2,2,2,2,2,3),(0.205882352941177,0.209150326797386,
0.212418300653595,0.215686274509804,0.218954248366013,0.222222222222222,
0.225490196078431),.UNSPECIFIED.)
CURVE()
GEOMETRIC_REPRESENTATION_ITEM()
RATIONAL_B_SPLINE_CURVE((1.,0.866025403784439,1.,0.866025403784439,1.,0.866025403784439,
1.,0.866025403784439,1.,0.866025403784439,1.,0.866025403784439,1.))
REPRESENTATION_ITEM('')
);
#4349=(
BOUNDED_CURVE()
B_SPLINE_CURVE(2,(#409966,#409967,#409968,#409969,#409970,#409971,#409972,
#409973,#409974,#409975,#409976,#409977,#409978),.UNSPECIFIED.,.F.,.F.)
B_SPLINE_CURVE_WITH_KNOTS((3,2,2,2,2,2,3),(0.225490196078431,0.22875816993464,
0.23202614379085,0.235294117647059,0.238562091503268,0.241830065359477,
0.245098039215686),.UNSPECIFIED.)
CURVE()
GEOMETRIC_REPRESENTATION_ITEM()
RATIONAL_B_SPLINE_CURVE((1.,0.866025403784439,1.,0.866025403784439,1.,0.866025403784439,
1.,0.866025403784439,1.,0.866025403784439,1.,0.866025403784439,1.))
REPRESENTATION_ITEM('')
);
#4350=(
BOUNDED_CURVE()
B_SPLINE_CURVE(2,(#409979,#409980,#409981,#409982,#409983,#409984,#409985,
#409986,#409987,#409988,#409989,#409990,#409991),.UNSPECIFIED.,.F.,.F.)
B_SPLINE_CURVE_WITH_KNOTS((3,2,2,2,2,2,3),(0.225490196078431,0.228758169934641,
0.23202614379085,0.235294117647059,0.238562091503268,0.241830065359477,
0.245098039215686),.UNSPECIFIED.)
CURVE()
GEOMETRIC_REPRESENTATION_ITEM()
RATIONAL_B_SPLINE_CURVE((1.,0.866025403784439,1.,0.866025403784439,1.,0.866025403784439,
1.,0.866025403784439,1.,0.866025403784439,1.,0.866025403784439,1.))
REPRESENTATION_ITEM('')
);
#4351=(
BOUNDED_CURVE()
B_SPLINE_CURVE(2,(#409996,#409997,#409998,#409999,#410000,#410001,#410002,
#410003,#410004,#410005,#410006,#410007,#410008),.UNSPECIFIED.,.F.,.F.)
B_SPLINE_CURVE_WITH_KNOTS((3,2,2,2,2,2,3),(0.245098039215686,0.248366013071895,
0.251633986928105,0.254901960784314,0.258169934640523,0.261437908496732,
0.264705882352941),.UNSPECIFIED.)
CURVE()
GEOMETRIC_REPRESENTATION_ITEM()
RATIONAL_B_SPLINE_CURVE((1.,0.866025403784439,1.,0.866025403784439,1.,0.866025403784439,
1.,0.866025403784439,1.,0.866025403784439,1.,0.866025403784439,1.))
REPRESENTATION_ITEM('')
);
#4352=(
BOUNDED_CURVE()
B_SPLINE_CURVE(2,(#410009,#410010,#410011,#410012,#410013,#410014,#410015,
#410016,#410017,#410018,#410019,#410020,#410021),.UNSPECIFIED.,.F.,.F.)
B_SPLINE_CURVE_WITH_KNOTS((3,2,2,2,2,2,3),(0.245098039215686,0.248366013071895,
0.251633986928105,0.254901960784314,0.258169934640523,0.261437908496732,
0.264705882352941),.UNSPECIFIED.)
CURVE()
GEOMETRIC_REPRESENTATION_ITEM()
RATIONAL_B_SPLINE_CURVE((1.,0.866025403784439,1.,0.866025403784439,1.,0.866025403784439,
1.,0.866025403784439,1.,0.866025403784439,1.,0.866025403784439,1.))
REPRESENTATION_ITEM('')
);
#4353=(
BOUNDED_CURVE()
B_SPLINE_CURVE(2,(#410026,#410027,#410028,#410029,#410030,#410031,#410032,
#410033,#410034,#410035,#410036,#410037,#410038),.UNSPECIFIED.,.F.,.F.)
B_SPLINE_CURVE_WITH_KNOTS((3,2,2,2,2,2,3),(0.264705882352941,0.26797385620915,
0.271241830065359,0.274509803921569,0.277777777777778,0.281045751633987,
0.284313725490196),.UNSPECIFIED.)
CURVE()
GEOMETRIC_REPRESENTATION_ITEM()
RATIONAL_B_SPLINE_CURVE((1.,0.866025403784439,1.,0.866025403784439,1.,0.866025403784439,
1.,0.866025403784439,1.,0.866025403784439,1.,0.866025403784439,1.))
REPRESENTATION_ITEM('')
);
#4354=(
BOUNDED_CURVE()
B_SPLINE_CURVE(2,(#410039,#410040,#410041,#410042,#410043,#410044,#410045,
#410046,#410047,#410048,#410049,#410050,#410051),.UNSPECIFIED.,.F.,.F.)
B_SPLINE_CURVE_WITH_KNOTS((3,2,2,2,2,2,3),(0.264705882352941,0.26797385620915,
0.271241830065359,0.274509803921569,0.277777777777778,0.281045751633987,
0.284313725490196),.UNSPECIFIED.)
CURVE()
GEOMETRIC_REPRESENTATION_ITEM()
RATIONAL_B_SPLINE_CURVE((1.,0.866025403784439,1.,0.866025403784439,1.,0.866025403784439,
1.,0.866025403784439,1.,0.866025403784439,1.,0.866025403784439,1.))
REPRESENTATION_ITEM('')
);
#4355=(
BOUNDED_CURVE()
B_SPLINE_CURVE(2,(#410056,#410057,#410058,#410059,#410060,#410061,#410062,
#410063,#410064,#410065,#410066,#410067,#410068),.UNSPECIFIED.,.F.,.F.)
B_SPLINE_CURVE_WITH_KNOTS((3,2,2,2,2,2,3),(0.284313725490196,0.287581699346405,
0.290849673202614,0.294117647058823,0.297385620915033,0.300653594771242,
0.303921568627451),.UNSPECIFIED.)
CURVE()
GEOMETRIC_REPRESENTATION_ITEM()
RATIONAL_B_SPLINE_CURVE((1.,0.866025403784439,1.,0.866025403784439,1.,0.866025403784439,
1.,0.866025403784439,1.,0.866025403784439,1.,0.866025403784439,1.))
REPRESENTATION_ITEM('')
);
#4356=(
BOUNDED_CURVE()
B_SPLINE_CURVE(2,(#410069,#410070,#410071,#410072,#410073,#410074,#410075,
#410076,#410077,#410078,#410079,#410080,#410081),.UNSPECIFIED.,.F.,.F.)
B_SPLINE_CURVE_WITH_KNOTS((3,2,2,2,2,2,3),(0.284313725490196,0.287581699346405,
0.290849673202614,0.294117647058824,0.297385620915033,0.300653594771242,
0.303921568627451),.UNSPECIFIED.)
CURVE()
GEOMETRIC_REPRESENTATION_ITEM()
RATIONAL_B_SPLINE_CURVE((1.,0.866025403784439,1.,0.866025403784439,1.,0.866025403784439,
1.,0.866025403784439,1.,0.866025403784439,1.,0.866025403784439,1.))
REPRESENTATION_ITEM('')
);
#4357=(
BOUNDED_CURVE()
B_SPLINE_CURVE(2,(#410086,#410087,#410088,#410089,#410090,#410091,#410092,
#410093,#410094,#410095,#410096,#410097,#410098),.UNSPECIFIED.,.F.,.F.)
B_SPLINE_CURVE_WITH_KNOTS((3,2,2,2,2,2,3),(0.303921568627451,0.30718954248366,
0.310457516339869,0.313725490196078,0.316993464052288,0.320261437908497,
0.323529411764706),.UNSPECIFIED.)
CURVE()
GEOMETRIC_REPRESENTATION_ITEM()
RATIONAL_B_SPLINE_CURVE((1.,0.866025403784439,1.,0.866025403784439,1.,0.866025403784439,
1.,0.866025403784439,1.,0.866025403784439,1.,0.866025403784439,1.))
REPRESENTATION_ITEM('')
);
#4358=(
BOUNDED_CURVE()
B_SPLINE_CURVE(2,(#410099,#410100,#410101,#410102,#410103,#410104,#410105,
#410106,#410107,#410108,#410109,#410110,#410111),.UNSPECIFIED.,.F.,.F.)
B_SPLINE_CURVE_WITH_KNOTS((3,2,2,2,2,2,3),(0.303921568627451,0.30718954248366,
0.310457516339869,0.313725490196078,0.316993464052288,0.320261437908497,
0.323529411764706),.UNSPECIFIED.)
CURVE()
GEOMETRIC_REPRESENTATION_ITEM()
RATIONAL_B_SPLINE_CURVE((1.,0.866025403784439,1.,0.866025403784439,1.,0.866025403784439,
1.,0.866025403784439,1.,0.866025403784439,1.,0.866025403784439,1.))
REPRESENTATION_ITEM('')
);
#4359=(
BOUNDED_CURVE()
B_SPLINE_CURVE(2,(#410116,#410117,#410118,#410119,#410120,#410121,#410122,
#410123,#410124,#410125,#410126,#410127,#410128),.UNSPECIFIED.,.F.,.F.)
B_SPLINE_CURVE_WITH_KNOTS((3,2,2,2,2,2,3),(0.323529411764706,0.326797385620915,
0.330065359477124,0.333333333333333,0.336601307189543,0.339869281045752,
0.343137254901961),.UNSPECIFIED.)
CURVE()
GEOMETRIC_REPRESENTATION_ITEM()
RATIONAL_B_SPLINE_CURVE((1.,0.866025403784439,1.,0.866025403784439,1.,0.866025403784439,
1.,0.866025403784439,1.,0.866025403784439,1.,0.866025403784439,1.))
REPRESENTATION_ITEM('')
);
#4360=(
BOUNDED_CURVE()
B_SPLINE_CURVE(2,(#410129,#410130,#410131,#410132,#410133,#410134,#410135,
#410136,#410137,#410138,#410139,#410140,#410141),.UNSPECIFIED.,.F.,.F.)
B_SPLINE_CURVE_WITH_KNOTS((3,2,2,2,2,2,3),(0.323529411764706,0.326797385620915,
0.330065359477124,0.333333333333333,0.336601307189543,0.339869281045752,
0.343137254901961),.UNSPECIFIED.)
CURVE()
GEOMETRIC_REPRESENTATION_ITEM()
RATIONAL_B_SPLINE_CURVE((1.,0.866025403784439,1.,0.866025403784439,1.,0.866025403784439,
1.,0.866025403784439,1.,0.866025403784439,1.,0.866025403784439,1.))
REPRESENTATION_ITEM('')
);
#4361=(
BOUNDED_CURVE()
B_SPLINE_CURVE(2,(#410146,#410147,#410148,#410149,#410150,#410151,#410152,
#410153,#410154,#410155,#410156,#410157,#410158),.UNSPECIFIED.,.F.,.F.)
B_SPLINE_CURVE_WITH_KNOTS((3,2,2,2,2,2,3),(0.343137254901961,0.34640522875817,
0.349673202614379,0.352941176470588,0.356209150326797,0.359477124183006,
0.362745098039216),.UNSPECIFIED.)
CURVE()
GEOMETRIC_REPRESENTATION_ITEM()
RATIONAL_B_SPLINE_CURVE((1.,0.866025403784439,1.,0.866025403784439,1.,0.866025403784439,
1.,0.866025403784439,1.,0.866025403784439,1.,0.866025403784439,1.))
REPRESENTATION_ITEM('')
);
#4362=(
BOUNDED_CURVE()
B_SPLINE_CURVE(2,(#410159,#410160,#410161,#410162,#410163,#410164,#410165,
#410166,#410167,#410168,#410169,#410170,#410171),.UNSPECIFIED.,.F.,.F.)
B_SPLINE_CURVE_WITH_KNOTS((3,2,2,2,2,2,3),(0.343137254901961,0.34640522875817,
0.349673202614379,0.352941176470588,0.356209150326797,0.359477124183007,
0.362745098039216),.UNSPECIFIED.)
CURVE()
GEOMETRIC_REPRESENTATION_ITEM()
RATIONAL_B_SPLINE_CURVE((1.,0.866025403784439,1.,0.866025403784439,1.,0.866025403784439,
1.,0.866025403784439,1.,0.866025403784439,1.,0.866025403784439,1.))
REPRESENTATION_ITEM('')
);
#4363=(
BOUNDED_CURVE()
B_SPLINE_CURVE(2,(#410176,#410177,#410178,#410179,#410180,#410181,#410182,
#410183,#410184,#410185,#410186,#410187,#410188),.UNSPECIFIED.,.F.,.F.)
B_SPLINE_CURVE_WITH_KNOTS((3,2,2,2,2,2,3),(0.362745098039216,0.366013071895425,
0.369281045751634,0.372549019607843,0.375816993464052,0.379084967320261,
0.382352941176471),.UNSPECIFIED.)
CURVE()
GEOMETRIC_REPRESENTATION_ITEM()
RATIONAL_B_SPLINE_CURVE((1.,0.866025403784439,1.,0.866025403784439,1.,0.866025403784439,
1.,0.866025403784439,1.,0.866025403784439,1.,0.866025403784439,1.))
REPRESENTATION_ITEM('')
);
#4364=(
BOUNDED_CURVE()
B_SPLINE_CURVE(2,(#410189,#410190,#410191,#410192,#410193,#410194,#410195,
#410196,#410197,#410198,#410199,#410200,#410201),.UNSPECIFIED.,.F.,.F.)
B_SPLINE_CURVE_WITH_KNOTS((3,2,2,2,2,2,3),(0.362745098039216,0.366013071895425,
0.369281045751634,0.372549019607843,0.375816993464052,0.379084967320261,
0.382352941176471),.UNSPECIFIED.)
CURVE()
GEOMETRIC_REPRESENTATION_ITEM()
RATIONAL_B_SPLINE_CURVE((1.,0.866025403784439,1.,0.866025403784439,1.,0.866025403784439,
1.,0.866025403784439,1.,0.866025403784439,1.,0.866025403784439,1.))
REPRESENTATION_ITEM('')
);
#4365=(
BOUNDED_CURVE()
B_SPLINE_CURVE(2,(#410206,#410207,#410208,#410209,#410210,#410211,#410212,
#410213,#410214,#410215,#410216,#410217,#410218),.UNSPECIFIED.,.F.,.F.)
B_SPLINE_CURVE_WITH_KNOTS((3,2,2,2,2,2,3),(0.382352941176471,0.38562091503268,
0.388888888888889,0.392156862745098,0.395424836601307,0.398692810457516,
0.401960784313726),.UNSPECIFIED.)
CURVE()
GEOMETRIC_REPRESENTATION_ITEM()
RATIONAL_B_SPLINE_CURVE((1.,0.866025403784439,1.,0.866025403784439,1.,0.866025403784439,
1.,0.866025403784439,1.,0.866025403784439,1.,0.866025403784439,1.))
REPRESENTATION_ITEM('')
);
#4366=(
BOUNDED_CURVE()
B_SPLINE_CURVE(2,(#410219,#410220,#410221,#410222,#410223,#410224,#410225,
#410226,#410227,#410228,#410229,#410230,#410231),.UNSPECIFIED.,.F.,.F.)
B_SPLINE_CURVE_WITH_KNOTS((3,2,2,2,2,2,3),(0.382352941176471,0.38562091503268,
0.388888888888889,0.392156862745098,0.395424836601307,0.398692810457516,
0.401960784313726),.UNSPECIFIED.)
CURVE()
GEOMETRIC_REPRESENTATION_ITEM()
RATIONAL_B_SPLINE_CURVE((1.,0.866025403784439,1.,0.866025403784439,1.,0.866025403784439,
1.,0.866025403784439,1.,0.866025403784439,1.,0.866025403784439,1.))
REPRESENTATION_ITEM('')
);
#4367=(
BOUNDED_CURVE()
B_SPLINE_CURVE(2,(#410236,#410237,#410238,#410239,#410240,#410241,#410242,
#410243,#410244,#410245,#410246,#410247,#410248),.UNSPECIFIED.,.F.,.F.)
B_SPLINE_CURVE_WITH_KNOTS((3,2,2,2,2,2,3),(0.401960784313726,0.405228758169935,
0.408496732026144,0.411764705882353,0.415032679738562,0.418300653594771,
0.42156862745098),.UNSPECIFIED.)
CURVE()
GEOMETRIC_REPRESENTATION_ITEM()
RATIONAL_B_SPLINE_CURVE((1.,0.866025403784439,1.,0.866025403784439,1.,0.866025403784439,
1.,0.866025403784439,1.,0.866025403784439,1.,0.866025403784439,1.))
REPRESENTATION_ITEM('')
);
#4368=(
BOUNDED_CURVE()
B_SPLINE_CURVE(2,(#410249,#410250,#410251,#410252,#410253,#410254,#410255,
#410256,#410257,#410258,#410259,#410260,#410261),.UNSPECIFIED.,.F.,.F.)
B_SPLINE_CURVE_WITH_KNOTS((3,2,2,2,2,2,3),(0.401960784313726,0.405228758169935,
0.408496732026144,0.411764705882353,0.415032679738562,0.418300653594771,
0.42156862745098),.UNSPECIFIED.)
CURVE()
GEOMETRIC_REPRESENTATION_ITEM()
RATIONAL_B_SPLINE_CURVE((1.,0.866025403784439,1.,0.866025403784439,1.,0.866025403784439,
1.,0.866025403784439,1.,0.866025403784439,1.,0.866025403784439,1.))
REPRESENTATION_ITEM('')
);
#4369=(
BOUNDED_CURVE()
B_SPLINE_CURVE(2,(#410266,#410267,#410268,#410269,#410270,#410271,#410272,
#410273,#410274,#410275,#410276,#410277,#410278),.UNSPECIFIED.,.F.,.F.)
B_SPLINE_CURVE_WITH_KNOTS((3,2,2,2,2,2,3),(0.42156862745098,0.424836601307189,
0.428104575163399,0.431372549019608,0.434640522875817,0.437908496732026,
0.441176470588235),.UNSPECIFIED.)
CURVE()
GEOMETRIC_REPRESENTATION_ITEM()
RATIONAL_B_SPLINE_CURVE((1.,0.866025403784439,1.,0.866025403784439,1.,0.866025403784439,
1.,0.866025403784439,1.,0.866025403784439,1.,0.866025403784439,1.))
REPRESENTATION_ITEM('')
);
#4370=(
BOUNDED_CURVE()
B_SPLINE_CURVE(2,(#410279,#410280,#410281,#410282,#410283,#410284,#410285,
#410286,#410287,#410288,#410289,#410290,#410291),.UNSPECIFIED.,.F.,.F.)
B_SPLINE_CURVE_WITH_KNOTS((3,2,2,2,2,2,3),(0.42156862745098,0.42483660130719,
0.428104575163399,0.431372549019608,0.434640522875817,0.437908496732026,
0.441176470588235),.UNSPECIFIED.)
CURVE()
GEOMETRIC_REPRESENTATION_ITEM()
RATIONAL_B_SPLINE_CURVE((1.,0.866025403784439,1.,0.866025403784439,1.,0.866025403784439,
1.,0.866025403784439,1.,0.866025403784439,1.,0.866025403784439,1.))
REPRESENTATION_ITEM('')
);
#4371=(
BOUNDED_CURVE()
B_SPLINE_CURVE(2,(#410296,#410297,#410298,#410299,#410300,#410301,#410302,
#410303,#410304,#410305,#410306,#410307,#410308),.UNSPECIFIED.,.F.,.F.)
B_SPLINE_CURVE_WITH_KNOTS((3,2,2,2,2,2,3),(0.441176470588235,0.444444444444444,
0.447712418300654,0.450980392156863,0.454248366013072,0.457516339869281,
0.46078431372549),.UNSPECIFIED.)
CURVE()
GEOMETRIC_REPRESENTATION_ITEM()
RATIONAL_B_SPLINE_CURVE((1.,0.866025403784439,1.,0.866025403784439,1.,0.866025403784439,
1.,0.866025403784439,1.,0.866025403784439,1.,0.866025403784439,1.))
REPRESENTATION_ITEM('')
);
#4372=(
BOUNDED_CURVE()
B_SPLINE_CURVE(2,(#410309,#410310,#410311,#410312,#410313,#410314,#410315,
#410316,#410317,#410318,#410319,#410320,#410321),.UNSPECIFIED.,.F.,.F.)
B_SPLINE_CURVE_WITH_KNOTS((3,2,2,2,2,2,3),(0.441176470588235,0.444444444444444,
0.447712418300654,0.450980392156863,0.454248366013072,0.457516339869281,
0.46078431372549),.UNSPECIFIED.)
CURVE()
GEOMETRIC_REPRESENTATION_ITEM()
RATIONAL_B_SPLINE_CURVE((1.,0.866025403784439,1.,0.866025403784439,1.,0.866025403784439,
1.,0.866025403784439,1.,0.866025403784439,1.,0.866025403784439,1.))
REPRESENTATION_ITEM('')
);
#4373=(
BOUNDED_CURVE()
B_SPLINE_CURVE(2,(#410326,#410327,#410328,#410329,#410330,#410331,#410332,
#410333,#410334,#410335,#410336,#410337,#410338),.UNSPECIFIED.,.F.,.F.)
B_SPLINE_CURVE_WITH_KNOTS((3,2,2,2,2,2,3),(0.46078431372549,0.464052287581699,
0.467320261437909,0.470588235294118,0.473856209150327,0.477124183006536,
0.480392156862745),.UNSPECIFIED.)
CURVE()
GEOMETRIC_REPRESENTATION_ITEM()
RATIONAL_B_SPLINE_CURVE((1.,0.866025403784439,1.,0.866025403784439,1.,0.866025403784439,
1.,0.866025403784439,1.,0.866025403784439,1.,0.866025403784439,1.))
REPRESENTATION_ITEM('')
);
#4374=(
BOUNDED_CURVE()
B_SPLINE_CURVE(2,(#410339,#410340,#410341,#410342,#410343,#410344,#410345,
#410346,#410347,#410348,#410349,#410350,#410351),.UNSPECIFIED.,.F.,.F.)
B_SPLINE_CURVE_WITH_KNOTS((3,2,2,2,2,2,3),(0.46078431372549,0.464052287581699,
0.467320261437908,0.470588235294118,0.473856209150327,0.477124183006536,
0.480392156862745),.UNSPECIFIED.)
CURVE()
GEOMETRIC_REPRESENTATION_ITEM()
RATIONAL_B_SPLINE_CURVE((1.,0.866025403784439,1.,0.866025403784439,1.,0.866025403784439,
1.,0.866025403784439,1.,0.866025403784439,1.,0.866025403784439,1.))
REPRESENTATION_ITEM('')
);
#4375=(
BOUNDED_CURVE()
B_SPLINE_CURVE(2,(#410356,#410357,#410358,#410359,#410360,#410361,#410362,
#410363,#410364,#410365,#410366,#410367,#410368),.UNSPECIFIED.,.F.,.F.)
B_SPLINE_CURVE_WITH_KNOTS((3,2,2,2,2,2,3),(0.480392156862745,0.483660130718954,
0.486928104575163,0.490196078431372,0.493464052287582,0.496732026143791,
0.5),.UNSPECIFIED.)
CURVE()
GEOMETRIC_REPRESENTATION_ITEM()
RATIONAL_B_SPLINE_CURVE((1.,0.866025403784439,1.,0.866025403784439,1.,0.866025403784439,
1.,0.866025403784439,1.,0.866025403784439,1.,0.866025403784439,1.))
REPRESENTATION_ITEM('')
);
#4376=(
BOUNDED_CURVE()
B_SPLINE_CURVE(2,(#410369,#410370,#410371,#410372,#410373,#410374,#410375,
#410376,#410377,#410378,#410379,#410380,#410381),.UNSPECIFIED.,.F.,.F.)
B_SPLINE_CURVE_WITH_KNOTS((3,2,2,2,2,2,3),(0.480392156862745,0.483660130718954,
0.486928104575163,0.490196078431373,0.493464052287582,0.496732026143791,
0.5),.UNSPECIFIED.)
CURVE()
GEOMETRIC_REPRESENTATION_ITEM()
RATIONAL_B_SPLINE_CURVE((1.,0.866025403784439,1.,0.866025403784439,1.,0.866025403784439,
1.,0.866025403784439,1.,0.866025403784439,1.,0.866025403784439,1.))
REPRESENTATION_ITEM('')
);
#4377=(
BOUNDED_CURVE()
B_SPLINE_CURVE(2,(#410386,#410387,#410388,#410389,#410390,#410391,#410392,
#410393,#410394,#410395,#410396,#410397,#410398),.UNSPECIFIED.,.F.,.F.)
B_SPLINE_CURVE_WITH_KNOTS((3,2,2,2,2,2,3),(0.5,0.503267973856209,0.506535947712418,
0.509803921568627,0.513071895424837,0.516339869281046,0.519607843137255),
 .UNSPECIFIED.)
CURVE()
GEOMETRIC_REPRESENTATION_ITEM()
RATIONAL_B_SPLINE_CURVE((1.,0.866025403784439,1.,0.866025403784439,1.,0.866025403784439,
1.,0.866025403784439,1.,0.866025403784439,1.,0.866025403784439,1.))
REPRESENTATION_ITEM('')
);
#4378=(
BOUNDED_CURVE()
B_SPLINE_CURVE(2,(#410399,#410400,#410401,#410402,#410403,#410404,#410405,
#410406,#410407,#410408,#410409,#410410,#410411),.UNSPECIFIED.,.F.,.F.)
B_SPLINE_CURVE_WITH_KNOTS((3,2,2,2,2,2,3),(0.5,0.503267973856209,0.506535947712418,
0.509803921568627,0.513071895424837,0.516339869281046,0.519607843137255),
 .UNSPECIFIED.)
CURVE()
GEOMETRIC_REPRESENTATION_ITEM()
RATIONAL_B_SPLINE_CURVE((1.,0.866025403784439,1.,0.866025403784439,1.,0.866025403784439,
1.,0.866025403784439,1.,0.866025403784439,1.,0.866025403784439,1.))
REPRESENTATION_ITEM('')
);
#4379=(
BOUNDED_CURVE()
B_SPLINE_CURVE(2,(#410416,#410417,#410418,#410419,#410420,#410421,#410422,
#410423,#410424,#410425,#410426,#410427,#410428),.UNSPECIFIED.,.F.,.F.)
B_SPLINE_CURVE_WITH_KNOTS((3,2,2,2,2,2,3),(0.519607843137255,0.522875816993464,
0.526143790849673,0.529411764705882,0.532679738562091,0.535947712418301,
0.53921568627451),.UNSPECIFIED.)
CURVE()
GEOMETRIC_REPRESENTATION_ITEM()
RATIONAL_B_SPLINE_CURVE((1.,0.866025403784439,1.,0.866025403784439,1.,0.866025403784439,
1.,0.866025403784439,1.,0.866025403784439,1.,0.866025403784439,1.))
REPRESENTATION_ITEM('')
);
#4380=(
BOUNDED_CURVE()
B_SPLINE_CURVE(2,(#410429,#410430,#410431,#410432,#410433,#410434,#410435,
#410436,#410437,#410438,#410439,#410440,#410441),.UNSPECIFIED.,.F.,.F.)
B_SPLINE_CURVE_WITH_KNOTS((3,2,2,2,2,2,3),(0.519607843137255,0.522875816993464,
0.526143790849673,0.529411764705882,0.532679738562091,0.535947712418301,
0.53921568627451),.UNSPECIFIED.)
CURVE()
GEOMETRIC_REPRESENTATION_ITEM()
RATIONAL_B_SPLINE_CURVE((1.,0.866025403784439,1.,0.866025403784439,1.,0.866025403784439,
1.,0.866025403784439,1.,0.866025403784439,1.,0.866025403784439,1.))
REPRESENTATION_ITEM('')
);
#4381=(
BOUNDED_CURVE()
B_SPLINE_CURVE(2,(#410446,#410447,#410448,#410449,#410450,#410451,#410452,
#410453,#410454,#410455,#410456,#410457,#410458),.UNSPECIFIED.,.F.,.F.)
B_SPLINE_CURVE_WITH_KNOTS((3,2,2,2,2,2,3),(0.53921568627451,0.542483660130719,
0.545751633986928,0.549019607843137,0.552287581699346,0.555555555555556,
0.558823529411765),.UNSPECIFIED.)
CURVE()
GEOMETRIC_REPRESENTATION_ITEM()
RATIONAL_B_SPLINE_CURVE((1.,0.866025403784439,1.,0.866025403784439,1.,0.866025403784439,
1.,0.866025403784439,1.,0.866025403784439,1.,0.866025403784439,1.))
REPRESENTATION_ITEM('')
);
#4382=(
BOUNDED_CURVE()
B_SPLINE_CURVE(2,(#410459,#410460,#410461,#410462,#410463,#410464,#410465,
#410466,#410467,#410468,#410469,#410470,#410471),.UNSPECIFIED.,.F.,.F.)
B_SPLINE_CURVE_WITH_KNOTS((3,2,2,2,2,2,3),(0.53921568627451,0.542483660130719,
0.545751633986928,0.549019607843137,0.552287581699346,0.555555555555556,
0.558823529411765),.UNSPECIFIED.)
CURVE()
GEOMETRIC_REPRESENTATION_ITEM()
RATIONAL_B_SPLINE_CURVE((1.,0.866025403784439,1.,0.866025403784439,1.,0.866025403784439,
1.,0.866025403784439,1.,0.866025403784439,1.,0.866025403784439,1.))
REPRESENTATION_ITEM('')
);
#4383=(
BOUNDED_CURVE()
B_SPLINE_CURVE(2,(#410476,#410477,#410478,#410479,#410480,#410481,#410482,
#410483,#410484,#410485,#410486,#410487,#410488),.UNSPECIFIED.,.F.,.F.)
B_SPLINE_CURVE_WITH_KNOTS((3,2,2,2,2,2,3),(0.558823529411765,0.562091503267974,
0.565359477124183,0.568627450980392,0.571895424836601,0.57516339869281,
0.57843137254902),.UNSPECIFIED.)
CURVE()
GEOMETRIC_REPRESENTATION_ITEM()
RATIONAL_B_SPLINE_CURVE((1.,0.866025403784439,1.,0.866025403784439,1.,0.866025403784439,
1.,0.866025403784439,1.,0.866025403784439,1.,0.866025403784439,1.))
REPRESENTATION_ITEM('')
);
#4384=(
BOUNDED_CURVE()
B_SPLINE_CURVE(2,(#410489,#410490,#410491,#410492,#410493,#410494,#410495,
#410496,#410497,#410498,#410499,#410500,#410501),.UNSPECIFIED.,.F.,.F.)
B_SPLINE_CURVE_WITH_KNOTS((3,2,2,2,2,2,3),(0.558823529411765,0.562091503267974,
0.565359477124183,0.568627450980392,0.571895424836601,0.57516339869281,
0.57843137254902),.UNSPECIFIED.)
CURVE()
GEOMETRIC_REPRESENTATION_ITEM()
RATIONAL_B_SPLINE_CURVE((1.,0.866025403784439,1.,0.866025403784439,1.,0.866025403784439,
1.,0.866025403784439,1.,0.866025403784439,1.,0.866025403784439,1.))
REPRESENTATION_ITEM('')
);
#4385=(
BOUNDED_CURVE()
B_SPLINE_CURVE(2,(#410506,#410507,#410508,#410509,#410510,#410511,#410512,
#410513,#410514,#410515,#410516,#410517,#410518),.UNSPECIFIED.,.F.,.F.)
B_SPLINE_CURVE_WITH_KNOTS((3,2,2,2,2,2,3),(0.57843137254902,0.581699346405229,
0.584967320261438,0.588235294117647,0.591503267973856,0.594771241830065,
0.598039215686274),.UNSPECIFIED.)
CURVE()
GEOMETRIC_REPRESENTATION_ITEM()
RATIONAL_B_SPLINE_CURVE((1.,0.866025403784439,1.,0.866025403784439,1.,0.866025403784439,
1.,0.866025403784439,1.,0.866025403784439,1.,0.866025403784439,1.))
REPRESENTATION_ITEM('')
);
#4386=(
BOUNDED_CURVE()
B_SPLINE_CURVE(2,(#410519,#410520,#410521,#410522,#410523,#410524,#410525,
#410526,#410527,#410528,#410529,#410530,#410531),.UNSPECIFIED.,.F.,.F.)
B_SPLINE_CURVE_WITH_KNOTS((3,2,2,2,2,2,3),(0.57843137254902,0.581699346405229,
0.584967320261438,0.588235294117647,0.591503267973856,0.594771241830065,
0.598039215686274),.UNSPECIFIED.)
CURVE()
GEOMETRIC_REPRESENTATION_ITEM()
RATIONAL_B_SPLINE_CURVE((1.,0.866025403784439,1.,0.866025403784439,1.,0.866025403784439,
1.,0.866025403784439,1.,0.866025403784439,1.,0.866025403784439,1.))
REPRESENTATION_ITEM('')
);
#4387=(
BOUNDED_CURVE()
B_SPLINE_CURVE(2,(#410536,#410537,#410538,#410539,#410540,#410541,#410542,
#410543,#410544,#410545,#410546,#410547,#410548),.UNSPECIFIED.,.F.,.F.)
B_SPLINE_CURVE_WITH_KNOTS((3,2,2,2,2,2,3),(0.598039215686274,0.601307189542484,
0.604575163398693,0.607843137254902,0.611111111111111,0.61437908496732,
0.617647058823529),.UNSPECIFIED.)
CURVE()
GEOMETRIC_REPRESENTATION_ITEM()
RATIONAL_B_SPLINE_CURVE((1.,0.866025403784439,1.,0.866025403784439,1.,0.866025403784439,
1.,0.866025403784439,1.,0.866025403784439,1.,0.866025403784439,1.))
REPRESENTATION_ITEM('')
);
#4388=(
BOUNDED_CURVE()
B_SPLINE_CURVE(2,(#410549,#410550,#410551,#410552,#410553,#410554,#410555,
#410556,#410557,#410558,#410559,#410560,#410561),.UNSPECIFIED.,.F.,.F.)
B_SPLINE_CURVE_WITH_KNOTS((3,2,2,2,2,2,3),(0.598039215686274,0.601307189542484,
0.604575163398693,0.607843137254902,0.611111111111111,0.61437908496732,
0.617647058823529),.UNSPECIFIED.)
CURVE()
GEOMETRIC_REPRESENTATION_ITEM()
RATIONAL_B_SPLINE_CURVE((1.,0.866025403784439,1.,0.866025403784439,1.,0.866025403784439,
1.,0.866025403784439,1.,0.866025403784439,1.,0.866025403784439,1.))
REPRESENTATION_ITEM('')
);
#4389=(
BOUNDED_CURVE()
B_SPLINE_CURVE(2,(#410566,#410567,#410568,#410569,#410570,#410571,#410572,
#410573,#410574,#410575,#410576,#410577,#410578),.UNSPECIFIED.,.F.,.F.)
B_SPLINE_CURVE_WITH_KNOTS((3,2,2,2,2,2,3),(0.617647058823529,0.620915032679739,
0.624183006535948,0.627450980392157,0.630718954248366,0.633986928104575,
0.637254901960784),.UNSPECIFIED.)
CURVE()
GEOMETRIC_REPRESENTATION_ITEM()
RATIONAL_B_SPLINE_CURVE((1.,0.866025403784439,1.,0.866025403784439,1.,0.866025403784439,
1.,0.866025403784439,1.,0.866025403784439,1.,0.866025403784439,1.))
REPRESENTATION_ITEM('')
);
#4390=(
BOUNDED_CURVE()
B_SPLINE_CURVE(2,(#410579,#410580,#410581,#410582,#410583,#410584,#410585,
#410586,#410587,#410588,#410589,#410590,#410591),.UNSPECIFIED.,.F.,.F.)
B_SPLINE_CURVE_WITH_KNOTS((3,2,2,2,2,2,3),(0.617647058823529,0.620915032679739,
0.624183006535948,0.627450980392157,0.630718954248366,0.633986928104575,
0.637254901960784),.UNSPECIFIED.)
CURVE()
GEOMETRIC_REPRESENTATION_ITEM()
RATIONAL_B_SPLINE_CURVE((1.,0.866025403784439,1.,0.866025403784439,1.,0.866025403784439,
1.,0.866025403784439,1.,0.866025403784439,1.,0.866025403784439,1.))
REPRESENTATION_ITEM('')
);
#4391=(
BOUNDED_CURVE()
B_SPLINE_CURVE(2,(#410596,#410597,#410598,#410599,#410600,#410601,#410602,
#410603,#410604,#410605,#410606,#410607,#410608),.UNSPECIFIED.,.F.,.F.)
B_SPLINE_CURVE_WITH_KNOTS((3,2,2,2,2,2,3),(0.637254901960784,0.640522875816993,
0.643790849673203,0.647058823529412,0.650326797385621,0.65359477124183,
0.656862745098039),.UNSPECIFIED.)
CURVE()
GEOMETRIC_REPRESENTATION_ITEM()
RATIONAL_B_SPLINE_CURVE((1.,0.866025403784439,1.,0.866025403784439,1.,0.866025403784439,
1.,0.866025403784439,1.,0.866025403784439,1.,0.866025403784439,1.))
REPRESENTATION_ITEM('')
);
#4392=(
BOUNDED_CURVE()
B_SPLINE_CURVE(2,(#410609,#410610,#410611,#410612,#410613,#410614,#410615,
#410616,#410617,#410618,#410619,#410620,#410621),.UNSPECIFIED.,.F.,.F.)
B_SPLINE_CURVE_WITH_KNOTS((3,2,2,2,2,2,3),(0.637254901960784,0.640522875816993,
0.643790849673203,0.647058823529412,0.650326797385621,0.65359477124183,
0.656862745098039),.UNSPECIFIED.)
CURVE()
GEOMETRIC_REPRESENTATION_ITEM()
RATIONAL_B_SPLINE_CURVE((1.,0.866025403784439,1.,0.866025403784439,1.,0.866025403784439,
1.,0.866025403784439,1.,0.866025403784439,1.,0.866025403784439,1.))
REPRESENTATION_ITEM('')
);
#4393=(
BOUNDED_CURVE()
B_SPLINE_CURVE(2,(#410626,#410627,#410628,#410629,#410630,#410631,#410632,
#410633,#410634,#410635,#410636,#410637,#410638),.UNSPECIFIED.,.F.,.F.)
B_SPLINE_CURVE_WITH_KNOTS((3,2,2,2,2,2,3),(0.656862745098039,0.660130718954248,
0.663398692810457,0.666666666666667,0.669934640522876,0.673202614379085,
0.676470588235294),.UNSPECIFIED.)
CURVE()
GEOMETRIC_REPRESENTATION_ITEM()
RATIONAL_B_SPLINE_CURVE((1.,0.866025403784439,1.,0.866025403784439,1.,0.866025403784439,
1.,0.866025403784439,1.,0.866025403784439,1.,0.866025403784439,1.))
REPRESENTATION_ITEM('')
);
#4394=(
BOUNDED_CURVE()
B_SPLINE_CURVE(2,(#410639,#410640,#410641,#410642,#410643,#410644,#410645,
#410646,#410647,#410648,#410649,#410650,#410651),.UNSPECIFIED.,.F.,.F.)
B_SPLINE_CURVE_WITH_KNOTS((3,2,2,2,2,2,3),(0.656862745098039,0.660130718954248,
0.663398692810457,0.666666666666667,0.669934640522876,0.673202614379085,
0.676470588235294),.UNSPECIFIED.)
CURVE()
GEOMETRIC_REPRESENTATION_ITEM()
RATIONAL_B_SPLINE_CURVE((1.,0.866025403784439,1.,0.866025403784439,1.,0.866025403784439,
1.,0.866025403784439,1.,0.866025403784439,1.,0.866025403784439,1.))
REPRESENTATION_ITEM('')
);
#4395=(
BOUNDED_CURVE()
B_SPLINE_CURVE(2,(#410656,#410657,#410658,#410659,#410660,#410661,#410662,
#410663,#410664,#410665,#410666,#410667,#410668),.UNSPECIFIED.,.F.,.F.)
B_SPLINE_CURVE_WITH_KNOTS((3,2,2,2,2,2,3),(0.676470588235294,0.679738562091503,
0.683006535947712,0.686274509803922,0.689542483660131,0.69281045751634,
0.696078431372549),.UNSPECIFIED.)
CURVE()
GEOMETRIC_REPRESENTATION_ITEM()
RATIONAL_B_SPLINE_CURVE((1.,0.866025403784439,1.,0.866025403784439,1.,0.866025403784439,
1.,0.866025403784439,1.,0.866025403784439,1.,0.866025403784439,1.))
REPRESENTATION_ITEM('')
);
#4396=(
BOUNDED_CURVE()
B_SPLINE_CURVE(2,(#410669,#410670,#410671,#410672,#410673,#410674,#410675,
#410676,#410677,#410678,#410679,#410680,#410681),.UNSPECIFIED.,.F.,.F.)
B_SPLINE_CURVE_WITH_KNOTS((3,2,2,2,2,2,3),(0.676470588235294,0.679738562091503,
0.683006535947712,0.686274509803922,0.689542483660131,0.69281045751634,
0.696078431372549),.UNSPECIFIED.)
CURVE()
GEOMETRIC_REPRESENTATION_ITEM()
RATIONAL_B_SPLINE_CURVE((1.,0.866025403784439,1.,0.866025403784439,1.,0.866025403784439,
1.,0.866025403784439,1.,0.866025403784439,1.,0.866025403784439,1.))
REPRESENTATION_ITEM('')
);
#4397=(
BOUNDED_CURVE()
B_SPLINE_CURVE(2,(#414250,#414251,#414252),.UNSPECIFIED.,.F.,.F.)
B_SPLINE_CURVE_WITH_KNOTS((3,3),(0.127655147271297,0.355324362692749),
 .UNSPECIFIED.)
CURVE()
GEOMETRIC_REPRESENTATION_ITEM()
RATIONAL_B_SPLINE_CURVE((1.37128129211021,1.58341924626905,1.37128129211021))
REPRESENTATION_ITEM('')
);
#4398=(
BOUNDED_CURVE()
B_SPLINE_CURVE(2,(#420116,#420117,#420118),.UNSPECIFIED.,.F.,.F.)
B_SPLINE_CURVE_WITH_KNOTS((3,3),(-0.35532436269275,-0.127655147271297),
 .UNSPECIFIED.)
CURVE()
GEOMETRIC_REPRESENTATION_ITEM()
RATIONAL_B_SPLINE_CURVE((1.37128129211021,1.58341924626905,1.37128129211021))
REPRESENTATION_ITEM('')
);
#4399=(
BOUNDED_CURVE()
B_SPLINE_CURVE(2,(#420126,#420127,#420128),.UNSPECIFIED.,.F.,.F.)
B_SPLINE_CURVE_WITH_KNOTS((3,3),(-0.355324362692752,-0.127655147271298),
 .UNSPECIFIED.)
CURVE()
GEOMETRIC_REPRESENTATION_ITEM()
RATIONAL_B_SPLINE_CURVE((1.37128129211021,1.58341924626906,1.37128129211021))
REPRESENTATION_ITEM('')
);
#4400=(
BOUNDED_CURVE()
B_SPLINE_CURVE(2,(#420131,#420132,#420133),.UNSPECIFIED.,.F.,.F.)
B_SPLINE_CURVE_WITH_KNOTS((3,3),(-0.355324362692752,-0.127655147271297),
 .UNSPECIFIED.)
CURVE()
GEOMETRIC_REPRESENTATION_ITEM()
RATIONAL_B_SPLINE_CURVE((1.37128129211021,1.58341924626906,1.37128129211021))
REPRESENTATION_ITEM('')
);
#4401=(
BOUNDED_CURVE()
B_SPLINE_CURVE(2,(#420136,#420137,#420138),.UNSPECIFIED.,.F.,.F.)
B_SPLINE_CURVE_WITH_KNOTS((3,3),(-0.35532436269275,-0.127655147271297),
 .UNSPECIFIED.)
CURVE()
GEOMETRIC_REPRESENTATION_ITEM()
RATIONAL_B_SPLINE_CURVE((1.37128129211021,1.58341924626905,1.37128129211021))
REPRESENTATION_ITEM('')
);
#4402=(
BOUNDED_CURVE()
B_SPLINE_CURVE(2,(#420140,#420141,#420142),.UNSPECIFIED.,.F.,.F.)
B_SPLINE_CURVE_WITH_KNOTS((3,3),(-0.35532436269275,-0.127655147271297),
 .UNSPECIFIED.)
CURVE()
GEOMETRIC_REPRESENTATION_ITEM()
RATIONAL_B_SPLINE_CURVE((1.37128129211021,1.58341924626905,1.37128129211021))
REPRESENTATION_ITEM('')
);
#4403=(
BOUNDED_CURVE()
B_SPLINE_CURVE(2,(#421377,#421378,#421379,#421380,#421381),
 .UNSPECIFIED.,.F.,.F.)
B_SPLINE_CURVE_WITH_KNOTS((3,2,3),(0.696078431372549,0.699346405228758,
0.700529377982283),.UNSPECIFIED.)
CURVE()
GEOMETRIC_REPRESENTATION_ITEM()
RATIONAL_B_SPLINE_CURVE((1.,0.866025403784439,1.,0.951502581121805,0.938116290834926))
REPRESENTATION_ITEM('')
);
#4404=(
BOUNDED_CURVE()
B_SPLINE_CURVE(2,(#421383,#421384,#421385,#421386,#421387,#421388,#421389),
 .UNSPECIFIED.,.F.,.F.)
B_SPLINE_CURVE_WITH_KNOTS((3,2,2,3),(0.696078431372549,0.699346405228758,
0.702614379084967,0.7029856219326),.UNSPECIFIED.)
CURVE()
GEOMETRIC_REPRESENTATION_ITEM()
RATIONAL_B_SPLINE_CURVE((1.,0.866025403784439,1.,0.866025403784439,1.,0.984780444153479,
0.973018780873287))
REPRESENTATION_ITEM('')
);
#4405=SHAPE_REPRESENTATION_RELATIONSHIP('SRR','None',#459330,#4426);
#4406=SHAPE_REPRESENTATION_RELATIONSHIP('SRR','None',#459331,#4427);
#4407=SHAPE_REPRESENTATION_RELATIONSHIP('SRR','None',#459332,#4428);
#4408=SHAPE_REPRESENTATION_RELATIONSHIP('SRR','None',#459333,#4429);
#4409=SHAPE_REPRESENTATION_RELATIONSHIP('SRR','None',#459334,#4430);
#4410=SHAPE_REPRESENTATION_RELATIONSHIP('SRR','None',#459335,#4431);
#4411=SHAPE_REPRESENTATION_RELATIONSHIP('SRR','None',#459336,#4432);
#4412=SHAPE_REPRESENTATION_RELATIONSHIP('SRR','None',#459337,#4433);
#4413=SHAPE_REPRESENTATION_RELATIONSHIP('SRR','None',#459338,#4434);
#4414=SHAPE_REPRESENTATION_RELATIONSHIP('SRR','None',#459340,#4435);
#4415=SHAPE_REPRESENTATION_RELATIONSHIP('SRR','None',#459341,#4436);
#4416=SHAPE_REPRESENTATION_RELATIONSHIP('SRR','None',#459342,#4437);
#4417=SHAPE_REPRESENTATION_RELATIONSHIP('SRR','None',#459343,#4438);
#4418=SHAPE_REPRESENTATION_RELATIONSHIP('SRR','None',#459344,#4439);
#4419=SHAPE_REPRESENTATION_RELATIONSHIP('SRR','None',#459345,#4440);
#4420=SHAPE_REPRESENTATION_RELATIONSHIP('SRR','None',#459346,#4441);
#4421=SHAPE_REPRESENTATION_RELATIONSHIP('SRR','None',#459348,#4442);
#4422=SHAPE_REPRESENTATION_RELATIONSHIP('SRR','None',#459349,#4443);
#4423=SHAPE_REPRESENTATION_RELATIONSHIP('SRR','None',#459350,#4444);
#4424=SHAPE_REPRESENTATION_RELATIONSHIP('SRR','None',#459351,#4445);
#4425=SHAPE_REPRESENTATION_RELATIONSHIP('SRR','None',#459352,#4446);
#4426=ADVANCED_BREP_SHAPE_REPRESENTATION('',(#4447),#459219);
#4427=ADVANCED_BREP_SHAPE_REPRESENTATION('',(#4448,#4449),#459220);
#4428=ADVANCED_BREP_SHAPE_REPRESENTATION('',(#4450,#1620),#459221);
#4429=ADVANCED_BREP_SHAPE_REPRESENTATION('',(#4451),#459222);
#4430=ADVANCED_BREP_SHAPE_REPRESENTATION('',(#4452),#459223);
#4431=ADVANCED_BREP_SHAPE_REPRESENTATION('',(#4453),#459224);
#4432=ADVANCED_BREP_SHAPE_REPRESENTATION('',(#4454,#4455),#459225);
#4433=ADVANCED_BREP_SHAPE_REPRESENTATION('',(#4456,#4457),#459226);
#4434=ADVANCED_BREP_SHAPE_REPRESENTATION('',(#4458,#4459,#4460,#4461,#4462,
#4463,#4464,#4465,#4466),#459227);
#4435=ADVANCED_BREP_SHAPE_REPRESENTATION('',(#4467),#459229);
#4436=ADVANCED_BREP_SHAPE_REPRESENTATION('',(#4468),#459230);
#4437=ADVANCED_BREP_SHAPE_REPRESENTATION('',(#4469,#4470,#4471,#4472,#4473,
#4474,#4475,#4476,#4477,#4478,#4479,#4480,#4481,#4482,#4483,#4484),#459231);
#4438=ADVANCED_BREP_SHAPE_REPRESENTATION('',(#4485),#459232);
#4439=ADVANCED_BREP_SHAPE_REPRESENTATION('',(#4486),#459233);
#4440=ADVANCED_BREP_SHAPE_REPRESENTATION('',(#4487),#459234);
#4441=ADVANCED_BREP_SHAPE_REPRESENTATION('',(#4488),#459235);
#4442=ADVANCED_BREP_SHAPE_REPRESENTATION('',(#4489),#459237);
#4443=ADVANCED_BREP_SHAPE_REPRESENTATION('',(#4490),#459238);
#4444=ADVANCED_BREP_SHAPE_REPRESENTATION('',(#4491),#459239);
#4445=ADVANCED_BREP_SHAPE_REPRESENTATION('',(#4492),#459240);
#4446=ADVANCED_BREP_SHAPE_REPRESENTATION('',(#4493),#459241);
#4447=MANIFOLD_SOLID_BREP('NEMA14 body',#94623);
#4448=MANIFOLD_SOLID_BREP('Fitting body',#94624);
#4449=MANIFOLD_SOLID_BREP('Fixer',#94625);
#4450=MANIFOLD_SOLID_BREP('Body',#94626);
#4451=MANIFOLD_SOLID_BREP('Rocker',#94629);
#4452=MANIFOLD_SOLID_BREP('Shaft body',#94630);
#4453=MANIFOLD_SOLID_BREP('Shaft body',#94631);
#4454=MANIFOLD_SOLID_BREP('Feed gear',#94632);
#4455=MANIFOLD_SOLID_BREP('Drive gear',#94633);
#4456=MANIFOLD_SOLID_BREP('Gear44',#94634);
#4457=MANIFOLD_SOLID_BREP('Gear17',#94635);
#4458=MANIFOLD_SOLID_BREP('Bearing body',#94636);
#4459=MANIFOLD_SOLID_BREP('Roller 1',#94637);
#4460=MANIFOLD_SOLID_BREP('Roller 2',#94638);
#4461=MANIFOLD_SOLID_BREP('Roller 3',#94639);
#4462=MANIFOLD_SOLID_BREP('Roller 4',#94640);
#4463=MANIFOLD_SOLID_BREP('Roller 5',#94641);
#4464=MANIFOLD_SOLID_BREP('Roller 6',#94642);
#4465=MANIFOLD_SOLID_BREP('Roller 7',#94643);
#4466=MANIFOLD_SOLID_BREP('Roller 8',#94644);
#4467=MANIFOLD_SOLID_BREP('Body1',#94645);
#4468=MANIFOLD_SOLID_BREP('Body1',#94646);
#4469=MANIFOLD_SOLID_BREP('Body1',#94647);
#4470=MANIFOLD_SOLID_BREP('Body2',#94648);
#4471=MANIFOLD_SOLID_BREP('Body3',#94649);
#4472=MANIFOLD_SOLID_BREP('Body4',#94650);
#4473=MANIFOLD_SOLID_BREP('Body5',#94651);
#4474=MANIFOLD_SOLID_BREP('Body6',#94652);
#4475=MANIFOLD_SOLID_BREP('Body7',#94653);
#4476=MANIFOLD_SOLID_BREP('Body8',#94654);
#4477=MANIFOLD_SOLID_BREP('Body9',#94655);
#4478=MANIFOLD_SOLID_BREP('Body10',#94656);
#4479=MANIFOLD_SOLID_BREP('Body11',#94657);
#4480=MANIFOLD_SOLID_BREP('Body12',#94658);
#4481=MANIFOLD_SOLID_BREP('Body13',#94659);
#4482=MANIFOLD_SOLID_BREP('Body14',#94660);
#4483=MANIFOLD_SOLID_BREP('Body15',#94661);
#4484=MANIFOLD_SOLID_BREP('Body16',#94662);
#4485=MANIFOLD_SOLID_BREP('Body',#94663);
#4486=MANIFOLD_SOLID_BREP('Body1',#94664);
#4487=MANIFOLD_SOLID_BREP('Body',#94665);
#4488=MANIFOLD_SOLID_BREP('Body',#94666);
#4489=MANIFOLD_SOLID_BREP('E3D V6 heathink',#94667);
#4490=MANIFOLD_SOLID_BREP('E3D V6 throat',#94668);
#4491=MANIFOLD_SOLID_BREP('Body1',#94669);
#4492=MANIFOLD_SOLID_BREP('E3D V6 nozzle',#94670);
#4493=MANIFOLD_SOLID_BREP('E3D V6 heatblock',#94671);
#4494=STYLED_ITEM('',(#459540),#88842);
#4495=STYLED_ITEM('',(#459540),#88843);
#4496=STYLED_ITEM('',(#459540),#88846);
#4497=STYLED_ITEM('',(#459540),#88849);
#4498=STYLED_ITEM('',(#459540),#88881);
#4499=STYLED_ITEM('',(#459540),#88885);
#4500=STYLED_ITEM('',(#459540),#88886);
#4501=STYLED_ITEM('',(#459540),#88887);
#4502=STYLED_ITEM('',(#459540),#88888);
#4503=STYLED_ITEM('',(#459540),#88889);
#4504=STYLED_ITEM('',(#459540),#88890);
#4505=STYLED_ITEM('',(#459540),#88891);
#4506=STYLED_ITEM('',(#459540),#88892);
#4507=STYLED_ITEM('',(#459540),#88893);
#4508=STYLED_ITEM('',(#459540),#88894);
#4509=STYLED_ITEM('',(#459540),#88895);
#4510=STYLED_ITEM('',(#459540),#88896);
#4511=STYLED_ITEM('',(#459540),#88897);
#4512=STYLED_ITEM('',(#459540),#88898);
#4513=STYLED_ITEM('',(#459540),#88899);
#4514=STYLED_ITEM('',(#459540),#88900);
#4515=STYLED_ITEM('',(#459540),#88901);
#4516=STYLED_ITEM('',(#459540),#88902);
#4517=STYLED_ITEM('',(#459540),#88903);
#4518=STYLED_ITEM('',(#459540),#88904);
#4519=STYLED_ITEM('',(#459540),#88905);
#4520=STYLED_ITEM('',(#459540),#88906);
#4521=STYLED_ITEM('',(#459540),#88907);
#4522=STYLED_ITEM('',(#459540),#88908);
#4523=STYLED_ITEM('',(#459540),#88909);
#4524=STYLED_ITEM('',(#459540),#88910);
#4525=STYLED_ITEM('',(#459540),#88911);
#4526=STYLED_ITEM('',(#459540),#88912);
#4527=STYLED_ITEM('',(#459540),#88913);
#4528=STYLED_ITEM('',(#459540),#88914);
#4529=STYLED_ITEM('',(#459540),#88915);
#4530=STYLED_ITEM('',(#459540),#88916);
#4531=STYLED_ITEM('',(#459540),#88917);
#4532=STYLED_ITEM('',(#459540),#88918);
#4533=STYLED_ITEM('',(#459540),#88919);
#4534=STYLED_ITEM('',(#459540),#88920);
#4535=STYLED_ITEM('',(#459540),#88921);
#4536=STYLED_ITEM('',(#459540),#88922);
#4537=STYLED_ITEM('',(#459540),#88923);
#4538=STYLED_ITEM('',(#459540),#88924);
#4539=STYLED_ITEM('',(#459540),#88925);
#4540=STYLED_ITEM('',(#459540),#88926);
#4541=STYLED_ITEM('',(#459540),#88927);
#4542=STYLED_ITEM('',(#459540),#88928);
#4543=STYLED_ITEM('',(#459540),#88929);
#4544=STYLED_ITEM('',(#459540),#88930);
#4545=STYLED_ITEM('',(#459540),#88931);
#4546=STYLED_ITEM('',(#459540),#88932);
#4547=STYLED_ITEM('',(#459540),#88933);
#4548=STYLED_ITEM('',(#459540),#88934);
#4549=STYLED_ITEM('',(#459540),#88935);
#4550=STYLED_ITEM('',(#459540),#88936);
#4551=STYLED_ITEM('',(#459540),#88937);
#4552=STYLED_ITEM('',(#459540),#88938);
#4553=STYLED_ITEM('',(#459540),#88939);
#4554=STYLED_ITEM('',(#459540),#88940);
#4555=STYLED_ITEM('',(#459540),#88941);
#4556=STYLED_ITEM('',(#459540),#88942);
#4557=STYLED_ITEM('',(#459540),#88943);
#4558=STYLED_ITEM('',(#459540),#88944);
#4559=STYLED_ITEM('',(#459540),#88945);
#4560=STYLED_ITEM('',(#459540),#88946);
#4561=STYLED_ITEM('',(#459540),#88947);
#4562=STYLED_ITEM('',(#459540),#88948);
#4563=STYLED_ITEM('',(#459540),#88949);
#4564=STYLED_ITEM('',(#459540),#88997);
#4565=STYLED_ITEM('',(#459540),#88999);
#4566=STYLED_ITEM('',(#459540),#4447);
#4567=STYLED_ITEM('',(#459519),#4448);
#4568=STYLED_ITEM('',(#459519),#4449);
#4569=STYLED_ITEM('',(#459505),#4450);
#4570=STYLED_ITEM('',(#459505),#1620);
#4571=STYLED_ITEM('',(#459519),#4451);
#4572=STYLED_ITEM('',(#459526),#4452);
#4573=STYLED_ITEM('',(#459526),#4453);
#4574=STYLED_ITEM('',(#459512),#4454);
#4575=STYLED_ITEM('',(#459512),#4455);
#4576=STYLED_ITEM('',(#459519),#4456);
#4577=STYLED_ITEM('',(#459519),#4457);
#4578=STYLED_ITEM('',(#459526),#4458);
#4579=STYLED_ITEM('',(#459526),#4459);
#4580=STYLED_ITEM('',(#459526),#4460);
#4581=STYLED_ITEM('',(#459526),#4461);
#4582=STYLED_ITEM('',(#459526),#4462);
#4583=STYLED_ITEM('',(#459526),#4463);
#4584=STYLED_ITEM('',(#459526),#4464);
#4585=STYLED_ITEM('',(#459526),#4465);
#4586=STYLED_ITEM('',(#459526),#4466);
#4587=STYLED_ITEM('',(#459533),#4467);
#4588=STYLED_ITEM('',(#459526),#4468);
#4589=STYLED_ITEM('',(#459526),#4469);
#4590=STYLED_ITEM('',(#459526),#4470);
#4591=STYLED_ITEM('',(#459526),#4471);
#4592=STYLED_ITEM('',(#459526),#4472);
#4593=STYLED_ITEM('',(#459526),#4473);
#4594=STYLED_ITEM('',(#459526),#4474);
#4595=STYLED_ITEM('',(#459526),#4475);
#4596=STYLED_ITEM('',(#459526),#4476);
#4597=STYLED_ITEM('',(#459526),#4477);
#4598=STYLED_ITEM('',(#459526),#4478);
#4599=STYLED_ITEM('',(#459526),#4479);
#4600=STYLED_ITEM('',(#459526),#4480);
#4601=STYLED_ITEM('',(#459526),#4481);
#4602=STYLED_ITEM('',(#459526),#4482);
#4603=STYLED_ITEM('',(#459526),#4483);
#4604=STYLED_ITEM('',(#459526),#4484);
#4605=STYLED_ITEM('',(#459533),#4485);
#4606=STYLED_ITEM('',(#459533),#4486);
#4607=STYLED_ITEM('',(#459533),#4487);
#4608=STYLED_ITEM('',(#459533),#4488);
#4609=STYLED_ITEM('',(#459519),#4489);
#4610=STYLED_ITEM('',(#459519),#4490);
#4611=STYLED_ITEM('',(#459540),#4491);
#4612=STYLED_ITEM('',(#459519),#4492);
#4613=STYLED_ITEM('',(#459505),#4493);
#4614=CONICAL_SURFACE('',#94946,7.95,0.785398163397448);
#4615=CONICAL_SURFACE('',#94953,18.2,0.785398163397448);
#4616=CONICAL_SURFACE('',#94962,18.2,0.785398163397437);
#4617=CONICAL_SURFACE('',#94970,2.55,0.785398163397459);
#4618=CONICAL_SURFACE('',#94977,18.2,0.785398163397459);
#4619=CONICAL_SURFACE('',#94978,1.05,0.785398163397442);
#4620=CONICAL_SURFACE('',#94981,3.45000000056584,0.785398163397459);
#4621=CONICAL_SURFACE('',#94984,1.05,0.785398163397449);
#4622=CONICAL_SURFACE('',#94986,1.05,0.785398163397451);
#4623=CONICAL_SURFACE('',#94989,3.44999999943895,0.785398163397441);
#4624=CONICAL_SURFACE('',#94992,1.05,0.785398163397451);
#4625=CONICAL_SURFACE('',#94995,3.44999999943895,0.785398163397441);
#4626=CONICAL_SURFACE('',#94999,1.05,0.785398163397451);
#4627=CONICAL_SURFACE('',#95002,18.2,0.785398163397448);
#4628=CONICAL_SURFACE('',#95004,1.05,0.785398163397449);
#4629=CONICAL_SURFACE('',#95008,3.45000000056584,0.785398163397459);
#4630=CONICAL_SURFACE('',#95012,1.05,0.785398163397442);
#4631=CONICAL_SURFACE('',#95015,18.2,0.785398163397437);
#4632=CONICAL_SURFACE('',#95017,1.05,0.785398163397451);
#4633=CONICAL_SURFACE('',#95029,1.15,0.785398163397448);
#4634=CONICAL_SURFACE('',#95118,17.45,1.10714871779409);
#4635=CONICAL_SURFACE('',#95122,17.45,1.10714871779411);
#4636=CONICAL_SURFACE('',#95129,17.45,1.10714871779409);
#4637=CONICAL_SURFACE('',#95133,17.45,1.10714871779411);
#4638=CONICAL_SURFACE('',#95137,17.45,1.10714871779409);
#4639=CONICAL_SURFACE('',#95141,17.45,1.10714871779411);
#4640=CONICAL_SURFACE('',#95145,17.45,1.10714871779409);
#4641=CONICAL_SURFACE('',#95149,17.45,1.10714871779411);
#4642=CONICAL_SURFACE('',#95153,17.45,1.10714871779409);
#4643=CONICAL_SURFACE('',#95157,17.45,1.10714871779411);
#4644=CONICAL_SURFACE('',#95161,17.45,1.10714871779409);
#4645=CONICAL_SURFACE('',#95165,17.45,1.10714871779411);
#4646=CONICAL_SURFACE('',#95169,17.45,1.10714871779409);
#4647=CONICAL_SURFACE('',#95173,17.45,1.10714871779411);
#4648=CONICAL_SURFACE('',#95177,17.45,1.10714871779409);
#4649=CONICAL_SURFACE('',#95181,17.45,1.10714871779411);
#4650=CONICAL_SURFACE('',#95185,17.45,1.10714871779409);
#4651=CONICAL_SURFACE('',#95189,17.45,1.10714871779411);
#4652=CONICAL_SURFACE('',#95193,17.45,1.10714871779409);
#4653=CONICAL_SURFACE('',#95197,17.45,1.10714871779411);
#4654=CONICAL_SURFACE('',#95201,17.45,1.10714871779409);
#4655=CONICAL_SURFACE('',#95205,17.45,1.10714871779411);
#4656=CONICAL_SURFACE('',#95209,17.45,1.10714871779409);
#4657=CONICAL_SURFACE('',#95213,17.45,1.10714871779411);
#4658=CONICAL_SURFACE('',#95217,17.45,1.10714871779409);
#4659=CONICAL_SURFACE('',#95221,17.45,1.10714871779411);
#4660=CONICAL_SURFACE('',#95225,17.45,1.10714871779409);
#4661=CONICAL_SURFACE('',#95229,17.45,1.10714871779411);
#4662=CONICAL_SURFACE('',#95234,17.45,1.10714871779409);
#4663=CONICAL_SURFACE('',#95238,17.45,1.10714871779411);
#4664=CONICAL_SURFACE('',#95253,3.5,0.321750554396642);
#4665=CONICAL_SURFACE('',#95255,3.5,0.321750554396642);
#4666=CONICAL_SURFACE('',#95257,3.5,0.321750554396642);
#4667=CONICAL_SURFACE('',#95259,4.,0.558599315343569);
#4668=CONICAL_SURFACE('',#95261,4.,0.558599315343569);
#4669=CONICAL_SURFACE('',#95263,4.,0.558599315343569);
#4670=CONICAL_SURFACE('',#95281,3.5,0.321750554396642);
#4671=CONICAL_SURFACE('',#95283,4.,0.558599315343569);
#4672=CONICAL_SURFACE('',#95787,2.35,0.785398163397448);
#4673=CONICAL_SURFACE('',#95933,17.8449617393671,0.785398163397452);
#4674=CONICAL_SURFACE('',#95988,4.45,0.785398163397449);
#4675=CONICAL_SURFACE('',#96034,8.94496173936711,0.785398163397449);
#4676=CONICAL_SURFACE('',#96037,2.15,0.785398163397448);
#4677=CONICAL_SURFACE('',#96648,1.70000000000068,0.785398163409378);
#4678=CONICAL_SURFACE('',#96655,1.70000000000068,0.785398163385518);
#4679=CONICAL_SURFACE('',#96656,3.3,0.785398163405255);
#4680=CONICAL_SURFACE('',#96688,1.7,0.785398163397448);
#4681=CONICAL_SURFACE('',#96694,1.7,0.785398163397448);
#4682=CONICAL_SURFACE('',#96712,3.3,0.785398163417184);
#4683=CONICAL_SURFACE('',#96758,3.025,0.785398163397444);
#4684=CONICAL_SURFACE('',#96777,3.95,0.78539816339745);
#4685=CONICAL_SURFACE('',#96784,2.25,0.982793723247329);
#4686=CONICAL_SURFACE('',#96794,2.15000000000002,0.78539816339767);
#4687=CONICAL_SURFACE('',#96823,4.45,0.785398163397449);
#4688=CONICAL_SURFACE('',#96825,4.45,0.785398163397449);
#4689=CONICAL_SURFACE('',#96840,8.94496173936711,0.78539816339745);
#4690=CONICAL_SURFACE('',#96849,3.625,0.483447001567199);
#4691=CONICAL_SURFACE('',#96853,1.1,0.588002603547571);
#4692=CONICAL_SURFACE('',#96856,4.43137084989847,0.78539816339745);
#4693=CONICAL_SURFACE('',#96858,4.43137084989847,0.78539816339745);
#4694=CONICAL_SURFACE('',#96860,4.43137084989847,0.78539816339745);
#4695=CONICAL_SURFACE('',#96871,2.75,0.785398163397449);
#4696=CONICAL_SURFACE('',#96872,2.75,0.785398163397449);
#4697=CONICAL_SURFACE('',#96910,3.2,0.785398163397448);
#4698=CONICAL_SURFACE('',#96934,17.8449617393671,0.785398163397452);
#4699=CONICAL_SURFACE('',#96987,3.15,0.785398163397448);
#4700=CONICAL_SURFACE('',#97073,4.68747748340553,0.483447001567199);
#4701=CONICAL_SURFACE('',#97074,4.325,0.785398163397448);
#4702=CONICAL_SURFACE('',#97156,3.3,0.785398163397448);
#4703=CONICAL_SURFACE('',#97159,3.3,0.785398163397448);
#4704=CONICAL_SURFACE('',#97173,4.45,0.785398163397448);
#4705=CONICAL_SURFACE('',#97175,4.45,0.785398163397449);
#4706=CONICAL_SURFACE('',#97185,4.1,0.785398163397445);
#4707=CONICAL_SURFACE('',#97187,4.1,0.785398163397445);
#4708=CONICAL_SURFACE('',#97224,1.4,0.785398163397448);
#4709=CONICAL_SURFACE('',#97230,1.4,0.785398163397448);
#4710=CONICAL_SURFACE('',#97234,1.45,0.785398163397455);
#4711=CONICAL_SURFACE('',#97240,1.45,0.785398163397447);
#4712=CONICAL_SURFACE('',#97454,2.9,0.78539816250733);
#4713=CONICAL_SURFACE('',#97458,1.5,0.78539816250733);
#4714=CONICAL_SURFACE('',#97462,1.5,0.78539816250733);
#4715=CONICAL_SURFACE('',#97466,8.8,0.78539816250733);
#4716=CONICAL_SURFACE('',#97470,1.7,0.78539816250733);
#4717=CONICAL_SURFACE('',#97473,1.7,0.78539816250733);
#4718=CONICAL_SURFACE('',#97476,3.3,0.78539816250733);
#4719=CONICAL_SURFACE('',#97480,2.5,0.78539816250733);
#4720=CONICAL_SURFACE('',#97485,9.,0.78539816250733);
#4721=CONICAL_SURFACE('',#97494,2.272884449,1.04719754999232);
#4722=CONICAL_SURFACE('',#97498,1.816666667,1.04719754999232);
#4723=CONICAL_SURFACE('',#97499,2.272884449,1.04719754999232);
#4724=CONICAL_SURFACE('',#97503,1.816666667,1.04719754999232);
#4725=CONICAL_SURFACE('',#97504,2.272884449,1.04719754999232);
#4726=CONICAL_SURFACE('',#97508,1.816666667,1.04719754999232);
#4727=CONICAL_SURFACE('',#97509,2.272884449,1.04719754999232);
#4728=CONICAL_SURFACE('',#97513,1.816666667,1.04719754999232);
#4729=CONICAL_SURFACE('',#97514,2.272884449,1.04719754999232);
#4730=CONICAL_SURFACE('',#97518,1.816666667,1.04719754999232);
#4731=CONICAL_SURFACE('',#97519,2.272884449,1.04719754999232);
#4732=CONICAL_SURFACE('',#97523,1.816666667,1.04719754999232);
#4733=CONICAL_SURFACE('',#97524,2.272884449,1.04719754999232);
#4734=CONICAL_SURFACE('',#97528,1.816666667,1.04719754999232);
#4735=CONICAL_SURFACE('',#97529,2.272884449,1.04719754999232);
#4736=CONICAL_SURFACE('',#97533,1.816666667,1.04719754999232);
#4737=CONICAL_SURFACE('',#97534,2.272884449,1.04719754999232);
#4738=CONICAL_SURFACE('',#97538,1.816666667,1.04719754999232);
#4739=CONICAL_SURFACE('',#97539,2.272884449,1.04719754999232);
#4740=CONICAL_SURFACE('',#97543,1.816666667,1.04719754999232);
#4741=CONICAL_SURFACE('',#97544,2.272884449,1.04719754999232);
#4742=CONICAL_SURFACE('',#97548,1.816666667,1.04719754999232);
#4743=CONICAL_SURFACE('',#97549,2.272884449,1.04719754999232);
#4744=CONICAL_SURFACE('',#97553,1.816666667,1.04719754999232);
#4745=CONICAL_SURFACE('',#97554,2.272884449,1.04719754999232);
#4746=CONICAL_SURFACE('',#97558,1.816666667,1.04719754999232);
#4747=CONICAL_SURFACE('',#97559,2.272884449,1.04719754999232);
#4748=CONICAL_SURFACE('',#97563,1.816666667,1.04719754999232);
#4749=CONICAL_SURFACE('',#97564,2.272884449,1.04719754999232);
#4750=CONICAL_SURFACE('',#97568,1.816666667,1.04719754999232);
#4751=CONICAL_SURFACE('',#97569,2.272884449,1.04719754999232);
#4752=CONICAL_SURFACE('',#97573,1.816666667,1.04719754999232);
#4753=CONICAL_SURFACE('',#97574,2.272884449,1.04719754999232);
#4754=CONICAL_SURFACE('',#97578,1.816666667,1.04719754999232);
#4755=CONICAL_SURFACE('',#97579,2.272884449,1.04719754999232);
#4756=CONICAL_SURFACE('',#97583,1.816666667,1.04719754999232);
#4757=CONICAL_SURFACE('',#97584,2.272884449,1.04719754999232);
#4758=CONICAL_SURFACE('',#97588,1.816666667,1.04719754999232);
#4759=CONICAL_SURFACE('',#97589,2.272884449,1.04719754999232);
#4760=CONICAL_SURFACE('',#97593,1.816666667,1.04719754999232);
#4761=CONICAL_SURFACE('',#97594,2.272884449,1.04719754999232);
#4762=CONICAL_SURFACE('',#97598,1.816666667,1.04719754999232);
#4763=CONICAL_SURFACE('',#97599,2.272884449,1.04719754999232);
#4764=CONICAL_SURFACE('',#97603,1.816666667,1.04719754999232);
#4765=CONICAL_SURFACE('',#97604,2.272884449,1.04719754999232);
#4766=CONICAL_SURFACE('',#97608,1.816666667,1.04719754999232);
#4767=CONICAL_SURFACE('',#97609,2.272884449,1.04719754999232);
#4768=CONICAL_SURFACE('',#97613,1.816666667,1.04719754999232);
#4769=CONICAL_SURFACE('',#97614,2.272884449,1.04719754999232);
#4770=CONICAL_SURFACE('',#97618,1.816666667,1.04719754999232);
#4771=CONICAL_SURFACE('',#97619,2.272884449,1.04719754999232);
#4772=CONICAL_SURFACE('',#97623,1.816666667,1.04719754999232);
#4773=CONICAL_SURFACE('',#97624,2.272884449,1.04719754999232);
#4774=CONICAL_SURFACE('',#97628,1.816666667,1.04719754999232);
#4775=CONICAL_SURFACE('',#97629,2.272884449,1.04719754999232);
#4776=CONICAL_SURFACE('',#97633,1.816666667,1.04719754999232);
#4777=CONICAL_SURFACE('',#97634,2.272884449,1.04719754999232);
#4778=CONICAL_SURFACE('',#97638,1.816666667,1.04719754999232);
#4779=CONICAL_SURFACE('',#97639,2.272884449,1.04719754999232);
#4780=CONICAL_SURFACE('',#97643,1.816666667,1.04719754999232);
#4781=CONICAL_SURFACE('',#97644,2.272884449,1.04719754999232);
#4782=CONICAL_SURFACE('',#97648,1.816666667,1.04719754999232);
#4783=CONICAL_SURFACE('',#97649,2.272884449,1.04719754999232);
#4784=CONICAL_SURFACE('',#97653,1.816666667,1.04719754999232);
#4785=CONICAL_SURFACE('',#97654,2.272884449,1.04719754999232);
#4786=CONICAL_SURFACE('',#97658,1.816666667,1.04719754999232);
#4787=CONICAL_SURFACE('',#97659,2.272884449,1.04719754999232);
#4788=CONICAL_SURFACE('',#97663,1.816666667,1.04719754999232);
#4789=CONICAL_SURFACE('',#97664,2.272884449,1.04719754999232);
#4790=CONICAL_SURFACE('',#97668,1.816666667,1.04719754999232);
#4791=CONICAL_SURFACE('',#97669,2.272884449,1.04719754999232);
#4792=CONICAL_SURFACE('',#97673,1.816666667,1.04719754999232);
#4793=CONICAL_SURFACE('',#97674,2.272884449,1.04719754999232);
#4794=CONICAL_SURFACE('',#97678,1.816666667,1.04719754999232);
#4795=CONICAL_SURFACE('',#97679,2.272884449,1.04719754999232);
#4796=CONICAL_SURFACE('',#97683,1.816666667,1.04719754999232);
#4797=CONICAL_SURFACE('',#97684,2.272884449,1.04719754999232);
#4798=CONICAL_SURFACE('',#97688,1.816666667,1.04719754999232);
#4799=CONICAL_SURFACE('',#97689,2.272884449,1.04719754999232);
#4800=CONICAL_SURFACE('',#97693,1.816666667,1.04719754999232);
#4801=CONICAL_SURFACE('',#97694,2.272884449,1.04719754999232);
#4802=CONICAL_SURFACE('',#97698,1.816666667,1.04719754999232);
#4803=CONICAL_SURFACE('',#97699,2.272884449,1.04719754999232);
#4804=CONICAL_SURFACE('',#97703,1.816666667,1.04719754999232);
#4805=CONICAL_SURFACE('',#97704,2.272884449,1.04719754999232);
#4806=CONICAL_SURFACE('',#97708,1.816666667,1.04719754999232);
#4807=CONICAL_SURFACE('',#97709,2.272884449,1.04719754999232);
#4808=CONICAL_SURFACE('',#97713,1.816666667,1.04719754999232);
#4809=CONICAL_SURFACE('',#97714,2.272884449,1.04719754999232);
#4810=CONICAL_SURFACE('',#97718,1.816666667,1.04719754999232);
#4811=CONICAL_SURFACE('',#97719,2.272884449,1.04719754999232);
#4812=CONICAL_SURFACE('',#97723,1.816666667,1.04719754999232);
#4813=CONICAL_SURFACE('',#97724,2.272884449,1.04719754999232);
#4814=CONICAL_SURFACE('',#97728,1.816666667,1.04719754999232);
#4815=CONICAL_SURFACE('',#97729,2.272884449,1.04719754999232);
#4816=CONICAL_SURFACE('',#97733,1.816666667,1.04719754999232);
#4817=CONICAL_SURFACE('',#97734,2.272884449,1.04719754999232);
#4818=CONICAL_SURFACE('',#97738,1.816666667,1.04719754999232);
#4819=CONICAL_SURFACE('',#97739,2.272884449,1.04719754999232);
#4820=CONICAL_SURFACE('',#97743,1.816666667,1.04719754999232);
#4821=CONICAL_SURFACE('',#97744,2.272884449,1.04719754999232);
#4822=CONICAL_SURFACE('',#97748,1.816666667,1.04719754999232);
#4823=CONICAL_SURFACE('',#97749,2.272884449,1.04719754999232);
#4824=CONICAL_SURFACE('',#97753,1.816666667,1.04719754999232);
#4825=CONICAL_SURFACE('',#97754,2.272884449,1.04719754999232);
#4826=CONICAL_SURFACE('',#97758,1.816666667,1.04719754999232);
#4827=CONICAL_SURFACE('',#97759,2.272884449,1.04719754999232);
#4828=CONICAL_SURFACE('',#97763,1.816666667,1.04719754999232);
#4829=CONICAL_SURFACE('',#97764,2.272884449,1.04719754999232);
#4830=CONICAL_SURFACE('',#97768,1.816666667,1.04719754999232);
#4831=CONICAL_SURFACE('',#97769,2.272884449,1.04719754999232);
#4832=CONICAL_SURFACE('',#97773,1.816666667,1.04719754999232);
#4833=CONICAL_SURFACE('',#97774,2.272884449,1.04719754999232);
#4834=CONICAL_SURFACE('',#97778,1.816666667,1.04719754999232);
#4835=CONICAL_SURFACE('',#97779,2.272884449,1.04719754999232);
#4836=CONICAL_SURFACE('',#97783,1.816666667,1.04719754999232);
#4837=CONICAL_SURFACE('',#97784,2.272884449,1.04719754999232);
#4838=CONICAL_SURFACE('',#97788,1.816666667,1.04719754999232);
#4839=CONICAL_SURFACE('',#97789,2.272884449,1.04719754999232);
#4840=CONICAL_SURFACE('',#97793,1.816666667,1.04719754999232);
#4841=CONICAL_SURFACE('',#97794,2.272884449,1.04719754999232);
#4842=CONICAL_SURFACE('',#97798,1.816666667,1.04719754999232);
#4843=CONICAL_SURFACE('',#97799,2.272884449,1.04719754999232);
#4844=CONICAL_SURFACE('',#97803,1.816666667,1.04719754999232);
#4845=CONICAL_SURFACE('',#97804,2.272884449,1.04719754999232);
#4846=CONICAL_SURFACE('',#97808,1.816666667,1.04719754999232);
#4847=CONICAL_SURFACE('',#97809,2.272884449,1.04719754999232);
#4848=CONICAL_SURFACE('',#97813,1.816666667,1.04719754999232);
#4849=CONICAL_SURFACE('',#97814,2.272884449,1.04719754999232);
#4850=CONICAL_SURFACE('',#97818,1.816666667,1.04719754999232);
#4851=CONICAL_SURFACE('',#97819,2.272884449,1.04719754999232);
#4852=CONICAL_SURFACE('',#97823,1.816666667,1.04719754999232);
#4853=CONICAL_SURFACE('',#97824,2.272884449,1.04719754999232);
#4854=CONICAL_SURFACE('',#97828,1.816666667,1.04719754999232);
#4855=CONICAL_SURFACE('',#97829,2.272884449,1.04719754999232);
#4856=CONICAL_SURFACE('',#97833,1.816666667,1.04719754999232);
#4857=CONICAL_SURFACE('',#97834,2.272884449,1.04719754999232);
#4858=CONICAL_SURFACE('',#97838,1.816666667,1.04719754999232);
#4859=CONICAL_SURFACE('',#97839,2.272884449,1.04719754999232);
#4860=CONICAL_SURFACE('',#97843,1.816666667,1.04719754999232);
#4861=CONICAL_SURFACE('',#98979,0.4875,0.785398163397448);
#4862=CONICAL_SURFACE('',#98985,0.4875,0.785398163397448);
#4863=CONICAL_SURFACE('',#98988,0.4875,0.785398163397492);
#4864=CONICAL_SURFACE('',#98994,0.4875,0.785398163397492);
#4865=CONICAL_SURFACE('',#98997,0.4875,0.785398163397448);
#4866=CONICAL_SURFACE('',#99003,0.4875,0.785398163397448);
#4867=CONICAL_SURFACE('',#99006,0.4875,0.78539816339745);
#4868=CONICAL_SURFACE('',#99012,0.4875,0.78539816339745);
#4869=CONICAL_SURFACE('',#99015,0.4875,0.785398163397448);
#4870=CONICAL_SURFACE('',#99021,0.4875,0.785398163397448);
#4871=CONICAL_SURFACE('',#99024,0.4875,0.78539816339745);
#4872=CONICAL_SURFACE('',#99030,0.4875,0.78539816339745);
#4873=CONICAL_SURFACE('',#99033,0.4875,0.785398163397448);
#4874=CONICAL_SURFACE('',#99039,0.4875,0.785398163397448);
#4875=CONICAL_SURFACE('',#99042,0.4875,0.78539816339745);
#4876=CONICAL_SURFACE('',#99048,0.4875,0.78539816339745);
#4877=CONICAL_SURFACE('',#99119,1.15470053837925,0.78539816339745);
#4878=CONICAL_SURFACE('',#99127,1.125,0.785398163397447);
#4879=CONICAL_SURFACE('',#99141,1.15470053837925,0.78539816339745);
#4880=CONICAL_SURFACE('',#99142,1.15470053837925,0.78539816339745);
#4881=CONICAL_SURFACE('',#99143,1.15470053837925,0.78539816339745);
#4882=CONICAL_SURFACE('',#99144,1.15470053837925,0.78539816339745);
#4883=CONICAL_SURFACE('',#99145,1.15470053837925,0.78539816339745);
#4884=CONICAL_SURFACE('',#99180,2.875,0.78539816339745);
#4885=CONICAL_SURFACE('',#99186,3.,0.785398163397449);
#4886=CONICAL_SURFACE('',#99194,1.625,0.785398163397448);
#4887=CONICAL_SURFACE('',#99200,1.5,0.785398163397449);
#4888=CONICAL_SURFACE('',#99283,1.15470053837925,0.78539816339745);
#4889=CONICAL_SURFACE('',#99291,1.125,0.785398163397446);
#4890=CONICAL_SURFACE('',#99305,1.15470053837925,0.78539816339745);
#4891=CONICAL_SURFACE('',#99306,1.15470053837925,0.78539816339745);
#4892=CONICAL_SURFACE('',#99307,1.15470053837925,0.78539816339745);
#4893=CONICAL_SURFACE('',#99308,1.15470053837925,0.78539816339745);
#4894=CONICAL_SURFACE('',#99309,1.15470053837925,0.78539816339745);
#4895=CONICAL_SURFACE('',#99351,1.25000000000001,0.78539816339745);
#4896=CONICAL_SURFACE('',#99356,0.866025403784441,0.78539816339745);
#4897=CONICAL_SURFACE('',#99361,2.5,0.785398163397448);
#4898=CONICAL_SURFACE('',#99371,0.866025403784441,0.78539816339745);
#4899=CONICAL_SURFACE('',#99372,0.866025403784441,0.78539816339745);
#4900=CONICAL_SURFACE('',#99373,0.866025403784441,0.78539816339745);
#4901=CONICAL_SURFACE('',#99374,0.866025403784441,0.78539816339745);
#4902=CONICAL_SURFACE('',#99375,0.866025403784441,0.78539816339745);
#4903=CONICAL_SURFACE('',#99447,999.999999999989,0.785398163397443);
#4904=CONICAL_SURFACE('',#99449,1.17524047358083,0.785398163397453);
#4905=CONICAL_SURFACE('',#99451,1.17524047358083,0.785398163397453);
#4906=CONICAL_SURFACE('',#99454,999.999999999989,0.785398163397443);
#4907=CONICAL_SURFACE('',#99459,1.25,1.0471975511966);
#4908=CONICAL_SURFACE('',#99466,1.44337567297406,0.78539816339745);
#4909=CONICAL_SURFACE('',#99472,2.54610912703474,0.785398163397439);
#4910=CONICAL_SURFACE('',#99477,2.73389087296526,0.785398163397455);
#4911=CONICAL_SURFACE('',#100392,1.44337567297406,0.78539816339745);
#4912=CONICAL_SURFACE('',#100393,1.44337567297406,0.78539816339745);
#4913=CONICAL_SURFACE('',#100394,1.44337567297406,0.78539816339745);
#4914=CONICAL_SURFACE('',#100395,1.44337567297406,0.78539816339745);
#4915=CONICAL_SURFACE('',#100396,1.44337567297406,0.78539816339745);
#4916=CONICAL_SURFACE('',#100400,2.75,0.78539816339745);
#4917=CONICAL_SURFACE('',#100439,2.75,0.78539816339745);
#4918=CONICAL_SURFACE('',#100462,2.75,0.78539816339745);
#4919=CONICAL_SURFACE('',#100485,2.75,0.78539816339745);
#4920=CONICAL_SURFACE('',#100508,2.75,0.78539816339745);
#4921=CONICAL_SURFACE('',#100531,2.75,0.78539816339745);
#4922=CONICAL_SURFACE('',#100554,2.75,0.78539816339745);
#4923=CONICAL_SURFACE('',#100577,2.75,0.78539816339745);
#4924=CONICAL_SURFACE('',#100600,2.75,0.78539816339745);
#4925=CONICAL_SURFACE('',#100623,2.75,0.78539816339745);
#4926=CONICAL_SURFACE('',#100646,2.75,0.78539816339745);
#4927=CONICAL_SURFACE('',#100669,2.75,0.78539816339745);
#4928=CONICAL_SURFACE('',#100692,2.75,0.78539816339745);
#4929=CONICAL_SURFACE('',#100715,2.75,0.78539816339745);
#4930=CONICAL_SURFACE('',#100738,2.75,0.78539816339745);
#4931=CONICAL_SURFACE('',#100761,2.75,0.78539816339745);
#4932=CONICAL_SURFACE('',#100784,2.75,0.78539816339745);
#4933=CONICAL_SURFACE('',#100807,2.75,0.78539816339745);
#4934=CONICAL_SURFACE('',#100830,2.75,0.78539816339745);
#4935=CONICAL_SURFACE('',#100853,2.75,0.78539816339745);
#4936=CONICAL_SURFACE('',#100876,2.75,0.78539816339745);
#4937=CONICAL_SURFACE('',#100899,2.75,0.78539816339745);
#4938=CONICAL_SURFACE('',#100922,2.75,0.78539816339745);
#4939=CONICAL_SURFACE('',#100945,2.75,0.78539816339745);
#4940=CONICAL_SURFACE('',#100968,2.75,0.78539816339745);
#4941=CONICAL_SURFACE('',#100991,2.75,0.78539816339745);
#4942=CONICAL_SURFACE('',#101014,2.75,0.78539816339745);
#4943=CONICAL_SURFACE('',#101037,2.75,0.78539816339745);
#4944=CONICAL_SURFACE('',#101060,2.75,0.78539816339745);
#4945=CONICAL_SURFACE('',#101083,2.75,0.78539816339745);
#4946=CONICAL_SURFACE('',#101106,2.75,0.78539816339745);
#4947=CONICAL_SURFACE('',#101129,2.75,0.78539816339745);
#4948=CONICAL_SURFACE('',#101152,2.75,0.78539816339745);
#4949=CONICAL_SURFACE('',#101175,2.75,0.78539816339745);
#4950=CONICAL_SURFACE('',#101198,2.75,0.78539816339745);
#4951=CONICAL_SURFACE('',#101221,2.75,0.78539816339745);
#4952=CONICAL_SURFACE('',#101244,2.75,0.78539816339745);
#4953=CONICAL_SURFACE('',#101267,2.75,0.78539816339745);
#4954=CONICAL_SURFACE('',#101290,2.75,0.78539816339745);
#4955=CONICAL_SURFACE('',#101313,2.75,0.78539816339745);
#4956=CONICAL_SURFACE('',#101336,2.75,0.78539816339745);
#4957=CONICAL_SURFACE('',#101359,2.75,0.78539816339745);
#4958=CONICAL_SURFACE('',#101382,2.75,0.78539816339745);
#4959=CONICAL_SURFACE('',#101405,2.75,0.78539816339745);
#4960=CONICAL_SURFACE('',#101428,2.75,0.78539816339745);
#4961=CONICAL_SURFACE('',#101451,2.75,0.78539816339745);
#4962=CONICAL_SURFACE('',#101474,2.75,0.78539816339745);
#4963=CONICAL_SURFACE('',#101497,2.75,0.78539816339745);
#4964=CONICAL_SURFACE('',#101520,2.75,0.78539816339745);
#4965=CONICAL_SURFACE('',#101543,2.75,0.78539816339745);
#4966=CONICAL_SURFACE('',#101566,2.75,0.78539816339745);
#4967=CONICAL_SURFACE('',#101589,2.75,0.78539816339745);
#4968=CONICAL_SURFACE('',#101612,2.75,0.78539816339745);
#4969=CONICAL_SURFACE('',#101635,2.75,0.78539816339745);
#4970=CONICAL_SURFACE('',#101658,2.75,0.78539816339745);
#4971=CONICAL_SURFACE('',#101681,2.75,0.78539816339745);
#4972=CONICAL_SURFACE('',#101704,2.75,0.78539816339745);
#4973=CONICAL_SURFACE('',#101727,2.75,0.78539816339745);
#4974=CONICAL_SURFACE('',#101750,2.75,0.78539816339745);
#4975=CONICAL_SURFACE('',#101773,2.75,0.78539816339745);
#4976=CONICAL_SURFACE('',#101796,2.75,0.78539816339745);
#4977=CONICAL_SURFACE('',#101819,2.75,0.78539816339745);
#4978=CONICAL_SURFACE('',#101842,2.75,0.78539816339745);
#4979=CONICAL_SURFACE('',#101865,2.75,0.78539816339745);
#4980=CONICAL_SURFACE('',#101888,2.75,0.78539816339745);
#4981=CONICAL_SURFACE('',#101911,2.75,0.78539816339745);
#4982=CONICAL_SURFACE('',#101934,2.75,0.78539816339745);
#4983=CONICAL_SURFACE('',#101957,2.75,0.78539816339745);
#4984=CONICAL_SURFACE('',#101980,2.75,0.78539816339745);
#4985=CONICAL_SURFACE('',#102003,2.75,0.78539816339745);
#4986=CONICAL_SURFACE('',#102026,2.75,0.78539816339745);
#4987=CONICAL_SURFACE('',#102049,2.75,0.78539816339745);
#4988=CONICAL_SURFACE('',#102072,2.75,0.78539816339745);
#4989=CONICAL_SURFACE('',#102095,2.75,0.78539816339745);
#4990=CONICAL_SURFACE('',#102118,2.75,0.78539816339745);
#4991=CONICAL_SURFACE('',#102141,2.75,0.78539816339745);
#4992=CONICAL_SURFACE('',#102164,2.75,0.78539816339745);
#4993=CONICAL_SURFACE('',#102187,2.75,0.78539816339745);
#4994=CONICAL_SURFACE('',#102210,2.75,0.78539816339745);
#4995=CONICAL_SURFACE('',#102233,2.75,0.78539816339745);
#4996=CONICAL_SURFACE('',#102256,2.75,0.78539816339745);
#4997=CONICAL_SURFACE('',#102279,2.75,0.78539816339745);
#4998=CONICAL_SURFACE('',#102302,2.75,0.78539816339745);
#4999=CONICAL_SURFACE('',#102325,2.75,0.78539816339745);
#5000=CONICAL_SURFACE('',#102348,2.75,0.78539816339745);
#5001=CONICAL_SURFACE('',#102371,2.75,0.78539816339745);
#5002=CONICAL_SURFACE('',#102394,2.75,0.78539816339745);
#5003=CONICAL_SURFACE('',#102417,2.75,0.78539816339745);
#5004=CONICAL_SURFACE('',#102440,2.75,0.78539816339745);
#5005=CONICAL_SURFACE('',#102463,2.75,0.78539816339745);
#5006=CONICAL_SURFACE('',#102486,2.75,0.78539816339745);
#5007=CONICAL_SURFACE('',#102509,2.75,0.78539816339745);
#5008=CONICAL_SURFACE('',#102532,2.75,0.78539816339745);
#5009=CONICAL_SURFACE('',#102555,2.75,0.78539816339745);
#5010=CONICAL_SURFACE('',#102578,2.75,0.78539816339745);
#5011=CONICAL_SURFACE('',#102601,2.75,0.78539816339745);
#5012=CONICAL_SURFACE('',#102624,2.75,0.78539816339745);
#5013=CONICAL_SURFACE('',#102647,2.75,0.78539816339745);
#5014=CONICAL_SURFACE('',#102686,999.999999999989,0.785398163397443);
#5015=CONICAL_SURFACE('',#102688,1.17524047358087,0.785398163397454);
#5016=CONICAL_SURFACE('',#103115,1.17524047358087,0.785398163397454);
#5017=CONICAL_SURFACE('',#103117,1.50000000000006,0.785398163397447);
#5018=CONICAL_SURFACE('',#103119,999.999999999989,0.785398163397443);
#5019=CONICAL_SURFACE('',#103120,1.25,1.0471975511966);
#5020=CONICAL_SURFACE('',#103127,1.44337567297406,0.78539816339745);
#5021=CONICAL_SURFACE('',#103133,2.55577460325564,0.785398163397375);
#5022=CONICAL_SURFACE('',#103138,2.72422539674441,0.785398163397447);
#5023=CONICAL_SURFACE('',#103557,1.44337567297406,0.78539816339745);
#5024=CONICAL_SURFACE('',#103558,1.44337567297406,0.78539816339745);
#5025=CONICAL_SURFACE('',#103559,1.44337567297406,0.78539816339745);
#5026=CONICAL_SURFACE('',#103560,1.44337567297406,0.78539816339745);
#5027=CONICAL_SURFACE('',#103561,1.44337567297406,0.78539816339745);
#5028=CONICAL_SURFACE('',#103564,2.75,0.78539816339745);
#5029=CONICAL_SURFACE('',#103598,2.75,0.78539816339745);
#5030=CONICAL_SURFACE('',#103619,2.75,0.78539816339745);
#5031=CONICAL_SURFACE('',#103640,2.75,0.78539816339745);
#5032=CONICAL_SURFACE('',#103661,2.75,0.78539816339745);
#5033=CONICAL_SURFACE('',#103682,2.75,0.78539816339745);
#5034=CONICAL_SURFACE('',#103703,2.75,0.78539816339745);
#5035=CONICAL_SURFACE('',#103724,2.75,0.78539816339745);
#5036=CONICAL_SURFACE('',#103745,2.75,0.78539816339745);
#5037=CONICAL_SURFACE('',#103766,2.75,0.78539816339745);
#5038=CONICAL_SURFACE('',#103787,2.75,0.78539816339745);
#5039=CONICAL_SURFACE('',#103808,2.75,0.78539816339745);
#5040=CONICAL_SURFACE('',#103829,2.75,0.78539816339745);
#5041=CONICAL_SURFACE('',#103850,2.75,0.78539816339745);
#5042=CONICAL_SURFACE('',#103871,2.75,0.78539816339745);
#5043=CONICAL_SURFACE('',#103892,2.75,0.78539816339745);
#5044=CONICAL_SURFACE('',#103913,2.75,0.78539816339745);
#5045=CONICAL_SURFACE('',#103934,2.75,0.78539816339745);
#5046=CONICAL_SURFACE('',#103955,2.75,0.78539816339745);
#5047=CONICAL_SURFACE('',#103976,2.75,0.78539816339745);
#5048=CONICAL_SURFACE('',#103997,2.75,0.78539816339745);
#5049=CONICAL_SURFACE('',#104018,2.75,0.78539816339745);
#5050=CONICAL_SURFACE('',#104039,2.75,0.78539816339745);
#5051=CONICAL_SURFACE('',#104060,2.75,0.78539816339745);
#5052=CONICAL_SURFACE('',#104081,2.75,0.78539816339745);
#5053=CONICAL_SURFACE('',#104102,2.75,0.78539816339745);
#5054=CONICAL_SURFACE('',#104123,2.75,0.78539816339745);
#5055=CONICAL_SURFACE('',#104144,2.75,0.78539816339745);
#5056=CONICAL_SURFACE('',#104165,2.75,0.78539816339745);
#5057=CONICAL_SURFACE('',#104186,2.75,0.78539816339745);
#5058=CONICAL_SURFACE('',#104207,2.75,0.78539816339745);
#5059=CONICAL_SURFACE('',#104228,2.75,0.78539816339745);
#5060=CONICAL_SURFACE('',#104249,2.75,0.78539816339745);
#5061=CONICAL_SURFACE('',#104270,2.75,0.78539816339745);
#5062=CONICAL_SURFACE('',#104291,2.75,0.78539816339745);
#5063=CONICAL_SURFACE('',#104312,2.75,0.78539816339745);
#5064=CONICAL_SURFACE('',#104333,2.75,0.78539816339745);
#5065=CONICAL_SURFACE('',#104354,2.75,0.78539816339745);
#5066=CONICAL_SURFACE('',#104375,2.75,0.78539816339745);
#5067=CONICAL_SURFACE('',#104396,2.75,0.78539816339745);
#5068=CONICAL_SURFACE('',#104417,2.75,0.78539816339745);
#5069=CONICAL_SURFACE('',#104438,2.75,0.78539816339745);
#5070=CONICAL_SURFACE('',#104459,2.75,0.78539816339745);
#5071=CONICAL_SURFACE('',#104480,2.75,0.78539816339745);
#5072=CONICAL_SURFACE('',#104501,2.75,0.78539816339745);
#5073=CONICAL_SURFACE('',#104522,2.75,0.78539816339745);
#5074=CONICAL_SURFACE('',#104543,2.75,0.78539816339745);
#5075=CONICAL_SURFACE('',#104564,2.75,0.78539816339745);
#5076=CONICAL_SURFACE('',#104585,2.75,0.78539816339745);
#5077=CONICAL_SURFACE('',#104606,2.75,0.78539816339745);
#5078=CONICAL_SURFACE('',#104627,2.75,0.78539816339745);
#5079=CONICAL_SURFACE('',#104648,2.75,0.78539816339745);
#5080=CONICAL_SURFACE('',#104669,2.75,0.78539816339745);
#5081=CONICAL_SURFACE('',#104690,2.75,0.78539816339745);
#5082=CONICAL_SURFACE('',#104711,2.75,0.78539816339745);
#5083=CONICAL_SURFACE('',#104732,2.75,0.78539816339745);
#5084=CONICAL_SURFACE('',#104753,2.75,0.78539816339745);
#5085=CONICAL_SURFACE('',#104774,2.75,0.78539816339745);
#5086=CONICAL_SURFACE('',#104795,2.75,0.78539816339745);
#5087=CONICAL_SURFACE('',#104816,2.75,0.78539816339745);
#5088=CONICAL_SURFACE('',#104837,2.75,0.78539816339745);
#5089=CONICAL_SURFACE('',#104858,2.75,0.78539816339745);
#5090=CONICAL_SURFACE('',#104879,2.75,0.78539816339745);
#5091=CONICAL_SURFACE('',#104900,2.75,0.78539816339745);
#5092=CONICAL_SURFACE('',#104921,2.75,0.78539816339745);
#5093=CONICAL_SURFACE('',#104942,2.75,0.78539816339745);
#5094=CONICAL_SURFACE('',#104963,2.75,0.78539816339745);
#5095=CONICAL_SURFACE('',#104984,2.75,0.78539816339745);
#5096=CONICAL_SURFACE('',#105005,2.75,0.78539816339745);
#5097=CONICAL_SURFACE('',#105026,2.75,0.78539816339745);
#5098=CONICAL_SURFACE('',#105047,2.75,0.78539816339745);
#5099=CONICAL_SURFACE('',#105068,2.75,0.78539816339745);
#5100=CONICAL_SURFACE('',#105089,2.75,0.78539816339745);
#5101=CONICAL_SURFACE('',#105110,2.75,0.78539816339745);
#5102=CONICAL_SURFACE('',#105131,2.75,0.78539816339745);
#5103=CONICAL_SURFACE('',#105152,2.75,0.78539816339745);
#5104=CONICAL_SURFACE('',#105173,2.75,0.78539816339745);
#5105=CONICAL_SURFACE('',#105260,2.25,0.785398163397451);
#5106=CONICAL_SURFACE('',#105276,1.99999999999997,0.785398163397454);
#5107=CONICAL_SURFACE('',#105410,2.5,0.78539816339745);
#5108=CONICAL_SURFACE('',#105423,2.1,0.78539816339745);
#5109=CONICAL_SURFACE('',#105466,0.75,0.832981266674432);
#5110=CONICAL_SURFACE('',#105472,0.2,0.832981266674432);
#5111=CONICAL_SURFACE('',#105474,0.5,0.785398163397446);
#5112=CONICAL_SURFACE('',#105479,1.5,0.785398163397446);
#5113=FACE_BOUND('',#12182,.T.);
#5114=FACE_BOUND('',#12186,.T.);
#5115=FACE_BOUND('',#12190,.T.);
#5116=FACE_BOUND('',#12194,.T.);
#5117=FACE_BOUND('',#12198,.T.);
#5118=FACE_BOUND('',#12201,.T.);
#5119=FACE_BOUND('',#12232,.T.);
#5120=FACE_BOUND('',#12233,.T.);
#5121=FACE_BOUND('',#12234,.T.);
#5122=FACE_BOUND('',#12241,.T.);
#5123=FACE_BOUND('',#12244,.T.);
#5124=FACE_BOUND('',#12374,.T.);
#5125=FACE_BOUND('',#12377,.T.);
#5126=FACE_BOUND('',#12581,.T.);
#5127=FACE_BOUND('',#12584,.T.);
#5128=FACE_BOUND('',#12585,.T.);
#5129=FACE_BOUND('',#12590,.T.);
#5130=FACE_BOUND('',#12591,.T.);
#5131=FACE_BOUND('',#12592,.T.);
#5132=FACE_BOUND('',#12593,.T.);
#5133=FACE_BOUND('',#12594,.T.);
#5134=FACE_BOUND('',#12605,.T.);
#5135=FACE_BOUND('',#12648,.T.);
#5136=FACE_BOUND('',#12676,.T.);
#5137=FACE_BOUND('',#12677,.T.);
#5138=FACE_BOUND('',#12689,.T.);
#5139=FACE_BOUND('',#12708,.T.);
#5140=FACE_BOUND('',#12768,.T.);
#5141=FACE_BOUND('',#12943,.T.);
#5142=FACE_BOUND('',#12965,.T.);
#5143=FACE_BOUND('',#12969,.T.);
#5144=FACE_BOUND('',#13002,.T.);
#5145=FACE_BOUND('',#13027,.T.);
#5146=FACE_BOUND('',#13029,.T.);
#5147=FACE_BOUND('',#13030,.T.);
#5148=FACE_BOUND('',#13031,.T.);
#5149=FACE_BOUND('',#13045,.T.);
#5150=FACE_BOUND('',#13069,.T.);
#5151=FACE_BOUND('',#13071,.T.);
#5152=FACE_BOUND('',#13080,.T.);
#5153=FACE_BOUND('',#13083,.T.);
#5154=FACE_BOUND('',#13089,.T.);
#5155=FACE_BOUND('',#13123,.T.);
#5156=FACE_BOUND('',#13130,.T.);
#5157=FACE_BOUND('',#13147,.T.);
#5158=FACE_BOUND('',#13199,.T.);
#5159=FACE_BOUND('',#13213,.T.);
#5160=FACE_BOUND('',#13214,.T.);
#5161=FACE_BOUND('',#13215,.T.);
#5162=FACE_BOUND('',#13230,.T.);
#5163=FACE_BOUND('',#13257,.T.);
#5164=FACE_BOUND('',#13264,.T.);
#5165=FACE_BOUND('',#13266,.T.);
#5166=FACE_BOUND('',#13270,.T.);
#5167=FACE_BOUND('',#13272,.T.);
#5168=FACE_BOUND('',#13278,.T.);
#5169=FACE_BOUND('',#13281,.T.);
#5170=FACE_BOUND('',#13390,.T.);
#5171=FACE_BOUND('',#13392,.T.);
#5172=FACE_BOUND('',#13393,.T.);
#5173=FACE_BOUND('',#13394,.T.);
#5174=FACE_BOUND('',#13396,.T.);
#5175=FACE_BOUND('',#13397,.T.);
#5176=FACE_BOUND('',#13398,.T.);
#5177=FACE_BOUND('',#13633,.T.);
#5178=FACE_BOUND('',#13634,.T.);
#5179=FACE_BOUND('',#13635,.T.);
#5180=FACE_BOUND('',#13636,.T.);
#5181=FACE_BOUND('',#13637,.T.);
#5182=FACE_BOUND('',#13675,.T.);
#5183=FACE_BOUND('',#13676,.T.);
#5184=FACE_BOUND('',#13677,.T.);
#5185=FACE_BOUND('',#13787,.T.);
#5186=FACE_BOUND('',#13791,.T.);
#5187=FACE_BOUND('',#13996,.T.);
#5188=FACE_BOUND('',#14004,.T.);
#5189=FACE_BOUND('',#14010,.T.);
#5190=FACE_BOUND('',#14013,.T.);
#5191=FACE_BOUND('',#14066,.T.);
#5192=FACE_BOUND('',#14120,.T.);
#5193=FACE_BOUND('',#14123,.T.);
#5194=FACE_BOUND('',#14125,.T.);
#5195=FACE_BOUND('',#14126,.T.);
#5196=FACE_BOUND('',#14127,.T.);
#5197=FACE_BOUND('',#14128,.T.);
#5198=FACE_BOUND('',#14129,.T.);
#5199=FACE_BOUND('',#14130,.T.);
#5200=FACE_BOUND('',#14131,.T.);
#5201=FACE_BOUND('',#14134,.T.);
#5202=FACE_BOUND('',#14135,.T.);
#5203=FACE_BOUND('',#14136,.T.);
#5204=FACE_BOUND('',#14137,.T.);
#5205=FACE_BOUND('',#14138,.T.);
#5206=FACE_BOUND('',#14139,.T.);
#5207=FACE_BOUND('',#14140,.T.);
#5208=FACE_BOUND('',#14143,.T.);
#5209=FACE_BOUND('',#14282,.T.);
#5210=FACE_BOUND('',#14288,.T.);
#5211=FACE_BOUND('',#14290,.T.);
#5212=FACE_BOUND('',#14292,.T.);
#5213=FACE_BOUND('',#14323,.T.);
#5214=FACE_BOUND('',#14325,.T.);
#5215=FACE_BOUND('',#14333,.T.);
#5216=FACE_BOUND('',#14335,.T.);
#5217=FACE_BOUND('',#14351,.T.);
#5218=FACE_BOUND('',#14353,.T.);
#5219=FACE_BOUND('',#14357,.T.);
#5220=FACE_BOUND('',#14359,.T.);
#5221=FACE_BOUND('',#14393,.T.);
#5222=FACE_BOUND('',#14399,.T.);
#5223=FACE_BOUND('',#14401,.T.);
#5224=FACE_BOUND('',#14403,.T.);
#5225=FACE_BOUND('',#14454,.T.);
#5226=FACE_BOUND('',#14649,.T.);
#5227=FACE_BOUND('',#14664,.T.);
#5228=FACE_BOUND('',#16574,.T.);
#5229=FACE_BOUND('',#16581,.T.);
#5230=FACE_BOUND('',#17895,.T.);
#5231=FACE_BOUND('',#17896,.T.);
#5232=FACE_BOUND('',#17897,.T.);
#5233=FACE_BOUND('',#17898,.T.);
#5234=FACE_BOUND('',#17899,.T.);
#5235=FACE_BOUND('',#17904,.T.);
#5236=FACE_BOUND('',#17905,.T.);
#5237=FACE_BOUND('',#17906,.T.);
#5238=FACE_BOUND('',#17907,.T.);
#5239=FACE_BOUND('',#17908,.T.);
#5240=FACE_BOUND('',#17934,.T.);
#5241=FACE_BOUND('',#17936,.T.);
#5242=FACE_BOUND('',#17938,.T.);
#5243=FACE_BOUND('',#17940,.T.);
#5244=FACE_BOUND('',#17942,.T.);
#5245=FACE_BOUND('',#17944,.T.);
#5246=FACE_BOUND('',#17946,.T.);
#5247=FACE_BOUND('',#17948,.T.);
#5248=FACE_BOUND('',#17950,.T.);
#5249=FACE_BOUND('',#17952,.T.);
#5250=FACE_BOUND('',#17954,.T.);
#5251=FACE_BOUND('',#17956,.T.);
#5252=FACE_BOUND('',#17958,.T.);
#5253=FACE_BOUND('',#17960,.T.);
#5254=FACE_BOUND('',#17962,.T.);
#5255=FACE_BOUND('',#17964,.T.);
#5256=FACE_BOUND('',#17966,.T.);
#5257=FACE_BOUND('',#17968,.T.);
#5258=FACE_BOUND('',#17970,.T.);
#5259=FACE_BOUND('',#17972,.T.);
#5260=FACE_BOUND('',#18019,.T.);
#5261=FACE_BOUND('',#18033,.T.);
#5262=FACE_BOUND('',#18036,.T.);
#5263=FACE_BOUND('',#18038,.T.);
#5264=FACE_BOUND('',#18040,.T.);
#5265=FACE_BOUND('',#18044,.T.);
#5266=FACE_BOUND('',#18063,.T.);
#5267=FACE_BOUND('',#18074,.T.);
#5268=FACE_BOUND('',#18076,.T.);
#5269=FACE_BOUND('',#18084,.T.);
#5270=FACE_BOUND('',#18094,.T.);
#5271=FACE_BOUND('',#18095,.T.);
#5272=FACE_BOUND('',#18099,.T.);
#5273=FACE_BOUND('',#18100,.T.);
#5274=FACE_BOUND('',#18102,.T.);
#5275=FACE_BOUND('',#18103,.T.);
#5276=FACE_BOUND('',#18105,.T.);
#5277=FACE_BOUND('',#18107,.T.);
#5278=PLANE('',#94935);
#5279=PLANE('',#94940);
#5280=PLANE('',#94951);
#5281=PLANE('',#94960);
#5282=PLANE('',#94968);
#5283=PLANE('',#94973);
#5284=PLANE('',#94980);
#5285=PLANE('',#94983);
#5286=PLANE('',#94988);
#5287=PLANE('',#94991);
#5288=PLANE('',#94994);
#5289=PLANE('',#94998);
#5290=PLANE('',#95007);
#5291=PLANE('',#95011);
#5292=PLANE('',#95021);
#5293=PLANE('',#95024);
#5294=PLANE('',#95025);
#5295=PLANE('',#95028);
#5296=PLANE('',#95034);
#5297=PLANE('',#95055);
#5298=PLANE('',#95056);
#5299=PLANE('',#95078);
#5300=PLANE('',#95080);
#5301=PLANE('',#95083);
#5302=PLANE('',#95085);
#5303=PLANE('',#95087);
#5304=PLANE('',#95089);
#5305=PLANE('',#95091);
#5306=PLANE('',#95093);
#5307=PLANE('',#95095);
#5308=PLANE('',#95097);
#5309=PLANE('',#95099);
#5310=PLANE('',#95101);
#5311=PLANE('',#95103);
#5312=PLANE('',#95105);
#5313=PLANE('',#95107);
#5314=PLANE('',#95109);
#5315=PLANE('',#95111);
#5316=PLANE('',#95113);
#5317=PLANE('',#95115);
#5318=PLANE('',#95117);
#5319=PLANE('',#95241);
#5320=PLANE('',#95242);
#5321=PLANE('',#95244);
#5322=PLANE('',#95247);
#5323=PLANE('',#95250);
#5324=PLANE('',#95265);
#5325=PLANE('',#95267);
#5326=PLANE('',#95269);
#5327=PLANE('',#95279);
#5328=PLANE('',#95285);
#5329=PLANE('',#95294);
#5330=PLANE('',#95298);
#5331=PLANE('',#95299);
#5332=PLANE('',#95300);
#5333=PLANE('',#95301);
#5334=PLANE('',#95302);
#5335=PLANE('',#95303);
#5336=PLANE('',#95304);
#5337=PLANE('',#95305);
#5338=PLANE('',#95306);
#5339=PLANE('',#95307);
#5340=PLANE('',#95308);
#5341=PLANE('',#95309);
#5342=PLANE('',#95310);
#5343=PLANE('',#95314);
#5344=PLANE('',#95315);
#5345=PLANE('',#95334);
#5346=PLANE('',#95335);
#5347=PLANE('',#95336);
#5348=PLANE('',#95337);
#5349=PLANE('',#95338);
#5350=PLANE('',#95339);
#5351=PLANE('',#95340);
#5352=PLANE('',#95379);
#5353=PLANE('',#95382);
#5354=PLANE('',#95383);
#5355=PLANE('',#95427);
#5356=PLANE('',#95443);
#5357=PLANE('',#95444);
#5358=PLANE('',#95483);
#5359=PLANE('',#95490);
#5360=PLANE('',#95525);
#5361=PLANE('',#95530);
#5362=PLANE('',#95533);
#5363=PLANE('',#95534);
#5364=PLANE('',#95580);
#5365=PLANE('',#95587);
#5366=PLANE('',#95590);
#5367=PLANE('',#95625);
#5368=PLANE('',#95630);
#5369=PLANE('',#95684);
#5370=PLANE('',#95698);
#5371=PLANE('',#95741);
#5372=PLANE('',#95772);
#5373=PLANE('',#95773);
#5374=PLANE('',#95791);
#5375=PLANE('',#95795);
#5376=PLANE('',#95799);
#5377=PLANE('',#95817);
#5378=PLANE('',#95836);
#5379=PLANE('',#95839);
#5380=PLANE('',#95840);
#5381=PLANE('',#95860);
#5382=PLANE('',#95865);
#5383=PLANE('',#95866);
#5384=PLANE('',#95877);
#5385=PLANE('',#95880);
#5386=PLANE('',#95894);
#5387=PLANE('',#95895);
#5388=PLANE('',#95899);
#5389=PLANE('',#95901);
#5390=PLANE('',#95915);
#5391=PLANE('',#95917);
#5392=PLANE('',#95918);
#5393=PLANE('',#95923);
#5394=PLANE('',#95925);
#5395=PLANE('',#95932);
#5396=PLANE('',#95935);
#5397=PLANE('',#95936);
#5398=PLANE('',#95938);
#5399=PLANE('',#95945);
#5400=PLANE('',#95951);
#5401=PLANE('',#95958);
#5402=PLANE('',#95966);
#5403=PLANE('',#95968);
#5404=PLANE('',#95973);
#5405=PLANE('',#95981);
#5406=PLANE('',#95993);
#5407=PLANE('',#95995);
#5408=PLANE('',#95997);
#5409=PLANE('',#95998);
#5410=PLANE('',#96002);
#5411=PLANE('',#96007);
#5412=PLANE('',#96012);
#5413=PLANE('',#96015);
#5414=PLANE('',#96016);
#5415=PLANE('',#96025);
#5416=PLANE('',#96031);
#5417=PLANE('',#96039);
#5418=PLANE('',#96041);
#5419=PLANE('',#96043);
#5420=PLANE('',#96044);
#5421=PLANE('',#96046);
#5422=PLANE('',#96047);
#5423=PLANE('',#96055);
#5424=PLANE('',#96071);
#5425=PLANE('',#96105);
#5426=PLANE('',#96134);
#5427=PLANE('',#96137);
#5428=PLANE('',#96157);
#5429=PLANE('',#96159);
#5430=PLANE('',#96165);
#5431=PLANE('',#96170);
#5432=PLANE('',#96176);
#5433=PLANE('',#96177);
#5434=PLANE('',#96195);
#5435=PLANE('',#96197);
#5436=PLANE('',#96200);
#5437=PLANE('',#96213);
#5438=PLANE('',#96238);
#5439=PLANE('',#96241);
#5440=PLANE('',#96244);
#5441=PLANE('',#96291);
#5442=PLANE('',#96294);
#5443=PLANE('',#96301);
#5444=PLANE('',#96343);
#5445=PLANE('',#96346);
#5446=PLANE('',#96347);
#5447=PLANE('',#96395);
#5448=PLANE('',#96396);
#5449=PLANE('',#96417);
#5450=PLANE('',#96422);
#5451=PLANE('',#96473);
#5452=PLANE('',#96476);
#5453=PLANE('',#96477);
#5454=PLANE('',#96512);
#5455=PLANE('',#96524);
#5456=PLANE('',#96553);
#5457=PLANE('',#96556);
#5458=PLANE('',#96565);
#5459=PLANE('',#96568);
#5460=PLANE('',#96578);
#5461=PLANE('',#96579);
#5462=PLANE('',#96594);
#5463=PLANE('',#96598);
#5464=PLANE('',#96605);
#5465=PLANE('',#96618);
#5466=PLANE('',#96621);
#5467=PLANE('',#96645);
#5468=PLANE('',#96652);
#5469=PLANE('',#96657);
#5470=PLANE('',#96660);
#5471=PLANE('',#96663);
#5472=PLANE('',#96667);
#5473=PLANE('',#96668);
#5474=PLANE('',#96672);
#5475=PLANE('',#96683);
#5476=PLANE('',#96687);
#5477=PLANE('',#96689);
#5478=PLANE('',#96693);
#5479=PLANE('',#96695);
#5480=PLANE('',#96696);
#5481=PLANE('',#96698);
#5482=PLANE('',#96699);
#5483=PLANE('',#96702);
#5484=PLANE('',#96704);
#5485=PLANE('',#96707);
#5486=PLANE('',#96714);
#5487=PLANE('',#96717);
#5488=PLANE('',#96723);
#5489=PLANE('',#96732);
#5490=PLANE('',#96734);
#5491=PLANE('',#96739);
#5492=PLANE('',#96744);
#5493=PLANE('',#96752);
#5494=PLANE('',#96753);
#5495=PLANE('',#96780);
#5496=PLANE('',#96810);
#5497=PLANE('',#96818);
#5498=PLANE('',#96829);
#5499=PLANE('',#96831);
#5500=PLANE('',#96838);
#5501=PLANE('',#96839);
#5502=PLANE('',#96848);
#5503=PLANE('',#96850);
#5504=PLANE('',#96861);
#5505=PLANE('',#96875);
#5506=PLANE('',#96879);
#5507=PLANE('',#96880);
#5508=PLANE('',#96916);
#5509=PLANE('',#96923);
#5510=PLANE('',#96930);
#5511=PLANE('',#96937);
#5512=PLANE('',#96944);
#5513=PLANE('',#96947);
#5514=PLANE('',#96951);
#5515=PLANE('',#96954);
#5516=PLANE('',#96957);
#5517=PLANE('',#96960);
#5518=PLANE('',#96968);
#5519=PLANE('',#96984);
#5520=PLANE('',#96988);
#5521=PLANE('',#96989);
#5522=PLANE('',#97008);
#5523=PLANE('',#97012);
#5524=PLANE('',#97013);
#5525=PLANE('',#97014);
#5526=PLANE('',#97018);
#5527=PLANE('',#97031);
#5528=PLANE('',#97036);
#5529=PLANE('',#97041);
#5530=PLANE('',#97047);
#5531=PLANE('',#97056);
#5532=PLANE('',#97062);
#5533=PLANE('',#97064);
#5534=PLANE('',#97068);
#5535=PLANE('',#97070);
#5536=PLANE('',#97071);
#5537=PLANE('',#97075);
#5538=PLANE('',#97076);
#5539=PLANE('',#97077);
#5540=PLANE('',#97081);
#5541=PLANE('',#97083);
#5542=PLANE('',#97085);
#5543=PLANE('',#97089);
#5544=PLANE('',#97090);
#5545=PLANE('',#97091);
#5546=PLANE('',#97092);
#5547=PLANE('',#97094);
#5548=PLANE('',#97095);
#5549=PLANE('',#97096);
#5550=PLANE('',#97103);
#5551=PLANE('',#97112);
#5552=PLANE('',#97113);
#5553=PLANE('',#97122);
#5554=PLANE('',#97123);
#5555=PLANE('',#97127);
#5556=PLANE('',#97130);
#5557=PLANE('',#97131);
#5558=PLANE('',#97134);
#5559=PLANE('',#97136);
#5560=PLANE('',#97137);
#5561=PLANE('',#97138);
#5562=PLANE('',#97139);
#5563=PLANE('',#97143);
#5564=PLANE('',#97144);
#5565=PLANE('',#97151);
#5566=PLANE('',#97152);
#5567=PLANE('',#97158);
#5568=PLANE('',#97161);
#5569=PLANE('',#97162);
#5570=PLANE('',#97165);
#5571=PLANE('',#97168);
#5572=PLANE('',#97170);
#5573=PLANE('',#97171);
#5574=PLANE('',#97177);
#5575=PLANE('',#97181);
#5576=PLANE('',#97189);
#5577=PLANE('',#97193);
#5578=PLANE('',#97199);
#5579=PLANE('',#97201);
#5580=PLANE('',#97204);
#5581=PLANE('',#97206);
#5582=PLANE('',#97209);
#5583=PLANE('',#97211);
#5584=PLANE('',#97212);
#5585=PLANE('',#97218);
#5586=PLANE('',#97219);
#5587=PLANE('',#97229);
#5588=PLANE('',#97232);
#5589=PLANE('',#97239);
#5590=PLANE('',#97242);
#5591=PLANE('',#97491);
#5592=PLANE('',#97492);
#5593=PLANE('',#97493);
#5594=PLANE('',#97922);
#5595=PLANE('',#98149);
#5596=PLANE('',#98366);
#5597=PLANE('',#98367);
#5598=PLANE('',#98368);
#5599=PLANE('',#98369);
#5600=PLANE('',#98370);
#5601=PLANE('',#98380);
#5602=PLANE('',#98386);
#5603=PLANE('',#98390);
#5604=PLANE('',#98396);
#5605=PLANE('',#98403);
#5606=PLANE('',#98430);
#5607=PLANE('',#98431);
#5608=PLANE('',#98688);
#5609=PLANE('',#98701);
#5610=PLANE('',#98708);
#5611=PLANE('',#98709);
#5612=PLANE('',#98710);
#5613=PLANE('',#98749);
#5614=PLANE('',#98752);
#5615=PLANE('',#98755);
#5616=PLANE('',#98758);
#5617=PLANE('',#98761);
#5618=PLANE('',#98764);
#5619=PLANE('',#98767);
#5620=PLANE('',#98770);
#5621=PLANE('',#98773);
#5622=PLANE('',#98776);
#5623=PLANE('',#98779);
#5624=PLANE('',#98782);
#5625=PLANE('',#98785);
#5626=PLANE('',#98788);
#5627=PLANE('',#98791);
#5628=PLANE('',#98794);
#5629=PLANE('',#98797);
#5630=PLANE('',#98800);
#5631=PLANE('',#98801);
#5632=PLANE('',#98819);
#5633=PLANE('',#98821);
#5634=PLANE('',#98823);
#5635=PLANE('',#98825);
#5636=PLANE('',#98826);
#5637=PLANE('',#98828);
#5638=PLANE('',#98829);
#5639=PLANE('',#98832);
#5640=PLANE('',#98834);
#5641=PLANE('',#98837);
#5642=PLANE('',#98838);
#5643=PLANE('',#98840);
#5644=PLANE('',#98841);
#5645=PLANE('',#98844);
#5646=PLANE('',#98846);
#5647=PLANE('',#98849);
#5648=PLANE('',#98850);
#5649=PLANE('',#98855);
#5650=PLANE('',#98861);
#5651=PLANE('',#98911);
#5652=PLANE('',#98915);
#5653=PLANE('',#98920);
#5654=PLANE('',#98923);
#5655=PLANE('',#98928);
#5656=PLANE('',#98931);
#5657=PLANE('',#98936);
#5658=PLANE('',#98939);
#5659=PLANE('',#98944);
#5660=PLANE('',#98947);
#5661=PLANE('',#98952);
#5662=PLANE('',#98955);
#5663=PLANE('',#98960);
#5664=PLANE('',#98963);
#5665=PLANE('',#98968);
#5666=PLANE('',#98971);
#5667=PLANE('',#98976);
#5668=PLANE('',#98984);
#5669=PLANE('',#98987);
#5670=PLANE('',#98993);
#5671=PLANE('',#98996);
#5672=PLANE('',#99002);
#5673=PLANE('',#99005);
#5674=PLANE('',#99011);
#5675=PLANE('',#99014);
#5676=PLANE('',#99020);
#5677=PLANE('',#99023);
#5678=PLANE('',#99029);
#5679=PLANE('',#99032);
#5680=PLANE('',#99038);
#5681=PLANE('',#99041);
#5682=PLANE('',#99047);
#5683=PLANE('',#99050);
#5684=PLANE('',#99132);
#5685=PLANE('',#99133);
#5686=PLANE('',#99134);
#5687=PLANE('',#99135);
#5688=PLANE('',#99146);
#5689=PLANE('',#99147);
#5690=PLANE('',#99148);
#5691=PLANE('',#99149);
#5692=PLANE('',#99150);
#5693=PLANE('',#99151);
#5694=PLANE('',#99152);
#5695=PLANE('',#99164);
#5696=PLANE('',#99167);
#5697=PLANE('',#99188);
#5698=PLANE('',#99189);
#5699=PLANE('',#99206);
#5700=PLANE('',#99207);
#5701=PLANE('',#99238);
#5702=PLANE('',#99239);
#5703=PLANE('',#99246);
#5704=PLANE('',#99247);
#5705=PLANE('',#99295);
#5706=PLANE('',#99296);
#5707=PLANE('',#99298);
#5708=PLANE('',#99299);
#5709=PLANE('',#99310);
#5710=PLANE('',#99311);
#5711=PLANE('',#99312);
#5712=PLANE('',#99313);
#5713=PLANE('',#99314);
#5714=PLANE('',#99315);
#5715=PLANE('',#99316);
#5716=PLANE('',#99364);
#5717=PLANE('',#99370);
#5718=PLANE('',#99376);
#5719=PLANE('',#99377);
#5720=PLANE('',#99378);
#5721=PLANE('',#99379);
#5722=PLANE('',#99380);
#5723=PLANE('',#99381);
#5724=PLANE('',#99382);
#5725=PLANE('',#99383);
#5726=PLANE('',#100367);
#5727=PLANE('',#100369);
#5728=PLANE('',#100371);
#5729=PLANE('',#100372);
#5730=PLANE('',#100373);
#5731=PLANE('',#100374);
#5732=PLANE('',#100375);
#5733=PLANE('',#100376);
#5734=PLANE('',#100385);
#5735=PLANE('',#100386);
#5736=PLANE('',#100387);
#5737=PLANE('',#100388);
#5738=PLANE('',#100389);
#5739=PLANE('',#100390);
#5740=PLANE('',#100391);
#5741=PLANE('',#100397);
#5742=PLANE('',#100398);
#5743=PLANE('',#100417);
#5744=PLANE('',#100419);
#5745=PLANE('',#100440);
#5746=PLANE('',#100442);
#5747=PLANE('',#100463);
#5748=PLANE('',#100465);
#5749=PLANE('',#100486);
#5750=PLANE('',#100488);
#5751=PLANE('',#100509);
#5752=PLANE('',#100511);
#5753=PLANE('',#100532);
#5754=PLANE('',#100534);
#5755=PLANE('',#100555);
#5756=PLANE('',#100557);
#5757=PLANE('',#100578);
#5758=PLANE('',#100580);
#5759=PLANE('',#100601);
#5760=PLANE('',#100603);
#5761=PLANE('',#100624);
#5762=PLANE('',#100626);
#5763=PLANE('',#100647);
#5764=PLANE('',#100649);
#5765=PLANE('',#100670);
#5766=PLANE('',#100672);
#5767=PLANE('',#100693);
#5768=PLANE('',#100695);
#5769=PLANE('',#100716);
#5770=PLANE('',#100718);
#5771=PLANE('',#100739);
#5772=PLANE('',#100741);
#5773=PLANE('',#100762);
#5774=PLANE('',#100764);
#5775=PLANE('',#100785);
#5776=PLANE('',#100787);
#5777=PLANE('',#100808);
#5778=PLANE('',#100810);
#5779=PLANE('',#100831);
#5780=PLANE('',#100833);
#5781=PLANE('',#100854);
#5782=PLANE('',#100856);
#5783=PLANE('',#100877);
#5784=PLANE('',#100879);
#5785=PLANE('',#100900);
#5786=PLANE('',#100902);
#5787=PLANE('',#100923);
#5788=PLANE('',#100925);
#5789=PLANE('',#100946);
#5790=PLANE('',#100948);
#5791=PLANE('',#100969);
#5792=PLANE('',#100971);
#5793=PLANE('',#100992);
#5794=PLANE('',#100994);
#5795=PLANE('',#101015);
#5796=PLANE('',#101017);
#5797=PLANE('',#101038);
#5798=PLANE('',#101040);
#5799=PLANE('',#101061);
#5800=PLANE('',#101063);
#5801=PLANE('',#101084);
#5802=PLANE('',#101086);
#5803=PLANE('',#101107);
#5804=PLANE('',#101109);
#5805=PLANE('',#101130);
#5806=PLANE('',#101132);
#5807=PLANE('',#101153);
#5808=PLANE('',#101155);
#5809=PLANE('',#101176);
#5810=PLANE('',#101178);
#5811=PLANE('',#101199);
#5812=PLANE('',#101201);
#5813=PLANE('',#101222);
#5814=PLANE('',#101224);
#5815=PLANE('',#101245);
#5816=PLANE('',#101247);
#5817=PLANE('',#101268);
#5818=PLANE('',#101270);
#5819=PLANE('',#101291);
#5820=PLANE('',#101293);
#5821=PLANE('',#101314);
#5822=PLANE('',#101316);
#5823=PLANE('',#101337);
#5824=PLANE('',#101339);
#5825=PLANE('',#101360);
#5826=PLANE('',#101362);
#5827=PLANE('',#101383);
#5828=PLANE('',#101385);
#5829=PLANE('',#101406);
#5830=PLANE('',#101408);
#5831=PLANE('',#101429);
#5832=PLANE('',#101431);
#5833=PLANE('',#101452);
#5834=PLANE('',#101454);
#5835=PLANE('',#101475);
#5836=PLANE('',#101477);
#5837=PLANE('',#101498);
#5838=PLANE('',#101500);
#5839=PLANE('',#101521);
#5840=PLANE('',#101523);
#5841=PLANE('',#101544);
#5842=PLANE('',#101546);
#5843=PLANE('',#101567);
#5844=PLANE('',#101569);
#5845=PLANE('',#101590);
#5846=PLANE('',#101592);
#5847=PLANE('',#101613);
#5848=PLANE('',#101615);
#5849=PLANE('',#101636);
#5850=PLANE('',#101638);
#5851=PLANE('',#101659);
#5852=PLANE('',#101661);
#5853=PLANE('',#101682);
#5854=PLANE('',#101684);
#5855=PLANE('',#101705);
#5856=PLANE('',#101707);
#5857=PLANE('',#101728);
#5858=PLANE('',#101730);
#5859=PLANE('',#101751);
#5860=PLANE('',#101753);
#5861=PLANE('',#101774);
#5862=PLANE('',#101776);
#5863=PLANE('',#101797);
#5864=PLANE('',#101799);
#5865=PLANE('',#101820);
#5866=PLANE('',#101822);
#5867=PLANE('',#101843);
#5868=PLANE('',#101845);
#5869=PLANE('',#101866);
#5870=PLANE('',#101868);
#5871=PLANE('',#101889);
#5872=PLANE('',#101891);
#5873=PLANE('',#101912);
#5874=PLANE('',#101914);
#5875=PLANE('',#101935);
#5876=PLANE('',#101937);
#5877=PLANE('',#101958);
#5878=PLANE('',#101960);
#5879=PLANE('',#101981);
#5880=PLANE('',#101983);
#5881=PLANE('',#102004);
#5882=PLANE('',#102006);
#5883=PLANE('',#102027);
#5884=PLANE('',#102029);
#5885=PLANE('',#102050);
#5886=PLANE('',#102052);
#5887=PLANE('',#102073);
#5888=PLANE('',#102075);
#5889=PLANE('',#102096);
#5890=PLANE('',#102098);
#5891=PLANE('',#102119);
#5892=PLANE('',#102121);
#5893=PLANE('',#102142);
#5894=PLANE('',#102144);
#5895=PLANE('',#102165);
#5896=PLANE('',#102167);
#5897=PLANE('',#102188);
#5898=PLANE('',#102190);
#5899=PLANE('',#102211);
#5900=PLANE('',#102213);
#5901=PLANE('',#102234);
#5902=PLANE('',#102236);
#5903=PLANE('',#102257);
#5904=PLANE('',#102259);
#5905=PLANE('',#102280);
#5906=PLANE('',#102282);
#5907=PLANE('',#102303);
#5908=PLANE('',#102305);
#5909=PLANE('',#102326);
#5910=PLANE('',#102328);
#5911=PLANE('',#102349);
#5912=PLANE('',#102351);
#5913=PLANE('',#102372);
#5914=PLANE('',#102374);
#5915=PLANE('',#102395);
#5916=PLANE('',#102397);
#5917=PLANE('',#102418);
#5918=PLANE('',#102420);
#5919=PLANE('',#102441);
#5920=PLANE('',#102443);
#5921=PLANE('',#102464);
#5922=PLANE('',#102466);
#5923=PLANE('',#102487);
#5924=PLANE('',#102489);
#5925=PLANE('',#102510);
#5926=PLANE('',#102512);
#5927=PLANE('',#102533);
#5928=PLANE('',#102535);
#5929=PLANE('',#102556);
#5930=PLANE('',#102558);
#5931=PLANE('',#102579);
#5932=PLANE('',#102581);
#5933=PLANE('',#102602);
#5934=PLANE('',#102604);
#5935=PLANE('',#102625);
#5936=PLANE('',#102627);
#5937=PLANE('',#103531);
#5938=PLANE('',#103533);
#5939=PLANE('',#103535);
#5940=PLANE('',#103536);
#5941=PLANE('',#103537);
#5942=PLANE('',#103538);
#5943=PLANE('',#103539);
#5944=PLANE('',#103540);
#5945=PLANE('',#103541);
#5946=PLANE('',#103550);
#5947=PLANE('',#103551);
#5948=PLANE('',#103552);
#5949=PLANE('',#103553);
#5950=PLANE('',#103554);
#5951=PLANE('',#103555);
#5952=PLANE('',#103556);
#5953=PLANE('',#103562);
#5954=PLANE('',#103578);
#5955=PLANE('',#103580);
#5956=PLANE('',#103599);
#5957=PLANE('',#103601);
#5958=PLANE('',#103620);
#5959=PLANE('',#103622);
#5960=PLANE('',#103641);
#5961=PLANE('',#103643);
#5962=PLANE('',#103662);
#5963=PLANE('',#103664);
#5964=PLANE('',#103683);
#5965=PLANE('',#103685);
#5966=PLANE('',#103704);
#5967=PLANE('',#103706);
#5968=PLANE('',#103725);
#5969=PLANE('',#103727);
#5970=PLANE('',#103746);
#5971=PLANE('',#103748);
#5972=PLANE('',#103767);
#5973=PLANE('',#103769);
#5974=PLANE('',#103788);
#5975=PLANE('',#103790);
#5976=PLANE('',#103809);
#5977=PLANE('',#103811);
#5978=PLANE('',#103830);
#5979=PLANE('',#103832);
#5980=PLANE('',#103851);
#5981=PLANE('',#103853);
#5982=PLANE('',#103872);
#5983=PLANE('',#103874);
#5984=PLANE('',#103893);
#5985=PLANE('',#103895);
#5986=PLANE('',#103914);
#5987=PLANE('',#103916);
#5988=PLANE('',#103935);
#5989=PLANE('',#103937);
#5990=PLANE('',#103956);
#5991=PLANE('',#103958);
#5992=PLANE('',#103977);
#5993=PLANE('',#103979);
#5994=PLANE('',#103998);
#5995=PLANE('',#104000);
#5996=PLANE('',#104019);
#5997=PLANE('',#104021);
#5998=PLANE('',#104040);
#5999=PLANE('',#104042);
#6000=PLANE('',#104061);
#6001=PLANE('',#104063);
#6002=PLANE('',#104082);
#6003=PLANE('',#104084);
#6004=PLANE('',#104103);
#6005=PLANE('',#104105);
#6006=PLANE('',#104124);
#6007=PLANE('',#104126);
#6008=PLANE('',#104145);
#6009=PLANE('',#104147);
#6010=PLANE('',#104166);
#6011=PLANE('',#104168);
#6012=PLANE('',#104187);
#6013=PLANE('',#104189);
#6014=PLANE('',#104208);
#6015=PLANE('',#104210);
#6016=PLANE('',#104229);
#6017=PLANE('',#104231);
#6018=PLANE('',#104250);
#6019=PLANE('',#104252);
#6020=PLANE('',#104271);
#6021=PLANE('',#104273);
#6022=PLANE('',#104292);
#6023=PLANE('',#104294);
#6024=PLANE('',#104313);
#6025=PLANE('',#104315);
#6026=PLANE('',#104334);
#6027=PLANE('',#104336);
#6028=PLANE('',#104355);
#6029=PLANE('',#104357);
#6030=PLANE('',#104376);
#6031=PLANE('',#104378);
#6032=PLANE('',#104397);
#6033=PLANE('',#104399);
#6034=PLANE('',#104418);
#6035=PLANE('',#104420);
#6036=PLANE('',#104439);
#6037=PLANE('',#104441);
#6038=PLANE('',#104460);
#6039=PLANE('',#104462);
#6040=PLANE('',#104481);
#6041=PLANE('',#104483);
#6042=PLANE('',#104502);
#6043=PLANE('',#104504);
#6044=PLANE('',#104523);
#6045=PLANE('',#104525);
#6046=PLANE('',#104544);
#6047=PLANE('',#104546);
#6048=PLANE('',#104565);
#6049=PLANE('',#104567);
#6050=PLANE('',#104586);
#6051=PLANE('',#104588);
#6052=PLANE('',#104607);
#6053=PLANE('',#104609);
#6054=PLANE('',#104628);
#6055=PLANE('',#104630);
#6056=PLANE('',#104649);
#6057=PLANE('',#104651);
#6058=PLANE('',#104670);
#6059=PLANE('',#104672);
#6060=PLANE('',#104691);
#6061=PLANE('',#104693);
#6062=PLANE('',#104712);
#6063=PLANE('',#104714);
#6064=PLANE('',#104733);
#6065=PLANE('',#104735);
#6066=PLANE('',#104754);
#6067=PLANE('',#104756);
#6068=PLANE('',#104775);
#6069=PLANE('',#104777);
#6070=PLANE('',#104796);
#6071=PLANE('',#104798);
#6072=PLANE('',#104817);
#6073=PLANE('',#104819);
#6074=PLANE('',#104838);
#6075=PLANE('',#104840);
#6076=PLANE('',#104859);
#6077=PLANE('',#104861);
#6078=PLANE('',#104880);
#6079=PLANE('',#104882);
#6080=PLANE('',#104901);
#6081=PLANE('',#104903);
#6082=PLANE('',#104922);
#6083=PLANE('',#104924);
#6084=PLANE('',#104943);
#6085=PLANE('',#104945);
#6086=PLANE('',#104964);
#6087=PLANE('',#104966);
#6088=PLANE('',#104985);
#6089=PLANE('',#104987);
#6090=PLANE('',#105006);
#6091=PLANE('',#105008);
#6092=PLANE('',#105027);
#6093=PLANE('',#105029);
#6094=PLANE('',#105048);
#6095=PLANE('',#105050);
#6096=PLANE('',#105069);
#6097=PLANE('',#105071);
#6098=PLANE('',#105090);
#6099=PLANE('',#105092);
#6100=PLANE('',#105111);
#6101=PLANE('',#105113);
#6102=PLANE('',#105132);
#6103=PLANE('',#105134);
#6104=PLANE('',#105153);
#6105=PLANE('',#105155);
#6106=PLANE('',#105266);
#6107=PLANE('',#105269);
#6108=PLANE('',#105337);
#6109=PLANE('',#105338);
#6110=PLANE('',#105339);
#6111=PLANE('',#105340);
#6112=PLANE('',#105341);
#6113=PLANE('',#105342);
#6114=PLANE('',#105343);
#6115=PLANE('',#105344);
#6116=PLANE('',#105345);
#6117=PLANE('',#105346);
#6118=PLANE('',#105347);
#6119=PLANE('',#105348);
#6120=PLANE('',#105349);
#6121=PLANE('',#105350);
#6122=PLANE('',#105351);
#6123=PLANE('',#105352);
#6124=PLANE('',#105353);
#6125=PLANE('',#105354);
#6126=PLANE('',#105355);
#6127=PLANE('',#105356);
#6128=PLANE('',#105401);
#6129=PLANE('',#105405);
#6130=PLANE('',#105427);
#6131=PLANE('',#105428);
#6132=PLANE('',#105429);
#6133=PLANE('',#105430);
#6134=PLANE('',#105432);
#6135=PLANE('',#105439);
#6136=PLANE('',#105455);
#6137=PLANE('',#105459);
#6138=PLANE('',#105462);
#6139=PLANE('',#105485);
#6140=PLANE('',#105486);
#6141=PLANE('',#105487);
#6142=PLANE('',#105488);
#6143=PLANE('',#105489);
#6144=PLANE('',#105490);
#6145=PLANE('',#105491);
#6146=PLANE('',#105492);
#6147=PLANE('',#105493);
#6148=PLANE('',#105513);
#6149=PLANE('',#105514);
#6150=PLANE('',#105515);
#6151=PLANE('',#105516);
#6152=PLANE('',#105517);
#6153=PLANE('',#105518);
#6154=PLANE('',#105519);
#6155=PLANE('',#105520);
#6156=PLANE('',#105521);
#6157=PLANE('',#105522);
#6158=PLANE('',#105523);
#6159=PLANE('',#105524);
#6160=PLANE('',#105525);
#6161=PLANE('',#105526);
#6162=PLANE('',#105527);
#6163=PLANE('',#105528);
#6164=PLANE('',#105529);
#6165=PLANE('',#105530);
#6166=PLANE('',#105531);
#6167=PLANE('',#105532);
#6168=PLANE('',#105533);
#6169=PLANE('',#105534);
#6170=PLANE('',#105535);
#6171=PLANE('',#105536);
#6172=PLANE('',#105537);
#6173=PLANE('',#105538);
#6174=PLANE('',#105539);
#6175=PLANE('',#105540);
#6176=PLANE('',#105541);
#6177=PLANE('',#105542);
#6178=PLANE('',#105543);
#6179=PLANE('',#105544);
#6180=PLANE('',#105545);
#6181=B_SPLINE_SURFACE_WITH_KNOTS('',3,3,((#136116,#136117,#136118,#136119,
#136120,#136121,#136122,#136123,#136124,#136125,#136126,#136127,#136128,
#136129,#136130,#136131,#136132,#136133,#136134,#136135,#136136,#136137,
#136138,#136139,#136140,#136141,#136142,#136143,#136144,#136145,#136146),
(#136147,#136148,#136149,#136150,#136151,#136152,#136153,#136154,#136155,
#136156,#136157,#136158,#136159,#136160,#136161,#136162,#136163,#136164,
#136165,#136166,#136167,#136168,#136169,#136170,#136171,#136172,#136173,
#136174,#136175,#136176,#136177),(#136178,#136179,#136180,#136181,#136182,
#136183,#136184,#136185,#136186,#136187,#136188,#136189,#136190,#136191,
#136192,#136193,#136194,#136195,#136196,#136197,#136198,#136199,#136200,
#136201,#136202,#136203,#136204,#136205,#136206,#136207,#136208),(#136209,
#136210,#136211,#136212,#136213,#136214,#136215,#136216,#136217,#136218,
#136219,#136220,#136221,#136222,#136223,#136224,#136225,#136226,#136227,
#136228,#136229,#136230,#136231,#136232,#136233,#136234,#136235,#136236,
#136237,#136238,#136239)),.UNSPECIFIED.,.F.,.F.,.F.,(4,4),(4,1,1,1,1,1,
1,1,1,1,1,1,1,1,1,1,1,1,1,1,1,1,1,1,1,1,1,1,4),(-0.000238175110720029,0.0327432610208062),
(11.8551230884687,12.8251224678821,13.7948836721847,14.7646448764874,15.7344060807901,
16.7041672850928,17.6739284893955,18.6436896936982,19.6134508980009,20.5832121023036,
21.5529733066062,22.5227345109089,23.4924957152116,24.4622569195143,25.432018123817,
26.4017793281197,27.3715405324224,28.3413017367251,29.3110629410278,30.2808241453304,
31.2505853496331,32.2203465539358,33.1901077582385,34.1598689625412,35.1296301668439,
36.0993913711466,37.0691525754493,38.038913779752,39.0090475285257),
 .UNSPECIFIED.);
#6182=B_SPLINE_SURFACE_WITH_KNOTS('',3,3,((#136336,#136337,#136338,#136339,
#136340,#136341,#136342,#136343,#136344,#136345,#136346,#136347,#136348,
#136349,#136350,#136351,#136352,#136353,#136354,#136355,#136356,#136357,
#136358,#136359,#136360,#136361,#136362,#136363,#136364,#136365,#136366),
(#136367,#136368,#136369,#136370,#136371,#136372,#136373,#136374,#136375,
#136376,#136377,#136378,#136379,#136380,#136381,#136382,#136383,#136384,
#136385,#136386,#136387,#136388,#136389,#136390,#136391,#136392,#136393,
#136394,#136395,#136396,#136397),(#136398,#136399,#136400,#136401,#136402,
#136403,#136404,#136405,#136406,#136407,#136408,#136409,#136410,#136411,
#136412,#136413,#136414,#136415,#136416,#136417,#136418,#136419,#136420,
#136421,#136422,#136423,#136424,#136425,#136426,#136427,#136428),(#136429,
#136430,#136431,#136432,#136433,#136434,#136435,#136436,#136437,#136438,
#136439,#136440,#136441,#136442,#136443,#136444,#136445,#136446,#136447,
#136448,#136449,#136450,#136451,#136452,#136453,#136454,#136455,#136456,
#136457,#136458,#136459)),.UNSPECIFIED.,.F.,.F.,.F.,(4,4),(4,1,1,1,1,1,
1,1,1,1,1,1,1,1,1,1,1,1,1,1,1,1,1,1,1,1,1,1,4),(-0.000593092618099697,0.0323402178569243),
(14.3981249632437,15.3681613312746,16.3379225355772,17.3076837398799,18.2774449441826,
19.2472061484853,20.216967352788,21.1867285570907,22.1564897613934,23.1262509656961,
24.0960121699988,25.0657733743014,26.0355345786041,27.0052957829068,27.9750569872095,
28.9448181915122,29.9145793958149,30.8843406001176,31.8541018044203,32.8238630087229,
33.7936242130256,34.7633854173283,35.733146621631,36.7029078259337,37.6726690302364,
38.6424302345391,39.6121914388418,40.5819526431444,41.5517138474471),
 .UNSPECIFIED.);
#6183=B_SPLINE_SURFACE_WITH_KNOTS('',3,3,((#136639,#136640,#136641,#136642,
#136643,#136644,#136645,#136646,#136647,#136648,#136649,#136650,#136651,
#136652,#136653,#136654,#136655,#136656,#136657,#136658,#136659,#136660,
#136661,#136662,#136663,#136664,#136665,#136666,#136667,#136668,#136669),
(#136670,#136671,#136672,#136673,#136674,#136675,#136676,#136677,#136678,
#136679,#136680,#136681,#136682,#136683,#136684,#136685,#136686,#136687,
#136688,#136689,#136690,#136691,#136692,#136693,#136694,#136695,#136696,
#136697,#136698,#136699,#136700),(#136701,#136702,#136703,#136704,#136705,
#136706,#136707,#136708,#136709,#136710,#136711,#136712,#136713,#136714,
#136715,#136716,#136717,#136718,#136719,#136720,#136721,#136722,#136723,
#136724,#136725,#136726,#136727,#136728,#136729,#136730,#136731),(#136732,
#136733,#136734,#136735,#136736,#136737,#136738,#136739,#136740,#136741,
#136742,#136743,#136744,#136745,#136746,#136747,#136748,#136749,#136750,
#136751,#136752,#136753,#136754,#136755,#136756,#136757,#136758,#136759,
#136760,#136761,#136762)),.UNSPECIFIED.,.F.,.F.,.F.,(4,4),(4,1,1,1,1,1,
1,1,1,1,1,1,1,1,1,1,1,1,1,1,1,1,1,1,1,1,1,1,4),(-0.000238191648974563,0.0327432700752779),
(11.8551230719304,12.825122467882,13.7948836721847,14.7646448764874,15.7344060807901,
16.7041672850928,17.6739284893955,18.6436896936982,19.6134508980009,20.5832121023035,
21.5529733066062,22.5227345109089,23.4924957152116,24.4622569195143,25.432018123817,
26.4017793281197,27.3715405324224,28.3413017367251,29.3110629410277,30.2808241453304,
31.2505853496331,32.2203465539358,33.1901077582385,34.1598689625412,35.1296301668439,
36.0993913711466,37.0691525754492,38.0389137797519,39.0090475313925),
 .UNSPECIFIED.);
#6184=B_SPLINE_SURFACE_WITH_KNOTS('',3,3,((#136859,#136860,#136861,#136862,
#136863,#136864,#136865,#136866,#136867,#136868,#136869,#136870,#136871,
#136872,#136873,#136874,#136875,#136876,#136877,#136878,#136879,#136880,
#136881,#136882,#136883,#136884,#136885,#136886,#136887,#136888,#136889),
(#136890,#136891,#136892,#136893,#136894,#136895,#136896,#136897,#136898,
#136899,#136900,#136901,#136902,#136903,#136904,#136905,#136906,#136907,
#136908,#136909,#136910,#136911,#136912,#136913,#136914,#136915,#136916,
#136917,#136918,#136919,#136920),(#136921,#136922,#136923,#136924,#136925,
#136926,#136927,#136928,#136929,#136930,#136931,#136932,#136933,#136934,
#136935,#136936,#136937,#136938,#136939,#136940,#136941,#136942,#136943,
#136944,#136945,#136946,#136947,#136948,#136949,#136950,#136951),(#136952,
#136953,#136954,#136955,#136956,#136957,#136958,#136959,#136960,#136961,
#136962,#136963,#136964,#136965,#136966,#136967,#136968,#136969,#136970,
#136971,#136972,#136973,#136974,#136975,#136976,#136977,#136978,#136979,
#136980,#136981,#136982)),.UNSPECIFIED.,.F.,.F.,.F.,(4,4),(4,1,1,1,1,1,
1,1,1,1,1,1,1,1,1,1,1,1,1,1,1,1,1,1,1,1,1,1,4),(-0.000593069084645025,0.0323402181589899),
(14.3981249570381,15.3681613312745,16.3379225355772,17.3076837398799,18.2774449441826,
19.2472061484853,20.216967352788,21.1867285570907,22.1564897613934,23.1262509656961,
24.0960121699987,25.0657733743014,26.0355345786041,27.0052957829068,27.9750569872095,
28.9448181915122,29.9145793958149,30.8843406001176,31.8541018044202,32.8238630087229,
33.7936242130256,34.7633854173283,35.733146621631,36.7029078259337,37.6726690302364,
38.6424302345391,39.6121914388417,40.5819526431444,41.5517138474471),
 .UNSPECIFIED.);
#6185=B_SPLINE_SURFACE_WITH_KNOTS('',3,1,((#137824,#137825),(#137826,#137827),
(#137828,#137829),(#137830,#137831),(#137832,#137833),(#137834,#137835)),
 .UNSPECIFIED.,.F.,.F.,.F.,(4,1,1,4),(2,2),(0.,0.285714285714286,0.571428571428571,
1.),(0.,0.576),.UNSPECIFIED.);
#6186=B_SPLINE_SURFACE_WITH_KNOTS('',3,1,((#137839,#137840),(#137841,#137842),
(#137843,#137844),(#137845,#137846),(#137847,#137848),(#137849,#137850)),
 .UNSPECIFIED.,.F.,.F.,.F.,(4,2,4),(2,2),(0.,0.483208689475554,1.),(0.,
0.576000000000006),.UNSPECIFIED.);
#6187=B_SPLINE_SURFACE_WITH_KNOTS('',3,1,((#137861,#137862),(#137863,#137864),
(#137865,#137866),(#137867,#137868),(#137869,#137870),(#137871,#137872)),
 .UNSPECIFIED.,.F.,.F.,.F.,(4,1,1,4),(2,2),(0.,0.285714285714286,0.571428571428571,
1.),(0.,0.576),.UNSPECIFIED.);
#6188=B_SPLINE_SURFACE_WITH_KNOTS('',3,1,((#137876,#137877),(#137878,#137879),
(#137880,#137881),(#137882,#137883),(#137884,#137885),(#137886,#137887)),
 .UNSPECIFIED.,.F.,.F.,.F.,(4,2,4),(2,2),(0.,0.483208689475554,1.),(0.,
0.576000000000006),.UNSPECIFIED.);
#6189=B_SPLINE_SURFACE_WITH_KNOTS('',3,1,((#137895,#137896),(#137897,#137898),
(#137899,#137900),(#137901,#137902),(#137903,#137904),(#137905,#137906)),
 .UNSPECIFIED.,.F.,.F.,.F.,(4,1,1,4),(2,2),(0.,0.285714285714286,0.571428571428571,
1.),(0.,0.576),.UNSPECIFIED.);
#6190=B_SPLINE_SURFACE_WITH_KNOTS('',3,1,((#137910,#137911),(#137912,#137913),
(#137914,#137915),(#137916,#137917),(#137918,#137919),(#137920,#137921)),
 .UNSPECIFIED.,.F.,.F.,.F.,(4,2,4),(2,2),(0.,0.483208689475554,1.),(0.,
0.576000000000006),.UNSPECIFIED.);
#6191=B_SPLINE_SURFACE_WITH_KNOTS('',3,1,((#137929,#137930),(#137931,#137932),
(#137933,#137934),(#137935,#137936),(#137937,#137938),(#137939,#137940)),
 .UNSPECIFIED.,.F.,.F.,.F.,(4,1,1,4),(2,2),(0.,0.285714285714286,0.571428571428571,
1.),(0.,0.576),.UNSPECIFIED.);
#6192=B_SPLINE_SURFACE_WITH_KNOTS('',3,1,((#137944,#137945),(#137946,#137947),
(#137948,#137949),(#137950,#137951),(#137952,#137953),(#137954,#137955)),
 .UNSPECIFIED.,.F.,.F.,.F.,(4,2,4),(2,2),(0.,0.483208689475554,1.),(0.,
0.576000000000006),.UNSPECIFIED.);
#6193=B_SPLINE_SURFACE_WITH_KNOTS('',3,1,((#137963,#137964),(#137965,#137966),
(#137967,#137968),(#137969,#137970),(#137971,#137972),(#137973,#137974)),
 .UNSPECIFIED.,.F.,.F.,.F.,(4,1,1,4),(2,2),(0.,0.285714285714286,0.571428571428571,
1.),(0.,0.576),.UNSPECIFIED.);
#6194=B_SPLINE_SURFACE_WITH_KNOTS('',3,1,((#137978,#137979),(#137980,#137981),
(#137982,#137983),(#137984,#137985),(#137986,#137987),(#137988,#137989)),
 .UNSPECIFIED.,.F.,.F.,.F.,(4,2,4),(2,2),(0.,0.483208689475554,1.),(0.,
0.576000000000006),.UNSPECIFIED.);
#6195=B_SPLINE_SURFACE_WITH_KNOTS('',3,1,((#137997,#137998),(#137999,#138000),
(#138001,#138002),(#138003,#138004),(#138005,#138006),(#138007,#138008)),
 .UNSPECIFIED.,.F.,.F.,.F.,(4,1,1,4),(2,2),(0.,0.285714285714286,0.571428571428571,
1.),(0.,0.576),.UNSPECIFIED.);
#6196=B_SPLINE_SURFACE_WITH_KNOTS('',3,1,((#138012,#138013),(#138014,#138015),
(#138016,#138017),(#138018,#138019),(#138020,#138021),(#138022,#138023)),
 .UNSPECIFIED.,.F.,.F.,.F.,(4,2,4),(2,2),(0.,0.483208689475554,1.),(0.,
0.576000000000006),.UNSPECIFIED.);
#6197=B_SPLINE_SURFACE_WITH_KNOTS('',3,1,((#138031,#138032),(#138033,#138034),
(#138035,#138036),(#138037,#138038),(#138039,#138040),(#138041,#138042)),
 .UNSPECIFIED.,.F.,.F.,.F.,(4,1,1,4),(2,2),(0.,0.285714285714286,0.571428571428571,
1.),(0.,0.576),.UNSPECIFIED.);
#6198=B_SPLINE_SURFACE_WITH_KNOTS('',3,1,((#138046,#138047),(#138048,#138049),
(#138050,#138051),(#138052,#138053),(#138054,#138055),(#138056,#138057)),
 .UNSPECIFIED.,.F.,.F.,.F.,(4,2,4),(2,2),(0.,0.483208689475554,1.),(0.,
0.576000000000006),.UNSPECIFIED.);
#6199=B_SPLINE_SURFACE_WITH_KNOTS('',3,1,((#138065,#138066),(#138067,#138068),
(#138069,#138070),(#138071,#138072),(#138073,#138074),(#138075,#138076)),
 .UNSPECIFIED.,.F.,.F.,.F.,(4,1,1,4),(2,2),(0.,0.285714285714286,0.571428571428571,
1.),(0.,0.576),.UNSPECIFIED.);
#6200=B_SPLINE_SURFACE_WITH_KNOTS('',3,1,((#138080,#138081),(#138082,#138083),
(#138084,#138085),(#138086,#138087),(#138088,#138089),(#138090,#138091)),
 .UNSPECIFIED.,.F.,.F.,.F.,(4,2,4),(2,2),(0.,0.483208689475554,1.),(0.,
0.576000000000006),.UNSPECIFIED.);
#6201=B_SPLINE_SURFACE_WITH_KNOTS('',3,1,((#138099,#138100),(#138101,#138102),
(#138103,#138104),(#138105,#138106),(#138107,#138108),(#138109,#138110)),
 .UNSPECIFIED.,.F.,.F.,.F.,(4,1,1,4),(2,2),(0.,0.285714285714286,0.571428571428571,
1.),(0.,0.576),.UNSPECIFIED.);
#6202=B_SPLINE_SURFACE_WITH_KNOTS('',3,1,((#138114,#138115),(#138116,#138117),
(#138118,#138119),(#138120,#138121),(#138122,#138123),(#138124,#138125)),
 .UNSPECIFIED.,.F.,.F.,.F.,(4,2,4),(2,2),(0.,0.483208689475554,1.),(0.,
0.576000000000006),.UNSPECIFIED.);
#6203=B_SPLINE_SURFACE_WITH_KNOTS('',3,1,((#138132,#138133),(#138134,#138135),
(#138136,#138137),(#138138,#138139),(#138140,#138141),(#138142,#138143)),
 .UNSPECIFIED.,.F.,.F.,.F.,(4,1,1,4),(2,2),(0.,0.285714285714286,0.571428571428571,
1.),(0.,0.576),.UNSPECIFIED.);
#6204=B_SPLINE_SURFACE_WITH_KNOTS('',3,1,((#138147,#138148),(#138149,#138150),
(#138151,#138152),(#138153,#138154),(#138155,#138156),(#138157,#138158)),
 .UNSPECIFIED.,.F.,.F.,.F.,(4,2,4),(2,2),(0.,0.483208689475554,1.),(0.,
0.576000000000006),.UNSPECIFIED.);
#6205=B_SPLINE_SURFACE_WITH_KNOTS('',3,3,((#140119,#140120,#140121,#140122,
#140123,#140124,#140125,#140126,#140127),(#140128,#140129,#140130,#140131,
#140132,#140133,#140134,#140135,#140136),(#140137,#140138,#140139,#140140,
#140141,#140142,#140143,#140144,#140145),(#140146,#140147,#140148,#140149,
#140150,#140151,#140152,#140153,#140154),(#140155,#140156,#140157,#140158,
#140159,#140160,#140161,#140162,#140163)),.UNSPECIFIED.,.F.,.F.,.F.,(4,
1,4),(4,1,1,1,1,1,4),(0.,0.571428571428571,1.),(0.461365642517441,0.594297668650691,
0.72722969478394,0.793695707850564,0.860161720917189,0.893394727450501,
0.926627733983813),.UNSPECIFIED.);
#6206=B_SPLINE_SURFACE_WITH_KNOTS('',3,3,((#140218,#140219,#140220,#140221,
#140222,#140223),(#140224,#140225,#140226,#140227,#140228,#140229),(#140230,
#140231,#140232,#140233,#140234,#140235),(#140236,#140237,#140238,#140239,
#140240,#140241)),.UNSPECIFIED.,.F.,.F.,.F.,(4,4),(4,1,1,4),(0.,1.),(8.11743420200643E-14,
0.0357756929344898,0.0596261548907622,0.0834766168470346),.UNSPECIFIED.);
#6207=B_SPLINE_SURFACE_WITH_KNOTS('',3,3,((#140256,#140257,#140258,#140259,
#140260,#140261,#140262),(#140263,#140264,#140265,#140266,#140267,#140268,
#140269),(#140270,#140271,#140272,#140273,#140274,#140275,#140276),(#140277,
#140278,#140279,#140280,#140281,#140282,#140283),(#140284,#140285,#140286,
#140287,#140288,#140289,#140290)),.UNSPECIFIED.,.F.,.F.,.F.,(4,1,4),(4,
1,1,1,4),(0.,0.571428571428571,1.),(0.,0.0576772753326012,0.115354550665202,
0.173031825997804,0.403740927328209),.UNSPECIFIED.);
#6208=B_SPLINE_SURFACE_WITH_KNOTS('',3,3,((#144750,#144751,#144752,#144753,
#144754),(#144755,#144756,#144757,#144758,#144759),(#144760,#144761,#144762,
#144763,#144764),(#144765,#144766,#144767,#144768,#144769),(#144770,#144771,
#144772,#144773,#144774)),.UNSPECIFIED.,.F.,.F.,.F.,(4,1,4),(4,1,4),(0.,
0.5,1.),(0.,0.0637546478056962,0.148760844879958),.UNSPECIFIED.);
#6209=B_SPLINE_SURFACE_WITH_KNOTS('',3,3,((#144837,#144838,#144839,#144840,
#144841,#144842,#144843,#144844,#144845,#144846,#144847,#144848,#144849),
(#144850,#144851,#144852,#144853,#144854,#144855,#144856,#144857,#144858,
#144859,#144860,#144861,#144862),(#144863,#144864,#144865,#144866,#144867,
#144868,#144869,#144870,#144871,#144872,#144873,#144874,#144875),(#144876,
#144877,#144878,#144879,#144880,#144881,#144882,#144883,#144884,#144885,
#144886,#144887,#144888),(#144889,#144890,#144891,#144892,#144893,#144894,
#144895,#144896,#144897,#144898,#144899,#144900,#144901)),.UNSPECIFIED.,
 .F.,.F.,.F.,(4,1,4),(4,1,1,1,1,1,1,1,1,1,4),(0.,0.5,1.),(-0.195457271730056,
-0.191966963306305,-0.188476654882554,-0.181496038035052,-0.167534804340048,
-0.13961233695004,-0.125651103255036,-0.111689869560032,-0.0837674021700239,
-0.0558449347800159,0.),.UNSPECIFIED.);
#6210=B_SPLINE_SURFACE_WITH_KNOTS('',3,3,((#145209,#145210,#145211,#145212),
(#145213,#145214,#145215,#145216),(#145217,#145218,#145219,#145220),(#145221,
#145222,#145223,#145224)),.UNSPECIFIED.,.F.,.F.,.F.,(4,4),(4,4),(0.,1.),
(-0.185221475089327,0.29949531162374),.UNSPECIFIED.);
#6211=B_SPLINE_SURFACE_WITH_KNOTS('',3,3,((#145225,#145226,#145227,#145228),
(#145229,#145230,#145231,#145232),(#145233,#145234,#145235,#145236),(#145237,
#145238,#145239,#145240)),.UNSPECIFIED.,.F.,.F.,.F.,(4,4),(4,4),(0.,1.),
(-0.35010463104534,0.22917017018593),.UNSPECIFIED.);
#6212=B_SPLINE_SURFACE_WITH_KNOTS('',3,3,((#145242,#145243,#145244,#145245,
#145246,#145247),(#145248,#145249,#145250,#145251,#145252,#145253),(#145254,
#145255,#145256,#145257,#145258,#145259),(#145260,#145261,#145262,#145263,
#145264,#145265)),.UNSPECIFIED.,.F.,.F.,.F.,(4,4),(4,1,1,4),(0.,1.),(-0.346299380282928,
-0.321815335614959,-0.312633818864471,-0.303452302113982),.UNSPECIFIED.);
#6213=B_SPLINE_SURFACE_WITH_KNOTS('',3,3,((#145274,#145275,#145276,#145277,
#145278),(#145279,#145280,#145281,#145282,#145283),(#145284,#145285,#145286,
#145287,#145288),(#145289,#145290,#145291,#145292,#145293)),
 .UNSPECIFIED.,.F.,.F.,.F.,(4,4),(4,1,4),(0.,1.),(-0.700638140826161,-0.192826413836344,
0.484255888816744),.UNSPECIFIED.);
#6214=B_SPLINE_SURFACE_WITH_KNOTS('',3,3,((#145297,#145298,#145299,#145300,
#145301),(#145302,#145303,#145304,#145305,#145306),(#145307,#145308,#145309,
#145310,#145311),(#145312,#145313,#145314,#145315,#145316)),
 .UNSPECIFIED.,.F.,.F.,.F.,(4,4),(4,1,4),(0.,1.),(-0.780128599420792,-0.0310350531663454,
0.53078510652449),.UNSPECIFIED.);
#6215=B_SPLINE_SURFACE_WITH_KNOTS('',5,1,((#153547,#153548),(#153549,#153550),
(#153551,#153552),(#153553,#153554),(#153555,#153556),(#153557,#153558),
(#153559,#153560),(#153561,#153562),(#153563,#153564),(#153565,#153566),
(#153567,#153568),(#153569,#153570),(#153571,#153572),(#153573,#153574),
(#153575,#153576),(#153577,#153578),(#153579,#153580),(#153581,#153582),
(#153583,#153584),(#153585,#153586),(#153587,#153588),(#153589,#153590),
(#153591,#153592),(#153593,#153594),(#153595,#153596),(#153597,#153598),
(#153599,#153600),(#153601,#153602),(#153603,#153604),(#153605,#153606),
(#153607,#153608),(#153609,#153610),(#153611,#153612),(#153613,#153614),
(#153615,#153616),(#153617,#153618),(#153619,#153620),(#153621,#153622),
(#153623,#153624),(#153625,#153626),(#153627,#153628),(#153629,#153630),
(#153631,#153632),(#153633,#153634),(#153635,#153636),(#153637,#153638),
(#153639,#153640),(#153641,#153642),(#153643,#153644),(#153645,#153646),
(#153647,#153648),(#153649,#153650),(#153651,#153652),(#153653,#153654),
(#153655,#153656),(#153657,#153658),(#153659,#153660),(#153661,#153662),
(#153663,#153664),(#153665,#153666),(#153667,#153668),(#153669,#153670),
(#153671,#153672),(#153673,#153674),(#153675,#153676),(#153677,#153678),
(#153679,#153680),(#153681,#153682),(#153683,#153684),(#153685,#153686),
(#153687,#153688),(#153689,#153690),(#153691,#153692),(#153693,#153694),
(#153695,#153696),(#153697,#153698),(#153699,#153700),(#153701,#153702),
(#153703,#153704),(#153705,#153706),(#153707,#153708),(#153709,#153710),
(#153711,#153712),(#153713,#153714),(#153715,#153716),(#153717,#153718),
(#153719,#153720),(#153721,#153722),(#153723,#153724),(#153725,#153726),
(#153727,#153728),(#153729,#153730),(#153731,#153732),(#153733,#153734),
(#153735,#153736),(#153737,#153738),(#153739,#153740),(#153741,#153742),
(#153743,#153744),(#153745,#153746),(#153747,#153748),(#153749,#153750),
(#153751,#153752),(#153753,#153754),(#153755,#153756),(#153757,#153758),
(#153759,#153760),(#153761,#153762),(#153763,#153764),(#153765,#153766),
(#153767,#153768),(#153769,#153770),(#153771,#153772),(#153773,#153774),
(#153775,#153776),(#153777,#153778),(#153779,#153780),(#153781,#153782),
(#153783,#153784),(#153785,#153786),(#153787,#153788),(#153789,#153790),
(#153791,#153792),(#153793,#153794),(#153795,#153796),(#153797,#153798),
(#153799,#153800),(#153801,#153802),(#153803,#153804),(#153805,#153806),
(#153807,#153808),(#153809,#153810),(#153811,#153812),(#153813,#153814),
(#153815,#153816),(#153817,#153818),(#153819,#153820),(#153821,#153822),
(#153823,#153824),(#153825,#153826),(#153827,#153828),(#153829,#153830),
(#153831,#153832),(#153833,#153834),(#153835,#153836),(#153837,#153838),
(#153839,#153840),(#153841,#153842),(#153843,#153844),(#153845,#153846),
(#153847,#153848),(#153849,#153850),(#153851,#153852),(#153853,#153854),
(#153855,#153856),(#153857,#153858),(#153859,#153860),(#153861,#153862),
(#153863,#153864),(#153865,#153866),(#153867,#153868),(#153869,#153870),
(#153871,#153872),(#153873,#153874),(#153875,#153876),(#153877,#153878),
(#153879,#153880),(#153881,#153882),(#153883,#153884),(#153885,#153886),
(#153887,#153888),(#153889,#153890),(#153891,#153892),(#153893,#153894),
(#153895,#153896),(#153897,#153898),(#153899,#153900),(#153901,#153902),
(#153903,#153904),(#153905,#153906),(#153907,#153908),(#153909,#153910),
(#153911,#153912),(#153913,#153914),(#153915,#153916),(#153917,#153918),
(#153919,#153920),(#153921,#153922),(#153923,#153924),(#153925,#153926),
(#153927,#153928),(#153929,#153930),(#153931,#153932),(#153933,#153934),
(#153935,#153936),(#153937,#153938),(#153939,#153940),(#153941,#153942),
(#153943,#153944),(#153945,#153946),(#153947,#153948),(#153949,#153950),
(#153951,#153952),(#153953,#153954),(#153955,#153956),(#153957,#153958),
(#153959,#153960),(#153961,#153962),(#153963,#153964),(#153965,#153966),
(#153967,#153968),(#153969,#153970),(#153971,#153972),(#153973,#153974),
(#153975,#153976),(#153977,#153978),(#153979,#153980),(#153981,#153982),
(#153983,#153984),(#153985,#153986),(#153987,#153988),(#153989,#153990),
(#153991,#153992),(#153993,#153994),(#153995,#153996),(#153997,#153998),
(#153999,#154000),(#154001,#154002),(#154003,#154004),(#154005,#154006),
(#154007,#154008),(#154009,#154010),(#154011,#154012),(#154013,#154014),
(#154015,#154016),(#154017,#154018),(#154019,#154020),(#154021,#154022),
(#154023,#154024),(#154025,#154026),(#154027,#154028),(#154029,#154030),
(#154031,#154032),(#154033,#154034),(#154035,#154036),(#154037,#154038),
(#154039,#154040),(#154041,#154042),(#154043,#154044),(#154045,#154046),
(#154047,#154048),(#154049,#154050),(#154051,#154052),(#154053,#154054),
(#154055,#154056),(#154057,#154058),(#154059,#154060),(#154061,#154062),
(#154063,#154064),(#154065,#154066),(#154067,#154068),(#154069,#154070),
(#154071,#154072),(#154073,#154074),(#154075,#154076),(#154077,#154078),
(#154079,#154080),(#154081,#154082),(#154083,#154084),(#154085,#154086),
(#154087,#154088),(#154089,#154090),(#154091,#154092),(#154093,#154094),
(#154095,#154096),(#154097,#154098),(#154099,#154100),(#154101,#154102),
(#154103,#154104),(#154105,#154106),(#154107,#154108),(#154109,#154110),
(#154111,#154112),(#154113,#154114),(#154115,#154116),(#154117,#154118),
(#154119,#154120),(#154121,#154122),(#154123,#154124),(#154125,#154126),
(#154127,#154128),(#154129,#154130),(#154131,#154132),(#154133,#154134),
(#154135,#154136),(#154137,#154138),(#154139,#154140),(#154141,#154142),
(#154143,#154144),(#154145,#154146),(#154147,#154148),(#154149,#154150),
(#154151,#154152),(#154153,#154154),(#154155,#154156),(#154157,#154158),
(#154159,#154160),(#154161,#154162),(#154163,#154164),(#154165,#154166),
(#154167,#154168),(#154169,#154170),(#154171,#154172),(#154173,#154174),
(#154175,#154176),(#154177,#154178),(#154179,#154180),(#154181,#154182),
(#154183,#154184),(#154185,#154186),(#154187,#154188),(#154189,#154190),
(#154191,#154192),(#154193,#154194),(#154195,#154196),(#154197,#154198),
(#154199,#154200),(#154201,#154202),(#154203,#154204),(#154205,#154206),
(#154207,#154208),(#154209,#154210),(#154211,#154212),(#154213,#154214),
(#154215,#154216),(#154217,#154218),(#154219,#154220),(#154221,#154222),
(#154223,#154224),(#154225,#154226),(#154227,#154228),(#154229,#154230),
(#154231,#154232),(#154233,#154234),(#154235,#154236),(#154237,#154238),
(#154239,#154240),(#154241,#154242),(#154243,#154244),(#154245,#154246),
(#154247,#154248),(#154249,#154250),(#154251,#154252),(#154253,#154254),
(#154255,#154256),(#154257,#154258),(#154259,#154260),(#154261,#154262),
(#154263,#154264),(#154265,#154266),(#154267,#154268),(#154269,#154270),
(#154271,#154272),(#154273,#154274),(#154275,#154276),(#154277,#154278),
(#154279,#154280),(#154281,#154282),(#154283,#154284),(#154285,#154286),
(#154287,#154288),(#154289,#154290),(#154291,#154292),(#154293,#154294),
(#154295,#154296),(#154297,#154298),(#154299,#154300),(#154301,#154302),
(#154303,#154304),(#154305,#154306),(#154307,#154308),(#154309,#154310),
(#154311,#154312),(#154313,#154314),(#154315,#154316),(#154317,#154318),
(#154319,#154320),(#154321,#154322),(#154323,#154324),(#154325,#154326),
(#154327,#154328),(#154329,#154330),(#154331,#154332),(#154333,#154334),
(#154335,#154336),(#154337,#154338),(#154339,#154340),(#154341,#154342),
(#154343,#154344),(#154345,#154346),(#154347,#154348),(#154349,#154350),
(#154351,#154352),(#154353,#154354),(#154355,#154356),(#154357,#154358),
(#154359,#154360),(#154361,#154362),(#154363,#154364),(#154365,#154366),
(#154367,#154368),(#154369,#154370),(#154371,#154372),(#154373,#154374),
(#154375,#154376),(#154377,#154378),(#154379,#154380),(#154381,#154382),
(#154383,#154384),(#154385,#154386),(#154387,#154388),(#154389,#154390),
(#154391,#154392),(#154393,#154394),(#154395,#154396),(#154397,#154398),
(#154399,#154400),(#154401,#154402),(#154403,#154404),(#154405,#154406),
(#154407,#154408),(#154409,#154410),(#154411,#154412),(#154413,#154414),
(#154415,#154416),(#154417,#154418),(#154419,#154420),(#154421,#154422),
(#154423,#154424),(#154425,#154426),(#154427,#154428),(#154429,#154430),
(#154431,#154432),(#154433,#154434),(#154435,#154436),(#154437,#154438),
(#154439,#154440),(#154441,#154442),(#154443,#154444),(#154445,#154446),
(#154447,#154448),(#154449,#154450),(#154451,#154452),(#154453,#154454),
(#154455,#154456),(#154457,#154458),(#154459,#154460),(#154461,#154462),
(#154463,#154464),(#154465,#154466),(#154467,#154468),(#154469,#154470),
(#154471,#154472),(#154473,#154474),(#154475,#154476),(#154477,#154478),
(#154479,#154480),(#154481,#154482),(#154483,#154484),(#154485,#154486),
(#154487,#154488),(#154489,#154490)),.UNSPECIFIED.,.F.,.F.,.F.,(6,1,1,1,
1,1,1,1,1,1,1,1,1,1,1,1,1,1,1,1,1,1,1,1,1,1,1,1,1,1,1,1,1,1,1,1,1,1,1,1,
1,1,1,1,1,1,1,1,1,1,1,1,1,1,1,1,1,1,1,1,1,1,1,1,1,1,1,1,1,1,1,1,1,1,1,1,
1,1,1,1,1,1,1,1,1,1,1,1,1,1,1,1,1,1,1,1,1,1,1,1,1,1,1,1,1,1,1,1,1,1,1,1,
1,1,1,1,1,1,1,1,1,1,1,1,1,1,1,1,1,1,1,1,1,1,1,1,1,1,1,1,1,1,1,1,1,1,1,1,
1,1,1,1,1,1,1,1,1,1,1,1,1,1,1,1,1,1,1,1,1,1,1,1,1,1,1,1,1,1,1,1,1,1,1,1,
1,1,1,1,1,1,1,1,1,1,1,1,1,1,1,1,1,1,1,1,1,1,1,1,1,1,1,1,1,1,1,1,1,1,1,1,
1,1,1,1,1,1,1,1,1,1,1,1,1,1,1,1,1,1,1,1,1,1,1,1,1,1,1,1,1,1,1,1,1,1,1,1,
1,1,1,1,1,1,1,1,1,1,1,1,1,1,1,1,1,1,1,1,1,1,1,1,1,1,1,1,1,1,1,1,1,1,1,1,
1,1,1,1,1,1,1,1,1,1,1,1,1,1,1,1,1,1,1,1,1,1,1,1,1,1,1,1,1,1,1,1,1,1,1,1,
1,1,1,1,1,1,1,1,1,1,1,1,1,1,1,1,1,1,1,1,1,1,1,1,1,1,1,1,1,1,1,1,1,1,1,1,
1,1,1,1,1,1,1,1,1,1,1,1,1,1,1,1,1,1,1,1,1,1,1,1,1,1,1,1,1,1,1,1,1,1,1,1,
1,1,1,1,1,1,1,1,1,1,1,1,1,1,1,1,1,1,1,1,1,1,1,1,1,1,1,1,1,1,1,1,1,1,1,1,
1,1,1,1,1,1,1,1,1,1,1,1,1,1,1,1,1,1,1,1,1,1,1,1,1,1,1,1,1,1,1,6),(2,2),
(0.143172103,0.144954128,0.146788991,0.148623853,0.150458716,0.152293578,
0.15412844,0.155963303,0.157798165,0.159633028,0.16146789,0.163302752,0.165137615,
0.166972477,0.168807339,0.170642202,0.172477064,0.174311927,0.176146789,
0.177981651,0.179816514,0.181651376,0.183486239,0.185321101,0.187155963,
0.188990826,0.190825688,0.19266055,0.194495413,0.196330275,0.198165138,
0.2,0.201834862,0.203669725,0.205504587,0.20733945,0.209174312,0.211009174,
0.212844037,0.214678899,0.216513761,0.218348624,0.220183486,0.222018349,
0.223853211,0.225688073,0.227522936,0.229357798,0.231192661,0.233027523,
0.234862385,0.236697248,0.23853211,0.240366972,0.242201835,0.244036697,
0.24587156,0.247706422,0.249541284,0.251376147,0.253211009,0.255045872,
0.256880734,0.258715596,0.260550459,0.262385321,0.264220183,0.266055046,
0.267889908,0.269724771,0.271559633,0.273394495,0.275229358,0.27706422,
0.278899083,0.280733945,0.282568807,0.28440367,0.286238532,0.288073394,
0.289908257,0.291743119,0.293577982,0.295412844,0.297247706,0.299082569,
0.300917431,0.302752294,0.304587156,0.306422018,0.308256881,0.310091743,
0.311926606,0.313761468,0.31559633,0.317431193,0.319266055,0.321100917,
0.32293578,0.324770642,0.326605505,0.328440367,0.330275229,0.332110092,
0.333944954,0.335779817,0.337614679,0.339449541,0.341284404,0.343119266,
0.344954128,0.346788991,0.348623853,0.350458716,0.352293578,0.35412844,
0.355963303,0.357798165,0.359633028,0.36146789,0.363302752,0.365137615,
0.366972477,0.368807339,0.370642202,0.372477064,0.374311927,0.376146789,
0.377981651,0.379816514,0.381651376,0.383486239,0.385321101,0.387155963,
0.388990826,0.390825688,0.39266055,0.394495413,0.396330275,0.398165138,
0.4,0.401834862,0.403669725,0.405504587,0.40733945,0.409174312,0.411009174,
0.412844037,0.414678899,0.416513761,0.418348624,0.420183486,0.422018349,
0.423853211,0.425688073,0.427522936,0.429357798,0.431192661,0.433027523,
0.434862385,0.436697248,0.43853211,0.440366972,0.442201835,0.444036697,
0.44587156,0.447706422,0.449541284,0.451376147,0.453211009,0.455045872,
0.456880734,0.458715596,0.460550459,0.462385321,0.464220183,0.466055046,
0.467889908,0.469724771,0.471559633,0.473394495,0.475229358,0.47706422,
0.478899083,0.480733945,0.482568807,0.48440367,0.486238532,0.488073394,
0.489908257,0.491743119,0.493577982,0.495412844,0.497247706,0.499082569,
0.500917431,0.502752294,0.504587156,0.506422018,0.508256881,0.510091743,
0.511926606,0.513761468,0.51559633,0.517431193,0.519266055,0.521100917,
0.52293578,0.524770642,0.526605505,0.528440367,0.530275229,0.532110092,
0.533944954,0.535779817,0.537614679,0.539449541,0.541284404,0.543119266,
0.544954128,0.546788991,0.548623853,0.550458716,0.552293578,0.55412844,
0.555963303,0.557798165,0.559633028,0.56146789,0.563302752,0.565137615,
0.566972477,0.568807339,0.570642202,0.572477064,0.574311927,0.576146789,
0.577981651,0.579816514,0.581651376,0.583486239,0.585321101,0.587155963,
0.588990826,0.590825688,0.59266055,0.594495413,0.596330275,0.598165138,
0.6,0.601834862,0.603669725,0.605504587,0.60733945,0.609174312,0.611009174,
0.612844037,0.614678899,0.616513761,0.618348624,0.620183486,0.622018349,
0.623853211,0.625688073,0.627522936,0.629357798,0.631192661,0.633027523,
0.634862385,0.636697248,0.63853211,0.640366972,0.642201835,0.644036697,
0.64587156,0.647706422,0.649541284,0.651376147,0.653211009,0.655045872,
0.656880734,0.658715596,0.660550459,0.662385321,0.664220183,0.666055046,
0.667889908,0.669724771,0.671559633,0.673394495,0.675229358,0.67706422,
0.678899083,0.680733945,0.682568807,0.68440367,0.686238532,0.688073394,
0.689908257,0.691743119,0.693577982,0.695412844,0.697247706,0.699082569,
0.700917431,0.702752294,0.704587156,0.706422018,0.708256881,0.710091743,
0.711926606,0.713761468,0.71559633,0.717431193,0.719266055,0.721100917,
0.72293578,0.724770642,0.726605505,0.728440367,0.730275229,0.732110092,
0.733944954,0.735779817,0.737614679,0.739449541,0.741284404,0.743119266,
0.744954128,0.746788991,0.748623853,0.750458716,0.752293578,0.75412844,
0.755963303,0.757798165,0.759633028,0.76146789,0.763302752,0.765137615,
0.766972477,0.768807339,0.770642202,0.772477064,0.774311927,0.776146789,
0.777981651,0.779816514,0.781651376,0.783486239,0.785321101,0.787155963,
0.788990826,0.790825688,0.79266055,0.794495413,0.796330275,0.798165138,
0.8,0.801834862,0.803669725,0.805504587,0.80733945,0.809174312,0.811009174,
0.812844037,0.814678899,0.816513761,0.818348624,0.820183486,0.822018349,
0.823853211,0.825688073,0.827522936,0.829357798,0.831192661,0.833027523,
0.834862385,0.836697248,0.83853211,0.840366972,0.842201835,0.844036697,
0.84587156,0.847706422,0.849541284,0.851376147,0.853211009,0.855045872,
0.856880734,0.858715596,0.860550459,0.862385321,0.864220183,0.866055046,
0.867889908,0.869724771,0.871559633,0.873394495,0.875229358,0.87706422,
0.878899083,0.880733945,0.882568807,0.88440367,0.886238532,0.888073394,
0.889908257,0.891743119,0.893577982,0.895412844,0.897247706,0.899082569,
0.900917431,0.902752294,0.904587156,0.906422018,0.908256881,0.910091743,
0.911926606,0.913761468,0.91559633,0.917431193,0.919266055,0.921100917,
0.92293578,0.924770642,0.926605505,0.928440367,0.930275229,0.932110092,
0.933944954,0.935779817,0.937614679,0.939449541,0.941284404,0.943119266,
0.944954128,0.946788991,0.948623853,0.950458716,0.952293578,0.95412844,
0.955963303,0.957798165,0.959633028,0.96146789,0.963302752,0.965137615,
0.966972477,0.968807339,0.970642202,0.972477064,0.974311927,0.976146789,
0.977981651,0.979816514,0.981651376,0.983486239,0.985321101,0.987155963,
0.988990826,0.990825688,0.99266055,0.994495413,0.996330275,0.998165138,
1.),(0.,0.36),.UNSPECIFIED.);
#6216=B_SPLINE_SURFACE_WITH_KNOTS('',5,1,((#155436,#155437),(#155438,#155439),
(#155440,#155441),(#155442,#155443),(#155444,#155445),(#155446,#155447),
(#155448,#155449),(#155450,#155451),(#155452,#155453),(#155454,#155455),
(#155456,#155457),(#155458,#155459),(#155460,#155461),(#155462,#155463),
(#155464,#155465),(#155466,#155467),(#155468,#155469),(#155470,#155471),
(#155472,#155473),(#155474,#155475),(#155476,#155477),(#155478,#155479),
(#155480,#155481),(#155482,#155483),(#155484,#155485),(#155486,#155487),
(#155488,#155489),(#155490,#155491),(#155492,#155493),(#155494,#155495),
(#155496,#155497),(#155498,#155499),(#155500,#155501),(#155502,#155503),
(#155504,#155505),(#155506,#155507),(#155508,#155509),(#155510,#155511),
(#155512,#155513),(#155514,#155515),(#155516,#155517),(#155518,#155519),
(#155520,#155521),(#155522,#155523),(#155524,#155525),(#155526,#155527),
(#155528,#155529),(#155530,#155531),(#155532,#155533),(#155534,#155535),
(#155536,#155537),(#155538,#155539),(#155540,#155541),(#155542,#155543),
(#155544,#155545),(#155546,#155547),(#155548,#155549),(#155550,#155551),
(#155552,#155553),(#155554,#155555),(#155556,#155557),(#155558,#155559),
(#155560,#155561),(#155562,#155563),(#155564,#155565),(#155566,#155567),
(#155568,#155569),(#155570,#155571),(#155572,#155573),(#155574,#155575),
(#155576,#155577),(#155578,#155579),(#155580,#155581),(#155582,#155583),
(#155584,#155585),(#155586,#155587),(#155588,#155589),(#155590,#155591),
(#155592,#155593),(#155594,#155595),(#155596,#155597),(#155598,#155599),
(#155600,#155601),(#155602,#155603),(#155604,#155605),(#155606,#155607),
(#155608,#155609),(#155610,#155611),(#155612,#155613),(#155614,#155615),
(#155616,#155617),(#155618,#155619),(#155620,#155621),(#155622,#155623),
(#155624,#155625),(#155626,#155627),(#155628,#155629),(#155630,#155631),
(#155632,#155633),(#155634,#155635),(#155636,#155637),(#155638,#155639),
(#155640,#155641),(#155642,#155643),(#155644,#155645),(#155646,#155647),
(#155648,#155649),(#155650,#155651),(#155652,#155653),(#155654,#155655),
(#155656,#155657),(#155658,#155659),(#155660,#155661),(#155662,#155663),
(#155664,#155665),(#155666,#155667),(#155668,#155669),(#155670,#155671),
(#155672,#155673),(#155674,#155675),(#155676,#155677),(#155678,#155679),
(#155680,#155681),(#155682,#155683),(#155684,#155685),(#155686,#155687),
(#155688,#155689),(#155690,#155691),(#155692,#155693),(#155694,#155695),
(#155696,#155697),(#155698,#155699),(#155700,#155701),(#155702,#155703),
(#155704,#155705),(#155706,#155707),(#155708,#155709),(#155710,#155711),
(#155712,#155713),(#155714,#155715),(#155716,#155717),(#155718,#155719),
(#155720,#155721),(#155722,#155723),(#155724,#155725),(#155726,#155727),
(#155728,#155729),(#155730,#155731),(#155732,#155733),(#155734,#155735),
(#155736,#155737),(#155738,#155739),(#155740,#155741),(#155742,#155743),
(#155744,#155745),(#155746,#155747),(#155748,#155749),(#155750,#155751),
(#155752,#155753),(#155754,#155755),(#155756,#155757),(#155758,#155759),
(#155760,#155761),(#155762,#155763),(#155764,#155765),(#155766,#155767),
(#155768,#155769),(#155770,#155771),(#155772,#155773),(#155774,#155775),
(#155776,#155777),(#155778,#155779),(#155780,#155781),(#155782,#155783),
(#155784,#155785),(#155786,#155787),(#155788,#155789),(#155790,#155791),
(#155792,#155793),(#155794,#155795),(#155796,#155797),(#155798,#155799),
(#155800,#155801),(#155802,#155803),(#155804,#155805),(#155806,#155807),
(#155808,#155809),(#155810,#155811),(#155812,#155813),(#155814,#155815),
(#155816,#155817),(#155818,#155819),(#155820,#155821),(#155822,#155823),
(#155824,#155825),(#155826,#155827),(#155828,#155829),(#155830,#155831),
(#155832,#155833),(#155834,#155835),(#155836,#155837),(#155838,#155839),
(#155840,#155841),(#155842,#155843),(#155844,#155845),(#155846,#155847),
(#155848,#155849),(#155850,#155851),(#155852,#155853),(#155854,#155855),
(#155856,#155857),(#155858,#155859),(#155860,#155861),(#155862,#155863),
(#155864,#155865),(#155866,#155867),(#155868,#155869),(#155870,#155871),
(#155872,#155873),(#155874,#155875),(#155876,#155877),(#155878,#155879),
(#155880,#155881),(#155882,#155883),(#155884,#155885),(#155886,#155887),
(#155888,#155889),(#155890,#155891),(#155892,#155893),(#155894,#155895),
(#155896,#155897),(#155898,#155899),(#155900,#155901),(#155902,#155903),
(#155904,#155905),(#155906,#155907),(#155908,#155909),(#155910,#155911),
(#155912,#155913),(#155914,#155915),(#155916,#155917),(#155918,#155919),
(#155920,#155921),(#155922,#155923),(#155924,#155925),(#155926,#155927),
(#155928,#155929),(#155930,#155931),(#155932,#155933),(#155934,#155935),
(#155936,#155937),(#155938,#155939),(#155940,#155941),(#155942,#155943),
(#155944,#155945),(#155946,#155947),(#155948,#155949),(#155950,#155951),
(#155952,#155953),(#155954,#155955),(#155956,#155957),(#155958,#155959),
(#155960,#155961),(#155962,#155963),(#155964,#155965),(#155966,#155967),
(#155968,#155969),(#155970,#155971),(#155972,#155973),(#155974,#155975),
(#155976,#155977),(#155978,#155979),(#155980,#155981),(#155982,#155983),
(#155984,#155985),(#155986,#155987),(#155988,#155989),(#155990,#155991),
(#155992,#155993),(#155994,#155995),(#155996,#155997),(#155998,#155999),
(#156000,#156001),(#156002,#156003),(#156004,#156005),(#156006,#156007),
(#156008,#156009),(#156010,#156011),(#156012,#156013),(#156014,#156015),
(#156016,#156017),(#156018,#156019),(#156020,#156021),(#156022,#156023),
(#156024,#156025),(#156026,#156027),(#156028,#156029),(#156030,#156031),
(#156032,#156033),(#156034,#156035),(#156036,#156037),(#156038,#156039),
(#156040,#156041),(#156042,#156043),(#156044,#156045),(#156046,#156047),
(#156048,#156049),(#156050,#156051),(#156052,#156053),(#156054,#156055),
(#156056,#156057),(#156058,#156059),(#156060,#156061),(#156062,#156063),
(#156064,#156065),(#156066,#156067),(#156068,#156069),(#156070,#156071),
(#156072,#156073),(#156074,#156075),(#156076,#156077),(#156078,#156079),
(#156080,#156081),(#156082,#156083),(#156084,#156085),(#156086,#156087),
(#156088,#156089),(#156090,#156091),(#156092,#156093),(#156094,#156095),
(#156096,#156097),(#156098,#156099),(#156100,#156101),(#156102,#156103),
(#156104,#156105),(#156106,#156107),(#156108,#156109),(#156110,#156111),
(#156112,#156113),(#156114,#156115),(#156116,#156117),(#156118,#156119),
(#156120,#156121),(#156122,#156123),(#156124,#156125),(#156126,#156127),
(#156128,#156129),(#156130,#156131),(#156132,#156133),(#156134,#156135),
(#156136,#156137),(#156138,#156139),(#156140,#156141),(#156142,#156143),
(#156144,#156145),(#156146,#156147),(#156148,#156149),(#156150,#156151),
(#156152,#156153),(#156154,#156155),(#156156,#156157),(#156158,#156159),
(#156160,#156161),(#156162,#156163),(#156164,#156165),(#156166,#156167),
(#156168,#156169),(#156170,#156171),(#156172,#156173),(#156174,#156175),
(#156176,#156177),(#156178,#156179),(#156180,#156181),(#156182,#156183),
(#156184,#156185),(#156186,#156187),(#156188,#156189),(#156190,#156191),
(#156192,#156193),(#156194,#156195),(#156196,#156197),(#156198,#156199),
(#156200,#156201),(#156202,#156203),(#156204,#156205),(#156206,#156207),
(#156208,#156209),(#156210,#156211),(#156212,#156213),(#156214,#156215),
(#156216,#156217),(#156218,#156219),(#156220,#156221),(#156222,#156223),
(#156224,#156225),(#156226,#156227),(#156228,#156229),(#156230,#156231),
(#156232,#156233),(#156234,#156235),(#156236,#156237),(#156238,#156239),
(#156240,#156241),(#156242,#156243),(#156244,#156245),(#156246,#156247),
(#156248,#156249),(#156250,#156251),(#156252,#156253),(#156254,#156255),
(#156256,#156257),(#156258,#156259),(#156260,#156261),(#156262,#156263),
(#156264,#156265),(#156266,#156267),(#156268,#156269),(#156270,#156271),
(#156272,#156273),(#156274,#156275),(#156276,#156277),(#156278,#156279),
(#156280,#156281),(#156282,#156283),(#156284,#156285),(#156286,#156287),
(#156288,#156289),(#156290,#156291),(#156292,#156293),(#156294,#156295),
(#156296,#156297),(#156298,#156299),(#156300,#156301),(#156302,#156303),
(#156304,#156305),(#156306,#156307),(#156308,#156309),(#156310,#156311),
(#156312,#156313),(#156314,#156315),(#156316,#156317),(#156318,#156319),
(#156320,#156321),(#156322,#156323),(#156324,#156325),(#156326,#156327),
(#156328,#156329),(#156330,#156331),(#156332,#156333),(#156334,#156335),
(#156336,#156337),(#156338,#156339),(#156340,#156341),(#156342,#156343),
(#156344,#156345),(#156346,#156347),(#156348,#156349),(#156350,#156351),
(#156352,#156353),(#156354,#156355),(#156356,#156357),(#156358,#156359),
(#156360,#156361),(#156362,#156363),(#156364,#156365),(#156366,#156367),
(#156368,#156369),(#156370,#156371),(#156372,#156373),(#156374,#156375),
(#156376,#156377),(#156378,#156379)),.UNSPECIFIED.,.F.,.F.,.F.,(6,1,1,1,
1,1,1,1,1,1,1,1,1,1,1,1,1,1,1,1,1,1,1,1,1,1,1,1,1,1,1,1,1,1,1,1,1,1,1,1,
1,1,1,1,1,1,1,1,1,1,1,1,1,1,1,1,1,1,1,1,1,1,1,1,1,1,1,1,1,1,1,1,1,1,1,1,
1,1,1,1,1,1,1,1,1,1,1,1,1,1,1,1,1,1,1,1,1,1,1,1,1,1,1,1,1,1,1,1,1,1,1,1,
1,1,1,1,1,1,1,1,1,1,1,1,1,1,1,1,1,1,1,1,1,1,1,1,1,1,1,1,1,1,1,1,1,1,1,1,
1,1,1,1,1,1,1,1,1,1,1,1,1,1,1,1,1,1,1,1,1,1,1,1,1,1,1,1,1,1,1,1,1,1,1,1,
1,1,1,1,1,1,1,1,1,1,1,1,1,1,1,1,1,1,1,1,1,1,1,1,1,1,1,1,1,1,1,1,1,1,1,1,
1,1,1,1,1,1,1,1,1,1,1,1,1,1,1,1,1,1,1,1,1,1,1,1,1,1,1,1,1,1,1,1,1,1,1,1,
1,1,1,1,1,1,1,1,1,1,1,1,1,1,1,1,1,1,1,1,1,1,1,1,1,1,1,1,1,1,1,1,1,1,1,1,
1,1,1,1,1,1,1,1,1,1,1,1,1,1,1,1,1,1,1,1,1,1,1,1,1,1,1,1,1,1,1,1,1,1,1,1,
1,1,1,1,1,1,1,1,1,1,1,1,1,1,1,1,1,1,1,1,1,1,1,1,1,1,1,1,1,1,1,1,1,1,1,1,
1,1,1,1,1,1,1,1,1,1,1,1,1,1,1,1,1,1,1,1,1,1,1,1,1,1,1,1,1,1,1,1,1,1,1,1,
1,1,1,1,1,1,1,1,1,1,1,1,1,1,1,1,1,1,1,1,1,1,1,1,1,1,1,1,1,1,1,1,1,1,1,1,
1,1,1,1,1,1,1,1,1,1,1,1,1,1,1,1,1,1,1,1,1,1,1,1,1,1,1,1,1,1,1,6),(2,2),
(-1.,-0.998165138,-0.996330275,-0.994495413,-0.99266055,-0.990825688,-0.988990826,
-0.987155963,-0.985321101,-0.983486239,-0.981651376,-0.979816514,-0.977981651,
-0.976146789,-0.974311927,-0.972477064,-0.970642202,-0.968807339,-0.966972477,
-0.965137615,-0.963302752,-0.96146789,-0.959633028,-0.957798165,-0.955963303,
-0.95412844,-0.952293578,-0.950458716,-0.948623853,-0.946788991,-0.944954128,
-0.943119266,-0.941284404,-0.939449541,-0.937614679,-0.935779817,-0.933944954,
-0.932110092,-0.930275229,-0.928440367,-0.926605505,-0.924770642,-0.92293578,
-0.921100917,-0.919266055,-0.917431193,-0.91559633,-0.913761468,-0.911926606,
-0.910091743,-0.908256881,-0.906422018,-0.904587156,-0.902752294,-0.900917431,
-0.899082569,-0.897247706,-0.895412844,-0.893577982,-0.891743119,-0.889908257,
-0.888073394,-0.886238532,-0.88440367,-0.882568807,-0.880733945,-0.878899083,
-0.87706422,-0.875229358,-0.873394495,-0.871559633,-0.869724771,-0.867889908,
-0.866055046,-0.864220183,-0.862385321,-0.860550459,-0.858715596,-0.856880734,
-0.855045872,-0.853211009,-0.851376147,-0.849541284,-0.847706422,-0.84587156,
-0.844036697,-0.842201835,-0.840366972,-0.83853211,-0.836697248,-0.834862385,
-0.833027523,-0.831192661,-0.829357798,-0.827522936,-0.825688073,-0.823853211,
-0.822018349,-0.820183486,-0.818348624,-0.816513761,-0.814678899,-0.812844037,
-0.811009174,-0.809174312,-0.80733945,-0.805504587,-0.803669725,-0.801834862,
-0.8,-0.798165138,-0.796330275,-0.794495413,-0.79266055,-0.790825688,-0.788990826,
-0.787155963,-0.785321101,-0.783486239,-0.781651376,-0.779816514,-0.777981651,
-0.776146789,-0.774311927,-0.772477064,-0.770642202,-0.768807339,-0.766972477,
-0.765137615,-0.763302752,-0.76146789,-0.759633028,-0.757798165,-0.755963303,
-0.75412844,-0.752293578,-0.750458716,-0.748623853,-0.746788991,-0.744954128,
-0.743119266,-0.741284404,-0.739449541,-0.737614679,-0.735779817,-0.733944954,
-0.732110092,-0.730275229,-0.728440367,-0.726605505,-0.724770642,-0.72293578,
-0.721100917,-0.719266055,-0.717431193,-0.71559633,-0.713761468,-0.711926606,
-0.710091743,-0.708256881,-0.706422018,-0.704587156,-0.702752294,-0.700917431,
-0.699082569,-0.697247706,-0.695412844,-0.693577982,-0.691743119,-0.689908257,
-0.688073394,-0.686238532,-0.68440367,-0.682568807,-0.680733945,-0.678899083,
-0.67706422,-0.675229358,-0.673394495,-0.671559633,-0.669724771,-0.667889908,
-0.666055046,-0.664220183,-0.662385321,-0.660550459,-0.658715596,-0.656880734,
-0.655045872,-0.653211009,-0.651376147,-0.649541284,-0.647706422,-0.64587156,
-0.644036697,-0.642201835,-0.640366972,-0.63853211,-0.636697248,-0.634862385,
-0.633027523,-0.631192661,-0.629357798,-0.627522936,-0.625688073,-0.623853211,
-0.622018349,-0.620183486,-0.618348624,-0.616513761,-0.614678899,-0.612844037,
-0.611009174,-0.609174312,-0.60733945,-0.605504587,-0.603669725,-0.601834862,
-0.6,-0.598165138,-0.596330275,-0.594495413,-0.59266055,-0.590825688,-0.588990826,
-0.587155963,-0.585321101,-0.583486239,-0.581651376,-0.579816514,-0.577981651,
-0.576146789,-0.574311927,-0.572477064,-0.570642202,-0.568807339,-0.566972477,
-0.565137615,-0.563302752,-0.56146789,-0.559633028,-0.557798165,-0.555963303,
-0.55412844,-0.552293578,-0.550458716,-0.548623853,-0.546788991,-0.544954128,
-0.543119266,-0.541284404,-0.539449541,-0.537614679,-0.535779817,-0.533944954,
-0.532110092,-0.530275229,-0.528440367,-0.526605505,-0.524770642,-0.52293578,
-0.521100917,-0.519266055,-0.517431193,-0.51559633,-0.513761468,-0.511926606,
-0.510091743,-0.508256881,-0.506422018,-0.504587156,-0.502752294,-0.500917431,
-0.499082569,-0.497247706,-0.495412844,-0.493577982,-0.491743119,-0.489908257,
-0.488073394,-0.486238532,-0.48440367,-0.482568807,-0.480733945,-0.478899083,
-0.47706422,-0.475229358,-0.473394495,-0.471559633,-0.469724771,-0.467889908,
-0.466055046,-0.464220183,-0.462385321,-0.460550459,-0.458715596,-0.456880734,
-0.455045872,-0.453211009,-0.451376147,-0.449541284,-0.447706422,-0.44587156,
-0.444036697,-0.442201835,-0.440366972,-0.43853211,-0.436697248,-0.434862385,
-0.433027523,-0.431192661,-0.429357798,-0.427522936,-0.425688073,-0.423853211,
-0.422018349,-0.420183486,-0.418348624,-0.416513761,-0.414678899,-0.412844037,
-0.411009174,-0.409174312,-0.40733945,-0.405504587,-0.403669725,-0.401834862,
-0.4,-0.398165138,-0.396330275,-0.394495413,-0.39266055,-0.390825688,-0.388990826,
-0.387155963,-0.385321101,-0.383486239,-0.381651376,-0.379816514,-0.377981651,
-0.376146789,-0.374311927,-0.372477064,-0.370642202,-0.368807339,-0.366972477,
-0.365137615,-0.363302752,-0.36146789,-0.359633028,-0.357798165,-0.355963303,
-0.35412844,-0.352293578,-0.350458716,-0.348623853,-0.346788991,-0.344954128,
-0.343119266,-0.341284404,-0.339449541,-0.337614679,-0.335779817,-0.333944954,
-0.332110092,-0.330275229,-0.328440367,-0.326605505,-0.324770642,-0.32293578,
-0.321100917,-0.319266055,-0.317431193,-0.31559633,-0.313761468,-0.311926606,
-0.310091743,-0.308256881,-0.306422018,-0.304587156,-0.302752294,-0.300917431,
-0.299082569,-0.297247706,-0.295412844,-0.293577982,-0.291743119,-0.289908257,
-0.288073394,-0.286238532,-0.28440367,-0.282568807,-0.280733945,-0.278899083,
-0.27706422,-0.275229358,-0.273394495,-0.271559633,-0.269724771,-0.267889908,
-0.266055046,-0.264220183,-0.262385321,-0.260550459,-0.258715596,-0.256880734,
-0.255045872,-0.253211009,-0.251376147,-0.249541284,-0.247706422,-0.24587156,
-0.244036697,-0.242201835,-0.240366972,-0.23853211,-0.236697248,-0.234862385,
-0.233027523,-0.231192661,-0.229357798,-0.227522936,-0.225688073,-0.223853211,
-0.222018349,-0.220183486,-0.218348624,-0.216513761,-0.214678899,-0.212844037,
-0.211009174,-0.209174312,-0.20733945,-0.205504587,-0.203669725,-0.201834862,
-0.2,-0.198165138,-0.196330275,-0.194495413,-0.19266055,-0.190825688,-0.188990826,
-0.187155963,-0.185321101,-0.183486239,-0.181651376,-0.179816514,-0.177981651,
-0.176146789,-0.174311927,-0.172477064,-0.170642202,-0.168807339,-0.166972477,
-0.165137615,-0.163302752,-0.16146789,-0.159633028,-0.157798165,-0.155963303,
-0.15412844,-0.152293578,-0.150458716,-0.148623853,-0.146788991,-0.144954128,
-0.143172103),(0.,0.36),.UNSPECIFIED.);
#6217=B_SPLINE_SURFACE_WITH_KNOTS('',5,1,((#157342,#157343),(#157344,#157345),
(#157346,#157347),(#157348,#157349),(#157350,#157351),(#157352,#157353),
(#157354,#157355),(#157356,#157357),(#157358,#157359),(#157360,#157361),
(#157362,#157363),(#157364,#157365),(#157366,#157367),(#157368,#157369),
(#157370,#157371),(#157372,#157373),(#157374,#157375),(#157376,#157377),
(#157378,#157379),(#157380,#157381),(#157382,#157383),(#157384,#157385),
(#157386,#157387),(#157388,#157389),(#157390,#157391),(#157392,#157393),
(#157394,#157395),(#157396,#157397),(#157398,#157399),(#157400,#157401),
(#157402,#157403),(#157404,#157405),(#157406,#157407),(#157408,#157409),
(#157410,#157411),(#157412,#157413),(#157414,#157415),(#157416,#157417),
(#157418,#157419),(#157420,#157421),(#157422,#157423),(#157424,#157425),
(#157426,#157427),(#157428,#157429),(#157430,#157431),(#157432,#157433),
(#157434,#157435),(#157436,#157437),(#157438,#157439),(#157440,#157441),
(#157442,#157443),(#157444,#157445),(#157446,#157447),(#157448,#157449),
(#157450,#157451),(#157452,#157453),(#157454,#157455),(#157456,#157457),
(#157458,#157459),(#157460,#157461),(#157462,#157463),(#157464,#157465),
(#157466,#157467),(#157468,#157469),(#157470,#157471),(#157472,#157473),
(#157474,#157475),(#157476,#157477),(#157478,#157479),(#157480,#157481),
(#157482,#157483),(#157484,#157485),(#157486,#157487),(#157488,#157489),
(#157490,#157491),(#157492,#157493),(#157494,#157495),(#157496,#157497),
(#157498,#157499),(#157500,#157501),(#157502,#157503),(#157504,#157505),
(#157506,#157507),(#157508,#157509),(#157510,#157511),(#157512,#157513),
(#157514,#157515),(#157516,#157517),(#157518,#157519),(#157520,#157521),
(#157522,#157523),(#157524,#157525),(#157526,#157527),(#157528,#157529),
(#157530,#157531),(#157532,#157533),(#157534,#157535),(#157536,#157537),
(#157538,#157539),(#157540,#157541),(#157542,#157543),(#157544,#157545),
(#157546,#157547),(#157548,#157549),(#157550,#157551),(#157552,#157553),
(#157554,#157555),(#157556,#157557),(#157558,#157559),(#157560,#157561),
(#157562,#157563),(#157564,#157565),(#157566,#157567),(#157568,#157569),
(#157570,#157571),(#157572,#157573),(#157574,#157575),(#157576,#157577),
(#157578,#157579),(#157580,#157581),(#157582,#157583),(#157584,#157585),
(#157586,#157587),(#157588,#157589),(#157590,#157591),(#157592,#157593),
(#157594,#157595),(#157596,#157597),(#157598,#157599),(#157600,#157601),
(#157602,#157603),(#157604,#157605),(#157606,#157607),(#157608,#157609),
(#157610,#157611),(#157612,#157613),(#157614,#157615),(#157616,#157617),
(#157618,#157619),(#157620,#157621),(#157622,#157623),(#157624,#157625),
(#157626,#157627),(#157628,#157629),(#157630,#157631),(#157632,#157633),
(#157634,#157635),(#157636,#157637),(#157638,#157639),(#157640,#157641),
(#157642,#157643),(#157644,#157645),(#157646,#157647),(#157648,#157649),
(#157650,#157651),(#157652,#157653),(#157654,#157655),(#157656,#157657),
(#157658,#157659),(#157660,#157661),(#157662,#157663),(#157664,#157665),
(#157666,#157667),(#157668,#157669),(#157670,#157671),(#157672,#157673),
(#157674,#157675),(#157676,#157677),(#157678,#157679),(#157680,#157681),
(#157682,#157683),(#157684,#157685),(#157686,#157687),(#157688,#157689),
(#157690,#157691),(#157692,#157693),(#157694,#157695),(#157696,#157697),
(#157698,#157699),(#157700,#157701),(#157702,#157703),(#157704,#157705),
(#157706,#157707),(#157708,#157709),(#157710,#157711),(#157712,#157713),
(#157714,#157715),(#157716,#157717),(#157718,#157719),(#157720,#157721),
(#157722,#157723),(#157724,#157725),(#157726,#157727),(#157728,#157729),
(#157730,#157731),(#157732,#157733),(#157734,#157735),(#157736,#157737),
(#157738,#157739),(#157740,#157741),(#157742,#157743),(#157744,#157745),
(#157746,#157747),(#157748,#157749),(#157750,#157751),(#157752,#157753),
(#157754,#157755),(#157756,#157757),(#157758,#157759),(#157760,#157761),
(#157762,#157763),(#157764,#157765),(#157766,#157767),(#157768,#157769),
(#157770,#157771),(#157772,#157773),(#157774,#157775),(#157776,#157777),
(#157778,#157779),(#157780,#157781),(#157782,#157783),(#157784,#157785),
(#157786,#157787),(#157788,#157789),(#157790,#157791),(#157792,#157793),
(#157794,#157795),(#157796,#157797),(#157798,#157799),(#157800,#157801),
(#157802,#157803),(#157804,#157805),(#157806,#157807),(#157808,#157809),
(#157810,#157811),(#157812,#157813),(#157814,#157815),(#157816,#157817),
(#157818,#157819),(#157820,#157821),(#157822,#157823),(#157824,#157825),
(#157826,#157827),(#157828,#157829),(#157830,#157831),(#157832,#157833),
(#157834,#157835),(#157836,#157837),(#157838,#157839),(#157840,#157841),
(#157842,#157843),(#157844,#157845),(#157846,#157847),(#157848,#157849),
(#157850,#157851),(#157852,#157853),(#157854,#157855),(#157856,#157857),
(#157858,#157859),(#157860,#157861),(#157862,#157863),(#157864,#157865),
(#157866,#157867),(#157868,#157869),(#157870,#157871),(#157872,#157873),
(#157874,#157875),(#157876,#157877),(#157878,#157879),(#157880,#157881),
(#157882,#157883),(#157884,#157885),(#157886,#157887),(#157888,#157889),
(#157890,#157891),(#157892,#157893),(#157894,#157895),(#157896,#157897),
(#157898,#157899),(#157900,#157901),(#157902,#157903),(#157904,#157905),
(#157906,#157907),(#157908,#157909),(#157910,#157911),(#157912,#157913),
(#157914,#157915),(#157916,#157917),(#157918,#157919),(#157920,#157921),
(#157922,#157923),(#157924,#157925),(#157926,#157927),(#157928,#157929),
(#157930,#157931),(#157932,#157933),(#157934,#157935),(#157936,#157937),
(#157938,#157939),(#157940,#157941),(#157942,#157943),(#157944,#157945),
(#157946,#157947),(#157948,#157949),(#157950,#157951),(#157952,#157953),
(#157954,#157955),(#157956,#157957),(#157958,#157959),(#157960,#157961),
(#157962,#157963),(#157964,#157965),(#157966,#157967),(#157968,#157969),
(#157970,#157971),(#157972,#157973),(#157974,#157975),(#157976,#157977),
(#157978,#157979),(#157980,#157981),(#157982,#157983),(#157984,#157985),
(#157986,#157987),(#157988,#157989),(#157990,#157991),(#157992,#157993),
(#157994,#157995),(#157996,#157997),(#157998,#157999),(#158000,#158001),
(#158002,#158003),(#158004,#158005),(#158006,#158007),(#158008,#158009),
(#158010,#158011),(#158012,#158013),(#158014,#158015),(#158016,#158017),
(#158018,#158019),(#158020,#158021),(#158022,#158023),(#158024,#158025),
(#158026,#158027),(#158028,#158029),(#158030,#158031),(#158032,#158033),
(#158034,#158035),(#158036,#158037),(#158038,#158039),(#158040,#158041),
(#158042,#158043),(#158044,#158045),(#158046,#158047),(#158048,#158049),
(#158050,#158051),(#158052,#158053),(#158054,#158055),(#158056,#158057),
(#158058,#158059),(#158060,#158061),(#158062,#158063),(#158064,#158065),
(#158066,#158067),(#158068,#158069),(#158070,#158071),(#158072,#158073),
(#158074,#158075),(#158076,#158077),(#158078,#158079),(#158080,#158081),
(#158082,#158083),(#158084,#158085),(#158086,#158087),(#158088,#158089),
(#158090,#158091),(#158092,#158093),(#158094,#158095),(#158096,#158097),
(#158098,#158099),(#158100,#158101),(#158102,#158103),(#158104,#158105),
(#158106,#158107),(#158108,#158109),(#158110,#158111),(#158112,#158113),
(#158114,#158115),(#158116,#158117),(#158118,#158119),(#158120,#158121),
(#158122,#158123),(#158124,#158125),(#158126,#158127),(#158128,#158129),
(#158130,#158131),(#158132,#158133),(#158134,#158135),(#158136,#158137),
(#158138,#158139),(#158140,#158141),(#158142,#158143),(#158144,#158145),
(#158146,#158147),(#158148,#158149),(#158150,#158151),(#158152,#158153),
(#158154,#158155),(#158156,#158157),(#158158,#158159),(#158160,#158161),
(#158162,#158163),(#158164,#158165),(#158166,#158167),(#158168,#158169),
(#158170,#158171),(#158172,#158173),(#158174,#158175),(#158176,#158177),
(#158178,#158179),(#158180,#158181),(#158182,#158183),(#158184,#158185),
(#158186,#158187),(#158188,#158189),(#158190,#158191),(#158192,#158193),
(#158194,#158195),(#158196,#158197),(#158198,#158199),(#158200,#158201),
(#158202,#158203),(#158204,#158205),(#158206,#158207),(#158208,#158209),
(#158210,#158211),(#158212,#158213),(#158214,#158215),(#158216,#158217),
(#158218,#158219),(#158220,#158221),(#158222,#158223),(#158224,#158225),
(#158226,#158227),(#158228,#158229),(#158230,#158231),(#158232,#158233),
(#158234,#158235),(#158236,#158237),(#158238,#158239),(#158240,#158241),
(#158242,#158243),(#158244,#158245),(#158246,#158247),(#158248,#158249),
(#158250,#158251),(#158252,#158253),(#158254,#158255),(#158256,#158257),
(#158258,#158259),(#158260,#158261),(#158262,#158263),(#158264,#158265),
(#158266,#158267),(#158268,#158269),(#158270,#158271),(#158272,#158273),
(#158274,#158275),(#158276,#158277),(#158278,#158279),(#158280,#158281),
(#158282,#158283),(#158284,#158285)),.UNSPECIFIED.,.F.,.F.,.F.,(6,1,1,1,
1,1,1,1,1,1,1,1,1,1,1,1,1,1,1,1,1,1,1,1,1,1,1,1,1,1,1,1,1,1,1,1,1,1,1,1,
1,1,1,1,1,1,1,1,1,1,1,1,1,1,1,1,1,1,1,1,1,1,1,1,1,1,1,1,1,1,1,1,1,1,1,1,
1,1,1,1,1,1,1,1,1,1,1,1,1,1,1,1,1,1,1,1,1,1,1,1,1,1,1,1,1,1,1,1,1,1,1,1,
1,1,1,1,1,1,1,1,1,1,1,1,1,1,1,1,1,1,1,1,1,1,1,1,1,1,1,1,1,1,1,1,1,1,1,1,
1,1,1,1,1,1,1,1,1,1,1,1,1,1,1,1,1,1,1,1,1,1,1,1,1,1,1,1,1,1,1,1,1,1,1,1,
1,1,1,1,1,1,1,1,1,1,1,1,1,1,1,1,1,1,1,1,1,1,1,1,1,1,1,1,1,1,1,1,1,1,1,1,
1,1,1,1,1,1,1,1,1,1,1,1,1,1,1,1,1,1,1,1,1,1,1,1,1,1,1,1,1,1,1,1,1,1,1,1,
1,1,1,1,1,1,1,1,1,1,1,1,1,1,1,1,1,1,1,1,1,1,1,1,1,1,1,1,1,1,1,1,1,1,1,1,
1,1,1,1,1,1,1,1,1,1,1,1,1,1,1,1,1,1,1,1,1,1,1,1,1,1,1,1,1,1,1,1,1,1,1,1,
1,1,1,1,1,1,1,1,1,1,1,1,1,1,1,1,1,1,1,1,1,1,1,1,1,1,1,1,1,1,1,1,1,1,1,1,
1,1,1,1,1,1,1,1,1,1,1,1,1,1,1,1,1,1,1,1,1,1,1,1,1,1,1,1,1,1,1,1,1,1,1,1,
1,1,1,1,1,1,1,1,1,1,1,1,1,1,1,1,1,1,1,1,1,1,1,1,1,1,1,1,1,1,1,1,1,1,1,1,
1,1,1,1,1,1,1,1,1,1,1,1,1,1,1,1,1,1,1,1,1,1,1,1,1,1,1,1,1,1,1,6),(2,2),
(-1.,-0.998165138,-0.996330275,-0.994495413,-0.99266055,-0.990825688,-0.988990826,
-0.987155963,-0.985321101,-0.983486239,-0.981651376,-0.979816514,-0.977981651,
-0.976146789,-0.974311927,-0.972477064,-0.970642202,-0.968807339,-0.966972477,
-0.965137615,-0.963302752,-0.96146789,-0.959633028,-0.957798165,-0.955963303,
-0.95412844,-0.952293578,-0.950458716,-0.948623853,-0.946788991,-0.944954128,
-0.943119266,-0.941284404,-0.939449541,-0.937614679,-0.935779817,-0.933944954,
-0.932110092,-0.930275229,-0.928440367,-0.926605505,-0.924770642,-0.92293578,
-0.921100917,-0.919266055,-0.917431193,-0.91559633,-0.913761468,-0.911926606,
-0.910091743,-0.908256881,-0.906422018,-0.904587156,-0.902752294,-0.900917431,
-0.899082569,-0.897247706,-0.895412844,-0.893577982,-0.891743119,-0.889908257,
-0.888073394,-0.886238532,-0.88440367,-0.882568807,-0.880733945,-0.878899083,
-0.87706422,-0.875229358,-0.873394495,-0.871559633,-0.869724771,-0.867889908,
-0.866055046,-0.864220183,-0.862385321,-0.860550459,-0.858715596,-0.856880734,
-0.855045872,-0.853211009,-0.851376147,-0.849541284,-0.847706422,-0.84587156,
-0.844036697,-0.842201835,-0.840366972,-0.83853211,-0.836697248,-0.834862385,
-0.833027523,-0.831192661,-0.829357798,-0.827522936,-0.825688073,-0.823853211,
-0.822018349,-0.820183486,-0.818348624,-0.816513761,-0.814678899,-0.812844037,
-0.811009174,-0.809174312,-0.80733945,-0.805504587,-0.803669725,-0.801834862,
-0.8,-0.798165138,-0.796330275,-0.794495413,-0.79266055,-0.790825688,-0.788990826,
-0.787155963,-0.785321101,-0.783486239,-0.781651376,-0.779816514,-0.777981651,
-0.776146789,-0.774311927,-0.772477064,-0.770642202,-0.768807339,-0.766972477,
-0.765137615,-0.763302752,-0.76146789,-0.759633028,-0.757798165,-0.755963303,
-0.75412844,-0.752293578,-0.750458716,-0.748623853,-0.746788991,-0.744954128,
-0.743119266,-0.741284404,-0.739449541,-0.737614679,-0.735779817,-0.733944954,
-0.732110092,-0.730275229,-0.728440367,-0.726605505,-0.724770642,-0.72293578,
-0.721100917,-0.719266055,-0.717431193,-0.71559633,-0.713761468,-0.711926606,
-0.710091743,-0.708256881,-0.706422018,-0.704587156,-0.702752294,-0.700917431,
-0.699082569,-0.697247706,-0.695412844,-0.693577982,-0.691743119,-0.689908257,
-0.688073394,-0.686238532,-0.68440367,-0.682568807,-0.680733945,-0.678899083,
-0.67706422,-0.675229358,-0.673394495,-0.671559633,-0.669724771,-0.667889908,
-0.666055046,-0.664220183,-0.662385321,-0.660550459,-0.658715596,-0.656880734,
-0.655045872,-0.653211009,-0.651376147,-0.649541284,-0.647706422,-0.64587156,
-0.644036697,-0.642201835,-0.640366972,-0.63853211,-0.636697248,-0.634862385,
-0.633027523,-0.631192661,-0.629357798,-0.627522936,-0.625688073,-0.623853211,
-0.622018349,-0.620183486,-0.618348624,-0.616513761,-0.614678899,-0.612844037,
-0.611009174,-0.609174312,-0.60733945,-0.605504587,-0.603669725,-0.601834862,
-0.6,-0.598165138,-0.596330275,-0.594495413,-0.59266055,-0.590825688,-0.588990826,
-0.587155963,-0.585321101,-0.583486239,-0.581651376,-0.579816514,-0.577981651,
-0.576146789,-0.574311927,-0.572477064,-0.570642202,-0.568807339,-0.566972477,
-0.565137615,-0.563302752,-0.56146789,-0.559633028,-0.557798165,-0.555963303,
-0.55412844,-0.552293578,-0.550458716,-0.548623853,-0.546788991,-0.544954128,
-0.543119266,-0.541284404,-0.539449541,-0.537614679,-0.535779817,-0.533944954,
-0.532110092,-0.530275229,-0.528440367,-0.526605505,-0.524770642,-0.52293578,
-0.521100917,-0.519266055,-0.517431193,-0.51559633,-0.513761468,-0.511926606,
-0.510091743,-0.508256881,-0.506422018,-0.504587156,-0.502752294,-0.500917431,
-0.499082569,-0.497247706,-0.495412844,-0.493577982,-0.491743119,-0.489908257,
-0.488073394,-0.486238532,-0.48440367,-0.482568807,-0.480733945,-0.478899083,
-0.47706422,-0.475229358,-0.473394495,-0.471559633,-0.469724771,-0.467889908,
-0.466055046,-0.464220183,-0.462385321,-0.460550459,-0.458715596,-0.456880734,
-0.455045872,-0.453211009,-0.451376147,-0.449541284,-0.447706422,-0.44587156,
-0.444036697,-0.442201835,-0.440366972,-0.43853211,-0.436697248,-0.434862385,
-0.433027523,-0.431192661,-0.429357798,-0.427522936,-0.425688073,-0.423853211,
-0.422018349,-0.420183486,-0.418348624,-0.416513761,-0.414678899,-0.412844037,
-0.411009174,-0.409174312,-0.40733945,-0.405504587,-0.403669725,-0.401834862,
-0.4,-0.398165138,-0.396330275,-0.394495413,-0.39266055,-0.390825688,-0.388990826,
-0.387155963,-0.385321101,-0.383486239,-0.381651376,-0.379816514,-0.377981651,
-0.376146789,-0.374311927,-0.372477064,-0.370642202,-0.368807339,-0.366972477,
-0.365137615,-0.363302752,-0.36146789,-0.359633028,-0.357798165,-0.355963303,
-0.35412844,-0.352293578,-0.350458716,-0.348623853,-0.346788991,-0.344954128,
-0.343119266,-0.341284404,-0.339449541,-0.337614679,-0.335779817,-0.333944954,
-0.332110092,-0.330275229,-0.328440367,-0.326605505,-0.324770642,-0.32293578,
-0.321100917,-0.319266055,-0.317431193,-0.31559633,-0.313761468,-0.311926606,
-0.310091743,-0.308256881,-0.306422018,-0.304587156,-0.302752294,-0.300917431,
-0.299082569,-0.297247706,-0.295412844,-0.293577982,-0.291743119,-0.289908257,
-0.288073394,-0.286238532,-0.28440367,-0.282568807,-0.280733945,-0.278899083,
-0.27706422,-0.275229358,-0.273394495,-0.271559633,-0.269724771,-0.267889908,
-0.266055046,-0.264220183,-0.262385321,-0.260550459,-0.258715596,-0.256880734,
-0.255045872,-0.253211009,-0.251376147,-0.249541284,-0.247706422,-0.24587156,
-0.244036697,-0.242201835,-0.240366972,-0.23853211,-0.236697248,-0.234862385,
-0.233027523,-0.231192661,-0.229357798,-0.227522936,-0.225688073,-0.223853211,
-0.222018349,-0.220183486,-0.218348624,-0.216513761,-0.214678899,-0.212844037,
-0.211009174,-0.209174312,-0.20733945,-0.205504587,-0.203669725,-0.201834862,
-0.2,-0.198165138,-0.196330275,-0.194495413,-0.19266055,-0.190825688,-0.188990826,
-0.187155963,-0.185321101,-0.183486239,-0.181651376,-0.179816514,-0.177981651,
-0.176146789,-0.174311927,-0.172477064,-0.170642202,-0.168807339,-0.166972477,
-0.165137615,-0.163302752,-0.16146789,-0.159633028,-0.157798165,-0.155963303,
-0.15412844,-0.152293578,-0.150458716,-0.148623853,-0.146788991,-0.144954128,
-0.143172103),(0.,0.36),.UNSPECIFIED.);
#6218=B_SPLINE_SURFACE_WITH_KNOTS('',5,1,((#158927,#158928),(#158929,#158930),
(#158931,#158932),(#158933,#158934),(#158935,#158936),(#158937,#158938),
(#158939,#158940),(#158941,#158942),(#158943,#158944),(#158945,#158946),
(#158947,#158948),(#158949,#158950),(#158951,#158952),(#158953,#158954),
(#158955,#158956),(#158957,#158958),(#158959,#158960),(#158961,#158962),
(#158963,#158964),(#158965,#158966),(#158967,#158968),(#158969,#158970),
(#158971,#158972),(#158973,#158974),(#158975,#158976),(#158977,#158978),
(#158979,#158980),(#158981,#158982),(#158983,#158984),(#158985,#158986),
(#158987,#158988),(#158989,#158990),(#158991,#158992),(#158993,#158994),
(#158995,#158996),(#158997,#158998),(#158999,#159000),(#159001,#159002),
(#159003,#159004),(#159005,#159006),(#159007,#159008),(#159009,#159010),
(#159011,#159012),(#159013,#159014),(#159015,#159016),(#159017,#159018),
(#159019,#159020),(#159021,#159022),(#159023,#159024),(#159025,#159026),
(#159027,#159028),(#159029,#159030),(#159031,#159032),(#159033,#159034),
(#159035,#159036),(#159037,#159038),(#159039,#159040),(#159041,#159042),
(#159043,#159044),(#159045,#159046),(#159047,#159048),(#159049,#159050),
(#159051,#159052),(#159053,#159054),(#159055,#159056),(#159057,#159058),
(#159059,#159060),(#159061,#159062),(#159063,#159064),(#159065,#159066),
(#159067,#159068),(#159069,#159070),(#159071,#159072),(#159073,#159074),
(#159075,#159076),(#159077,#159078),(#159079,#159080),(#159081,#159082),
(#159083,#159084),(#159085,#159086),(#159087,#159088),(#159089,#159090),
(#159091,#159092),(#159093,#159094),(#159095,#159096),(#159097,#159098),
(#159099,#159100),(#159101,#159102),(#159103,#159104),(#159105,#159106),
(#159107,#159108),(#159109,#159110),(#159111,#159112),(#159113,#159114),
(#159115,#159116),(#159117,#159118),(#159119,#159120),(#159121,#159122),
(#159123,#159124),(#159125,#159126),(#159127,#159128),(#159129,#159130),
(#159131,#159132),(#159133,#159134),(#159135,#159136),(#159137,#159138),
(#159139,#159140),(#159141,#159142),(#159143,#159144),(#159145,#159146),
(#159147,#159148),(#159149,#159150),(#159151,#159152),(#159153,#159154),
(#159155,#159156),(#159157,#159158),(#159159,#159160),(#159161,#159162),
(#159163,#159164),(#159165,#159166),(#159167,#159168),(#159169,#159170),
(#159171,#159172),(#159173,#159174),(#159175,#159176),(#159177,#159178),
(#159179,#159180),(#159181,#159182),(#159183,#159184),(#159185,#159186),
(#159187,#159188),(#159189,#159190),(#159191,#159192),(#159193,#159194),
(#159195,#159196),(#159197,#159198),(#159199,#159200),(#159201,#159202),
(#159203,#159204),(#159205,#159206),(#159207,#159208),(#159209,#159210),
(#159211,#159212),(#159213,#159214),(#159215,#159216),(#159217,#159218),
(#159219,#159220),(#159221,#159222),(#159223,#159224),(#159225,#159226),
(#159227,#159228),(#159229,#159230),(#159231,#159232),(#159233,#159234),
(#159235,#159236),(#159237,#159238),(#159239,#159240),(#159241,#159242),
(#159243,#159244),(#159245,#159246),(#159247,#159248),(#159249,#159250),
(#159251,#159252),(#159253,#159254),(#159255,#159256),(#159257,#159258),
(#159259,#159260),(#159261,#159262),(#159263,#159264),(#159265,#159266),
(#159267,#159268),(#159269,#159270),(#159271,#159272),(#159273,#159274),
(#159275,#159276),(#159277,#159278),(#159279,#159280),(#159281,#159282),
(#159283,#159284),(#159285,#159286),(#159287,#159288),(#159289,#159290),
(#159291,#159292),(#159293,#159294),(#159295,#159296),(#159297,#159298),
(#159299,#159300),(#159301,#159302),(#159303,#159304),(#159305,#159306),
(#159307,#159308),(#159309,#159310),(#159311,#159312),(#159313,#159314),
(#159315,#159316),(#159317,#159318),(#159319,#159320),(#159321,#159322),
(#159323,#159324),(#159325,#159326),(#159327,#159328),(#159329,#159330),
(#159331,#159332),(#159333,#159334),(#159335,#159336),(#159337,#159338),
(#159339,#159340),(#159341,#159342),(#159343,#159344),(#159345,#159346),
(#159347,#159348),(#159349,#159350),(#159351,#159352),(#159353,#159354),
(#159355,#159356),(#159357,#159358),(#159359,#159360),(#159361,#159362),
(#159363,#159364),(#159365,#159366),(#159367,#159368),(#159369,#159370),
(#159371,#159372),(#159373,#159374),(#159375,#159376),(#159377,#159378),
(#159379,#159380),(#159381,#159382),(#159383,#159384),(#159385,#159386),
(#159387,#159388),(#159389,#159390),(#159391,#159392),(#159393,#159394),
(#159395,#159396),(#159397,#159398),(#159399,#159400),(#159401,#159402),
(#159403,#159404),(#159405,#159406),(#159407,#159408),(#159409,#159410),
(#159411,#159412),(#159413,#159414),(#159415,#159416),(#159417,#159418),
(#159419,#159420),(#159421,#159422),(#159423,#159424),(#159425,#159426),
(#159427,#159428),(#159429,#159430),(#159431,#159432),(#159433,#159434),
(#159435,#159436),(#159437,#159438),(#159439,#159440),(#159441,#159442),
(#159443,#159444),(#159445,#159446),(#159447,#159448),(#159449,#159450),
(#159451,#159452),(#159453,#159454),(#159455,#159456),(#159457,#159458),
(#159459,#159460),(#159461,#159462),(#159463,#159464),(#159465,#159466),
(#159467,#159468),(#159469,#159470),(#159471,#159472),(#159473,#159474),
(#159475,#159476),(#159477,#159478),(#159479,#159480),(#159481,#159482),
(#159483,#159484),(#159485,#159486),(#159487,#159488),(#159489,#159490),
(#159491,#159492),(#159493,#159494),(#159495,#159496),(#159497,#159498),
(#159499,#159500),(#159501,#159502),(#159503,#159504),(#159505,#159506),
(#159507,#159508),(#159509,#159510),(#159511,#159512),(#159513,#159514),
(#159515,#159516),(#159517,#159518),(#159519,#159520),(#159521,#159522),
(#159523,#159524),(#159525,#159526),(#159527,#159528),(#159529,#159530),
(#159531,#159532),(#159533,#159534),(#159535,#159536),(#159537,#159538),
(#159539,#159540),(#159541,#159542),(#159543,#159544),(#159545,#159546),
(#159547,#159548),(#159549,#159550),(#159551,#159552),(#159553,#159554),
(#159555,#159556),(#159557,#159558),(#159559,#159560),(#159561,#159562),
(#159563,#159564),(#159565,#159566),(#159567,#159568),(#159569,#159570),
(#159571,#159572),(#159573,#159574),(#159575,#159576),(#159577,#159578),
(#159579,#159580),(#159581,#159582),(#159583,#159584),(#159585,#159586),
(#159587,#159588),(#159589,#159590),(#159591,#159592),(#159593,#159594),
(#159595,#159596),(#159597,#159598),(#159599,#159600),(#159601,#159602),
(#159603,#159604),(#159605,#159606),(#159607,#159608),(#159609,#159610),
(#159611,#159612),(#159613,#159614),(#159615,#159616),(#159617,#159618),
(#159619,#159620),(#159621,#159622),(#159623,#159624),(#159625,#159626),
(#159627,#159628),(#159629,#159630),(#159631,#159632),(#159633,#159634),
(#159635,#159636),(#159637,#159638),(#159639,#159640),(#159641,#159642),
(#159643,#159644),(#159645,#159646),(#159647,#159648),(#159649,#159650),
(#159651,#159652),(#159653,#159654),(#159655,#159656),(#159657,#159658),
(#159659,#159660),(#159661,#159662),(#159663,#159664),(#159665,#159666),
(#159667,#159668),(#159669,#159670),(#159671,#159672),(#159673,#159674),
(#159675,#159676),(#159677,#159678),(#159679,#159680),(#159681,#159682),
(#159683,#159684),(#159685,#159686),(#159687,#159688),(#159689,#159690),
(#159691,#159692),(#159693,#159694),(#159695,#159696),(#159697,#159698),
(#159699,#159700),(#159701,#159702),(#159703,#159704),(#159705,#159706),
(#159707,#159708),(#159709,#159710),(#159711,#159712),(#159713,#159714),
(#159715,#159716),(#159717,#159718),(#159719,#159720),(#159721,#159722),
(#159723,#159724),(#159725,#159726),(#159727,#159728),(#159729,#159730),
(#159731,#159732),(#159733,#159734),(#159735,#159736),(#159737,#159738),
(#159739,#159740),(#159741,#159742),(#159743,#159744),(#159745,#159746),
(#159747,#159748),(#159749,#159750),(#159751,#159752),(#159753,#159754),
(#159755,#159756),(#159757,#159758),(#159759,#159760),(#159761,#159762),
(#159763,#159764),(#159765,#159766),(#159767,#159768),(#159769,#159770),
(#159771,#159772),(#159773,#159774),(#159775,#159776),(#159777,#159778),
(#159779,#159780),(#159781,#159782),(#159783,#159784),(#159785,#159786),
(#159787,#159788),(#159789,#159790),(#159791,#159792),(#159793,#159794),
(#159795,#159796),(#159797,#159798),(#159799,#159800),(#159801,#159802),
(#159803,#159804),(#159805,#159806),(#159807,#159808),(#159809,#159810),
(#159811,#159812),(#159813,#159814),(#159815,#159816),(#159817,#159818),
(#159819,#159820),(#159821,#159822),(#159823,#159824),(#159825,#159826),
(#159827,#159828),(#159829,#159830),(#159831,#159832),(#159833,#159834),
(#159835,#159836),(#159837,#159838),(#159839,#159840),(#159841,#159842),
(#159843,#159844),(#159845,#159846),(#159847,#159848),(#159849,#159850),
(#159851,#159852),(#159853,#159854),(#159855,#159856),(#159857,#159858),
(#159859,#159860),(#159861,#159862),(#159863,#159864),(#159865,#159866),
(#159867,#159868),(#159869,#159870)),.UNSPECIFIED.,.F.,.F.,.F.,(6,1,1,1,
1,1,1,1,1,1,1,1,1,1,1,1,1,1,1,1,1,1,1,1,1,1,1,1,1,1,1,1,1,1,1,1,1,1,1,1,
1,1,1,1,1,1,1,1,1,1,1,1,1,1,1,1,1,1,1,1,1,1,1,1,1,1,1,1,1,1,1,1,1,1,1,1,
1,1,1,1,1,1,1,1,1,1,1,1,1,1,1,1,1,1,1,1,1,1,1,1,1,1,1,1,1,1,1,1,1,1,1,1,
1,1,1,1,1,1,1,1,1,1,1,1,1,1,1,1,1,1,1,1,1,1,1,1,1,1,1,1,1,1,1,1,1,1,1,1,
1,1,1,1,1,1,1,1,1,1,1,1,1,1,1,1,1,1,1,1,1,1,1,1,1,1,1,1,1,1,1,1,1,1,1,1,
1,1,1,1,1,1,1,1,1,1,1,1,1,1,1,1,1,1,1,1,1,1,1,1,1,1,1,1,1,1,1,1,1,1,1,1,
1,1,1,1,1,1,1,1,1,1,1,1,1,1,1,1,1,1,1,1,1,1,1,1,1,1,1,1,1,1,1,1,1,1,1,1,
1,1,1,1,1,1,1,1,1,1,1,1,1,1,1,1,1,1,1,1,1,1,1,1,1,1,1,1,1,1,1,1,1,1,1,1,
1,1,1,1,1,1,1,1,1,1,1,1,1,1,1,1,1,1,1,1,1,1,1,1,1,1,1,1,1,1,1,1,1,1,1,1,
1,1,1,1,1,1,1,1,1,1,1,1,1,1,1,1,1,1,1,1,1,1,1,1,1,1,1,1,1,1,1,1,1,1,1,1,
1,1,1,1,1,1,1,1,1,1,1,1,1,1,1,1,1,1,1,1,1,1,1,1,1,1,1,1,1,1,1,1,1,1,1,1,
1,1,1,1,1,1,1,1,1,1,1,1,1,1,1,1,1,1,1,1,1,1,1,1,1,1,1,1,1,1,1,1,1,1,1,1,
1,1,1,1,1,1,1,1,1,1,1,1,1,1,1,1,1,1,1,1,1,1,1,1,1,1,1,1,1,1,1,6),(2,2),
(0.143172103,0.144954128,0.146788991,0.148623853,0.150458716,0.152293578,
0.15412844,0.155963303,0.157798165,0.159633028,0.16146789,0.163302752,0.165137615,
0.166972477,0.168807339,0.170642202,0.172477064,0.174311927,0.176146789,
0.177981651,0.179816514,0.181651376,0.183486239,0.185321101,0.187155963,
0.188990826,0.190825688,0.19266055,0.194495413,0.196330275,0.198165138,
0.2,0.201834862,0.203669725,0.205504587,0.20733945,0.209174312,0.211009174,
0.212844037,0.214678899,0.216513761,0.218348624,0.220183486,0.222018349,
0.223853211,0.225688073,0.227522936,0.229357798,0.231192661,0.233027523,
0.234862385,0.236697248,0.23853211,0.240366972,0.242201835,0.244036697,
0.24587156,0.247706422,0.249541284,0.251376147,0.253211009,0.255045872,
0.256880734,0.258715596,0.260550459,0.262385321,0.264220183,0.266055046,
0.267889908,0.269724771,0.271559633,0.273394495,0.275229358,0.27706422,
0.278899083,0.280733945,0.282568807,0.28440367,0.286238532,0.288073394,
0.289908257,0.291743119,0.293577982,0.295412844,0.297247706,0.299082569,
0.300917431,0.302752294,0.304587156,0.306422018,0.308256881,0.310091743,
0.311926606,0.313761468,0.31559633,0.317431193,0.319266055,0.321100917,
0.32293578,0.324770642,0.326605505,0.328440367,0.330275229,0.332110092,
0.333944954,0.335779817,0.337614679,0.339449541,0.341284404,0.343119266,
0.344954128,0.346788991,0.348623853,0.350458716,0.352293578,0.35412844,
0.355963303,0.357798165,0.359633028,0.36146789,0.363302752,0.365137615,
0.366972477,0.368807339,0.370642202,0.372477064,0.374311927,0.376146789,
0.377981651,0.379816514,0.381651376,0.383486239,0.385321101,0.387155963,
0.388990826,0.390825688,0.39266055,0.394495413,0.396330275,0.398165138,
0.4,0.401834862,0.403669725,0.405504587,0.40733945,0.409174312,0.411009174,
0.412844037,0.414678899,0.416513761,0.418348624,0.420183486,0.422018349,
0.423853211,0.425688073,0.427522936,0.429357798,0.431192661,0.433027523,
0.434862385,0.436697248,0.43853211,0.440366972,0.442201835,0.444036697,
0.44587156,0.447706422,0.449541284,0.451376147,0.453211009,0.455045872,
0.456880734,0.458715596,0.460550459,0.462385321,0.464220183,0.466055046,
0.467889908,0.469724771,0.471559633,0.473394495,0.475229358,0.47706422,
0.478899083,0.480733945,0.482568807,0.48440367,0.486238532,0.488073394,
0.489908257,0.491743119,0.493577982,0.495412844,0.497247706,0.499082569,
0.500917431,0.502752294,0.504587156,0.506422018,0.508256881,0.510091743,
0.511926606,0.513761468,0.51559633,0.517431193,0.519266055,0.521100917,
0.52293578,0.524770642,0.526605505,0.528440367,0.530275229,0.532110092,
0.533944954,0.535779817,0.537614679,0.539449541,0.541284404,0.543119266,
0.544954128,0.546788991,0.548623853,0.550458716,0.552293578,0.55412844,
0.555963303,0.557798165,0.559633028,0.56146789,0.563302752,0.565137615,
0.566972477,0.568807339,0.570642202,0.572477064,0.574311927,0.576146789,
0.577981651,0.579816514,0.581651376,0.583486239,0.585321101,0.587155963,
0.588990826,0.590825688,0.59266055,0.594495413,0.596330275,0.598165138,
0.6,0.601834862,0.603669725,0.605504587,0.60733945,0.609174312,0.611009174,
0.612844037,0.614678899,0.616513761,0.618348624,0.620183486,0.622018349,
0.623853211,0.625688073,0.627522936,0.629357798,0.631192661,0.633027523,
0.634862385,0.636697248,0.63853211,0.640366972,0.642201835,0.644036697,
0.64587156,0.647706422,0.649541284,0.651376147,0.653211009,0.655045872,
0.656880734,0.658715596,0.660550459,0.662385321,0.664220183,0.666055046,
0.667889908,0.669724771,0.671559633,0.673394495,0.675229358,0.67706422,
0.678899083,0.680733945,0.682568807,0.68440367,0.686238532,0.688073394,
0.689908257,0.691743119,0.693577982,0.695412844,0.697247706,0.699082569,
0.700917431,0.702752294,0.704587156,0.706422018,0.708256881,0.710091743,
0.711926606,0.713761468,0.71559633,0.717431193,0.719266055,0.721100917,
0.72293578,0.724770642,0.726605505,0.728440367,0.730275229,0.732110092,
0.733944954,0.735779817,0.737614679,0.739449541,0.741284404,0.743119266,
0.744954128,0.746788991,0.748623853,0.750458716,0.752293578,0.75412844,
0.755963303,0.757798165,0.759633028,0.76146789,0.763302752,0.765137615,
0.766972477,0.768807339,0.770642202,0.772477064,0.774311927,0.776146789,
0.777981651,0.779816514,0.781651376,0.783486239,0.785321101,0.787155963,
0.788990826,0.790825688,0.79266055,0.794495413,0.796330275,0.798165138,
0.8,0.801834862,0.803669725,0.805504587,0.80733945,0.809174312,0.811009174,
0.812844037,0.814678899,0.816513761,0.818348624,0.820183486,0.822018349,
0.823853211,0.825688073,0.827522936,0.829357798,0.831192661,0.833027523,
0.834862385,0.836697248,0.83853211,0.840366972,0.842201835,0.844036697,
0.84587156,0.847706422,0.849541284,0.851376147,0.853211009,0.855045872,
0.856880734,0.858715596,0.860550459,0.862385321,0.864220183,0.866055046,
0.867889908,0.869724771,0.871559633,0.873394495,0.875229358,0.87706422,
0.878899083,0.880733945,0.882568807,0.88440367,0.886238532,0.888073394,
0.889908257,0.891743119,0.893577982,0.895412844,0.897247706,0.899082569,
0.900917431,0.902752294,0.904587156,0.906422018,0.908256881,0.910091743,
0.911926606,0.913761468,0.91559633,0.917431193,0.919266055,0.921100917,
0.92293578,0.924770642,0.926605505,0.928440367,0.930275229,0.932110092,
0.933944954,0.935779817,0.937614679,0.939449541,0.941284404,0.943119266,
0.944954128,0.946788991,0.948623853,0.950458716,0.952293578,0.95412844,
0.955963303,0.957798165,0.959633028,0.96146789,0.963302752,0.965137615,
0.966972477,0.968807339,0.970642202,0.972477064,0.974311927,0.976146789,
0.977981651,0.979816514,0.981651376,0.983486239,0.985321101,0.987155963,
0.988990826,0.990825688,0.99266055,0.994495413,0.996330275,0.998165138,
1.),(0.,0.36),.UNSPECIFIED.);
#6219=B_SPLINE_SURFACE_WITH_KNOTS('',5,1,((#160830,#160831),(#160832,#160833),
(#160834,#160835),(#160836,#160837),(#160838,#160839),(#160840,#160841),
(#160842,#160843),(#160844,#160845),(#160846,#160847),(#160848,#160849),
(#160850,#160851),(#160852,#160853),(#160854,#160855),(#160856,#160857),
(#160858,#160859),(#160860,#160861),(#160862,#160863),(#160864,#160865),
(#160866,#160867),(#160868,#160869),(#160870,#160871),(#160872,#160873),
(#160874,#160875),(#160876,#160877),(#160878,#160879),(#160880,#160881),
(#160882,#160883),(#160884,#160885),(#160886,#160887),(#160888,#160889),
(#160890,#160891),(#160892,#160893),(#160894,#160895),(#160896,#160897),
(#160898,#160899),(#160900,#160901),(#160902,#160903),(#160904,#160905),
(#160906,#160907),(#160908,#160909),(#160910,#160911),(#160912,#160913),
(#160914,#160915),(#160916,#160917),(#160918,#160919),(#160920,#160921),
(#160922,#160923),(#160924,#160925),(#160926,#160927),(#160928,#160929),
(#160930,#160931),(#160932,#160933),(#160934,#160935),(#160936,#160937),
(#160938,#160939),(#160940,#160941),(#160942,#160943),(#160944,#160945),
(#160946,#160947),(#160948,#160949),(#160950,#160951),(#160952,#160953),
(#160954,#160955),(#160956,#160957),(#160958,#160959),(#160960,#160961),
(#160962,#160963),(#160964,#160965),(#160966,#160967),(#160968,#160969),
(#160970,#160971),(#160972,#160973),(#160974,#160975),(#160976,#160977),
(#160978,#160979),(#160980,#160981),(#160982,#160983),(#160984,#160985),
(#160986,#160987),(#160988,#160989),(#160990,#160991),(#160992,#160993),
(#160994,#160995),(#160996,#160997),(#160998,#160999),(#161000,#161001),
(#161002,#161003),(#161004,#161005),(#161006,#161007),(#161008,#161009),
(#161010,#161011),(#161012,#161013),(#161014,#161015),(#161016,#161017),
(#161018,#161019),(#161020,#161021),(#161022,#161023),(#161024,#161025),
(#161026,#161027),(#161028,#161029),(#161030,#161031),(#161032,#161033),
(#161034,#161035),(#161036,#161037),(#161038,#161039),(#161040,#161041),
(#161042,#161043),(#161044,#161045),(#161046,#161047),(#161048,#161049),
(#161050,#161051),(#161052,#161053),(#161054,#161055),(#161056,#161057),
(#161058,#161059),(#161060,#161061),(#161062,#161063),(#161064,#161065),
(#161066,#161067),(#161068,#161069),(#161070,#161071),(#161072,#161073),
(#161074,#161075),(#161076,#161077),(#161078,#161079),(#161080,#161081),
(#161082,#161083),(#161084,#161085),(#161086,#161087),(#161088,#161089),
(#161090,#161091),(#161092,#161093),(#161094,#161095),(#161096,#161097),
(#161098,#161099),(#161100,#161101),(#161102,#161103),(#161104,#161105),
(#161106,#161107),(#161108,#161109),(#161110,#161111),(#161112,#161113),
(#161114,#161115),(#161116,#161117),(#161118,#161119),(#161120,#161121),
(#161122,#161123),(#161124,#161125),(#161126,#161127),(#161128,#161129),
(#161130,#161131),(#161132,#161133),(#161134,#161135),(#161136,#161137),
(#161138,#161139),(#161140,#161141),(#161142,#161143),(#161144,#161145),
(#161146,#161147),(#161148,#161149),(#161150,#161151),(#161152,#161153),
(#161154,#161155),(#161156,#161157),(#161158,#161159),(#161160,#161161),
(#161162,#161163),(#161164,#161165),(#161166,#161167),(#161168,#161169),
(#161170,#161171),(#161172,#161173),(#161174,#161175),(#161176,#161177),
(#161178,#161179),(#161180,#161181),(#161182,#161183),(#161184,#161185),
(#161186,#161187),(#161188,#161189),(#161190,#161191),(#161192,#161193),
(#161194,#161195),(#161196,#161197),(#161198,#161199),(#161200,#161201),
(#161202,#161203),(#161204,#161205),(#161206,#161207),(#161208,#161209),
(#161210,#161211),(#161212,#161213),(#161214,#161215),(#161216,#161217),
(#161218,#161219),(#161220,#161221),(#161222,#161223),(#161224,#161225),
(#161226,#161227),(#161228,#161229),(#161230,#161231),(#161232,#161233),
(#161234,#161235),(#161236,#161237),(#161238,#161239),(#161240,#161241),
(#161242,#161243),(#161244,#161245),(#161246,#161247),(#161248,#161249),
(#161250,#161251),(#161252,#161253),(#161254,#161255),(#161256,#161257),
(#161258,#161259),(#161260,#161261),(#161262,#161263),(#161264,#161265),
(#161266,#161267),(#161268,#161269),(#161270,#161271),(#161272,#161273),
(#161274,#161275),(#161276,#161277),(#161278,#161279),(#161280,#161281),
(#161282,#161283),(#161284,#161285),(#161286,#161287),(#161288,#161289),
(#161290,#161291),(#161292,#161293),(#161294,#161295),(#161296,#161297),
(#161298,#161299),(#161300,#161301),(#161302,#161303),(#161304,#161305),
(#161306,#161307),(#161308,#161309),(#161310,#161311),(#161312,#161313),
(#161314,#161315),(#161316,#161317),(#161318,#161319),(#161320,#161321),
(#161322,#161323),(#161324,#161325),(#161326,#161327),(#161328,#161329),
(#161330,#161331),(#161332,#161333),(#161334,#161335),(#161336,#161337),
(#161338,#161339),(#161340,#161341),(#161342,#161343),(#161344,#161345),
(#161346,#161347),(#161348,#161349),(#161350,#161351),(#161352,#161353),
(#161354,#161355),(#161356,#161357),(#161358,#161359),(#161360,#161361),
(#161362,#161363),(#161364,#161365),(#161366,#161367),(#161368,#161369),
(#161370,#161371),(#161372,#161373),(#161374,#161375),(#161376,#161377),
(#161378,#161379),(#161380,#161381),(#161382,#161383),(#161384,#161385),
(#161386,#161387),(#161388,#161389),(#161390,#161391),(#161392,#161393),
(#161394,#161395),(#161396,#161397),(#161398,#161399),(#161400,#161401),
(#161402,#161403),(#161404,#161405),(#161406,#161407),(#161408,#161409),
(#161410,#161411),(#161412,#161413),(#161414,#161415),(#161416,#161417),
(#161418,#161419),(#161420,#161421),(#161422,#161423),(#161424,#161425),
(#161426,#161427),(#161428,#161429),(#161430,#161431),(#161432,#161433),
(#161434,#161435),(#161436,#161437),(#161438,#161439),(#161440,#161441),
(#161442,#161443),(#161444,#161445),(#161446,#161447),(#161448,#161449),
(#161450,#161451),(#161452,#161453),(#161454,#161455),(#161456,#161457),
(#161458,#161459),(#161460,#161461),(#161462,#161463),(#161464,#161465),
(#161466,#161467),(#161468,#161469),(#161470,#161471),(#161472,#161473),
(#161474,#161475),(#161476,#161477),(#161478,#161479),(#161480,#161481),
(#161482,#161483),(#161484,#161485),(#161486,#161487),(#161488,#161489),
(#161490,#161491),(#161492,#161493),(#161494,#161495),(#161496,#161497),
(#161498,#161499),(#161500,#161501),(#161502,#161503),(#161504,#161505),
(#161506,#161507),(#161508,#161509),(#161510,#161511),(#161512,#161513),
(#161514,#161515),(#161516,#161517),(#161518,#161519),(#161520,#161521),
(#161522,#161523),(#161524,#161525),(#161526,#161527),(#161528,#161529),
(#161530,#161531),(#161532,#161533),(#161534,#161535),(#161536,#161537),
(#161538,#161539),(#161540,#161541),(#161542,#161543),(#161544,#161545),
(#161546,#161547),(#161548,#161549),(#161550,#161551),(#161552,#161553),
(#161554,#161555),(#161556,#161557),(#161558,#161559),(#161560,#161561),
(#161562,#161563),(#161564,#161565),(#161566,#161567),(#161568,#161569),
(#161570,#161571),(#161572,#161573),(#161574,#161575),(#161576,#161577),
(#161578,#161579),(#161580,#161581),(#161582,#161583),(#161584,#161585),
(#161586,#161587),(#161588,#161589),(#161590,#161591),(#161592,#161593),
(#161594,#161595),(#161596,#161597),(#161598,#161599),(#161600,#161601),
(#161602,#161603),(#161604,#161605),(#161606,#161607),(#161608,#161609),
(#161610,#161611),(#161612,#161613),(#161614,#161615),(#161616,#161617),
(#161618,#161619),(#161620,#161621),(#161622,#161623),(#161624,#161625),
(#161626,#161627),(#161628,#161629),(#161630,#161631),(#161632,#161633),
(#161634,#161635),(#161636,#161637),(#161638,#161639),(#161640,#161641),
(#161642,#161643),(#161644,#161645),(#161646,#161647),(#161648,#161649),
(#161650,#161651),(#161652,#161653),(#161654,#161655),(#161656,#161657),
(#161658,#161659),(#161660,#161661),(#161662,#161663),(#161664,#161665),
(#161666,#161667),(#161668,#161669),(#161670,#161671),(#161672,#161673),
(#161674,#161675),(#161676,#161677),(#161678,#161679),(#161680,#161681),
(#161682,#161683),(#161684,#161685),(#161686,#161687),(#161688,#161689),
(#161690,#161691),(#161692,#161693),(#161694,#161695),(#161696,#161697),
(#161698,#161699),(#161700,#161701),(#161702,#161703),(#161704,#161705),
(#161706,#161707),(#161708,#161709),(#161710,#161711),(#161712,#161713),
(#161714,#161715),(#161716,#161717),(#161718,#161719),(#161720,#161721),
(#161722,#161723),(#161724,#161725),(#161726,#161727),(#161728,#161729),
(#161730,#161731),(#161732,#161733),(#161734,#161735),(#161736,#161737),
(#161738,#161739),(#161740,#161741),(#161742,#161743),(#161744,#161745),
(#161746,#161747),(#161748,#161749),(#161750,#161751),(#161752,#161753),
(#161754,#161755),(#161756,#161757),(#161758,#161759),(#161760,#161761),
(#161762,#161763),(#161764,#161765),(#161766,#161767),(#161768,#161769),
(#161770,#161771),(#161772,#161773)),.UNSPECIFIED.,.F.,.F.,.F.,(6,1,1,1,
1,1,1,1,1,1,1,1,1,1,1,1,1,1,1,1,1,1,1,1,1,1,1,1,1,1,1,1,1,1,1,1,1,1,1,1,
1,1,1,1,1,1,1,1,1,1,1,1,1,1,1,1,1,1,1,1,1,1,1,1,1,1,1,1,1,1,1,1,1,1,1,1,
1,1,1,1,1,1,1,1,1,1,1,1,1,1,1,1,1,1,1,1,1,1,1,1,1,1,1,1,1,1,1,1,1,1,1,1,
1,1,1,1,1,1,1,1,1,1,1,1,1,1,1,1,1,1,1,1,1,1,1,1,1,1,1,1,1,1,1,1,1,1,1,1,
1,1,1,1,1,1,1,1,1,1,1,1,1,1,1,1,1,1,1,1,1,1,1,1,1,1,1,1,1,1,1,1,1,1,1,1,
1,1,1,1,1,1,1,1,1,1,1,1,1,1,1,1,1,1,1,1,1,1,1,1,1,1,1,1,1,1,1,1,1,1,1,1,
1,1,1,1,1,1,1,1,1,1,1,1,1,1,1,1,1,1,1,1,1,1,1,1,1,1,1,1,1,1,1,1,1,1,1,1,
1,1,1,1,1,1,1,1,1,1,1,1,1,1,1,1,1,1,1,1,1,1,1,1,1,1,1,1,1,1,1,1,1,1,1,1,
1,1,1,1,1,1,1,1,1,1,1,1,1,1,1,1,1,1,1,1,1,1,1,1,1,1,1,1,1,1,1,1,1,1,1,1,
1,1,1,1,1,1,1,1,1,1,1,1,1,1,1,1,1,1,1,1,1,1,1,1,1,1,1,1,1,1,1,1,1,1,1,1,
1,1,1,1,1,1,1,1,1,1,1,1,1,1,1,1,1,1,1,1,1,1,1,1,1,1,1,1,1,1,1,1,1,1,1,1,
1,1,1,1,1,1,1,1,1,1,1,1,1,1,1,1,1,1,1,1,1,1,1,1,1,1,1,1,1,1,1,1,1,1,1,1,
1,1,1,1,1,1,1,1,1,1,1,1,1,1,1,1,1,1,1,1,1,1,1,1,1,1,1,1,1,1,1,6),(2,2),
(0.143172103,0.144954128,0.146788991,0.148623853,0.150458716,0.152293578,
0.15412844,0.155963303,0.157798165,0.159633028,0.16146789,0.163302752,0.165137615,
0.166972477,0.168807339,0.170642202,0.172477064,0.174311927,0.176146789,
0.177981651,0.179816514,0.181651376,0.183486239,0.185321101,0.187155963,
0.188990826,0.190825688,0.19266055,0.194495413,0.196330275,0.198165138,
0.2,0.201834862,0.203669725,0.205504587,0.20733945,0.209174312,0.211009174,
0.212844037,0.214678899,0.216513761,0.218348624,0.220183486,0.222018349,
0.223853211,0.225688073,0.227522936,0.229357798,0.231192661,0.233027523,
0.234862385,0.236697248,0.23853211,0.240366972,0.242201835,0.244036697,
0.24587156,0.247706422,0.249541284,0.251376147,0.253211009,0.255045872,
0.256880734,0.258715596,0.260550459,0.262385321,0.264220183,0.266055046,
0.267889908,0.269724771,0.271559633,0.273394495,0.275229358,0.27706422,
0.278899083,0.280733945,0.282568807,0.28440367,0.286238532,0.288073394,
0.289908257,0.291743119,0.293577982,0.295412844,0.297247706,0.299082569,
0.300917431,0.302752294,0.304587156,0.306422018,0.308256881,0.310091743,
0.311926606,0.313761468,0.31559633,0.317431193,0.319266055,0.321100917,
0.32293578,0.324770642,0.326605505,0.328440367,0.330275229,0.332110092,
0.333944954,0.335779817,0.337614679,0.339449541,0.341284404,0.343119266,
0.344954128,0.346788991,0.348623853,0.350458716,0.352293578,0.35412844,
0.355963303,0.357798165,0.359633028,0.36146789,0.363302752,0.365137615,
0.366972477,0.368807339,0.370642202,0.372477064,0.374311927,0.376146789,
0.377981651,0.379816514,0.381651376,0.383486239,0.385321101,0.387155963,
0.388990826,0.390825688,0.39266055,0.394495413,0.396330275,0.398165138,
0.4,0.401834862,0.403669725,0.405504587,0.40733945,0.409174312,0.411009174,
0.412844037,0.414678899,0.416513761,0.418348624,0.420183486,0.422018349,
0.423853211,0.425688073,0.427522936,0.429357798,0.431192661,0.433027523,
0.434862385,0.436697248,0.43853211,0.440366972,0.442201835,0.444036697,
0.44587156,0.447706422,0.449541284,0.451376147,0.453211009,0.455045872,
0.456880734,0.458715596,0.460550459,0.462385321,0.464220183,0.466055046,
0.467889908,0.469724771,0.471559633,0.473394495,0.475229358,0.47706422,
0.478899083,0.480733945,0.482568807,0.48440367,0.486238532,0.488073394,
0.489908257,0.491743119,0.493577982,0.495412844,0.497247706,0.499082569,
0.500917431,0.502752294,0.504587156,0.506422018,0.508256881,0.510091743,
0.511926606,0.513761468,0.51559633,0.517431193,0.519266055,0.521100917,
0.52293578,0.524770642,0.526605505,0.528440367,0.530275229,0.532110092,
0.533944954,0.535779817,0.537614679,0.539449541,0.541284404,0.543119266,
0.544954128,0.546788991,0.548623853,0.550458716,0.552293578,0.55412844,
0.555963303,0.557798165,0.559633028,0.56146789,0.563302752,0.565137615,
0.566972477,0.568807339,0.570642202,0.572477064,0.574311927,0.576146789,
0.577981651,0.579816514,0.581651376,0.583486239,0.585321101,0.587155963,
0.588990826,0.590825688,0.59266055,0.594495413,0.596330275,0.598165138,
0.6,0.601834862,0.603669725,0.605504587,0.60733945,0.609174312,0.611009174,
0.612844037,0.614678899,0.616513761,0.618348624,0.620183486,0.622018349,
0.623853211,0.625688073,0.627522936,0.629357798,0.631192661,0.633027523,
0.634862385,0.636697248,0.63853211,0.640366972,0.642201835,0.644036697,
0.64587156,0.647706422,0.649541284,0.651376147,0.653211009,0.655045872,
0.656880734,0.658715596,0.660550459,0.662385321,0.664220183,0.666055046,
0.667889908,0.669724771,0.671559633,0.673394495,0.675229358,0.67706422,
0.678899083,0.680733945,0.682568807,0.68440367,0.686238532,0.688073394,
0.689908257,0.691743119,0.693577982,0.695412844,0.697247706,0.699082569,
0.700917431,0.702752294,0.704587156,0.706422018,0.708256881,0.710091743,
0.711926606,0.713761468,0.71559633,0.717431193,0.719266055,0.721100917,
0.72293578,0.724770642,0.726605505,0.728440367,0.730275229,0.732110092,
0.733944954,0.735779817,0.737614679,0.739449541,0.741284404,0.743119266,
0.744954128,0.746788991,0.748623853,0.750458716,0.752293578,0.75412844,
0.755963303,0.757798165,0.759633028,0.76146789,0.763302752,0.765137615,
0.766972477,0.768807339,0.770642202,0.772477064,0.774311927,0.776146789,
0.777981651,0.779816514,0.781651376,0.783486239,0.785321101,0.787155963,
0.788990826,0.790825688,0.79266055,0.794495413,0.796330275,0.798165138,
0.8,0.801834862,0.803669725,0.805504587,0.80733945,0.809174312,0.811009174,
0.812844037,0.814678899,0.816513761,0.818348624,0.820183486,0.822018349,
0.823853211,0.825688073,0.827522936,0.829357798,0.831192661,0.833027523,
0.834862385,0.836697248,0.83853211,0.840366972,0.842201835,0.844036697,
0.84587156,0.847706422,0.849541284,0.851376147,0.853211009,0.855045872,
0.856880734,0.858715596,0.860550459,0.862385321,0.864220183,0.866055046,
0.867889908,0.869724771,0.871559633,0.873394495,0.875229358,0.87706422,
0.878899083,0.880733945,0.882568807,0.88440367,0.886238532,0.888073394,
0.889908257,0.891743119,0.893577982,0.895412844,0.897247706,0.899082569,
0.900917431,0.902752294,0.904587156,0.906422018,0.908256881,0.910091743,
0.911926606,0.913761468,0.91559633,0.917431193,0.919266055,0.921100917,
0.92293578,0.924770642,0.926605505,0.928440367,0.930275229,0.932110092,
0.933944954,0.935779817,0.937614679,0.939449541,0.941284404,0.943119266,
0.944954128,0.946788991,0.948623853,0.950458716,0.952293578,0.95412844,
0.955963303,0.957798165,0.959633028,0.96146789,0.963302752,0.965137615,
0.966972477,0.968807339,0.970642202,0.972477064,0.974311927,0.976146789,
0.977981651,0.979816514,0.981651376,0.983486239,0.985321101,0.987155963,
0.988990826,0.990825688,0.99266055,0.994495413,0.996330275,0.998165138,
1.),(0.,0.36),.UNSPECIFIED.);
#6220=B_SPLINE_SURFACE_WITH_KNOTS('',5,1,((#162430,#162431),(#162432,#162433),
(#162434,#162435),(#162436,#162437),(#162438,#162439),(#162440,#162441),
(#162442,#162443),(#162444,#162445),(#162446,#162447),(#162448,#162449),
(#162450,#162451),(#162452,#162453),(#162454,#162455),(#162456,#162457),
(#162458,#162459),(#162460,#162461),(#162462,#162463),(#162464,#162465),
(#162466,#162467),(#162468,#162469),(#162470,#162471),(#162472,#162473),
(#162474,#162475),(#162476,#162477),(#162478,#162479),(#162480,#162481),
(#162482,#162483),(#162484,#162485),(#162486,#162487),(#162488,#162489),
(#162490,#162491),(#162492,#162493),(#162494,#162495),(#162496,#162497),
(#162498,#162499),(#162500,#162501),(#162502,#162503),(#162504,#162505),
(#162506,#162507),(#162508,#162509),(#162510,#162511),(#162512,#162513),
(#162514,#162515),(#162516,#162517),(#162518,#162519),(#162520,#162521),
(#162522,#162523),(#162524,#162525),(#162526,#162527),(#162528,#162529),
(#162530,#162531),(#162532,#162533),(#162534,#162535),(#162536,#162537),
(#162538,#162539),(#162540,#162541),(#162542,#162543),(#162544,#162545),
(#162546,#162547),(#162548,#162549),(#162550,#162551),(#162552,#162553),
(#162554,#162555),(#162556,#162557),(#162558,#162559),(#162560,#162561),
(#162562,#162563),(#162564,#162565),(#162566,#162567),(#162568,#162569),
(#162570,#162571),(#162572,#162573),(#162574,#162575),(#162576,#162577),
(#162578,#162579),(#162580,#162581),(#162582,#162583),(#162584,#162585),
(#162586,#162587),(#162588,#162589),(#162590,#162591),(#162592,#162593),
(#162594,#162595),(#162596,#162597),(#162598,#162599),(#162600,#162601),
(#162602,#162603),(#162604,#162605),(#162606,#162607),(#162608,#162609),
(#162610,#162611),(#162612,#162613),(#162614,#162615),(#162616,#162617),
(#162618,#162619),(#162620,#162621),(#162622,#162623),(#162624,#162625),
(#162626,#162627),(#162628,#162629),(#162630,#162631),(#162632,#162633),
(#162634,#162635),(#162636,#162637),(#162638,#162639),(#162640,#162641),
(#162642,#162643),(#162644,#162645),(#162646,#162647),(#162648,#162649),
(#162650,#162651),(#162652,#162653),(#162654,#162655),(#162656,#162657),
(#162658,#162659),(#162660,#162661),(#162662,#162663),(#162664,#162665),
(#162666,#162667),(#162668,#162669),(#162670,#162671),(#162672,#162673),
(#162674,#162675),(#162676,#162677),(#162678,#162679),(#162680,#162681),
(#162682,#162683),(#162684,#162685),(#162686,#162687),(#162688,#162689),
(#162690,#162691),(#162692,#162693),(#162694,#162695),(#162696,#162697),
(#162698,#162699),(#162700,#162701),(#162702,#162703),(#162704,#162705),
(#162706,#162707),(#162708,#162709),(#162710,#162711),(#162712,#162713),
(#162714,#162715),(#162716,#162717),(#162718,#162719),(#162720,#162721),
(#162722,#162723),(#162724,#162725),(#162726,#162727),(#162728,#162729),
(#162730,#162731),(#162732,#162733),(#162734,#162735),(#162736,#162737),
(#162738,#162739),(#162740,#162741),(#162742,#162743),(#162744,#162745),
(#162746,#162747),(#162748,#162749),(#162750,#162751),(#162752,#162753),
(#162754,#162755),(#162756,#162757),(#162758,#162759),(#162760,#162761),
(#162762,#162763),(#162764,#162765),(#162766,#162767),(#162768,#162769),
(#162770,#162771),(#162772,#162773),(#162774,#162775),(#162776,#162777),
(#162778,#162779),(#162780,#162781),(#162782,#162783),(#162784,#162785),
(#162786,#162787),(#162788,#162789),(#162790,#162791),(#162792,#162793),
(#162794,#162795),(#162796,#162797),(#162798,#162799),(#162800,#162801),
(#162802,#162803),(#162804,#162805),(#162806,#162807),(#162808,#162809),
(#162810,#162811),(#162812,#162813),(#162814,#162815),(#162816,#162817),
(#162818,#162819),(#162820,#162821),(#162822,#162823),(#162824,#162825),
(#162826,#162827),(#162828,#162829),(#162830,#162831),(#162832,#162833),
(#162834,#162835),(#162836,#162837),(#162838,#162839),(#162840,#162841),
(#162842,#162843),(#162844,#162845),(#162846,#162847),(#162848,#162849),
(#162850,#162851),(#162852,#162853),(#162854,#162855),(#162856,#162857),
(#162858,#162859),(#162860,#162861),(#162862,#162863),(#162864,#162865),
(#162866,#162867),(#162868,#162869),(#162870,#162871),(#162872,#162873),
(#162874,#162875),(#162876,#162877),(#162878,#162879),(#162880,#162881),
(#162882,#162883),(#162884,#162885),(#162886,#162887),(#162888,#162889),
(#162890,#162891),(#162892,#162893),(#162894,#162895),(#162896,#162897),
(#162898,#162899),(#162900,#162901),(#162902,#162903),(#162904,#162905),
(#162906,#162907),(#162908,#162909),(#162910,#162911),(#162912,#162913),
(#162914,#162915),(#162916,#162917),(#162918,#162919),(#162920,#162921),
(#162922,#162923),(#162924,#162925),(#162926,#162927),(#162928,#162929),
(#162930,#162931),(#162932,#162933),(#162934,#162935),(#162936,#162937),
(#162938,#162939),(#162940,#162941),(#162942,#162943),(#162944,#162945),
(#162946,#162947),(#162948,#162949),(#162950,#162951),(#162952,#162953),
(#162954,#162955),(#162956,#162957),(#162958,#162959),(#162960,#162961),
(#162962,#162963),(#162964,#162965),(#162966,#162967),(#162968,#162969),
(#162970,#162971),(#162972,#162973),(#162974,#162975),(#162976,#162977),
(#162978,#162979),(#162980,#162981),(#162982,#162983),(#162984,#162985),
(#162986,#162987),(#162988,#162989),(#162990,#162991),(#162992,#162993),
(#162994,#162995),(#162996,#162997),(#162998,#162999),(#163000,#163001),
(#163002,#163003),(#163004,#163005),(#163006,#163007),(#163008,#163009),
(#163010,#163011),(#163012,#163013),(#163014,#163015),(#163016,#163017),
(#163018,#163019),(#163020,#163021),(#163022,#163023),(#163024,#163025),
(#163026,#163027),(#163028,#163029),(#163030,#163031),(#163032,#163033),
(#163034,#163035),(#163036,#163037),(#163038,#163039),(#163040,#163041),
(#163042,#163043),(#163044,#163045),(#163046,#163047),(#163048,#163049),
(#163050,#163051),(#163052,#163053),(#163054,#163055),(#163056,#163057),
(#163058,#163059),(#163060,#163061),(#163062,#163063),(#163064,#163065),
(#163066,#163067),(#163068,#163069),(#163070,#163071),(#163072,#163073),
(#163074,#163075),(#163076,#163077),(#163078,#163079),(#163080,#163081),
(#163082,#163083),(#163084,#163085),(#163086,#163087),(#163088,#163089),
(#163090,#163091),(#163092,#163093),(#163094,#163095),(#163096,#163097),
(#163098,#163099),(#163100,#163101),(#163102,#163103),(#163104,#163105),
(#163106,#163107),(#163108,#163109),(#163110,#163111),(#163112,#163113),
(#163114,#163115),(#163116,#163117),(#163118,#163119),(#163120,#163121),
(#163122,#163123),(#163124,#163125),(#163126,#163127),(#163128,#163129),
(#163130,#163131),(#163132,#163133),(#163134,#163135),(#163136,#163137),
(#163138,#163139),(#163140,#163141),(#163142,#163143),(#163144,#163145),
(#163146,#163147),(#163148,#163149),(#163150,#163151),(#163152,#163153),
(#163154,#163155),(#163156,#163157),(#163158,#163159),(#163160,#163161),
(#163162,#163163),(#163164,#163165),(#163166,#163167),(#163168,#163169),
(#163170,#163171),(#163172,#163173),(#163174,#163175),(#163176,#163177),
(#163178,#163179),(#163180,#163181),(#163182,#163183),(#163184,#163185),
(#163186,#163187),(#163188,#163189),(#163190,#163191),(#163192,#163193),
(#163194,#163195),(#163196,#163197),(#163198,#163199),(#163200,#163201),
(#163202,#163203),(#163204,#163205),(#163206,#163207),(#163208,#163209),
(#163210,#163211),(#163212,#163213),(#163214,#163215),(#163216,#163217),
(#163218,#163219),(#163220,#163221),(#163222,#163223),(#163224,#163225),
(#163226,#163227),(#163228,#163229),(#163230,#163231),(#163232,#163233),
(#163234,#163235),(#163236,#163237),(#163238,#163239),(#163240,#163241),
(#163242,#163243),(#163244,#163245),(#163246,#163247),(#163248,#163249),
(#163250,#163251),(#163252,#163253),(#163254,#163255),(#163256,#163257),
(#163258,#163259),(#163260,#163261),(#163262,#163263),(#163264,#163265),
(#163266,#163267),(#163268,#163269),(#163270,#163271),(#163272,#163273),
(#163274,#163275),(#163276,#163277),(#163278,#163279),(#163280,#163281),
(#163282,#163283),(#163284,#163285),(#163286,#163287),(#163288,#163289),
(#163290,#163291),(#163292,#163293),(#163294,#163295),(#163296,#163297),
(#163298,#163299),(#163300,#163301),(#163302,#163303),(#163304,#163305),
(#163306,#163307),(#163308,#163309),(#163310,#163311),(#163312,#163313),
(#163314,#163315),(#163316,#163317),(#163318,#163319),(#163320,#163321),
(#163322,#163323),(#163324,#163325),(#163326,#163327),(#163328,#163329),
(#163330,#163331),(#163332,#163333),(#163334,#163335),(#163336,#163337),
(#163338,#163339),(#163340,#163341),(#163342,#163343),(#163344,#163345),
(#163346,#163347),(#163348,#163349),(#163350,#163351),(#163352,#163353),
(#163354,#163355),(#163356,#163357),(#163358,#163359),(#163360,#163361),
(#163362,#163363),(#163364,#163365),(#163366,#163367),(#163368,#163369),
(#163370,#163371),(#163372,#163373)),.UNSPECIFIED.,.F.,.F.,.F.,(6,1,1,1,
1,1,1,1,1,1,1,1,1,1,1,1,1,1,1,1,1,1,1,1,1,1,1,1,1,1,1,1,1,1,1,1,1,1,1,1,
1,1,1,1,1,1,1,1,1,1,1,1,1,1,1,1,1,1,1,1,1,1,1,1,1,1,1,1,1,1,1,1,1,1,1,1,
1,1,1,1,1,1,1,1,1,1,1,1,1,1,1,1,1,1,1,1,1,1,1,1,1,1,1,1,1,1,1,1,1,1,1,1,
1,1,1,1,1,1,1,1,1,1,1,1,1,1,1,1,1,1,1,1,1,1,1,1,1,1,1,1,1,1,1,1,1,1,1,1,
1,1,1,1,1,1,1,1,1,1,1,1,1,1,1,1,1,1,1,1,1,1,1,1,1,1,1,1,1,1,1,1,1,1,1,1,
1,1,1,1,1,1,1,1,1,1,1,1,1,1,1,1,1,1,1,1,1,1,1,1,1,1,1,1,1,1,1,1,1,1,1,1,
1,1,1,1,1,1,1,1,1,1,1,1,1,1,1,1,1,1,1,1,1,1,1,1,1,1,1,1,1,1,1,1,1,1,1,1,
1,1,1,1,1,1,1,1,1,1,1,1,1,1,1,1,1,1,1,1,1,1,1,1,1,1,1,1,1,1,1,1,1,1,1,1,
1,1,1,1,1,1,1,1,1,1,1,1,1,1,1,1,1,1,1,1,1,1,1,1,1,1,1,1,1,1,1,1,1,1,1,1,
1,1,1,1,1,1,1,1,1,1,1,1,1,1,1,1,1,1,1,1,1,1,1,1,1,1,1,1,1,1,1,1,1,1,1,1,
1,1,1,1,1,1,1,1,1,1,1,1,1,1,1,1,1,1,1,1,1,1,1,1,1,1,1,1,1,1,1,1,1,1,1,1,
1,1,1,1,1,1,1,1,1,1,1,1,1,1,1,1,1,1,1,1,1,1,1,1,1,1,1,1,1,1,1,1,1,1,1,1,
1,1,1,1,1,1,1,1,1,1,1,1,1,1,1,1,1,1,1,1,1,1,1,1,1,1,1,1,1,1,1,6),(2,2),
(-1.,-0.998165138,-0.996330275,-0.994495413,-0.99266055,-0.990825688,-0.988990826,
-0.987155963,-0.985321101,-0.983486239,-0.981651376,-0.979816514,-0.977981651,
-0.976146789,-0.974311927,-0.972477064,-0.970642202,-0.968807339,-0.966972477,
-0.965137615,-0.963302752,-0.96146789,-0.959633028,-0.957798165,-0.955963303,
-0.95412844,-0.952293578,-0.950458716,-0.948623853,-0.946788991,-0.944954128,
-0.943119266,-0.941284404,-0.939449541,-0.937614679,-0.935779817,-0.933944954,
-0.932110092,-0.930275229,-0.928440367,-0.926605505,-0.924770642,-0.92293578,
-0.921100917,-0.919266055,-0.917431193,-0.91559633,-0.913761468,-0.911926606,
-0.910091743,-0.908256881,-0.906422018,-0.904587156,-0.902752294,-0.900917431,
-0.899082569,-0.897247706,-0.895412844,-0.893577982,-0.891743119,-0.889908257,
-0.888073394,-0.886238532,-0.88440367,-0.882568807,-0.880733945,-0.878899083,
-0.87706422,-0.875229358,-0.873394495,-0.871559633,-0.869724771,-0.867889908,
-0.866055046,-0.864220183,-0.862385321,-0.860550459,-0.858715596,-0.856880734,
-0.855045872,-0.853211009,-0.851376147,-0.849541284,-0.847706422,-0.84587156,
-0.844036697,-0.842201835,-0.840366972,-0.83853211,-0.836697248,-0.834862385,
-0.833027523,-0.831192661,-0.829357798,-0.827522936,-0.825688073,-0.823853211,
-0.822018349,-0.820183486,-0.818348624,-0.816513761,-0.814678899,-0.812844037,
-0.811009174,-0.809174312,-0.80733945,-0.805504587,-0.803669725,-0.801834862,
-0.8,-0.798165138,-0.796330275,-0.794495413,-0.79266055,-0.790825688,-0.788990826,
-0.787155963,-0.785321101,-0.783486239,-0.781651376,-0.779816514,-0.777981651,
-0.776146789,-0.774311927,-0.772477064,-0.770642202,-0.768807339,-0.766972477,
-0.765137615,-0.763302752,-0.76146789,-0.759633028,-0.757798165,-0.755963303,
-0.75412844,-0.752293578,-0.750458716,-0.748623853,-0.746788991,-0.744954128,
-0.743119266,-0.741284404,-0.739449541,-0.737614679,-0.735779817,-0.733944954,
-0.732110092,-0.730275229,-0.728440367,-0.726605505,-0.724770642,-0.72293578,
-0.721100917,-0.719266055,-0.717431193,-0.71559633,-0.713761468,-0.711926606,
-0.710091743,-0.708256881,-0.706422018,-0.704587156,-0.702752294,-0.700917431,
-0.699082569,-0.697247706,-0.695412844,-0.693577982,-0.691743119,-0.689908257,
-0.688073394,-0.686238532,-0.68440367,-0.682568807,-0.680733945,-0.678899083,
-0.67706422,-0.675229358,-0.673394495,-0.671559633,-0.669724771,-0.667889908,
-0.666055046,-0.664220183,-0.662385321,-0.660550459,-0.658715596,-0.656880734,
-0.655045872,-0.653211009,-0.651376147,-0.649541284,-0.647706422,-0.64587156,
-0.644036697,-0.642201835,-0.640366972,-0.63853211,-0.636697248,-0.634862385,
-0.633027523,-0.631192661,-0.629357798,-0.627522936,-0.625688073,-0.623853211,
-0.622018349,-0.620183486,-0.618348624,-0.616513761,-0.614678899,-0.612844037,
-0.611009174,-0.609174312,-0.60733945,-0.605504587,-0.603669725,-0.601834862,
-0.6,-0.598165138,-0.596330275,-0.594495413,-0.59266055,-0.590825688,-0.588990826,
-0.587155963,-0.585321101,-0.583486239,-0.581651376,-0.579816514,-0.577981651,
-0.576146789,-0.574311927,-0.572477064,-0.570642202,-0.568807339,-0.566972477,
-0.565137615,-0.563302752,-0.56146789,-0.559633028,-0.557798165,-0.555963303,
-0.55412844,-0.552293578,-0.550458716,-0.548623853,-0.546788991,-0.544954128,
-0.543119266,-0.541284404,-0.539449541,-0.537614679,-0.535779817,-0.533944954,
-0.532110092,-0.530275229,-0.528440367,-0.526605505,-0.524770642,-0.52293578,
-0.521100917,-0.519266055,-0.517431193,-0.51559633,-0.513761468,-0.511926606,
-0.510091743,-0.508256881,-0.506422018,-0.504587156,-0.502752294,-0.500917431,
-0.499082569,-0.497247706,-0.495412844,-0.493577982,-0.491743119,-0.489908257,
-0.488073394,-0.486238532,-0.48440367,-0.482568807,-0.480733945,-0.478899083,
-0.47706422,-0.475229358,-0.473394495,-0.471559633,-0.469724771,-0.467889908,
-0.466055046,-0.464220183,-0.462385321,-0.460550459,-0.458715596,-0.456880734,
-0.455045872,-0.453211009,-0.451376147,-0.449541284,-0.447706422,-0.44587156,
-0.444036697,-0.442201835,-0.440366972,-0.43853211,-0.436697248,-0.434862385,
-0.433027523,-0.431192661,-0.429357798,-0.427522936,-0.425688073,-0.423853211,
-0.422018349,-0.420183486,-0.418348624,-0.416513761,-0.414678899,-0.412844037,
-0.411009174,-0.409174312,-0.40733945,-0.405504587,-0.403669725,-0.401834862,
-0.4,-0.398165138,-0.396330275,-0.394495413,-0.39266055,-0.390825688,-0.388990826,
-0.387155963,-0.385321101,-0.383486239,-0.381651376,-0.379816514,-0.377981651,
-0.376146789,-0.374311927,-0.372477064,-0.370642202,-0.368807339,-0.366972477,
-0.365137615,-0.363302752,-0.36146789,-0.359633028,-0.357798165,-0.355963303,
-0.35412844,-0.352293578,-0.350458716,-0.348623853,-0.346788991,-0.344954128,
-0.343119266,-0.341284404,-0.339449541,-0.337614679,-0.335779817,-0.333944954,
-0.332110092,-0.330275229,-0.328440367,-0.326605505,-0.324770642,-0.32293578,
-0.321100917,-0.319266055,-0.317431193,-0.31559633,-0.313761468,-0.311926606,
-0.310091743,-0.308256881,-0.306422018,-0.304587156,-0.302752294,-0.300917431,
-0.299082569,-0.297247706,-0.295412844,-0.293577982,-0.291743119,-0.289908257,
-0.288073394,-0.286238532,-0.28440367,-0.282568807,-0.280733945,-0.278899083,
-0.27706422,-0.275229358,-0.273394495,-0.271559633,-0.269724771,-0.267889908,
-0.266055046,-0.264220183,-0.262385321,-0.260550459,-0.258715596,-0.256880734,
-0.255045872,-0.253211009,-0.251376147,-0.249541284,-0.247706422,-0.24587156,
-0.244036697,-0.242201835,-0.240366972,-0.23853211,-0.236697248,-0.234862385,
-0.233027523,-0.231192661,-0.229357798,-0.227522936,-0.225688073,-0.223853211,
-0.222018349,-0.220183486,-0.218348624,-0.216513761,-0.214678899,-0.212844037,
-0.211009174,-0.209174312,-0.20733945,-0.205504587,-0.203669725,-0.201834862,
-0.2,-0.198165138,-0.196330275,-0.194495413,-0.19266055,-0.190825688,-0.188990826,
-0.187155963,-0.185321101,-0.183486239,-0.181651376,-0.179816514,-0.177981651,
-0.176146789,-0.174311927,-0.172477064,-0.170642202,-0.168807339,-0.166972477,
-0.165137615,-0.163302752,-0.16146789,-0.159633028,-0.157798165,-0.155963303,
-0.15412844,-0.152293578,-0.150458716,-0.148623853,-0.146788991,-0.144954128,
-0.143172103),(0.,0.36),.UNSPECIFIED.);
#6221=B_SPLINE_SURFACE_WITH_KNOTS('',5,1,((#164030,#164031),(#164032,#164033),
(#164034,#164035),(#164036,#164037),(#164038,#164039),(#164040,#164041),
(#164042,#164043),(#164044,#164045),(#164046,#164047),(#164048,#164049),
(#164050,#164051),(#164052,#164053),(#164054,#164055),(#164056,#164057),
(#164058,#164059),(#164060,#164061),(#164062,#164063),(#164064,#164065),
(#164066,#164067),(#164068,#164069),(#164070,#164071),(#164072,#164073),
(#164074,#164075),(#164076,#164077),(#164078,#164079),(#164080,#164081),
(#164082,#164083),(#164084,#164085),(#164086,#164087),(#164088,#164089),
(#164090,#164091),(#164092,#164093),(#164094,#164095),(#164096,#164097),
(#164098,#164099),(#164100,#164101),(#164102,#164103),(#164104,#164105),
(#164106,#164107),(#164108,#164109),(#164110,#164111),(#164112,#164113),
(#164114,#164115),(#164116,#164117),(#164118,#164119),(#164120,#164121),
(#164122,#164123),(#164124,#164125),(#164126,#164127),(#164128,#164129),
(#164130,#164131),(#164132,#164133),(#164134,#164135),(#164136,#164137),
(#164138,#164139),(#164140,#164141),(#164142,#164143),(#164144,#164145),
(#164146,#164147),(#164148,#164149),(#164150,#164151),(#164152,#164153),
(#164154,#164155),(#164156,#164157),(#164158,#164159),(#164160,#164161),
(#164162,#164163),(#164164,#164165),(#164166,#164167),(#164168,#164169),
(#164170,#164171),(#164172,#164173),(#164174,#164175),(#164176,#164177),
(#164178,#164179),(#164180,#164181),(#164182,#164183),(#164184,#164185),
(#164186,#164187),(#164188,#164189),(#164190,#164191),(#164192,#164193),
(#164194,#164195),(#164196,#164197),(#164198,#164199),(#164200,#164201),
(#164202,#164203),(#164204,#164205),(#164206,#164207),(#164208,#164209),
(#164210,#164211),(#164212,#164213),(#164214,#164215),(#164216,#164217),
(#164218,#164219),(#164220,#164221),(#164222,#164223),(#164224,#164225),
(#164226,#164227),(#164228,#164229),(#164230,#164231),(#164232,#164233),
(#164234,#164235),(#164236,#164237),(#164238,#164239),(#164240,#164241),
(#164242,#164243),(#164244,#164245),(#164246,#164247),(#164248,#164249),
(#164250,#164251),(#164252,#164253),(#164254,#164255),(#164256,#164257),
(#164258,#164259),(#164260,#164261),(#164262,#164263),(#164264,#164265),
(#164266,#164267),(#164268,#164269),(#164270,#164271),(#164272,#164273),
(#164274,#164275),(#164276,#164277),(#164278,#164279),(#164280,#164281),
(#164282,#164283),(#164284,#164285),(#164286,#164287),(#164288,#164289),
(#164290,#164291),(#164292,#164293),(#164294,#164295),(#164296,#164297),
(#164298,#164299),(#164300,#164301),(#164302,#164303),(#164304,#164305),
(#164306,#164307),(#164308,#164309),(#164310,#164311),(#164312,#164313),
(#164314,#164315),(#164316,#164317),(#164318,#164319),(#164320,#164321),
(#164322,#164323),(#164324,#164325),(#164326,#164327),(#164328,#164329),
(#164330,#164331),(#164332,#164333),(#164334,#164335),(#164336,#164337),
(#164338,#164339),(#164340,#164341),(#164342,#164343),(#164344,#164345),
(#164346,#164347),(#164348,#164349),(#164350,#164351),(#164352,#164353),
(#164354,#164355),(#164356,#164357),(#164358,#164359),(#164360,#164361),
(#164362,#164363),(#164364,#164365),(#164366,#164367),(#164368,#164369),
(#164370,#164371),(#164372,#164373),(#164374,#164375),(#164376,#164377),
(#164378,#164379),(#164380,#164381),(#164382,#164383),(#164384,#164385),
(#164386,#164387),(#164388,#164389),(#164390,#164391),(#164392,#164393),
(#164394,#164395),(#164396,#164397),(#164398,#164399),(#164400,#164401),
(#164402,#164403),(#164404,#164405),(#164406,#164407),(#164408,#164409),
(#164410,#164411),(#164412,#164413),(#164414,#164415),(#164416,#164417),
(#164418,#164419),(#164420,#164421),(#164422,#164423),(#164424,#164425),
(#164426,#164427),(#164428,#164429),(#164430,#164431),(#164432,#164433),
(#164434,#164435),(#164436,#164437),(#164438,#164439),(#164440,#164441),
(#164442,#164443),(#164444,#164445),(#164446,#164447),(#164448,#164449),
(#164450,#164451),(#164452,#164453),(#164454,#164455),(#164456,#164457),
(#164458,#164459),(#164460,#164461),(#164462,#164463),(#164464,#164465),
(#164466,#164467),(#164468,#164469),(#164470,#164471),(#164472,#164473),
(#164474,#164475),(#164476,#164477),(#164478,#164479),(#164480,#164481),
(#164482,#164483),(#164484,#164485),(#164486,#164487),(#164488,#164489),
(#164490,#164491),(#164492,#164493),(#164494,#164495),(#164496,#164497),
(#164498,#164499),(#164500,#164501),(#164502,#164503),(#164504,#164505),
(#164506,#164507),(#164508,#164509),(#164510,#164511),(#164512,#164513),
(#164514,#164515),(#164516,#164517),(#164518,#164519),(#164520,#164521),
(#164522,#164523),(#164524,#164525),(#164526,#164527),(#164528,#164529),
(#164530,#164531),(#164532,#164533),(#164534,#164535),(#164536,#164537),
(#164538,#164539),(#164540,#164541),(#164542,#164543),(#164544,#164545),
(#164546,#164547),(#164548,#164549),(#164550,#164551),(#164552,#164553),
(#164554,#164555),(#164556,#164557),(#164558,#164559),(#164560,#164561),
(#164562,#164563),(#164564,#164565),(#164566,#164567),(#164568,#164569),
(#164570,#164571),(#164572,#164573),(#164574,#164575),(#164576,#164577),
(#164578,#164579),(#164580,#164581),(#164582,#164583),(#164584,#164585),
(#164586,#164587),(#164588,#164589),(#164590,#164591),(#164592,#164593),
(#164594,#164595),(#164596,#164597),(#164598,#164599),(#164600,#164601),
(#164602,#164603),(#164604,#164605),(#164606,#164607),(#164608,#164609),
(#164610,#164611),(#164612,#164613),(#164614,#164615),(#164616,#164617),
(#164618,#164619),(#164620,#164621),(#164622,#164623),(#164624,#164625),
(#164626,#164627),(#164628,#164629),(#164630,#164631),(#164632,#164633),
(#164634,#164635),(#164636,#164637),(#164638,#164639),(#164640,#164641),
(#164642,#164643),(#164644,#164645),(#164646,#164647),(#164648,#164649),
(#164650,#164651),(#164652,#164653),(#164654,#164655),(#164656,#164657),
(#164658,#164659),(#164660,#164661),(#164662,#164663),(#164664,#164665),
(#164666,#164667),(#164668,#164669),(#164670,#164671),(#164672,#164673),
(#164674,#164675),(#164676,#164677),(#164678,#164679),(#164680,#164681),
(#164682,#164683),(#164684,#164685),(#164686,#164687),(#164688,#164689),
(#164690,#164691),(#164692,#164693),(#164694,#164695),(#164696,#164697),
(#164698,#164699),(#164700,#164701),(#164702,#164703),(#164704,#164705),
(#164706,#164707),(#164708,#164709),(#164710,#164711),(#164712,#164713),
(#164714,#164715),(#164716,#164717),(#164718,#164719),(#164720,#164721),
(#164722,#164723),(#164724,#164725),(#164726,#164727),(#164728,#164729),
(#164730,#164731),(#164732,#164733),(#164734,#164735),(#164736,#164737),
(#164738,#164739),(#164740,#164741),(#164742,#164743),(#164744,#164745),
(#164746,#164747),(#164748,#164749),(#164750,#164751),(#164752,#164753),
(#164754,#164755),(#164756,#164757),(#164758,#164759),(#164760,#164761),
(#164762,#164763),(#164764,#164765),(#164766,#164767),(#164768,#164769),
(#164770,#164771),(#164772,#164773),(#164774,#164775),(#164776,#164777),
(#164778,#164779),(#164780,#164781),(#164782,#164783),(#164784,#164785),
(#164786,#164787),(#164788,#164789),(#164790,#164791),(#164792,#164793),
(#164794,#164795),(#164796,#164797),(#164798,#164799),(#164800,#164801),
(#164802,#164803),(#164804,#164805),(#164806,#164807),(#164808,#164809),
(#164810,#164811),(#164812,#164813),(#164814,#164815),(#164816,#164817),
(#164818,#164819),(#164820,#164821),(#164822,#164823),(#164824,#164825),
(#164826,#164827),(#164828,#164829),(#164830,#164831),(#164832,#164833),
(#164834,#164835),(#164836,#164837),(#164838,#164839),(#164840,#164841),
(#164842,#164843),(#164844,#164845),(#164846,#164847),(#164848,#164849),
(#164850,#164851),(#164852,#164853),(#164854,#164855),(#164856,#164857),
(#164858,#164859),(#164860,#164861),(#164862,#164863),(#164864,#164865),
(#164866,#164867),(#164868,#164869),(#164870,#164871),(#164872,#164873),
(#164874,#164875),(#164876,#164877),(#164878,#164879),(#164880,#164881),
(#164882,#164883),(#164884,#164885),(#164886,#164887),(#164888,#164889),
(#164890,#164891),(#164892,#164893),(#164894,#164895),(#164896,#164897),
(#164898,#164899),(#164900,#164901),(#164902,#164903),(#164904,#164905),
(#164906,#164907),(#164908,#164909),(#164910,#164911),(#164912,#164913),
(#164914,#164915),(#164916,#164917),(#164918,#164919),(#164920,#164921),
(#164922,#164923),(#164924,#164925),(#164926,#164927),(#164928,#164929),
(#164930,#164931),(#164932,#164933),(#164934,#164935),(#164936,#164937),
(#164938,#164939),(#164940,#164941),(#164942,#164943),(#164944,#164945),
(#164946,#164947),(#164948,#164949),(#164950,#164951),(#164952,#164953),
(#164954,#164955),(#164956,#164957),(#164958,#164959),(#164960,#164961),
(#164962,#164963),(#164964,#164965),(#164966,#164967),(#164968,#164969),
(#164970,#164971),(#164972,#164973)),.UNSPECIFIED.,.F.,.F.,.F.,(6,1,1,1,
1,1,1,1,1,1,1,1,1,1,1,1,1,1,1,1,1,1,1,1,1,1,1,1,1,1,1,1,1,1,1,1,1,1,1,1,
1,1,1,1,1,1,1,1,1,1,1,1,1,1,1,1,1,1,1,1,1,1,1,1,1,1,1,1,1,1,1,1,1,1,1,1,
1,1,1,1,1,1,1,1,1,1,1,1,1,1,1,1,1,1,1,1,1,1,1,1,1,1,1,1,1,1,1,1,1,1,1,1,
1,1,1,1,1,1,1,1,1,1,1,1,1,1,1,1,1,1,1,1,1,1,1,1,1,1,1,1,1,1,1,1,1,1,1,1,
1,1,1,1,1,1,1,1,1,1,1,1,1,1,1,1,1,1,1,1,1,1,1,1,1,1,1,1,1,1,1,1,1,1,1,1,
1,1,1,1,1,1,1,1,1,1,1,1,1,1,1,1,1,1,1,1,1,1,1,1,1,1,1,1,1,1,1,1,1,1,1,1,
1,1,1,1,1,1,1,1,1,1,1,1,1,1,1,1,1,1,1,1,1,1,1,1,1,1,1,1,1,1,1,1,1,1,1,1,
1,1,1,1,1,1,1,1,1,1,1,1,1,1,1,1,1,1,1,1,1,1,1,1,1,1,1,1,1,1,1,1,1,1,1,1,
1,1,1,1,1,1,1,1,1,1,1,1,1,1,1,1,1,1,1,1,1,1,1,1,1,1,1,1,1,1,1,1,1,1,1,1,
1,1,1,1,1,1,1,1,1,1,1,1,1,1,1,1,1,1,1,1,1,1,1,1,1,1,1,1,1,1,1,1,1,1,1,1,
1,1,1,1,1,1,1,1,1,1,1,1,1,1,1,1,1,1,1,1,1,1,1,1,1,1,1,1,1,1,1,1,1,1,1,1,
1,1,1,1,1,1,1,1,1,1,1,1,1,1,1,1,1,1,1,1,1,1,1,1,1,1,1,1,1,1,1,1,1,1,1,1,
1,1,1,1,1,1,1,1,1,1,1,1,1,1,1,1,1,1,1,1,1,1,1,1,1,1,1,1,1,1,1,6),(2,2),
(-1.,-0.998165138,-0.996330275,-0.994495413,-0.99266055,-0.990825688,-0.988990826,
-0.987155963,-0.985321101,-0.983486239,-0.981651376,-0.979816514,-0.977981651,
-0.976146789,-0.974311927,-0.972477064,-0.970642202,-0.968807339,-0.966972477,
-0.965137615,-0.963302752,-0.96146789,-0.959633028,-0.957798165,-0.955963303,
-0.95412844,-0.952293578,-0.950458716,-0.948623853,-0.946788991,-0.944954128,
-0.943119266,-0.941284404,-0.939449541,-0.937614679,-0.935779817,-0.933944954,
-0.932110092,-0.930275229,-0.928440367,-0.926605505,-0.924770642,-0.92293578,
-0.921100917,-0.919266055,-0.917431193,-0.91559633,-0.913761468,-0.911926606,
-0.910091743,-0.908256881,-0.906422018,-0.904587156,-0.902752294,-0.900917431,
-0.899082569,-0.897247706,-0.895412844,-0.893577982,-0.891743119,-0.889908257,
-0.888073394,-0.886238532,-0.88440367,-0.882568807,-0.880733945,-0.878899083,
-0.87706422,-0.875229358,-0.873394495,-0.871559633,-0.869724771,-0.867889908,
-0.866055046,-0.864220183,-0.862385321,-0.860550459,-0.858715596,-0.856880734,
-0.855045872,-0.853211009,-0.851376147,-0.849541284,-0.847706422,-0.84587156,
-0.844036697,-0.842201835,-0.840366972,-0.83853211,-0.836697248,-0.834862385,
-0.833027523,-0.831192661,-0.829357798,-0.827522936,-0.825688073,-0.823853211,
-0.822018349,-0.820183486,-0.818348624,-0.816513761,-0.814678899,-0.812844037,
-0.811009174,-0.809174312,-0.80733945,-0.805504587,-0.803669725,-0.801834862,
-0.8,-0.798165138,-0.796330275,-0.794495413,-0.79266055,-0.790825688,-0.788990826,
-0.787155963,-0.785321101,-0.783486239,-0.781651376,-0.779816514,-0.777981651,
-0.776146789,-0.774311927,-0.772477064,-0.770642202,-0.768807339,-0.766972477,
-0.765137615,-0.763302752,-0.76146789,-0.759633028,-0.757798165,-0.755963303,
-0.75412844,-0.752293578,-0.750458716,-0.748623853,-0.746788991,-0.744954128,
-0.743119266,-0.741284404,-0.739449541,-0.737614679,-0.735779817,-0.733944954,
-0.732110092,-0.730275229,-0.728440367,-0.726605505,-0.724770642,-0.72293578,
-0.721100917,-0.719266055,-0.717431193,-0.71559633,-0.713761468,-0.711926606,
-0.710091743,-0.708256881,-0.706422018,-0.704587156,-0.702752294,-0.700917431,
-0.699082569,-0.697247706,-0.695412844,-0.693577982,-0.691743119,-0.689908257,
-0.688073394,-0.686238532,-0.68440367,-0.682568807,-0.680733945,-0.678899083,
-0.67706422,-0.675229358,-0.673394495,-0.671559633,-0.669724771,-0.667889908,
-0.666055046,-0.664220183,-0.662385321,-0.660550459,-0.658715596,-0.656880734,
-0.655045872,-0.653211009,-0.651376147,-0.649541284,-0.647706422,-0.64587156,
-0.644036697,-0.642201835,-0.640366972,-0.63853211,-0.636697248,-0.634862385,
-0.633027523,-0.631192661,-0.629357798,-0.627522936,-0.625688073,-0.623853211,
-0.622018349,-0.620183486,-0.618348624,-0.616513761,-0.614678899,-0.612844037,
-0.611009174,-0.609174312,-0.60733945,-0.605504587,-0.603669725,-0.601834862,
-0.6,-0.598165138,-0.596330275,-0.594495413,-0.59266055,-0.590825688,-0.588990826,
-0.587155963,-0.585321101,-0.583486239,-0.581651376,-0.579816514,-0.577981651,
-0.576146789,-0.574311927,-0.572477064,-0.570642202,-0.568807339,-0.566972477,
-0.565137615,-0.563302752,-0.56146789,-0.559633028,-0.557798165,-0.555963303,
-0.55412844,-0.552293578,-0.550458716,-0.548623853,-0.546788991,-0.544954128,
-0.543119266,-0.541284404,-0.539449541,-0.537614679,-0.535779817,-0.533944954,
-0.532110092,-0.530275229,-0.528440367,-0.526605505,-0.524770642,-0.52293578,
-0.521100917,-0.519266055,-0.517431193,-0.51559633,-0.513761468,-0.511926606,
-0.510091743,-0.508256881,-0.506422018,-0.504587156,-0.502752294,-0.500917431,
-0.499082569,-0.497247706,-0.495412844,-0.493577982,-0.491743119,-0.489908257,
-0.488073394,-0.486238532,-0.48440367,-0.482568807,-0.480733945,-0.478899083,
-0.47706422,-0.475229358,-0.473394495,-0.471559633,-0.469724771,-0.467889908,
-0.466055046,-0.464220183,-0.462385321,-0.460550459,-0.458715596,-0.456880734,
-0.455045872,-0.453211009,-0.451376147,-0.449541284,-0.447706422,-0.44587156,
-0.444036697,-0.442201835,-0.440366972,-0.43853211,-0.436697248,-0.434862385,
-0.433027523,-0.431192661,-0.429357798,-0.427522936,-0.425688073,-0.423853211,
-0.422018349,-0.420183486,-0.418348624,-0.416513761,-0.414678899,-0.412844037,
-0.411009174,-0.409174312,-0.40733945,-0.405504587,-0.403669725,-0.401834862,
-0.4,-0.398165138,-0.396330275,-0.394495413,-0.39266055,-0.390825688,-0.388990826,
-0.387155963,-0.385321101,-0.383486239,-0.381651376,-0.379816514,-0.377981651,
-0.376146789,-0.374311927,-0.372477064,-0.370642202,-0.368807339,-0.366972477,
-0.365137615,-0.363302752,-0.36146789,-0.359633028,-0.357798165,-0.355963303,
-0.35412844,-0.352293578,-0.350458716,-0.348623853,-0.346788991,-0.344954128,
-0.343119266,-0.341284404,-0.339449541,-0.337614679,-0.335779817,-0.333944954,
-0.332110092,-0.330275229,-0.328440367,-0.326605505,-0.324770642,-0.32293578,
-0.321100917,-0.319266055,-0.317431193,-0.31559633,-0.313761468,-0.311926606,
-0.310091743,-0.308256881,-0.306422018,-0.304587156,-0.302752294,-0.300917431,
-0.299082569,-0.297247706,-0.295412844,-0.293577982,-0.291743119,-0.289908257,
-0.288073394,-0.286238532,-0.28440367,-0.282568807,-0.280733945,-0.278899083,
-0.27706422,-0.275229358,-0.273394495,-0.271559633,-0.269724771,-0.267889908,
-0.266055046,-0.264220183,-0.262385321,-0.260550459,-0.258715596,-0.256880734,
-0.255045872,-0.253211009,-0.251376147,-0.249541284,-0.247706422,-0.24587156,
-0.244036697,-0.242201835,-0.240366972,-0.23853211,-0.236697248,-0.234862385,
-0.233027523,-0.231192661,-0.229357798,-0.227522936,-0.225688073,-0.223853211,
-0.222018349,-0.220183486,-0.218348624,-0.216513761,-0.214678899,-0.212844037,
-0.211009174,-0.209174312,-0.20733945,-0.205504587,-0.203669725,-0.201834862,
-0.2,-0.198165138,-0.196330275,-0.194495413,-0.19266055,-0.190825688,-0.188990826,
-0.187155963,-0.185321101,-0.183486239,-0.181651376,-0.179816514,-0.177981651,
-0.176146789,-0.174311927,-0.172477064,-0.170642202,-0.168807339,-0.166972477,
-0.165137615,-0.163302752,-0.16146789,-0.159633028,-0.157798165,-0.155963303,
-0.15412844,-0.152293578,-0.150458716,-0.148623853,-0.146788991,-0.144954128,
-0.143172103),(0.,0.36),.UNSPECIFIED.);
#6222=B_SPLINE_SURFACE_WITH_KNOTS('',5,1,((#165627,#165628),(#165629,#165630),
(#165631,#165632),(#165633,#165634),(#165635,#165636),(#165637,#165638),
(#165639,#165640),(#165641,#165642),(#165643,#165644),(#165645,#165646),
(#165647,#165648),(#165649,#165650),(#165651,#165652),(#165653,#165654),
(#165655,#165656),(#165657,#165658),(#165659,#165660),(#165661,#165662),
(#165663,#165664),(#165665,#165666),(#165667,#165668),(#165669,#165670),
(#165671,#165672),(#165673,#165674),(#165675,#165676),(#165677,#165678),
(#165679,#165680),(#165681,#165682),(#165683,#165684),(#165685,#165686),
(#165687,#165688),(#165689,#165690),(#165691,#165692),(#165693,#165694),
(#165695,#165696),(#165697,#165698),(#165699,#165700),(#165701,#165702),
(#165703,#165704),(#165705,#165706),(#165707,#165708),(#165709,#165710),
(#165711,#165712),(#165713,#165714),(#165715,#165716),(#165717,#165718),
(#165719,#165720),(#165721,#165722),(#165723,#165724),(#165725,#165726),
(#165727,#165728),(#165729,#165730),(#165731,#165732),(#165733,#165734),
(#165735,#165736),(#165737,#165738),(#165739,#165740),(#165741,#165742),
(#165743,#165744),(#165745,#165746),(#165747,#165748),(#165749,#165750),
(#165751,#165752),(#165753,#165754),(#165755,#165756),(#165757,#165758),
(#165759,#165760),(#165761,#165762),(#165763,#165764),(#165765,#165766),
(#165767,#165768),(#165769,#165770),(#165771,#165772),(#165773,#165774),
(#165775,#165776),(#165777,#165778),(#165779,#165780),(#165781,#165782),
(#165783,#165784),(#165785,#165786),(#165787,#165788),(#165789,#165790),
(#165791,#165792),(#165793,#165794),(#165795,#165796),(#165797,#165798),
(#165799,#165800),(#165801,#165802),(#165803,#165804),(#165805,#165806),
(#165807,#165808),(#165809,#165810),(#165811,#165812),(#165813,#165814),
(#165815,#165816),(#165817,#165818),(#165819,#165820),(#165821,#165822),
(#165823,#165824),(#165825,#165826),(#165827,#165828),(#165829,#165830),
(#165831,#165832),(#165833,#165834),(#165835,#165836),(#165837,#165838),
(#165839,#165840),(#165841,#165842),(#165843,#165844),(#165845,#165846),
(#165847,#165848),(#165849,#165850),(#165851,#165852),(#165853,#165854),
(#165855,#165856),(#165857,#165858),(#165859,#165860),(#165861,#165862),
(#165863,#165864),(#165865,#165866),(#165867,#165868),(#165869,#165870),
(#165871,#165872),(#165873,#165874),(#165875,#165876),(#165877,#165878),
(#165879,#165880),(#165881,#165882),(#165883,#165884),(#165885,#165886),
(#165887,#165888),(#165889,#165890),(#165891,#165892),(#165893,#165894),
(#165895,#165896),(#165897,#165898),(#165899,#165900),(#165901,#165902),
(#165903,#165904),(#165905,#165906),(#165907,#165908),(#165909,#165910),
(#165911,#165912),(#165913,#165914),(#165915,#165916),(#165917,#165918),
(#165919,#165920),(#165921,#165922),(#165923,#165924),(#165925,#165926),
(#165927,#165928),(#165929,#165930),(#165931,#165932),(#165933,#165934),
(#165935,#165936),(#165937,#165938),(#165939,#165940),(#165941,#165942),
(#165943,#165944),(#165945,#165946),(#165947,#165948),(#165949,#165950),
(#165951,#165952),(#165953,#165954),(#165955,#165956),(#165957,#165958),
(#165959,#165960),(#165961,#165962),(#165963,#165964),(#165965,#165966),
(#165967,#165968),(#165969,#165970),(#165971,#165972),(#165973,#165974),
(#165975,#165976),(#165977,#165978),(#165979,#165980),(#165981,#165982),
(#165983,#165984),(#165985,#165986),(#165987,#165988),(#165989,#165990),
(#165991,#165992),(#165993,#165994),(#165995,#165996),(#165997,#165998),
(#165999,#166000),(#166001,#166002),(#166003,#166004),(#166005,#166006),
(#166007,#166008),(#166009,#166010),(#166011,#166012),(#166013,#166014),
(#166015,#166016),(#166017,#166018),(#166019,#166020),(#166021,#166022),
(#166023,#166024),(#166025,#166026),(#166027,#166028),(#166029,#166030),
(#166031,#166032),(#166033,#166034),(#166035,#166036),(#166037,#166038),
(#166039,#166040),(#166041,#166042),(#166043,#166044),(#166045,#166046),
(#166047,#166048),(#166049,#166050),(#166051,#166052),(#166053,#166054),
(#166055,#166056),(#166057,#166058),(#166059,#166060),(#166061,#166062),
(#166063,#166064),(#166065,#166066),(#166067,#166068),(#166069,#166070),
(#166071,#166072),(#166073,#166074),(#166075,#166076),(#166077,#166078),
(#166079,#166080),(#166081,#166082),(#166083,#166084),(#166085,#166086),
(#166087,#166088),(#166089,#166090),(#166091,#166092),(#166093,#166094),
(#166095,#166096),(#166097,#166098),(#166099,#166100),(#166101,#166102),
(#166103,#166104),(#166105,#166106),(#166107,#166108),(#166109,#166110),
(#166111,#166112),(#166113,#166114),(#166115,#166116),(#166117,#166118),
(#166119,#166120),(#166121,#166122),(#166123,#166124),(#166125,#166126),
(#166127,#166128),(#166129,#166130),(#166131,#166132),(#166133,#166134),
(#166135,#166136),(#166137,#166138),(#166139,#166140),(#166141,#166142),
(#166143,#166144),(#166145,#166146),(#166147,#166148),(#166149,#166150),
(#166151,#166152),(#166153,#166154),(#166155,#166156),(#166157,#166158),
(#166159,#166160),(#166161,#166162),(#166163,#166164),(#166165,#166166),
(#166167,#166168),(#166169,#166170),(#166171,#166172),(#166173,#166174),
(#166175,#166176),(#166177,#166178),(#166179,#166180),(#166181,#166182),
(#166183,#166184),(#166185,#166186),(#166187,#166188),(#166189,#166190),
(#166191,#166192),(#166193,#166194),(#166195,#166196),(#166197,#166198),
(#166199,#166200),(#166201,#166202),(#166203,#166204),(#166205,#166206),
(#166207,#166208),(#166209,#166210),(#166211,#166212),(#166213,#166214),
(#166215,#166216),(#166217,#166218),(#166219,#166220),(#166221,#166222),
(#166223,#166224),(#166225,#166226),(#166227,#166228),(#166229,#166230),
(#166231,#166232),(#166233,#166234),(#166235,#166236),(#166237,#166238),
(#166239,#166240),(#166241,#166242),(#166243,#166244),(#166245,#166246),
(#166247,#166248),(#166249,#166250),(#166251,#166252),(#166253,#166254),
(#166255,#166256),(#166257,#166258),(#166259,#166260),(#166261,#166262),
(#166263,#166264),(#166265,#166266),(#166267,#166268),(#166269,#166270),
(#166271,#166272),(#166273,#166274),(#166275,#166276),(#166277,#166278),
(#166279,#166280),(#166281,#166282),(#166283,#166284),(#166285,#166286),
(#166287,#166288),(#166289,#166290),(#166291,#166292),(#166293,#166294),
(#166295,#166296),(#166297,#166298),(#166299,#166300),(#166301,#166302),
(#166303,#166304),(#166305,#166306),(#166307,#166308),(#166309,#166310),
(#166311,#166312),(#166313,#166314),(#166315,#166316),(#166317,#166318),
(#166319,#166320),(#166321,#166322),(#166323,#166324),(#166325,#166326),
(#166327,#166328),(#166329,#166330),(#166331,#166332),(#166333,#166334),
(#166335,#166336),(#166337,#166338),(#166339,#166340),(#166341,#166342),
(#166343,#166344),(#166345,#166346),(#166347,#166348),(#166349,#166350),
(#166351,#166352),(#166353,#166354),(#166355,#166356),(#166357,#166358),
(#166359,#166360),(#166361,#166362),(#166363,#166364),(#166365,#166366),
(#166367,#166368),(#166369,#166370),(#166371,#166372),(#166373,#166374),
(#166375,#166376),(#166377,#166378),(#166379,#166380),(#166381,#166382),
(#166383,#166384),(#166385,#166386),(#166387,#166388),(#166389,#166390),
(#166391,#166392),(#166393,#166394),(#166395,#166396),(#166397,#166398),
(#166399,#166400),(#166401,#166402),(#166403,#166404),(#166405,#166406),
(#166407,#166408),(#166409,#166410),(#166411,#166412),(#166413,#166414),
(#166415,#166416),(#166417,#166418),(#166419,#166420),(#166421,#166422),
(#166423,#166424),(#166425,#166426),(#166427,#166428),(#166429,#166430),
(#166431,#166432),(#166433,#166434),(#166435,#166436),(#166437,#166438),
(#166439,#166440),(#166441,#166442),(#166443,#166444),(#166445,#166446),
(#166447,#166448),(#166449,#166450),(#166451,#166452),(#166453,#166454),
(#166455,#166456),(#166457,#166458),(#166459,#166460),(#166461,#166462),
(#166463,#166464),(#166465,#166466),(#166467,#166468),(#166469,#166470),
(#166471,#166472),(#166473,#166474),(#166475,#166476),(#166477,#166478),
(#166479,#166480),(#166481,#166482),(#166483,#166484),(#166485,#166486),
(#166487,#166488),(#166489,#166490),(#166491,#166492),(#166493,#166494),
(#166495,#166496),(#166497,#166498),(#166499,#166500),(#166501,#166502),
(#166503,#166504),(#166505,#166506),(#166507,#166508),(#166509,#166510),
(#166511,#166512),(#166513,#166514),(#166515,#166516),(#166517,#166518),
(#166519,#166520),(#166521,#166522),(#166523,#166524),(#166525,#166526),
(#166527,#166528),(#166529,#166530),(#166531,#166532),(#166533,#166534),
(#166535,#166536),(#166537,#166538),(#166539,#166540),(#166541,#166542),
(#166543,#166544),(#166545,#166546),(#166547,#166548),(#166549,#166550),
(#166551,#166552),(#166553,#166554),(#166555,#166556),(#166557,#166558),
(#166559,#166560),(#166561,#166562),(#166563,#166564),(#166565,#166566),
(#166567,#166568),(#166569,#166570)),.UNSPECIFIED.,.F.,.F.,.F.,(6,1,1,1,
1,1,1,1,1,1,1,1,1,1,1,1,1,1,1,1,1,1,1,1,1,1,1,1,1,1,1,1,1,1,1,1,1,1,1,1,
1,1,1,1,1,1,1,1,1,1,1,1,1,1,1,1,1,1,1,1,1,1,1,1,1,1,1,1,1,1,1,1,1,1,1,1,
1,1,1,1,1,1,1,1,1,1,1,1,1,1,1,1,1,1,1,1,1,1,1,1,1,1,1,1,1,1,1,1,1,1,1,1,
1,1,1,1,1,1,1,1,1,1,1,1,1,1,1,1,1,1,1,1,1,1,1,1,1,1,1,1,1,1,1,1,1,1,1,1,
1,1,1,1,1,1,1,1,1,1,1,1,1,1,1,1,1,1,1,1,1,1,1,1,1,1,1,1,1,1,1,1,1,1,1,1,
1,1,1,1,1,1,1,1,1,1,1,1,1,1,1,1,1,1,1,1,1,1,1,1,1,1,1,1,1,1,1,1,1,1,1,1,
1,1,1,1,1,1,1,1,1,1,1,1,1,1,1,1,1,1,1,1,1,1,1,1,1,1,1,1,1,1,1,1,1,1,1,1,
1,1,1,1,1,1,1,1,1,1,1,1,1,1,1,1,1,1,1,1,1,1,1,1,1,1,1,1,1,1,1,1,1,1,1,1,
1,1,1,1,1,1,1,1,1,1,1,1,1,1,1,1,1,1,1,1,1,1,1,1,1,1,1,1,1,1,1,1,1,1,1,1,
1,1,1,1,1,1,1,1,1,1,1,1,1,1,1,1,1,1,1,1,1,1,1,1,1,1,1,1,1,1,1,1,1,1,1,1,
1,1,1,1,1,1,1,1,1,1,1,1,1,1,1,1,1,1,1,1,1,1,1,1,1,1,1,1,1,1,1,1,1,1,1,1,
1,1,1,1,1,1,1,1,1,1,1,1,1,1,1,1,1,1,1,1,1,1,1,1,1,1,1,1,1,1,1,1,1,1,1,1,
1,1,1,1,1,1,1,1,1,1,1,1,1,1,1,1,1,1,1,1,1,1,1,1,1,1,1,1,1,1,1,6),(2,2),
(0.143172103,0.144954128,0.146788991,0.148623853,0.150458716,0.152293578,
0.15412844,0.155963303,0.157798165,0.159633028,0.16146789,0.163302752,0.165137615,
0.166972477,0.168807339,0.170642202,0.172477064,0.174311927,0.176146789,
0.177981651,0.179816514,0.181651376,0.183486239,0.185321101,0.187155963,
0.188990826,0.190825688,0.19266055,0.194495413,0.196330275,0.198165138,
0.2,0.201834862,0.203669725,0.205504587,0.20733945,0.209174312,0.211009174,
0.212844037,0.214678899,0.216513761,0.218348624,0.220183486,0.222018349,
0.223853211,0.225688073,0.227522936,0.229357798,0.231192661,0.233027523,
0.234862385,0.236697248,0.23853211,0.240366972,0.242201835,0.244036697,
0.24587156,0.247706422,0.249541284,0.251376147,0.253211009,0.255045872,
0.256880734,0.258715596,0.260550459,0.262385321,0.264220183,0.266055046,
0.267889908,0.269724771,0.271559633,0.273394495,0.275229358,0.27706422,
0.278899083,0.280733945,0.282568807,0.28440367,0.286238532,0.288073394,
0.289908257,0.291743119,0.293577982,0.295412844,0.297247706,0.299082569,
0.300917431,0.302752294,0.304587156,0.306422018,0.308256881,0.310091743,
0.311926606,0.313761468,0.31559633,0.317431193,0.319266055,0.321100917,
0.32293578,0.324770642,0.326605505,0.328440367,0.330275229,0.332110092,
0.333944954,0.335779817,0.337614679,0.339449541,0.341284404,0.343119266,
0.344954128,0.346788991,0.348623853,0.350458716,0.352293578,0.35412844,
0.355963303,0.357798165,0.359633028,0.36146789,0.363302752,0.365137615,
0.366972477,0.368807339,0.370642202,0.372477064,0.374311927,0.376146789,
0.377981651,0.379816514,0.381651376,0.383486239,0.385321101,0.387155963,
0.388990826,0.390825688,0.39266055,0.394495413,0.396330275,0.398165138,
0.4,0.401834862,0.403669725,0.405504587,0.40733945,0.409174312,0.411009174,
0.412844037,0.414678899,0.416513761,0.418348624,0.420183486,0.422018349,
0.423853211,0.425688073,0.427522936,0.429357798,0.431192661,0.433027523,
0.434862385,0.436697248,0.43853211,0.440366972,0.442201835,0.444036697,
0.44587156,0.447706422,0.449541284,0.451376147,0.453211009,0.455045872,
0.456880734,0.458715596,0.460550459,0.462385321,0.464220183,0.466055046,
0.467889908,0.469724771,0.471559633,0.473394495,0.475229358,0.47706422,
0.478899083,0.480733945,0.482568807,0.48440367,0.486238532,0.488073394,
0.489908257,0.491743119,0.493577982,0.495412844,0.497247706,0.499082569,
0.500917431,0.502752294,0.504587156,0.506422018,0.508256881,0.510091743,
0.511926606,0.513761468,0.51559633,0.517431193,0.519266055,0.521100917,
0.52293578,0.524770642,0.526605505,0.528440367,0.530275229,0.532110092,
0.533944954,0.535779817,0.537614679,0.539449541,0.541284404,0.543119266,
0.544954128,0.546788991,0.548623853,0.550458716,0.552293578,0.55412844,
0.555963303,0.557798165,0.559633028,0.56146789,0.563302752,0.565137615,
0.566972477,0.568807339,0.570642202,0.572477064,0.574311927,0.576146789,
0.577981651,0.579816514,0.581651376,0.583486239,0.585321101,0.587155963,
0.588990826,0.590825688,0.59266055,0.594495413,0.596330275,0.598165138,
0.6,0.601834862,0.603669725,0.605504587,0.60733945,0.609174312,0.611009174,
0.612844037,0.614678899,0.616513761,0.618348624,0.620183486,0.622018349,
0.623853211,0.625688073,0.627522936,0.629357798,0.631192661,0.633027523,
0.634862385,0.636697248,0.63853211,0.640366972,0.642201835,0.644036697,
0.64587156,0.647706422,0.649541284,0.651376147,0.653211009,0.655045872,
0.656880734,0.658715596,0.660550459,0.662385321,0.664220183,0.666055046,
0.667889908,0.669724771,0.671559633,0.673394495,0.675229358,0.67706422,
0.678899083,0.680733945,0.682568807,0.68440367,0.686238532,0.688073394,
0.689908257,0.691743119,0.693577982,0.695412844,0.697247706,0.699082569,
0.700917431,0.702752294,0.704587156,0.706422018,0.708256881,0.710091743,
0.711926606,0.713761468,0.71559633,0.717431193,0.719266055,0.721100917,
0.72293578,0.724770642,0.726605505,0.728440367,0.730275229,0.732110092,
0.733944954,0.735779817,0.737614679,0.739449541,0.741284404,0.743119266,
0.744954128,0.746788991,0.748623853,0.750458716,0.752293578,0.75412844,
0.755963303,0.757798165,0.759633028,0.76146789,0.763302752,0.765137615,
0.766972477,0.768807339,0.770642202,0.772477064,0.774311927,0.776146789,
0.777981651,0.779816514,0.781651376,0.783486239,0.785321101,0.787155963,
0.788990826,0.790825688,0.79266055,0.794495413,0.796330275,0.798165138,
0.8,0.801834862,0.803669725,0.805504587,0.80733945,0.809174312,0.811009174,
0.812844037,0.814678899,0.816513761,0.818348624,0.820183486,0.822018349,
0.823853211,0.825688073,0.827522936,0.829357798,0.831192661,0.833027523,
0.834862385,0.836697248,0.83853211,0.840366972,0.842201835,0.844036697,
0.84587156,0.847706422,0.849541284,0.851376147,0.853211009,0.855045872,
0.856880734,0.858715596,0.860550459,0.862385321,0.864220183,0.866055046,
0.867889908,0.869724771,0.871559633,0.873394495,0.875229358,0.87706422,
0.878899083,0.880733945,0.882568807,0.88440367,0.886238532,0.888073394,
0.889908257,0.891743119,0.893577982,0.895412844,0.897247706,0.899082569,
0.900917431,0.902752294,0.904587156,0.906422018,0.908256881,0.910091743,
0.911926606,0.913761468,0.91559633,0.917431193,0.919266055,0.921100917,
0.92293578,0.924770642,0.926605505,0.928440367,0.930275229,0.932110092,
0.933944954,0.935779817,0.937614679,0.939449541,0.941284404,0.943119266,
0.944954128,0.946788991,0.948623853,0.950458716,0.952293578,0.95412844,
0.955963303,0.957798165,0.959633028,0.96146789,0.963302752,0.965137615,
0.966972477,0.968807339,0.970642202,0.972477064,0.974311927,0.976146789,
0.977981651,0.979816514,0.981651376,0.983486239,0.985321101,0.987155963,
0.988990826,0.990825688,0.99266055,0.994495413,0.996330275,0.998165138,
1.),(0.,0.36),.UNSPECIFIED.);
#6223=B_SPLINE_SURFACE_WITH_KNOTS('',5,1,((#167230,#167231),(#167232,#167233),
(#167234,#167235),(#167236,#167237),(#167238,#167239),(#167240,#167241),
(#167242,#167243),(#167244,#167245),(#167246,#167247),(#167248,#167249),
(#167250,#167251),(#167252,#167253),(#167254,#167255),(#167256,#167257),
(#167258,#167259),(#167260,#167261),(#167262,#167263),(#167264,#167265),
(#167266,#167267),(#167268,#167269),(#167270,#167271),(#167272,#167273),
(#167274,#167275),(#167276,#167277),(#167278,#167279),(#167280,#167281),
(#167282,#167283),(#167284,#167285),(#167286,#167287),(#167288,#167289),
(#167290,#167291),(#167292,#167293),(#167294,#167295),(#167296,#167297),
(#167298,#167299),(#167300,#167301),(#167302,#167303),(#167304,#167305),
(#167306,#167307),(#167308,#167309),(#167310,#167311),(#167312,#167313),
(#167314,#167315),(#167316,#167317),(#167318,#167319),(#167320,#167321),
(#167322,#167323),(#167324,#167325),(#167326,#167327),(#167328,#167329),
(#167330,#167331),(#167332,#167333),(#167334,#167335),(#167336,#167337),
(#167338,#167339),(#167340,#167341),(#167342,#167343),(#167344,#167345),
(#167346,#167347),(#167348,#167349),(#167350,#167351),(#167352,#167353),
(#167354,#167355),(#167356,#167357),(#167358,#167359),(#167360,#167361),
(#167362,#167363),(#167364,#167365),(#167366,#167367),(#167368,#167369),
(#167370,#167371),(#167372,#167373),(#167374,#167375),(#167376,#167377),
(#167378,#167379),(#167380,#167381),(#167382,#167383),(#167384,#167385),
(#167386,#167387),(#167388,#167389),(#167390,#167391),(#167392,#167393),
(#167394,#167395),(#167396,#167397),(#167398,#167399),(#167400,#167401),
(#167402,#167403),(#167404,#167405),(#167406,#167407),(#167408,#167409),
(#167410,#167411),(#167412,#167413),(#167414,#167415),(#167416,#167417),
(#167418,#167419),(#167420,#167421),(#167422,#167423),(#167424,#167425),
(#167426,#167427),(#167428,#167429),(#167430,#167431),(#167432,#167433),
(#167434,#167435),(#167436,#167437),(#167438,#167439),(#167440,#167441),
(#167442,#167443),(#167444,#167445),(#167446,#167447),(#167448,#167449),
(#167450,#167451),(#167452,#167453),(#167454,#167455),(#167456,#167457),
(#167458,#167459),(#167460,#167461),(#167462,#167463),(#167464,#167465),
(#167466,#167467),(#167468,#167469),(#167470,#167471),(#167472,#167473),
(#167474,#167475),(#167476,#167477),(#167478,#167479),(#167480,#167481),
(#167482,#167483),(#167484,#167485),(#167486,#167487),(#167488,#167489),
(#167490,#167491),(#167492,#167493),(#167494,#167495),(#167496,#167497),
(#167498,#167499),(#167500,#167501),(#167502,#167503),(#167504,#167505),
(#167506,#167507),(#167508,#167509),(#167510,#167511),(#167512,#167513),
(#167514,#167515),(#167516,#167517),(#167518,#167519),(#167520,#167521),
(#167522,#167523),(#167524,#167525),(#167526,#167527),(#167528,#167529),
(#167530,#167531),(#167532,#167533),(#167534,#167535),(#167536,#167537),
(#167538,#167539),(#167540,#167541),(#167542,#167543),(#167544,#167545),
(#167546,#167547),(#167548,#167549),(#167550,#167551),(#167552,#167553),
(#167554,#167555),(#167556,#167557),(#167558,#167559),(#167560,#167561),
(#167562,#167563),(#167564,#167565),(#167566,#167567),(#167568,#167569),
(#167570,#167571),(#167572,#167573),(#167574,#167575),(#167576,#167577),
(#167578,#167579),(#167580,#167581),(#167582,#167583),(#167584,#167585),
(#167586,#167587),(#167588,#167589),(#167590,#167591),(#167592,#167593),
(#167594,#167595),(#167596,#167597),(#167598,#167599),(#167600,#167601),
(#167602,#167603),(#167604,#167605),(#167606,#167607),(#167608,#167609),
(#167610,#167611),(#167612,#167613),(#167614,#167615),(#167616,#167617),
(#167618,#167619),(#167620,#167621),(#167622,#167623),(#167624,#167625),
(#167626,#167627),(#167628,#167629),(#167630,#167631),(#167632,#167633),
(#167634,#167635),(#167636,#167637),(#167638,#167639),(#167640,#167641),
(#167642,#167643),(#167644,#167645),(#167646,#167647),(#167648,#167649),
(#167650,#167651),(#167652,#167653),(#167654,#167655),(#167656,#167657),
(#167658,#167659),(#167660,#167661),(#167662,#167663),(#167664,#167665),
(#167666,#167667),(#167668,#167669),(#167670,#167671),(#167672,#167673),
(#167674,#167675),(#167676,#167677),(#167678,#167679),(#167680,#167681),
(#167682,#167683),(#167684,#167685),(#167686,#167687),(#167688,#167689),
(#167690,#167691),(#167692,#167693),(#167694,#167695),(#167696,#167697),
(#167698,#167699),(#167700,#167701),(#167702,#167703),(#167704,#167705),
(#167706,#167707),(#167708,#167709),(#167710,#167711),(#167712,#167713),
(#167714,#167715),(#167716,#167717),(#167718,#167719),(#167720,#167721),
(#167722,#167723),(#167724,#167725),(#167726,#167727),(#167728,#167729),
(#167730,#167731),(#167732,#167733),(#167734,#167735),(#167736,#167737),
(#167738,#167739),(#167740,#167741),(#167742,#167743),(#167744,#167745),
(#167746,#167747),(#167748,#167749),(#167750,#167751),(#167752,#167753),
(#167754,#167755),(#167756,#167757),(#167758,#167759),(#167760,#167761),
(#167762,#167763),(#167764,#167765),(#167766,#167767),(#167768,#167769),
(#167770,#167771),(#167772,#167773),(#167774,#167775),(#167776,#167777),
(#167778,#167779),(#167780,#167781),(#167782,#167783),(#167784,#167785),
(#167786,#167787),(#167788,#167789),(#167790,#167791),(#167792,#167793),
(#167794,#167795),(#167796,#167797),(#167798,#167799),(#167800,#167801),
(#167802,#167803),(#167804,#167805),(#167806,#167807),(#167808,#167809),
(#167810,#167811),(#167812,#167813),(#167814,#167815),(#167816,#167817),
(#167818,#167819),(#167820,#167821),(#167822,#167823),(#167824,#167825),
(#167826,#167827),(#167828,#167829),(#167830,#167831),(#167832,#167833),
(#167834,#167835),(#167836,#167837),(#167838,#167839),(#167840,#167841),
(#167842,#167843),(#167844,#167845),(#167846,#167847),(#167848,#167849),
(#167850,#167851),(#167852,#167853),(#167854,#167855),(#167856,#167857),
(#167858,#167859),(#167860,#167861),(#167862,#167863),(#167864,#167865),
(#167866,#167867),(#167868,#167869),(#167870,#167871),(#167872,#167873),
(#167874,#167875),(#167876,#167877),(#167878,#167879),(#167880,#167881),
(#167882,#167883),(#167884,#167885),(#167886,#167887),(#167888,#167889),
(#167890,#167891),(#167892,#167893),(#167894,#167895),(#167896,#167897),
(#167898,#167899),(#167900,#167901),(#167902,#167903),(#167904,#167905),
(#167906,#167907),(#167908,#167909),(#167910,#167911),(#167912,#167913),
(#167914,#167915),(#167916,#167917),(#167918,#167919),(#167920,#167921),
(#167922,#167923),(#167924,#167925),(#167926,#167927),(#167928,#167929),
(#167930,#167931),(#167932,#167933),(#167934,#167935),(#167936,#167937),
(#167938,#167939),(#167940,#167941),(#167942,#167943),(#167944,#167945),
(#167946,#167947),(#167948,#167949),(#167950,#167951),(#167952,#167953),
(#167954,#167955),(#167956,#167957),(#167958,#167959),(#167960,#167961),
(#167962,#167963),(#167964,#167965),(#167966,#167967),(#167968,#167969),
(#167970,#167971),(#167972,#167973),(#167974,#167975),(#167976,#167977),
(#167978,#167979),(#167980,#167981),(#167982,#167983),(#167984,#167985),
(#167986,#167987),(#167988,#167989),(#167990,#167991),(#167992,#167993),
(#167994,#167995),(#167996,#167997),(#167998,#167999),(#168000,#168001),
(#168002,#168003),(#168004,#168005),(#168006,#168007),(#168008,#168009),
(#168010,#168011),(#168012,#168013),(#168014,#168015),(#168016,#168017),
(#168018,#168019),(#168020,#168021),(#168022,#168023),(#168024,#168025),
(#168026,#168027),(#168028,#168029),(#168030,#168031),(#168032,#168033),
(#168034,#168035),(#168036,#168037),(#168038,#168039),(#168040,#168041),
(#168042,#168043),(#168044,#168045),(#168046,#168047),(#168048,#168049),
(#168050,#168051),(#168052,#168053),(#168054,#168055),(#168056,#168057),
(#168058,#168059),(#168060,#168061),(#168062,#168063),(#168064,#168065),
(#168066,#168067),(#168068,#168069),(#168070,#168071),(#168072,#168073),
(#168074,#168075),(#168076,#168077),(#168078,#168079),(#168080,#168081),
(#168082,#168083),(#168084,#168085),(#168086,#168087),(#168088,#168089),
(#168090,#168091),(#168092,#168093),(#168094,#168095),(#168096,#168097),
(#168098,#168099),(#168100,#168101),(#168102,#168103),(#168104,#168105),
(#168106,#168107),(#168108,#168109),(#168110,#168111),(#168112,#168113),
(#168114,#168115),(#168116,#168117),(#168118,#168119),(#168120,#168121),
(#168122,#168123),(#168124,#168125),(#168126,#168127),(#168128,#168129),
(#168130,#168131),(#168132,#168133),(#168134,#168135),(#168136,#168137),
(#168138,#168139),(#168140,#168141),(#168142,#168143),(#168144,#168145),
(#168146,#168147),(#168148,#168149),(#168150,#168151),(#168152,#168153),
(#168154,#168155),(#168156,#168157),(#168158,#168159),(#168160,#168161),
(#168162,#168163),(#168164,#168165),(#168166,#168167),(#168168,#168169),
(#168170,#168171),(#168172,#168173)),.UNSPECIFIED.,.F.,.F.,.F.,(6,1,1,1,
1,1,1,1,1,1,1,1,1,1,1,1,1,1,1,1,1,1,1,1,1,1,1,1,1,1,1,1,1,1,1,1,1,1,1,1,
1,1,1,1,1,1,1,1,1,1,1,1,1,1,1,1,1,1,1,1,1,1,1,1,1,1,1,1,1,1,1,1,1,1,1,1,
1,1,1,1,1,1,1,1,1,1,1,1,1,1,1,1,1,1,1,1,1,1,1,1,1,1,1,1,1,1,1,1,1,1,1,1,
1,1,1,1,1,1,1,1,1,1,1,1,1,1,1,1,1,1,1,1,1,1,1,1,1,1,1,1,1,1,1,1,1,1,1,1,
1,1,1,1,1,1,1,1,1,1,1,1,1,1,1,1,1,1,1,1,1,1,1,1,1,1,1,1,1,1,1,1,1,1,1,1,
1,1,1,1,1,1,1,1,1,1,1,1,1,1,1,1,1,1,1,1,1,1,1,1,1,1,1,1,1,1,1,1,1,1,1,1,
1,1,1,1,1,1,1,1,1,1,1,1,1,1,1,1,1,1,1,1,1,1,1,1,1,1,1,1,1,1,1,1,1,1,1,1,
1,1,1,1,1,1,1,1,1,1,1,1,1,1,1,1,1,1,1,1,1,1,1,1,1,1,1,1,1,1,1,1,1,1,1,1,
1,1,1,1,1,1,1,1,1,1,1,1,1,1,1,1,1,1,1,1,1,1,1,1,1,1,1,1,1,1,1,1,1,1,1,1,
1,1,1,1,1,1,1,1,1,1,1,1,1,1,1,1,1,1,1,1,1,1,1,1,1,1,1,1,1,1,1,1,1,1,1,1,
1,1,1,1,1,1,1,1,1,1,1,1,1,1,1,1,1,1,1,1,1,1,1,1,1,1,1,1,1,1,1,1,1,1,1,1,
1,1,1,1,1,1,1,1,1,1,1,1,1,1,1,1,1,1,1,1,1,1,1,1,1,1,1,1,1,1,1,1,1,1,1,1,
1,1,1,1,1,1,1,1,1,1,1,1,1,1,1,1,1,1,1,1,1,1,1,1,1,1,1,1,1,1,1,6),(2,2),
(0.143172103,0.144954128,0.146788991,0.148623853,0.150458716,0.152293578,
0.15412844,0.155963303,0.157798165,0.159633028,0.16146789,0.163302752,0.165137615,
0.166972477,0.168807339,0.170642202,0.172477064,0.174311927,0.176146789,
0.177981651,0.179816514,0.181651376,0.183486239,0.185321101,0.187155963,
0.188990826,0.190825688,0.19266055,0.194495413,0.196330275,0.198165138,
0.2,0.201834862,0.203669725,0.205504587,0.20733945,0.209174312,0.211009174,
0.212844037,0.214678899,0.216513761,0.218348624,0.220183486,0.222018349,
0.223853211,0.225688073,0.227522936,0.229357798,0.231192661,0.233027523,
0.234862385,0.236697248,0.23853211,0.240366972,0.242201835,0.244036697,
0.24587156,0.247706422,0.249541284,0.251376147,0.253211009,0.255045872,
0.256880734,0.258715596,0.260550459,0.262385321,0.264220183,0.266055046,
0.267889908,0.269724771,0.271559633,0.273394495,0.275229358,0.27706422,
0.278899083,0.280733945,0.282568807,0.28440367,0.286238532,0.288073394,
0.289908257,0.291743119,0.293577982,0.295412844,0.297247706,0.299082569,
0.300917431,0.302752294,0.304587156,0.306422018,0.308256881,0.310091743,
0.311926606,0.313761468,0.31559633,0.317431193,0.319266055,0.321100917,
0.32293578,0.324770642,0.326605505,0.328440367,0.330275229,0.332110092,
0.333944954,0.335779817,0.337614679,0.339449541,0.341284404,0.343119266,
0.344954128,0.346788991,0.348623853,0.350458716,0.352293578,0.35412844,
0.355963303,0.357798165,0.359633028,0.36146789,0.363302752,0.365137615,
0.366972477,0.368807339,0.370642202,0.372477064,0.374311927,0.376146789,
0.377981651,0.379816514,0.381651376,0.383486239,0.385321101,0.387155963,
0.388990826,0.390825688,0.39266055,0.394495413,0.396330275,0.398165138,
0.4,0.401834862,0.403669725,0.405504587,0.40733945,0.409174312,0.411009174,
0.412844037,0.414678899,0.416513761,0.418348624,0.420183486,0.422018349,
0.423853211,0.425688073,0.427522936,0.429357798,0.431192661,0.433027523,
0.434862385,0.436697248,0.43853211,0.440366972,0.442201835,0.444036697,
0.44587156,0.447706422,0.449541284,0.451376147,0.453211009,0.455045872,
0.456880734,0.458715596,0.460550459,0.462385321,0.464220183,0.466055046,
0.467889908,0.469724771,0.471559633,0.473394495,0.475229358,0.47706422,
0.478899083,0.480733945,0.482568807,0.48440367,0.486238532,0.488073394,
0.489908257,0.491743119,0.493577982,0.495412844,0.497247706,0.499082569,
0.500917431,0.502752294,0.504587156,0.506422018,0.508256881,0.510091743,
0.511926606,0.513761468,0.51559633,0.517431193,0.519266055,0.521100917,
0.52293578,0.524770642,0.526605505,0.528440367,0.530275229,0.532110092,
0.533944954,0.535779817,0.537614679,0.539449541,0.541284404,0.543119266,
0.544954128,0.546788991,0.548623853,0.550458716,0.552293578,0.55412844,
0.555963303,0.557798165,0.559633028,0.56146789,0.563302752,0.565137615,
0.566972477,0.568807339,0.570642202,0.572477064,0.574311927,0.576146789,
0.577981651,0.579816514,0.581651376,0.583486239,0.585321101,0.587155963,
0.588990826,0.590825688,0.59266055,0.594495413,0.596330275,0.598165138,
0.6,0.601834862,0.603669725,0.605504587,0.60733945,0.609174312,0.611009174,
0.612844037,0.614678899,0.616513761,0.618348624,0.620183486,0.622018349,
0.623853211,0.625688073,0.627522936,0.629357798,0.631192661,0.633027523,
0.634862385,0.636697248,0.63853211,0.640366972,0.642201835,0.644036697,
0.64587156,0.647706422,0.649541284,0.651376147,0.653211009,0.655045872,
0.656880734,0.658715596,0.660550459,0.662385321,0.664220183,0.666055046,
0.667889908,0.669724771,0.671559633,0.673394495,0.675229358,0.67706422,
0.678899083,0.680733945,0.682568807,0.68440367,0.686238532,0.688073394,
0.689908257,0.691743119,0.693577982,0.695412844,0.697247706,0.699082569,
0.700917431,0.702752294,0.704587156,0.706422018,0.708256881,0.710091743,
0.711926606,0.713761468,0.71559633,0.717431193,0.719266055,0.721100917,
0.72293578,0.724770642,0.726605505,0.728440367,0.730275229,0.732110092,
0.733944954,0.735779817,0.737614679,0.739449541,0.741284404,0.743119266,
0.744954128,0.746788991,0.748623853,0.750458716,0.752293578,0.75412844,
0.755963303,0.757798165,0.759633028,0.76146789,0.763302752,0.765137615,
0.766972477,0.768807339,0.770642202,0.772477064,0.774311927,0.776146789,
0.777981651,0.779816514,0.781651376,0.783486239,0.785321101,0.787155963,
0.788990826,0.790825688,0.79266055,0.794495413,0.796330275,0.798165138,
0.8,0.801834862,0.803669725,0.805504587,0.80733945,0.809174312,0.811009174,
0.812844037,0.814678899,0.816513761,0.818348624,0.820183486,0.822018349,
0.823853211,0.825688073,0.827522936,0.829357798,0.831192661,0.833027523,
0.834862385,0.836697248,0.83853211,0.840366972,0.842201835,0.844036697,
0.84587156,0.847706422,0.849541284,0.851376147,0.853211009,0.855045872,
0.856880734,0.858715596,0.860550459,0.862385321,0.864220183,0.866055046,
0.867889908,0.869724771,0.871559633,0.873394495,0.875229358,0.87706422,
0.878899083,0.880733945,0.882568807,0.88440367,0.886238532,0.888073394,
0.889908257,0.891743119,0.893577982,0.895412844,0.897247706,0.899082569,
0.900917431,0.902752294,0.904587156,0.906422018,0.908256881,0.910091743,
0.911926606,0.913761468,0.91559633,0.917431193,0.919266055,0.921100917,
0.92293578,0.924770642,0.926605505,0.928440367,0.930275229,0.932110092,
0.933944954,0.935779817,0.937614679,0.939449541,0.941284404,0.943119266,
0.944954128,0.946788991,0.948623853,0.950458716,0.952293578,0.95412844,
0.955963303,0.957798165,0.959633028,0.96146789,0.963302752,0.965137615,
0.966972477,0.968807339,0.970642202,0.972477064,0.974311927,0.976146789,
0.977981651,0.979816514,0.981651376,0.983486239,0.985321101,0.987155963,
0.988990826,0.990825688,0.99266055,0.994495413,0.996330275,0.998165138,
1.),(0.,0.36),.UNSPECIFIED.);
#6224=B_SPLINE_SURFACE_WITH_KNOTS('',5,1,((#169118,#169119),(#169120,#169121),
(#169122,#169123),(#169124,#169125),(#169126,#169127),(#169128,#169129),
(#169130,#169131),(#169132,#169133),(#169134,#169135),(#169136,#169137),
(#169138,#169139),(#169140,#169141),(#169142,#169143),(#169144,#169145),
(#169146,#169147),(#169148,#169149),(#169150,#169151),(#169152,#169153),
(#169154,#169155),(#169156,#169157),(#169158,#169159),(#169160,#169161),
(#169162,#169163),(#169164,#169165),(#169166,#169167),(#169168,#169169),
(#169170,#169171),(#169172,#169173),(#169174,#169175),(#169176,#169177),
(#169178,#169179),(#169180,#169181),(#169182,#169183),(#169184,#169185),
(#169186,#169187),(#169188,#169189),(#169190,#169191),(#169192,#169193),
(#169194,#169195),(#169196,#169197),(#169198,#169199),(#169200,#169201),
(#169202,#169203),(#169204,#169205),(#169206,#169207),(#169208,#169209),
(#169210,#169211),(#169212,#169213),(#169214,#169215),(#169216,#169217),
(#169218,#169219),(#169220,#169221),(#169222,#169223),(#169224,#169225),
(#169226,#169227),(#169228,#169229),(#169230,#169231),(#169232,#169233),
(#169234,#169235),(#169236,#169237),(#169238,#169239),(#169240,#169241),
(#169242,#169243),(#169244,#169245),(#169246,#169247),(#169248,#169249),
(#169250,#169251),(#169252,#169253),(#169254,#169255),(#169256,#169257),
(#169258,#169259),(#169260,#169261),(#169262,#169263),(#169264,#169265),
(#169266,#169267),(#169268,#169269),(#169270,#169271),(#169272,#169273),
(#169274,#169275),(#169276,#169277),(#169278,#169279),(#169280,#169281),
(#169282,#169283),(#169284,#169285),(#169286,#169287),(#169288,#169289),
(#169290,#169291),(#169292,#169293),(#169294,#169295),(#169296,#169297),
(#169298,#169299),(#169300,#169301),(#169302,#169303),(#169304,#169305),
(#169306,#169307),(#169308,#169309),(#169310,#169311),(#169312,#169313),
(#169314,#169315),(#169316,#169317),(#169318,#169319),(#169320,#169321),
(#169322,#169323),(#169324,#169325),(#169326,#169327),(#169328,#169329),
(#169330,#169331),(#169332,#169333),(#169334,#169335),(#169336,#169337),
(#169338,#169339),(#169340,#169341),(#169342,#169343),(#169344,#169345),
(#169346,#169347),(#169348,#169349),(#169350,#169351),(#169352,#169353),
(#169354,#169355),(#169356,#169357),(#169358,#169359),(#169360,#169361),
(#169362,#169363),(#169364,#169365),(#169366,#169367),(#169368,#169369),
(#169370,#169371),(#169372,#169373),(#169374,#169375),(#169376,#169377),
(#169378,#169379),(#169380,#169381),(#169382,#169383),(#169384,#169385),
(#169386,#169387),(#169388,#169389),(#169390,#169391),(#169392,#169393),
(#169394,#169395),(#169396,#169397),(#169398,#169399),(#169400,#169401),
(#169402,#169403),(#169404,#169405),(#169406,#169407),(#169408,#169409),
(#169410,#169411),(#169412,#169413),(#169414,#169415),(#169416,#169417),
(#169418,#169419),(#169420,#169421),(#169422,#169423),(#169424,#169425),
(#169426,#169427),(#169428,#169429),(#169430,#169431),(#169432,#169433),
(#169434,#169435),(#169436,#169437),(#169438,#169439),(#169440,#169441),
(#169442,#169443),(#169444,#169445),(#169446,#169447),(#169448,#169449),
(#169450,#169451),(#169452,#169453),(#169454,#169455),(#169456,#169457),
(#169458,#169459),(#169460,#169461),(#169462,#169463),(#169464,#169465),
(#169466,#169467),(#169468,#169469),(#169470,#169471),(#169472,#169473),
(#169474,#169475),(#169476,#169477),(#169478,#169479),(#169480,#169481),
(#169482,#169483),(#169484,#169485),(#169486,#169487),(#169488,#169489),
(#169490,#169491),(#169492,#169493),(#169494,#169495),(#169496,#169497),
(#169498,#169499),(#169500,#169501),(#169502,#169503),(#169504,#169505),
(#169506,#169507),(#169508,#169509),(#169510,#169511),(#169512,#169513),
(#169514,#169515),(#169516,#169517),(#169518,#169519),(#169520,#169521),
(#169522,#169523),(#169524,#169525),(#169526,#169527),(#169528,#169529),
(#169530,#169531),(#169532,#169533),(#169534,#169535),(#169536,#169537),
(#169538,#169539),(#169540,#169541),(#169542,#169543),(#169544,#169545),
(#169546,#169547),(#169548,#169549),(#169550,#169551),(#169552,#169553),
(#169554,#169555),(#169556,#169557),(#169558,#169559),(#169560,#169561),
(#169562,#169563),(#169564,#169565),(#169566,#169567),(#169568,#169569),
(#169570,#169571),(#169572,#169573),(#169574,#169575),(#169576,#169577),
(#169578,#169579),(#169580,#169581),(#169582,#169583),(#169584,#169585),
(#169586,#169587),(#169588,#169589),(#169590,#169591),(#169592,#169593),
(#169594,#169595),(#169596,#169597),(#169598,#169599),(#169600,#169601),
(#169602,#169603),(#169604,#169605),(#169606,#169607),(#169608,#169609),
(#169610,#169611),(#169612,#169613),(#169614,#169615),(#169616,#169617),
(#169618,#169619),(#169620,#169621),(#169622,#169623),(#169624,#169625),
(#169626,#169627),(#169628,#169629),(#169630,#169631),(#169632,#169633),
(#169634,#169635),(#169636,#169637),(#169638,#169639),(#169640,#169641),
(#169642,#169643),(#169644,#169645),(#169646,#169647),(#169648,#169649),
(#169650,#169651),(#169652,#169653),(#169654,#169655),(#169656,#169657),
(#169658,#169659),(#169660,#169661),(#169662,#169663),(#169664,#169665),
(#169666,#169667),(#169668,#169669),(#169670,#169671),(#169672,#169673),
(#169674,#169675),(#169676,#169677),(#169678,#169679),(#169680,#169681),
(#169682,#169683),(#169684,#169685),(#169686,#169687),(#169688,#169689),
(#169690,#169691),(#169692,#169693),(#169694,#169695),(#169696,#169697),
(#169698,#169699),(#169700,#169701),(#169702,#169703),(#169704,#169705),
(#169706,#169707),(#169708,#169709),(#169710,#169711),(#169712,#169713),
(#169714,#169715),(#169716,#169717),(#169718,#169719),(#169720,#169721),
(#169722,#169723),(#169724,#169725),(#169726,#169727),(#169728,#169729),
(#169730,#169731),(#169732,#169733),(#169734,#169735),(#169736,#169737),
(#169738,#169739),(#169740,#169741),(#169742,#169743),(#169744,#169745),
(#169746,#169747),(#169748,#169749),(#169750,#169751),(#169752,#169753),
(#169754,#169755),(#169756,#169757),(#169758,#169759),(#169760,#169761),
(#169762,#169763),(#169764,#169765),(#169766,#169767),(#169768,#169769),
(#169770,#169771),(#169772,#169773),(#169774,#169775),(#169776,#169777),
(#169778,#169779),(#169780,#169781),(#169782,#169783),(#169784,#169785),
(#169786,#169787),(#169788,#169789),(#169790,#169791),(#169792,#169793),
(#169794,#169795),(#169796,#169797),(#169798,#169799),(#169800,#169801),
(#169802,#169803),(#169804,#169805),(#169806,#169807),(#169808,#169809),
(#169810,#169811),(#169812,#169813),(#169814,#169815),(#169816,#169817),
(#169818,#169819),(#169820,#169821),(#169822,#169823),(#169824,#169825),
(#169826,#169827),(#169828,#169829),(#169830,#169831),(#169832,#169833),
(#169834,#169835),(#169836,#169837),(#169838,#169839),(#169840,#169841),
(#169842,#169843),(#169844,#169845),(#169846,#169847),(#169848,#169849),
(#169850,#169851),(#169852,#169853),(#169854,#169855),(#169856,#169857),
(#169858,#169859),(#169860,#169861),(#169862,#169863),(#169864,#169865),
(#169866,#169867),(#169868,#169869),(#169870,#169871),(#169872,#169873),
(#169874,#169875),(#169876,#169877),(#169878,#169879),(#169880,#169881),
(#169882,#169883),(#169884,#169885),(#169886,#169887),(#169888,#169889),
(#169890,#169891),(#169892,#169893),(#169894,#169895),(#169896,#169897),
(#169898,#169899),(#169900,#169901),(#169902,#169903),(#169904,#169905),
(#169906,#169907),(#169908,#169909),(#169910,#169911),(#169912,#169913),
(#169914,#169915),(#169916,#169917),(#169918,#169919),(#169920,#169921),
(#169922,#169923),(#169924,#169925),(#169926,#169927),(#169928,#169929),
(#169930,#169931),(#169932,#169933),(#169934,#169935),(#169936,#169937),
(#169938,#169939),(#169940,#169941),(#169942,#169943),(#169944,#169945),
(#169946,#169947),(#169948,#169949),(#169950,#169951),(#169952,#169953),
(#169954,#169955),(#169956,#169957),(#169958,#169959),(#169960,#169961),
(#169962,#169963),(#169964,#169965),(#169966,#169967),(#169968,#169969),
(#169970,#169971),(#169972,#169973),(#169974,#169975),(#169976,#169977),
(#169978,#169979),(#169980,#169981),(#169982,#169983),(#169984,#169985),
(#169986,#169987),(#169988,#169989),(#169990,#169991),(#169992,#169993),
(#169994,#169995),(#169996,#169997),(#169998,#169999),(#170000,#170001),
(#170002,#170003),(#170004,#170005),(#170006,#170007),(#170008,#170009),
(#170010,#170011),(#170012,#170013),(#170014,#170015),(#170016,#170017),
(#170018,#170019),(#170020,#170021),(#170022,#170023),(#170024,#170025),
(#170026,#170027),(#170028,#170029),(#170030,#170031),(#170032,#170033),
(#170034,#170035),(#170036,#170037),(#170038,#170039),(#170040,#170041),
(#170042,#170043),(#170044,#170045),(#170046,#170047),(#170048,#170049),
(#170050,#170051),(#170052,#170053),(#170054,#170055),(#170056,#170057),
(#170058,#170059),(#170060,#170061)),.UNSPECIFIED.,.F.,.F.,.F.,(6,1,1,1,
1,1,1,1,1,1,1,1,1,1,1,1,1,1,1,1,1,1,1,1,1,1,1,1,1,1,1,1,1,1,1,1,1,1,1,1,
1,1,1,1,1,1,1,1,1,1,1,1,1,1,1,1,1,1,1,1,1,1,1,1,1,1,1,1,1,1,1,1,1,1,1,1,
1,1,1,1,1,1,1,1,1,1,1,1,1,1,1,1,1,1,1,1,1,1,1,1,1,1,1,1,1,1,1,1,1,1,1,1,
1,1,1,1,1,1,1,1,1,1,1,1,1,1,1,1,1,1,1,1,1,1,1,1,1,1,1,1,1,1,1,1,1,1,1,1,
1,1,1,1,1,1,1,1,1,1,1,1,1,1,1,1,1,1,1,1,1,1,1,1,1,1,1,1,1,1,1,1,1,1,1,1,
1,1,1,1,1,1,1,1,1,1,1,1,1,1,1,1,1,1,1,1,1,1,1,1,1,1,1,1,1,1,1,1,1,1,1,1,
1,1,1,1,1,1,1,1,1,1,1,1,1,1,1,1,1,1,1,1,1,1,1,1,1,1,1,1,1,1,1,1,1,1,1,1,
1,1,1,1,1,1,1,1,1,1,1,1,1,1,1,1,1,1,1,1,1,1,1,1,1,1,1,1,1,1,1,1,1,1,1,1,
1,1,1,1,1,1,1,1,1,1,1,1,1,1,1,1,1,1,1,1,1,1,1,1,1,1,1,1,1,1,1,1,1,1,1,1,
1,1,1,1,1,1,1,1,1,1,1,1,1,1,1,1,1,1,1,1,1,1,1,1,1,1,1,1,1,1,1,1,1,1,1,1,
1,1,1,1,1,1,1,1,1,1,1,1,1,1,1,1,1,1,1,1,1,1,1,1,1,1,1,1,1,1,1,1,1,1,1,1,
1,1,1,1,1,1,1,1,1,1,1,1,1,1,1,1,1,1,1,1,1,1,1,1,1,1,1,1,1,1,1,1,1,1,1,1,
1,1,1,1,1,1,1,1,1,1,1,1,1,1,1,1,1,1,1,1,1,1,1,1,1,1,1,1,1,1,1,6),(2,2),
(-1.,-0.998165138,-0.996330275,-0.994495413,-0.99266055,-0.990825688,-0.988990826,
-0.987155963,-0.985321101,-0.983486239,-0.981651376,-0.979816514,-0.977981651,
-0.976146789,-0.974311927,-0.972477064,-0.970642202,-0.968807339,-0.966972477,
-0.965137615,-0.963302752,-0.96146789,-0.959633028,-0.957798165,-0.955963303,
-0.95412844,-0.952293578,-0.950458716,-0.948623853,-0.946788991,-0.944954128,
-0.943119266,-0.941284404,-0.939449541,-0.937614679,-0.935779817,-0.933944954,
-0.932110092,-0.930275229,-0.928440367,-0.926605505,-0.924770642,-0.92293578,
-0.921100917,-0.919266055,-0.917431193,-0.91559633,-0.913761468,-0.911926606,
-0.910091743,-0.908256881,-0.906422018,-0.904587156,-0.902752294,-0.900917431,
-0.899082569,-0.897247706,-0.895412844,-0.893577982,-0.891743119,-0.889908257,
-0.888073394,-0.886238532,-0.88440367,-0.882568807,-0.880733945,-0.878899083,
-0.87706422,-0.875229358,-0.873394495,-0.871559633,-0.869724771,-0.867889908,
-0.866055046,-0.864220183,-0.862385321,-0.860550459,-0.858715596,-0.856880734,
-0.855045872,-0.853211009,-0.851376147,-0.849541284,-0.847706422,-0.84587156,
-0.844036697,-0.842201835,-0.840366972,-0.83853211,-0.836697248,-0.834862385,
-0.833027523,-0.831192661,-0.829357798,-0.827522936,-0.825688073,-0.823853211,
-0.822018349,-0.820183486,-0.818348624,-0.816513761,-0.814678899,-0.812844037,
-0.811009174,-0.809174312,-0.80733945,-0.805504587,-0.803669725,-0.801834862,
-0.8,-0.798165138,-0.796330275,-0.794495413,-0.79266055,-0.790825688,-0.788990826,
-0.787155963,-0.785321101,-0.783486239,-0.781651376,-0.779816514,-0.777981651,
-0.776146789,-0.774311927,-0.772477064,-0.770642202,-0.768807339,-0.766972477,
-0.765137615,-0.763302752,-0.76146789,-0.759633028,-0.757798165,-0.755963303,
-0.75412844,-0.752293578,-0.750458716,-0.748623853,-0.746788991,-0.744954128,
-0.743119266,-0.741284404,-0.739449541,-0.737614679,-0.735779817,-0.733944954,
-0.732110092,-0.730275229,-0.728440367,-0.726605505,-0.724770642,-0.72293578,
-0.721100917,-0.719266055,-0.717431193,-0.71559633,-0.713761468,-0.711926606,
-0.710091743,-0.708256881,-0.706422018,-0.704587156,-0.702752294,-0.700917431,
-0.699082569,-0.697247706,-0.695412844,-0.693577982,-0.691743119,-0.689908257,
-0.688073394,-0.686238532,-0.68440367,-0.682568807,-0.680733945,-0.678899083,
-0.67706422,-0.675229358,-0.673394495,-0.671559633,-0.669724771,-0.667889908,
-0.666055046,-0.664220183,-0.662385321,-0.660550459,-0.658715596,-0.656880734,
-0.655045872,-0.653211009,-0.651376147,-0.649541284,-0.647706422,-0.64587156,
-0.644036697,-0.642201835,-0.640366972,-0.63853211,-0.636697248,-0.634862385,
-0.633027523,-0.631192661,-0.629357798,-0.627522936,-0.625688073,-0.623853211,
-0.622018349,-0.620183486,-0.618348624,-0.616513761,-0.614678899,-0.612844037,
-0.611009174,-0.609174312,-0.60733945,-0.605504587,-0.603669725,-0.601834862,
-0.6,-0.598165138,-0.596330275,-0.594495413,-0.59266055,-0.590825688,-0.588990826,
-0.587155963,-0.585321101,-0.583486239,-0.581651376,-0.579816514,-0.577981651,
-0.576146789,-0.574311927,-0.572477064,-0.570642202,-0.568807339,-0.566972477,
-0.565137615,-0.563302752,-0.56146789,-0.559633028,-0.557798165,-0.555963303,
-0.55412844,-0.552293578,-0.550458716,-0.548623853,-0.546788991,-0.544954128,
-0.543119266,-0.541284404,-0.539449541,-0.537614679,-0.535779817,-0.533944954,
-0.532110092,-0.530275229,-0.528440367,-0.526605505,-0.524770642,-0.52293578,
-0.521100917,-0.519266055,-0.517431193,-0.51559633,-0.513761468,-0.511926606,
-0.510091743,-0.508256881,-0.506422018,-0.504587156,-0.502752294,-0.500917431,
-0.499082569,-0.497247706,-0.495412844,-0.493577982,-0.491743119,-0.489908257,
-0.488073394,-0.486238532,-0.48440367,-0.482568807,-0.480733945,-0.478899083,
-0.47706422,-0.475229358,-0.473394495,-0.471559633,-0.469724771,-0.467889908,
-0.466055046,-0.464220183,-0.462385321,-0.460550459,-0.458715596,-0.456880734,
-0.455045872,-0.453211009,-0.451376147,-0.449541284,-0.447706422,-0.44587156,
-0.444036697,-0.442201835,-0.440366972,-0.43853211,-0.436697248,-0.434862385,
-0.433027523,-0.431192661,-0.429357798,-0.427522936,-0.425688073,-0.423853211,
-0.422018349,-0.420183486,-0.418348624,-0.416513761,-0.414678899,-0.412844037,
-0.411009174,-0.409174312,-0.40733945,-0.405504587,-0.403669725,-0.401834862,
-0.4,-0.398165138,-0.396330275,-0.394495413,-0.39266055,-0.390825688,-0.388990826,
-0.387155963,-0.385321101,-0.383486239,-0.381651376,-0.379816514,-0.377981651,
-0.376146789,-0.374311927,-0.372477064,-0.370642202,-0.368807339,-0.366972477,
-0.365137615,-0.363302752,-0.36146789,-0.359633028,-0.357798165,-0.355963303,
-0.35412844,-0.352293578,-0.350458716,-0.348623853,-0.346788991,-0.344954128,
-0.343119266,-0.341284404,-0.339449541,-0.337614679,-0.335779817,-0.333944954,
-0.332110092,-0.330275229,-0.328440367,-0.326605505,-0.324770642,-0.32293578,
-0.321100917,-0.319266055,-0.317431193,-0.31559633,-0.313761468,-0.311926606,
-0.310091743,-0.308256881,-0.306422018,-0.304587156,-0.302752294,-0.300917431,
-0.299082569,-0.297247706,-0.295412844,-0.293577982,-0.291743119,-0.289908257,
-0.288073394,-0.286238532,-0.28440367,-0.282568807,-0.280733945,-0.278899083,
-0.27706422,-0.275229358,-0.273394495,-0.271559633,-0.269724771,-0.267889908,
-0.266055046,-0.264220183,-0.262385321,-0.260550459,-0.258715596,-0.256880734,
-0.255045872,-0.253211009,-0.251376147,-0.249541284,-0.247706422,-0.24587156,
-0.244036697,-0.242201835,-0.240366972,-0.23853211,-0.236697248,-0.234862385,
-0.233027523,-0.231192661,-0.229357798,-0.227522936,-0.225688073,-0.223853211,
-0.222018349,-0.220183486,-0.218348624,-0.216513761,-0.214678899,-0.212844037,
-0.211009174,-0.209174312,-0.20733945,-0.205504587,-0.203669725,-0.201834862,
-0.2,-0.198165138,-0.196330275,-0.194495413,-0.19266055,-0.190825688,-0.188990826,
-0.187155963,-0.185321101,-0.183486239,-0.181651376,-0.179816514,-0.177981651,
-0.176146789,-0.174311927,-0.172477064,-0.170642202,-0.168807339,-0.166972477,
-0.165137615,-0.163302752,-0.16146789,-0.159633028,-0.157798165,-0.155963303,
-0.15412844,-0.152293578,-0.150458716,-0.148623853,-0.146788991,-0.144954128,
-0.143172103),(0.,0.36),.UNSPECIFIED.);
#6225=B_SPLINE_SURFACE_WITH_KNOTS('',5,1,((#171024,#171025),(#171026,#171027),
(#171028,#171029),(#171030,#171031),(#171032,#171033),(#171034,#171035),
(#171036,#171037),(#171038,#171039),(#171040,#171041),(#171042,#171043),
(#171044,#171045),(#171046,#171047),(#171048,#171049),(#171050,#171051),
(#171052,#171053),(#171054,#171055),(#171056,#171057),(#171058,#171059),
(#171060,#171061),(#171062,#171063),(#171064,#171065),(#171066,#171067),
(#171068,#171069),(#171070,#171071),(#171072,#171073),(#171074,#171075),
(#171076,#171077),(#171078,#171079),(#171080,#171081),(#171082,#171083),
(#171084,#171085),(#171086,#171087),(#171088,#171089),(#171090,#171091),
(#171092,#171093),(#171094,#171095),(#171096,#171097),(#171098,#171099),
(#171100,#171101),(#171102,#171103),(#171104,#171105),(#171106,#171107),
(#171108,#171109),(#171110,#171111),(#171112,#171113),(#171114,#171115),
(#171116,#171117),(#171118,#171119),(#171120,#171121),(#171122,#171123),
(#171124,#171125),(#171126,#171127),(#171128,#171129),(#171130,#171131),
(#171132,#171133),(#171134,#171135),(#171136,#171137),(#171138,#171139),
(#171140,#171141),(#171142,#171143),(#171144,#171145),(#171146,#171147),
(#171148,#171149),(#171150,#171151),(#171152,#171153),(#171154,#171155),
(#171156,#171157),(#171158,#171159),(#171160,#171161),(#171162,#171163),
(#171164,#171165),(#171166,#171167),(#171168,#171169),(#171170,#171171),
(#171172,#171173),(#171174,#171175),(#171176,#171177),(#171178,#171179),
(#171180,#171181),(#171182,#171183),(#171184,#171185),(#171186,#171187),
(#171188,#171189),(#171190,#171191),(#171192,#171193),(#171194,#171195),
(#171196,#171197),(#171198,#171199),(#171200,#171201),(#171202,#171203),
(#171204,#171205),(#171206,#171207),(#171208,#171209),(#171210,#171211),
(#171212,#171213),(#171214,#171215),(#171216,#171217),(#171218,#171219),
(#171220,#171221),(#171222,#171223),(#171224,#171225),(#171226,#171227),
(#171228,#171229),(#171230,#171231),(#171232,#171233),(#171234,#171235),
(#171236,#171237),(#171238,#171239),(#171240,#171241),(#171242,#171243),
(#171244,#171245),(#171246,#171247),(#171248,#171249),(#171250,#171251),
(#171252,#171253),(#171254,#171255),(#171256,#171257),(#171258,#171259),
(#171260,#171261),(#171262,#171263),(#171264,#171265),(#171266,#171267),
(#171268,#171269),(#171270,#171271),(#171272,#171273),(#171274,#171275),
(#171276,#171277),(#171278,#171279),(#171280,#171281),(#171282,#171283),
(#171284,#171285),(#171286,#171287),(#171288,#171289),(#171290,#171291),
(#171292,#171293),(#171294,#171295),(#171296,#171297),(#171298,#171299),
(#171300,#171301),(#171302,#171303),(#171304,#171305),(#171306,#171307),
(#171308,#171309),(#171310,#171311),(#171312,#171313),(#171314,#171315),
(#171316,#171317),(#171318,#171319),(#171320,#171321),(#171322,#171323),
(#171324,#171325),(#171326,#171327),(#171328,#171329),(#171330,#171331),
(#171332,#171333),(#171334,#171335),(#171336,#171337),(#171338,#171339),
(#171340,#171341),(#171342,#171343),(#171344,#171345),(#171346,#171347),
(#171348,#171349),(#171350,#171351),(#171352,#171353),(#171354,#171355),
(#171356,#171357),(#171358,#171359),(#171360,#171361),(#171362,#171363),
(#171364,#171365),(#171366,#171367),(#171368,#171369),(#171370,#171371),
(#171372,#171373),(#171374,#171375),(#171376,#171377),(#171378,#171379),
(#171380,#171381),(#171382,#171383),(#171384,#171385),(#171386,#171387),
(#171388,#171389),(#171390,#171391),(#171392,#171393),(#171394,#171395),
(#171396,#171397),(#171398,#171399),(#171400,#171401),(#171402,#171403),
(#171404,#171405),(#171406,#171407),(#171408,#171409),(#171410,#171411),
(#171412,#171413),(#171414,#171415),(#171416,#171417),(#171418,#171419),
(#171420,#171421),(#171422,#171423),(#171424,#171425),(#171426,#171427),
(#171428,#171429),(#171430,#171431),(#171432,#171433),(#171434,#171435),
(#171436,#171437),(#171438,#171439),(#171440,#171441),(#171442,#171443),
(#171444,#171445),(#171446,#171447),(#171448,#171449),(#171450,#171451),
(#171452,#171453),(#171454,#171455),(#171456,#171457),(#171458,#171459),
(#171460,#171461),(#171462,#171463),(#171464,#171465),(#171466,#171467),
(#171468,#171469),(#171470,#171471),(#171472,#171473),(#171474,#171475),
(#171476,#171477),(#171478,#171479),(#171480,#171481),(#171482,#171483),
(#171484,#171485),(#171486,#171487),(#171488,#171489),(#171490,#171491),
(#171492,#171493),(#171494,#171495),(#171496,#171497),(#171498,#171499),
(#171500,#171501),(#171502,#171503),(#171504,#171505),(#171506,#171507),
(#171508,#171509),(#171510,#171511),(#171512,#171513),(#171514,#171515),
(#171516,#171517),(#171518,#171519),(#171520,#171521),(#171522,#171523),
(#171524,#171525),(#171526,#171527),(#171528,#171529),(#171530,#171531),
(#171532,#171533),(#171534,#171535),(#171536,#171537),(#171538,#171539),
(#171540,#171541),(#171542,#171543),(#171544,#171545),(#171546,#171547),
(#171548,#171549),(#171550,#171551),(#171552,#171553),(#171554,#171555),
(#171556,#171557),(#171558,#171559),(#171560,#171561),(#171562,#171563),
(#171564,#171565),(#171566,#171567),(#171568,#171569),(#171570,#171571),
(#171572,#171573),(#171574,#171575),(#171576,#171577),(#171578,#171579),
(#171580,#171581),(#171582,#171583),(#171584,#171585),(#171586,#171587),
(#171588,#171589),(#171590,#171591),(#171592,#171593),(#171594,#171595),
(#171596,#171597),(#171598,#171599),(#171600,#171601),(#171602,#171603),
(#171604,#171605),(#171606,#171607),(#171608,#171609),(#171610,#171611),
(#171612,#171613),(#171614,#171615),(#171616,#171617),(#171618,#171619),
(#171620,#171621),(#171622,#171623),(#171624,#171625),(#171626,#171627),
(#171628,#171629),(#171630,#171631),(#171632,#171633),(#171634,#171635),
(#171636,#171637),(#171638,#171639),(#171640,#171641),(#171642,#171643),
(#171644,#171645),(#171646,#171647),(#171648,#171649),(#171650,#171651),
(#171652,#171653),(#171654,#171655),(#171656,#171657),(#171658,#171659),
(#171660,#171661),(#171662,#171663),(#171664,#171665),(#171666,#171667),
(#171668,#171669),(#171670,#171671),(#171672,#171673),(#171674,#171675),
(#171676,#171677),(#171678,#171679),(#171680,#171681),(#171682,#171683),
(#171684,#171685),(#171686,#171687),(#171688,#171689),(#171690,#171691),
(#171692,#171693),(#171694,#171695),(#171696,#171697),(#171698,#171699),
(#171700,#171701),(#171702,#171703),(#171704,#171705),(#171706,#171707),
(#171708,#171709),(#171710,#171711),(#171712,#171713),(#171714,#171715),
(#171716,#171717),(#171718,#171719),(#171720,#171721),(#171722,#171723),
(#171724,#171725),(#171726,#171727),(#171728,#171729),(#171730,#171731),
(#171732,#171733),(#171734,#171735),(#171736,#171737),(#171738,#171739),
(#171740,#171741),(#171742,#171743),(#171744,#171745),(#171746,#171747),
(#171748,#171749),(#171750,#171751),(#171752,#171753),(#171754,#171755),
(#171756,#171757),(#171758,#171759),(#171760,#171761),(#171762,#171763),
(#171764,#171765),(#171766,#171767),(#171768,#171769),(#171770,#171771),
(#171772,#171773),(#171774,#171775),(#171776,#171777),(#171778,#171779),
(#171780,#171781),(#171782,#171783),(#171784,#171785),(#171786,#171787),
(#171788,#171789),(#171790,#171791),(#171792,#171793),(#171794,#171795),
(#171796,#171797),(#171798,#171799),(#171800,#171801),(#171802,#171803),
(#171804,#171805),(#171806,#171807),(#171808,#171809),(#171810,#171811),
(#171812,#171813),(#171814,#171815),(#171816,#171817),(#171818,#171819),
(#171820,#171821),(#171822,#171823),(#171824,#171825),(#171826,#171827),
(#171828,#171829),(#171830,#171831),(#171832,#171833),(#171834,#171835),
(#171836,#171837),(#171838,#171839),(#171840,#171841),(#171842,#171843),
(#171844,#171845),(#171846,#171847),(#171848,#171849),(#171850,#171851),
(#171852,#171853),(#171854,#171855),(#171856,#171857),(#171858,#171859),
(#171860,#171861),(#171862,#171863),(#171864,#171865),(#171866,#171867),
(#171868,#171869),(#171870,#171871),(#171872,#171873),(#171874,#171875),
(#171876,#171877),(#171878,#171879),(#171880,#171881),(#171882,#171883),
(#171884,#171885),(#171886,#171887),(#171888,#171889),(#171890,#171891),
(#171892,#171893),(#171894,#171895),(#171896,#171897),(#171898,#171899),
(#171900,#171901),(#171902,#171903),(#171904,#171905),(#171906,#171907),
(#171908,#171909),(#171910,#171911),(#171912,#171913),(#171914,#171915),
(#171916,#171917),(#171918,#171919),(#171920,#171921),(#171922,#171923),
(#171924,#171925),(#171926,#171927),(#171928,#171929),(#171930,#171931),
(#171932,#171933),(#171934,#171935),(#171936,#171937),(#171938,#171939),
(#171940,#171941),(#171942,#171943),(#171944,#171945),(#171946,#171947),
(#171948,#171949),(#171950,#171951),(#171952,#171953),(#171954,#171955),
(#171956,#171957),(#171958,#171959),(#171960,#171961),(#171962,#171963),
(#171964,#171965),(#171966,#171967)),.UNSPECIFIED.,.F.,.F.,.F.,(6,1,1,1,
1,1,1,1,1,1,1,1,1,1,1,1,1,1,1,1,1,1,1,1,1,1,1,1,1,1,1,1,1,1,1,1,1,1,1,1,
1,1,1,1,1,1,1,1,1,1,1,1,1,1,1,1,1,1,1,1,1,1,1,1,1,1,1,1,1,1,1,1,1,1,1,1,
1,1,1,1,1,1,1,1,1,1,1,1,1,1,1,1,1,1,1,1,1,1,1,1,1,1,1,1,1,1,1,1,1,1,1,1,
1,1,1,1,1,1,1,1,1,1,1,1,1,1,1,1,1,1,1,1,1,1,1,1,1,1,1,1,1,1,1,1,1,1,1,1,
1,1,1,1,1,1,1,1,1,1,1,1,1,1,1,1,1,1,1,1,1,1,1,1,1,1,1,1,1,1,1,1,1,1,1,1,
1,1,1,1,1,1,1,1,1,1,1,1,1,1,1,1,1,1,1,1,1,1,1,1,1,1,1,1,1,1,1,1,1,1,1,1,
1,1,1,1,1,1,1,1,1,1,1,1,1,1,1,1,1,1,1,1,1,1,1,1,1,1,1,1,1,1,1,1,1,1,1,1,
1,1,1,1,1,1,1,1,1,1,1,1,1,1,1,1,1,1,1,1,1,1,1,1,1,1,1,1,1,1,1,1,1,1,1,1,
1,1,1,1,1,1,1,1,1,1,1,1,1,1,1,1,1,1,1,1,1,1,1,1,1,1,1,1,1,1,1,1,1,1,1,1,
1,1,1,1,1,1,1,1,1,1,1,1,1,1,1,1,1,1,1,1,1,1,1,1,1,1,1,1,1,1,1,1,1,1,1,1,
1,1,1,1,1,1,1,1,1,1,1,1,1,1,1,1,1,1,1,1,1,1,1,1,1,1,1,1,1,1,1,1,1,1,1,1,
1,1,1,1,1,1,1,1,1,1,1,1,1,1,1,1,1,1,1,1,1,1,1,1,1,1,1,1,1,1,1,1,1,1,1,1,
1,1,1,1,1,1,1,1,1,1,1,1,1,1,1,1,1,1,1,1,1,1,1,1,1,1,1,1,1,1,1,6),(2,2),
(-1.,-0.998165138,-0.996330275,-0.994495413,-0.99266055,-0.990825688,-0.988990826,
-0.987155963,-0.985321101,-0.983486239,-0.981651376,-0.979816514,-0.977981651,
-0.976146789,-0.974311927,-0.972477064,-0.970642202,-0.968807339,-0.966972477,
-0.965137615,-0.963302752,-0.96146789,-0.959633028,-0.957798165,-0.955963303,
-0.95412844,-0.952293578,-0.950458716,-0.948623853,-0.946788991,-0.944954128,
-0.943119266,-0.941284404,-0.939449541,-0.937614679,-0.935779817,-0.933944954,
-0.932110092,-0.930275229,-0.928440367,-0.926605505,-0.924770642,-0.92293578,
-0.921100917,-0.919266055,-0.917431193,-0.91559633,-0.913761468,-0.911926606,
-0.910091743,-0.908256881,-0.906422018,-0.904587156,-0.902752294,-0.900917431,
-0.899082569,-0.897247706,-0.895412844,-0.893577982,-0.891743119,-0.889908257,
-0.888073394,-0.886238532,-0.88440367,-0.882568807,-0.880733945,-0.878899083,
-0.87706422,-0.875229358,-0.873394495,-0.871559633,-0.869724771,-0.867889908,
-0.866055046,-0.864220183,-0.862385321,-0.860550459,-0.858715596,-0.856880734,
-0.855045872,-0.853211009,-0.851376147,-0.849541284,-0.847706422,-0.84587156,
-0.844036697,-0.842201835,-0.840366972,-0.83853211,-0.836697248,-0.834862385,
-0.833027523,-0.831192661,-0.829357798,-0.827522936,-0.825688073,-0.823853211,
-0.822018349,-0.820183486,-0.818348624,-0.816513761,-0.814678899,-0.812844037,
-0.811009174,-0.809174312,-0.80733945,-0.805504587,-0.803669725,-0.801834862,
-0.8,-0.798165138,-0.796330275,-0.794495413,-0.79266055,-0.790825688,-0.788990826,
-0.787155963,-0.785321101,-0.783486239,-0.781651376,-0.779816514,-0.777981651,
-0.776146789,-0.774311927,-0.772477064,-0.770642202,-0.768807339,-0.766972477,
-0.765137615,-0.763302752,-0.76146789,-0.759633028,-0.757798165,-0.755963303,
-0.75412844,-0.752293578,-0.750458716,-0.748623853,-0.746788991,-0.744954128,
-0.743119266,-0.741284404,-0.739449541,-0.737614679,-0.735779817,-0.733944954,
-0.732110092,-0.730275229,-0.728440367,-0.726605505,-0.724770642,-0.72293578,
-0.721100917,-0.719266055,-0.717431193,-0.71559633,-0.713761468,-0.711926606,
-0.710091743,-0.708256881,-0.706422018,-0.704587156,-0.702752294,-0.700917431,
-0.699082569,-0.697247706,-0.695412844,-0.693577982,-0.691743119,-0.689908257,
-0.688073394,-0.686238532,-0.68440367,-0.682568807,-0.680733945,-0.678899083,
-0.67706422,-0.675229358,-0.673394495,-0.671559633,-0.669724771,-0.667889908,
-0.666055046,-0.664220183,-0.662385321,-0.660550459,-0.658715596,-0.656880734,
-0.655045872,-0.653211009,-0.651376147,-0.649541284,-0.647706422,-0.64587156,
-0.644036697,-0.642201835,-0.640366972,-0.63853211,-0.636697248,-0.634862385,
-0.633027523,-0.631192661,-0.629357798,-0.627522936,-0.625688073,-0.623853211,
-0.622018349,-0.620183486,-0.618348624,-0.616513761,-0.614678899,-0.612844037,
-0.611009174,-0.609174312,-0.60733945,-0.605504587,-0.603669725,-0.601834862,
-0.6,-0.598165138,-0.596330275,-0.594495413,-0.59266055,-0.590825688,-0.588990826,
-0.587155963,-0.585321101,-0.583486239,-0.581651376,-0.579816514,-0.577981651,
-0.576146789,-0.574311927,-0.572477064,-0.570642202,-0.568807339,-0.566972477,
-0.565137615,-0.563302752,-0.56146789,-0.559633028,-0.557798165,-0.555963303,
-0.55412844,-0.552293578,-0.550458716,-0.548623853,-0.546788991,-0.544954128,
-0.543119266,-0.541284404,-0.539449541,-0.537614679,-0.535779817,-0.533944954,
-0.532110092,-0.530275229,-0.528440367,-0.526605505,-0.524770642,-0.52293578,
-0.521100917,-0.519266055,-0.517431193,-0.51559633,-0.513761468,-0.511926606,
-0.510091743,-0.508256881,-0.506422018,-0.504587156,-0.502752294,-0.500917431,
-0.499082569,-0.497247706,-0.495412844,-0.493577982,-0.491743119,-0.489908257,
-0.488073394,-0.486238532,-0.48440367,-0.482568807,-0.480733945,-0.478899083,
-0.47706422,-0.475229358,-0.473394495,-0.471559633,-0.469724771,-0.467889908,
-0.466055046,-0.464220183,-0.462385321,-0.460550459,-0.458715596,-0.456880734,
-0.455045872,-0.453211009,-0.451376147,-0.449541284,-0.447706422,-0.44587156,
-0.444036697,-0.442201835,-0.440366972,-0.43853211,-0.436697248,-0.434862385,
-0.433027523,-0.431192661,-0.429357798,-0.427522936,-0.425688073,-0.423853211,
-0.422018349,-0.420183486,-0.418348624,-0.416513761,-0.414678899,-0.412844037,
-0.411009174,-0.409174312,-0.40733945,-0.405504587,-0.403669725,-0.401834862,
-0.4,-0.398165138,-0.396330275,-0.394495413,-0.39266055,-0.390825688,-0.388990826,
-0.387155963,-0.385321101,-0.383486239,-0.381651376,-0.379816514,-0.377981651,
-0.376146789,-0.374311927,-0.372477064,-0.370642202,-0.368807339,-0.366972477,
-0.365137615,-0.363302752,-0.36146789,-0.359633028,-0.357798165,-0.355963303,
-0.35412844,-0.352293578,-0.350458716,-0.348623853,-0.346788991,-0.344954128,
-0.343119266,-0.341284404,-0.339449541,-0.337614679,-0.335779817,-0.333944954,
-0.332110092,-0.330275229,-0.328440367,-0.326605505,-0.324770642,-0.32293578,
-0.321100917,-0.319266055,-0.317431193,-0.31559633,-0.313761468,-0.311926606,
-0.310091743,-0.308256881,-0.306422018,-0.304587156,-0.302752294,-0.300917431,
-0.299082569,-0.297247706,-0.295412844,-0.293577982,-0.291743119,-0.289908257,
-0.288073394,-0.286238532,-0.28440367,-0.282568807,-0.280733945,-0.278899083,
-0.27706422,-0.275229358,-0.273394495,-0.271559633,-0.269724771,-0.267889908,
-0.266055046,-0.264220183,-0.262385321,-0.260550459,-0.258715596,-0.256880734,
-0.255045872,-0.253211009,-0.251376147,-0.249541284,-0.247706422,-0.24587156,
-0.244036697,-0.242201835,-0.240366972,-0.23853211,-0.236697248,-0.234862385,
-0.233027523,-0.231192661,-0.229357798,-0.227522936,-0.225688073,-0.223853211,
-0.222018349,-0.220183486,-0.218348624,-0.216513761,-0.214678899,-0.212844037,
-0.211009174,-0.209174312,-0.20733945,-0.205504587,-0.203669725,-0.201834862,
-0.2,-0.198165138,-0.196330275,-0.194495413,-0.19266055,-0.190825688,-0.188990826,
-0.187155963,-0.185321101,-0.183486239,-0.181651376,-0.179816514,-0.177981651,
-0.176146789,-0.174311927,-0.172477064,-0.170642202,-0.168807339,-0.166972477,
-0.165137615,-0.163302752,-0.16146789,-0.159633028,-0.157798165,-0.155963303,
-0.15412844,-0.152293578,-0.150458716,-0.148623853,-0.146788991,-0.144954128,
-0.143172103),(0.,0.36),.UNSPECIFIED.);
#6226=B_SPLINE_SURFACE_WITH_KNOTS('',5,1,((#172909,#172910),(#172911,#172912),
(#172913,#172914),(#172915,#172916),(#172917,#172918),(#172919,#172920),
(#172921,#172922),(#172923,#172924),(#172925,#172926),(#172927,#172928),
(#172929,#172930),(#172931,#172932),(#172933,#172934),(#172935,#172936),
(#172937,#172938),(#172939,#172940),(#172941,#172942),(#172943,#172944),
(#172945,#172946),(#172947,#172948),(#172949,#172950),(#172951,#172952),
(#172953,#172954),(#172955,#172956),(#172957,#172958),(#172959,#172960),
(#172961,#172962),(#172963,#172964),(#172965,#172966),(#172967,#172968),
(#172969,#172970),(#172971,#172972),(#172973,#172974),(#172975,#172976),
(#172977,#172978),(#172979,#172980),(#172981,#172982),(#172983,#172984),
(#172985,#172986),(#172987,#172988),(#172989,#172990),(#172991,#172992),
(#172993,#172994),(#172995,#172996),(#172997,#172998),(#172999,#173000),
(#173001,#173002),(#173003,#173004),(#173005,#173006),(#173007,#173008),
(#173009,#173010),(#173011,#173012),(#173013,#173014),(#173015,#173016),
(#173017,#173018),(#173019,#173020),(#173021,#173022),(#173023,#173024),
(#173025,#173026),(#173027,#173028),(#173029,#173030),(#173031,#173032),
(#173033,#173034),(#173035,#173036),(#173037,#173038),(#173039,#173040),
(#173041,#173042),(#173043,#173044),(#173045,#173046),(#173047,#173048),
(#173049,#173050),(#173051,#173052),(#173053,#173054),(#173055,#173056),
(#173057,#173058),(#173059,#173060),(#173061,#173062),(#173063,#173064),
(#173065,#173066),(#173067,#173068),(#173069,#173070),(#173071,#173072),
(#173073,#173074),(#173075,#173076),(#173077,#173078),(#173079,#173080),
(#173081,#173082),(#173083,#173084),(#173085,#173086),(#173087,#173088),
(#173089,#173090),(#173091,#173092),(#173093,#173094),(#173095,#173096),
(#173097,#173098),(#173099,#173100),(#173101,#173102),(#173103,#173104),
(#173105,#173106),(#173107,#173108),(#173109,#173110),(#173111,#173112),
(#173113,#173114),(#173115,#173116),(#173117,#173118),(#173119,#173120),
(#173121,#173122),(#173123,#173124),(#173125,#173126),(#173127,#173128),
(#173129,#173130),(#173131,#173132),(#173133,#173134),(#173135,#173136),
(#173137,#173138),(#173139,#173140),(#173141,#173142),(#173143,#173144),
(#173145,#173146),(#173147,#173148),(#173149,#173150),(#173151,#173152),
(#173153,#173154),(#173155,#173156),(#173157,#173158),(#173159,#173160),
(#173161,#173162),(#173163,#173164),(#173165,#173166),(#173167,#173168),
(#173169,#173170),(#173171,#173172),(#173173,#173174),(#173175,#173176),
(#173177,#173178),(#173179,#173180),(#173181,#173182),(#173183,#173184),
(#173185,#173186),(#173187,#173188),(#173189,#173190),(#173191,#173192),
(#173193,#173194),(#173195,#173196),(#173197,#173198),(#173199,#173200),
(#173201,#173202),(#173203,#173204),(#173205,#173206),(#173207,#173208),
(#173209,#173210),(#173211,#173212),(#173213,#173214),(#173215,#173216),
(#173217,#173218),(#173219,#173220),(#173221,#173222),(#173223,#173224),
(#173225,#173226),(#173227,#173228),(#173229,#173230),(#173231,#173232),
(#173233,#173234),(#173235,#173236),(#173237,#173238),(#173239,#173240),
(#173241,#173242),(#173243,#173244),(#173245,#173246),(#173247,#173248),
(#173249,#173250),(#173251,#173252),(#173253,#173254),(#173255,#173256),
(#173257,#173258),(#173259,#173260),(#173261,#173262),(#173263,#173264),
(#173265,#173266),(#173267,#173268),(#173269,#173270),(#173271,#173272),
(#173273,#173274),(#173275,#173276),(#173277,#173278),(#173279,#173280),
(#173281,#173282),(#173283,#173284),(#173285,#173286),(#173287,#173288),
(#173289,#173290),(#173291,#173292),(#173293,#173294),(#173295,#173296),
(#173297,#173298),(#173299,#173300),(#173301,#173302),(#173303,#173304),
(#173305,#173306),(#173307,#173308),(#173309,#173310),(#173311,#173312),
(#173313,#173314),(#173315,#173316),(#173317,#173318),(#173319,#173320),
(#173321,#173322),(#173323,#173324),(#173325,#173326),(#173327,#173328),
(#173329,#173330),(#173331,#173332),(#173333,#173334),(#173335,#173336),
(#173337,#173338),(#173339,#173340),(#173341,#173342),(#173343,#173344),
(#173345,#173346),(#173347,#173348),(#173349,#173350),(#173351,#173352),
(#173353,#173354),(#173355,#173356),(#173357,#173358),(#173359,#173360),
(#173361,#173362),(#173363,#173364),(#173365,#173366),(#173367,#173368),
(#173369,#173370),(#173371,#173372),(#173373,#173374),(#173375,#173376),
(#173377,#173378),(#173379,#173380),(#173381,#173382),(#173383,#173384),
(#173385,#173386),(#173387,#173388),(#173389,#173390),(#173391,#173392),
(#173393,#173394),(#173395,#173396),(#173397,#173398),(#173399,#173400),
(#173401,#173402),(#173403,#173404),(#173405,#173406),(#173407,#173408),
(#173409,#173410),(#173411,#173412),(#173413,#173414),(#173415,#173416),
(#173417,#173418),(#173419,#173420),(#173421,#173422),(#173423,#173424),
(#173425,#173426),(#173427,#173428),(#173429,#173430),(#173431,#173432),
(#173433,#173434),(#173435,#173436),(#173437,#173438),(#173439,#173440),
(#173441,#173442),(#173443,#173444),(#173445,#173446),(#173447,#173448),
(#173449,#173450),(#173451,#173452),(#173453,#173454),(#173455,#173456),
(#173457,#173458),(#173459,#173460),(#173461,#173462),(#173463,#173464),
(#173465,#173466),(#173467,#173468),(#173469,#173470),(#173471,#173472),
(#173473,#173474),(#173475,#173476),(#173477,#173478),(#173479,#173480),
(#173481,#173482),(#173483,#173484),(#173485,#173486),(#173487,#173488),
(#173489,#173490),(#173491,#173492),(#173493,#173494),(#173495,#173496),
(#173497,#173498),(#173499,#173500),(#173501,#173502),(#173503,#173504),
(#173505,#173506),(#173507,#173508),(#173509,#173510),(#173511,#173512),
(#173513,#173514),(#173515,#173516),(#173517,#173518),(#173519,#173520),
(#173521,#173522),(#173523,#173524),(#173525,#173526),(#173527,#173528),
(#173529,#173530),(#173531,#173532),(#173533,#173534),(#173535,#173536),
(#173537,#173538),(#173539,#173540),(#173541,#173542),(#173543,#173544),
(#173545,#173546),(#173547,#173548),(#173549,#173550),(#173551,#173552),
(#173553,#173554),(#173555,#173556),(#173557,#173558),(#173559,#173560),
(#173561,#173562),(#173563,#173564),(#173565,#173566),(#173567,#173568),
(#173569,#173570),(#173571,#173572),(#173573,#173574),(#173575,#173576),
(#173577,#173578),(#173579,#173580),(#173581,#173582),(#173583,#173584),
(#173585,#173586),(#173587,#173588),(#173589,#173590),(#173591,#173592),
(#173593,#173594),(#173595,#173596),(#173597,#173598),(#173599,#173600),
(#173601,#173602),(#173603,#173604),(#173605,#173606),(#173607,#173608),
(#173609,#173610),(#173611,#173612),(#173613,#173614),(#173615,#173616),
(#173617,#173618),(#173619,#173620),(#173621,#173622),(#173623,#173624),
(#173625,#173626),(#173627,#173628),(#173629,#173630),(#173631,#173632),
(#173633,#173634),(#173635,#173636),(#173637,#173638),(#173639,#173640),
(#173641,#173642),(#173643,#173644),(#173645,#173646),(#173647,#173648),
(#173649,#173650),(#173651,#173652),(#173653,#173654),(#173655,#173656),
(#173657,#173658),(#173659,#173660),(#173661,#173662),(#173663,#173664),
(#173665,#173666),(#173667,#173668),(#173669,#173670),(#173671,#173672),
(#173673,#173674),(#173675,#173676),(#173677,#173678),(#173679,#173680),
(#173681,#173682),(#173683,#173684),(#173685,#173686),(#173687,#173688),
(#173689,#173690),(#173691,#173692),(#173693,#173694),(#173695,#173696),
(#173697,#173698),(#173699,#173700),(#173701,#173702),(#173703,#173704),
(#173705,#173706),(#173707,#173708),(#173709,#173710),(#173711,#173712),
(#173713,#173714),(#173715,#173716),(#173717,#173718),(#173719,#173720),
(#173721,#173722),(#173723,#173724),(#173725,#173726),(#173727,#173728),
(#173729,#173730),(#173731,#173732),(#173733,#173734),(#173735,#173736),
(#173737,#173738),(#173739,#173740),(#173741,#173742),(#173743,#173744),
(#173745,#173746),(#173747,#173748),(#173749,#173750),(#173751,#173752),
(#173753,#173754),(#173755,#173756),(#173757,#173758),(#173759,#173760),
(#173761,#173762),(#173763,#173764),(#173765,#173766),(#173767,#173768),
(#173769,#173770),(#173771,#173772),(#173773,#173774),(#173775,#173776),
(#173777,#173778),(#173779,#173780),(#173781,#173782),(#173783,#173784),
(#173785,#173786),(#173787,#173788),(#173789,#173790),(#173791,#173792),
(#173793,#173794),(#173795,#173796),(#173797,#173798),(#173799,#173800),
(#173801,#173802),(#173803,#173804),(#173805,#173806),(#173807,#173808),
(#173809,#173810),(#173811,#173812),(#173813,#173814),(#173815,#173816),
(#173817,#173818),(#173819,#173820),(#173821,#173822),(#173823,#173824),
(#173825,#173826),(#173827,#173828),(#173829,#173830),(#173831,#173832),
(#173833,#173834),(#173835,#173836),(#173837,#173838),(#173839,#173840),
(#173841,#173842),(#173843,#173844),(#173845,#173846),(#173847,#173848),
(#173849,#173850),(#173851,#173852)),.UNSPECIFIED.,.F.,.F.,.F.,(6,1,1,1,
1,1,1,1,1,1,1,1,1,1,1,1,1,1,1,1,1,1,1,1,1,1,1,1,1,1,1,1,1,1,1,1,1,1,1,1,
1,1,1,1,1,1,1,1,1,1,1,1,1,1,1,1,1,1,1,1,1,1,1,1,1,1,1,1,1,1,1,1,1,1,1,1,
1,1,1,1,1,1,1,1,1,1,1,1,1,1,1,1,1,1,1,1,1,1,1,1,1,1,1,1,1,1,1,1,1,1,1,1,
1,1,1,1,1,1,1,1,1,1,1,1,1,1,1,1,1,1,1,1,1,1,1,1,1,1,1,1,1,1,1,1,1,1,1,1,
1,1,1,1,1,1,1,1,1,1,1,1,1,1,1,1,1,1,1,1,1,1,1,1,1,1,1,1,1,1,1,1,1,1,1,1,
1,1,1,1,1,1,1,1,1,1,1,1,1,1,1,1,1,1,1,1,1,1,1,1,1,1,1,1,1,1,1,1,1,1,1,1,
1,1,1,1,1,1,1,1,1,1,1,1,1,1,1,1,1,1,1,1,1,1,1,1,1,1,1,1,1,1,1,1,1,1,1,1,
1,1,1,1,1,1,1,1,1,1,1,1,1,1,1,1,1,1,1,1,1,1,1,1,1,1,1,1,1,1,1,1,1,1,1,1,
1,1,1,1,1,1,1,1,1,1,1,1,1,1,1,1,1,1,1,1,1,1,1,1,1,1,1,1,1,1,1,1,1,1,1,1,
1,1,1,1,1,1,1,1,1,1,1,1,1,1,1,1,1,1,1,1,1,1,1,1,1,1,1,1,1,1,1,1,1,1,1,1,
1,1,1,1,1,1,1,1,1,1,1,1,1,1,1,1,1,1,1,1,1,1,1,1,1,1,1,1,1,1,1,1,1,1,1,1,
1,1,1,1,1,1,1,1,1,1,1,1,1,1,1,1,1,1,1,1,1,1,1,1,1,1,1,1,1,1,1,1,1,1,1,1,
1,1,1,1,1,1,1,1,1,1,1,1,1,1,1,1,1,1,1,1,1,1,1,1,1,1,1,1,1,1,1,6),(2,2),
(0.143172103,0.144954128,0.146788991,0.148623853,0.150458716,0.152293578,
0.15412844,0.155963303,0.157798165,0.159633028,0.16146789,0.163302752,0.165137615,
0.166972477,0.168807339,0.170642202,0.172477064,0.174311927,0.176146789,
0.177981651,0.179816514,0.181651376,0.183486239,0.185321101,0.187155963,
0.188990826,0.190825688,0.19266055,0.194495413,0.196330275,0.198165138,
0.2,0.201834862,0.203669725,0.205504587,0.20733945,0.209174312,0.211009174,
0.212844037,0.214678899,0.216513761,0.218348624,0.220183486,0.222018349,
0.223853211,0.225688073,0.227522936,0.229357798,0.231192661,0.233027523,
0.234862385,0.236697248,0.23853211,0.240366972,0.242201835,0.244036697,
0.24587156,0.247706422,0.249541284,0.251376147,0.253211009,0.255045872,
0.256880734,0.258715596,0.260550459,0.262385321,0.264220183,0.266055046,
0.267889908,0.269724771,0.271559633,0.273394495,0.275229358,0.27706422,
0.278899083,0.280733945,0.282568807,0.28440367,0.286238532,0.288073394,
0.289908257,0.291743119,0.293577982,0.295412844,0.297247706,0.299082569,
0.300917431,0.302752294,0.304587156,0.306422018,0.308256881,0.310091743,
0.311926606,0.313761468,0.31559633,0.317431193,0.319266055,0.321100917,
0.32293578,0.324770642,0.326605505,0.328440367,0.330275229,0.332110092,
0.333944954,0.335779817,0.337614679,0.339449541,0.341284404,0.343119266,
0.344954128,0.346788991,0.348623853,0.350458716,0.352293578,0.35412844,
0.355963303,0.357798165,0.359633028,0.36146789,0.363302752,0.365137615,
0.366972477,0.368807339,0.370642202,0.372477064,0.374311927,0.376146789,
0.377981651,0.379816514,0.381651376,0.383486239,0.385321101,0.387155963,
0.388990826,0.390825688,0.39266055,0.394495413,0.396330275,0.398165138,
0.4,0.401834862,0.403669725,0.405504587,0.40733945,0.409174312,0.411009174,
0.412844037,0.414678899,0.416513761,0.418348624,0.420183486,0.422018349,
0.423853211,0.425688073,0.427522936,0.429357798,0.431192661,0.433027523,
0.434862385,0.436697248,0.43853211,0.440366972,0.442201835,0.444036697,
0.44587156,0.447706422,0.449541284,0.451376147,0.453211009,0.455045872,
0.456880734,0.458715596,0.460550459,0.462385321,0.464220183,0.466055046,
0.467889908,0.469724771,0.471559633,0.473394495,0.475229358,0.47706422,
0.478899083,0.480733945,0.482568807,0.48440367,0.486238532,0.488073394,
0.489908257,0.491743119,0.493577982,0.495412844,0.497247706,0.499082569,
0.500917431,0.502752294,0.504587156,0.506422018,0.508256881,0.510091743,
0.511926606,0.513761468,0.51559633,0.517431193,0.519266055,0.521100917,
0.52293578,0.524770642,0.526605505,0.528440367,0.530275229,0.532110092,
0.533944954,0.535779817,0.537614679,0.539449541,0.541284404,0.543119266,
0.544954128,0.546788991,0.548623853,0.550458716,0.552293578,0.55412844,
0.555963303,0.557798165,0.559633028,0.56146789,0.563302752,0.565137615,
0.566972477,0.568807339,0.570642202,0.572477064,0.574311927,0.576146789,
0.577981651,0.579816514,0.581651376,0.583486239,0.585321101,0.587155963,
0.588990826,0.590825688,0.59266055,0.594495413,0.596330275,0.598165138,
0.6,0.601834862,0.603669725,0.605504587,0.60733945,0.609174312,0.611009174,
0.612844037,0.614678899,0.616513761,0.618348624,0.620183486,0.622018349,
0.623853211,0.625688073,0.627522936,0.629357798,0.631192661,0.633027523,
0.634862385,0.636697248,0.63853211,0.640366972,0.642201835,0.644036697,
0.64587156,0.647706422,0.649541284,0.651376147,0.653211009,0.655045872,
0.656880734,0.658715596,0.660550459,0.662385321,0.664220183,0.666055046,
0.667889908,0.669724771,0.671559633,0.673394495,0.675229358,0.67706422,
0.678899083,0.680733945,0.682568807,0.68440367,0.686238532,0.688073394,
0.689908257,0.691743119,0.693577982,0.695412844,0.697247706,0.699082569,
0.700917431,0.702752294,0.704587156,0.706422018,0.708256881,0.710091743,
0.711926606,0.713761468,0.71559633,0.717431193,0.719266055,0.721100917,
0.72293578,0.724770642,0.726605505,0.728440367,0.730275229,0.732110092,
0.733944954,0.735779817,0.737614679,0.739449541,0.741284404,0.743119266,
0.744954128,0.746788991,0.748623853,0.750458716,0.752293578,0.75412844,
0.755963303,0.757798165,0.759633028,0.76146789,0.763302752,0.765137615,
0.766972477,0.768807339,0.770642202,0.772477064,0.774311927,0.776146789,
0.777981651,0.779816514,0.781651376,0.783486239,0.785321101,0.787155963,
0.788990826,0.790825688,0.79266055,0.794495413,0.796330275,0.798165138,
0.8,0.801834862,0.803669725,0.805504587,0.80733945,0.809174312,0.811009174,
0.812844037,0.814678899,0.816513761,0.818348624,0.820183486,0.822018349,
0.823853211,0.825688073,0.827522936,0.829357798,0.831192661,0.833027523,
0.834862385,0.836697248,0.83853211,0.840366972,0.842201835,0.844036697,
0.84587156,0.847706422,0.849541284,0.851376147,0.853211009,0.855045872,
0.856880734,0.858715596,0.860550459,0.862385321,0.864220183,0.866055046,
0.867889908,0.869724771,0.871559633,0.873394495,0.875229358,0.87706422,
0.878899083,0.880733945,0.882568807,0.88440367,0.886238532,0.888073394,
0.889908257,0.891743119,0.893577982,0.895412844,0.897247706,0.899082569,
0.900917431,0.902752294,0.904587156,0.906422018,0.908256881,0.910091743,
0.911926606,0.913761468,0.91559633,0.917431193,0.919266055,0.921100917,
0.92293578,0.924770642,0.926605505,0.928440367,0.930275229,0.932110092,
0.933944954,0.935779817,0.937614679,0.939449541,0.941284404,0.943119266,
0.944954128,0.946788991,0.948623853,0.950458716,0.952293578,0.95412844,
0.955963303,0.957798165,0.959633028,0.96146789,0.963302752,0.965137615,
0.966972477,0.968807339,0.970642202,0.972477064,0.974311927,0.976146789,
0.977981651,0.979816514,0.981651376,0.983486239,0.985321101,0.987155963,
0.988990826,0.990825688,0.99266055,0.994495413,0.996330275,0.998165138,
1.),(0.,0.36),.UNSPECIFIED.);
#6227=B_SPLINE_SURFACE_WITH_KNOTS('',5,1,((#174512,#174513),(#174514,#174515),
(#174516,#174517),(#174518,#174519),(#174520,#174521),(#174522,#174523),
(#174524,#174525),(#174526,#174527),(#174528,#174529),(#174530,#174531),
(#174532,#174533),(#174534,#174535),(#174536,#174537),(#174538,#174539),
(#174540,#174541),(#174542,#174543),(#174544,#174545),(#174546,#174547),
(#174548,#174549),(#174550,#174551),(#174552,#174553),(#174554,#174555),
(#174556,#174557),(#174558,#174559),(#174560,#174561),(#174562,#174563),
(#174564,#174565),(#174566,#174567),(#174568,#174569),(#174570,#174571),
(#174572,#174573),(#174574,#174575),(#174576,#174577),(#174578,#174579),
(#174580,#174581),(#174582,#174583),(#174584,#174585),(#174586,#174587),
(#174588,#174589),(#174590,#174591),(#174592,#174593),(#174594,#174595),
(#174596,#174597),(#174598,#174599),(#174600,#174601),(#174602,#174603),
(#174604,#174605),(#174606,#174607),(#174608,#174609),(#174610,#174611),
(#174612,#174613),(#174614,#174615),(#174616,#174617),(#174618,#174619),
(#174620,#174621),(#174622,#174623),(#174624,#174625),(#174626,#174627),
(#174628,#174629),(#174630,#174631),(#174632,#174633),(#174634,#174635),
(#174636,#174637),(#174638,#174639),(#174640,#174641),(#174642,#174643),
(#174644,#174645),(#174646,#174647),(#174648,#174649),(#174650,#174651),
(#174652,#174653),(#174654,#174655),(#174656,#174657),(#174658,#174659),
(#174660,#174661),(#174662,#174663),(#174664,#174665),(#174666,#174667),
(#174668,#174669),(#174670,#174671),(#174672,#174673),(#174674,#174675),
(#174676,#174677),(#174678,#174679),(#174680,#174681),(#174682,#174683),
(#174684,#174685),(#174686,#174687),(#174688,#174689),(#174690,#174691),
(#174692,#174693),(#174694,#174695),(#174696,#174697),(#174698,#174699),
(#174700,#174701),(#174702,#174703),(#174704,#174705),(#174706,#174707),
(#174708,#174709),(#174710,#174711),(#174712,#174713),(#174714,#174715),
(#174716,#174717),(#174718,#174719),(#174720,#174721),(#174722,#174723),
(#174724,#174725),(#174726,#174727),(#174728,#174729),(#174730,#174731),
(#174732,#174733),(#174734,#174735),(#174736,#174737),(#174738,#174739),
(#174740,#174741),(#174742,#174743),(#174744,#174745),(#174746,#174747),
(#174748,#174749),(#174750,#174751),(#174752,#174753),(#174754,#174755),
(#174756,#174757),(#174758,#174759),(#174760,#174761),(#174762,#174763),
(#174764,#174765),(#174766,#174767),(#174768,#174769),(#174770,#174771),
(#174772,#174773),(#174774,#174775),(#174776,#174777),(#174778,#174779),
(#174780,#174781),(#174782,#174783),(#174784,#174785),(#174786,#174787),
(#174788,#174789),(#174790,#174791),(#174792,#174793),(#174794,#174795),
(#174796,#174797),(#174798,#174799),(#174800,#174801),(#174802,#174803),
(#174804,#174805),(#174806,#174807),(#174808,#174809),(#174810,#174811),
(#174812,#174813),(#174814,#174815),(#174816,#174817),(#174818,#174819),
(#174820,#174821),(#174822,#174823),(#174824,#174825),(#174826,#174827),
(#174828,#174829),(#174830,#174831),(#174832,#174833),(#174834,#174835),
(#174836,#174837),(#174838,#174839),(#174840,#174841),(#174842,#174843),
(#174844,#174845),(#174846,#174847),(#174848,#174849),(#174850,#174851),
(#174852,#174853),(#174854,#174855),(#174856,#174857),(#174858,#174859),
(#174860,#174861),(#174862,#174863),(#174864,#174865),(#174866,#174867),
(#174868,#174869),(#174870,#174871),(#174872,#174873),(#174874,#174875),
(#174876,#174877),(#174878,#174879),(#174880,#174881),(#174882,#174883),
(#174884,#174885),(#174886,#174887),(#174888,#174889),(#174890,#174891),
(#174892,#174893),(#174894,#174895),(#174896,#174897),(#174898,#174899),
(#174900,#174901),(#174902,#174903),(#174904,#174905),(#174906,#174907),
(#174908,#174909),(#174910,#174911),(#174912,#174913),(#174914,#174915),
(#174916,#174917),(#174918,#174919),(#174920,#174921),(#174922,#174923),
(#174924,#174925),(#174926,#174927),(#174928,#174929),(#174930,#174931),
(#174932,#174933),(#174934,#174935),(#174936,#174937),(#174938,#174939),
(#174940,#174941),(#174942,#174943),(#174944,#174945),(#174946,#174947),
(#174948,#174949),(#174950,#174951),(#174952,#174953),(#174954,#174955),
(#174956,#174957),(#174958,#174959),(#174960,#174961),(#174962,#174963),
(#174964,#174965),(#174966,#174967),(#174968,#174969),(#174970,#174971),
(#174972,#174973),(#174974,#174975),(#174976,#174977),(#174978,#174979),
(#174980,#174981),(#174982,#174983),(#174984,#174985),(#174986,#174987),
(#174988,#174989),(#174990,#174991),(#174992,#174993),(#174994,#174995),
(#174996,#174997),(#174998,#174999),(#175000,#175001),(#175002,#175003),
(#175004,#175005),(#175006,#175007),(#175008,#175009),(#175010,#175011),
(#175012,#175013),(#175014,#175015),(#175016,#175017),(#175018,#175019),
(#175020,#175021),(#175022,#175023),(#175024,#175025),(#175026,#175027),
(#175028,#175029),(#175030,#175031),(#175032,#175033),(#175034,#175035),
(#175036,#175037),(#175038,#175039),(#175040,#175041),(#175042,#175043),
(#175044,#175045),(#175046,#175047),(#175048,#175049),(#175050,#175051),
(#175052,#175053),(#175054,#175055),(#175056,#175057),(#175058,#175059),
(#175060,#175061),(#175062,#175063),(#175064,#175065),(#175066,#175067),
(#175068,#175069),(#175070,#175071),(#175072,#175073),(#175074,#175075),
(#175076,#175077),(#175078,#175079),(#175080,#175081),(#175082,#175083),
(#175084,#175085),(#175086,#175087),(#175088,#175089),(#175090,#175091),
(#175092,#175093),(#175094,#175095),(#175096,#175097),(#175098,#175099),
(#175100,#175101),(#175102,#175103),(#175104,#175105),(#175106,#175107),
(#175108,#175109),(#175110,#175111),(#175112,#175113),(#175114,#175115),
(#175116,#175117),(#175118,#175119),(#175120,#175121),(#175122,#175123),
(#175124,#175125),(#175126,#175127),(#175128,#175129),(#175130,#175131),
(#175132,#175133),(#175134,#175135),(#175136,#175137),(#175138,#175139),
(#175140,#175141),(#175142,#175143),(#175144,#175145),(#175146,#175147),
(#175148,#175149),(#175150,#175151),(#175152,#175153),(#175154,#175155),
(#175156,#175157),(#175158,#175159),(#175160,#175161),(#175162,#175163),
(#175164,#175165),(#175166,#175167),(#175168,#175169),(#175170,#175171),
(#175172,#175173),(#175174,#175175),(#175176,#175177),(#175178,#175179),
(#175180,#175181),(#175182,#175183),(#175184,#175185),(#175186,#175187),
(#175188,#175189),(#175190,#175191),(#175192,#175193),(#175194,#175195),
(#175196,#175197),(#175198,#175199),(#175200,#175201),(#175202,#175203),
(#175204,#175205),(#175206,#175207),(#175208,#175209),(#175210,#175211),
(#175212,#175213),(#175214,#175215),(#175216,#175217),(#175218,#175219),
(#175220,#175221),(#175222,#175223),(#175224,#175225),(#175226,#175227),
(#175228,#175229),(#175230,#175231),(#175232,#175233),(#175234,#175235),
(#175236,#175237),(#175238,#175239),(#175240,#175241),(#175242,#175243),
(#175244,#175245),(#175246,#175247),(#175248,#175249),(#175250,#175251),
(#175252,#175253),(#175254,#175255),(#175256,#175257),(#175258,#175259),
(#175260,#175261),(#175262,#175263),(#175264,#175265),(#175266,#175267),
(#175268,#175269),(#175270,#175271),(#175272,#175273),(#175274,#175275),
(#175276,#175277),(#175278,#175279),(#175280,#175281),(#175282,#175283),
(#175284,#175285),(#175286,#175287),(#175288,#175289),(#175290,#175291),
(#175292,#175293),(#175294,#175295),(#175296,#175297),(#175298,#175299),
(#175300,#175301),(#175302,#175303),(#175304,#175305),(#175306,#175307),
(#175308,#175309),(#175310,#175311),(#175312,#175313),(#175314,#175315),
(#175316,#175317),(#175318,#175319),(#175320,#175321),(#175322,#175323),
(#175324,#175325),(#175326,#175327),(#175328,#175329),(#175330,#175331),
(#175332,#175333),(#175334,#175335),(#175336,#175337),(#175338,#175339),
(#175340,#175341),(#175342,#175343),(#175344,#175345),(#175346,#175347),
(#175348,#175349),(#175350,#175351),(#175352,#175353),(#175354,#175355),
(#175356,#175357),(#175358,#175359),(#175360,#175361),(#175362,#175363),
(#175364,#175365),(#175366,#175367),(#175368,#175369),(#175370,#175371),
(#175372,#175373),(#175374,#175375),(#175376,#175377),(#175378,#175379),
(#175380,#175381),(#175382,#175383),(#175384,#175385),(#175386,#175387),
(#175388,#175389),(#175390,#175391),(#175392,#175393),(#175394,#175395),
(#175396,#175397),(#175398,#175399),(#175400,#175401),(#175402,#175403),
(#175404,#175405),(#175406,#175407),(#175408,#175409),(#175410,#175411),
(#175412,#175413),(#175414,#175415),(#175416,#175417),(#175418,#175419),
(#175420,#175421),(#175422,#175423),(#175424,#175425),(#175426,#175427),
(#175428,#175429),(#175430,#175431),(#175432,#175433),(#175434,#175435),
(#175436,#175437),(#175438,#175439),(#175440,#175441),(#175442,#175443),
(#175444,#175445),(#175446,#175447),(#175448,#175449),(#175450,#175451),
(#175452,#175453),(#175454,#175455)),.UNSPECIFIED.,.F.,.F.,.F.,(6,1,1,1,
1,1,1,1,1,1,1,1,1,1,1,1,1,1,1,1,1,1,1,1,1,1,1,1,1,1,1,1,1,1,1,1,1,1,1,1,
1,1,1,1,1,1,1,1,1,1,1,1,1,1,1,1,1,1,1,1,1,1,1,1,1,1,1,1,1,1,1,1,1,1,1,1,
1,1,1,1,1,1,1,1,1,1,1,1,1,1,1,1,1,1,1,1,1,1,1,1,1,1,1,1,1,1,1,1,1,1,1,1,
1,1,1,1,1,1,1,1,1,1,1,1,1,1,1,1,1,1,1,1,1,1,1,1,1,1,1,1,1,1,1,1,1,1,1,1,
1,1,1,1,1,1,1,1,1,1,1,1,1,1,1,1,1,1,1,1,1,1,1,1,1,1,1,1,1,1,1,1,1,1,1,1,
1,1,1,1,1,1,1,1,1,1,1,1,1,1,1,1,1,1,1,1,1,1,1,1,1,1,1,1,1,1,1,1,1,1,1,1,
1,1,1,1,1,1,1,1,1,1,1,1,1,1,1,1,1,1,1,1,1,1,1,1,1,1,1,1,1,1,1,1,1,1,1,1,
1,1,1,1,1,1,1,1,1,1,1,1,1,1,1,1,1,1,1,1,1,1,1,1,1,1,1,1,1,1,1,1,1,1,1,1,
1,1,1,1,1,1,1,1,1,1,1,1,1,1,1,1,1,1,1,1,1,1,1,1,1,1,1,1,1,1,1,1,1,1,1,1,
1,1,1,1,1,1,1,1,1,1,1,1,1,1,1,1,1,1,1,1,1,1,1,1,1,1,1,1,1,1,1,1,1,1,1,1,
1,1,1,1,1,1,1,1,1,1,1,1,1,1,1,1,1,1,1,1,1,1,1,1,1,1,1,1,1,1,1,1,1,1,1,1,
1,1,1,1,1,1,1,1,1,1,1,1,1,1,1,1,1,1,1,1,1,1,1,1,1,1,1,1,1,1,1,1,1,1,1,1,
1,1,1,1,1,1,1,1,1,1,1,1,1,1,1,1,1,1,1,1,1,1,1,1,1,1,1,1,1,1,1,6),(2,2),
(0.143172103,0.144954128,0.146788991,0.148623853,0.150458716,0.152293578,
0.15412844,0.155963303,0.157798165,0.159633028,0.16146789,0.163302752,0.165137615,
0.166972477,0.168807339,0.170642202,0.172477064,0.174311927,0.176146789,
0.177981651,0.179816514,0.181651376,0.183486239,0.185321101,0.187155963,
0.188990826,0.190825688,0.19266055,0.194495413,0.196330275,0.198165138,
0.2,0.201834862,0.203669725,0.205504587,0.20733945,0.209174312,0.211009174,
0.212844037,0.214678899,0.216513761,0.218348624,0.220183486,0.222018349,
0.223853211,0.225688073,0.227522936,0.229357798,0.231192661,0.233027523,
0.234862385,0.236697248,0.23853211,0.240366972,0.242201835,0.244036697,
0.24587156,0.247706422,0.249541284,0.251376147,0.253211009,0.255045872,
0.256880734,0.258715596,0.260550459,0.262385321,0.264220183,0.266055046,
0.267889908,0.269724771,0.271559633,0.273394495,0.275229358,0.27706422,
0.278899083,0.280733945,0.282568807,0.28440367,0.286238532,0.288073394,
0.289908257,0.291743119,0.293577982,0.295412844,0.297247706,0.299082569,
0.300917431,0.302752294,0.304587156,0.306422018,0.308256881,0.310091743,
0.311926606,0.313761468,0.31559633,0.317431193,0.319266055,0.321100917,
0.32293578,0.324770642,0.326605505,0.328440367,0.330275229,0.332110092,
0.333944954,0.335779817,0.337614679,0.339449541,0.341284404,0.343119266,
0.344954128,0.346788991,0.348623853,0.350458716,0.352293578,0.35412844,
0.355963303,0.357798165,0.359633028,0.36146789,0.363302752,0.365137615,
0.366972477,0.368807339,0.370642202,0.372477064,0.374311927,0.376146789,
0.377981651,0.379816514,0.381651376,0.383486239,0.385321101,0.387155963,
0.388990826,0.390825688,0.39266055,0.394495413,0.396330275,0.398165138,
0.4,0.401834862,0.403669725,0.405504587,0.40733945,0.409174312,0.411009174,
0.412844037,0.414678899,0.416513761,0.418348624,0.420183486,0.422018349,
0.423853211,0.425688073,0.427522936,0.429357798,0.431192661,0.433027523,
0.434862385,0.436697248,0.43853211,0.440366972,0.442201835,0.444036697,
0.44587156,0.447706422,0.449541284,0.451376147,0.453211009,0.455045872,
0.456880734,0.458715596,0.460550459,0.462385321,0.464220183,0.466055046,
0.467889908,0.469724771,0.471559633,0.473394495,0.475229358,0.47706422,
0.478899083,0.480733945,0.482568807,0.48440367,0.486238532,0.488073394,
0.489908257,0.491743119,0.493577982,0.495412844,0.497247706,0.499082569,
0.500917431,0.502752294,0.504587156,0.506422018,0.508256881,0.510091743,
0.511926606,0.513761468,0.51559633,0.517431193,0.519266055,0.521100917,
0.52293578,0.524770642,0.526605505,0.528440367,0.530275229,0.532110092,
0.533944954,0.535779817,0.537614679,0.539449541,0.541284404,0.543119266,
0.544954128,0.546788991,0.548623853,0.550458716,0.552293578,0.55412844,
0.555963303,0.557798165,0.559633028,0.56146789,0.563302752,0.565137615,
0.566972477,0.568807339,0.570642202,0.572477064,0.574311927,0.576146789,
0.577981651,0.579816514,0.581651376,0.583486239,0.585321101,0.587155963,
0.588990826,0.590825688,0.59266055,0.594495413,0.596330275,0.598165138,
0.6,0.601834862,0.603669725,0.605504587,0.60733945,0.609174312,0.611009174,
0.612844037,0.614678899,0.616513761,0.618348624,0.620183486,0.622018349,
0.623853211,0.625688073,0.627522936,0.629357798,0.631192661,0.633027523,
0.634862385,0.636697248,0.63853211,0.640366972,0.642201835,0.644036697,
0.64587156,0.647706422,0.649541284,0.651376147,0.653211009,0.655045872,
0.656880734,0.658715596,0.660550459,0.662385321,0.664220183,0.666055046,
0.667889908,0.669724771,0.671559633,0.673394495,0.675229358,0.67706422,
0.678899083,0.680733945,0.682568807,0.68440367,0.686238532,0.688073394,
0.689908257,0.691743119,0.693577982,0.695412844,0.697247706,0.699082569,
0.700917431,0.702752294,0.704587156,0.706422018,0.708256881,0.710091743,
0.711926606,0.713761468,0.71559633,0.717431193,0.719266055,0.721100917,
0.72293578,0.724770642,0.726605505,0.728440367,0.730275229,0.732110092,
0.733944954,0.735779817,0.737614679,0.739449541,0.741284404,0.743119266,
0.744954128,0.746788991,0.748623853,0.750458716,0.752293578,0.75412844,
0.755963303,0.757798165,0.759633028,0.76146789,0.763302752,0.765137615,
0.766972477,0.768807339,0.770642202,0.772477064,0.774311927,0.776146789,
0.777981651,0.779816514,0.781651376,0.783486239,0.785321101,0.787155963,
0.788990826,0.790825688,0.79266055,0.794495413,0.796330275,0.798165138,
0.8,0.801834862,0.803669725,0.805504587,0.80733945,0.809174312,0.811009174,
0.812844037,0.814678899,0.816513761,0.818348624,0.820183486,0.822018349,
0.823853211,0.825688073,0.827522936,0.829357798,0.831192661,0.833027523,
0.834862385,0.836697248,0.83853211,0.840366972,0.842201835,0.844036697,
0.84587156,0.847706422,0.849541284,0.851376147,0.853211009,0.855045872,
0.856880734,0.858715596,0.860550459,0.862385321,0.864220183,0.866055046,
0.867889908,0.869724771,0.871559633,0.873394495,0.875229358,0.87706422,
0.878899083,0.880733945,0.882568807,0.88440367,0.886238532,0.888073394,
0.889908257,0.891743119,0.893577982,0.895412844,0.897247706,0.899082569,
0.900917431,0.902752294,0.904587156,0.906422018,0.908256881,0.910091743,
0.911926606,0.913761468,0.91559633,0.917431193,0.919266055,0.921100917,
0.92293578,0.924770642,0.926605505,0.928440367,0.930275229,0.932110092,
0.933944954,0.935779817,0.937614679,0.939449541,0.941284404,0.943119266,
0.944954128,0.946788991,0.948623853,0.950458716,0.952293578,0.95412844,
0.955963303,0.957798165,0.959633028,0.96146789,0.963302752,0.965137615,
0.966972477,0.968807339,0.970642202,0.972477064,0.974311927,0.976146789,
0.977981651,0.979816514,0.981651376,0.983486239,0.985321101,0.987155963,
0.988990826,0.990825688,0.99266055,0.994495413,0.996330275,0.998165138,
1.),(0.,0.36),.UNSPECIFIED.);
#6228=B_SPLINE_SURFACE_WITH_KNOTS('',5,1,((#176109,#176110),(#176111,#176112),
(#176113,#176114),(#176115,#176116),(#176117,#176118),(#176119,#176120),
(#176121,#176122),(#176123,#176124),(#176125,#176126),(#176127,#176128),
(#176129,#176130),(#176131,#176132),(#176133,#176134),(#176135,#176136),
(#176137,#176138),(#176139,#176140),(#176141,#176142),(#176143,#176144),
(#176145,#176146),(#176147,#176148),(#176149,#176150),(#176151,#176152),
(#176153,#176154),(#176155,#176156),(#176157,#176158),(#176159,#176160),
(#176161,#176162),(#176163,#176164),(#176165,#176166),(#176167,#176168),
(#176169,#176170),(#176171,#176172),(#176173,#176174),(#176175,#176176),
(#176177,#176178),(#176179,#176180),(#176181,#176182),(#176183,#176184),
(#176185,#176186),(#176187,#176188),(#176189,#176190),(#176191,#176192),
(#176193,#176194),(#176195,#176196),(#176197,#176198),(#176199,#176200),
(#176201,#176202),(#176203,#176204),(#176205,#176206),(#176207,#176208),
(#176209,#176210),(#176211,#176212),(#176213,#176214),(#176215,#176216),
(#176217,#176218),(#176219,#176220),(#176221,#176222),(#176223,#176224),
(#176225,#176226),(#176227,#176228),(#176229,#176230),(#176231,#176232),
(#176233,#176234),(#176235,#176236),(#176237,#176238),(#176239,#176240),
(#176241,#176242),(#176243,#176244),(#176245,#176246),(#176247,#176248),
(#176249,#176250),(#176251,#176252),(#176253,#176254),(#176255,#176256),
(#176257,#176258),(#176259,#176260),(#176261,#176262),(#176263,#176264),
(#176265,#176266),(#176267,#176268),(#176269,#176270),(#176271,#176272),
(#176273,#176274),(#176275,#176276),(#176277,#176278),(#176279,#176280),
(#176281,#176282),(#176283,#176284),(#176285,#176286),(#176287,#176288),
(#176289,#176290),(#176291,#176292),(#176293,#176294),(#176295,#176296),
(#176297,#176298),(#176299,#176300),(#176301,#176302),(#176303,#176304),
(#176305,#176306),(#176307,#176308),(#176309,#176310),(#176311,#176312),
(#176313,#176314),(#176315,#176316),(#176317,#176318),(#176319,#176320),
(#176321,#176322),(#176323,#176324),(#176325,#176326),(#176327,#176328),
(#176329,#176330),(#176331,#176332),(#176333,#176334),(#176335,#176336),
(#176337,#176338),(#176339,#176340),(#176341,#176342),(#176343,#176344),
(#176345,#176346),(#176347,#176348),(#176349,#176350),(#176351,#176352),
(#176353,#176354),(#176355,#176356),(#176357,#176358),(#176359,#176360),
(#176361,#176362),(#176363,#176364),(#176365,#176366),(#176367,#176368),
(#176369,#176370),(#176371,#176372),(#176373,#176374),(#176375,#176376),
(#176377,#176378),(#176379,#176380),(#176381,#176382),(#176383,#176384),
(#176385,#176386),(#176387,#176388),(#176389,#176390),(#176391,#176392),
(#176393,#176394),(#176395,#176396),(#176397,#176398),(#176399,#176400),
(#176401,#176402),(#176403,#176404),(#176405,#176406),(#176407,#176408),
(#176409,#176410),(#176411,#176412),(#176413,#176414),(#176415,#176416),
(#176417,#176418),(#176419,#176420),(#176421,#176422),(#176423,#176424),
(#176425,#176426),(#176427,#176428),(#176429,#176430),(#176431,#176432),
(#176433,#176434),(#176435,#176436),(#176437,#176438),(#176439,#176440),
(#176441,#176442),(#176443,#176444),(#176445,#176446),(#176447,#176448),
(#176449,#176450),(#176451,#176452),(#176453,#176454),(#176455,#176456),
(#176457,#176458),(#176459,#176460),(#176461,#176462),(#176463,#176464),
(#176465,#176466),(#176467,#176468),(#176469,#176470),(#176471,#176472),
(#176473,#176474),(#176475,#176476),(#176477,#176478),(#176479,#176480),
(#176481,#176482),(#176483,#176484),(#176485,#176486),(#176487,#176488),
(#176489,#176490),(#176491,#176492),(#176493,#176494),(#176495,#176496),
(#176497,#176498),(#176499,#176500),(#176501,#176502),(#176503,#176504),
(#176505,#176506),(#176507,#176508),(#176509,#176510),(#176511,#176512),
(#176513,#176514),(#176515,#176516),(#176517,#176518),(#176519,#176520),
(#176521,#176522),(#176523,#176524),(#176525,#176526),(#176527,#176528),
(#176529,#176530),(#176531,#176532),(#176533,#176534),(#176535,#176536),
(#176537,#176538),(#176539,#176540),(#176541,#176542),(#176543,#176544),
(#176545,#176546),(#176547,#176548),(#176549,#176550),(#176551,#176552),
(#176553,#176554),(#176555,#176556),(#176557,#176558),(#176559,#176560),
(#176561,#176562),(#176563,#176564),(#176565,#176566),(#176567,#176568),
(#176569,#176570),(#176571,#176572),(#176573,#176574),(#176575,#176576),
(#176577,#176578),(#176579,#176580),(#176581,#176582),(#176583,#176584),
(#176585,#176586),(#176587,#176588),(#176589,#176590),(#176591,#176592),
(#176593,#176594),(#176595,#176596),(#176597,#176598),(#176599,#176600),
(#176601,#176602),(#176603,#176604),(#176605,#176606),(#176607,#176608),
(#176609,#176610),(#176611,#176612),(#176613,#176614),(#176615,#176616),
(#176617,#176618),(#176619,#176620),(#176621,#176622),(#176623,#176624),
(#176625,#176626),(#176627,#176628),(#176629,#176630),(#176631,#176632),
(#176633,#176634),(#176635,#176636),(#176637,#176638),(#176639,#176640),
(#176641,#176642),(#176643,#176644),(#176645,#176646),(#176647,#176648),
(#176649,#176650),(#176651,#176652),(#176653,#176654),(#176655,#176656),
(#176657,#176658),(#176659,#176660),(#176661,#176662),(#176663,#176664),
(#176665,#176666),(#176667,#176668),(#176669,#176670),(#176671,#176672),
(#176673,#176674),(#176675,#176676),(#176677,#176678),(#176679,#176680),
(#176681,#176682),(#176683,#176684),(#176685,#176686),(#176687,#176688),
(#176689,#176690),(#176691,#176692),(#176693,#176694),(#176695,#176696),
(#176697,#176698),(#176699,#176700),(#176701,#176702),(#176703,#176704),
(#176705,#176706),(#176707,#176708),(#176709,#176710),(#176711,#176712),
(#176713,#176714),(#176715,#176716),(#176717,#176718),(#176719,#176720),
(#176721,#176722),(#176723,#176724),(#176725,#176726),(#176727,#176728),
(#176729,#176730),(#176731,#176732),(#176733,#176734),(#176735,#176736),
(#176737,#176738),(#176739,#176740),(#176741,#176742),(#176743,#176744),
(#176745,#176746),(#176747,#176748),(#176749,#176750),(#176751,#176752),
(#176753,#176754),(#176755,#176756),(#176757,#176758),(#176759,#176760),
(#176761,#176762),(#176763,#176764),(#176765,#176766),(#176767,#176768),
(#176769,#176770),(#176771,#176772),(#176773,#176774),(#176775,#176776),
(#176777,#176778),(#176779,#176780),(#176781,#176782),(#176783,#176784),
(#176785,#176786),(#176787,#176788),(#176789,#176790),(#176791,#176792),
(#176793,#176794),(#176795,#176796),(#176797,#176798),(#176799,#176800),
(#176801,#176802),(#176803,#176804),(#176805,#176806),(#176807,#176808),
(#176809,#176810),(#176811,#176812),(#176813,#176814),(#176815,#176816),
(#176817,#176818),(#176819,#176820),(#176821,#176822),(#176823,#176824),
(#176825,#176826),(#176827,#176828),(#176829,#176830),(#176831,#176832),
(#176833,#176834),(#176835,#176836),(#176837,#176838),(#176839,#176840),
(#176841,#176842),(#176843,#176844),(#176845,#176846),(#176847,#176848),
(#176849,#176850),(#176851,#176852),(#176853,#176854),(#176855,#176856),
(#176857,#176858),(#176859,#176860),(#176861,#176862),(#176863,#176864),
(#176865,#176866),(#176867,#176868),(#176869,#176870),(#176871,#176872),
(#176873,#176874),(#176875,#176876),(#176877,#176878),(#176879,#176880),
(#176881,#176882),(#176883,#176884),(#176885,#176886),(#176887,#176888),
(#176889,#176890),(#176891,#176892),(#176893,#176894),(#176895,#176896),
(#176897,#176898),(#176899,#176900),(#176901,#176902),(#176903,#176904),
(#176905,#176906),(#176907,#176908),(#176909,#176910),(#176911,#176912),
(#176913,#176914),(#176915,#176916),(#176917,#176918),(#176919,#176920),
(#176921,#176922),(#176923,#176924),(#176925,#176926),(#176927,#176928),
(#176929,#176930),(#176931,#176932),(#176933,#176934),(#176935,#176936),
(#176937,#176938),(#176939,#176940),(#176941,#176942),(#176943,#176944),
(#176945,#176946),(#176947,#176948),(#176949,#176950),(#176951,#176952),
(#176953,#176954),(#176955,#176956),(#176957,#176958),(#176959,#176960),
(#176961,#176962),(#176963,#176964),(#176965,#176966),(#176967,#176968),
(#176969,#176970),(#176971,#176972),(#176973,#176974),(#176975,#176976),
(#176977,#176978),(#176979,#176980),(#176981,#176982),(#176983,#176984),
(#176985,#176986),(#176987,#176988),(#176989,#176990),(#176991,#176992),
(#176993,#176994),(#176995,#176996),(#176997,#176998),(#176999,#177000),
(#177001,#177002),(#177003,#177004),(#177005,#177006),(#177007,#177008),
(#177009,#177010),(#177011,#177012),(#177013,#177014),(#177015,#177016),
(#177017,#177018),(#177019,#177020),(#177021,#177022),(#177023,#177024),
(#177025,#177026),(#177027,#177028),(#177029,#177030),(#177031,#177032),
(#177033,#177034),(#177035,#177036),(#177037,#177038),(#177039,#177040),
(#177041,#177042),(#177043,#177044),(#177045,#177046),(#177047,#177048),
(#177049,#177050),(#177051,#177052)),.UNSPECIFIED.,.F.,.F.,.F.,(6,1,1,1,
1,1,1,1,1,1,1,1,1,1,1,1,1,1,1,1,1,1,1,1,1,1,1,1,1,1,1,1,1,1,1,1,1,1,1,1,
1,1,1,1,1,1,1,1,1,1,1,1,1,1,1,1,1,1,1,1,1,1,1,1,1,1,1,1,1,1,1,1,1,1,1,1,
1,1,1,1,1,1,1,1,1,1,1,1,1,1,1,1,1,1,1,1,1,1,1,1,1,1,1,1,1,1,1,1,1,1,1,1,
1,1,1,1,1,1,1,1,1,1,1,1,1,1,1,1,1,1,1,1,1,1,1,1,1,1,1,1,1,1,1,1,1,1,1,1,
1,1,1,1,1,1,1,1,1,1,1,1,1,1,1,1,1,1,1,1,1,1,1,1,1,1,1,1,1,1,1,1,1,1,1,1,
1,1,1,1,1,1,1,1,1,1,1,1,1,1,1,1,1,1,1,1,1,1,1,1,1,1,1,1,1,1,1,1,1,1,1,1,
1,1,1,1,1,1,1,1,1,1,1,1,1,1,1,1,1,1,1,1,1,1,1,1,1,1,1,1,1,1,1,1,1,1,1,1,
1,1,1,1,1,1,1,1,1,1,1,1,1,1,1,1,1,1,1,1,1,1,1,1,1,1,1,1,1,1,1,1,1,1,1,1,
1,1,1,1,1,1,1,1,1,1,1,1,1,1,1,1,1,1,1,1,1,1,1,1,1,1,1,1,1,1,1,1,1,1,1,1,
1,1,1,1,1,1,1,1,1,1,1,1,1,1,1,1,1,1,1,1,1,1,1,1,1,1,1,1,1,1,1,1,1,1,1,1,
1,1,1,1,1,1,1,1,1,1,1,1,1,1,1,1,1,1,1,1,1,1,1,1,1,1,1,1,1,1,1,1,1,1,1,1,
1,1,1,1,1,1,1,1,1,1,1,1,1,1,1,1,1,1,1,1,1,1,1,1,1,1,1,1,1,1,1,1,1,1,1,1,
1,1,1,1,1,1,1,1,1,1,1,1,1,1,1,1,1,1,1,1,1,1,1,1,1,1,1,1,1,1,1,6),(2,2),
(-1.,-0.998165138,-0.996330275,-0.994495413,-0.99266055,-0.990825688,-0.988990826,
-0.987155963,-0.985321101,-0.983486239,-0.981651376,-0.979816514,-0.977981651,
-0.976146789,-0.974311927,-0.972477064,-0.970642202,-0.968807339,-0.966972477,
-0.965137615,-0.963302752,-0.96146789,-0.959633028,-0.957798165,-0.955963303,
-0.95412844,-0.952293578,-0.950458716,-0.948623853,-0.946788991,-0.944954128,
-0.943119266,-0.941284404,-0.939449541,-0.937614679,-0.935779817,-0.933944954,
-0.932110092,-0.930275229,-0.928440367,-0.926605505,-0.924770642,-0.92293578,
-0.921100917,-0.919266055,-0.917431193,-0.91559633,-0.913761468,-0.911926606,
-0.910091743,-0.908256881,-0.906422018,-0.904587156,-0.902752294,-0.900917431,
-0.899082569,-0.897247706,-0.895412844,-0.893577982,-0.891743119,-0.889908257,
-0.888073394,-0.886238532,-0.88440367,-0.882568807,-0.880733945,-0.878899083,
-0.87706422,-0.875229358,-0.873394495,-0.871559633,-0.869724771,-0.867889908,
-0.866055046,-0.864220183,-0.862385321,-0.860550459,-0.858715596,-0.856880734,
-0.855045872,-0.853211009,-0.851376147,-0.849541284,-0.847706422,-0.84587156,
-0.844036697,-0.842201835,-0.840366972,-0.83853211,-0.836697248,-0.834862385,
-0.833027523,-0.831192661,-0.829357798,-0.827522936,-0.825688073,-0.823853211,
-0.822018349,-0.820183486,-0.818348624,-0.816513761,-0.814678899,-0.812844037,
-0.811009174,-0.809174312,-0.80733945,-0.805504587,-0.803669725,-0.801834862,
-0.8,-0.798165138,-0.796330275,-0.794495413,-0.79266055,-0.790825688,-0.788990826,
-0.787155963,-0.785321101,-0.783486239,-0.781651376,-0.779816514,-0.777981651,
-0.776146789,-0.774311927,-0.772477064,-0.770642202,-0.768807339,-0.766972477,
-0.765137615,-0.763302752,-0.76146789,-0.759633028,-0.757798165,-0.755963303,
-0.75412844,-0.752293578,-0.750458716,-0.748623853,-0.746788991,-0.744954128,
-0.743119266,-0.741284404,-0.739449541,-0.737614679,-0.735779817,-0.733944954,
-0.732110092,-0.730275229,-0.728440367,-0.726605505,-0.724770642,-0.72293578,
-0.721100917,-0.719266055,-0.717431193,-0.71559633,-0.713761468,-0.711926606,
-0.710091743,-0.708256881,-0.706422018,-0.704587156,-0.702752294,-0.700917431,
-0.699082569,-0.697247706,-0.695412844,-0.693577982,-0.691743119,-0.689908257,
-0.688073394,-0.686238532,-0.68440367,-0.682568807,-0.680733945,-0.678899083,
-0.67706422,-0.675229358,-0.673394495,-0.671559633,-0.669724771,-0.667889908,
-0.666055046,-0.664220183,-0.662385321,-0.660550459,-0.658715596,-0.656880734,
-0.655045872,-0.653211009,-0.651376147,-0.649541284,-0.647706422,-0.64587156,
-0.644036697,-0.642201835,-0.640366972,-0.63853211,-0.636697248,-0.634862385,
-0.633027523,-0.631192661,-0.629357798,-0.627522936,-0.625688073,-0.623853211,
-0.622018349,-0.620183486,-0.618348624,-0.616513761,-0.614678899,-0.612844037,
-0.611009174,-0.609174312,-0.60733945,-0.605504587,-0.603669725,-0.601834862,
-0.6,-0.598165138,-0.596330275,-0.594495413,-0.59266055,-0.590825688,-0.588990826,
-0.587155963,-0.585321101,-0.583486239,-0.581651376,-0.579816514,-0.577981651,
-0.576146789,-0.574311927,-0.572477064,-0.570642202,-0.568807339,-0.566972477,
-0.565137615,-0.563302752,-0.56146789,-0.559633028,-0.557798165,-0.555963303,
-0.55412844,-0.552293578,-0.550458716,-0.548623853,-0.546788991,-0.544954128,
-0.543119266,-0.541284404,-0.539449541,-0.537614679,-0.535779817,-0.533944954,
-0.532110092,-0.530275229,-0.528440367,-0.526605505,-0.524770642,-0.52293578,
-0.521100917,-0.519266055,-0.517431193,-0.51559633,-0.513761468,-0.511926606,
-0.510091743,-0.508256881,-0.506422018,-0.504587156,-0.502752294,-0.500917431,
-0.499082569,-0.497247706,-0.495412844,-0.493577982,-0.491743119,-0.489908257,
-0.488073394,-0.486238532,-0.48440367,-0.482568807,-0.480733945,-0.478899083,
-0.47706422,-0.475229358,-0.473394495,-0.471559633,-0.469724771,-0.467889908,
-0.466055046,-0.464220183,-0.462385321,-0.460550459,-0.458715596,-0.456880734,
-0.455045872,-0.453211009,-0.451376147,-0.449541284,-0.447706422,-0.44587156,
-0.444036697,-0.442201835,-0.440366972,-0.43853211,-0.436697248,-0.434862385,
-0.433027523,-0.431192661,-0.429357798,-0.427522936,-0.425688073,-0.423853211,
-0.422018349,-0.420183486,-0.418348624,-0.416513761,-0.414678899,-0.412844037,
-0.411009174,-0.409174312,-0.40733945,-0.405504587,-0.403669725,-0.401834862,
-0.4,-0.398165138,-0.396330275,-0.394495413,-0.39266055,-0.390825688,-0.388990826,
-0.387155963,-0.385321101,-0.383486239,-0.381651376,-0.379816514,-0.377981651,
-0.376146789,-0.374311927,-0.372477064,-0.370642202,-0.368807339,-0.366972477,
-0.365137615,-0.363302752,-0.36146789,-0.359633028,-0.357798165,-0.355963303,
-0.35412844,-0.352293578,-0.350458716,-0.348623853,-0.346788991,-0.344954128,
-0.343119266,-0.341284404,-0.339449541,-0.337614679,-0.335779817,-0.333944954,
-0.332110092,-0.330275229,-0.328440367,-0.326605505,-0.324770642,-0.32293578,
-0.321100917,-0.319266055,-0.317431193,-0.31559633,-0.313761468,-0.311926606,
-0.310091743,-0.308256881,-0.306422018,-0.304587156,-0.302752294,-0.300917431,
-0.299082569,-0.297247706,-0.295412844,-0.293577982,-0.291743119,-0.289908257,
-0.288073394,-0.286238532,-0.28440367,-0.282568807,-0.280733945,-0.278899083,
-0.27706422,-0.275229358,-0.273394495,-0.271559633,-0.269724771,-0.267889908,
-0.266055046,-0.264220183,-0.262385321,-0.260550459,-0.258715596,-0.256880734,
-0.255045872,-0.253211009,-0.251376147,-0.249541284,-0.247706422,-0.24587156,
-0.244036697,-0.242201835,-0.240366972,-0.23853211,-0.236697248,-0.234862385,
-0.233027523,-0.231192661,-0.229357798,-0.227522936,-0.225688073,-0.223853211,
-0.222018349,-0.220183486,-0.218348624,-0.216513761,-0.214678899,-0.212844037,
-0.211009174,-0.209174312,-0.20733945,-0.205504587,-0.203669725,-0.201834862,
-0.2,-0.198165138,-0.196330275,-0.194495413,-0.19266055,-0.190825688,-0.188990826,
-0.187155963,-0.185321101,-0.183486239,-0.181651376,-0.179816514,-0.177981651,
-0.176146789,-0.174311927,-0.172477064,-0.170642202,-0.168807339,-0.166972477,
-0.165137615,-0.163302752,-0.16146789,-0.159633028,-0.157798165,-0.155963303,
-0.15412844,-0.152293578,-0.150458716,-0.148623853,-0.146788991,-0.144954128,
-0.143172103),(0.,0.36),.UNSPECIFIED.);
#6229=B_SPLINE_SURFACE_WITH_KNOTS('',5,1,((#177721,#177722),(#177723,#177724),
(#177725,#177726),(#177727,#177728),(#177729,#177730),(#177731,#177732),
(#177733,#177734),(#177735,#177736),(#177737,#177738),(#177739,#177740),
(#177741,#177742),(#177743,#177744),(#177745,#177746),(#177747,#177748),
(#177749,#177750),(#177751,#177752),(#177753,#177754),(#177755,#177756),
(#177757,#177758),(#177759,#177760),(#177761,#177762),(#177763,#177764),
(#177765,#177766),(#177767,#177768),(#177769,#177770),(#177771,#177772),
(#177773,#177774),(#177775,#177776),(#177777,#177778),(#177779,#177780),
(#177781,#177782),(#177783,#177784),(#177785,#177786),(#177787,#177788),
(#177789,#177790),(#177791,#177792),(#177793,#177794),(#177795,#177796),
(#177797,#177798),(#177799,#177800),(#177801,#177802),(#177803,#177804),
(#177805,#177806),(#177807,#177808),(#177809,#177810),(#177811,#177812),
(#177813,#177814),(#177815,#177816),(#177817,#177818),(#177819,#177820),
(#177821,#177822),(#177823,#177824),(#177825,#177826),(#177827,#177828),
(#177829,#177830),(#177831,#177832),(#177833,#177834),(#177835,#177836),
(#177837,#177838),(#177839,#177840),(#177841,#177842),(#177843,#177844),
(#177845,#177846),(#177847,#177848),(#177849,#177850),(#177851,#177852),
(#177853,#177854),(#177855,#177856),(#177857,#177858),(#177859,#177860),
(#177861,#177862),(#177863,#177864),(#177865,#177866),(#177867,#177868),
(#177869,#177870),(#177871,#177872),(#177873,#177874),(#177875,#177876),
(#177877,#177878),(#177879,#177880),(#177881,#177882),(#177883,#177884),
(#177885,#177886),(#177887,#177888),(#177889,#177890),(#177891,#177892),
(#177893,#177894),(#177895,#177896),(#177897,#177898),(#177899,#177900),
(#177901,#177902),(#177903,#177904),(#177905,#177906),(#177907,#177908),
(#177909,#177910),(#177911,#177912),(#177913,#177914),(#177915,#177916),
(#177917,#177918),(#177919,#177920),(#177921,#177922),(#177923,#177924),
(#177925,#177926),(#177927,#177928),(#177929,#177930),(#177931,#177932),
(#177933,#177934),(#177935,#177936),(#177937,#177938),(#177939,#177940),
(#177941,#177942),(#177943,#177944),(#177945,#177946),(#177947,#177948),
(#177949,#177950),(#177951,#177952),(#177953,#177954),(#177955,#177956),
(#177957,#177958),(#177959,#177960),(#177961,#177962),(#177963,#177964),
(#177965,#177966),(#177967,#177968),(#177969,#177970),(#177971,#177972),
(#177973,#177974),(#177975,#177976),(#177977,#177978),(#177979,#177980),
(#177981,#177982),(#177983,#177984),(#177985,#177986),(#177987,#177988),
(#177989,#177990),(#177991,#177992),(#177993,#177994),(#177995,#177996),
(#177997,#177998),(#177999,#178000),(#178001,#178002),(#178003,#178004),
(#178005,#178006),(#178007,#178008),(#178009,#178010),(#178011,#178012),
(#178013,#178014),(#178015,#178016),(#178017,#178018),(#178019,#178020),
(#178021,#178022),(#178023,#178024),(#178025,#178026),(#178027,#178028),
(#178029,#178030),(#178031,#178032),(#178033,#178034),(#178035,#178036),
(#178037,#178038),(#178039,#178040),(#178041,#178042),(#178043,#178044),
(#178045,#178046),(#178047,#178048),(#178049,#178050),(#178051,#178052),
(#178053,#178054),(#178055,#178056),(#178057,#178058),(#178059,#178060),
(#178061,#178062),(#178063,#178064),(#178065,#178066),(#178067,#178068),
(#178069,#178070),(#178071,#178072),(#178073,#178074),(#178075,#178076),
(#178077,#178078),(#178079,#178080),(#178081,#178082),(#178083,#178084),
(#178085,#178086),(#178087,#178088),(#178089,#178090),(#178091,#178092),
(#178093,#178094),(#178095,#178096),(#178097,#178098),(#178099,#178100),
(#178101,#178102),(#178103,#178104),(#178105,#178106),(#178107,#178108),
(#178109,#178110),(#178111,#178112),(#178113,#178114),(#178115,#178116),
(#178117,#178118),(#178119,#178120),(#178121,#178122),(#178123,#178124),
(#178125,#178126),(#178127,#178128),(#178129,#178130),(#178131,#178132),
(#178133,#178134),(#178135,#178136),(#178137,#178138),(#178139,#178140),
(#178141,#178142),(#178143,#178144),(#178145,#178146),(#178147,#178148),
(#178149,#178150),(#178151,#178152),(#178153,#178154),(#178155,#178156),
(#178157,#178158),(#178159,#178160),(#178161,#178162),(#178163,#178164),
(#178165,#178166),(#178167,#178168),(#178169,#178170),(#178171,#178172),
(#178173,#178174),(#178175,#178176),(#178177,#178178),(#178179,#178180),
(#178181,#178182),(#178183,#178184),(#178185,#178186),(#178187,#178188),
(#178189,#178190),(#178191,#178192),(#178193,#178194),(#178195,#178196),
(#178197,#178198),(#178199,#178200),(#178201,#178202),(#178203,#178204),
(#178205,#178206),(#178207,#178208),(#178209,#178210),(#178211,#178212),
(#178213,#178214),(#178215,#178216),(#178217,#178218),(#178219,#178220),
(#178221,#178222),(#178223,#178224),(#178225,#178226),(#178227,#178228),
(#178229,#178230),(#178231,#178232),(#178233,#178234),(#178235,#178236),
(#178237,#178238),(#178239,#178240),(#178241,#178242),(#178243,#178244),
(#178245,#178246),(#178247,#178248),(#178249,#178250),(#178251,#178252),
(#178253,#178254),(#178255,#178256),(#178257,#178258),(#178259,#178260),
(#178261,#178262),(#178263,#178264),(#178265,#178266),(#178267,#178268),
(#178269,#178270),(#178271,#178272),(#178273,#178274),(#178275,#178276),
(#178277,#178278),(#178279,#178280),(#178281,#178282),(#178283,#178284),
(#178285,#178286),(#178287,#178288),(#178289,#178290),(#178291,#178292),
(#178293,#178294),(#178295,#178296),(#178297,#178298),(#178299,#178300),
(#178301,#178302),(#178303,#178304),(#178305,#178306),(#178307,#178308),
(#178309,#178310),(#178311,#178312),(#178313,#178314),(#178315,#178316),
(#178317,#178318),(#178319,#178320),(#178321,#178322),(#178323,#178324),
(#178325,#178326),(#178327,#178328),(#178329,#178330),(#178331,#178332),
(#178333,#178334),(#178335,#178336),(#178337,#178338),(#178339,#178340),
(#178341,#178342),(#178343,#178344),(#178345,#178346),(#178347,#178348),
(#178349,#178350),(#178351,#178352),(#178353,#178354),(#178355,#178356),
(#178357,#178358),(#178359,#178360),(#178361,#178362),(#178363,#178364),
(#178365,#178366),(#178367,#178368),(#178369,#178370),(#178371,#178372),
(#178373,#178374),(#178375,#178376),(#178377,#178378),(#178379,#178380),
(#178381,#178382),(#178383,#178384),(#178385,#178386),(#178387,#178388),
(#178389,#178390),(#178391,#178392),(#178393,#178394),(#178395,#178396),
(#178397,#178398),(#178399,#178400),(#178401,#178402),(#178403,#178404),
(#178405,#178406),(#178407,#178408),(#178409,#178410),(#178411,#178412),
(#178413,#178414),(#178415,#178416),(#178417,#178418),(#178419,#178420),
(#178421,#178422),(#178423,#178424),(#178425,#178426),(#178427,#178428),
(#178429,#178430),(#178431,#178432),(#178433,#178434),(#178435,#178436),
(#178437,#178438),(#178439,#178440),(#178441,#178442),(#178443,#178444),
(#178445,#178446),(#178447,#178448),(#178449,#178450),(#178451,#178452),
(#178453,#178454),(#178455,#178456),(#178457,#178458),(#178459,#178460),
(#178461,#178462),(#178463,#178464),(#178465,#178466),(#178467,#178468),
(#178469,#178470),(#178471,#178472),(#178473,#178474),(#178475,#178476),
(#178477,#178478),(#178479,#178480),(#178481,#178482),(#178483,#178484),
(#178485,#178486),(#178487,#178488),(#178489,#178490),(#178491,#178492),
(#178493,#178494),(#178495,#178496),(#178497,#178498),(#178499,#178500),
(#178501,#178502),(#178503,#178504),(#178505,#178506),(#178507,#178508),
(#178509,#178510),(#178511,#178512),(#178513,#178514),(#178515,#178516),
(#178517,#178518),(#178519,#178520),(#178521,#178522),(#178523,#178524),
(#178525,#178526),(#178527,#178528),(#178529,#178530),(#178531,#178532),
(#178533,#178534),(#178535,#178536),(#178537,#178538),(#178539,#178540),
(#178541,#178542),(#178543,#178544),(#178545,#178546),(#178547,#178548),
(#178549,#178550),(#178551,#178552),(#178553,#178554),(#178555,#178556),
(#178557,#178558),(#178559,#178560),(#178561,#178562),(#178563,#178564),
(#178565,#178566),(#178567,#178568),(#178569,#178570),(#178571,#178572),
(#178573,#178574),(#178575,#178576),(#178577,#178578),(#178579,#178580),
(#178581,#178582),(#178583,#178584),(#178585,#178586),(#178587,#178588),
(#178589,#178590),(#178591,#178592),(#178593,#178594),(#178595,#178596),
(#178597,#178598),(#178599,#178600),(#178601,#178602),(#178603,#178604),
(#178605,#178606),(#178607,#178608),(#178609,#178610),(#178611,#178612),
(#178613,#178614),(#178615,#178616),(#178617,#178618),(#178619,#178620),
(#178621,#178622),(#178623,#178624),(#178625,#178626),(#178627,#178628),
(#178629,#178630),(#178631,#178632),(#178633,#178634),(#178635,#178636),
(#178637,#178638),(#178639,#178640),(#178641,#178642),(#178643,#178644),
(#178645,#178646),(#178647,#178648),(#178649,#178650),(#178651,#178652),
(#178653,#178654),(#178655,#178656),(#178657,#178658),(#178659,#178660),
(#178661,#178662),(#178663,#178664)),.UNSPECIFIED.,.F.,.F.,.F.,(6,1,1,1,
1,1,1,1,1,1,1,1,1,1,1,1,1,1,1,1,1,1,1,1,1,1,1,1,1,1,1,1,1,1,1,1,1,1,1,1,
1,1,1,1,1,1,1,1,1,1,1,1,1,1,1,1,1,1,1,1,1,1,1,1,1,1,1,1,1,1,1,1,1,1,1,1,
1,1,1,1,1,1,1,1,1,1,1,1,1,1,1,1,1,1,1,1,1,1,1,1,1,1,1,1,1,1,1,1,1,1,1,1,
1,1,1,1,1,1,1,1,1,1,1,1,1,1,1,1,1,1,1,1,1,1,1,1,1,1,1,1,1,1,1,1,1,1,1,1,
1,1,1,1,1,1,1,1,1,1,1,1,1,1,1,1,1,1,1,1,1,1,1,1,1,1,1,1,1,1,1,1,1,1,1,1,
1,1,1,1,1,1,1,1,1,1,1,1,1,1,1,1,1,1,1,1,1,1,1,1,1,1,1,1,1,1,1,1,1,1,1,1,
1,1,1,1,1,1,1,1,1,1,1,1,1,1,1,1,1,1,1,1,1,1,1,1,1,1,1,1,1,1,1,1,1,1,1,1,
1,1,1,1,1,1,1,1,1,1,1,1,1,1,1,1,1,1,1,1,1,1,1,1,1,1,1,1,1,1,1,1,1,1,1,1,
1,1,1,1,1,1,1,1,1,1,1,1,1,1,1,1,1,1,1,1,1,1,1,1,1,1,1,1,1,1,1,1,1,1,1,1,
1,1,1,1,1,1,1,1,1,1,1,1,1,1,1,1,1,1,1,1,1,1,1,1,1,1,1,1,1,1,1,1,1,1,1,1,
1,1,1,1,1,1,1,1,1,1,1,1,1,1,1,1,1,1,1,1,1,1,1,1,1,1,1,1,1,1,1,1,1,1,1,1,
1,1,1,1,1,1,1,1,1,1,1,1,1,1,1,1,1,1,1,1,1,1,1,1,1,1,1,1,1,1,1,1,1,1,1,1,
1,1,1,1,1,1,1,1,1,1,1,1,1,1,1,1,1,1,1,1,1,1,1,1,1,1,1,1,1,1,1,6),(2,2),
(-1.,-0.998165138,-0.996330275,-0.994495413,-0.99266055,-0.990825688,-0.988990826,
-0.987155963,-0.985321101,-0.983486239,-0.981651376,-0.979816514,-0.977981651,
-0.976146789,-0.974311927,-0.972477064,-0.970642202,-0.968807339,-0.966972477,
-0.965137615,-0.963302752,-0.96146789,-0.959633028,-0.957798165,-0.955963303,
-0.95412844,-0.952293578,-0.950458716,-0.948623853,-0.946788991,-0.944954128,
-0.943119266,-0.941284404,-0.939449541,-0.937614679,-0.935779817,-0.933944954,
-0.932110092,-0.930275229,-0.928440367,-0.926605505,-0.924770642,-0.92293578,
-0.921100917,-0.919266055,-0.917431193,-0.91559633,-0.913761468,-0.911926606,
-0.910091743,-0.908256881,-0.906422018,-0.904587156,-0.902752294,-0.900917431,
-0.899082569,-0.897247706,-0.895412844,-0.893577982,-0.891743119,-0.889908257,
-0.888073394,-0.886238532,-0.88440367,-0.882568807,-0.880733945,-0.878899083,
-0.87706422,-0.875229358,-0.873394495,-0.871559633,-0.869724771,-0.867889908,
-0.866055046,-0.864220183,-0.862385321,-0.860550459,-0.858715596,-0.856880734,
-0.855045872,-0.853211009,-0.851376147,-0.849541284,-0.847706422,-0.84587156,
-0.844036697,-0.842201835,-0.840366972,-0.83853211,-0.836697248,-0.834862385,
-0.833027523,-0.831192661,-0.829357798,-0.827522936,-0.825688073,-0.823853211,
-0.822018349,-0.820183486,-0.818348624,-0.816513761,-0.814678899,-0.812844037,
-0.811009174,-0.809174312,-0.80733945,-0.805504587,-0.803669725,-0.801834862,
-0.8,-0.798165138,-0.796330275,-0.794495413,-0.79266055,-0.790825688,-0.788990826,
-0.787155963,-0.785321101,-0.783486239,-0.781651376,-0.779816514,-0.777981651,
-0.776146789,-0.774311927,-0.772477064,-0.770642202,-0.768807339,-0.766972477,
-0.765137615,-0.763302752,-0.76146789,-0.759633028,-0.757798165,-0.755963303,
-0.75412844,-0.752293578,-0.750458716,-0.748623853,-0.746788991,-0.744954128,
-0.743119266,-0.741284404,-0.739449541,-0.737614679,-0.735779817,-0.733944954,
-0.732110092,-0.730275229,-0.728440367,-0.726605505,-0.724770642,-0.72293578,
-0.721100917,-0.719266055,-0.717431193,-0.71559633,-0.713761468,-0.711926606,
-0.710091743,-0.708256881,-0.706422018,-0.704587156,-0.702752294,-0.700917431,
-0.699082569,-0.697247706,-0.695412844,-0.693577982,-0.691743119,-0.689908257,
-0.688073394,-0.686238532,-0.68440367,-0.682568807,-0.680733945,-0.678899083,
-0.67706422,-0.675229358,-0.673394495,-0.671559633,-0.669724771,-0.667889908,
-0.666055046,-0.664220183,-0.662385321,-0.660550459,-0.658715596,-0.656880734,
-0.655045872,-0.653211009,-0.651376147,-0.649541284,-0.647706422,-0.64587156,
-0.644036697,-0.642201835,-0.640366972,-0.63853211,-0.636697248,-0.634862385,
-0.633027523,-0.631192661,-0.629357798,-0.627522936,-0.625688073,-0.623853211,
-0.622018349,-0.620183486,-0.618348624,-0.616513761,-0.614678899,-0.612844037,
-0.611009174,-0.609174312,-0.60733945,-0.605504587,-0.603669725,-0.601834862,
-0.6,-0.598165138,-0.596330275,-0.594495413,-0.59266055,-0.590825688,-0.588990826,
-0.587155963,-0.585321101,-0.583486239,-0.581651376,-0.579816514,-0.577981651,
-0.576146789,-0.574311927,-0.572477064,-0.570642202,-0.568807339,-0.566972477,
-0.565137615,-0.563302752,-0.56146789,-0.559633028,-0.557798165,-0.555963303,
-0.55412844,-0.552293578,-0.550458716,-0.548623853,-0.546788991,-0.544954128,
-0.543119266,-0.541284404,-0.539449541,-0.537614679,-0.535779817,-0.533944954,
-0.532110092,-0.530275229,-0.528440367,-0.526605505,-0.524770642,-0.52293578,
-0.521100917,-0.519266055,-0.517431193,-0.51559633,-0.513761468,-0.511926606,
-0.510091743,-0.508256881,-0.506422018,-0.504587156,-0.502752294,-0.500917431,
-0.499082569,-0.497247706,-0.495412844,-0.493577982,-0.491743119,-0.489908257,
-0.488073394,-0.486238532,-0.48440367,-0.482568807,-0.480733945,-0.478899083,
-0.47706422,-0.475229358,-0.473394495,-0.471559633,-0.469724771,-0.467889908,
-0.466055046,-0.464220183,-0.462385321,-0.460550459,-0.458715596,-0.456880734,
-0.455045872,-0.453211009,-0.451376147,-0.449541284,-0.447706422,-0.44587156,
-0.444036697,-0.442201835,-0.440366972,-0.43853211,-0.436697248,-0.434862385,
-0.433027523,-0.431192661,-0.429357798,-0.427522936,-0.425688073,-0.423853211,
-0.422018349,-0.420183486,-0.418348624,-0.416513761,-0.414678899,-0.412844037,
-0.411009174,-0.409174312,-0.40733945,-0.405504587,-0.403669725,-0.401834862,
-0.4,-0.398165138,-0.396330275,-0.394495413,-0.39266055,-0.390825688,-0.388990826,
-0.387155963,-0.385321101,-0.383486239,-0.381651376,-0.379816514,-0.377981651,
-0.376146789,-0.374311927,-0.372477064,-0.370642202,-0.368807339,-0.366972477,
-0.365137615,-0.363302752,-0.36146789,-0.359633028,-0.357798165,-0.355963303,
-0.35412844,-0.352293578,-0.350458716,-0.348623853,-0.346788991,-0.344954128,
-0.343119266,-0.341284404,-0.339449541,-0.337614679,-0.335779817,-0.333944954,
-0.332110092,-0.330275229,-0.328440367,-0.326605505,-0.324770642,-0.32293578,
-0.321100917,-0.319266055,-0.317431193,-0.31559633,-0.313761468,-0.311926606,
-0.310091743,-0.308256881,-0.306422018,-0.304587156,-0.302752294,-0.300917431,
-0.299082569,-0.297247706,-0.295412844,-0.293577982,-0.291743119,-0.289908257,
-0.288073394,-0.286238532,-0.28440367,-0.282568807,-0.280733945,-0.278899083,
-0.27706422,-0.275229358,-0.273394495,-0.271559633,-0.269724771,-0.267889908,
-0.266055046,-0.264220183,-0.262385321,-0.260550459,-0.258715596,-0.256880734,
-0.255045872,-0.253211009,-0.251376147,-0.249541284,-0.247706422,-0.24587156,
-0.244036697,-0.242201835,-0.240366972,-0.23853211,-0.236697248,-0.234862385,
-0.233027523,-0.231192661,-0.229357798,-0.227522936,-0.225688073,-0.223853211,
-0.222018349,-0.220183486,-0.218348624,-0.216513761,-0.214678899,-0.212844037,
-0.211009174,-0.209174312,-0.20733945,-0.205504587,-0.203669725,-0.201834862,
-0.2,-0.198165138,-0.196330275,-0.194495413,-0.19266055,-0.190825688,-0.188990826,
-0.187155963,-0.185321101,-0.183486239,-0.181651376,-0.179816514,-0.177981651,
-0.176146789,-0.174311927,-0.172477064,-0.170642202,-0.168807339,-0.166972477,
-0.165137615,-0.163302752,-0.16146789,-0.159633028,-0.157798165,-0.155963303,
-0.15412844,-0.152293578,-0.150458716,-0.148623853,-0.146788991,-0.144954128,
-0.143172104),(0.,0.36),.UNSPECIFIED.);
#6230=B_SPLINE_SURFACE_WITH_KNOTS('',5,1,((#179612,#179613),(#179614,#179615),
(#179616,#179617),(#179618,#179619),(#179620,#179621),(#179622,#179623),
(#179624,#179625),(#179626,#179627),(#179628,#179629),(#179630,#179631),
(#179632,#179633),(#179634,#179635),(#179636,#179637),(#179638,#179639),
(#179640,#179641),(#179642,#179643),(#179644,#179645),(#179646,#179647),
(#179648,#179649),(#179650,#179651),(#179652,#179653),(#179654,#179655),
(#179656,#179657),(#179658,#179659),(#179660,#179661),(#179662,#179663),
(#179664,#179665),(#179666,#179667),(#179668,#179669),(#179670,#179671),
(#179672,#179673),(#179674,#179675),(#179676,#179677),(#179678,#179679),
(#179680,#179681),(#179682,#179683),(#179684,#179685),(#179686,#179687),
(#179688,#179689),(#179690,#179691),(#179692,#179693),(#179694,#179695),
(#179696,#179697),(#179698,#179699),(#179700,#179701),(#179702,#179703),
(#179704,#179705),(#179706,#179707),(#179708,#179709),(#179710,#179711),
(#179712,#179713),(#179714,#179715),(#179716,#179717),(#179718,#179719),
(#179720,#179721),(#179722,#179723),(#179724,#179725),(#179726,#179727),
(#179728,#179729),(#179730,#179731),(#179732,#179733),(#179734,#179735),
(#179736,#179737),(#179738,#179739),(#179740,#179741),(#179742,#179743),
(#179744,#179745),(#179746,#179747),(#179748,#179749),(#179750,#179751),
(#179752,#179753),(#179754,#179755),(#179756,#179757),(#179758,#179759),
(#179760,#179761),(#179762,#179763),(#179764,#179765),(#179766,#179767),
(#179768,#179769),(#179770,#179771),(#179772,#179773),(#179774,#179775),
(#179776,#179777),(#179778,#179779),(#179780,#179781),(#179782,#179783),
(#179784,#179785),(#179786,#179787),(#179788,#179789),(#179790,#179791),
(#179792,#179793),(#179794,#179795),(#179796,#179797),(#179798,#179799),
(#179800,#179801),(#179802,#179803),(#179804,#179805),(#179806,#179807),
(#179808,#179809),(#179810,#179811),(#179812,#179813),(#179814,#179815),
(#179816,#179817),(#179818,#179819),(#179820,#179821),(#179822,#179823),
(#179824,#179825),(#179826,#179827),(#179828,#179829),(#179830,#179831),
(#179832,#179833),(#179834,#179835),(#179836,#179837),(#179838,#179839),
(#179840,#179841),(#179842,#179843),(#179844,#179845),(#179846,#179847),
(#179848,#179849),(#179850,#179851),(#179852,#179853),(#179854,#179855),
(#179856,#179857),(#179858,#179859),(#179860,#179861),(#179862,#179863),
(#179864,#179865),(#179866,#179867),(#179868,#179869),(#179870,#179871),
(#179872,#179873),(#179874,#179875),(#179876,#179877),(#179878,#179879),
(#179880,#179881),(#179882,#179883),(#179884,#179885),(#179886,#179887),
(#179888,#179889),(#179890,#179891),(#179892,#179893),(#179894,#179895),
(#179896,#179897),(#179898,#179899),(#179900,#179901),(#179902,#179903),
(#179904,#179905),(#179906,#179907),(#179908,#179909),(#179910,#179911),
(#179912,#179913),(#179914,#179915),(#179916,#179917),(#179918,#179919),
(#179920,#179921),(#179922,#179923),(#179924,#179925),(#179926,#179927),
(#179928,#179929),(#179930,#179931),(#179932,#179933),(#179934,#179935),
(#179936,#179937),(#179938,#179939),(#179940,#179941),(#179942,#179943),
(#179944,#179945),(#179946,#179947),(#179948,#179949),(#179950,#179951),
(#179952,#179953),(#179954,#179955),(#179956,#179957),(#179958,#179959),
(#179960,#179961),(#179962,#179963),(#179964,#179965),(#179966,#179967),
(#179968,#179969),(#179970,#179971),(#179972,#179973),(#179974,#179975),
(#179976,#179977),(#179978,#179979),(#179980,#179981),(#179982,#179983),
(#179984,#179985),(#179986,#179987),(#179988,#179989),(#179990,#179991),
(#179992,#179993),(#179994,#179995),(#179996,#179997),(#179998,#179999),
(#180000,#180001),(#180002,#180003),(#180004,#180005),(#180006,#180007),
(#180008,#180009),(#180010,#180011),(#180012,#180013),(#180014,#180015),
(#180016,#180017),(#180018,#180019),(#180020,#180021),(#180022,#180023),
(#180024,#180025),(#180026,#180027),(#180028,#180029),(#180030,#180031),
(#180032,#180033),(#180034,#180035),(#180036,#180037),(#180038,#180039),
(#180040,#180041),(#180042,#180043),(#180044,#180045),(#180046,#180047),
(#180048,#180049),(#180050,#180051),(#180052,#180053),(#180054,#180055),
(#180056,#180057),(#180058,#180059),(#180060,#180061),(#180062,#180063),
(#180064,#180065),(#180066,#180067),(#180068,#180069),(#180070,#180071),
(#180072,#180073),(#180074,#180075),(#180076,#180077),(#180078,#180079),
(#180080,#180081),(#180082,#180083),(#180084,#180085),(#180086,#180087),
(#180088,#180089),(#180090,#180091),(#180092,#180093),(#180094,#180095),
(#180096,#180097),(#180098,#180099),(#180100,#180101),(#180102,#180103),
(#180104,#180105),(#180106,#180107),(#180108,#180109),(#180110,#180111),
(#180112,#180113),(#180114,#180115),(#180116,#180117),(#180118,#180119),
(#180120,#180121),(#180122,#180123),(#180124,#180125),(#180126,#180127),
(#180128,#180129),(#180130,#180131),(#180132,#180133),(#180134,#180135),
(#180136,#180137),(#180138,#180139),(#180140,#180141),(#180142,#180143),
(#180144,#180145),(#180146,#180147),(#180148,#180149),(#180150,#180151),
(#180152,#180153),(#180154,#180155),(#180156,#180157),(#180158,#180159),
(#180160,#180161),(#180162,#180163),(#180164,#180165),(#180166,#180167),
(#180168,#180169),(#180170,#180171),(#180172,#180173),(#180174,#180175),
(#180176,#180177),(#180178,#180179),(#180180,#180181),(#180182,#180183),
(#180184,#180185),(#180186,#180187),(#180188,#180189),(#180190,#180191),
(#180192,#180193),(#180194,#180195),(#180196,#180197),(#180198,#180199),
(#180200,#180201),(#180202,#180203),(#180204,#180205),(#180206,#180207),
(#180208,#180209),(#180210,#180211),(#180212,#180213),(#180214,#180215),
(#180216,#180217),(#180218,#180219),(#180220,#180221),(#180222,#180223),
(#180224,#180225),(#180226,#180227),(#180228,#180229),(#180230,#180231),
(#180232,#180233),(#180234,#180235),(#180236,#180237),(#180238,#180239),
(#180240,#180241),(#180242,#180243),(#180244,#180245),(#180246,#180247),
(#180248,#180249),(#180250,#180251),(#180252,#180253),(#180254,#180255),
(#180256,#180257),(#180258,#180259),(#180260,#180261),(#180262,#180263),
(#180264,#180265),(#180266,#180267),(#180268,#180269),(#180270,#180271),
(#180272,#180273),(#180274,#180275),(#180276,#180277),(#180278,#180279),
(#180280,#180281),(#180282,#180283),(#180284,#180285),(#180286,#180287),
(#180288,#180289),(#180290,#180291),(#180292,#180293),(#180294,#180295),
(#180296,#180297),(#180298,#180299),(#180300,#180301),(#180302,#180303),
(#180304,#180305),(#180306,#180307),(#180308,#180309),(#180310,#180311),
(#180312,#180313),(#180314,#180315),(#180316,#180317),(#180318,#180319),
(#180320,#180321),(#180322,#180323),(#180324,#180325),(#180326,#180327),
(#180328,#180329),(#180330,#180331),(#180332,#180333),(#180334,#180335),
(#180336,#180337),(#180338,#180339),(#180340,#180341),(#180342,#180343),
(#180344,#180345),(#180346,#180347),(#180348,#180349),(#180350,#180351),
(#180352,#180353),(#180354,#180355),(#180356,#180357),(#180358,#180359),
(#180360,#180361),(#180362,#180363),(#180364,#180365),(#180366,#180367),
(#180368,#180369),(#180370,#180371),(#180372,#180373),(#180374,#180375),
(#180376,#180377),(#180378,#180379),(#180380,#180381),(#180382,#180383),
(#180384,#180385),(#180386,#180387),(#180388,#180389),(#180390,#180391),
(#180392,#180393),(#180394,#180395),(#180396,#180397),(#180398,#180399),
(#180400,#180401),(#180402,#180403),(#180404,#180405),(#180406,#180407),
(#180408,#180409),(#180410,#180411),(#180412,#180413),(#180414,#180415),
(#180416,#180417),(#180418,#180419),(#180420,#180421),(#180422,#180423),
(#180424,#180425),(#180426,#180427),(#180428,#180429),(#180430,#180431),
(#180432,#180433),(#180434,#180435),(#180436,#180437),(#180438,#180439),
(#180440,#180441),(#180442,#180443),(#180444,#180445),(#180446,#180447),
(#180448,#180449),(#180450,#180451),(#180452,#180453),(#180454,#180455),
(#180456,#180457),(#180458,#180459),(#180460,#180461),(#180462,#180463),
(#180464,#180465),(#180466,#180467),(#180468,#180469),(#180470,#180471),
(#180472,#180473),(#180474,#180475),(#180476,#180477),(#180478,#180479),
(#180480,#180481),(#180482,#180483),(#180484,#180485),(#180486,#180487),
(#180488,#180489),(#180490,#180491),(#180492,#180493),(#180494,#180495),
(#180496,#180497),(#180498,#180499),(#180500,#180501),(#180502,#180503),
(#180504,#180505),(#180506,#180507),(#180508,#180509),(#180510,#180511),
(#180512,#180513),(#180514,#180515),(#180516,#180517),(#180518,#180519),
(#180520,#180521),(#180522,#180523),(#180524,#180525),(#180526,#180527),
(#180528,#180529),(#180530,#180531),(#180532,#180533),(#180534,#180535),
(#180536,#180537),(#180538,#180539),(#180540,#180541),(#180542,#180543),
(#180544,#180545),(#180546,#180547),(#180548,#180549),(#180550,#180551),
(#180552,#180553),(#180554,#180555)),.UNSPECIFIED.,.F.,.F.,.F.,(6,1,1,1,
1,1,1,1,1,1,1,1,1,1,1,1,1,1,1,1,1,1,1,1,1,1,1,1,1,1,1,1,1,1,1,1,1,1,1,1,
1,1,1,1,1,1,1,1,1,1,1,1,1,1,1,1,1,1,1,1,1,1,1,1,1,1,1,1,1,1,1,1,1,1,1,1,
1,1,1,1,1,1,1,1,1,1,1,1,1,1,1,1,1,1,1,1,1,1,1,1,1,1,1,1,1,1,1,1,1,1,1,1,
1,1,1,1,1,1,1,1,1,1,1,1,1,1,1,1,1,1,1,1,1,1,1,1,1,1,1,1,1,1,1,1,1,1,1,1,
1,1,1,1,1,1,1,1,1,1,1,1,1,1,1,1,1,1,1,1,1,1,1,1,1,1,1,1,1,1,1,1,1,1,1,1,
1,1,1,1,1,1,1,1,1,1,1,1,1,1,1,1,1,1,1,1,1,1,1,1,1,1,1,1,1,1,1,1,1,1,1,1,
1,1,1,1,1,1,1,1,1,1,1,1,1,1,1,1,1,1,1,1,1,1,1,1,1,1,1,1,1,1,1,1,1,1,1,1,
1,1,1,1,1,1,1,1,1,1,1,1,1,1,1,1,1,1,1,1,1,1,1,1,1,1,1,1,1,1,1,1,1,1,1,1,
1,1,1,1,1,1,1,1,1,1,1,1,1,1,1,1,1,1,1,1,1,1,1,1,1,1,1,1,1,1,1,1,1,1,1,1,
1,1,1,1,1,1,1,1,1,1,1,1,1,1,1,1,1,1,1,1,1,1,1,1,1,1,1,1,1,1,1,1,1,1,1,1,
1,1,1,1,1,1,1,1,1,1,1,1,1,1,1,1,1,1,1,1,1,1,1,1,1,1,1,1,1,1,1,1,1,1,1,1,
1,1,1,1,1,1,1,1,1,1,1,1,1,1,1,1,1,1,1,1,1,1,1,1,1,1,1,1,1,1,1,1,1,1,1,1,
1,1,1,1,1,1,1,1,1,1,1,1,1,1,1,1,1,1,1,1,1,1,1,1,1,1,1,1,1,1,1,6),(2,2),
(0.143172103,0.144954128,0.146788991,0.148623853,0.150458716,0.152293578,
0.15412844,0.155963303,0.157798165,0.159633028,0.16146789,0.163302752,0.165137615,
0.166972477,0.168807339,0.170642202,0.172477064,0.174311927,0.176146789,
0.177981651,0.179816514,0.181651376,0.183486239,0.185321101,0.187155963,
0.188990826,0.190825688,0.19266055,0.194495413,0.196330275,0.198165138,
0.2,0.201834862,0.203669725,0.205504587,0.20733945,0.209174312,0.211009174,
0.212844037,0.214678899,0.216513761,0.218348624,0.220183486,0.222018349,
0.223853211,0.225688073,0.227522936,0.229357798,0.231192661,0.233027523,
0.234862385,0.236697248,0.23853211,0.240366972,0.242201835,0.244036697,
0.24587156,0.247706422,0.249541284,0.251376147,0.253211009,0.255045872,
0.256880734,0.258715596,0.260550459,0.262385321,0.264220183,0.266055046,
0.267889908,0.269724771,0.271559633,0.273394495,0.275229358,0.27706422,
0.278899083,0.280733945,0.282568807,0.28440367,0.286238532,0.288073394,
0.289908257,0.291743119,0.293577982,0.295412844,0.297247706,0.299082569,
0.300917431,0.302752294,0.304587156,0.306422018,0.308256881,0.310091743,
0.311926606,0.313761468,0.31559633,0.317431193,0.319266055,0.321100917,
0.32293578,0.324770642,0.326605505,0.328440367,0.330275229,0.332110092,
0.333944954,0.335779817,0.337614679,0.339449541,0.341284404,0.343119266,
0.344954128,0.346788991,0.348623853,0.350458716,0.352293578,0.35412844,
0.355963303,0.357798165,0.359633028,0.36146789,0.363302752,0.365137615,
0.366972477,0.368807339,0.370642202,0.372477064,0.374311927,0.376146789,
0.377981651,0.379816514,0.381651376,0.383486239,0.385321101,0.387155963,
0.388990826,0.390825688,0.39266055,0.394495413,0.396330275,0.398165138,
0.4,0.401834862,0.403669725,0.405504587,0.40733945,0.409174312,0.411009174,
0.412844037,0.414678899,0.416513761,0.418348624,0.420183486,0.422018349,
0.423853211,0.425688073,0.427522936,0.429357798,0.431192661,0.433027523,
0.434862385,0.436697248,0.43853211,0.440366972,0.442201835,0.444036697,
0.44587156,0.447706422,0.449541284,0.451376147,0.453211009,0.455045872,
0.456880734,0.458715596,0.460550459,0.462385321,0.464220183,0.466055046,
0.467889908,0.469724771,0.471559633,0.473394495,0.475229358,0.47706422,
0.478899083,0.480733945,0.482568807,0.48440367,0.486238532,0.488073394,
0.489908257,0.491743119,0.493577982,0.495412844,0.497247706,0.499082569,
0.500917431,0.502752294,0.504587156,0.506422018,0.508256881,0.510091743,
0.511926606,0.513761468,0.51559633,0.517431193,0.519266055,0.521100917,
0.52293578,0.524770642,0.526605505,0.528440367,0.530275229,0.532110092,
0.533944954,0.535779817,0.537614679,0.539449541,0.541284404,0.543119266,
0.544954128,0.546788991,0.548623853,0.550458716,0.552293578,0.55412844,
0.555963303,0.557798165,0.559633028,0.56146789,0.563302752,0.565137615,
0.566972477,0.568807339,0.570642202,0.572477064,0.574311927,0.576146789,
0.577981651,0.579816514,0.581651376,0.583486239,0.585321101,0.587155963,
0.588990826,0.590825688,0.59266055,0.594495413,0.596330275,0.598165138,
0.6,0.601834862,0.603669725,0.605504587,0.60733945,0.609174312,0.611009174,
0.612844037,0.614678899,0.616513761,0.618348624,0.620183486,0.622018349,
0.623853211,0.625688073,0.627522936,0.629357798,0.631192661,0.633027523,
0.634862385,0.636697248,0.63853211,0.640366972,0.642201835,0.644036697,
0.64587156,0.647706422,0.649541284,0.651376147,0.653211009,0.655045872,
0.656880734,0.658715596,0.660550459,0.662385321,0.664220183,0.666055046,
0.667889908,0.669724771,0.671559633,0.673394495,0.675229358,0.67706422,
0.678899083,0.680733945,0.682568807,0.68440367,0.686238532,0.688073394,
0.689908257,0.691743119,0.693577982,0.695412844,0.697247706,0.699082569,
0.700917431,0.702752294,0.704587156,0.706422018,0.708256881,0.710091743,
0.711926606,0.713761468,0.71559633,0.717431193,0.719266055,0.721100917,
0.72293578,0.724770642,0.726605505,0.728440367,0.730275229,0.732110092,
0.733944954,0.735779817,0.737614679,0.739449541,0.741284404,0.743119266,
0.744954128,0.746788991,0.748623853,0.750458716,0.752293578,0.75412844,
0.755963303,0.757798165,0.759633028,0.76146789,0.763302752,0.765137615,
0.766972477,0.768807339,0.770642202,0.772477064,0.774311927,0.776146789,
0.777981651,0.779816514,0.781651376,0.783486239,0.785321101,0.787155963,
0.788990826,0.790825688,0.79266055,0.794495413,0.796330275,0.798165138,
0.8,0.801834862,0.803669725,0.805504587,0.80733945,0.809174312,0.811009174,
0.812844037,0.814678899,0.816513761,0.818348624,0.820183486,0.822018349,
0.823853211,0.825688073,0.827522936,0.829357798,0.831192661,0.833027523,
0.834862385,0.836697248,0.83853211,0.840366972,0.842201835,0.844036697,
0.84587156,0.847706422,0.849541284,0.851376147,0.853211009,0.855045872,
0.856880734,0.858715596,0.860550459,0.862385321,0.864220183,0.866055046,
0.867889908,0.869724771,0.871559633,0.873394495,0.875229358,0.87706422,
0.878899083,0.880733945,0.882568807,0.88440367,0.886238532,0.888073394,
0.889908257,0.891743119,0.893577982,0.895412844,0.897247706,0.899082569,
0.900917431,0.902752294,0.904587156,0.906422018,0.908256881,0.910091743,
0.911926606,0.913761468,0.91559633,0.917431193,0.919266055,0.921100917,
0.92293578,0.924770642,0.926605505,0.928440367,0.930275229,0.932110092,
0.933944954,0.935779817,0.937614679,0.939449541,0.941284404,0.943119266,
0.944954128,0.946788991,0.948623853,0.950458716,0.952293578,0.95412844,
0.955963303,0.957798165,0.959633028,0.96146789,0.963302752,0.965137615,
0.966972477,0.968807339,0.970642202,0.972477064,0.974311927,0.976146789,
0.977981651,0.979816514,0.981651376,0.983486239,0.985321101,0.987155963,
0.988990826,0.990825688,0.99266055,0.994495413,0.996330275,0.998165138,
1.),(0.,0.36),.UNSPECIFIED.);
#6231=B_SPLINE_SURFACE_WITH_KNOTS('',5,1,((#181212,#181213),(#181214,#181215),
(#181216,#181217),(#181218,#181219),(#181220,#181221),(#181222,#181223),
(#181224,#181225),(#181226,#181227),(#181228,#181229),(#181230,#181231),
(#181232,#181233),(#181234,#181235),(#181236,#181237),(#181238,#181239),
(#181240,#181241),(#181242,#181243),(#181244,#181245),(#181246,#181247),
(#181248,#181249),(#181250,#181251),(#181252,#181253),(#181254,#181255),
(#181256,#181257),(#181258,#181259),(#181260,#181261),(#181262,#181263),
(#181264,#181265),(#181266,#181267),(#181268,#181269),(#181270,#181271),
(#181272,#181273),(#181274,#181275),(#181276,#181277),(#181278,#181279),
(#181280,#181281),(#181282,#181283),(#181284,#181285),(#181286,#181287),
(#181288,#181289),(#181290,#181291),(#181292,#181293),(#181294,#181295),
(#181296,#181297),(#181298,#181299),(#181300,#181301),(#181302,#181303),
(#181304,#181305),(#181306,#181307),(#181308,#181309),(#181310,#181311),
(#181312,#181313),(#181314,#181315),(#181316,#181317),(#181318,#181319),
(#181320,#181321),(#181322,#181323),(#181324,#181325),(#181326,#181327),
(#181328,#181329),(#181330,#181331),(#181332,#181333),(#181334,#181335),
(#181336,#181337),(#181338,#181339),(#181340,#181341),(#181342,#181343),
(#181344,#181345),(#181346,#181347),(#181348,#181349),(#181350,#181351),
(#181352,#181353),(#181354,#181355),(#181356,#181357),(#181358,#181359),
(#181360,#181361),(#181362,#181363),(#181364,#181365),(#181366,#181367),
(#181368,#181369),(#181370,#181371),(#181372,#181373),(#181374,#181375),
(#181376,#181377),(#181378,#181379),(#181380,#181381),(#181382,#181383),
(#181384,#181385),(#181386,#181387),(#181388,#181389),(#181390,#181391),
(#181392,#181393),(#181394,#181395),(#181396,#181397),(#181398,#181399),
(#181400,#181401),(#181402,#181403),(#181404,#181405),(#181406,#181407),
(#181408,#181409),(#181410,#181411),(#181412,#181413),(#181414,#181415),
(#181416,#181417),(#181418,#181419),(#181420,#181421),(#181422,#181423),
(#181424,#181425),(#181426,#181427),(#181428,#181429),(#181430,#181431),
(#181432,#181433),(#181434,#181435),(#181436,#181437),(#181438,#181439),
(#181440,#181441),(#181442,#181443),(#181444,#181445),(#181446,#181447),
(#181448,#181449),(#181450,#181451),(#181452,#181453),(#181454,#181455),
(#181456,#181457),(#181458,#181459),(#181460,#181461),(#181462,#181463),
(#181464,#181465),(#181466,#181467),(#181468,#181469),(#181470,#181471),
(#181472,#181473),(#181474,#181475),(#181476,#181477),(#181478,#181479),
(#181480,#181481),(#181482,#181483),(#181484,#181485),(#181486,#181487),
(#181488,#181489),(#181490,#181491),(#181492,#181493),(#181494,#181495),
(#181496,#181497),(#181498,#181499),(#181500,#181501),(#181502,#181503),
(#181504,#181505),(#181506,#181507),(#181508,#181509),(#181510,#181511),
(#181512,#181513),(#181514,#181515),(#181516,#181517),(#181518,#181519),
(#181520,#181521),(#181522,#181523),(#181524,#181525),(#181526,#181527),
(#181528,#181529),(#181530,#181531),(#181532,#181533),(#181534,#181535),
(#181536,#181537),(#181538,#181539),(#181540,#181541),(#181542,#181543),
(#181544,#181545),(#181546,#181547),(#181548,#181549),(#181550,#181551),
(#181552,#181553),(#181554,#181555),(#181556,#181557),(#181558,#181559),
(#181560,#181561),(#181562,#181563),(#181564,#181565),(#181566,#181567),
(#181568,#181569),(#181570,#181571),(#181572,#181573),(#181574,#181575),
(#181576,#181577),(#181578,#181579),(#181580,#181581),(#181582,#181583),
(#181584,#181585),(#181586,#181587),(#181588,#181589),(#181590,#181591),
(#181592,#181593),(#181594,#181595),(#181596,#181597),(#181598,#181599),
(#181600,#181601),(#181602,#181603),(#181604,#181605),(#181606,#181607),
(#181608,#181609),(#181610,#181611),(#181612,#181613),(#181614,#181615),
(#181616,#181617),(#181618,#181619),(#181620,#181621),(#181622,#181623),
(#181624,#181625),(#181626,#181627),(#181628,#181629),(#181630,#181631),
(#181632,#181633),(#181634,#181635),(#181636,#181637),(#181638,#181639),
(#181640,#181641),(#181642,#181643),(#181644,#181645),(#181646,#181647),
(#181648,#181649),(#181650,#181651),(#181652,#181653),(#181654,#181655),
(#181656,#181657),(#181658,#181659),(#181660,#181661),(#181662,#181663),
(#181664,#181665),(#181666,#181667),(#181668,#181669),(#181670,#181671),
(#181672,#181673),(#181674,#181675),(#181676,#181677),(#181678,#181679),
(#181680,#181681),(#181682,#181683),(#181684,#181685),(#181686,#181687),
(#181688,#181689),(#181690,#181691),(#181692,#181693),(#181694,#181695),
(#181696,#181697),(#181698,#181699),(#181700,#181701),(#181702,#181703),
(#181704,#181705),(#181706,#181707),(#181708,#181709),(#181710,#181711),
(#181712,#181713),(#181714,#181715),(#181716,#181717),(#181718,#181719),
(#181720,#181721),(#181722,#181723),(#181724,#181725),(#181726,#181727),
(#181728,#181729),(#181730,#181731),(#181732,#181733),(#181734,#181735),
(#181736,#181737),(#181738,#181739),(#181740,#181741),(#181742,#181743),
(#181744,#181745),(#181746,#181747),(#181748,#181749),(#181750,#181751),
(#181752,#181753),(#181754,#181755),(#181756,#181757),(#181758,#181759),
(#181760,#181761),(#181762,#181763),(#181764,#181765),(#181766,#181767),
(#181768,#181769),(#181770,#181771),(#181772,#181773),(#181774,#181775),
(#181776,#181777),(#181778,#181779),(#181780,#181781),(#181782,#181783),
(#181784,#181785),(#181786,#181787),(#181788,#181789),(#181790,#181791),
(#181792,#181793),(#181794,#181795),(#181796,#181797),(#181798,#181799),
(#181800,#181801),(#181802,#181803),(#181804,#181805),(#181806,#181807),
(#181808,#181809),(#181810,#181811),(#181812,#181813),(#181814,#181815),
(#181816,#181817),(#181818,#181819),(#181820,#181821),(#181822,#181823),
(#181824,#181825),(#181826,#181827),(#181828,#181829),(#181830,#181831),
(#181832,#181833),(#181834,#181835),(#181836,#181837),(#181838,#181839),
(#181840,#181841),(#181842,#181843),(#181844,#181845),(#181846,#181847),
(#181848,#181849),(#181850,#181851),(#181852,#181853),(#181854,#181855),
(#181856,#181857),(#181858,#181859),(#181860,#181861),(#181862,#181863),
(#181864,#181865),(#181866,#181867),(#181868,#181869),(#181870,#181871),
(#181872,#181873),(#181874,#181875),(#181876,#181877),(#181878,#181879),
(#181880,#181881),(#181882,#181883),(#181884,#181885),(#181886,#181887),
(#181888,#181889),(#181890,#181891),(#181892,#181893),(#181894,#181895),
(#181896,#181897),(#181898,#181899),(#181900,#181901),(#181902,#181903),
(#181904,#181905),(#181906,#181907),(#181908,#181909),(#181910,#181911),
(#181912,#181913),(#181914,#181915),(#181916,#181917),(#181918,#181919),
(#181920,#181921),(#181922,#181923),(#181924,#181925),(#181926,#181927),
(#181928,#181929),(#181930,#181931),(#181932,#181933),(#181934,#181935),
(#181936,#181937),(#181938,#181939),(#181940,#181941),(#181942,#181943),
(#181944,#181945),(#181946,#181947),(#181948,#181949),(#181950,#181951),
(#181952,#181953),(#181954,#181955),(#181956,#181957),(#181958,#181959),
(#181960,#181961),(#181962,#181963),(#181964,#181965),(#181966,#181967),
(#181968,#181969),(#181970,#181971),(#181972,#181973),(#181974,#181975),
(#181976,#181977),(#181978,#181979),(#181980,#181981),(#181982,#181983),
(#181984,#181985),(#181986,#181987),(#181988,#181989),(#181990,#181991),
(#181992,#181993),(#181994,#181995),(#181996,#181997),(#181998,#181999),
(#182000,#182001),(#182002,#182003),(#182004,#182005),(#182006,#182007),
(#182008,#182009),(#182010,#182011),(#182012,#182013),(#182014,#182015),
(#182016,#182017),(#182018,#182019),(#182020,#182021),(#182022,#182023),
(#182024,#182025),(#182026,#182027),(#182028,#182029),(#182030,#182031),
(#182032,#182033),(#182034,#182035),(#182036,#182037),(#182038,#182039),
(#182040,#182041),(#182042,#182043),(#182044,#182045),(#182046,#182047),
(#182048,#182049),(#182050,#182051),(#182052,#182053),(#182054,#182055),
(#182056,#182057),(#182058,#182059),(#182060,#182061),(#182062,#182063),
(#182064,#182065),(#182066,#182067),(#182068,#182069),(#182070,#182071),
(#182072,#182073),(#182074,#182075),(#182076,#182077),(#182078,#182079),
(#182080,#182081),(#182082,#182083),(#182084,#182085),(#182086,#182087),
(#182088,#182089),(#182090,#182091),(#182092,#182093),(#182094,#182095),
(#182096,#182097),(#182098,#182099),(#182100,#182101),(#182102,#182103),
(#182104,#182105),(#182106,#182107),(#182108,#182109),(#182110,#182111),
(#182112,#182113),(#182114,#182115),(#182116,#182117),(#182118,#182119),
(#182120,#182121),(#182122,#182123),(#182124,#182125),(#182126,#182127),
(#182128,#182129),(#182130,#182131),(#182132,#182133),(#182134,#182135),
(#182136,#182137),(#182138,#182139),(#182140,#182141),(#182142,#182143),
(#182144,#182145),(#182146,#182147),(#182148,#182149),(#182150,#182151),
(#182152,#182153),(#182154,#182155)),.UNSPECIFIED.,.F.,.F.,.F.,(6,1,1,1,
1,1,1,1,1,1,1,1,1,1,1,1,1,1,1,1,1,1,1,1,1,1,1,1,1,1,1,1,1,1,1,1,1,1,1,1,
1,1,1,1,1,1,1,1,1,1,1,1,1,1,1,1,1,1,1,1,1,1,1,1,1,1,1,1,1,1,1,1,1,1,1,1,
1,1,1,1,1,1,1,1,1,1,1,1,1,1,1,1,1,1,1,1,1,1,1,1,1,1,1,1,1,1,1,1,1,1,1,1,
1,1,1,1,1,1,1,1,1,1,1,1,1,1,1,1,1,1,1,1,1,1,1,1,1,1,1,1,1,1,1,1,1,1,1,1,
1,1,1,1,1,1,1,1,1,1,1,1,1,1,1,1,1,1,1,1,1,1,1,1,1,1,1,1,1,1,1,1,1,1,1,1,
1,1,1,1,1,1,1,1,1,1,1,1,1,1,1,1,1,1,1,1,1,1,1,1,1,1,1,1,1,1,1,1,1,1,1,1,
1,1,1,1,1,1,1,1,1,1,1,1,1,1,1,1,1,1,1,1,1,1,1,1,1,1,1,1,1,1,1,1,1,1,1,1,
1,1,1,1,1,1,1,1,1,1,1,1,1,1,1,1,1,1,1,1,1,1,1,1,1,1,1,1,1,1,1,1,1,1,1,1,
1,1,1,1,1,1,1,1,1,1,1,1,1,1,1,1,1,1,1,1,1,1,1,1,1,1,1,1,1,1,1,1,1,1,1,1,
1,1,1,1,1,1,1,1,1,1,1,1,1,1,1,1,1,1,1,1,1,1,1,1,1,1,1,1,1,1,1,1,1,1,1,1,
1,1,1,1,1,1,1,1,1,1,1,1,1,1,1,1,1,1,1,1,1,1,1,1,1,1,1,1,1,1,1,1,1,1,1,1,
1,1,1,1,1,1,1,1,1,1,1,1,1,1,1,1,1,1,1,1,1,1,1,1,1,1,1,1,1,1,1,1,1,1,1,1,
1,1,1,1,1,1,1,1,1,1,1,1,1,1,1,1,1,1,1,1,1,1,1,1,1,1,1,1,1,1,1,6),(2,2),
(0.143172103,0.144954128,0.146788991,0.148623853,0.150458716,0.152293578,
0.15412844,0.155963303,0.157798165,0.159633028,0.16146789,0.163302752,0.165137615,
0.166972477,0.168807339,0.170642202,0.172477064,0.174311927,0.176146789,
0.177981651,0.179816514,0.181651376,0.183486239,0.185321101,0.187155963,
0.188990826,0.190825688,0.19266055,0.194495413,0.196330275,0.198165138,
0.2,0.201834862,0.203669725,0.205504587,0.20733945,0.209174312,0.211009174,
0.212844037,0.214678899,0.216513761,0.218348624,0.220183486,0.222018349,
0.223853211,0.225688073,0.227522936,0.229357798,0.231192661,0.233027523,
0.234862385,0.236697248,0.23853211,0.240366972,0.242201835,0.244036697,
0.24587156,0.247706422,0.249541284,0.251376147,0.253211009,0.255045872,
0.256880734,0.258715596,0.260550459,0.262385321,0.264220183,0.266055046,
0.267889908,0.269724771,0.271559633,0.273394495,0.275229358,0.27706422,
0.278899083,0.280733945,0.282568807,0.28440367,0.286238532,0.288073394,
0.289908257,0.291743119,0.293577982,0.295412844,0.297247706,0.299082569,
0.300917431,0.302752294,0.304587156,0.306422018,0.308256881,0.310091743,
0.311926606,0.313761468,0.31559633,0.317431193,0.319266055,0.321100917,
0.32293578,0.324770642,0.326605505,0.328440367,0.330275229,0.332110092,
0.333944954,0.335779817,0.337614679,0.339449541,0.341284404,0.343119266,
0.344954128,0.346788991,0.348623853,0.350458716,0.352293578,0.35412844,
0.355963303,0.357798165,0.359633028,0.36146789,0.363302752,0.365137615,
0.366972477,0.368807339,0.370642202,0.372477064,0.374311927,0.376146789,
0.377981651,0.379816514,0.381651376,0.383486239,0.385321101,0.387155963,
0.388990826,0.390825688,0.39266055,0.394495413,0.396330275,0.398165138,
0.4,0.401834862,0.403669725,0.405504587,0.40733945,0.409174312,0.411009174,
0.412844037,0.414678899,0.416513761,0.418348624,0.420183486,0.422018349,
0.423853211,0.425688073,0.427522936,0.429357798,0.431192661,0.433027523,
0.434862385,0.436697248,0.43853211,0.440366972,0.442201835,0.444036697,
0.44587156,0.447706422,0.449541284,0.451376147,0.453211009,0.455045872,
0.456880734,0.458715596,0.460550459,0.462385321,0.464220183,0.466055046,
0.467889908,0.469724771,0.471559633,0.473394495,0.475229358,0.47706422,
0.478899083,0.480733945,0.482568807,0.48440367,0.486238532,0.488073394,
0.489908257,0.491743119,0.493577982,0.495412844,0.497247706,0.499082569,
0.500917431,0.502752294,0.504587156,0.506422018,0.508256881,0.510091743,
0.511926606,0.513761468,0.51559633,0.517431193,0.519266055,0.521100917,
0.52293578,0.524770642,0.526605505,0.528440367,0.530275229,0.532110092,
0.533944954,0.535779817,0.537614679,0.539449541,0.541284404,0.543119266,
0.544954128,0.546788991,0.548623853,0.550458716,0.552293578,0.55412844,
0.555963303,0.557798165,0.559633028,0.56146789,0.563302752,0.565137615,
0.566972477,0.568807339,0.570642202,0.572477064,0.574311927,0.576146789,
0.577981651,0.579816514,0.581651376,0.583486239,0.585321101,0.587155963,
0.588990826,0.590825688,0.59266055,0.594495413,0.596330275,0.598165138,
0.6,0.601834862,0.603669725,0.605504587,0.60733945,0.609174312,0.611009174,
0.612844037,0.614678899,0.616513761,0.618348624,0.620183486,0.622018349,
0.623853211,0.625688073,0.627522936,0.629357798,0.631192661,0.633027523,
0.634862385,0.636697248,0.63853211,0.640366972,0.642201835,0.644036697,
0.64587156,0.647706422,0.649541284,0.651376147,0.653211009,0.655045872,
0.656880734,0.658715596,0.660550459,0.662385321,0.664220183,0.666055046,
0.667889908,0.669724771,0.671559633,0.673394495,0.675229358,0.67706422,
0.678899083,0.680733945,0.682568807,0.68440367,0.686238532,0.688073394,
0.689908257,0.691743119,0.693577982,0.695412844,0.697247706,0.699082569,
0.700917431,0.702752294,0.704587156,0.706422018,0.708256881,0.710091743,
0.711926606,0.713761468,0.71559633,0.717431193,0.719266055,0.721100917,
0.72293578,0.724770642,0.726605505,0.728440367,0.730275229,0.732110092,
0.733944954,0.735779817,0.737614679,0.739449541,0.741284404,0.743119266,
0.744954128,0.746788991,0.748623853,0.750458716,0.752293578,0.75412844,
0.755963303,0.757798165,0.759633028,0.76146789,0.763302752,0.765137615,
0.766972477,0.768807339,0.770642202,0.772477064,0.774311927,0.776146789,
0.777981651,0.779816514,0.781651376,0.783486239,0.785321101,0.787155963,
0.788990826,0.790825688,0.79266055,0.794495413,0.796330275,0.798165138,
0.8,0.801834862,0.803669725,0.805504587,0.80733945,0.809174312,0.811009174,
0.812844037,0.814678899,0.816513761,0.818348624,0.820183486,0.822018349,
0.823853211,0.825688073,0.827522936,0.829357798,0.831192661,0.833027523,
0.834862385,0.836697248,0.83853211,0.840366972,0.842201835,0.844036697,
0.84587156,0.847706422,0.849541284,0.851376147,0.853211009,0.855045872,
0.856880734,0.858715596,0.860550459,0.862385321,0.864220183,0.866055046,
0.867889908,0.869724771,0.871559633,0.873394495,0.875229358,0.87706422,
0.878899083,0.880733945,0.882568807,0.88440367,0.886238532,0.888073394,
0.889908257,0.891743119,0.893577982,0.895412844,0.897247706,0.899082569,
0.900917431,0.902752294,0.904587156,0.906422018,0.908256881,0.910091743,
0.911926606,0.913761468,0.91559633,0.917431193,0.919266055,0.921100917,
0.92293578,0.924770642,0.926605505,0.928440367,0.930275229,0.932110092,
0.933944954,0.935779817,0.937614679,0.939449541,0.941284404,0.943119266,
0.944954128,0.946788991,0.948623853,0.950458716,0.952293578,0.95412844,
0.955963303,0.957798165,0.959633028,0.96146789,0.963302752,0.965137615,
0.966972477,0.968807339,0.970642202,0.972477064,0.974311927,0.976146789,
0.977981651,0.979816514,0.981651376,0.983486239,0.985321101,0.987155963,
0.988990826,0.990825688,0.99266055,0.994495413,0.996330275,0.998165138,
1.),(0.,0.36),.UNSPECIFIED.);
#6232=B_SPLINE_SURFACE_WITH_KNOTS('',5,1,((#182788,#182789),(#182790,#182791),
(#182792,#182793),(#182794,#182795),(#182796,#182797),(#182798,#182799),
(#182800,#182801),(#182802,#182803),(#182804,#182805),(#182806,#182807),
(#182808,#182809),(#182810,#182811),(#182812,#182813),(#182814,#182815),
(#182816,#182817),(#182818,#182819),(#182820,#182821),(#182822,#182823),
(#182824,#182825),(#182826,#182827),(#182828,#182829),(#182830,#182831),
(#182832,#182833),(#182834,#182835),(#182836,#182837),(#182838,#182839),
(#182840,#182841),(#182842,#182843),(#182844,#182845),(#182846,#182847),
(#182848,#182849),(#182850,#182851),(#182852,#182853),(#182854,#182855),
(#182856,#182857),(#182858,#182859),(#182860,#182861),(#182862,#182863),
(#182864,#182865),(#182866,#182867),(#182868,#182869),(#182870,#182871),
(#182872,#182873),(#182874,#182875),(#182876,#182877),(#182878,#182879),
(#182880,#182881),(#182882,#182883),(#182884,#182885),(#182886,#182887),
(#182888,#182889),(#182890,#182891),(#182892,#182893),(#182894,#182895),
(#182896,#182897),(#182898,#182899),(#182900,#182901),(#182902,#182903),
(#182904,#182905),(#182906,#182907),(#182908,#182909),(#182910,#182911),
(#182912,#182913),(#182914,#182915),(#182916,#182917),(#182918,#182919),
(#182920,#182921),(#182922,#182923),(#182924,#182925),(#182926,#182927),
(#182928,#182929),(#182930,#182931),(#182932,#182933),(#182934,#182935),
(#182936,#182937),(#182938,#182939),(#182940,#182941),(#182942,#182943),
(#182944,#182945),(#182946,#182947),(#182948,#182949),(#182950,#182951),
(#182952,#182953),(#182954,#182955),(#182956,#182957),(#182958,#182959),
(#182960,#182961),(#182962,#182963),(#182964,#182965),(#182966,#182967),
(#182968,#182969),(#182970,#182971),(#182972,#182973),(#182974,#182975),
(#182976,#182977),(#182978,#182979),(#182980,#182981),(#182982,#182983),
(#182984,#182985),(#182986,#182987),(#182988,#182989),(#182990,#182991),
(#182992,#182993),(#182994,#182995),(#182996,#182997),(#182998,#182999),
(#183000,#183001),(#183002,#183003),(#183004,#183005),(#183006,#183007),
(#183008,#183009),(#183010,#183011),(#183012,#183013),(#183014,#183015),
(#183016,#183017),(#183018,#183019),(#183020,#183021),(#183022,#183023),
(#183024,#183025),(#183026,#183027),(#183028,#183029),(#183030,#183031),
(#183032,#183033),(#183034,#183035),(#183036,#183037),(#183038,#183039),
(#183040,#183041),(#183042,#183043),(#183044,#183045),(#183046,#183047),
(#183048,#183049),(#183050,#183051),(#183052,#183053),(#183054,#183055),
(#183056,#183057),(#183058,#183059),(#183060,#183061),(#183062,#183063),
(#183064,#183065),(#183066,#183067),(#183068,#183069),(#183070,#183071),
(#183072,#183073),(#183074,#183075),(#183076,#183077),(#183078,#183079),
(#183080,#183081),(#183082,#183083),(#183084,#183085),(#183086,#183087),
(#183088,#183089),(#183090,#183091),(#183092,#183093),(#183094,#183095),
(#183096,#183097),(#183098,#183099),(#183100,#183101),(#183102,#183103),
(#183104,#183105),(#183106,#183107),(#183108,#183109),(#183110,#183111),
(#183112,#183113),(#183114,#183115),(#183116,#183117),(#183118,#183119),
(#183120,#183121),(#183122,#183123),(#183124,#183125),(#183126,#183127),
(#183128,#183129),(#183130,#183131),(#183132,#183133),(#183134,#183135),
(#183136,#183137),(#183138,#183139),(#183140,#183141),(#183142,#183143),
(#183144,#183145),(#183146,#183147),(#183148,#183149),(#183150,#183151),
(#183152,#183153),(#183154,#183155),(#183156,#183157),(#183158,#183159),
(#183160,#183161),(#183162,#183163),(#183164,#183165),(#183166,#183167),
(#183168,#183169),(#183170,#183171),(#183172,#183173),(#183174,#183175),
(#183176,#183177),(#183178,#183179),(#183180,#183181),(#183182,#183183),
(#183184,#183185),(#183186,#183187),(#183188,#183189),(#183190,#183191),
(#183192,#183193),(#183194,#183195),(#183196,#183197),(#183198,#183199),
(#183200,#183201),(#183202,#183203),(#183204,#183205),(#183206,#183207),
(#183208,#183209),(#183210,#183211),(#183212,#183213),(#183214,#183215),
(#183216,#183217),(#183218,#183219),(#183220,#183221),(#183222,#183223),
(#183224,#183225),(#183226,#183227),(#183228,#183229),(#183230,#183231),
(#183232,#183233),(#183234,#183235),(#183236,#183237),(#183238,#183239),
(#183240,#183241),(#183242,#183243),(#183244,#183245),(#183246,#183247),
(#183248,#183249),(#183250,#183251),(#183252,#183253),(#183254,#183255),
(#183256,#183257),(#183258,#183259),(#183260,#183261),(#183262,#183263),
(#183264,#183265),(#183266,#183267),(#183268,#183269),(#183270,#183271),
(#183272,#183273),(#183274,#183275),(#183276,#183277),(#183278,#183279),
(#183280,#183281),(#183282,#183283),(#183284,#183285),(#183286,#183287),
(#183288,#183289),(#183290,#183291),(#183292,#183293),(#183294,#183295),
(#183296,#183297),(#183298,#183299),(#183300,#183301),(#183302,#183303),
(#183304,#183305),(#183306,#183307),(#183308,#183309),(#183310,#183311),
(#183312,#183313),(#183314,#183315),(#183316,#183317),(#183318,#183319),
(#183320,#183321),(#183322,#183323),(#183324,#183325),(#183326,#183327),
(#183328,#183329),(#183330,#183331),(#183332,#183333),(#183334,#183335),
(#183336,#183337),(#183338,#183339),(#183340,#183341),(#183342,#183343),
(#183344,#183345),(#183346,#183347),(#183348,#183349),(#183350,#183351),
(#183352,#183353),(#183354,#183355),(#183356,#183357),(#183358,#183359),
(#183360,#183361),(#183362,#183363),(#183364,#183365),(#183366,#183367),
(#183368,#183369),(#183370,#183371),(#183372,#183373),(#183374,#183375),
(#183376,#183377),(#183378,#183379),(#183380,#183381),(#183382,#183383),
(#183384,#183385),(#183386,#183387),(#183388,#183389),(#183390,#183391),
(#183392,#183393),(#183394,#183395),(#183396,#183397),(#183398,#183399),
(#183400,#183401),(#183402,#183403),(#183404,#183405),(#183406,#183407),
(#183408,#183409),(#183410,#183411),(#183412,#183413),(#183414,#183415),
(#183416,#183417),(#183418,#183419),(#183420,#183421),(#183422,#183423),
(#183424,#183425),(#183426,#183427),(#183428,#183429),(#183430,#183431),
(#183432,#183433),(#183434,#183435),(#183436,#183437),(#183438,#183439),
(#183440,#183441),(#183442,#183443),(#183444,#183445),(#183446,#183447),
(#183448,#183449),(#183450,#183451),(#183452,#183453),(#183454,#183455),
(#183456,#183457),(#183458,#183459),(#183460,#183461),(#183462,#183463),
(#183464,#183465),(#183466,#183467),(#183468,#183469),(#183470,#183471),
(#183472,#183473),(#183474,#183475),(#183476,#183477),(#183478,#183479),
(#183480,#183481),(#183482,#183483),(#183484,#183485),(#183486,#183487),
(#183488,#183489),(#183490,#183491),(#183492,#183493),(#183494,#183495),
(#183496,#183497),(#183498,#183499),(#183500,#183501),(#183502,#183503),
(#183504,#183505),(#183506,#183507),(#183508,#183509),(#183510,#183511),
(#183512,#183513),(#183514,#183515),(#183516,#183517),(#183518,#183519),
(#183520,#183521),(#183522,#183523),(#183524,#183525),(#183526,#183527),
(#183528,#183529),(#183530,#183531),(#183532,#183533),(#183534,#183535),
(#183536,#183537),(#183538,#183539),(#183540,#183541),(#183542,#183543),
(#183544,#183545),(#183546,#183547),(#183548,#183549),(#183550,#183551),
(#183552,#183553),(#183554,#183555),(#183556,#183557),(#183558,#183559),
(#183560,#183561),(#183562,#183563),(#183564,#183565),(#183566,#183567),
(#183568,#183569),(#183570,#183571),(#183572,#183573),(#183574,#183575),
(#183576,#183577),(#183578,#183579),(#183580,#183581),(#183582,#183583),
(#183584,#183585),(#183586,#183587),(#183588,#183589),(#183590,#183591),
(#183592,#183593),(#183594,#183595),(#183596,#183597),(#183598,#183599),
(#183600,#183601),(#183602,#183603),(#183604,#183605),(#183606,#183607),
(#183608,#183609),(#183610,#183611),(#183612,#183613),(#183614,#183615),
(#183616,#183617),(#183618,#183619),(#183620,#183621),(#183622,#183623),
(#183624,#183625),(#183626,#183627),(#183628,#183629),(#183630,#183631),
(#183632,#183633),(#183634,#183635),(#183636,#183637),(#183638,#183639),
(#183640,#183641),(#183642,#183643),(#183644,#183645),(#183646,#183647),
(#183648,#183649),(#183650,#183651),(#183652,#183653),(#183654,#183655),
(#183656,#183657),(#183658,#183659),(#183660,#183661),(#183662,#183663),
(#183664,#183665),(#183666,#183667),(#183668,#183669),(#183670,#183671),
(#183672,#183673),(#183674,#183675),(#183676,#183677),(#183678,#183679),
(#183680,#183681),(#183682,#183683),(#183684,#183685),(#183686,#183687),
(#183688,#183689),(#183690,#183691),(#183692,#183693),(#183694,#183695),
(#183696,#183697),(#183698,#183699),(#183700,#183701),(#183702,#183703),
(#183704,#183705),(#183706,#183707),(#183708,#183709),(#183710,#183711),
(#183712,#183713),(#183714,#183715),(#183716,#183717),(#183718,#183719),
(#183720,#183721),(#183722,#183723),(#183724,#183725),(#183726,#183727),
(#183728,#183729),(#183730,#183731)),.UNSPECIFIED.,.F.,.F.,.F.,(6,1,1,1,
1,1,1,1,1,1,1,1,1,1,1,1,1,1,1,1,1,1,1,1,1,1,1,1,1,1,1,1,1,1,1,1,1,1,1,1,
1,1,1,1,1,1,1,1,1,1,1,1,1,1,1,1,1,1,1,1,1,1,1,1,1,1,1,1,1,1,1,1,1,1,1,1,
1,1,1,1,1,1,1,1,1,1,1,1,1,1,1,1,1,1,1,1,1,1,1,1,1,1,1,1,1,1,1,1,1,1,1,1,
1,1,1,1,1,1,1,1,1,1,1,1,1,1,1,1,1,1,1,1,1,1,1,1,1,1,1,1,1,1,1,1,1,1,1,1,
1,1,1,1,1,1,1,1,1,1,1,1,1,1,1,1,1,1,1,1,1,1,1,1,1,1,1,1,1,1,1,1,1,1,1,1,
1,1,1,1,1,1,1,1,1,1,1,1,1,1,1,1,1,1,1,1,1,1,1,1,1,1,1,1,1,1,1,1,1,1,1,1,
1,1,1,1,1,1,1,1,1,1,1,1,1,1,1,1,1,1,1,1,1,1,1,1,1,1,1,1,1,1,1,1,1,1,1,1,
1,1,1,1,1,1,1,1,1,1,1,1,1,1,1,1,1,1,1,1,1,1,1,1,1,1,1,1,1,1,1,1,1,1,1,1,
1,1,1,1,1,1,1,1,1,1,1,1,1,1,1,1,1,1,1,1,1,1,1,1,1,1,1,1,1,1,1,1,1,1,1,1,
1,1,1,1,1,1,1,1,1,1,1,1,1,1,1,1,1,1,1,1,1,1,1,1,1,1,1,1,1,1,1,1,1,1,1,1,
1,1,1,1,1,1,1,1,1,1,1,1,1,1,1,1,1,1,1,1,1,1,1,1,1,1,1,1,1,1,1,1,1,1,1,1,
1,1,1,1,1,1,1,1,1,1,1,1,1,1,1,1,1,1,1,1,1,1,1,1,1,1,1,1,1,1,1,1,1,1,1,1,
1,1,1,1,1,1,1,1,1,1,1,1,1,1,1,1,1,1,1,1,1,1,1,1,1,1,1,1,1,1,1,6),(2,2),
(-1.,-0.998165138,-0.996330275,-0.994495413,-0.99266055,-0.990825688,-0.988990826,
-0.987155963,-0.985321101,-0.983486239,-0.981651376,-0.979816514,-0.977981651,
-0.976146789,-0.974311927,-0.972477064,-0.970642202,-0.968807339,-0.966972477,
-0.965137615,-0.963302752,-0.96146789,-0.959633028,-0.957798165,-0.955963303,
-0.95412844,-0.952293578,-0.950458716,-0.948623853,-0.946788991,-0.944954128,
-0.943119266,-0.941284404,-0.939449541,-0.937614679,-0.935779817,-0.933944954,
-0.932110092,-0.930275229,-0.928440367,-0.926605505,-0.924770642,-0.92293578,
-0.921100917,-0.919266055,-0.917431193,-0.91559633,-0.913761468,-0.911926606,
-0.910091743,-0.908256881,-0.906422018,-0.904587156,-0.902752294,-0.900917431,
-0.899082569,-0.897247706,-0.895412844,-0.893577982,-0.891743119,-0.889908257,
-0.888073394,-0.886238532,-0.88440367,-0.882568807,-0.880733945,-0.878899083,
-0.87706422,-0.875229358,-0.873394495,-0.871559633,-0.869724771,-0.867889908,
-0.866055046,-0.864220183,-0.862385321,-0.860550459,-0.858715596,-0.856880734,
-0.855045872,-0.853211009,-0.851376147,-0.849541284,-0.847706422,-0.84587156,
-0.844036697,-0.842201835,-0.840366972,-0.83853211,-0.836697248,-0.834862385,
-0.833027523,-0.831192661,-0.829357798,-0.827522936,-0.825688073,-0.823853211,
-0.822018349,-0.820183486,-0.818348624,-0.816513761,-0.814678899,-0.812844037,
-0.811009174,-0.809174312,-0.80733945,-0.805504587,-0.803669725,-0.801834862,
-0.8,-0.798165138,-0.796330275,-0.794495413,-0.79266055,-0.790825688,-0.788990826,
-0.787155963,-0.785321101,-0.783486239,-0.781651376,-0.779816514,-0.777981651,
-0.776146789,-0.774311927,-0.772477064,-0.770642202,-0.768807339,-0.766972477,
-0.765137615,-0.763302752,-0.76146789,-0.759633028,-0.757798165,-0.755963303,
-0.75412844,-0.752293578,-0.750458716,-0.748623853,-0.746788991,-0.744954128,
-0.743119266,-0.741284404,-0.739449541,-0.737614679,-0.735779817,-0.733944954,
-0.732110092,-0.730275229,-0.728440367,-0.726605505,-0.724770642,-0.72293578,
-0.721100917,-0.719266055,-0.717431193,-0.71559633,-0.713761468,-0.711926606,
-0.710091743,-0.708256881,-0.706422018,-0.704587156,-0.702752294,-0.700917431,
-0.699082569,-0.697247706,-0.695412844,-0.693577982,-0.691743119,-0.689908257,
-0.688073394,-0.686238532,-0.68440367,-0.682568807,-0.680733945,-0.678899083,
-0.67706422,-0.675229358,-0.673394495,-0.671559633,-0.669724771,-0.667889908,
-0.666055046,-0.664220183,-0.662385321,-0.660550459,-0.658715596,-0.656880734,
-0.655045872,-0.653211009,-0.651376147,-0.649541284,-0.647706422,-0.64587156,
-0.644036697,-0.642201835,-0.640366972,-0.63853211,-0.636697248,-0.634862385,
-0.633027523,-0.631192661,-0.629357798,-0.627522936,-0.625688073,-0.623853211,
-0.622018349,-0.620183486,-0.618348624,-0.616513761,-0.614678899,-0.612844037,
-0.611009174,-0.609174312,-0.60733945,-0.605504587,-0.603669725,-0.601834862,
-0.6,-0.598165138,-0.596330275,-0.594495413,-0.59266055,-0.590825688,-0.588990826,
-0.587155963,-0.585321101,-0.583486239,-0.581651376,-0.579816514,-0.577981651,
-0.576146789,-0.574311927,-0.572477064,-0.570642202,-0.568807339,-0.566972477,
-0.565137615,-0.563302752,-0.56146789,-0.559633028,-0.557798165,-0.555963303,
-0.55412844,-0.552293578,-0.550458716,-0.548623853,-0.546788991,-0.544954128,
-0.543119266,-0.541284404,-0.539449541,-0.537614679,-0.535779817,-0.533944954,
-0.532110092,-0.530275229,-0.528440367,-0.526605505,-0.524770642,-0.52293578,
-0.521100917,-0.519266055,-0.517431193,-0.51559633,-0.513761468,-0.511926606,
-0.510091743,-0.508256881,-0.506422018,-0.504587156,-0.502752294,-0.500917431,
-0.499082569,-0.497247706,-0.495412844,-0.493577982,-0.491743119,-0.489908257,
-0.488073394,-0.486238532,-0.48440367,-0.482568807,-0.480733945,-0.478899083,
-0.47706422,-0.475229358,-0.473394495,-0.471559633,-0.469724771,-0.467889908,
-0.466055046,-0.464220183,-0.462385321,-0.460550459,-0.458715596,-0.456880734,
-0.455045872,-0.453211009,-0.451376147,-0.449541284,-0.447706422,-0.44587156,
-0.444036697,-0.442201835,-0.440366972,-0.43853211,-0.436697248,-0.434862385,
-0.433027523,-0.431192661,-0.429357798,-0.427522936,-0.425688073,-0.423853211,
-0.422018349,-0.420183486,-0.418348624,-0.416513761,-0.414678899,-0.412844037,
-0.411009174,-0.409174312,-0.40733945,-0.405504587,-0.403669725,-0.401834862,
-0.4,-0.398165138,-0.396330275,-0.394495413,-0.39266055,-0.390825688,-0.388990826,
-0.387155963,-0.385321101,-0.383486239,-0.381651376,-0.379816514,-0.377981651,
-0.376146789,-0.374311927,-0.372477064,-0.370642202,-0.368807339,-0.366972477,
-0.365137615,-0.363302752,-0.36146789,-0.359633028,-0.357798165,-0.355963303,
-0.35412844,-0.352293578,-0.350458716,-0.348623853,-0.346788991,-0.344954128,
-0.343119266,-0.341284404,-0.339449541,-0.337614679,-0.335779817,-0.333944954,
-0.332110092,-0.330275229,-0.328440367,-0.326605505,-0.324770642,-0.32293578,
-0.321100917,-0.319266055,-0.317431193,-0.31559633,-0.313761468,-0.311926606,
-0.310091743,-0.308256881,-0.306422018,-0.304587156,-0.302752294,-0.300917431,
-0.299082569,-0.297247706,-0.295412844,-0.293577982,-0.291743119,-0.289908257,
-0.288073394,-0.286238532,-0.28440367,-0.282568807,-0.280733945,-0.278899083,
-0.27706422,-0.275229358,-0.273394495,-0.271559633,-0.269724771,-0.267889908,
-0.266055046,-0.264220183,-0.262385321,-0.260550459,-0.258715596,-0.256880734,
-0.255045872,-0.253211009,-0.251376147,-0.249541284,-0.247706422,-0.24587156,
-0.244036697,-0.242201835,-0.240366972,-0.23853211,-0.236697248,-0.234862385,
-0.233027523,-0.231192661,-0.229357798,-0.227522936,-0.225688073,-0.223853211,
-0.222018349,-0.220183486,-0.218348624,-0.216513761,-0.214678899,-0.212844037,
-0.211009174,-0.209174312,-0.20733945,-0.205504587,-0.203669725,-0.201834862,
-0.2,-0.198165138,-0.196330275,-0.194495413,-0.19266055,-0.190825688,-0.188990826,
-0.187155963,-0.185321101,-0.183486239,-0.181651376,-0.179816514,-0.177981651,
-0.176146789,-0.174311927,-0.172477064,-0.170642202,-0.168807339,-0.166972477,
-0.165137615,-0.163302752,-0.16146789,-0.159633028,-0.157798165,-0.155963303,
-0.15412844,-0.152293578,-0.150458716,-0.148623853,-0.146788991,-0.144954128,
-0.143172103),(0.,0.36),.UNSPECIFIED.);
#6233=B_SPLINE_SURFACE_WITH_KNOTS('',5,1,((#184694,#184695),(#184696,#184697),
(#184698,#184699),(#184700,#184701),(#184702,#184703),(#184704,#184705),
(#184706,#184707),(#184708,#184709),(#184710,#184711),(#184712,#184713),
(#184714,#184715),(#184716,#184717),(#184718,#184719),(#184720,#184721),
(#184722,#184723),(#184724,#184725),(#184726,#184727),(#184728,#184729),
(#184730,#184731),(#184732,#184733),(#184734,#184735),(#184736,#184737),
(#184738,#184739),(#184740,#184741),(#184742,#184743),(#184744,#184745),
(#184746,#184747),(#184748,#184749),(#184750,#184751),(#184752,#184753),
(#184754,#184755),(#184756,#184757),(#184758,#184759),(#184760,#184761),
(#184762,#184763),(#184764,#184765),(#184766,#184767),(#184768,#184769),
(#184770,#184771),(#184772,#184773),(#184774,#184775),(#184776,#184777),
(#184778,#184779),(#184780,#184781),(#184782,#184783),(#184784,#184785),
(#184786,#184787),(#184788,#184789),(#184790,#184791),(#184792,#184793),
(#184794,#184795),(#184796,#184797),(#184798,#184799),(#184800,#184801),
(#184802,#184803),(#184804,#184805),(#184806,#184807),(#184808,#184809),
(#184810,#184811),(#184812,#184813),(#184814,#184815),(#184816,#184817),
(#184818,#184819),(#184820,#184821),(#184822,#184823),(#184824,#184825),
(#184826,#184827),(#184828,#184829),(#184830,#184831),(#184832,#184833),
(#184834,#184835),(#184836,#184837),(#184838,#184839),(#184840,#184841),
(#184842,#184843),(#184844,#184845),(#184846,#184847),(#184848,#184849),
(#184850,#184851),(#184852,#184853),(#184854,#184855),(#184856,#184857),
(#184858,#184859),(#184860,#184861),(#184862,#184863),(#184864,#184865),
(#184866,#184867),(#184868,#184869),(#184870,#184871),(#184872,#184873),
(#184874,#184875),(#184876,#184877),(#184878,#184879),(#184880,#184881),
(#184882,#184883),(#184884,#184885),(#184886,#184887),(#184888,#184889),
(#184890,#184891),(#184892,#184893),(#184894,#184895),(#184896,#184897),
(#184898,#184899),(#184900,#184901),(#184902,#184903),(#184904,#184905),
(#184906,#184907),(#184908,#184909),(#184910,#184911),(#184912,#184913),
(#184914,#184915),(#184916,#184917),(#184918,#184919),(#184920,#184921),
(#184922,#184923),(#184924,#184925),(#184926,#184927),(#184928,#184929),
(#184930,#184931),(#184932,#184933),(#184934,#184935),(#184936,#184937),
(#184938,#184939),(#184940,#184941),(#184942,#184943),(#184944,#184945),
(#184946,#184947),(#184948,#184949),(#184950,#184951),(#184952,#184953),
(#184954,#184955),(#184956,#184957),(#184958,#184959),(#184960,#184961),
(#184962,#184963),(#184964,#184965),(#184966,#184967),(#184968,#184969),
(#184970,#184971),(#184972,#184973),(#184974,#184975),(#184976,#184977),
(#184978,#184979),(#184980,#184981),(#184982,#184983),(#184984,#184985),
(#184986,#184987),(#184988,#184989),(#184990,#184991),(#184992,#184993),
(#184994,#184995),(#184996,#184997),(#184998,#184999),(#185000,#185001),
(#185002,#185003),(#185004,#185005),(#185006,#185007),(#185008,#185009),
(#185010,#185011),(#185012,#185013),(#185014,#185015),(#185016,#185017),
(#185018,#185019),(#185020,#185021),(#185022,#185023),(#185024,#185025),
(#185026,#185027),(#185028,#185029),(#185030,#185031),(#185032,#185033),
(#185034,#185035),(#185036,#185037),(#185038,#185039),(#185040,#185041),
(#185042,#185043),(#185044,#185045),(#185046,#185047),(#185048,#185049),
(#185050,#185051),(#185052,#185053),(#185054,#185055),(#185056,#185057),
(#185058,#185059),(#185060,#185061),(#185062,#185063),(#185064,#185065),
(#185066,#185067),(#185068,#185069),(#185070,#185071),(#185072,#185073),
(#185074,#185075),(#185076,#185077),(#185078,#185079),(#185080,#185081),
(#185082,#185083),(#185084,#185085),(#185086,#185087),(#185088,#185089),
(#185090,#185091),(#185092,#185093),(#185094,#185095),(#185096,#185097),
(#185098,#185099),(#185100,#185101),(#185102,#185103),(#185104,#185105),
(#185106,#185107),(#185108,#185109),(#185110,#185111),(#185112,#185113),
(#185114,#185115),(#185116,#185117),(#185118,#185119),(#185120,#185121),
(#185122,#185123),(#185124,#185125),(#185126,#185127),(#185128,#185129),
(#185130,#185131),(#185132,#185133),(#185134,#185135),(#185136,#185137),
(#185138,#185139),(#185140,#185141),(#185142,#185143),(#185144,#185145),
(#185146,#185147),(#185148,#185149),(#185150,#185151),(#185152,#185153),
(#185154,#185155),(#185156,#185157),(#185158,#185159),(#185160,#185161),
(#185162,#185163),(#185164,#185165),(#185166,#185167),(#185168,#185169),
(#185170,#185171),(#185172,#185173),(#185174,#185175),(#185176,#185177),
(#185178,#185179),(#185180,#185181),(#185182,#185183),(#185184,#185185),
(#185186,#185187),(#185188,#185189),(#185190,#185191),(#185192,#185193),
(#185194,#185195),(#185196,#185197),(#185198,#185199),(#185200,#185201),
(#185202,#185203),(#185204,#185205),(#185206,#185207),(#185208,#185209),
(#185210,#185211),(#185212,#185213),(#185214,#185215),(#185216,#185217),
(#185218,#185219),(#185220,#185221),(#185222,#185223),(#185224,#185225),
(#185226,#185227),(#185228,#185229),(#185230,#185231),(#185232,#185233),
(#185234,#185235),(#185236,#185237),(#185238,#185239),(#185240,#185241),
(#185242,#185243),(#185244,#185245),(#185246,#185247),(#185248,#185249),
(#185250,#185251),(#185252,#185253),(#185254,#185255),(#185256,#185257),
(#185258,#185259),(#185260,#185261),(#185262,#185263),(#185264,#185265),
(#185266,#185267),(#185268,#185269),(#185270,#185271),(#185272,#185273),
(#185274,#185275),(#185276,#185277),(#185278,#185279),(#185280,#185281),
(#185282,#185283),(#185284,#185285),(#185286,#185287),(#185288,#185289),
(#185290,#185291),(#185292,#185293),(#185294,#185295),(#185296,#185297),
(#185298,#185299),(#185300,#185301),(#185302,#185303),(#185304,#185305),
(#185306,#185307),(#185308,#185309),(#185310,#185311),(#185312,#185313),
(#185314,#185315),(#185316,#185317),(#185318,#185319),(#185320,#185321),
(#185322,#185323),(#185324,#185325),(#185326,#185327),(#185328,#185329),
(#185330,#185331),(#185332,#185333),(#185334,#185335),(#185336,#185337),
(#185338,#185339),(#185340,#185341),(#185342,#185343),(#185344,#185345),
(#185346,#185347),(#185348,#185349),(#185350,#185351),(#185352,#185353),
(#185354,#185355),(#185356,#185357),(#185358,#185359),(#185360,#185361),
(#185362,#185363),(#185364,#185365),(#185366,#185367),(#185368,#185369),
(#185370,#185371),(#185372,#185373),(#185374,#185375),(#185376,#185377),
(#185378,#185379),(#185380,#185381),(#185382,#185383),(#185384,#185385),
(#185386,#185387),(#185388,#185389),(#185390,#185391),(#185392,#185393),
(#185394,#185395),(#185396,#185397),(#185398,#185399),(#185400,#185401),
(#185402,#185403),(#185404,#185405),(#185406,#185407),(#185408,#185409),
(#185410,#185411),(#185412,#185413),(#185414,#185415),(#185416,#185417),
(#185418,#185419),(#185420,#185421),(#185422,#185423),(#185424,#185425),
(#185426,#185427),(#185428,#185429),(#185430,#185431),(#185432,#185433),
(#185434,#185435),(#185436,#185437),(#185438,#185439),(#185440,#185441),
(#185442,#185443),(#185444,#185445),(#185446,#185447),(#185448,#185449),
(#185450,#185451),(#185452,#185453),(#185454,#185455),(#185456,#185457),
(#185458,#185459),(#185460,#185461),(#185462,#185463),(#185464,#185465),
(#185466,#185467),(#185468,#185469),(#185470,#185471),(#185472,#185473),
(#185474,#185475),(#185476,#185477),(#185478,#185479),(#185480,#185481),
(#185482,#185483),(#185484,#185485),(#185486,#185487),(#185488,#185489),
(#185490,#185491),(#185492,#185493),(#185494,#185495),(#185496,#185497),
(#185498,#185499),(#185500,#185501),(#185502,#185503),(#185504,#185505),
(#185506,#185507),(#185508,#185509),(#185510,#185511),(#185512,#185513),
(#185514,#185515),(#185516,#185517),(#185518,#185519),(#185520,#185521),
(#185522,#185523),(#185524,#185525),(#185526,#185527),(#185528,#185529),
(#185530,#185531),(#185532,#185533),(#185534,#185535),(#185536,#185537),
(#185538,#185539),(#185540,#185541),(#185542,#185543),(#185544,#185545),
(#185546,#185547),(#185548,#185549),(#185550,#185551),(#185552,#185553),
(#185554,#185555),(#185556,#185557),(#185558,#185559),(#185560,#185561),
(#185562,#185563),(#185564,#185565),(#185566,#185567),(#185568,#185569),
(#185570,#185571),(#185572,#185573),(#185574,#185575),(#185576,#185577),
(#185578,#185579),(#185580,#185581),(#185582,#185583),(#185584,#185585),
(#185586,#185587),(#185588,#185589),(#185590,#185591),(#185592,#185593),
(#185594,#185595),(#185596,#185597),(#185598,#185599),(#185600,#185601),
(#185602,#185603),(#185604,#185605),(#185606,#185607),(#185608,#185609),
(#185610,#185611),(#185612,#185613),(#185614,#185615),(#185616,#185617),
(#185618,#185619),(#185620,#185621),(#185622,#185623),(#185624,#185625),
(#185626,#185627),(#185628,#185629),(#185630,#185631),(#185632,#185633),
(#185634,#185635),(#185636,#185637)),.UNSPECIFIED.,.F.,.F.,.F.,(6,1,1,1,
1,1,1,1,1,1,1,1,1,1,1,1,1,1,1,1,1,1,1,1,1,1,1,1,1,1,1,1,1,1,1,1,1,1,1,1,
1,1,1,1,1,1,1,1,1,1,1,1,1,1,1,1,1,1,1,1,1,1,1,1,1,1,1,1,1,1,1,1,1,1,1,1,
1,1,1,1,1,1,1,1,1,1,1,1,1,1,1,1,1,1,1,1,1,1,1,1,1,1,1,1,1,1,1,1,1,1,1,1,
1,1,1,1,1,1,1,1,1,1,1,1,1,1,1,1,1,1,1,1,1,1,1,1,1,1,1,1,1,1,1,1,1,1,1,1,
1,1,1,1,1,1,1,1,1,1,1,1,1,1,1,1,1,1,1,1,1,1,1,1,1,1,1,1,1,1,1,1,1,1,1,1,
1,1,1,1,1,1,1,1,1,1,1,1,1,1,1,1,1,1,1,1,1,1,1,1,1,1,1,1,1,1,1,1,1,1,1,1,
1,1,1,1,1,1,1,1,1,1,1,1,1,1,1,1,1,1,1,1,1,1,1,1,1,1,1,1,1,1,1,1,1,1,1,1,
1,1,1,1,1,1,1,1,1,1,1,1,1,1,1,1,1,1,1,1,1,1,1,1,1,1,1,1,1,1,1,1,1,1,1,1,
1,1,1,1,1,1,1,1,1,1,1,1,1,1,1,1,1,1,1,1,1,1,1,1,1,1,1,1,1,1,1,1,1,1,1,1,
1,1,1,1,1,1,1,1,1,1,1,1,1,1,1,1,1,1,1,1,1,1,1,1,1,1,1,1,1,1,1,1,1,1,1,1,
1,1,1,1,1,1,1,1,1,1,1,1,1,1,1,1,1,1,1,1,1,1,1,1,1,1,1,1,1,1,1,1,1,1,1,1,
1,1,1,1,1,1,1,1,1,1,1,1,1,1,1,1,1,1,1,1,1,1,1,1,1,1,1,1,1,1,1,1,1,1,1,1,
1,1,1,1,1,1,1,1,1,1,1,1,1,1,1,1,1,1,1,1,1,1,1,1,1,1,1,1,1,1,1,6),(2,2),
(-1.,-0.998165138,-0.996330275,-0.994495413,-0.99266055,-0.990825688,-0.988990826,
-0.987155963,-0.985321101,-0.983486239,-0.981651376,-0.979816514,-0.977981651,
-0.976146789,-0.974311927,-0.972477064,-0.970642202,-0.968807339,-0.966972477,
-0.965137615,-0.963302752,-0.96146789,-0.959633028,-0.957798165,-0.955963303,
-0.95412844,-0.952293578,-0.950458716,-0.948623853,-0.946788991,-0.944954128,
-0.943119266,-0.941284404,-0.939449541,-0.937614679,-0.935779817,-0.933944954,
-0.932110092,-0.930275229,-0.928440367,-0.926605505,-0.924770642,-0.92293578,
-0.921100917,-0.919266055,-0.917431193,-0.91559633,-0.913761468,-0.911926606,
-0.910091743,-0.908256881,-0.906422018,-0.904587156,-0.902752294,-0.900917431,
-0.899082569,-0.897247706,-0.895412844,-0.893577982,-0.891743119,-0.889908257,
-0.888073394,-0.886238532,-0.88440367,-0.882568807,-0.880733945,-0.878899083,
-0.87706422,-0.875229358,-0.873394495,-0.871559633,-0.869724771,-0.867889908,
-0.866055046,-0.864220183,-0.862385321,-0.860550459,-0.858715596,-0.856880734,
-0.855045872,-0.853211009,-0.851376147,-0.849541284,-0.847706422,-0.84587156,
-0.844036697,-0.842201835,-0.840366972,-0.83853211,-0.836697248,-0.834862385,
-0.833027523,-0.831192661,-0.829357798,-0.827522936,-0.825688073,-0.823853211,
-0.822018349,-0.820183486,-0.818348624,-0.816513761,-0.814678899,-0.812844037,
-0.811009174,-0.809174312,-0.80733945,-0.805504587,-0.803669725,-0.801834862,
-0.8,-0.798165138,-0.796330275,-0.794495413,-0.79266055,-0.790825688,-0.788990826,
-0.787155963,-0.785321101,-0.783486239,-0.781651376,-0.779816514,-0.777981651,
-0.776146789,-0.774311927,-0.772477064,-0.770642202,-0.768807339,-0.766972477,
-0.765137615,-0.763302752,-0.76146789,-0.759633028,-0.757798165,-0.755963303,
-0.75412844,-0.752293578,-0.750458716,-0.748623853,-0.746788991,-0.744954128,
-0.743119266,-0.741284404,-0.739449541,-0.737614679,-0.735779817,-0.733944954,
-0.732110092,-0.730275229,-0.728440367,-0.726605505,-0.724770642,-0.72293578,
-0.721100917,-0.719266055,-0.717431193,-0.71559633,-0.713761468,-0.711926606,
-0.710091743,-0.708256881,-0.706422018,-0.704587156,-0.702752294,-0.700917431,
-0.699082569,-0.697247706,-0.695412844,-0.693577982,-0.691743119,-0.689908257,
-0.688073394,-0.686238532,-0.68440367,-0.682568807,-0.680733945,-0.678899083,
-0.67706422,-0.675229358,-0.673394495,-0.671559633,-0.669724771,-0.667889908,
-0.666055046,-0.664220183,-0.662385321,-0.660550459,-0.658715596,-0.656880734,
-0.655045872,-0.653211009,-0.651376147,-0.649541284,-0.647706422,-0.64587156,
-0.644036697,-0.642201835,-0.640366972,-0.63853211,-0.636697248,-0.634862385,
-0.633027523,-0.631192661,-0.629357798,-0.627522936,-0.625688073,-0.623853211,
-0.622018349,-0.620183486,-0.618348624,-0.616513761,-0.614678899,-0.612844037,
-0.611009174,-0.609174312,-0.60733945,-0.605504587,-0.603669725,-0.601834862,
-0.6,-0.598165138,-0.596330275,-0.594495413,-0.59266055,-0.590825688,-0.588990826,
-0.587155963,-0.585321101,-0.583486239,-0.581651376,-0.579816514,-0.577981651,
-0.576146789,-0.574311927,-0.572477064,-0.570642202,-0.568807339,-0.566972477,
-0.565137615,-0.563302752,-0.56146789,-0.559633028,-0.557798165,-0.555963303,
-0.55412844,-0.552293578,-0.550458716,-0.548623853,-0.546788991,-0.544954128,
-0.543119266,-0.541284404,-0.539449541,-0.537614679,-0.535779817,-0.533944954,
-0.532110092,-0.530275229,-0.528440367,-0.526605505,-0.524770642,-0.52293578,
-0.521100917,-0.519266055,-0.517431193,-0.51559633,-0.513761468,-0.511926606,
-0.510091743,-0.508256881,-0.506422018,-0.504587156,-0.502752294,-0.500917431,
-0.499082569,-0.497247706,-0.495412844,-0.493577982,-0.491743119,-0.489908257,
-0.488073394,-0.486238532,-0.48440367,-0.482568807,-0.480733945,-0.478899083,
-0.47706422,-0.475229358,-0.473394495,-0.471559633,-0.469724771,-0.467889908,
-0.466055046,-0.464220183,-0.462385321,-0.460550459,-0.458715596,-0.456880734,
-0.455045872,-0.453211009,-0.451376147,-0.449541284,-0.447706422,-0.44587156,
-0.444036697,-0.442201835,-0.440366972,-0.43853211,-0.436697248,-0.434862385,
-0.433027523,-0.431192661,-0.429357798,-0.427522936,-0.425688073,-0.423853211,
-0.422018349,-0.420183486,-0.418348624,-0.416513761,-0.414678899,-0.412844037,
-0.411009174,-0.409174312,-0.40733945,-0.405504587,-0.403669725,-0.401834862,
-0.4,-0.398165138,-0.396330275,-0.394495413,-0.39266055,-0.390825688,-0.388990826,
-0.387155963,-0.385321101,-0.383486239,-0.381651376,-0.379816514,-0.377981651,
-0.376146789,-0.374311927,-0.372477064,-0.370642202,-0.368807339,-0.366972477,
-0.365137615,-0.363302752,-0.36146789,-0.359633028,-0.357798165,-0.355963303,
-0.35412844,-0.352293578,-0.350458716,-0.348623853,-0.346788991,-0.344954128,
-0.343119266,-0.341284404,-0.339449541,-0.337614679,-0.335779817,-0.333944954,
-0.332110092,-0.330275229,-0.328440367,-0.326605505,-0.324770642,-0.32293578,
-0.321100917,-0.319266055,-0.317431193,-0.31559633,-0.313761468,-0.311926606,
-0.310091743,-0.308256881,-0.306422018,-0.304587156,-0.302752294,-0.300917431,
-0.299082569,-0.297247706,-0.295412844,-0.293577982,-0.291743119,-0.289908257,
-0.288073394,-0.286238532,-0.28440367,-0.282568807,-0.280733945,-0.278899083,
-0.27706422,-0.275229358,-0.273394495,-0.271559633,-0.269724771,-0.267889908,
-0.266055046,-0.264220183,-0.262385321,-0.260550459,-0.258715596,-0.256880734,
-0.255045872,-0.253211009,-0.251376147,-0.249541284,-0.247706422,-0.24587156,
-0.244036697,-0.242201835,-0.240366972,-0.23853211,-0.236697248,-0.234862385,
-0.233027523,-0.231192661,-0.229357798,-0.227522936,-0.225688073,-0.223853211,
-0.222018349,-0.220183486,-0.218348624,-0.216513761,-0.214678899,-0.212844037,
-0.211009174,-0.209174312,-0.20733945,-0.205504587,-0.203669725,-0.201834862,
-0.2,-0.198165138,-0.196330275,-0.194495413,-0.19266055,-0.190825688,-0.188990826,
-0.187155963,-0.185321101,-0.183486239,-0.181651376,-0.179816514,-0.177981651,
-0.176146789,-0.174311927,-0.172477064,-0.170642202,-0.168807339,-0.166972477,
-0.165137615,-0.163302752,-0.16146789,-0.159633028,-0.157798165,-0.155963303,
-0.15412844,-0.152293578,-0.150458716,-0.148623853,-0.146788991,-0.144954128,
-0.143172103),(0.,0.36),.UNSPECIFIED.);
#6234=B_SPLINE_SURFACE_WITH_KNOTS('',5,1,((#186279,#186280),(#186281,#186282),
(#186283,#186284),(#186285,#186286),(#186287,#186288),(#186289,#186290),
(#186291,#186292),(#186293,#186294),(#186295,#186296),(#186297,#186298),
(#186299,#186300),(#186301,#186302),(#186303,#186304),(#186305,#186306),
(#186307,#186308),(#186309,#186310),(#186311,#186312),(#186313,#186314),
(#186315,#186316),(#186317,#186318),(#186319,#186320),(#186321,#186322),
(#186323,#186324),(#186325,#186326),(#186327,#186328),(#186329,#186330),
(#186331,#186332),(#186333,#186334),(#186335,#186336),(#186337,#186338),
(#186339,#186340),(#186341,#186342),(#186343,#186344),(#186345,#186346),
(#186347,#186348),(#186349,#186350),(#186351,#186352),(#186353,#186354),
(#186355,#186356),(#186357,#186358),(#186359,#186360),(#186361,#186362),
(#186363,#186364),(#186365,#186366),(#186367,#186368),(#186369,#186370),
(#186371,#186372),(#186373,#186374),(#186375,#186376),(#186377,#186378),
(#186379,#186380),(#186381,#186382),(#186383,#186384),(#186385,#186386),
(#186387,#186388),(#186389,#186390),(#186391,#186392),(#186393,#186394),
(#186395,#186396),(#186397,#186398),(#186399,#186400),(#186401,#186402),
(#186403,#186404),(#186405,#186406),(#186407,#186408),(#186409,#186410),
(#186411,#186412),(#186413,#186414),(#186415,#186416),(#186417,#186418),
(#186419,#186420),(#186421,#186422),(#186423,#186424),(#186425,#186426),
(#186427,#186428),(#186429,#186430),(#186431,#186432),(#186433,#186434),
(#186435,#186436),(#186437,#186438),(#186439,#186440),(#186441,#186442),
(#186443,#186444),(#186445,#186446),(#186447,#186448),(#186449,#186450),
(#186451,#186452),(#186453,#186454),(#186455,#186456),(#186457,#186458),
(#186459,#186460),(#186461,#186462),(#186463,#186464),(#186465,#186466),
(#186467,#186468),(#186469,#186470),(#186471,#186472),(#186473,#186474),
(#186475,#186476),(#186477,#186478),(#186479,#186480),(#186481,#186482),
(#186483,#186484),(#186485,#186486),(#186487,#186488),(#186489,#186490),
(#186491,#186492),(#186493,#186494),(#186495,#186496),(#186497,#186498),
(#186499,#186500),(#186501,#186502),(#186503,#186504),(#186505,#186506),
(#186507,#186508),(#186509,#186510),(#186511,#186512),(#186513,#186514),
(#186515,#186516),(#186517,#186518),(#186519,#186520),(#186521,#186522),
(#186523,#186524),(#186525,#186526),(#186527,#186528),(#186529,#186530),
(#186531,#186532),(#186533,#186534),(#186535,#186536),(#186537,#186538),
(#186539,#186540),(#186541,#186542),(#186543,#186544),(#186545,#186546),
(#186547,#186548),(#186549,#186550),(#186551,#186552),(#186553,#186554),
(#186555,#186556),(#186557,#186558),(#186559,#186560),(#186561,#186562),
(#186563,#186564),(#186565,#186566),(#186567,#186568),(#186569,#186570),
(#186571,#186572),(#186573,#186574),(#186575,#186576),(#186577,#186578),
(#186579,#186580),(#186581,#186582),(#186583,#186584),(#186585,#186586),
(#186587,#186588),(#186589,#186590),(#186591,#186592),(#186593,#186594),
(#186595,#186596),(#186597,#186598),(#186599,#186600),(#186601,#186602),
(#186603,#186604),(#186605,#186606),(#186607,#186608),(#186609,#186610),
(#186611,#186612),(#186613,#186614),(#186615,#186616),(#186617,#186618),
(#186619,#186620),(#186621,#186622),(#186623,#186624),(#186625,#186626),
(#186627,#186628),(#186629,#186630),(#186631,#186632),(#186633,#186634),
(#186635,#186636),(#186637,#186638),(#186639,#186640),(#186641,#186642),
(#186643,#186644),(#186645,#186646),(#186647,#186648),(#186649,#186650),
(#186651,#186652),(#186653,#186654),(#186655,#186656),(#186657,#186658),
(#186659,#186660),(#186661,#186662),(#186663,#186664),(#186665,#186666),
(#186667,#186668),(#186669,#186670),(#186671,#186672),(#186673,#186674),
(#186675,#186676),(#186677,#186678),(#186679,#186680),(#186681,#186682),
(#186683,#186684),(#186685,#186686),(#186687,#186688),(#186689,#186690),
(#186691,#186692),(#186693,#186694),(#186695,#186696),(#186697,#186698),
(#186699,#186700),(#186701,#186702),(#186703,#186704),(#186705,#186706),
(#186707,#186708),(#186709,#186710),(#186711,#186712),(#186713,#186714),
(#186715,#186716),(#186717,#186718),(#186719,#186720),(#186721,#186722),
(#186723,#186724),(#186725,#186726),(#186727,#186728),(#186729,#186730),
(#186731,#186732),(#186733,#186734),(#186735,#186736),(#186737,#186738),
(#186739,#186740),(#186741,#186742),(#186743,#186744),(#186745,#186746),
(#186747,#186748),(#186749,#186750),(#186751,#186752),(#186753,#186754),
(#186755,#186756),(#186757,#186758),(#186759,#186760),(#186761,#186762),
(#186763,#186764),(#186765,#186766),(#186767,#186768),(#186769,#186770),
(#186771,#186772),(#186773,#186774),(#186775,#186776),(#186777,#186778),
(#186779,#186780),(#186781,#186782),(#186783,#186784),(#186785,#186786),
(#186787,#186788),(#186789,#186790),(#186791,#186792),(#186793,#186794),
(#186795,#186796),(#186797,#186798),(#186799,#186800),(#186801,#186802),
(#186803,#186804),(#186805,#186806),(#186807,#186808),(#186809,#186810),
(#186811,#186812),(#186813,#186814),(#186815,#186816),(#186817,#186818),
(#186819,#186820),(#186821,#186822),(#186823,#186824),(#186825,#186826),
(#186827,#186828),(#186829,#186830),(#186831,#186832),(#186833,#186834),
(#186835,#186836),(#186837,#186838),(#186839,#186840),(#186841,#186842),
(#186843,#186844),(#186845,#186846),(#186847,#186848),(#186849,#186850),
(#186851,#186852),(#186853,#186854),(#186855,#186856),(#186857,#186858),
(#186859,#186860),(#186861,#186862),(#186863,#186864),(#186865,#186866),
(#186867,#186868),(#186869,#186870),(#186871,#186872),(#186873,#186874),
(#186875,#186876),(#186877,#186878),(#186879,#186880),(#186881,#186882),
(#186883,#186884),(#186885,#186886),(#186887,#186888),(#186889,#186890),
(#186891,#186892),(#186893,#186894),(#186895,#186896),(#186897,#186898),
(#186899,#186900),(#186901,#186902),(#186903,#186904),(#186905,#186906),
(#186907,#186908),(#186909,#186910),(#186911,#186912),(#186913,#186914),
(#186915,#186916),(#186917,#186918),(#186919,#186920),(#186921,#186922),
(#186923,#186924),(#186925,#186926),(#186927,#186928),(#186929,#186930),
(#186931,#186932),(#186933,#186934),(#186935,#186936),(#186937,#186938),
(#186939,#186940),(#186941,#186942),(#186943,#186944),(#186945,#186946),
(#186947,#186948),(#186949,#186950),(#186951,#186952),(#186953,#186954),
(#186955,#186956),(#186957,#186958),(#186959,#186960),(#186961,#186962),
(#186963,#186964),(#186965,#186966),(#186967,#186968),(#186969,#186970),
(#186971,#186972),(#186973,#186974),(#186975,#186976),(#186977,#186978),
(#186979,#186980),(#186981,#186982),(#186983,#186984),(#186985,#186986),
(#186987,#186988),(#186989,#186990),(#186991,#186992),(#186993,#186994),
(#186995,#186996),(#186997,#186998),(#186999,#187000),(#187001,#187002),
(#187003,#187004),(#187005,#187006),(#187007,#187008),(#187009,#187010),
(#187011,#187012),(#187013,#187014),(#187015,#187016),(#187017,#187018),
(#187019,#187020),(#187021,#187022),(#187023,#187024),(#187025,#187026),
(#187027,#187028),(#187029,#187030),(#187031,#187032),(#187033,#187034),
(#187035,#187036),(#187037,#187038),(#187039,#187040),(#187041,#187042),
(#187043,#187044),(#187045,#187046),(#187047,#187048),(#187049,#187050),
(#187051,#187052),(#187053,#187054),(#187055,#187056),(#187057,#187058),
(#187059,#187060),(#187061,#187062),(#187063,#187064),(#187065,#187066),
(#187067,#187068),(#187069,#187070),(#187071,#187072),(#187073,#187074),
(#187075,#187076),(#187077,#187078),(#187079,#187080),(#187081,#187082),
(#187083,#187084),(#187085,#187086),(#187087,#187088),(#187089,#187090),
(#187091,#187092),(#187093,#187094),(#187095,#187096),(#187097,#187098),
(#187099,#187100),(#187101,#187102),(#187103,#187104),(#187105,#187106),
(#187107,#187108),(#187109,#187110),(#187111,#187112),(#187113,#187114),
(#187115,#187116),(#187117,#187118),(#187119,#187120),(#187121,#187122),
(#187123,#187124),(#187125,#187126),(#187127,#187128),(#187129,#187130),
(#187131,#187132),(#187133,#187134),(#187135,#187136),(#187137,#187138),
(#187139,#187140),(#187141,#187142),(#187143,#187144),(#187145,#187146),
(#187147,#187148),(#187149,#187150),(#187151,#187152),(#187153,#187154),
(#187155,#187156),(#187157,#187158),(#187159,#187160),(#187161,#187162),
(#187163,#187164),(#187165,#187166),(#187167,#187168),(#187169,#187170),
(#187171,#187172),(#187173,#187174),(#187175,#187176),(#187177,#187178),
(#187179,#187180),(#187181,#187182),(#187183,#187184),(#187185,#187186),
(#187187,#187188),(#187189,#187190),(#187191,#187192),(#187193,#187194),
(#187195,#187196),(#187197,#187198),(#187199,#187200),(#187201,#187202),
(#187203,#187204),(#187205,#187206),(#187207,#187208),(#187209,#187210),
(#187211,#187212),(#187213,#187214),(#187215,#187216),(#187217,#187218),
(#187219,#187220),(#187221,#187222)),.UNSPECIFIED.,.F.,.F.,.F.,(6,1,1,1,
1,1,1,1,1,1,1,1,1,1,1,1,1,1,1,1,1,1,1,1,1,1,1,1,1,1,1,1,1,1,1,1,1,1,1,1,
1,1,1,1,1,1,1,1,1,1,1,1,1,1,1,1,1,1,1,1,1,1,1,1,1,1,1,1,1,1,1,1,1,1,1,1,
1,1,1,1,1,1,1,1,1,1,1,1,1,1,1,1,1,1,1,1,1,1,1,1,1,1,1,1,1,1,1,1,1,1,1,1,
1,1,1,1,1,1,1,1,1,1,1,1,1,1,1,1,1,1,1,1,1,1,1,1,1,1,1,1,1,1,1,1,1,1,1,1,
1,1,1,1,1,1,1,1,1,1,1,1,1,1,1,1,1,1,1,1,1,1,1,1,1,1,1,1,1,1,1,1,1,1,1,1,
1,1,1,1,1,1,1,1,1,1,1,1,1,1,1,1,1,1,1,1,1,1,1,1,1,1,1,1,1,1,1,1,1,1,1,1,
1,1,1,1,1,1,1,1,1,1,1,1,1,1,1,1,1,1,1,1,1,1,1,1,1,1,1,1,1,1,1,1,1,1,1,1,
1,1,1,1,1,1,1,1,1,1,1,1,1,1,1,1,1,1,1,1,1,1,1,1,1,1,1,1,1,1,1,1,1,1,1,1,
1,1,1,1,1,1,1,1,1,1,1,1,1,1,1,1,1,1,1,1,1,1,1,1,1,1,1,1,1,1,1,1,1,1,1,1,
1,1,1,1,1,1,1,1,1,1,1,1,1,1,1,1,1,1,1,1,1,1,1,1,1,1,1,1,1,1,1,1,1,1,1,1,
1,1,1,1,1,1,1,1,1,1,1,1,1,1,1,1,1,1,1,1,1,1,1,1,1,1,1,1,1,1,1,1,1,1,1,1,
1,1,1,1,1,1,1,1,1,1,1,1,1,1,1,1,1,1,1,1,1,1,1,1,1,1,1,1,1,1,1,1,1,1,1,1,
1,1,1,1,1,1,1,1,1,1,1,1,1,1,1,1,1,1,1,1,1,1,1,1,1,1,1,1,1,1,1,6),(2,2),
(0.143172103,0.144954128,0.146788991,0.148623853,0.150458716,0.152293578,
0.15412844,0.155963303,0.157798165,0.159633028,0.16146789,0.163302752,0.165137615,
0.166972477,0.168807339,0.170642202,0.172477064,0.174311927,0.176146789,
0.177981651,0.179816514,0.181651376,0.183486239,0.185321101,0.187155963,
0.188990826,0.190825688,0.19266055,0.194495413,0.196330275,0.198165138,
0.2,0.201834862,0.203669725,0.205504587,0.20733945,0.209174312,0.211009174,
0.212844037,0.214678899,0.216513761,0.218348624,0.220183486,0.222018349,
0.223853211,0.225688073,0.227522936,0.229357798,0.231192661,0.233027523,
0.234862385,0.236697248,0.23853211,0.240366972,0.242201835,0.244036697,
0.24587156,0.247706422,0.249541284,0.251376147,0.253211009,0.255045872,
0.256880734,0.258715596,0.260550459,0.262385321,0.264220183,0.266055046,
0.267889908,0.269724771,0.271559633,0.273394495,0.275229358,0.27706422,
0.278899083,0.280733945,0.282568807,0.28440367,0.286238532,0.288073394,
0.289908257,0.291743119,0.293577982,0.295412844,0.297247706,0.299082569,
0.300917431,0.302752294,0.304587156,0.306422018,0.308256881,0.310091743,
0.311926606,0.313761468,0.31559633,0.317431193,0.319266055,0.321100917,
0.32293578,0.324770642,0.326605505,0.328440367,0.330275229,0.332110092,
0.333944954,0.335779817,0.337614679,0.339449541,0.341284404,0.343119266,
0.344954128,0.346788991,0.348623853,0.350458716,0.352293578,0.35412844,
0.355963303,0.357798165,0.359633028,0.36146789,0.363302752,0.365137615,
0.366972477,0.368807339,0.370642202,0.372477064,0.374311927,0.376146789,
0.377981651,0.379816514,0.381651376,0.383486239,0.385321101,0.387155963,
0.388990826,0.390825688,0.39266055,0.394495413,0.396330275,0.398165138,
0.4,0.401834862,0.403669725,0.405504587,0.40733945,0.409174312,0.411009174,
0.412844037,0.414678899,0.416513761,0.418348624,0.420183486,0.422018349,
0.423853211,0.425688073,0.427522936,0.429357798,0.431192661,0.433027523,
0.434862385,0.436697248,0.43853211,0.440366972,0.442201835,0.444036697,
0.44587156,0.447706422,0.449541284,0.451376147,0.453211009,0.455045872,
0.456880734,0.458715596,0.460550459,0.462385321,0.464220183,0.466055046,
0.467889908,0.469724771,0.471559633,0.473394495,0.475229358,0.47706422,
0.478899083,0.480733945,0.482568807,0.48440367,0.486238532,0.488073394,
0.489908257,0.491743119,0.493577982,0.495412844,0.497247706,0.499082569,
0.500917431,0.502752294,0.504587156,0.506422018,0.508256881,0.510091743,
0.511926606,0.513761468,0.51559633,0.517431193,0.519266055,0.521100917,
0.52293578,0.524770642,0.526605505,0.528440367,0.530275229,0.532110092,
0.533944954,0.535779817,0.537614679,0.539449541,0.541284404,0.543119266,
0.544954128,0.546788991,0.548623853,0.550458716,0.552293578,0.55412844,
0.555963303,0.557798165,0.559633028,0.56146789,0.563302752,0.565137615,
0.566972477,0.568807339,0.570642202,0.572477064,0.574311927,0.576146789,
0.577981651,0.579816514,0.581651376,0.583486239,0.585321101,0.587155963,
0.588990826,0.590825688,0.59266055,0.594495413,0.596330275,0.598165138,
0.6,0.601834862,0.603669725,0.605504587,0.60733945,0.609174312,0.611009174,
0.612844037,0.614678899,0.616513761,0.618348624,0.620183486,0.622018349,
0.623853211,0.625688073,0.627522936,0.629357798,0.631192661,0.633027523,
0.634862385,0.636697248,0.63853211,0.640366972,0.642201835,0.644036697,
0.64587156,0.647706422,0.649541284,0.651376147,0.653211009,0.655045872,
0.656880734,0.658715596,0.660550459,0.662385321,0.664220183,0.666055046,
0.667889908,0.669724771,0.671559633,0.673394495,0.675229358,0.67706422,
0.678899083,0.680733945,0.682568807,0.68440367,0.686238532,0.688073394,
0.689908257,0.691743119,0.693577982,0.695412844,0.697247706,0.699082569,
0.700917431,0.702752294,0.704587156,0.706422018,0.708256881,0.710091743,
0.711926606,0.713761468,0.71559633,0.717431193,0.719266055,0.721100917,
0.72293578,0.724770642,0.726605505,0.728440367,0.730275229,0.732110092,
0.733944954,0.735779817,0.737614679,0.739449541,0.741284404,0.743119266,
0.744954128,0.746788991,0.748623853,0.750458716,0.752293578,0.75412844,
0.755963303,0.757798165,0.759633028,0.76146789,0.763302752,0.765137615,
0.766972477,0.768807339,0.770642202,0.772477064,0.774311927,0.776146789,
0.777981651,0.779816514,0.781651376,0.783486239,0.785321101,0.787155963,
0.788990826,0.790825688,0.79266055,0.794495413,0.796330275,0.798165138,
0.8,0.801834862,0.803669725,0.805504587,0.80733945,0.809174312,0.811009174,
0.812844037,0.814678899,0.816513761,0.818348624,0.820183486,0.822018349,
0.823853211,0.825688073,0.827522936,0.829357798,0.831192661,0.833027523,
0.834862385,0.836697248,0.83853211,0.840366972,0.842201835,0.844036697,
0.84587156,0.847706422,0.849541284,0.851376147,0.853211009,0.855045872,
0.856880734,0.858715596,0.860550459,0.862385321,0.864220183,0.866055046,
0.867889908,0.869724771,0.871559633,0.873394495,0.875229358,0.87706422,
0.878899083,0.880733945,0.882568807,0.88440367,0.886238532,0.888073394,
0.889908257,0.891743119,0.893577982,0.895412844,0.897247706,0.899082569,
0.900917431,0.902752294,0.904587156,0.906422018,0.908256881,0.910091743,
0.911926606,0.913761468,0.91559633,0.917431193,0.919266055,0.921100917,
0.92293578,0.924770642,0.926605505,0.928440367,0.930275229,0.932110092,
0.933944954,0.935779817,0.937614679,0.939449541,0.941284404,0.943119266,
0.944954128,0.946788991,0.948623853,0.950458716,0.952293578,0.95412844,
0.955963303,0.957798165,0.959633028,0.96146789,0.963302752,0.965137615,
0.966972477,0.968807339,0.970642202,0.972477064,0.974311927,0.976146789,
0.977981651,0.979816514,0.981651376,0.983486239,0.985321101,0.987155963,
0.988990826,0.990825688,0.99266055,0.994495413,0.996330275,0.998165138,
1.),(0.,0.36),.UNSPECIFIED.);
#6235=B_SPLINE_SURFACE_WITH_KNOTS('',5,1,((#187882,#187883),(#187884,#187885),
(#187886,#187887),(#187888,#187889),(#187890,#187891),(#187892,#187893),
(#187894,#187895),(#187896,#187897),(#187898,#187899),(#187900,#187901),
(#187902,#187903),(#187904,#187905),(#187906,#187907),(#187908,#187909),
(#187910,#187911),(#187912,#187913),(#187914,#187915),(#187916,#187917),
(#187918,#187919),(#187920,#187921),(#187922,#187923),(#187924,#187925),
(#187926,#187927),(#187928,#187929),(#187930,#187931),(#187932,#187933),
(#187934,#187935),(#187936,#187937),(#187938,#187939),(#187940,#187941),
(#187942,#187943),(#187944,#187945),(#187946,#187947),(#187948,#187949),
(#187950,#187951),(#187952,#187953),(#187954,#187955),(#187956,#187957),
(#187958,#187959),(#187960,#187961),(#187962,#187963),(#187964,#187965),
(#187966,#187967),(#187968,#187969),(#187970,#187971),(#187972,#187973),
(#187974,#187975),(#187976,#187977),(#187978,#187979),(#187980,#187981),
(#187982,#187983),(#187984,#187985),(#187986,#187987),(#187988,#187989),
(#187990,#187991),(#187992,#187993),(#187994,#187995),(#187996,#187997),
(#187998,#187999),(#188000,#188001),(#188002,#188003),(#188004,#188005),
(#188006,#188007),(#188008,#188009),(#188010,#188011),(#188012,#188013),
(#188014,#188015),(#188016,#188017),(#188018,#188019),(#188020,#188021),
(#188022,#188023),(#188024,#188025),(#188026,#188027),(#188028,#188029),
(#188030,#188031),(#188032,#188033),(#188034,#188035),(#188036,#188037),
(#188038,#188039),(#188040,#188041),(#188042,#188043),(#188044,#188045),
(#188046,#188047),(#188048,#188049),(#188050,#188051),(#188052,#188053),
(#188054,#188055),(#188056,#188057),(#188058,#188059),(#188060,#188061),
(#188062,#188063),(#188064,#188065),(#188066,#188067),(#188068,#188069),
(#188070,#188071),(#188072,#188073),(#188074,#188075),(#188076,#188077),
(#188078,#188079),(#188080,#188081),(#188082,#188083),(#188084,#188085),
(#188086,#188087),(#188088,#188089),(#188090,#188091),(#188092,#188093),
(#188094,#188095),(#188096,#188097),(#188098,#188099),(#188100,#188101),
(#188102,#188103),(#188104,#188105),(#188106,#188107),(#188108,#188109),
(#188110,#188111),(#188112,#188113),(#188114,#188115),(#188116,#188117),
(#188118,#188119),(#188120,#188121),(#188122,#188123),(#188124,#188125),
(#188126,#188127),(#188128,#188129),(#188130,#188131),(#188132,#188133),
(#188134,#188135),(#188136,#188137),(#188138,#188139),(#188140,#188141),
(#188142,#188143),(#188144,#188145),(#188146,#188147),(#188148,#188149),
(#188150,#188151),(#188152,#188153),(#188154,#188155),(#188156,#188157),
(#188158,#188159),(#188160,#188161),(#188162,#188163),(#188164,#188165),
(#188166,#188167),(#188168,#188169),(#188170,#188171),(#188172,#188173),
(#188174,#188175),(#188176,#188177),(#188178,#188179),(#188180,#188181),
(#188182,#188183),(#188184,#188185),(#188186,#188187),(#188188,#188189),
(#188190,#188191),(#188192,#188193),(#188194,#188195),(#188196,#188197),
(#188198,#188199),(#188200,#188201),(#188202,#188203),(#188204,#188205),
(#188206,#188207),(#188208,#188209),(#188210,#188211),(#188212,#188213),
(#188214,#188215),(#188216,#188217),(#188218,#188219),(#188220,#188221),
(#188222,#188223),(#188224,#188225),(#188226,#188227),(#188228,#188229),
(#188230,#188231),(#188232,#188233),(#188234,#188235),(#188236,#188237),
(#188238,#188239),(#188240,#188241),(#188242,#188243),(#188244,#188245),
(#188246,#188247),(#188248,#188249),(#188250,#188251),(#188252,#188253),
(#188254,#188255),(#188256,#188257),(#188258,#188259),(#188260,#188261),
(#188262,#188263),(#188264,#188265),(#188266,#188267),(#188268,#188269),
(#188270,#188271),(#188272,#188273),(#188274,#188275),(#188276,#188277),
(#188278,#188279),(#188280,#188281),(#188282,#188283),(#188284,#188285),
(#188286,#188287),(#188288,#188289),(#188290,#188291),(#188292,#188293),
(#188294,#188295),(#188296,#188297),(#188298,#188299),(#188300,#188301),
(#188302,#188303),(#188304,#188305),(#188306,#188307),(#188308,#188309),
(#188310,#188311),(#188312,#188313),(#188314,#188315),(#188316,#188317),
(#188318,#188319),(#188320,#188321),(#188322,#188323),(#188324,#188325),
(#188326,#188327),(#188328,#188329),(#188330,#188331),(#188332,#188333),
(#188334,#188335),(#188336,#188337),(#188338,#188339),(#188340,#188341),
(#188342,#188343),(#188344,#188345),(#188346,#188347),(#188348,#188349),
(#188350,#188351),(#188352,#188353),(#188354,#188355),(#188356,#188357),
(#188358,#188359),(#188360,#188361),(#188362,#188363),(#188364,#188365),
(#188366,#188367),(#188368,#188369),(#188370,#188371),(#188372,#188373),
(#188374,#188375),(#188376,#188377),(#188378,#188379),(#188380,#188381),
(#188382,#188383),(#188384,#188385),(#188386,#188387),(#188388,#188389),
(#188390,#188391),(#188392,#188393),(#188394,#188395),(#188396,#188397),
(#188398,#188399),(#188400,#188401),(#188402,#188403),(#188404,#188405),
(#188406,#188407),(#188408,#188409),(#188410,#188411),(#188412,#188413),
(#188414,#188415),(#188416,#188417),(#188418,#188419),(#188420,#188421),
(#188422,#188423),(#188424,#188425),(#188426,#188427),(#188428,#188429),
(#188430,#188431),(#188432,#188433),(#188434,#188435),(#188436,#188437),
(#188438,#188439),(#188440,#188441),(#188442,#188443),(#188444,#188445),
(#188446,#188447),(#188448,#188449),(#188450,#188451),(#188452,#188453),
(#188454,#188455),(#188456,#188457),(#188458,#188459),(#188460,#188461),
(#188462,#188463),(#188464,#188465),(#188466,#188467),(#188468,#188469),
(#188470,#188471),(#188472,#188473),(#188474,#188475),(#188476,#188477),
(#188478,#188479),(#188480,#188481),(#188482,#188483),(#188484,#188485),
(#188486,#188487),(#188488,#188489),(#188490,#188491),(#188492,#188493),
(#188494,#188495),(#188496,#188497),(#188498,#188499),(#188500,#188501),
(#188502,#188503),(#188504,#188505),(#188506,#188507),(#188508,#188509),
(#188510,#188511),(#188512,#188513),(#188514,#188515),(#188516,#188517),
(#188518,#188519),(#188520,#188521),(#188522,#188523),(#188524,#188525),
(#188526,#188527),(#188528,#188529),(#188530,#188531),(#188532,#188533),
(#188534,#188535),(#188536,#188537),(#188538,#188539),(#188540,#188541),
(#188542,#188543),(#188544,#188545),(#188546,#188547),(#188548,#188549),
(#188550,#188551),(#188552,#188553),(#188554,#188555),(#188556,#188557),
(#188558,#188559),(#188560,#188561),(#188562,#188563),(#188564,#188565),
(#188566,#188567),(#188568,#188569),(#188570,#188571),(#188572,#188573),
(#188574,#188575),(#188576,#188577),(#188578,#188579),(#188580,#188581),
(#188582,#188583),(#188584,#188585),(#188586,#188587),(#188588,#188589),
(#188590,#188591),(#188592,#188593),(#188594,#188595),(#188596,#188597),
(#188598,#188599),(#188600,#188601),(#188602,#188603),(#188604,#188605),
(#188606,#188607),(#188608,#188609),(#188610,#188611),(#188612,#188613),
(#188614,#188615),(#188616,#188617),(#188618,#188619),(#188620,#188621),
(#188622,#188623),(#188624,#188625),(#188626,#188627),(#188628,#188629),
(#188630,#188631),(#188632,#188633),(#188634,#188635),(#188636,#188637),
(#188638,#188639),(#188640,#188641),(#188642,#188643),(#188644,#188645),
(#188646,#188647),(#188648,#188649),(#188650,#188651),(#188652,#188653),
(#188654,#188655),(#188656,#188657),(#188658,#188659),(#188660,#188661),
(#188662,#188663),(#188664,#188665),(#188666,#188667),(#188668,#188669),
(#188670,#188671),(#188672,#188673),(#188674,#188675),(#188676,#188677),
(#188678,#188679),(#188680,#188681),(#188682,#188683),(#188684,#188685),
(#188686,#188687),(#188688,#188689),(#188690,#188691),(#188692,#188693),
(#188694,#188695),(#188696,#188697),(#188698,#188699),(#188700,#188701),
(#188702,#188703),(#188704,#188705),(#188706,#188707),(#188708,#188709),
(#188710,#188711),(#188712,#188713),(#188714,#188715),(#188716,#188717),
(#188718,#188719),(#188720,#188721),(#188722,#188723),(#188724,#188725),
(#188726,#188727),(#188728,#188729),(#188730,#188731),(#188732,#188733),
(#188734,#188735),(#188736,#188737),(#188738,#188739),(#188740,#188741),
(#188742,#188743),(#188744,#188745),(#188746,#188747),(#188748,#188749),
(#188750,#188751),(#188752,#188753),(#188754,#188755),(#188756,#188757),
(#188758,#188759),(#188760,#188761),(#188762,#188763),(#188764,#188765),
(#188766,#188767),(#188768,#188769),(#188770,#188771),(#188772,#188773),
(#188774,#188775),(#188776,#188777),(#188778,#188779),(#188780,#188781),
(#188782,#188783),(#188784,#188785),(#188786,#188787),(#188788,#188789),
(#188790,#188791),(#188792,#188793),(#188794,#188795),(#188796,#188797),
(#188798,#188799),(#188800,#188801),(#188802,#188803),(#188804,#188805),
(#188806,#188807),(#188808,#188809),(#188810,#188811),(#188812,#188813),
(#188814,#188815),(#188816,#188817),(#188818,#188819),(#188820,#188821),
(#188822,#188823),(#188824,#188825)),.UNSPECIFIED.,.F.,.F.,.F.,(6,1,1,1,
1,1,1,1,1,1,1,1,1,1,1,1,1,1,1,1,1,1,1,1,1,1,1,1,1,1,1,1,1,1,1,1,1,1,1,1,
1,1,1,1,1,1,1,1,1,1,1,1,1,1,1,1,1,1,1,1,1,1,1,1,1,1,1,1,1,1,1,1,1,1,1,1,
1,1,1,1,1,1,1,1,1,1,1,1,1,1,1,1,1,1,1,1,1,1,1,1,1,1,1,1,1,1,1,1,1,1,1,1,
1,1,1,1,1,1,1,1,1,1,1,1,1,1,1,1,1,1,1,1,1,1,1,1,1,1,1,1,1,1,1,1,1,1,1,1,
1,1,1,1,1,1,1,1,1,1,1,1,1,1,1,1,1,1,1,1,1,1,1,1,1,1,1,1,1,1,1,1,1,1,1,1,
1,1,1,1,1,1,1,1,1,1,1,1,1,1,1,1,1,1,1,1,1,1,1,1,1,1,1,1,1,1,1,1,1,1,1,1,
1,1,1,1,1,1,1,1,1,1,1,1,1,1,1,1,1,1,1,1,1,1,1,1,1,1,1,1,1,1,1,1,1,1,1,1,
1,1,1,1,1,1,1,1,1,1,1,1,1,1,1,1,1,1,1,1,1,1,1,1,1,1,1,1,1,1,1,1,1,1,1,1,
1,1,1,1,1,1,1,1,1,1,1,1,1,1,1,1,1,1,1,1,1,1,1,1,1,1,1,1,1,1,1,1,1,1,1,1,
1,1,1,1,1,1,1,1,1,1,1,1,1,1,1,1,1,1,1,1,1,1,1,1,1,1,1,1,1,1,1,1,1,1,1,1,
1,1,1,1,1,1,1,1,1,1,1,1,1,1,1,1,1,1,1,1,1,1,1,1,1,1,1,1,1,1,1,1,1,1,1,1,
1,1,1,1,1,1,1,1,1,1,1,1,1,1,1,1,1,1,1,1,1,1,1,1,1,1,1,1,1,1,1,1,1,1,1,1,
1,1,1,1,1,1,1,1,1,1,1,1,1,1,1,1,1,1,1,1,1,1,1,1,1,1,1,1,1,1,1,6),(2,2),
(0.143172103,0.144954128,0.146788991,0.148623853,0.150458716,0.152293578,
0.15412844,0.155963303,0.157798165,0.159633028,0.16146789,0.163302752,0.165137615,
0.166972477,0.168807339,0.170642202,0.172477064,0.174311927,0.176146789,
0.177981651,0.179816514,0.181651376,0.183486239,0.185321101,0.187155963,
0.188990826,0.190825688,0.19266055,0.194495413,0.196330275,0.198165138,
0.2,0.201834862,0.203669725,0.205504587,0.20733945,0.209174312,0.211009174,
0.212844037,0.214678899,0.216513761,0.218348624,0.220183486,0.222018349,
0.223853211,0.225688073,0.227522936,0.229357798,0.231192661,0.233027523,
0.234862385,0.236697248,0.23853211,0.240366972,0.242201835,0.244036697,
0.24587156,0.247706422,0.249541284,0.251376147,0.253211009,0.255045872,
0.256880734,0.258715596,0.260550459,0.262385321,0.264220183,0.266055046,
0.267889908,0.269724771,0.271559633,0.273394495,0.275229358,0.27706422,
0.278899083,0.280733945,0.282568807,0.28440367,0.286238532,0.288073394,
0.289908257,0.291743119,0.293577982,0.295412844,0.297247706,0.299082569,
0.300917431,0.302752294,0.304587156,0.306422018,0.308256881,0.310091743,
0.311926606,0.313761468,0.31559633,0.317431193,0.319266055,0.321100917,
0.32293578,0.324770642,0.326605505,0.328440367,0.330275229,0.332110092,
0.333944954,0.335779817,0.337614679,0.339449541,0.341284404,0.343119266,
0.344954128,0.346788991,0.348623853,0.350458716,0.352293578,0.35412844,
0.355963303,0.357798165,0.359633028,0.36146789,0.363302752,0.365137615,
0.366972477,0.368807339,0.370642202,0.372477064,0.374311927,0.376146789,
0.377981651,0.379816514,0.381651376,0.383486239,0.385321101,0.387155963,
0.388990826,0.390825688,0.39266055,0.394495413,0.396330275,0.398165138,
0.4,0.401834862,0.403669725,0.405504587,0.40733945,0.409174312,0.411009174,
0.412844037,0.414678899,0.416513761,0.418348624,0.420183486,0.422018349,
0.423853211,0.425688073,0.427522936,0.429357798,0.431192661,0.433027523,
0.434862385,0.436697248,0.43853211,0.440366972,0.442201835,0.444036697,
0.44587156,0.447706422,0.449541284,0.451376147,0.453211009,0.455045872,
0.456880734,0.458715596,0.460550459,0.462385321,0.464220183,0.466055046,
0.467889908,0.469724771,0.471559633,0.473394495,0.475229358,0.47706422,
0.478899083,0.480733945,0.482568807,0.48440367,0.486238532,0.488073394,
0.489908257,0.491743119,0.493577982,0.495412844,0.497247706,0.499082569,
0.500917431,0.502752294,0.504587156,0.506422018,0.508256881,0.510091743,
0.511926606,0.513761468,0.51559633,0.517431193,0.519266055,0.521100917,
0.52293578,0.524770642,0.526605505,0.528440367,0.530275229,0.532110092,
0.533944954,0.535779817,0.537614679,0.539449541,0.541284404,0.543119266,
0.544954128,0.546788991,0.548623853,0.550458716,0.552293578,0.55412844,
0.555963303,0.557798165,0.559633028,0.56146789,0.563302752,0.565137615,
0.566972477,0.568807339,0.570642202,0.572477064,0.574311927,0.576146789,
0.577981651,0.579816514,0.581651376,0.583486239,0.585321101,0.587155963,
0.588990826,0.590825688,0.59266055,0.594495413,0.596330275,0.598165138,
0.6,0.601834862,0.603669725,0.605504587,0.60733945,0.609174312,0.611009174,
0.612844037,0.614678899,0.616513761,0.618348624,0.620183486,0.622018349,
0.623853211,0.625688073,0.627522936,0.629357798,0.631192661,0.633027523,
0.634862385,0.636697248,0.63853211,0.640366972,0.642201835,0.644036697,
0.64587156,0.647706422,0.649541284,0.651376147,0.653211009,0.655045872,
0.656880734,0.658715596,0.660550459,0.662385321,0.664220183,0.666055046,
0.667889908,0.669724771,0.671559633,0.673394495,0.675229358,0.67706422,
0.678899083,0.680733945,0.682568807,0.68440367,0.686238532,0.688073394,
0.689908257,0.691743119,0.693577982,0.695412844,0.697247706,0.699082569,
0.700917431,0.702752294,0.704587156,0.706422018,0.708256881,0.710091743,
0.711926606,0.713761468,0.71559633,0.717431193,0.719266055,0.721100917,
0.72293578,0.724770642,0.726605505,0.728440367,0.730275229,0.732110092,
0.733944954,0.735779817,0.737614679,0.739449541,0.741284404,0.743119266,
0.744954128,0.746788991,0.748623853,0.750458716,0.752293578,0.75412844,
0.755963303,0.757798165,0.759633028,0.76146789,0.763302752,0.765137615,
0.766972477,0.768807339,0.770642202,0.772477064,0.774311927,0.776146789,
0.777981651,0.779816514,0.781651376,0.783486239,0.785321101,0.787155963,
0.788990826,0.790825688,0.79266055,0.794495413,0.796330275,0.798165138,
0.8,0.801834862,0.803669725,0.805504587,0.80733945,0.809174312,0.811009174,
0.812844037,0.814678899,0.816513761,0.818348624,0.820183486,0.822018349,
0.823853211,0.825688073,0.827522936,0.829357798,0.831192661,0.833027523,
0.834862385,0.836697248,0.83853211,0.840366972,0.842201835,0.844036697,
0.84587156,0.847706422,0.849541284,0.851376147,0.853211009,0.855045872,
0.856880734,0.858715596,0.860550459,0.862385321,0.864220183,0.866055046,
0.867889908,0.869724771,0.871559633,0.873394495,0.875229358,0.87706422,
0.878899083,0.880733945,0.882568807,0.88440367,0.886238532,0.888073394,
0.889908257,0.891743119,0.893577982,0.895412844,0.897247706,0.899082569,
0.900917431,0.902752294,0.904587156,0.906422018,0.908256881,0.910091743,
0.911926606,0.913761468,0.91559633,0.917431193,0.919266055,0.921100917,
0.92293578,0.924770642,0.926605505,0.928440367,0.930275229,0.932110092,
0.933944954,0.935779817,0.937614679,0.939449541,0.941284404,0.943119266,
0.944954128,0.946788991,0.948623853,0.950458716,0.952293578,0.95412844,
0.955963303,0.957798165,0.959633028,0.96146789,0.963302752,0.965137615,
0.966972477,0.968807339,0.970642202,0.972477064,0.974311927,0.976146789,
0.977981651,0.979816514,0.981651376,0.983486239,0.985321101,0.987155963,
0.988990826,0.990825688,0.99266055,0.994495413,0.996330275,0.998165138,
1.),(0.,0.36),.UNSPECIFIED.);
#6236=B_SPLINE_SURFACE_WITH_KNOTS('',5,1,((#189434,#189435),(#189436,#189437),
(#189438,#189439),(#189440,#189441),(#189442,#189443),(#189444,#189445),
(#189446,#189447),(#189448,#189449),(#189450,#189451),(#189452,#189453),
(#189454,#189455),(#189456,#189457),(#189458,#189459),(#189460,#189461),
(#189462,#189463),(#189464,#189465),(#189466,#189467),(#189468,#189469),
(#189470,#189471),(#189472,#189473),(#189474,#189475),(#189476,#189477),
(#189478,#189479),(#189480,#189481),(#189482,#189483),(#189484,#189485),
(#189486,#189487),(#189488,#189489),(#189490,#189491),(#189492,#189493),
(#189494,#189495),(#189496,#189497),(#189498,#189499),(#189500,#189501),
(#189502,#189503),(#189504,#189505),(#189506,#189507),(#189508,#189509),
(#189510,#189511),(#189512,#189513),(#189514,#189515),(#189516,#189517),
(#189518,#189519),(#189520,#189521),(#189522,#189523),(#189524,#189525),
(#189526,#189527),(#189528,#189529),(#189530,#189531),(#189532,#189533),
(#189534,#189535),(#189536,#189537),(#189538,#189539),(#189540,#189541),
(#189542,#189543),(#189544,#189545),(#189546,#189547),(#189548,#189549),
(#189550,#189551),(#189552,#189553),(#189554,#189555),(#189556,#189557),
(#189558,#189559),(#189560,#189561),(#189562,#189563),(#189564,#189565),
(#189566,#189567),(#189568,#189569),(#189570,#189571),(#189572,#189573),
(#189574,#189575),(#189576,#189577),(#189578,#189579),(#189580,#189581),
(#189582,#189583),(#189584,#189585),(#189586,#189587),(#189588,#189589),
(#189590,#189591),(#189592,#189593),(#189594,#189595),(#189596,#189597),
(#189598,#189599),(#189600,#189601),(#189602,#189603),(#189604,#189605),
(#189606,#189607),(#189608,#189609),(#189610,#189611),(#189612,#189613),
(#189614,#189615),(#189616,#189617),(#189618,#189619),(#189620,#189621),
(#189622,#189623),(#189624,#189625),(#189626,#189627),(#189628,#189629),
(#189630,#189631),(#189632,#189633),(#189634,#189635),(#189636,#189637),
(#189638,#189639),(#189640,#189641),(#189642,#189643),(#189644,#189645),
(#189646,#189647),(#189648,#189649),(#189650,#189651),(#189652,#189653),
(#189654,#189655),(#189656,#189657),(#189658,#189659),(#189660,#189661),
(#189662,#189663),(#189664,#189665),(#189666,#189667),(#189668,#189669),
(#189670,#189671),(#189672,#189673),(#189674,#189675),(#189676,#189677),
(#189678,#189679),(#189680,#189681),(#189682,#189683),(#189684,#189685),
(#189686,#189687),(#189688,#189689),(#189690,#189691),(#189692,#189693),
(#189694,#189695),(#189696,#189697),(#189698,#189699),(#189700,#189701),
(#189702,#189703),(#189704,#189705),(#189706,#189707),(#189708,#189709),
(#189710,#189711),(#189712,#189713),(#189714,#189715),(#189716,#189717),
(#189718,#189719),(#189720,#189721),(#189722,#189723),(#189724,#189725),
(#189726,#189727),(#189728,#189729),(#189730,#189731),(#189732,#189733),
(#189734,#189735),(#189736,#189737),(#189738,#189739),(#189740,#189741),
(#189742,#189743),(#189744,#189745),(#189746,#189747),(#189748,#189749),
(#189750,#189751),(#189752,#189753),(#189754,#189755),(#189756,#189757),
(#189758,#189759),(#189760,#189761),(#189762,#189763),(#189764,#189765),
(#189766,#189767),(#189768,#189769),(#189770,#189771),(#189772,#189773),
(#189774,#189775),(#189776,#189777),(#189778,#189779),(#189780,#189781),
(#189782,#189783),(#189784,#189785),(#189786,#189787),(#189788,#189789),
(#189790,#189791),(#189792,#189793),(#189794,#189795),(#189796,#189797),
(#189798,#189799),(#189800,#189801),(#189802,#189803),(#189804,#189805),
(#189806,#189807),(#189808,#189809),(#189810,#189811),(#189812,#189813),
(#189814,#189815),(#189816,#189817),(#189818,#189819),(#189820,#189821),
(#189822,#189823),(#189824,#189825),(#189826,#189827),(#189828,#189829),
(#189830,#189831),(#189832,#189833),(#189834,#189835),(#189836,#189837),
(#189838,#189839),(#189840,#189841),(#189842,#189843),(#189844,#189845),
(#189846,#189847),(#189848,#189849),(#189850,#189851),(#189852,#189853),
(#189854,#189855),(#189856,#189857),(#189858,#189859),(#189860,#189861),
(#189862,#189863),(#189864,#189865),(#189866,#189867),(#189868,#189869),
(#189870,#189871),(#189872,#189873),(#189874,#189875),(#189876,#189877),
(#189878,#189879),(#189880,#189881),(#189882,#189883),(#189884,#189885),
(#189886,#189887),(#189888,#189889),(#189890,#189891),(#189892,#189893),
(#189894,#189895),(#189896,#189897),(#189898,#189899),(#189900,#189901),
(#189902,#189903),(#189904,#189905),(#189906,#189907),(#189908,#189909),
(#189910,#189911),(#189912,#189913),(#189914,#189915),(#189916,#189917),
(#189918,#189919),(#189920,#189921),(#189922,#189923),(#189924,#189925),
(#189926,#189927),(#189928,#189929),(#189930,#189931),(#189932,#189933),
(#189934,#189935),(#189936,#189937),(#189938,#189939),(#189940,#189941),
(#189942,#189943),(#189944,#189945),(#189946,#189947),(#189948,#189949),
(#189950,#189951),(#189952,#189953),(#189954,#189955),(#189956,#189957),
(#189958,#189959),(#189960,#189961),(#189962,#189963),(#189964,#189965),
(#189966,#189967),(#189968,#189969),(#189970,#189971),(#189972,#189973),
(#189974,#189975),(#189976,#189977),(#189978,#189979),(#189980,#189981),
(#189982,#189983),(#189984,#189985),(#189986,#189987),(#189988,#189989),
(#189990,#189991),(#189992,#189993),(#189994,#189995),(#189996,#189997),
(#189998,#189999),(#190000,#190001),(#190002,#190003),(#190004,#190005),
(#190006,#190007),(#190008,#190009),(#190010,#190011),(#190012,#190013),
(#190014,#190015),(#190016,#190017),(#190018,#190019),(#190020,#190021),
(#190022,#190023),(#190024,#190025),(#190026,#190027),(#190028,#190029),
(#190030,#190031),(#190032,#190033),(#190034,#190035),(#190036,#190037),
(#190038,#190039),(#190040,#190041),(#190042,#190043),(#190044,#190045),
(#190046,#190047),(#190048,#190049),(#190050,#190051),(#190052,#190053),
(#190054,#190055),(#190056,#190057),(#190058,#190059),(#190060,#190061),
(#190062,#190063),(#190064,#190065),(#190066,#190067),(#190068,#190069),
(#190070,#190071),(#190072,#190073),(#190074,#190075),(#190076,#190077),
(#190078,#190079),(#190080,#190081),(#190082,#190083),(#190084,#190085),
(#190086,#190087),(#190088,#190089),(#190090,#190091),(#190092,#190093),
(#190094,#190095),(#190096,#190097),(#190098,#190099),(#190100,#190101),
(#190102,#190103),(#190104,#190105),(#190106,#190107),(#190108,#190109),
(#190110,#190111),(#190112,#190113),(#190114,#190115),(#190116,#190117),
(#190118,#190119),(#190120,#190121),(#190122,#190123),(#190124,#190125),
(#190126,#190127),(#190128,#190129),(#190130,#190131),(#190132,#190133),
(#190134,#190135),(#190136,#190137),(#190138,#190139),(#190140,#190141),
(#190142,#190143),(#190144,#190145),(#190146,#190147),(#190148,#190149),
(#190150,#190151),(#190152,#190153),(#190154,#190155),(#190156,#190157),
(#190158,#190159),(#190160,#190161),(#190162,#190163),(#190164,#190165),
(#190166,#190167),(#190168,#190169),(#190170,#190171),(#190172,#190173),
(#190174,#190175),(#190176,#190177),(#190178,#190179),(#190180,#190181),
(#190182,#190183),(#190184,#190185),(#190186,#190187),(#190188,#190189),
(#190190,#190191),(#190192,#190193),(#190194,#190195),(#190196,#190197),
(#190198,#190199),(#190200,#190201),(#190202,#190203),(#190204,#190205),
(#190206,#190207),(#190208,#190209),(#190210,#190211),(#190212,#190213),
(#190214,#190215),(#190216,#190217),(#190218,#190219),(#190220,#190221),
(#190222,#190223),(#190224,#190225),(#190226,#190227),(#190228,#190229),
(#190230,#190231),(#190232,#190233),(#190234,#190235),(#190236,#190237),
(#190238,#190239),(#190240,#190241),(#190242,#190243),(#190244,#190245),
(#190246,#190247),(#190248,#190249),(#190250,#190251),(#190252,#190253),
(#190254,#190255),(#190256,#190257),(#190258,#190259),(#190260,#190261),
(#190262,#190263),(#190264,#190265),(#190266,#190267),(#190268,#190269),
(#190270,#190271),(#190272,#190273),(#190274,#190275),(#190276,#190277),
(#190278,#190279),(#190280,#190281),(#190282,#190283),(#190284,#190285),
(#190286,#190287),(#190288,#190289),(#190290,#190291),(#190292,#190293),
(#190294,#190295),(#190296,#190297),(#190298,#190299),(#190300,#190301),
(#190302,#190303),(#190304,#190305),(#190306,#190307),(#190308,#190309),
(#190310,#190311),(#190312,#190313),(#190314,#190315),(#190316,#190317),
(#190318,#190319),(#190320,#190321),(#190322,#190323),(#190324,#190325),
(#190326,#190327),(#190328,#190329),(#190330,#190331),(#190332,#190333),
(#190334,#190335),(#190336,#190337),(#190338,#190339),(#190340,#190341),
(#190342,#190343),(#190344,#190345),(#190346,#190347),(#190348,#190349),
(#190350,#190351),(#190352,#190353),(#190354,#190355),(#190356,#190357),
(#190358,#190359),(#190360,#190361),(#190362,#190363),(#190364,#190365),
(#190366,#190367),(#190368,#190369),(#190370,#190371),(#190372,#190373),
(#190374,#190375),(#190376,#190377)),.UNSPECIFIED.,.F.,.F.,.F.,(6,1,1,1,
1,1,1,1,1,1,1,1,1,1,1,1,1,1,1,1,1,1,1,1,1,1,1,1,1,1,1,1,1,1,1,1,1,1,1,1,
1,1,1,1,1,1,1,1,1,1,1,1,1,1,1,1,1,1,1,1,1,1,1,1,1,1,1,1,1,1,1,1,1,1,1,1,
1,1,1,1,1,1,1,1,1,1,1,1,1,1,1,1,1,1,1,1,1,1,1,1,1,1,1,1,1,1,1,1,1,1,1,1,
1,1,1,1,1,1,1,1,1,1,1,1,1,1,1,1,1,1,1,1,1,1,1,1,1,1,1,1,1,1,1,1,1,1,1,1,
1,1,1,1,1,1,1,1,1,1,1,1,1,1,1,1,1,1,1,1,1,1,1,1,1,1,1,1,1,1,1,1,1,1,1,1,
1,1,1,1,1,1,1,1,1,1,1,1,1,1,1,1,1,1,1,1,1,1,1,1,1,1,1,1,1,1,1,1,1,1,1,1,
1,1,1,1,1,1,1,1,1,1,1,1,1,1,1,1,1,1,1,1,1,1,1,1,1,1,1,1,1,1,1,1,1,1,1,1,
1,1,1,1,1,1,1,1,1,1,1,1,1,1,1,1,1,1,1,1,1,1,1,1,1,1,1,1,1,1,1,1,1,1,1,1,
1,1,1,1,1,1,1,1,1,1,1,1,1,1,1,1,1,1,1,1,1,1,1,1,1,1,1,1,1,1,1,1,1,1,1,1,
1,1,1,1,1,1,1,1,1,1,1,1,1,1,1,1,1,1,1,1,1,1,1,1,1,1,1,1,1,1,1,1,1,1,1,1,
1,1,1,1,1,1,1,1,1,1,1,1,1,1,1,1,1,1,1,1,1,1,1,1,1,1,1,1,1,1,1,1,1,1,1,1,
1,1,1,1,1,1,1,1,1,1,1,1,1,1,1,1,1,1,1,1,1,1,1,1,1,1,1,1,1,1,1,1,1,1,1,1,
1,1,1,1,1,1,1,1,1,1,1,1,1,1,1,1,1,1,1,1,1,1,1,1,1,1,1,1,1,1,1,6),(2,2),
(-1.,-0.998165138,-0.996330275,-0.994495413,-0.99266055,-0.990825688,-0.988990826,
-0.987155963,-0.985321101,-0.983486239,-0.981651376,-0.979816514,-0.977981651,
-0.976146789,-0.974311927,-0.972477064,-0.970642202,-0.968807339,-0.966972477,
-0.965137615,-0.963302752,-0.96146789,-0.959633028,-0.957798165,-0.955963303,
-0.95412844,-0.952293578,-0.950458716,-0.948623853,-0.946788991,-0.944954128,
-0.943119266,-0.941284404,-0.939449541,-0.937614679,-0.935779817,-0.933944954,
-0.932110092,-0.930275229,-0.928440367,-0.926605505,-0.924770642,-0.92293578,
-0.921100917,-0.919266055,-0.917431193,-0.91559633,-0.913761468,-0.911926606,
-0.910091743,-0.908256881,-0.906422018,-0.904587156,-0.902752294,-0.900917431,
-0.899082569,-0.897247706,-0.895412844,-0.893577982,-0.891743119,-0.889908257,
-0.888073394,-0.886238532,-0.88440367,-0.882568807,-0.880733945,-0.878899083,
-0.87706422,-0.875229358,-0.873394495,-0.871559633,-0.869724771,-0.867889908,
-0.866055046,-0.864220183,-0.862385321,-0.860550459,-0.858715596,-0.856880734,
-0.855045872,-0.853211009,-0.851376147,-0.849541284,-0.847706422,-0.84587156,
-0.844036697,-0.842201835,-0.840366972,-0.83853211,-0.836697248,-0.834862385,
-0.833027523,-0.831192661,-0.829357798,-0.827522936,-0.825688073,-0.823853211,
-0.822018349,-0.820183486,-0.818348624,-0.816513761,-0.814678899,-0.812844037,
-0.811009174,-0.809174312,-0.80733945,-0.805504587,-0.803669725,-0.801834862,
-0.8,-0.798165138,-0.796330275,-0.794495413,-0.79266055,-0.790825688,-0.788990826,
-0.787155963,-0.785321101,-0.783486239,-0.781651376,-0.779816514,-0.777981651,
-0.776146789,-0.774311927,-0.772477064,-0.770642202,-0.768807339,-0.766972477,
-0.765137615,-0.763302752,-0.76146789,-0.759633028,-0.757798165,-0.755963303,
-0.75412844,-0.752293578,-0.750458716,-0.748623853,-0.746788991,-0.744954128,
-0.743119266,-0.741284404,-0.739449541,-0.737614679,-0.735779817,-0.733944954,
-0.732110092,-0.730275229,-0.728440367,-0.726605505,-0.724770642,-0.72293578,
-0.721100917,-0.719266055,-0.717431193,-0.71559633,-0.713761468,-0.711926606,
-0.710091743,-0.708256881,-0.706422018,-0.704587156,-0.702752294,-0.700917431,
-0.699082569,-0.697247706,-0.695412844,-0.693577982,-0.691743119,-0.689908257,
-0.688073394,-0.686238532,-0.68440367,-0.682568807,-0.680733945,-0.678899083,
-0.67706422,-0.675229358,-0.673394495,-0.671559633,-0.669724771,-0.667889908,
-0.666055046,-0.664220183,-0.662385321,-0.660550459,-0.658715596,-0.656880734,
-0.655045872,-0.653211009,-0.651376147,-0.649541284,-0.647706422,-0.64587156,
-0.644036697,-0.642201835,-0.640366972,-0.63853211,-0.636697248,-0.634862385,
-0.633027523,-0.631192661,-0.629357798,-0.627522936,-0.625688073,-0.623853211,
-0.622018349,-0.620183486,-0.618348624,-0.616513761,-0.614678899,-0.612844037,
-0.611009174,-0.609174312,-0.60733945,-0.605504587,-0.603669725,-0.601834862,
-0.6,-0.598165138,-0.596330275,-0.594495413,-0.59266055,-0.590825688,-0.588990826,
-0.587155963,-0.585321101,-0.583486239,-0.581651376,-0.579816514,-0.577981651,
-0.576146789,-0.574311927,-0.572477064,-0.570642202,-0.568807339,-0.566972477,
-0.565137615,-0.563302752,-0.56146789,-0.559633028,-0.557798165,-0.555963303,
-0.55412844,-0.552293578,-0.550458716,-0.548623853,-0.546788991,-0.544954128,
-0.543119266,-0.541284404,-0.539449541,-0.537614679,-0.535779817,-0.533944954,
-0.532110092,-0.530275229,-0.528440367,-0.526605505,-0.524770642,-0.52293578,
-0.521100917,-0.519266055,-0.517431193,-0.51559633,-0.513761468,-0.511926606,
-0.510091743,-0.508256881,-0.506422018,-0.504587156,-0.502752294,-0.500917431,
-0.499082569,-0.497247706,-0.495412844,-0.493577982,-0.491743119,-0.489908257,
-0.488073394,-0.486238532,-0.48440367,-0.482568807,-0.480733945,-0.478899083,
-0.47706422,-0.475229358,-0.473394495,-0.471559633,-0.469724771,-0.467889908,
-0.466055046,-0.464220183,-0.462385321,-0.460550459,-0.458715596,-0.456880734,
-0.455045872,-0.453211009,-0.451376147,-0.449541284,-0.447706422,-0.44587156,
-0.444036697,-0.442201835,-0.440366972,-0.43853211,-0.436697248,-0.434862385,
-0.433027523,-0.431192661,-0.429357798,-0.427522936,-0.425688073,-0.423853211,
-0.422018349,-0.420183486,-0.418348624,-0.416513761,-0.414678899,-0.412844037,
-0.411009174,-0.409174312,-0.40733945,-0.405504587,-0.403669725,-0.401834862,
-0.4,-0.398165138,-0.396330275,-0.394495413,-0.39266055,-0.390825688,-0.388990826,
-0.387155963,-0.385321101,-0.383486239,-0.381651376,-0.379816514,-0.377981651,
-0.376146789,-0.374311927,-0.372477064,-0.370642202,-0.368807339,-0.366972477,
-0.365137615,-0.363302752,-0.36146789,-0.359633028,-0.357798165,-0.355963303,
-0.35412844,-0.352293578,-0.350458716,-0.348623853,-0.346788991,-0.344954128,
-0.343119266,-0.341284404,-0.339449541,-0.337614679,-0.335779817,-0.333944954,
-0.332110092,-0.330275229,-0.328440367,-0.326605505,-0.324770642,-0.32293578,
-0.321100917,-0.319266055,-0.317431193,-0.31559633,-0.313761468,-0.311926606,
-0.310091743,-0.308256881,-0.306422018,-0.304587156,-0.302752294,-0.300917431,
-0.299082569,-0.297247706,-0.295412844,-0.293577982,-0.291743119,-0.289908257,
-0.288073394,-0.286238532,-0.28440367,-0.282568807,-0.280733945,-0.278899083,
-0.27706422,-0.275229358,-0.273394495,-0.271559633,-0.269724771,-0.267889908,
-0.266055046,-0.264220183,-0.262385321,-0.260550459,-0.258715596,-0.256880734,
-0.255045872,-0.253211009,-0.251376147,-0.249541284,-0.247706422,-0.24587156,
-0.244036697,-0.242201835,-0.240366972,-0.23853211,-0.236697248,-0.234862385,
-0.233027523,-0.231192661,-0.229357798,-0.227522936,-0.225688073,-0.223853211,
-0.222018349,-0.220183486,-0.218348624,-0.216513761,-0.214678899,-0.212844037,
-0.211009174,-0.209174312,-0.20733945,-0.205504587,-0.203669725,-0.201834862,
-0.2,-0.198165138,-0.196330275,-0.194495413,-0.19266055,-0.190825688,-0.188990826,
-0.187155963,-0.185321101,-0.183486239,-0.181651376,-0.179816514,-0.177981651,
-0.176146789,-0.174311927,-0.172477064,-0.170642202,-0.168807339,-0.166972477,
-0.165137615,-0.163302752,-0.16146789,-0.159633028,-0.157798165,-0.155963303,
-0.15412844,-0.152293578,-0.150458716,-0.148623853,-0.146788991,-0.144954128,
-0.143172103),(0.,0.36),.UNSPECIFIED.);
#6237=B_SPLINE_SURFACE_WITH_KNOTS('',5,1,((#191016,#191017),(#191018,#191019),
(#191020,#191021),(#191022,#191023),(#191024,#191025),(#191026,#191027),
(#191028,#191029),(#191030,#191031),(#191032,#191033),(#191034,#191035),
(#191036,#191037),(#191038,#191039),(#191040,#191041),(#191042,#191043),
(#191044,#191045),(#191046,#191047),(#191048,#191049),(#191050,#191051),
(#191052,#191053),(#191054,#191055),(#191056,#191057),(#191058,#191059),
(#191060,#191061),(#191062,#191063),(#191064,#191065),(#191066,#191067),
(#191068,#191069),(#191070,#191071),(#191072,#191073),(#191074,#191075),
(#191076,#191077),(#191078,#191079),(#191080,#191081),(#191082,#191083),
(#191084,#191085),(#191086,#191087),(#191088,#191089),(#191090,#191091),
(#191092,#191093),(#191094,#191095),(#191096,#191097),(#191098,#191099),
(#191100,#191101),(#191102,#191103),(#191104,#191105),(#191106,#191107),
(#191108,#191109),(#191110,#191111),(#191112,#191113),(#191114,#191115),
(#191116,#191117),(#191118,#191119),(#191120,#191121),(#191122,#191123),
(#191124,#191125),(#191126,#191127),(#191128,#191129),(#191130,#191131),
(#191132,#191133),(#191134,#191135),(#191136,#191137),(#191138,#191139),
(#191140,#191141),(#191142,#191143),(#191144,#191145),(#191146,#191147),
(#191148,#191149),(#191150,#191151),(#191152,#191153),(#191154,#191155),
(#191156,#191157),(#191158,#191159),(#191160,#191161),(#191162,#191163),
(#191164,#191165),(#191166,#191167),(#191168,#191169),(#191170,#191171),
(#191172,#191173),(#191174,#191175),(#191176,#191177),(#191178,#191179),
(#191180,#191181),(#191182,#191183),(#191184,#191185),(#191186,#191187),
(#191188,#191189),(#191190,#191191),(#191192,#191193),(#191194,#191195),
(#191196,#191197),(#191198,#191199),(#191200,#191201),(#191202,#191203),
(#191204,#191205),(#191206,#191207),(#191208,#191209),(#191210,#191211),
(#191212,#191213),(#191214,#191215),(#191216,#191217),(#191218,#191219),
(#191220,#191221),(#191222,#191223),(#191224,#191225),(#191226,#191227),
(#191228,#191229),(#191230,#191231),(#191232,#191233),(#191234,#191235),
(#191236,#191237),(#191238,#191239),(#191240,#191241),(#191242,#191243),
(#191244,#191245),(#191246,#191247),(#191248,#191249),(#191250,#191251),
(#191252,#191253),(#191254,#191255),(#191256,#191257),(#191258,#191259),
(#191260,#191261),(#191262,#191263),(#191264,#191265),(#191266,#191267),
(#191268,#191269),(#191270,#191271),(#191272,#191273),(#191274,#191275),
(#191276,#191277),(#191278,#191279),(#191280,#191281),(#191282,#191283),
(#191284,#191285),(#191286,#191287),(#191288,#191289),(#191290,#191291),
(#191292,#191293),(#191294,#191295),(#191296,#191297),(#191298,#191299),
(#191300,#191301),(#191302,#191303),(#191304,#191305),(#191306,#191307),
(#191308,#191309),(#191310,#191311),(#191312,#191313),(#191314,#191315),
(#191316,#191317),(#191318,#191319),(#191320,#191321),(#191322,#191323),
(#191324,#191325),(#191326,#191327),(#191328,#191329),(#191330,#191331),
(#191332,#191333),(#191334,#191335),(#191336,#191337),(#191338,#191339),
(#191340,#191341),(#191342,#191343),(#191344,#191345),(#191346,#191347),
(#191348,#191349),(#191350,#191351),(#191352,#191353),(#191354,#191355),
(#191356,#191357),(#191358,#191359),(#191360,#191361),(#191362,#191363),
(#191364,#191365),(#191366,#191367),(#191368,#191369),(#191370,#191371),
(#191372,#191373),(#191374,#191375),(#191376,#191377),(#191378,#191379),
(#191380,#191381),(#191382,#191383),(#191384,#191385),(#191386,#191387),
(#191388,#191389),(#191390,#191391),(#191392,#191393),(#191394,#191395),
(#191396,#191397),(#191398,#191399),(#191400,#191401),(#191402,#191403),
(#191404,#191405),(#191406,#191407),(#191408,#191409),(#191410,#191411),
(#191412,#191413),(#191414,#191415),(#191416,#191417),(#191418,#191419),
(#191420,#191421),(#191422,#191423),(#191424,#191425),(#191426,#191427),
(#191428,#191429),(#191430,#191431),(#191432,#191433),(#191434,#191435),
(#191436,#191437),(#191438,#191439),(#191440,#191441),(#191442,#191443),
(#191444,#191445),(#191446,#191447),(#191448,#191449),(#191450,#191451),
(#191452,#191453),(#191454,#191455),(#191456,#191457),(#191458,#191459),
(#191460,#191461),(#191462,#191463),(#191464,#191465),(#191466,#191467),
(#191468,#191469),(#191470,#191471),(#191472,#191473),(#191474,#191475),
(#191476,#191477),(#191478,#191479),(#191480,#191481),(#191482,#191483),
(#191484,#191485),(#191486,#191487),(#191488,#191489),(#191490,#191491),
(#191492,#191493),(#191494,#191495),(#191496,#191497),(#191498,#191499),
(#191500,#191501),(#191502,#191503),(#191504,#191505),(#191506,#191507),
(#191508,#191509),(#191510,#191511),(#191512,#191513),(#191514,#191515),
(#191516,#191517),(#191518,#191519),(#191520,#191521),(#191522,#191523),
(#191524,#191525),(#191526,#191527),(#191528,#191529),(#191530,#191531),
(#191532,#191533),(#191534,#191535),(#191536,#191537),(#191538,#191539),
(#191540,#191541),(#191542,#191543),(#191544,#191545),(#191546,#191547),
(#191548,#191549),(#191550,#191551),(#191552,#191553),(#191554,#191555),
(#191556,#191557),(#191558,#191559),(#191560,#191561),(#191562,#191563),
(#191564,#191565),(#191566,#191567),(#191568,#191569),(#191570,#191571),
(#191572,#191573),(#191574,#191575),(#191576,#191577),(#191578,#191579),
(#191580,#191581),(#191582,#191583),(#191584,#191585),(#191586,#191587),
(#191588,#191589),(#191590,#191591),(#191592,#191593),(#191594,#191595),
(#191596,#191597),(#191598,#191599),(#191600,#191601),(#191602,#191603),
(#191604,#191605),(#191606,#191607),(#191608,#191609),(#191610,#191611),
(#191612,#191613),(#191614,#191615),(#191616,#191617),(#191618,#191619),
(#191620,#191621),(#191622,#191623),(#191624,#191625),(#191626,#191627),
(#191628,#191629),(#191630,#191631),(#191632,#191633),(#191634,#191635),
(#191636,#191637),(#191638,#191639),(#191640,#191641),(#191642,#191643),
(#191644,#191645),(#191646,#191647),(#191648,#191649),(#191650,#191651),
(#191652,#191653),(#191654,#191655),(#191656,#191657),(#191658,#191659),
(#191660,#191661),(#191662,#191663),(#191664,#191665),(#191666,#191667),
(#191668,#191669),(#191670,#191671),(#191672,#191673),(#191674,#191675),
(#191676,#191677),(#191678,#191679),(#191680,#191681),(#191682,#191683),
(#191684,#191685),(#191686,#191687),(#191688,#191689),(#191690,#191691),
(#191692,#191693),(#191694,#191695),(#191696,#191697),(#191698,#191699),
(#191700,#191701),(#191702,#191703),(#191704,#191705),(#191706,#191707),
(#191708,#191709),(#191710,#191711),(#191712,#191713),(#191714,#191715),
(#191716,#191717),(#191718,#191719),(#191720,#191721),(#191722,#191723),
(#191724,#191725),(#191726,#191727),(#191728,#191729),(#191730,#191731),
(#191732,#191733),(#191734,#191735),(#191736,#191737),(#191738,#191739),
(#191740,#191741),(#191742,#191743),(#191744,#191745),(#191746,#191747),
(#191748,#191749),(#191750,#191751),(#191752,#191753),(#191754,#191755),
(#191756,#191757),(#191758,#191759),(#191760,#191761),(#191762,#191763),
(#191764,#191765),(#191766,#191767),(#191768,#191769),(#191770,#191771),
(#191772,#191773),(#191774,#191775),(#191776,#191777),(#191778,#191779),
(#191780,#191781),(#191782,#191783),(#191784,#191785),(#191786,#191787),
(#191788,#191789),(#191790,#191791),(#191792,#191793),(#191794,#191795),
(#191796,#191797),(#191798,#191799),(#191800,#191801),(#191802,#191803),
(#191804,#191805),(#191806,#191807),(#191808,#191809),(#191810,#191811),
(#191812,#191813),(#191814,#191815),(#191816,#191817),(#191818,#191819),
(#191820,#191821),(#191822,#191823),(#191824,#191825),(#191826,#191827),
(#191828,#191829),(#191830,#191831),(#191832,#191833),(#191834,#191835),
(#191836,#191837),(#191838,#191839),(#191840,#191841),(#191842,#191843),
(#191844,#191845),(#191846,#191847),(#191848,#191849),(#191850,#191851),
(#191852,#191853),(#191854,#191855),(#191856,#191857),(#191858,#191859),
(#191860,#191861),(#191862,#191863),(#191864,#191865),(#191866,#191867),
(#191868,#191869),(#191870,#191871),(#191872,#191873),(#191874,#191875),
(#191876,#191877),(#191878,#191879),(#191880,#191881),(#191882,#191883),
(#191884,#191885),(#191886,#191887),(#191888,#191889),(#191890,#191891),
(#191892,#191893),(#191894,#191895),(#191896,#191897),(#191898,#191899),
(#191900,#191901),(#191902,#191903),(#191904,#191905),(#191906,#191907),
(#191908,#191909),(#191910,#191911),(#191912,#191913),(#191914,#191915),
(#191916,#191917),(#191918,#191919),(#191920,#191921),(#191922,#191923),
(#191924,#191925),(#191926,#191927),(#191928,#191929),(#191930,#191931),
(#191932,#191933),(#191934,#191935),(#191936,#191937),(#191938,#191939),
(#191940,#191941),(#191942,#191943),(#191944,#191945),(#191946,#191947),
(#191948,#191949),(#191950,#191951),(#191952,#191953),(#191954,#191955),
(#191956,#191957),(#191958,#191959)),.UNSPECIFIED.,.F.,.F.,.F.,(6,1,1,1,
1,1,1,1,1,1,1,1,1,1,1,1,1,1,1,1,1,1,1,1,1,1,1,1,1,1,1,1,1,1,1,1,1,1,1,1,
1,1,1,1,1,1,1,1,1,1,1,1,1,1,1,1,1,1,1,1,1,1,1,1,1,1,1,1,1,1,1,1,1,1,1,1,
1,1,1,1,1,1,1,1,1,1,1,1,1,1,1,1,1,1,1,1,1,1,1,1,1,1,1,1,1,1,1,1,1,1,1,1,
1,1,1,1,1,1,1,1,1,1,1,1,1,1,1,1,1,1,1,1,1,1,1,1,1,1,1,1,1,1,1,1,1,1,1,1,
1,1,1,1,1,1,1,1,1,1,1,1,1,1,1,1,1,1,1,1,1,1,1,1,1,1,1,1,1,1,1,1,1,1,1,1,
1,1,1,1,1,1,1,1,1,1,1,1,1,1,1,1,1,1,1,1,1,1,1,1,1,1,1,1,1,1,1,1,1,1,1,1,
1,1,1,1,1,1,1,1,1,1,1,1,1,1,1,1,1,1,1,1,1,1,1,1,1,1,1,1,1,1,1,1,1,1,1,1,
1,1,1,1,1,1,1,1,1,1,1,1,1,1,1,1,1,1,1,1,1,1,1,1,1,1,1,1,1,1,1,1,1,1,1,1,
1,1,1,1,1,1,1,1,1,1,1,1,1,1,1,1,1,1,1,1,1,1,1,1,1,1,1,1,1,1,1,1,1,1,1,1,
1,1,1,1,1,1,1,1,1,1,1,1,1,1,1,1,1,1,1,1,1,1,1,1,1,1,1,1,1,1,1,1,1,1,1,1,
1,1,1,1,1,1,1,1,1,1,1,1,1,1,1,1,1,1,1,1,1,1,1,1,1,1,1,1,1,1,1,1,1,1,1,1,
1,1,1,1,1,1,1,1,1,1,1,1,1,1,1,1,1,1,1,1,1,1,1,1,1,1,1,1,1,1,1,1,1,1,1,1,
1,1,1,1,1,1,1,1,1,1,1,1,1,1,1,1,1,1,1,1,1,1,1,1,1,1,1,1,1,1,1,6),(2,2),
(-1.,-0.998165138,-0.996330275,-0.994495413,-0.99266055,-0.990825688,-0.988990826,
-0.987155963,-0.985321101,-0.983486239,-0.981651376,-0.979816514,-0.977981651,
-0.976146789,-0.974311927,-0.972477064,-0.970642202,-0.968807339,-0.966972477,
-0.965137615,-0.963302752,-0.96146789,-0.959633028,-0.957798165,-0.955963303,
-0.95412844,-0.952293578,-0.950458716,-0.948623853,-0.946788991,-0.944954128,
-0.943119266,-0.941284404,-0.939449541,-0.937614679,-0.935779817,-0.933944954,
-0.932110092,-0.930275229,-0.928440367,-0.926605505,-0.924770642,-0.92293578,
-0.921100917,-0.919266055,-0.917431193,-0.91559633,-0.913761468,-0.911926606,
-0.910091743,-0.908256881,-0.906422018,-0.904587156,-0.902752294,-0.900917431,
-0.899082569,-0.897247706,-0.895412844,-0.893577982,-0.891743119,-0.889908257,
-0.888073394,-0.886238532,-0.88440367,-0.882568807,-0.880733945,-0.878899083,
-0.87706422,-0.875229358,-0.873394495,-0.871559633,-0.869724771,-0.867889908,
-0.866055046,-0.864220183,-0.862385321,-0.860550459,-0.858715596,-0.856880734,
-0.855045872,-0.853211009,-0.851376147,-0.849541284,-0.847706422,-0.84587156,
-0.844036697,-0.842201835,-0.840366972,-0.83853211,-0.836697248,-0.834862385,
-0.833027523,-0.831192661,-0.829357798,-0.827522936,-0.825688073,-0.823853211,
-0.822018349,-0.820183486,-0.818348624,-0.816513761,-0.814678899,-0.812844037,
-0.811009174,-0.809174312,-0.80733945,-0.805504587,-0.803669725,-0.801834862,
-0.8,-0.798165138,-0.796330275,-0.794495413,-0.79266055,-0.790825688,-0.788990826,
-0.787155963,-0.785321101,-0.783486239,-0.781651376,-0.779816514,-0.777981651,
-0.776146789,-0.774311927,-0.772477064,-0.770642202,-0.768807339,-0.766972477,
-0.765137615,-0.763302752,-0.76146789,-0.759633028,-0.757798165,-0.755963303,
-0.75412844,-0.752293578,-0.750458716,-0.748623853,-0.746788991,-0.744954128,
-0.743119266,-0.741284404,-0.739449541,-0.737614679,-0.735779817,-0.733944954,
-0.732110092,-0.730275229,-0.728440367,-0.726605505,-0.724770642,-0.72293578,
-0.721100917,-0.719266055,-0.717431193,-0.71559633,-0.713761468,-0.711926606,
-0.710091743,-0.708256881,-0.706422018,-0.704587156,-0.702752294,-0.700917431,
-0.699082569,-0.697247706,-0.695412844,-0.693577982,-0.691743119,-0.689908257,
-0.688073394,-0.686238532,-0.68440367,-0.682568807,-0.680733945,-0.678899083,
-0.67706422,-0.675229358,-0.673394495,-0.671559633,-0.669724771,-0.667889908,
-0.666055046,-0.664220183,-0.662385321,-0.660550459,-0.658715596,-0.656880734,
-0.655045872,-0.653211009,-0.651376147,-0.649541284,-0.647706422,-0.64587156,
-0.644036697,-0.642201835,-0.640366972,-0.63853211,-0.636697248,-0.634862385,
-0.633027523,-0.631192661,-0.629357798,-0.627522936,-0.625688073,-0.623853211,
-0.622018349,-0.620183486,-0.618348624,-0.616513761,-0.614678899,-0.612844037,
-0.611009174,-0.609174312,-0.60733945,-0.605504587,-0.603669725,-0.601834862,
-0.6,-0.598165138,-0.596330275,-0.594495413,-0.59266055,-0.590825688,-0.588990826,
-0.587155963,-0.585321101,-0.583486239,-0.581651376,-0.579816514,-0.577981651,
-0.576146789,-0.574311927,-0.572477064,-0.570642202,-0.568807339,-0.566972477,
-0.565137615,-0.563302752,-0.56146789,-0.559633028,-0.557798165,-0.555963303,
-0.55412844,-0.552293578,-0.550458716,-0.548623853,-0.546788991,-0.544954128,
-0.543119266,-0.541284404,-0.539449541,-0.537614679,-0.535779817,-0.533944954,
-0.532110092,-0.530275229,-0.528440367,-0.526605505,-0.524770642,-0.52293578,
-0.521100917,-0.519266055,-0.517431193,-0.51559633,-0.513761468,-0.511926606,
-0.510091743,-0.508256881,-0.506422018,-0.504587156,-0.502752294,-0.500917431,
-0.499082569,-0.497247706,-0.495412844,-0.493577982,-0.491743119,-0.489908257,
-0.488073394,-0.486238532,-0.48440367,-0.482568807,-0.480733945,-0.478899083,
-0.47706422,-0.475229358,-0.473394495,-0.471559633,-0.469724771,-0.467889908,
-0.466055046,-0.464220183,-0.462385321,-0.460550459,-0.458715596,-0.456880734,
-0.455045872,-0.453211009,-0.451376147,-0.449541284,-0.447706422,-0.44587156,
-0.444036697,-0.442201835,-0.440366972,-0.43853211,-0.436697248,-0.434862385,
-0.433027523,-0.431192661,-0.429357798,-0.427522936,-0.425688073,-0.423853211,
-0.422018349,-0.420183486,-0.418348624,-0.416513761,-0.414678899,-0.412844037,
-0.411009174,-0.409174312,-0.40733945,-0.405504587,-0.403669725,-0.401834862,
-0.4,-0.398165138,-0.396330275,-0.394495413,-0.39266055,-0.390825688,-0.388990826,
-0.387155963,-0.385321101,-0.383486239,-0.381651376,-0.379816514,-0.377981651,
-0.376146789,-0.374311927,-0.372477064,-0.370642202,-0.368807339,-0.366972477,
-0.365137615,-0.363302752,-0.36146789,-0.359633028,-0.357798165,-0.355963303,
-0.35412844,-0.352293578,-0.350458716,-0.348623853,-0.346788991,-0.344954128,
-0.343119266,-0.341284404,-0.339449541,-0.337614679,-0.335779817,-0.333944954,
-0.332110092,-0.330275229,-0.328440367,-0.326605505,-0.324770642,-0.32293578,
-0.321100917,-0.319266055,-0.317431193,-0.31559633,-0.313761468,-0.311926606,
-0.310091743,-0.308256881,-0.306422018,-0.304587156,-0.302752294,-0.300917431,
-0.299082569,-0.297247706,-0.295412844,-0.293577982,-0.291743119,-0.289908257,
-0.288073394,-0.286238532,-0.28440367,-0.282568807,-0.280733945,-0.278899083,
-0.27706422,-0.275229358,-0.273394495,-0.271559633,-0.269724771,-0.267889908,
-0.266055046,-0.264220183,-0.262385321,-0.260550459,-0.258715596,-0.256880734,
-0.255045872,-0.253211009,-0.251376147,-0.249541284,-0.247706422,-0.24587156,
-0.244036697,-0.242201835,-0.240366972,-0.23853211,-0.236697248,-0.234862385,
-0.233027523,-0.231192661,-0.229357798,-0.227522936,-0.225688073,-0.223853211,
-0.222018349,-0.220183486,-0.218348624,-0.216513761,-0.214678899,-0.212844037,
-0.211009174,-0.209174312,-0.20733945,-0.205504587,-0.203669725,-0.201834862,
-0.2,-0.198165138,-0.196330275,-0.194495413,-0.19266055,-0.190825688,-0.188990826,
-0.187155963,-0.185321101,-0.183486239,-0.181651376,-0.179816514,-0.177981651,
-0.176146789,-0.174311927,-0.172477064,-0.170642202,-0.168807339,-0.166972477,
-0.165137615,-0.163302752,-0.16146789,-0.159633028,-0.157798165,-0.155963303,
-0.15412844,-0.152293578,-0.150458716,-0.148623853,-0.146788991,-0.144954128,
-0.143172103),(0.,0.36),.UNSPECIFIED.);
#6238=B_SPLINE_SURFACE_WITH_KNOTS('',5,1,((#192905,#192906),(#192907,#192908),
(#192909,#192910),(#192911,#192912),(#192913,#192914),(#192915,#192916),
(#192917,#192918),(#192919,#192920),(#192921,#192922),(#192923,#192924),
(#192925,#192926),(#192927,#192928),(#192929,#192930),(#192931,#192932),
(#192933,#192934),(#192935,#192936),(#192937,#192938),(#192939,#192940),
(#192941,#192942),(#192943,#192944),(#192945,#192946),(#192947,#192948),
(#192949,#192950),(#192951,#192952),(#192953,#192954),(#192955,#192956),
(#192957,#192958),(#192959,#192960),(#192961,#192962),(#192963,#192964),
(#192965,#192966),(#192967,#192968),(#192969,#192970),(#192971,#192972),
(#192973,#192974),(#192975,#192976),(#192977,#192978),(#192979,#192980),
(#192981,#192982),(#192983,#192984),(#192985,#192986),(#192987,#192988),
(#192989,#192990),(#192991,#192992),(#192993,#192994),(#192995,#192996),
(#192997,#192998),(#192999,#193000),(#193001,#193002),(#193003,#193004),
(#193005,#193006),(#193007,#193008),(#193009,#193010),(#193011,#193012),
(#193013,#193014),(#193015,#193016),(#193017,#193018),(#193019,#193020),
(#193021,#193022),(#193023,#193024),(#193025,#193026),(#193027,#193028),
(#193029,#193030),(#193031,#193032),(#193033,#193034),(#193035,#193036),
(#193037,#193038),(#193039,#193040),(#193041,#193042),(#193043,#193044),
(#193045,#193046),(#193047,#193048),(#193049,#193050),(#193051,#193052),
(#193053,#193054),(#193055,#193056),(#193057,#193058),(#193059,#193060),
(#193061,#193062),(#193063,#193064),(#193065,#193066),(#193067,#193068),
(#193069,#193070),(#193071,#193072),(#193073,#193074),(#193075,#193076),
(#193077,#193078),(#193079,#193080),(#193081,#193082),(#193083,#193084),
(#193085,#193086),(#193087,#193088),(#193089,#193090),(#193091,#193092),
(#193093,#193094),(#193095,#193096),(#193097,#193098),(#193099,#193100),
(#193101,#193102),(#193103,#193104),(#193105,#193106),(#193107,#193108),
(#193109,#193110),(#193111,#193112),(#193113,#193114),(#193115,#193116),
(#193117,#193118),(#193119,#193120),(#193121,#193122),(#193123,#193124),
(#193125,#193126),(#193127,#193128),(#193129,#193130),(#193131,#193132),
(#193133,#193134),(#193135,#193136),(#193137,#193138),(#193139,#193140),
(#193141,#193142),(#193143,#193144),(#193145,#193146),(#193147,#193148),
(#193149,#193150),(#193151,#193152),(#193153,#193154),(#193155,#193156),
(#193157,#193158),(#193159,#193160),(#193161,#193162),(#193163,#193164),
(#193165,#193166),(#193167,#193168),(#193169,#193170),(#193171,#193172),
(#193173,#193174),(#193175,#193176),(#193177,#193178),(#193179,#193180),
(#193181,#193182),(#193183,#193184),(#193185,#193186),(#193187,#193188),
(#193189,#193190),(#193191,#193192),(#193193,#193194),(#193195,#193196),
(#193197,#193198),(#193199,#193200),(#193201,#193202),(#193203,#193204),
(#193205,#193206),(#193207,#193208),(#193209,#193210),(#193211,#193212),
(#193213,#193214),(#193215,#193216),(#193217,#193218),(#193219,#193220),
(#193221,#193222),(#193223,#193224),(#193225,#193226),(#193227,#193228),
(#193229,#193230),(#193231,#193232),(#193233,#193234),(#193235,#193236),
(#193237,#193238),(#193239,#193240),(#193241,#193242),(#193243,#193244),
(#193245,#193246),(#193247,#193248),(#193249,#193250),(#193251,#193252),
(#193253,#193254),(#193255,#193256),(#193257,#193258),(#193259,#193260),
(#193261,#193262),(#193263,#193264),(#193265,#193266),(#193267,#193268),
(#193269,#193270),(#193271,#193272),(#193273,#193274),(#193275,#193276),
(#193277,#193278),(#193279,#193280),(#193281,#193282),(#193283,#193284),
(#193285,#193286),(#193287,#193288),(#193289,#193290),(#193291,#193292),
(#193293,#193294),(#193295,#193296),(#193297,#193298),(#193299,#193300),
(#193301,#193302),(#193303,#193304),(#193305,#193306),(#193307,#193308),
(#193309,#193310),(#193311,#193312),(#193313,#193314),(#193315,#193316),
(#193317,#193318),(#193319,#193320),(#193321,#193322),(#193323,#193324),
(#193325,#193326),(#193327,#193328),(#193329,#193330),(#193331,#193332),
(#193333,#193334),(#193335,#193336),(#193337,#193338),(#193339,#193340),
(#193341,#193342),(#193343,#193344),(#193345,#193346),(#193347,#193348),
(#193349,#193350),(#193351,#193352),(#193353,#193354),(#193355,#193356),
(#193357,#193358),(#193359,#193360),(#193361,#193362),(#193363,#193364),
(#193365,#193366),(#193367,#193368),(#193369,#193370),(#193371,#193372),
(#193373,#193374),(#193375,#193376),(#193377,#193378),(#193379,#193380),
(#193381,#193382),(#193383,#193384),(#193385,#193386),(#193387,#193388),
(#193389,#193390),(#193391,#193392),(#193393,#193394),(#193395,#193396),
(#193397,#193398),(#193399,#193400),(#193401,#193402),(#193403,#193404),
(#193405,#193406),(#193407,#193408),(#193409,#193410),(#193411,#193412),
(#193413,#193414),(#193415,#193416),(#193417,#193418),(#193419,#193420),
(#193421,#193422),(#193423,#193424),(#193425,#193426),(#193427,#193428),
(#193429,#193430),(#193431,#193432),(#193433,#193434),(#193435,#193436),
(#193437,#193438),(#193439,#193440),(#193441,#193442),(#193443,#193444),
(#193445,#193446),(#193447,#193448),(#193449,#193450),(#193451,#193452),
(#193453,#193454),(#193455,#193456),(#193457,#193458),(#193459,#193460),
(#193461,#193462),(#193463,#193464),(#193465,#193466),(#193467,#193468),
(#193469,#193470),(#193471,#193472),(#193473,#193474),(#193475,#193476),
(#193477,#193478),(#193479,#193480),(#193481,#193482),(#193483,#193484),
(#193485,#193486),(#193487,#193488),(#193489,#193490),(#193491,#193492),
(#193493,#193494),(#193495,#193496),(#193497,#193498),(#193499,#193500),
(#193501,#193502),(#193503,#193504),(#193505,#193506),(#193507,#193508),
(#193509,#193510),(#193511,#193512),(#193513,#193514),(#193515,#193516),
(#193517,#193518),(#193519,#193520),(#193521,#193522),(#193523,#193524),
(#193525,#193526),(#193527,#193528),(#193529,#193530),(#193531,#193532),
(#193533,#193534),(#193535,#193536),(#193537,#193538),(#193539,#193540),
(#193541,#193542),(#193543,#193544),(#193545,#193546),(#193547,#193548),
(#193549,#193550),(#193551,#193552),(#193553,#193554),(#193555,#193556),
(#193557,#193558),(#193559,#193560),(#193561,#193562),(#193563,#193564),
(#193565,#193566),(#193567,#193568),(#193569,#193570),(#193571,#193572),
(#193573,#193574),(#193575,#193576),(#193577,#193578),(#193579,#193580),
(#193581,#193582),(#193583,#193584),(#193585,#193586),(#193587,#193588),
(#193589,#193590),(#193591,#193592),(#193593,#193594),(#193595,#193596),
(#193597,#193598),(#193599,#193600),(#193601,#193602),(#193603,#193604),
(#193605,#193606),(#193607,#193608),(#193609,#193610),(#193611,#193612),
(#193613,#193614),(#193615,#193616),(#193617,#193618),(#193619,#193620),
(#193621,#193622),(#193623,#193624),(#193625,#193626),(#193627,#193628),
(#193629,#193630),(#193631,#193632),(#193633,#193634),(#193635,#193636),
(#193637,#193638),(#193639,#193640),(#193641,#193642),(#193643,#193644),
(#193645,#193646),(#193647,#193648),(#193649,#193650),(#193651,#193652),
(#193653,#193654),(#193655,#193656),(#193657,#193658),(#193659,#193660),
(#193661,#193662),(#193663,#193664),(#193665,#193666),(#193667,#193668),
(#193669,#193670),(#193671,#193672),(#193673,#193674),(#193675,#193676),
(#193677,#193678),(#193679,#193680),(#193681,#193682),(#193683,#193684),
(#193685,#193686),(#193687,#193688),(#193689,#193690),(#193691,#193692),
(#193693,#193694),(#193695,#193696),(#193697,#193698),(#193699,#193700),
(#193701,#193702),(#193703,#193704),(#193705,#193706),(#193707,#193708),
(#193709,#193710),(#193711,#193712),(#193713,#193714),(#193715,#193716),
(#193717,#193718),(#193719,#193720),(#193721,#193722),(#193723,#193724),
(#193725,#193726),(#193727,#193728),(#193729,#193730),(#193731,#193732),
(#193733,#193734),(#193735,#193736),(#193737,#193738),(#193739,#193740),
(#193741,#193742),(#193743,#193744),(#193745,#193746),(#193747,#193748),
(#193749,#193750),(#193751,#193752),(#193753,#193754),(#193755,#193756),
(#193757,#193758),(#193759,#193760),(#193761,#193762),(#193763,#193764),
(#193765,#193766),(#193767,#193768),(#193769,#193770),(#193771,#193772),
(#193773,#193774),(#193775,#193776),(#193777,#193778),(#193779,#193780),
(#193781,#193782),(#193783,#193784),(#193785,#193786),(#193787,#193788),
(#193789,#193790),(#193791,#193792),(#193793,#193794),(#193795,#193796),
(#193797,#193798),(#193799,#193800),(#193801,#193802),(#193803,#193804),
(#193805,#193806),(#193807,#193808),(#193809,#193810),(#193811,#193812),
(#193813,#193814),(#193815,#193816),(#193817,#193818),(#193819,#193820),
(#193821,#193822),(#193823,#193824),(#193825,#193826),(#193827,#193828),
(#193829,#193830),(#193831,#193832),(#193833,#193834),(#193835,#193836),
(#193837,#193838),(#193839,#193840),(#193841,#193842),(#193843,#193844),
(#193845,#193846),(#193847,#193848)),.UNSPECIFIED.,.F.,.F.,.F.,(6,1,1,1,
1,1,1,1,1,1,1,1,1,1,1,1,1,1,1,1,1,1,1,1,1,1,1,1,1,1,1,1,1,1,1,1,1,1,1,1,
1,1,1,1,1,1,1,1,1,1,1,1,1,1,1,1,1,1,1,1,1,1,1,1,1,1,1,1,1,1,1,1,1,1,1,1,
1,1,1,1,1,1,1,1,1,1,1,1,1,1,1,1,1,1,1,1,1,1,1,1,1,1,1,1,1,1,1,1,1,1,1,1,
1,1,1,1,1,1,1,1,1,1,1,1,1,1,1,1,1,1,1,1,1,1,1,1,1,1,1,1,1,1,1,1,1,1,1,1,
1,1,1,1,1,1,1,1,1,1,1,1,1,1,1,1,1,1,1,1,1,1,1,1,1,1,1,1,1,1,1,1,1,1,1,1,
1,1,1,1,1,1,1,1,1,1,1,1,1,1,1,1,1,1,1,1,1,1,1,1,1,1,1,1,1,1,1,1,1,1,1,1,
1,1,1,1,1,1,1,1,1,1,1,1,1,1,1,1,1,1,1,1,1,1,1,1,1,1,1,1,1,1,1,1,1,1,1,1,
1,1,1,1,1,1,1,1,1,1,1,1,1,1,1,1,1,1,1,1,1,1,1,1,1,1,1,1,1,1,1,1,1,1,1,1,
1,1,1,1,1,1,1,1,1,1,1,1,1,1,1,1,1,1,1,1,1,1,1,1,1,1,1,1,1,1,1,1,1,1,1,1,
1,1,1,1,1,1,1,1,1,1,1,1,1,1,1,1,1,1,1,1,1,1,1,1,1,1,1,1,1,1,1,1,1,1,1,1,
1,1,1,1,1,1,1,1,1,1,1,1,1,1,1,1,1,1,1,1,1,1,1,1,1,1,1,1,1,1,1,1,1,1,1,1,
1,1,1,1,1,1,1,1,1,1,1,1,1,1,1,1,1,1,1,1,1,1,1,1,1,1,1,1,1,1,1,1,1,1,1,1,
1,1,1,1,1,1,1,1,1,1,1,1,1,1,1,1,1,1,1,1,1,1,1,1,1,1,1,1,1,1,1,6),(2,2),
(0.143172103,0.144954128,0.146788991,0.148623853,0.150458716,0.152293578,
0.15412844,0.155963303,0.157798165,0.159633028,0.16146789,0.163302752,0.165137615,
0.166972477,0.168807339,0.170642202,0.172477064,0.174311927,0.176146789,
0.177981651,0.179816514,0.181651376,0.183486239,0.185321101,0.187155963,
0.188990826,0.190825688,0.19266055,0.194495413,0.196330275,0.198165138,
0.2,0.201834862,0.203669725,0.205504587,0.20733945,0.209174312,0.211009174,
0.212844037,0.214678899,0.216513761,0.218348624,0.220183486,0.222018349,
0.223853211,0.225688073,0.227522936,0.229357798,0.231192661,0.233027523,
0.234862385,0.236697248,0.23853211,0.240366972,0.242201835,0.244036697,
0.24587156,0.247706422,0.249541284,0.251376147,0.253211009,0.255045872,
0.256880734,0.258715596,0.260550459,0.262385321,0.264220183,0.266055046,
0.267889908,0.269724771,0.271559633,0.273394495,0.275229358,0.27706422,
0.278899083,0.280733945,0.282568807,0.28440367,0.286238532,0.288073394,
0.289908257,0.291743119,0.293577982,0.295412844,0.297247706,0.299082569,
0.300917431,0.302752294,0.304587156,0.306422018,0.308256881,0.310091743,
0.311926606,0.313761468,0.31559633,0.317431193,0.319266055,0.321100917,
0.32293578,0.324770642,0.326605505,0.328440367,0.330275229,0.332110092,
0.333944954,0.335779817,0.337614679,0.339449541,0.341284404,0.343119266,
0.344954128,0.346788991,0.348623853,0.350458716,0.352293578,0.35412844,
0.355963303,0.357798165,0.359633028,0.36146789,0.363302752,0.365137615,
0.366972477,0.368807339,0.370642202,0.372477064,0.374311927,0.376146789,
0.377981651,0.379816514,0.381651376,0.383486239,0.385321101,0.387155963,
0.388990826,0.390825688,0.39266055,0.394495413,0.396330275,0.398165138,
0.4,0.401834862,0.403669725,0.405504587,0.40733945,0.409174312,0.411009174,
0.412844037,0.414678899,0.416513761,0.418348624,0.420183486,0.422018349,
0.423853211,0.425688073,0.427522936,0.429357798,0.431192661,0.433027523,
0.434862385,0.436697248,0.43853211,0.440366972,0.442201835,0.444036697,
0.44587156,0.447706422,0.449541284,0.451376147,0.453211009,0.455045872,
0.456880734,0.458715596,0.460550459,0.462385321,0.464220183,0.466055046,
0.467889908,0.469724771,0.471559633,0.473394495,0.475229358,0.47706422,
0.478899083,0.480733945,0.482568807,0.48440367,0.486238532,0.488073394,
0.489908257,0.491743119,0.493577982,0.495412844,0.497247706,0.499082569,
0.500917431,0.502752294,0.504587156,0.506422018,0.508256881,0.510091743,
0.511926606,0.513761468,0.51559633,0.517431193,0.519266055,0.521100917,
0.52293578,0.524770642,0.526605505,0.528440367,0.530275229,0.532110092,
0.533944954,0.535779817,0.537614679,0.539449541,0.541284404,0.543119266,
0.544954128,0.546788991,0.548623853,0.550458716,0.552293578,0.55412844,
0.555963303,0.557798165,0.559633028,0.56146789,0.563302752,0.565137615,
0.566972477,0.568807339,0.570642202,0.572477064,0.574311927,0.576146789,
0.577981651,0.579816514,0.581651376,0.583486239,0.585321101,0.587155963,
0.588990826,0.590825688,0.59266055,0.594495413,0.596330275,0.598165138,
0.6,0.601834862,0.603669725,0.605504587,0.60733945,0.609174312,0.611009174,
0.612844037,0.614678899,0.616513761,0.618348624,0.620183486,0.622018349,
0.623853211,0.625688073,0.627522936,0.629357798,0.631192661,0.633027523,
0.634862385,0.636697248,0.63853211,0.640366972,0.642201835,0.644036697,
0.64587156,0.647706422,0.649541284,0.651376147,0.653211009,0.655045872,
0.656880734,0.658715596,0.660550459,0.662385321,0.664220183,0.666055046,
0.667889908,0.669724771,0.671559633,0.673394495,0.675229358,0.67706422,
0.678899083,0.680733945,0.682568807,0.68440367,0.686238532,0.688073394,
0.689908257,0.691743119,0.693577982,0.695412844,0.697247706,0.699082569,
0.700917431,0.702752294,0.704587156,0.706422018,0.708256881,0.710091743,
0.711926606,0.713761468,0.71559633,0.717431193,0.719266055,0.721100917,
0.72293578,0.724770642,0.726605505,0.728440367,0.730275229,0.732110092,
0.733944954,0.735779817,0.737614679,0.739449541,0.741284404,0.743119266,
0.744954128,0.746788991,0.748623853,0.750458716,0.752293578,0.75412844,
0.755963303,0.757798165,0.759633028,0.76146789,0.763302752,0.765137615,
0.766972477,0.768807339,0.770642202,0.772477064,0.774311927,0.776146789,
0.777981651,0.779816514,0.781651376,0.783486239,0.785321101,0.787155963,
0.788990826,0.790825688,0.79266055,0.794495413,0.796330275,0.798165138,
0.8,0.801834862,0.803669725,0.805504587,0.80733945,0.809174312,0.811009174,
0.812844037,0.814678899,0.816513761,0.818348624,0.820183486,0.822018349,
0.823853211,0.825688073,0.827522936,0.829357798,0.831192661,0.833027523,
0.834862385,0.836697248,0.83853211,0.840366972,0.842201835,0.844036697,
0.84587156,0.847706422,0.849541284,0.851376147,0.853211009,0.855045872,
0.856880734,0.858715596,0.860550459,0.862385321,0.864220183,0.866055046,
0.867889908,0.869724771,0.871559633,0.873394495,0.875229358,0.87706422,
0.878899083,0.880733945,0.882568807,0.88440367,0.886238532,0.888073394,
0.889908257,0.891743119,0.893577982,0.895412844,0.897247706,0.899082569,
0.900917431,0.902752294,0.904587156,0.906422018,0.908256881,0.910091743,
0.911926606,0.913761468,0.91559633,0.917431193,0.919266055,0.921100917,
0.92293578,0.924770642,0.926605505,0.928440367,0.930275229,0.932110092,
0.933944954,0.935779817,0.937614679,0.939449541,0.941284404,0.943119266,
0.944954128,0.946788991,0.948623853,0.950458716,0.952293578,0.95412844,
0.955963303,0.957798165,0.959633028,0.96146789,0.963302752,0.965137615,
0.966972477,0.968807339,0.970642202,0.972477064,0.974311927,0.976146789,
0.977981651,0.979816514,0.981651376,0.983486239,0.985321101,0.987155963,
0.988990826,0.990825688,0.99266055,0.994495413,0.996330275,0.998165138,
1.),(0.,0.36),.UNSPECIFIED.);
#6239=B_SPLINE_SURFACE_WITH_KNOTS('',5,1,((#194484,#194485),(#194486,#194487),
(#194488,#194489),(#194490,#194491),(#194492,#194493),(#194494,#194495),
(#194496,#194497),(#194498,#194499),(#194500,#194501),(#194502,#194503),
(#194504,#194505),(#194506,#194507),(#194508,#194509),(#194510,#194511),
(#194512,#194513),(#194514,#194515),(#194516,#194517),(#194518,#194519),
(#194520,#194521),(#194522,#194523),(#194524,#194525),(#194526,#194527),
(#194528,#194529),(#194530,#194531),(#194532,#194533),(#194534,#194535),
(#194536,#194537),(#194538,#194539),(#194540,#194541),(#194542,#194543),
(#194544,#194545),(#194546,#194547),(#194548,#194549),(#194550,#194551),
(#194552,#194553),(#194554,#194555),(#194556,#194557),(#194558,#194559),
(#194560,#194561),(#194562,#194563),(#194564,#194565),(#194566,#194567),
(#194568,#194569),(#194570,#194571),(#194572,#194573),(#194574,#194575),
(#194576,#194577),(#194578,#194579),(#194580,#194581),(#194582,#194583),
(#194584,#194585),(#194586,#194587),(#194588,#194589),(#194590,#194591),
(#194592,#194593),(#194594,#194595),(#194596,#194597),(#194598,#194599),
(#194600,#194601),(#194602,#194603),(#194604,#194605),(#194606,#194607),
(#194608,#194609),(#194610,#194611),(#194612,#194613),(#194614,#194615),
(#194616,#194617),(#194618,#194619),(#194620,#194621),(#194622,#194623),
(#194624,#194625),(#194626,#194627),(#194628,#194629),(#194630,#194631),
(#194632,#194633),(#194634,#194635),(#194636,#194637),(#194638,#194639),
(#194640,#194641),(#194642,#194643),(#194644,#194645),(#194646,#194647),
(#194648,#194649),(#194650,#194651),(#194652,#194653),(#194654,#194655),
(#194656,#194657),(#194658,#194659),(#194660,#194661),(#194662,#194663),
(#194664,#194665),(#194666,#194667),(#194668,#194669),(#194670,#194671),
(#194672,#194673),(#194674,#194675),(#194676,#194677),(#194678,#194679),
(#194680,#194681),(#194682,#194683),(#194684,#194685),(#194686,#194687),
(#194688,#194689),(#194690,#194691),(#194692,#194693),(#194694,#194695),
(#194696,#194697),(#194698,#194699),(#194700,#194701),(#194702,#194703),
(#194704,#194705),(#194706,#194707),(#194708,#194709),(#194710,#194711),
(#194712,#194713),(#194714,#194715),(#194716,#194717),(#194718,#194719),
(#194720,#194721),(#194722,#194723),(#194724,#194725),(#194726,#194727),
(#194728,#194729),(#194730,#194731),(#194732,#194733),(#194734,#194735),
(#194736,#194737),(#194738,#194739),(#194740,#194741),(#194742,#194743),
(#194744,#194745),(#194746,#194747),(#194748,#194749),(#194750,#194751),
(#194752,#194753),(#194754,#194755),(#194756,#194757),(#194758,#194759),
(#194760,#194761),(#194762,#194763),(#194764,#194765),(#194766,#194767),
(#194768,#194769),(#194770,#194771),(#194772,#194773),(#194774,#194775),
(#194776,#194777),(#194778,#194779),(#194780,#194781),(#194782,#194783),
(#194784,#194785),(#194786,#194787),(#194788,#194789),(#194790,#194791),
(#194792,#194793),(#194794,#194795),(#194796,#194797),(#194798,#194799),
(#194800,#194801),(#194802,#194803),(#194804,#194805),(#194806,#194807),
(#194808,#194809),(#194810,#194811),(#194812,#194813),(#194814,#194815),
(#194816,#194817),(#194818,#194819),(#194820,#194821),(#194822,#194823),
(#194824,#194825),(#194826,#194827),(#194828,#194829),(#194830,#194831),
(#194832,#194833),(#194834,#194835),(#194836,#194837),(#194838,#194839),
(#194840,#194841),(#194842,#194843),(#194844,#194845),(#194846,#194847),
(#194848,#194849),(#194850,#194851),(#194852,#194853),(#194854,#194855),
(#194856,#194857),(#194858,#194859),(#194860,#194861),(#194862,#194863),
(#194864,#194865),(#194866,#194867),(#194868,#194869),(#194870,#194871),
(#194872,#194873),(#194874,#194875),(#194876,#194877),(#194878,#194879),
(#194880,#194881),(#194882,#194883),(#194884,#194885),(#194886,#194887),
(#194888,#194889),(#194890,#194891),(#194892,#194893),(#194894,#194895),
(#194896,#194897),(#194898,#194899),(#194900,#194901),(#194902,#194903),
(#194904,#194905),(#194906,#194907),(#194908,#194909),(#194910,#194911),
(#194912,#194913),(#194914,#194915),(#194916,#194917),(#194918,#194919),
(#194920,#194921),(#194922,#194923),(#194924,#194925),(#194926,#194927),
(#194928,#194929),(#194930,#194931),(#194932,#194933),(#194934,#194935),
(#194936,#194937),(#194938,#194939),(#194940,#194941),(#194942,#194943),
(#194944,#194945),(#194946,#194947),(#194948,#194949),(#194950,#194951),
(#194952,#194953),(#194954,#194955),(#194956,#194957),(#194958,#194959),
(#194960,#194961),(#194962,#194963),(#194964,#194965),(#194966,#194967),
(#194968,#194969),(#194970,#194971),(#194972,#194973),(#194974,#194975),
(#194976,#194977),(#194978,#194979),(#194980,#194981),(#194982,#194983),
(#194984,#194985),(#194986,#194987),(#194988,#194989),(#194990,#194991),
(#194992,#194993),(#194994,#194995),(#194996,#194997),(#194998,#194999),
(#195000,#195001),(#195002,#195003),(#195004,#195005),(#195006,#195007),
(#195008,#195009),(#195010,#195011),(#195012,#195013),(#195014,#195015),
(#195016,#195017),(#195018,#195019),(#195020,#195021),(#195022,#195023),
(#195024,#195025),(#195026,#195027),(#195028,#195029),(#195030,#195031),
(#195032,#195033),(#195034,#195035),(#195036,#195037),(#195038,#195039),
(#195040,#195041),(#195042,#195043),(#195044,#195045),(#195046,#195047),
(#195048,#195049),(#195050,#195051),(#195052,#195053),(#195054,#195055),
(#195056,#195057),(#195058,#195059),(#195060,#195061),(#195062,#195063),
(#195064,#195065),(#195066,#195067),(#195068,#195069),(#195070,#195071),
(#195072,#195073),(#195074,#195075),(#195076,#195077),(#195078,#195079),
(#195080,#195081),(#195082,#195083),(#195084,#195085),(#195086,#195087),
(#195088,#195089),(#195090,#195091),(#195092,#195093),(#195094,#195095),
(#195096,#195097),(#195098,#195099),(#195100,#195101),(#195102,#195103),
(#195104,#195105),(#195106,#195107),(#195108,#195109),(#195110,#195111),
(#195112,#195113),(#195114,#195115),(#195116,#195117),(#195118,#195119),
(#195120,#195121),(#195122,#195123),(#195124,#195125),(#195126,#195127),
(#195128,#195129),(#195130,#195131),(#195132,#195133),(#195134,#195135),
(#195136,#195137),(#195138,#195139),(#195140,#195141),(#195142,#195143),
(#195144,#195145),(#195146,#195147),(#195148,#195149),(#195150,#195151),
(#195152,#195153),(#195154,#195155),(#195156,#195157),(#195158,#195159),
(#195160,#195161),(#195162,#195163),(#195164,#195165),(#195166,#195167),
(#195168,#195169),(#195170,#195171),(#195172,#195173),(#195174,#195175),
(#195176,#195177),(#195178,#195179),(#195180,#195181),(#195182,#195183),
(#195184,#195185),(#195186,#195187),(#195188,#195189),(#195190,#195191),
(#195192,#195193),(#195194,#195195),(#195196,#195197),(#195198,#195199),
(#195200,#195201),(#195202,#195203),(#195204,#195205),(#195206,#195207),
(#195208,#195209),(#195210,#195211),(#195212,#195213),(#195214,#195215),
(#195216,#195217),(#195218,#195219),(#195220,#195221),(#195222,#195223),
(#195224,#195225),(#195226,#195227),(#195228,#195229),(#195230,#195231),
(#195232,#195233),(#195234,#195235),(#195236,#195237),(#195238,#195239),
(#195240,#195241),(#195242,#195243),(#195244,#195245),(#195246,#195247),
(#195248,#195249),(#195250,#195251),(#195252,#195253),(#195254,#195255),
(#195256,#195257),(#195258,#195259),(#195260,#195261),(#195262,#195263),
(#195264,#195265),(#195266,#195267),(#195268,#195269),(#195270,#195271),
(#195272,#195273),(#195274,#195275),(#195276,#195277),(#195278,#195279),
(#195280,#195281),(#195282,#195283),(#195284,#195285),(#195286,#195287),
(#195288,#195289),(#195290,#195291),(#195292,#195293),(#195294,#195295),
(#195296,#195297),(#195298,#195299),(#195300,#195301),(#195302,#195303),
(#195304,#195305),(#195306,#195307),(#195308,#195309),(#195310,#195311),
(#195312,#195313),(#195314,#195315),(#195316,#195317),(#195318,#195319),
(#195320,#195321),(#195322,#195323),(#195324,#195325),(#195326,#195327),
(#195328,#195329),(#195330,#195331),(#195332,#195333),(#195334,#195335),
(#195336,#195337),(#195338,#195339),(#195340,#195341),(#195342,#195343),
(#195344,#195345),(#195346,#195347),(#195348,#195349),(#195350,#195351),
(#195352,#195353),(#195354,#195355),(#195356,#195357),(#195358,#195359),
(#195360,#195361),(#195362,#195363),(#195364,#195365),(#195366,#195367),
(#195368,#195369),(#195370,#195371),(#195372,#195373),(#195374,#195375),
(#195376,#195377),(#195378,#195379),(#195380,#195381),(#195382,#195383),
(#195384,#195385),(#195386,#195387),(#195388,#195389),(#195390,#195391),
(#195392,#195393),(#195394,#195395),(#195396,#195397),(#195398,#195399),
(#195400,#195401),(#195402,#195403),(#195404,#195405),(#195406,#195407),
(#195408,#195409),(#195410,#195411),(#195412,#195413),(#195414,#195415),
(#195416,#195417),(#195418,#195419),(#195420,#195421),(#195422,#195423),
(#195424,#195425),(#195426,#195427)),.UNSPECIFIED.,.F.,.F.,.F.,(6,1,1,1,
1,1,1,1,1,1,1,1,1,1,1,1,1,1,1,1,1,1,1,1,1,1,1,1,1,1,1,1,1,1,1,1,1,1,1,1,
1,1,1,1,1,1,1,1,1,1,1,1,1,1,1,1,1,1,1,1,1,1,1,1,1,1,1,1,1,1,1,1,1,1,1,1,
1,1,1,1,1,1,1,1,1,1,1,1,1,1,1,1,1,1,1,1,1,1,1,1,1,1,1,1,1,1,1,1,1,1,1,1,
1,1,1,1,1,1,1,1,1,1,1,1,1,1,1,1,1,1,1,1,1,1,1,1,1,1,1,1,1,1,1,1,1,1,1,1,
1,1,1,1,1,1,1,1,1,1,1,1,1,1,1,1,1,1,1,1,1,1,1,1,1,1,1,1,1,1,1,1,1,1,1,1,
1,1,1,1,1,1,1,1,1,1,1,1,1,1,1,1,1,1,1,1,1,1,1,1,1,1,1,1,1,1,1,1,1,1,1,1,
1,1,1,1,1,1,1,1,1,1,1,1,1,1,1,1,1,1,1,1,1,1,1,1,1,1,1,1,1,1,1,1,1,1,1,1,
1,1,1,1,1,1,1,1,1,1,1,1,1,1,1,1,1,1,1,1,1,1,1,1,1,1,1,1,1,1,1,1,1,1,1,1,
1,1,1,1,1,1,1,1,1,1,1,1,1,1,1,1,1,1,1,1,1,1,1,1,1,1,1,1,1,1,1,1,1,1,1,1,
1,1,1,1,1,1,1,1,1,1,1,1,1,1,1,1,1,1,1,1,1,1,1,1,1,1,1,1,1,1,1,1,1,1,1,1,
1,1,1,1,1,1,1,1,1,1,1,1,1,1,1,1,1,1,1,1,1,1,1,1,1,1,1,1,1,1,1,1,1,1,1,1,
1,1,1,1,1,1,1,1,1,1,1,1,1,1,1,1,1,1,1,1,1,1,1,1,1,1,1,1,1,1,1,1,1,1,1,1,
1,1,1,1,1,1,1,1,1,1,1,1,1,1,1,1,1,1,1,1,1,1,1,1,1,1,1,1,1,1,1,6),(2,2),
(0.143172103,0.144954128,0.146788991,0.148623853,0.150458716,0.152293578,
0.15412844,0.155963303,0.157798165,0.159633028,0.16146789,0.163302752,0.165137615,
0.166972477,0.168807339,0.170642202,0.172477064,0.174311927,0.176146789,
0.177981651,0.179816514,0.181651376,0.183486239,0.185321101,0.187155963,
0.188990826,0.190825688,0.19266055,0.194495413,0.196330275,0.198165138,
0.2,0.201834862,0.203669725,0.205504587,0.20733945,0.209174312,0.211009174,
0.212844037,0.214678899,0.216513761,0.218348624,0.220183486,0.222018349,
0.223853211,0.225688073,0.227522936,0.229357798,0.231192661,0.233027523,
0.234862385,0.236697248,0.23853211,0.240366972,0.242201835,0.244036697,
0.24587156,0.247706422,0.249541284,0.251376147,0.253211009,0.255045872,
0.256880734,0.258715596,0.260550459,0.262385321,0.264220183,0.266055046,
0.267889908,0.269724771,0.271559633,0.273394495,0.275229358,0.27706422,
0.278899083,0.280733945,0.282568807,0.28440367,0.286238532,0.288073394,
0.289908257,0.291743119,0.293577982,0.295412844,0.297247706,0.299082569,
0.300917431,0.302752294,0.304587156,0.306422018,0.308256881,0.310091743,
0.311926606,0.313761468,0.31559633,0.317431193,0.319266055,0.321100917,
0.32293578,0.324770642,0.326605505,0.328440367,0.330275229,0.332110092,
0.333944954,0.335779817,0.337614679,0.339449541,0.341284404,0.343119266,
0.344954128,0.346788991,0.348623853,0.350458716,0.352293578,0.35412844,
0.355963303,0.357798165,0.359633028,0.36146789,0.363302752,0.365137615,
0.366972477,0.368807339,0.370642202,0.372477064,0.374311927,0.376146789,
0.377981651,0.379816514,0.381651376,0.383486239,0.385321101,0.387155963,
0.388990826,0.390825688,0.39266055,0.394495413,0.396330275,0.398165138,
0.4,0.401834862,0.403669725,0.405504587,0.40733945,0.409174312,0.411009174,
0.412844037,0.414678899,0.416513761,0.418348624,0.420183486,0.422018349,
0.423853211,0.425688073,0.427522936,0.429357798,0.431192661,0.433027523,
0.434862385,0.436697248,0.43853211,0.440366972,0.442201835,0.444036697,
0.44587156,0.447706422,0.449541284,0.451376147,0.453211009,0.455045872,
0.456880734,0.458715596,0.460550459,0.462385321,0.464220183,0.466055046,
0.467889908,0.469724771,0.471559633,0.473394495,0.475229358,0.47706422,
0.478899083,0.480733945,0.482568807,0.48440367,0.486238532,0.488073394,
0.489908257,0.491743119,0.493577982,0.495412844,0.497247706,0.499082569,
0.500917431,0.502752294,0.504587156,0.506422018,0.508256881,0.510091743,
0.511926606,0.513761468,0.51559633,0.517431193,0.519266055,0.521100917,
0.52293578,0.524770642,0.526605505,0.528440367,0.530275229,0.532110092,
0.533944954,0.535779817,0.537614679,0.539449541,0.541284404,0.543119266,
0.544954128,0.546788991,0.548623853,0.550458716,0.552293578,0.55412844,
0.555963303,0.557798165,0.559633028,0.56146789,0.563302752,0.565137615,
0.566972477,0.568807339,0.570642202,0.572477064,0.574311927,0.576146789,
0.577981651,0.579816514,0.581651376,0.583486239,0.585321101,0.587155963,
0.588990826,0.590825688,0.59266055,0.594495413,0.596330275,0.598165138,
0.6,0.601834862,0.603669725,0.605504587,0.60733945,0.609174312,0.611009174,
0.612844037,0.614678899,0.616513761,0.618348624,0.620183486,0.622018349,
0.623853211,0.625688073,0.627522936,0.629357798,0.631192661,0.633027523,
0.634862385,0.636697248,0.63853211,0.640366972,0.642201835,0.644036697,
0.64587156,0.647706422,0.649541284,0.651376147,0.653211009,0.655045872,
0.656880734,0.658715596,0.660550459,0.662385321,0.664220183,0.666055046,
0.667889908,0.669724771,0.671559633,0.673394495,0.675229358,0.67706422,
0.678899083,0.680733945,0.682568807,0.68440367,0.686238532,0.688073394,
0.689908257,0.691743119,0.693577982,0.695412844,0.697247706,0.699082569,
0.700917431,0.702752294,0.704587156,0.706422018,0.708256881,0.710091743,
0.711926606,0.713761468,0.71559633,0.717431193,0.719266055,0.721100917,
0.72293578,0.724770642,0.726605505,0.728440367,0.730275229,0.732110092,
0.733944954,0.735779817,0.737614679,0.739449541,0.741284404,0.743119266,
0.744954128,0.746788991,0.748623853,0.750458716,0.752293578,0.75412844,
0.755963303,0.757798165,0.759633028,0.76146789,0.763302752,0.765137615,
0.766972477,0.768807339,0.770642202,0.772477064,0.774311927,0.776146789,
0.777981651,0.779816514,0.781651376,0.783486239,0.785321101,0.787155963,
0.788990826,0.790825688,0.79266055,0.794495413,0.796330275,0.798165138,
0.8,0.801834862,0.803669725,0.805504587,0.80733945,0.809174312,0.811009174,
0.812844037,0.814678899,0.816513761,0.818348624,0.820183486,0.822018349,
0.823853211,0.825688073,0.827522936,0.829357798,0.831192661,0.833027523,
0.834862385,0.836697248,0.83853211,0.840366972,0.842201835,0.844036697,
0.84587156,0.847706422,0.849541284,0.851376147,0.853211009,0.855045872,
0.856880734,0.858715596,0.860550459,0.862385321,0.864220183,0.866055046,
0.867889908,0.869724771,0.871559633,0.873394495,0.875229358,0.87706422,
0.878899083,0.880733945,0.882568807,0.88440367,0.886238532,0.888073394,
0.889908257,0.891743119,0.893577982,0.895412844,0.897247706,0.899082569,
0.900917431,0.902752294,0.904587156,0.906422018,0.908256881,0.910091743,
0.911926606,0.913761468,0.91559633,0.917431193,0.919266055,0.921100917,
0.92293578,0.924770642,0.926605505,0.928440367,0.930275229,0.932110092,
0.933944954,0.935779817,0.937614679,0.939449541,0.941284404,0.943119266,
0.944954128,0.946788991,0.948623853,0.950458716,0.952293578,0.95412844,
0.955963303,0.957798165,0.959633028,0.96146789,0.963302752,0.965137615,
0.966972477,0.968807339,0.970642202,0.972477064,0.974311927,0.976146789,
0.977981651,0.979816514,0.981651376,0.983486239,0.985321101,0.987155963,
0.988990826,0.990825688,0.99266055,0.994495413,0.996330275,0.998165138,
1.),(0.,0.36),.UNSPECIFIED.);
#6240=B_SPLINE_SURFACE_WITH_KNOTS('',5,1,((#196054,#196055),(#196056,#196057),
(#196058,#196059),(#196060,#196061),(#196062,#196063),(#196064,#196065),
(#196066,#196067),(#196068,#196069),(#196070,#196071),(#196072,#196073),
(#196074,#196075),(#196076,#196077),(#196078,#196079),(#196080,#196081),
(#196082,#196083),(#196084,#196085),(#196086,#196087),(#196088,#196089),
(#196090,#196091),(#196092,#196093),(#196094,#196095),(#196096,#196097),
(#196098,#196099),(#196100,#196101),(#196102,#196103),(#196104,#196105),
(#196106,#196107),(#196108,#196109),(#196110,#196111),(#196112,#196113),
(#196114,#196115),(#196116,#196117),(#196118,#196119),(#196120,#196121),
(#196122,#196123),(#196124,#196125),(#196126,#196127),(#196128,#196129),
(#196130,#196131),(#196132,#196133),(#196134,#196135),(#196136,#196137),
(#196138,#196139),(#196140,#196141),(#196142,#196143),(#196144,#196145),
(#196146,#196147),(#196148,#196149),(#196150,#196151),(#196152,#196153),
(#196154,#196155),(#196156,#196157),(#196158,#196159),(#196160,#196161),
(#196162,#196163),(#196164,#196165),(#196166,#196167),(#196168,#196169),
(#196170,#196171),(#196172,#196173),(#196174,#196175),(#196176,#196177),
(#196178,#196179),(#196180,#196181),(#196182,#196183),(#196184,#196185),
(#196186,#196187),(#196188,#196189),(#196190,#196191),(#196192,#196193),
(#196194,#196195),(#196196,#196197),(#196198,#196199),(#196200,#196201),
(#196202,#196203),(#196204,#196205),(#196206,#196207),(#196208,#196209),
(#196210,#196211),(#196212,#196213),(#196214,#196215),(#196216,#196217),
(#196218,#196219),(#196220,#196221),(#196222,#196223),(#196224,#196225),
(#196226,#196227),(#196228,#196229),(#196230,#196231),(#196232,#196233),
(#196234,#196235),(#196236,#196237),(#196238,#196239),(#196240,#196241),
(#196242,#196243),(#196244,#196245),(#196246,#196247),(#196248,#196249),
(#196250,#196251),(#196252,#196253),(#196254,#196255),(#196256,#196257),
(#196258,#196259),(#196260,#196261),(#196262,#196263),(#196264,#196265),
(#196266,#196267),(#196268,#196269),(#196270,#196271),(#196272,#196273),
(#196274,#196275),(#196276,#196277),(#196278,#196279),(#196280,#196281),
(#196282,#196283),(#196284,#196285),(#196286,#196287),(#196288,#196289),
(#196290,#196291),(#196292,#196293),(#196294,#196295),(#196296,#196297),
(#196298,#196299),(#196300,#196301),(#196302,#196303),(#196304,#196305),
(#196306,#196307),(#196308,#196309),(#196310,#196311),(#196312,#196313),
(#196314,#196315),(#196316,#196317),(#196318,#196319),(#196320,#196321),
(#196322,#196323),(#196324,#196325),(#196326,#196327),(#196328,#196329),
(#196330,#196331),(#196332,#196333),(#196334,#196335),(#196336,#196337),
(#196338,#196339),(#196340,#196341),(#196342,#196343),(#196344,#196345),
(#196346,#196347),(#196348,#196349),(#196350,#196351),(#196352,#196353),
(#196354,#196355),(#196356,#196357),(#196358,#196359),(#196360,#196361),
(#196362,#196363),(#196364,#196365),(#196366,#196367),(#196368,#196369),
(#196370,#196371),(#196372,#196373),(#196374,#196375),(#196376,#196377),
(#196378,#196379),(#196380,#196381),(#196382,#196383),(#196384,#196385),
(#196386,#196387),(#196388,#196389),(#196390,#196391),(#196392,#196393),
(#196394,#196395),(#196396,#196397),(#196398,#196399),(#196400,#196401),
(#196402,#196403),(#196404,#196405),(#196406,#196407),(#196408,#196409),
(#196410,#196411),(#196412,#196413),(#196414,#196415),(#196416,#196417),
(#196418,#196419),(#196420,#196421),(#196422,#196423),(#196424,#196425),
(#196426,#196427),(#196428,#196429),(#196430,#196431),(#196432,#196433),
(#196434,#196435),(#196436,#196437),(#196438,#196439),(#196440,#196441),
(#196442,#196443),(#196444,#196445),(#196446,#196447),(#196448,#196449),
(#196450,#196451),(#196452,#196453),(#196454,#196455),(#196456,#196457),
(#196458,#196459),(#196460,#196461),(#196462,#196463),(#196464,#196465),
(#196466,#196467),(#196468,#196469),(#196470,#196471),(#196472,#196473),
(#196474,#196475),(#196476,#196477),(#196478,#196479),(#196480,#196481),
(#196482,#196483),(#196484,#196485),(#196486,#196487),(#196488,#196489),
(#196490,#196491),(#196492,#196493),(#196494,#196495),(#196496,#196497),
(#196498,#196499),(#196500,#196501),(#196502,#196503),(#196504,#196505),
(#196506,#196507),(#196508,#196509),(#196510,#196511),(#196512,#196513),
(#196514,#196515),(#196516,#196517),(#196518,#196519),(#196520,#196521),
(#196522,#196523),(#196524,#196525),(#196526,#196527),(#196528,#196529),
(#196530,#196531),(#196532,#196533),(#196534,#196535),(#196536,#196537),
(#196538,#196539),(#196540,#196541),(#196542,#196543),(#196544,#196545),
(#196546,#196547),(#196548,#196549),(#196550,#196551),(#196552,#196553),
(#196554,#196555),(#196556,#196557),(#196558,#196559),(#196560,#196561),
(#196562,#196563),(#196564,#196565),(#196566,#196567),(#196568,#196569),
(#196570,#196571),(#196572,#196573),(#196574,#196575),(#196576,#196577),
(#196578,#196579),(#196580,#196581),(#196582,#196583),(#196584,#196585),
(#196586,#196587),(#196588,#196589),(#196590,#196591),(#196592,#196593),
(#196594,#196595),(#196596,#196597),(#196598,#196599),(#196600,#196601),
(#196602,#196603),(#196604,#196605),(#196606,#196607),(#196608,#196609),
(#196610,#196611),(#196612,#196613),(#196614,#196615),(#196616,#196617),
(#196618,#196619),(#196620,#196621),(#196622,#196623),(#196624,#196625),
(#196626,#196627),(#196628,#196629),(#196630,#196631),(#196632,#196633),
(#196634,#196635),(#196636,#196637),(#196638,#196639),(#196640,#196641),
(#196642,#196643),(#196644,#196645),(#196646,#196647),(#196648,#196649),
(#196650,#196651),(#196652,#196653),(#196654,#196655),(#196656,#196657),
(#196658,#196659),(#196660,#196661),(#196662,#196663),(#196664,#196665),
(#196666,#196667),(#196668,#196669),(#196670,#196671),(#196672,#196673),
(#196674,#196675),(#196676,#196677),(#196678,#196679),(#196680,#196681),
(#196682,#196683),(#196684,#196685),(#196686,#196687),(#196688,#196689),
(#196690,#196691),(#196692,#196693),(#196694,#196695),(#196696,#196697),
(#196698,#196699),(#196700,#196701),(#196702,#196703),(#196704,#196705),
(#196706,#196707),(#196708,#196709),(#196710,#196711),(#196712,#196713),
(#196714,#196715),(#196716,#196717),(#196718,#196719),(#196720,#196721),
(#196722,#196723),(#196724,#196725),(#196726,#196727),(#196728,#196729),
(#196730,#196731),(#196732,#196733),(#196734,#196735),(#196736,#196737),
(#196738,#196739),(#196740,#196741),(#196742,#196743),(#196744,#196745),
(#196746,#196747),(#196748,#196749),(#196750,#196751),(#196752,#196753),
(#196754,#196755),(#196756,#196757),(#196758,#196759),(#196760,#196761),
(#196762,#196763),(#196764,#196765),(#196766,#196767),(#196768,#196769),
(#196770,#196771),(#196772,#196773),(#196774,#196775),(#196776,#196777),
(#196778,#196779),(#196780,#196781),(#196782,#196783),(#196784,#196785),
(#196786,#196787),(#196788,#196789),(#196790,#196791),(#196792,#196793),
(#196794,#196795),(#196796,#196797),(#196798,#196799),(#196800,#196801),
(#196802,#196803),(#196804,#196805),(#196806,#196807),(#196808,#196809),
(#196810,#196811),(#196812,#196813),(#196814,#196815),(#196816,#196817),
(#196818,#196819),(#196820,#196821),(#196822,#196823),(#196824,#196825),
(#196826,#196827),(#196828,#196829),(#196830,#196831),(#196832,#196833),
(#196834,#196835),(#196836,#196837),(#196838,#196839),(#196840,#196841),
(#196842,#196843),(#196844,#196845),(#196846,#196847),(#196848,#196849),
(#196850,#196851),(#196852,#196853),(#196854,#196855),(#196856,#196857),
(#196858,#196859),(#196860,#196861),(#196862,#196863),(#196864,#196865),
(#196866,#196867),(#196868,#196869),(#196870,#196871),(#196872,#196873),
(#196874,#196875),(#196876,#196877),(#196878,#196879),(#196880,#196881),
(#196882,#196883),(#196884,#196885),(#196886,#196887),(#196888,#196889),
(#196890,#196891),(#196892,#196893),(#196894,#196895),(#196896,#196897),
(#196898,#196899),(#196900,#196901),(#196902,#196903),(#196904,#196905),
(#196906,#196907),(#196908,#196909),(#196910,#196911),(#196912,#196913),
(#196914,#196915),(#196916,#196917),(#196918,#196919),(#196920,#196921),
(#196922,#196923),(#196924,#196925),(#196926,#196927),(#196928,#196929),
(#196930,#196931),(#196932,#196933),(#196934,#196935),(#196936,#196937),
(#196938,#196939),(#196940,#196941),(#196942,#196943),(#196944,#196945),
(#196946,#196947),(#196948,#196949),(#196950,#196951),(#196952,#196953),
(#196954,#196955),(#196956,#196957),(#196958,#196959),(#196960,#196961),
(#196962,#196963),(#196964,#196965),(#196966,#196967),(#196968,#196969),
(#196970,#196971),(#196972,#196973),(#196974,#196975),(#196976,#196977),
(#196978,#196979),(#196980,#196981),(#196982,#196983),(#196984,#196985),
(#196986,#196987),(#196988,#196989),(#196990,#196991),(#196992,#196993),
(#196994,#196995),(#196996,#196997)),.UNSPECIFIED.,.F.,.F.,.F.,(6,1,1,1,
1,1,1,1,1,1,1,1,1,1,1,1,1,1,1,1,1,1,1,1,1,1,1,1,1,1,1,1,1,1,1,1,1,1,1,1,
1,1,1,1,1,1,1,1,1,1,1,1,1,1,1,1,1,1,1,1,1,1,1,1,1,1,1,1,1,1,1,1,1,1,1,1,
1,1,1,1,1,1,1,1,1,1,1,1,1,1,1,1,1,1,1,1,1,1,1,1,1,1,1,1,1,1,1,1,1,1,1,1,
1,1,1,1,1,1,1,1,1,1,1,1,1,1,1,1,1,1,1,1,1,1,1,1,1,1,1,1,1,1,1,1,1,1,1,1,
1,1,1,1,1,1,1,1,1,1,1,1,1,1,1,1,1,1,1,1,1,1,1,1,1,1,1,1,1,1,1,1,1,1,1,1,
1,1,1,1,1,1,1,1,1,1,1,1,1,1,1,1,1,1,1,1,1,1,1,1,1,1,1,1,1,1,1,1,1,1,1,1,
1,1,1,1,1,1,1,1,1,1,1,1,1,1,1,1,1,1,1,1,1,1,1,1,1,1,1,1,1,1,1,1,1,1,1,1,
1,1,1,1,1,1,1,1,1,1,1,1,1,1,1,1,1,1,1,1,1,1,1,1,1,1,1,1,1,1,1,1,1,1,1,1,
1,1,1,1,1,1,1,1,1,1,1,1,1,1,1,1,1,1,1,1,1,1,1,1,1,1,1,1,1,1,1,1,1,1,1,1,
1,1,1,1,1,1,1,1,1,1,1,1,1,1,1,1,1,1,1,1,1,1,1,1,1,1,1,1,1,1,1,1,1,1,1,1,
1,1,1,1,1,1,1,1,1,1,1,1,1,1,1,1,1,1,1,1,1,1,1,1,1,1,1,1,1,1,1,1,1,1,1,1,
1,1,1,1,1,1,1,1,1,1,1,1,1,1,1,1,1,1,1,1,1,1,1,1,1,1,1,1,1,1,1,1,1,1,1,1,
1,1,1,1,1,1,1,1,1,1,1,1,1,1,1,1,1,1,1,1,1,1,1,1,1,1,1,1,1,1,1,6),(2,2),
(-1.,-0.998165138,-0.996330275,-0.994495413,-0.99266055,-0.990825688,-0.988990826,
-0.987155963,-0.985321101,-0.983486239,-0.981651376,-0.979816514,-0.977981651,
-0.976146789,-0.974311927,-0.972477064,-0.970642202,-0.968807339,-0.966972477,
-0.965137615,-0.963302752,-0.96146789,-0.959633028,-0.957798165,-0.955963303,
-0.95412844,-0.952293578,-0.950458716,-0.948623853,-0.946788991,-0.944954128,
-0.943119266,-0.941284404,-0.939449541,-0.937614679,-0.935779817,-0.933944954,
-0.932110092,-0.930275229,-0.928440367,-0.926605505,-0.924770642,-0.92293578,
-0.921100917,-0.919266055,-0.917431193,-0.91559633,-0.913761468,-0.911926606,
-0.910091743,-0.908256881,-0.906422018,-0.904587156,-0.902752294,-0.900917431,
-0.899082569,-0.897247706,-0.895412844,-0.893577982,-0.891743119,-0.889908257,
-0.888073394,-0.886238532,-0.88440367,-0.882568807,-0.880733945,-0.878899083,
-0.87706422,-0.875229358,-0.873394495,-0.871559633,-0.869724771,-0.867889908,
-0.866055046,-0.864220183,-0.862385321,-0.860550459,-0.858715596,-0.856880734,
-0.855045872,-0.853211009,-0.851376147,-0.849541284,-0.847706422,-0.84587156,
-0.844036697,-0.842201835,-0.840366972,-0.83853211,-0.836697248,-0.834862385,
-0.833027523,-0.831192661,-0.829357798,-0.827522936,-0.825688073,-0.823853211,
-0.822018349,-0.820183486,-0.818348624,-0.816513761,-0.814678899,-0.812844037,
-0.811009174,-0.809174312,-0.80733945,-0.805504587,-0.803669725,-0.801834862,
-0.8,-0.798165138,-0.796330275,-0.794495413,-0.79266055,-0.790825688,-0.788990826,
-0.787155963,-0.785321101,-0.783486239,-0.781651376,-0.779816514,-0.777981651,
-0.776146789,-0.774311927,-0.772477064,-0.770642202,-0.768807339,-0.766972477,
-0.765137615,-0.763302752,-0.76146789,-0.759633028,-0.757798165,-0.755963303,
-0.75412844,-0.752293578,-0.750458716,-0.748623853,-0.746788991,-0.744954128,
-0.743119266,-0.741284404,-0.739449541,-0.737614679,-0.735779817,-0.733944954,
-0.732110092,-0.730275229,-0.728440367,-0.726605505,-0.724770642,-0.72293578,
-0.721100917,-0.719266055,-0.717431193,-0.71559633,-0.713761468,-0.711926606,
-0.710091743,-0.708256881,-0.706422018,-0.704587156,-0.702752294,-0.700917431,
-0.699082569,-0.697247706,-0.695412844,-0.693577982,-0.691743119,-0.689908257,
-0.688073394,-0.686238532,-0.68440367,-0.682568807,-0.680733945,-0.678899083,
-0.67706422,-0.675229358,-0.673394495,-0.671559633,-0.669724771,-0.667889908,
-0.666055046,-0.664220183,-0.662385321,-0.660550459,-0.658715596,-0.656880734,
-0.655045872,-0.653211009,-0.651376147,-0.649541284,-0.647706422,-0.64587156,
-0.644036697,-0.642201835,-0.640366972,-0.63853211,-0.636697248,-0.634862385,
-0.633027523,-0.631192661,-0.629357798,-0.627522936,-0.625688073,-0.623853211,
-0.622018349,-0.620183486,-0.618348624,-0.616513761,-0.614678899,-0.612844037,
-0.611009174,-0.609174312,-0.60733945,-0.605504587,-0.603669725,-0.601834862,
-0.6,-0.598165138,-0.596330275,-0.594495413,-0.59266055,-0.590825688,-0.588990826,
-0.587155963,-0.585321101,-0.583486239,-0.581651376,-0.579816514,-0.577981651,
-0.576146789,-0.574311927,-0.572477064,-0.570642202,-0.568807339,-0.566972477,
-0.565137615,-0.563302752,-0.56146789,-0.559633028,-0.557798165,-0.555963303,
-0.55412844,-0.552293578,-0.550458716,-0.548623853,-0.546788991,-0.544954128,
-0.543119266,-0.541284404,-0.539449541,-0.537614679,-0.535779817,-0.533944954,
-0.532110092,-0.530275229,-0.528440367,-0.526605505,-0.524770642,-0.52293578,
-0.521100917,-0.519266055,-0.517431193,-0.51559633,-0.513761468,-0.511926606,
-0.510091743,-0.508256881,-0.506422018,-0.504587156,-0.502752294,-0.500917431,
-0.499082569,-0.497247706,-0.495412844,-0.493577982,-0.491743119,-0.489908257,
-0.488073394,-0.486238532,-0.48440367,-0.482568807,-0.480733945,-0.478899083,
-0.47706422,-0.475229358,-0.473394495,-0.471559633,-0.469724771,-0.467889908,
-0.466055046,-0.464220183,-0.462385321,-0.460550459,-0.458715596,-0.456880734,
-0.455045872,-0.453211009,-0.451376147,-0.449541284,-0.447706422,-0.44587156,
-0.444036697,-0.442201835,-0.440366972,-0.43853211,-0.436697248,-0.434862385,
-0.433027523,-0.431192661,-0.429357798,-0.427522936,-0.425688073,-0.423853211,
-0.422018349,-0.420183486,-0.418348624,-0.416513761,-0.414678899,-0.412844037,
-0.411009174,-0.409174312,-0.40733945,-0.405504587,-0.403669725,-0.401834862,
-0.4,-0.398165138,-0.396330275,-0.394495413,-0.39266055,-0.390825688,-0.388990826,
-0.387155963,-0.385321101,-0.383486239,-0.381651376,-0.379816514,-0.377981651,
-0.376146789,-0.374311927,-0.372477064,-0.370642202,-0.368807339,-0.366972477,
-0.365137615,-0.363302752,-0.36146789,-0.359633028,-0.357798165,-0.355963303,
-0.35412844,-0.352293578,-0.350458716,-0.348623853,-0.346788991,-0.344954128,
-0.343119266,-0.341284404,-0.339449541,-0.337614679,-0.335779817,-0.333944954,
-0.332110092,-0.330275229,-0.328440367,-0.326605505,-0.324770642,-0.32293578,
-0.321100917,-0.319266055,-0.317431193,-0.31559633,-0.313761468,-0.311926606,
-0.310091743,-0.308256881,-0.306422018,-0.304587156,-0.302752294,-0.300917431,
-0.299082569,-0.297247706,-0.295412844,-0.293577982,-0.291743119,-0.289908257,
-0.288073394,-0.286238532,-0.28440367,-0.282568807,-0.280733945,-0.278899083,
-0.27706422,-0.275229358,-0.273394495,-0.271559633,-0.269724771,-0.267889908,
-0.266055046,-0.264220183,-0.262385321,-0.260550459,-0.258715596,-0.256880734,
-0.255045872,-0.253211009,-0.251376147,-0.249541284,-0.247706422,-0.24587156,
-0.244036697,-0.242201835,-0.240366972,-0.23853211,-0.236697248,-0.234862385,
-0.233027523,-0.231192661,-0.229357798,-0.227522936,-0.225688073,-0.223853211,
-0.222018349,-0.220183486,-0.218348624,-0.216513761,-0.214678899,-0.212844037,
-0.211009174,-0.209174312,-0.20733945,-0.205504587,-0.203669725,-0.201834862,
-0.2,-0.198165138,-0.196330275,-0.194495413,-0.19266055,-0.190825688,-0.188990826,
-0.187155963,-0.185321101,-0.183486239,-0.181651376,-0.179816514,-0.177981651,
-0.176146789,-0.174311927,-0.172477064,-0.170642202,-0.168807339,-0.166972477,
-0.165137615,-0.163302752,-0.16146789,-0.159633028,-0.157798165,-0.155963303,
-0.15412844,-0.152293578,-0.150458716,-0.148623853,-0.146788991,-0.144954128,
-0.143172103),(0.,0.36),.UNSPECIFIED.);
#6241=B_SPLINE_SURFACE_WITH_KNOTS('',5,1,((#197960,#197961),(#197962,#197963),
(#197964,#197965),(#197966,#197967),(#197968,#197969),(#197970,#197971),
(#197972,#197973),(#197974,#197975),(#197976,#197977),(#197978,#197979),
(#197980,#197981),(#197982,#197983),(#197984,#197985),(#197986,#197987),
(#197988,#197989),(#197990,#197991),(#197992,#197993),(#197994,#197995),
(#197996,#197997),(#197998,#197999),(#198000,#198001),(#198002,#198003),
(#198004,#198005),(#198006,#198007),(#198008,#198009),(#198010,#198011),
(#198012,#198013),(#198014,#198015),(#198016,#198017),(#198018,#198019),
(#198020,#198021),(#198022,#198023),(#198024,#198025),(#198026,#198027),
(#198028,#198029),(#198030,#198031),(#198032,#198033),(#198034,#198035),
(#198036,#198037),(#198038,#198039),(#198040,#198041),(#198042,#198043),
(#198044,#198045),(#198046,#198047),(#198048,#198049),(#198050,#198051),
(#198052,#198053),(#198054,#198055),(#198056,#198057),(#198058,#198059),
(#198060,#198061),(#198062,#198063),(#198064,#198065),(#198066,#198067),
(#198068,#198069),(#198070,#198071),(#198072,#198073),(#198074,#198075),
(#198076,#198077),(#198078,#198079),(#198080,#198081),(#198082,#198083),
(#198084,#198085),(#198086,#198087),(#198088,#198089),(#198090,#198091),
(#198092,#198093),(#198094,#198095),(#198096,#198097),(#198098,#198099),
(#198100,#198101),(#198102,#198103),(#198104,#198105),(#198106,#198107),
(#198108,#198109),(#198110,#198111),(#198112,#198113),(#198114,#198115),
(#198116,#198117),(#198118,#198119),(#198120,#198121),(#198122,#198123),
(#198124,#198125),(#198126,#198127),(#198128,#198129),(#198130,#198131),
(#198132,#198133),(#198134,#198135),(#198136,#198137),(#198138,#198139),
(#198140,#198141),(#198142,#198143),(#198144,#198145),(#198146,#198147),
(#198148,#198149),(#198150,#198151),(#198152,#198153),(#198154,#198155),
(#198156,#198157),(#198158,#198159),(#198160,#198161),(#198162,#198163),
(#198164,#198165),(#198166,#198167),(#198168,#198169),(#198170,#198171),
(#198172,#198173),(#198174,#198175),(#198176,#198177),(#198178,#198179),
(#198180,#198181),(#198182,#198183),(#198184,#198185),(#198186,#198187),
(#198188,#198189),(#198190,#198191),(#198192,#198193),(#198194,#198195),
(#198196,#198197),(#198198,#198199),(#198200,#198201),(#198202,#198203),
(#198204,#198205),(#198206,#198207),(#198208,#198209),(#198210,#198211),
(#198212,#198213),(#198214,#198215),(#198216,#198217),(#198218,#198219),
(#198220,#198221),(#198222,#198223),(#198224,#198225),(#198226,#198227),
(#198228,#198229),(#198230,#198231),(#198232,#198233),(#198234,#198235),
(#198236,#198237),(#198238,#198239),(#198240,#198241),(#198242,#198243),
(#198244,#198245),(#198246,#198247),(#198248,#198249),(#198250,#198251),
(#198252,#198253),(#198254,#198255),(#198256,#198257),(#198258,#198259),
(#198260,#198261),(#198262,#198263),(#198264,#198265),(#198266,#198267),
(#198268,#198269),(#198270,#198271),(#198272,#198273),(#198274,#198275),
(#198276,#198277),(#198278,#198279),(#198280,#198281),(#198282,#198283),
(#198284,#198285),(#198286,#198287),(#198288,#198289),(#198290,#198291),
(#198292,#198293),(#198294,#198295),(#198296,#198297),(#198298,#198299),
(#198300,#198301),(#198302,#198303),(#198304,#198305),(#198306,#198307),
(#198308,#198309),(#198310,#198311),(#198312,#198313),(#198314,#198315),
(#198316,#198317),(#198318,#198319),(#198320,#198321),(#198322,#198323),
(#198324,#198325),(#198326,#198327),(#198328,#198329),(#198330,#198331),
(#198332,#198333),(#198334,#198335),(#198336,#198337),(#198338,#198339),
(#198340,#198341),(#198342,#198343),(#198344,#198345),(#198346,#198347),
(#198348,#198349),(#198350,#198351),(#198352,#198353),(#198354,#198355),
(#198356,#198357),(#198358,#198359),(#198360,#198361),(#198362,#198363),
(#198364,#198365),(#198366,#198367),(#198368,#198369),(#198370,#198371),
(#198372,#198373),(#198374,#198375),(#198376,#198377),(#198378,#198379),
(#198380,#198381),(#198382,#198383),(#198384,#198385),(#198386,#198387),
(#198388,#198389),(#198390,#198391),(#198392,#198393),(#198394,#198395),
(#198396,#198397),(#198398,#198399),(#198400,#198401),(#198402,#198403),
(#198404,#198405),(#198406,#198407),(#198408,#198409),(#198410,#198411),
(#198412,#198413),(#198414,#198415),(#198416,#198417),(#198418,#198419),
(#198420,#198421),(#198422,#198423),(#198424,#198425),(#198426,#198427),
(#198428,#198429),(#198430,#198431),(#198432,#198433),(#198434,#198435),
(#198436,#198437),(#198438,#198439),(#198440,#198441),(#198442,#198443),
(#198444,#198445),(#198446,#198447),(#198448,#198449),(#198450,#198451),
(#198452,#198453),(#198454,#198455),(#198456,#198457),(#198458,#198459),
(#198460,#198461),(#198462,#198463),(#198464,#198465),(#198466,#198467),
(#198468,#198469),(#198470,#198471),(#198472,#198473),(#198474,#198475),
(#198476,#198477),(#198478,#198479),(#198480,#198481),(#198482,#198483),
(#198484,#198485),(#198486,#198487),(#198488,#198489),(#198490,#198491),
(#198492,#198493),(#198494,#198495),(#198496,#198497),(#198498,#198499),
(#198500,#198501),(#198502,#198503),(#198504,#198505),(#198506,#198507),
(#198508,#198509),(#198510,#198511),(#198512,#198513),(#198514,#198515),
(#198516,#198517),(#198518,#198519),(#198520,#198521),(#198522,#198523),
(#198524,#198525),(#198526,#198527),(#198528,#198529),(#198530,#198531),
(#198532,#198533),(#198534,#198535),(#198536,#198537),(#198538,#198539),
(#198540,#198541),(#198542,#198543),(#198544,#198545),(#198546,#198547),
(#198548,#198549),(#198550,#198551),(#198552,#198553),(#198554,#198555),
(#198556,#198557),(#198558,#198559),(#198560,#198561),(#198562,#198563),
(#198564,#198565),(#198566,#198567),(#198568,#198569),(#198570,#198571),
(#198572,#198573),(#198574,#198575),(#198576,#198577),(#198578,#198579),
(#198580,#198581),(#198582,#198583),(#198584,#198585),(#198586,#198587),
(#198588,#198589),(#198590,#198591),(#198592,#198593),(#198594,#198595),
(#198596,#198597),(#198598,#198599),(#198600,#198601),(#198602,#198603),
(#198604,#198605),(#198606,#198607),(#198608,#198609),(#198610,#198611),
(#198612,#198613),(#198614,#198615),(#198616,#198617),(#198618,#198619),
(#198620,#198621),(#198622,#198623),(#198624,#198625),(#198626,#198627),
(#198628,#198629),(#198630,#198631),(#198632,#198633),(#198634,#198635),
(#198636,#198637),(#198638,#198639),(#198640,#198641),(#198642,#198643),
(#198644,#198645),(#198646,#198647),(#198648,#198649),(#198650,#198651),
(#198652,#198653),(#198654,#198655),(#198656,#198657),(#198658,#198659),
(#198660,#198661),(#198662,#198663),(#198664,#198665),(#198666,#198667),
(#198668,#198669),(#198670,#198671),(#198672,#198673),(#198674,#198675),
(#198676,#198677),(#198678,#198679),(#198680,#198681),(#198682,#198683),
(#198684,#198685),(#198686,#198687),(#198688,#198689),(#198690,#198691),
(#198692,#198693),(#198694,#198695),(#198696,#198697),(#198698,#198699),
(#198700,#198701),(#198702,#198703),(#198704,#198705),(#198706,#198707),
(#198708,#198709),(#198710,#198711),(#198712,#198713),(#198714,#198715),
(#198716,#198717),(#198718,#198719),(#198720,#198721),(#198722,#198723),
(#198724,#198725),(#198726,#198727),(#198728,#198729),(#198730,#198731),
(#198732,#198733),(#198734,#198735),(#198736,#198737),(#198738,#198739),
(#198740,#198741),(#198742,#198743),(#198744,#198745),(#198746,#198747),
(#198748,#198749),(#198750,#198751),(#198752,#198753),(#198754,#198755),
(#198756,#198757),(#198758,#198759),(#198760,#198761),(#198762,#198763),
(#198764,#198765),(#198766,#198767),(#198768,#198769),(#198770,#198771),
(#198772,#198773),(#198774,#198775),(#198776,#198777),(#198778,#198779),
(#198780,#198781),(#198782,#198783),(#198784,#198785),(#198786,#198787),
(#198788,#198789),(#198790,#198791),(#198792,#198793),(#198794,#198795),
(#198796,#198797),(#198798,#198799),(#198800,#198801),(#198802,#198803),
(#198804,#198805),(#198806,#198807),(#198808,#198809),(#198810,#198811),
(#198812,#198813),(#198814,#198815),(#198816,#198817),(#198818,#198819),
(#198820,#198821),(#198822,#198823),(#198824,#198825),(#198826,#198827),
(#198828,#198829),(#198830,#198831),(#198832,#198833),(#198834,#198835),
(#198836,#198837),(#198838,#198839),(#198840,#198841),(#198842,#198843),
(#198844,#198845),(#198846,#198847),(#198848,#198849),(#198850,#198851),
(#198852,#198853),(#198854,#198855),(#198856,#198857),(#198858,#198859),
(#198860,#198861),(#198862,#198863),(#198864,#198865),(#198866,#198867),
(#198868,#198869),(#198870,#198871),(#198872,#198873),(#198874,#198875),
(#198876,#198877),(#198878,#198879),(#198880,#198881),(#198882,#198883),
(#198884,#198885),(#198886,#198887),(#198888,#198889),(#198890,#198891),
(#198892,#198893),(#198894,#198895),(#198896,#198897),(#198898,#198899),
(#198900,#198901),(#198902,#198903)),.UNSPECIFIED.,.F.,.F.,.F.,(6,1,1,1,
1,1,1,1,1,1,1,1,1,1,1,1,1,1,1,1,1,1,1,1,1,1,1,1,1,1,1,1,1,1,1,1,1,1,1,1,
1,1,1,1,1,1,1,1,1,1,1,1,1,1,1,1,1,1,1,1,1,1,1,1,1,1,1,1,1,1,1,1,1,1,1,1,
1,1,1,1,1,1,1,1,1,1,1,1,1,1,1,1,1,1,1,1,1,1,1,1,1,1,1,1,1,1,1,1,1,1,1,1,
1,1,1,1,1,1,1,1,1,1,1,1,1,1,1,1,1,1,1,1,1,1,1,1,1,1,1,1,1,1,1,1,1,1,1,1,
1,1,1,1,1,1,1,1,1,1,1,1,1,1,1,1,1,1,1,1,1,1,1,1,1,1,1,1,1,1,1,1,1,1,1,1,
1,1,1,1,1,1,1,1,1,1,1,1,1,1,1,1,1,1,1,1,1,1,1,1,1,1,1,1,1,1,1,1,1,1,1,1,
1,1,1,1,1,1,1,1,1,1,1,1,1,1,1,1,1,1,1,1,1,1,1,1,1,1,1,1,1,1,1,1,1,1,1,1,
1,1,1,1,1,1,1,1,1,1,1,1,1,1,1,1,1,1,1,1,1,1,1,1,1,1,1,1,1,1,1,1,1,1,1,1,
1,1,1,1,1,1,1,1,1,1,1,1,1,1,1,1,1,1,1,1,1,1,1,1,1,1,1,1,1,1,1,1,1,1,1,1,
1,1,1,1,1,1,1,1,1,1,1,1,1,1,1,1,1,1,1,1,1,1,1,1,1,1,1,1,1,1,1,1,1,1,1,1,
1,1,1,1,1,1,1,1,1,1,1,1,1,1,1,1,1,1,1,1,1,1,1,1,1,1,1,1,1,1,1,1,1,1,1,1,
1,1,1,1,1,1,1,1,1,1,1,1,1,1,1,1,1,1,1,1,1,1,1,1,1,1,1,1,1,1,1,1,1,1,1,1,
1,1,1,1,1,1,1,1,1,1,1,1,1,1,1,1,1,1,1,1,1,1,1,1,1,1,1,1,1,1,1,6),(2,2),
(-1.,-0.998165138,-0.996330275,-0.994495413,-0.99266055,-0.990825688,-0.988990826,
-0.987155963,-0.985321101,-0.983486239,-0.981651376,-0.979816514,-0.977981651,
-0.976146789,-0.974311927,-0.972477064,-0.970642202,-0.968807339,-0.966972477,
-0.965137615,-0.963302752,-0.96146789,-0.959633028,-0.957798165,-0.955963303,
-0.95412844,-0.952293578,-0.950458716,-0.948623853,-0.946788991,-0.944954128,
-0.943119266,-0.941284404,-0.939449541,-0.937614679,-0.935779817,-0.933944954,
-0.932110092,-0.930275229,-0.928440367,-0.926605505,-0.924770642,-0.92293578,
-0.921100917,-0.919266055,-0.917431193,-0.91559633,-0.913761468,-0.911926606,
-0.910091743,-0.908256881,-0.906422018,-0.904587156,-0.902752294,-0.900917431,
-0.899082569,-0.897247706,-0.895412844,-0.893577982,-0.891743119,-0.889908257,
-0.888073394,-0.886238532,-0.88440367,-0.882568807,-0.880733945,-0.878899083,
-0.87706422,-0.875229358,-0.873394495,-0.871559633,-0.869724771,-0.867889908,
-0.866055046,-0.864220183,-0.862385321,-0.860550459,-0.858715596,-0.856880734,
-0.855045872,-0.853211009,-0.851376147,-0.849541284,-0.847706422,-0.84587156,
-0.844036697,-0.842201835,-0.840366972,-0.83853211,-0.836697248,-0.834862385,
-0.833027523,-0.831192661,-0.829357798,-0.827522936,-0.825688073,-0.823853211,
-0.822018349,-0.820183486,-0.818348624,-0.816513761,-0.814678899,-0.812844037,
-0.811009174,-0.809174312,-0.80733945,-0.805504587,-0.803669725,-0.801834862,
-0.8,-0.798165138,-0.796330275,-0.794495413,-0.79266055,-0.790825688,-0.788990826,
-0.787155963,-0.785321101,-0.783486239,-0.781651376,-0.779816514,-0.777981651,
-0.776146789,-0.774311927,-0.772477064,-0.770642202,-0.768807339,-0.766972477,
-0.765137615,-0.763302752,-0.76146789,-0.759633028,-0.757798165,-0.755963303,
-0.75412844,-0.752293578,-0.750458716,-0.748623853,-0.746788991,-0.744954128,
-0.743119266,-0.741284404,-0.739449541,-0.737614679,-0.735779817,-0.733944954,
-0.732110092,-0.730275229,-0.728440367,-0.726605505,-0.724770642,-0.72293578,
-0.721100917,-0.719266055,-0.717431193,-0.71559633,-0.713761468,-0.711926606,
-0.710091743,-0.708256881,-0.706422018,-0.704587156,-0.702752294,-0.700917431,
-0.699082569,-0.697247706,-0.695412844,-0.693577982,-0.691743119,-0.689908257,
-0.688073394,-0.686238532,-0.68440367,-0.682568807,-0.680733945,-0.678899083,
-0.67706422,-0.675229358,-0.673394495,-0.671559633,-0.669724771,-0.667889908,
-0.666055046,-0.664220183,-0.662385321,-0.660550459,-0.658715596,-0.656880734,
-0.655045872,-0.653211009,-0.651376147,-0.649541284,-0.647706422,-0.64587156,
-0.644036697,-0.642201835,-0.640366972,-0.63853211,-0.636697248,-0.634862385,
-0.633027523,-0.631192661,-0.629357798,-0.627522936,-0.625688073,-0.623853211,
-0.622018349,-0.620183486,-0.618348624,-0.616513761,-0.614678899,-0.612844037,
-0.611009174,-0.609174312,-0.60733945,-0.605504587,-0.603669725,-0.601834862,
-0.6,-0.598165138,-0.596330275,-0.594495413,-0.59266055,-0.590825688,-0.588990826,
-0.587155963,-0.585321101,-0.583486239,-0.581651376,-0.579816514,-0.577981651,
-0.576146789,-0.574311927,-0.572477064,-0.570642202,-0.568807339,-0.566972477,
-0.565137615,-0.563302752,-0.56146789,-0.559633028,-0.557798165,-0.555963303,
-0.55412844,-0.552293578,-0.550458716,-0.548623853,-0.546788991,-0.544954128,
-0.543119266,-0.541284404,-0.539449541,-0.537614679,-0.535779817,-0.533944954,
-0.532110092,-0.530275229,-0.528440367,-0.526605505,-0.524770642,-0.52293578,
-0.521100917,-0.519266055,-0.517431193,-0.51559633,-0.513761468,-0.511926606,
-0.510091743,-0.508256881,-0.506422018,-0.504587156,-0.502752294,-0.500917431,
-0.499082569,-0.497247706,-0.495412844,-0.493577982,-0.491743119,-0.489908257,
-0.488073394,-0.486238532,-0.48440367,-0.482568807,-0.480733945,-0.478899083,
-0.47706422,-0.475229358,-0.473394495,-0.471559633,-0.469724771,-0.467889908,
-0.466055046,-0.464220183,-0.462385321,-0.460550459,-0.458715596,-0.456880734,
-0.455045872,-0.453211009,-0.451376147,-0.449541284,-0.447706422,-0.44587156,
-0.444036697,-0.442201835,-0.440366972,-0.43853211,-0.436697248,-0.434862385,
-0.433027523,-0.431192661,-0.429357798,-0.427522936,-0.425688073,-0.423853211,
-0.422018349,-0.420183486,-0.418348624,-0.416513761,-0.414678899,-0.412844037,
-0.411009174,-0.409174312,-0.40733945,-0.405504587,-0.403669725,-0.401834862,
-0.4,-0.398165138,-0.396330275,-0.394495413,-0.39266055,-0.390825688,-0.388990826,
-0.387155963,-0.385321101,-0.383486239,-0.381651376,-0.379816514,-0.377981651,
-0.376146789,-0.374311927,-0.372477064,-0.370642202,-0.368807339,-0.366972477,
-0.365137615,-0.363302752,-0.36146789,-0.359633028,-0.357798165,-0.355963303,
-0.35412844,-0.352293578,-0.350458716,-0.348623853,-0.346788991,-0.344954128,
-0.343119266,-0.341284404,-0.339449541,-0.337614679,-0.335779817,-0.333944954,
-0.332110092,-0.330275229,-0.328440367,-0.326605505,-0.324770642,-0.32293578,
-0.321100917,-0.319266055,-0.317431193,-0.31559633,-0.313761468,-0.311926606,
-0.310091743,-0.308256881,-0.306422018,-0.304587156,-0.302752294,-0.300917431,
-0.299082569,-0.297247706,-0.295412844,-0.293577982,-0.291743119,-0.289908257,
-0.288073394,-0.286238532,-0.28440367,-0.282568807,-0.280733945,-0.278899083,
-0.27706422,-0.275229358,-0.273394495,-0.271559633,-0.269724771,-0.267889908,
-0.266055046,-0.264220183,-0.262385321,-0.260550459,-0.258715596,-0.256880734,
-0.255045872,-0.253211009,-0.251376147,-0.249541284,-0.247706422,-0.24587156,
-0.244036697,-0.242201835,-0.240366972,-0.23853211,-0.236697248,-0.234862385,
-0.233027523,-0.231192661,-0.229357798,-0.227522936,-0.225688073,-0.223853211,
-0.222018349,-0.220183486,-0.218348624,-0.216513761,-0.214678899,-0.212844037,
-0.211009174,-0.209174312,-0.20733945,-0.205504587,-0.203669725,-0.201834862,
-0.2,-0.198165138,-0.196330275,-0.194495413,-0.19266055,-0.190825688,-0.188990826,
-0.187155963,-0.185321101,-0.183486239,-0.181651376,-0.179816514,-0.177981651,
-0.176146789,-0.174311927,-0.172477064,-0.170642202,-0.168807339,-0.166972477,
-0.165137615,-0.163302752,-0.16146789,-0.159633028,-0.157798165,-0.155963303,
-0.15412844,-0.152293578,-0.150458716,-0.148623853,-0.146788991,-0.144954128,
-0.143172104),(0.,0.36),.UNSPECIFIED.);
#6242=B_SPLINE_SURFACE_WITH_KNOTS('',5,1,((#199518,#199519),(#199520,#199521),
(#199522,#199523),(#199524,#199525),(#199526,#199527),(#199528,#199529),
(#199530,#199531),(#199532,#199533),(#199534,#199535),(#199536,#199537),
(#199538,#199539),(#199540,#199541),(#199542,#199543),(#199544,#199545),
(#199546,#199547),(#199548,#199549),(#199550,#199551),(#199552,#199553),
(#199554,#199555),(#199556,#199557),(#199558,#199559),(#199560,#199561),
(#199562,#199563),(#199564,#199565),(#199566,#199567),(#199568,#199569),
(#199570,#199571),(#199572,#199573),(#199574,#199575),(#199576,#199577),
(#199578,#199579),(#199580,#199581),(#199582,#199583),(#199584,#199585),
(#199586,#199587),(#199588,#199589),(#199590,#199591),(#199592,#199593),
(#199594,#199595),(#199596,#199597),(#199598,#199599),(#199600,#199601),
(#199602,#199603),(#199604,#199605),(#199606,#199607),(#199608,#199609),
(#199610,#199611),(#199612,#199613),(#199614,#199615),(#199616,#199617),
(#199618,#199619),(#199620,#199621),(#199622,#199623),(#199624,#199625),
(#199626,#199627),(#199628,#199629),(#199630,#199631),(#199632,#199633),
(#199634,#199635),(#199636,#199637),(#199638,#199639),(#199640,#199641),
(#199642,#199643),(#199644,#199645),(#199646,#199647),(#199648,#199649),
(#199650,#199651),(#199652,#199653),(#199654,#199655),(#199656,#199657),
(#199658,#199659),(#199660,#199661),(#199662,#199663),(#199664,#199665),
(#199666,#199667),(#199668,#199669),(#199670,#199671),(#199672,#199673),
(#199674,#199675),(#199676,#199677),(#199678,#199679),(#199680,#199681),
(#199682,#199683),(#199684,#199685),(#199686,#199687),(#199688,#199689),
(#199690,#199691),(#199692,#199693),(#199694,#199695),(#199696,#199697),
(#199698,#199699),(#199700,#199701),(#199702,#199703),(#199704,#199705),
(#199706,#199707),(#199708,#199709),(#199710,#199711),(#199712,#199713),
(#199714,#199715),(#199716,#199717),(#199718,#199719),(#199720,#199721),
(#199722,#199723),(#199724,#199725),(#199726,#199727),(#199728,#199729),
(#199730,#199731),(#199732,#199733),(#199734,#199735),(#199736,#199737),
(#199738,#199739),(#199740,#199741),(#199742,#199743),(#199744,#199745),
(#199746,#199747),(#199748,#199749),(#199750,#199751),(#199752,#199753),
(#199754,#199755),(#199756,#199757),(#199758,#199759),(#199760,#199761),
(#199762,#199763),(#199764,#199765),(#199766,#199767),(#199768,#199769),
(#199770,#199771),(#199772,#199773),(#199774,#199775),(#199776,#199777),
(#199778,#199779),(#199780,#199781),(#199782,#199783),(#199784,#199785),
(#199786,#199787),(#199788,#199789),(#199790,#199791),(#199792,#199793),
(#199794,#199795),(#199796,#199797),(#199798,#199799),(#199800,#199801),
(#199802,#199803),(#199804,#199805),(#199806,#199807),(#199808,#199809),
(#199810,#199811),(#199812,#199813),(#199814,#199815),(#199816,#199817),
(#199818,#199819),(#199820,#199821),(#199822,#199823),(#199824,#199825),
(#199826,#199827),(#199828,#199829),(#199830,#199831),(#199832,#199833),
(#199834,#199835),(#199836,#199837),(#199838,#199839),(#199840,#199841),
(#199842,#199843),(#199844,#199845),(#199846,#199847),(#199848,#199849),
(#199850,#199851),(#199852,#199853),(#199854,#199855),(#199856,#199857),
(#199858,#199859),(#199860,#199861),(#199862,#199863),(#199864,#199865),
(#199866,#199867),(#199868,#199869),(#199870,#199871),(#199872,#199873),
(#199874,#199875),(#199876,#199877),(#199878,#199879),(#199880,#199881),
(#199882,#199883),(#199884,#199885),(#199886,#199887),(#199888,#199889),
(#199890,#199891),(#199892,#199893),(#199894,#199895),(#199896,#199897),
(#199898,#199899),(#199900,#199901),(#199902,#199903),(#199904,#199905),
(#199906,#199907),(#199908,#199909),(#199910,#199911),(#199912,#199913),
(#199914,#199915),(#199916,#199917),(#199918,#199919),(#199920,#199921),
(#199922,#199923),(#199924,#199925),(#199926,#199927),(#199928,#199929),
(#199930,#199931),(#199932,#199933),(#199934,#199935),(#199936,#199937),
(#199938,#199939),(#199940,#199941),(#199942,#199943),(#199944,#199945),
(#199946,#199947),(#199948,#199949),(#199950,#199951),(#199952,#199953),
(#199954,#199955),(#199956,#199957),(#199958,#199959),(#199960,#199961),
(#199962,#199963),(#199964,#199965),(#199966,#199967),(#199968,#199969),
(#199970,#199971),(#199972,#199973),(#199974,#199975),(#199976,#199977),
(#199978,#199979),(#199980,#199981),(#199982,#199983),(#199984,#199985),
(#199986,#199987),(#199988,#199989),(#199990,#199991),(#199992,#199993),
(#199994,#199995),(#199996,#199997),(#199998,#199999),(#200000,#200001),
(#200002,#200003),(#200004,#200005),(#200006,#200007),(#200008,#200009),
(#200010,#200011),(#200012,#200013),(#200014,#200015),(#200016,#200017),
(#200018,#200019),(#200020,#200021),(#200022,#200023),(#200024,#200025),
(#200026,#200027),(#200028,#200029),(#200030,#200031),(#200032,#200033),
(#200034,#200035),(#200036,#200037),(#200038,#200039),(#200040,#200041),
(#200042,#200043),(#200044,#200045),(#200046,#200047),(#200048,#200049),
(#200050,#200051),(#200052,#200053),(#200054,#200055),(#200056,#200057),
(#200058,#200059),(#200060,#200061),(#200062,#200063),(#200064,#200065),
(#200066,#200067),(#200068,#200069),(#200070,#200071),(#200072,#200073),
(#200074,#200075),(#200076,#200077),(#200078,#200079),(#200080,#200081),
(#200082,#200083),(#200084,#200085),(#200086,#200087),(#200088,#200089),
(#200090,#200091),(#200092,#200093),(#200094,#200095),(#200096,#200097),
(#200098,#200099),(#200100,#200101),(#200102,#200103),(#200104,#200105),
(#200106,#200107),(#200108,#200109),(#200110,#200111),(#200112,#200113),
(#200114,#200115),(#200116,#200117),(#200118,#200119),(#200120,#200121),
(#200122,#200123),(#200124,#200125),(#200126,#200127),(#200128,#200129),
(#200130,#200131),(#200132,#200133),(#200134,#200135),(#200136,#200137),
(#200138,#200139),(#200140,#200141),(#200142,#200143),(#200144,#200145),
(#200146,#200147),(#200148,#200149),(#200150,#200151),(#200152,#200153),
(#200154,#200155),(#200156,#200157),(#200158,#200159),(#200160,#200161),
(#200162,#200163),(#200164,#200165),(#200166,#200167),(#200168,#200169),
(#200170,#200171),(#200172,#200173),(#200174,#200175),(#200176,#200177),
(#200178,#200179),(#200180,#200181),(#200182,#200183),(#200184,#200185),
(#200186,#200187),(#200188,#200189),(#200190,#200191),(#200192,#200193),
(#200194,#200195),(#200196,#200197),(#200198,#200199),(#200200,#200201),
(#200202,#200203),(#200204,#200205),(#200206,#200207),(#200208,#200209),
(#200210,#200211),(#200212,#200213),(#200214,#200215),(#200216,#200217),
(#200218,#200219),(#200220,#200221),(#200222,#200223),(#200224,#200225),
(#200226,#200227),(#200228,#200229),(#200230,#200231),(#200232,#200233),
(#200234,#200235),(#200236,#200237),(#200238,#200239),(#200240,#200241),
(#200242,#200243),(#200244,#200245),(#200246,#200247),(#200248,#200249),
(#200250,#200251),(#200252,#200253),(#200254,#200255),(#200256,#200257),
(#200258,#200259),(#200260,#200261),(#200262,#200263),(#200264,#200265),
(#200266,#200267),(#200268,#200269),(#200270,#200271),(#200272,#200273),
(#200274,#200275),(#200276,#200277),(#200278,#200279),(#200280,#200281),
(#200282,#200283),(#200284,#200285),(#200286,#200287),(#200288,#200289),
(#200290,#200291),(#200292,#200293),(#200294,#200295),(#200296,#200297),
(#200298,#200299),(#200300,#200301),(#200302,#200303),(#200304,#200305),
(#200306,#200307),(#200308,#200309),(#200310,#200311),(#200312,#200313),
(#200314,#200315),(#200316,#200317),(#200318,#200319),(#200320,#200321),
(#200322,#200323),(#200324,#200325),(#200326,#200327),(#200328,#200329),
(#200330,#200331),(#200332,#200333),(#200334,#200335),(#200336,#200337),
(#200338,#200339),(#200340,#200341),(#200342,#200343),(#200344,#200345),
(#200346,#200347),(#200348,#200349),(#200350,#200351),(#200352,#200353),
(#200354,#200355),(#200356,#200357),(#200358,#200359),(#200360,#200361),
(#200362,#200363),(#200364,#200365),(#200366,#200367),(#200368,#200369),
(#200370,#200371),(#200372,#200373),(#200374,#200375),(#200376,#200377),
(#200378,#200379),(#200380,#200381),(#200382,#200383),(#200384,#200385),
(#200386,#200387),(#200388,#200389),(#200390,#200391),(#200392,#200393),
(#200394,#200395),(#200396,#200397),(#200398,#200399),(#200400,#200401),
(#200402,#200403),(#200404,#200405),(#200406,#200407),(#200408,#200409),
(#200410,#200411),(#200412,#200413),(#200414,#200415),(#200416,#200417),
(#200418,#200419),(#200420,#200421),(#200422,#200423),(#200424,#200425),
(#200426,#200427),(#200428,#200429),(#200430,#200431),(#200432,#200433),
(#200434,#200435),(#200436,#200437),(#200438,#200439),(#200440,#200441),
(#200442,#200443),(#200444,#200445),(#200446,#200447),(#200448,#200449),
(#200450,#200451),(#200452,#200453),(#200454,#200455),(#200456,#200457),
(#200458,#200459),(#200460,#200461)),.UNSPECIFIED.,.F.,.F.,.F.,(6,1,1,1,
1,1,1,1,1,1,1,1,1,1,1,1,1,1,1,1,1,1,1,1,1,1,1,1,1,1,1,1,1,1,1,1,1,1,1,1,
1,1,1,1,1,1,1,1,1,1,1,1,1,1,1,1,1,1,1,1,1,1,1,1,1,1,1,1,1,1,1,1,1,1,1,1,
1,1,1,1,1,1,1,1,1,1,1,1,1,1,1,1,1,1,1,1,1,1,1,1,1,1,1,1,1,1,1,1,1,1,1,1,
1,1,1,1,1,1,1,1,1,1,1,1,1,1,1,1,1,1,1,1,1,1,1,1,1,1,1,1,1,1,1,1,1,1,1,1,
1,1,1,1,1,1,1,1,1,1,1,1,1,1,1,1,1,1,1,1,1,1,1,1,1,1,1,1,1,1,1,1,1,1,1,1,
1,1,1,1,1,1,1,1,1,1,1,1,1,1,1,1,1,1,1,1,1,1,1,1,1,1,1,1,1,1,1,1,1,1,1,1,
1,1,1,1,1,1,1,1,1,1,1,1,1,1,1,1,1,1,1,1,1,1,1,1,1,1,1,1,1,1,1,1,1,1,1,1,
1,1,1,1,1,1,1,1,1,1,1,1,1,1,1,1,1,1,1,1,1,1,1,1,1,1,1,1,1,1,1,1,1,1,1,1,
1,1,1,1,1,1,1,1,1,1,1,1,1,1,1,1,1,1,1,1,1,1,1,1,1,1,1,1,1,1,1,1,1,1,1,1,
1,1,1,1,1,1,1,1,1,1,1,1,1,1,1,1,1,1,1,1,1,1,1,1,1,1,1,1,1,1,1,1,1,1,1,1,
1,1,1,1,1,1,1,1,1,1,1,1,1,1,1,1,1,1,1,1,1,1,1,1,1,1,1,1,1,1,1,1,1,1,1,1,
1,1,1,1,1,1,1,1,1,1,1,1,1,1,1,1,1,1,1,1,1,1,1,1,1,1,1,1,1,1,1,1,1,1,1,1,
1,1,1,1,1,1,1,1,1,1,1,1,1,1,1,1,1,1,1,1,1,1,1,1,1,1,1,1,1,1,1,6),(2,2),
(0.143172104,0.144954128,0.146788991,0.148623853,0.150458716,0.152293578,
0.15412844,0.155963303,0.157798165,0.159633028,0.16146789,0.163302752,0.165137615,
0.166972477,0.168807339,0.170642202,0.172477064,0.174311927,0.176146789,
0.177981651,0.179816514,0.181651376,0.183486239,0.185321101,0.187155963,
0.188990826,0.190825688,0.19266055,0.194495413,0.196330275,0.198165138,
0.2,0.201834862,0.203669725,0.205504587,0.20733945,0.209174312,0.211009174,
0.212844037,0.214678899,0.216513761,0.218348624,0.220183486,0.222018349,
0.223853211,0.225688073,0.227522936,0.229357798,0.231192661,0.233027523,
0.234862385,0.236697248,0.23853211,0.240366972,0.242201835,0.244036697,
0.24587156,0.247706422,0.249541284,0.251376147,0.253211009,0.255045872,
0.256880734,0.258715596,0.260550459,0.262385321,0.264220183,0.266055046,
0.267889908,0.269724771,0.271559633,0.273394495,0.275229358,0.27706422,
0.278899083,0.280733945,0.282568807,0.28440367,0.286238532,0.288073394,
0.289908257,0.291743119,0.293577982,0.295412844,0.297247706,0.299082569,
0.300917431,0.302752294,0.304587156,0.306422018,0.308256881,0.310091743,
0.311926606,0.313761468,0.31559633,0.317431193,0.319266055,0.321100917,
0.32293578,0.324770642,0.326605505,0.328440367,0.330275229,0.332110092,
0.333944954,0.335779817,0.337614679,0.339449541,0.341284404,0.343119266,
0.344954128,0.346788991,0.348623853,0.350458716,0.352293578,0.35412844,
0.355963303,0.357798165,0.359633028,0.36146789,0.363302752,0.365137615,
0.366972477,0.368807339,0.370642202,0.372477064,0.374311927,0.376146789,
0.377981651,0.379816514,0.381651376,0.383486239,0.385321101,0.387155963,
0.388990826,0.390825688,0.39266055,0.394495413,0.396330275,0.398165138,
0.4,0.401834862,0.403669725,0.405504587,0.40733945,0.409174312,0.411009174,
0.412844037,0.414678899,0.416513761,0.418348624,0.420183486,0.422018349,
0.423853211,0.425688073,0.427522936,0.429357798,0.431192661,0.433027523,
0.434862385,0.436697248,0.43853211,0.440366972,0.442201835,0.444036697,
0.44587156,0.447706422,0.449541284,0.451376147,0.453211009,0.455045872,
0.456880734,0.458715596,0.460550459,0.462385321,0.464220183,0.466055046,
0.467889908,0.469724771,0.471559633,0.473394495,0.475229358,0.47706422,
0.478899083,0.480733945,0.482568807,0.48440367,0.486238532,0.488073394,
0.489908257,0.491743119,0.493577982,0.495412844,0.497247706,0.499082569,
0.500917431,0.502752294,0.504587156,0.506422018,0.508256881,0.510091743,
0.511926606,0.513761468,0.51559633,0.517431193,0.519266055,0.521100917,
0.52293578,0.524770642,0.526605505,0.528440367,0.530275229,0.532110092,
0.533944954,0.535779817,0.537614679,0.539449541,0.541284404,0.543119266,
0.544954128,0.546788991,0.548623853,0.550458716,0.552293578,0.55412844,
0.555963303,0.557798165,0.559633028,0.56146789,0.563302752,0.565137615,
0.566972477,0.568807339,0.570642202,0.572477064,0.574311927,0.576146789,
0.577981651,0.579816514,0.581651376,0.583486239,0.585321101,0.587155963,
0.588990826,0.590825688,0.59266055,0.594495413,0.596330275,0.598165138,
0.6,0.601834862,0.603669725,0.605504587,0.60733945,0.609174312,0.611009174,
0.612844037,0.614678899,0.616513761,0.618348624,0.620183486,0.622018349,
0.623853211,0.625688073,0.627522936,0.629357798,0.631192661,0.633027523,
0.634862385,0.636697248,0.63853211,0.640366972,0.642201835,0.644036697,
0.64587156,0.647706422,0.649541284,0.651376147,0.653211009,0.655045872,
0.656880734,0.658715596,0.660550459,0.662385321,0.664220183,0.666055046,
0.667889908,0.669724771,0.671559633,0.673394495,0.675229358,0.67706422,
0.678899083,0.680733945,0.682568807,0.68440367,0.686238532,0.688073394,
0.689908257,0.691743119,0.693577982,0.695412844,0.697247706,0.699082569,
0.700917431,0.702752294,0.704587156,0.706422018,0.708256881,0.710091743,
0.711926606,0.713761468,0.71559633,0.717431193,0.719266055,0.721100917,
0.72293578,0.724770642,0.726605505,0.728440367,0.730275229,0.732110092,
0.733944954,0.735779817,0.737614679,0.739449541,0.741284404,0.743119266,
0.744954128,0.746788991,0.748623853,0.750458716,0.752293578,0.75412844,
0.755963303,0.757798165,0.759633028,0.76146789,0.763302752,0.765137615,
0.766972477,0.768807339,0.770642202,0.772477064,0.774311927,0.776146789,
0.777981651,0.779816514,0.781651376,0.783486239,0.785321101,0.787155963,
0.788990826,0.790825688,0.79266055,0.794495413,0.796330275,0.798165138,
0.8,0.801834862,0.803669725,0.805504587,0.80733945,0.809174312,0.811009174,
0.812844037,0.814678899,0.816513761,0.818348624,0.820183486,0.822018349,
0.823853211,0.825688073,0.827522936,0.829357798,0.831192661,0.833027523,
0.834862385,0.836697248,0.83853211,0.840366972,0.842201835,0.844036697,
0.84587156,0.847706422,0.849541284,0.851376147,0.853211009,0.855045872,
0.856880734,0.858715596,0.860550459,0.862385321,0.864220183,0.866055046,
0.867889908,0.869724771,0.871559633,0.873394495,0.875229358,0.87706422,
0.878899083,0.880733945,0.882568807,0.88440367,0.886238532,0.888073394,
0.889908257,0.891743119,0.893577982,0.895412844,0.897247706,0.899082569,
0.900917431,0.902752294,0.904587156,0.906422018,0.908256881,0.910091743,
0.911926606,0.913761468,0.91559633,0.917431193,0.919266055,0.921100917,
0.92293578,0.924770642,0.926605505,0.928440367,0.930275229,0.932110092,
0.933944954,0.935779817,0.937614679,0.939449541,0.941284404,0.943119266,
0.944954128,0.946788991,0.948623853,0.950458716,0.952293578,0.95412844,
0.955963303,0.957798165,0.959633028,0.96146789,0.963302752,0.965137615,
0.966972477,0.968807339,0.970642202,0.972477064,0.974311927,0.976146789,
0.977981651,0.979816514,0.981651376,0.983486239,0.985321101,0.987155963,
0.988990826,0.990825688,0.99266055,0.994495413,0.996330275,0.998165138,
1.),(0.,0.36),.UNSPECIFIED.);
#6243=B_SPLINE_SURFACE_WITH_KNOTS('',5,1,((#201118,#201119),(#201120,#201121),
(#201122,#201123),(#201124,#201125),(#201126,#201127),(#201128,#201129),
(#201130,#201131),(#201132,#201133),(#201134,#201135),(#201136,#201137),
(#201138,#201139),(#201140,#201141),(#201142,#201143),(#201144,#201145),
(#201146,#201147),(#201148,#201149),(#201150,#201151),(#201152,#201153),
(#201154,#201155),(#201156,#201157),(#201158,#201159),(#201160,#201161),
(#201162,#201163),(#201164,#201165),(#201166,#201167),(#201168,#201169),
(#201170,#201171),(#201172,#201173),(#201174,#201175),(#201176,#201177),
(#201178,#201179),(#201180,#201181),(#201182,#201183),(#201184,#201185),
(#201186,#201187),(#201188,#201189),(#201190,#201191),(#201192,#201193),
(#201194,#201195),(#201196,#201197),(#201198,#201199),(#201200,#201201),
(#201202,#201203),(#201204,#201205),(#201206,#201207),(#201208,#201209),
(#201210,#201211),(#201212,#201213),(#201214,#201215),(#201216,#201217),
(#201218,#201219),(#201220,#201221),(#201222,#201223),(#201224,#201225),
(#201226,#201227),(#201228,#201229),(#201230,#201231),(#201232,#201233),
(#201234,#201235),(#201236,#201237),(#201238,#201239),(#201240,#201241),
(#201242,#201243),(#201244,#201245),(#201246,#201247),(#201248,#201249),
(#201250,#201251),(#201252,#201253),(#201254,#201255),(#201256,#201257),
(#201258,#201259),(#201260,#201261),(#201262,#201263),(#201264,#201265),
(#201266,#201267),(#201268,#201269),(#201270,#201271),(#201272,#201273),
(#201274,#201275),(#201276,#201277),(#201278,#201279),(#201280,#201281),
(#201282,#201283),(#201284,#201285),(#201286,#201287),(#201288,#201289),
(#201290,#201291),(#201292,#201293),(#201294,#201295),(#201296,#201297),
(#201298,#201299),(#201300,#201301),(#201302,#201303),(#201304,#201305),
(#201306,#201307),(#201308,#201309),(#201310,#201311),(#201312,#201313),
(#201314,#201315),(#201316,#201317),(#201318,#201319),(#201320,#201321),
(#201322,#201323),(#201324,#201325),(#201326,#201327),(#201328,#201329),
(#201330,#201331),(#201332,#201333),(#201334,#201335),(#201336,#201337),
(#201338,#201339),(#201340,#201341),(#201342,#201343),(#201344,#201345),
(#201346,#201347),(#201348,#201349),(#201350,#201351),(#201352,#201353),
(#201354,#201355),(#201356,#201357),(#201358,#201359),(#201360,#201361),
(#201362,#201363),(#201364,#201365),(#201366,#201367),(#201368,#201369),
(#201370,#201371),(#201372,#201373),(#201374,#201375),(#201376,#201377),
(#201378,#201379),(#201380,#201381),(#201382,#201383),(#201384,#201385),
(#201386,#201387),(#201388,#201389),(#201390,#201391),(#201392,#201393),
(#201394,#201395),(#201396,#201397),(#201398,#201399),(#201400,#201401),
(#201402,#201403),(#201404,#201405),(#201406,#201407),(#201408,#201409),
(#201410,#201411),(#201412,#201413),(#201414,#201415),(#201416,#201417),
(#201418,#201419),(#201420,#201421),(#201422,#201423),(#201424,#201425),
(#201426,#201427),(#201428,#201429),(#201430,#201431),(#201432,#201433),
(#201434,#201435),(#201436,#201437),(#201438,#201439),(#201440,#201441),
(#201442,#201443),(#201444,#201445),(#201446,#201447),(#201448,#201449),
(#201450,#201451),(#201452,#201453),(#201454,#201455),(#201456,#201457),
(#201458,#201459),(#201460,#201461),(#201462,#201463),(#201464,#201465),
(#201466,#201467),(#201468,#201469),(#201470,#201471),(#201472,#201473),
(#201474,#201475),(#201476,#201477),(#201478,#201479),(#201480,#201481),
(#201482,#201483),(#201484,#201485),(#201486,#201487),(#201488,#201489),
(#201490,#201491),(#201492,#201493),(#201494,#201495),(#201496,#201497),
(#201498,#201499),(#201500,#201501),(#201502,#201503),(#201504,#201505),
(#201506,#201507),(#201508,#201509),(#201510,#201511),(#201512,#201513),
(#201514,#201515),(#201516,#201517),(#201518,#201519),(#201520,#201521),
(#201522,#201523),(#201524,#201525),(#201526,#201527),(#201528,#201529),
(#201530,#201531),(#201532,#201533),(#201534,#201535),(#201536,#201537),
(#201538,#201539),(#201540,#201541),(#201542,#201543),(#201544,#201545),
(#201546,#201547),(#201548,#201549),(#201550,#201551),(#201552,#201553),
(#201554,#201555),(#201556,#201557),(#201558,#201559),(#201560,#201561),
(#201562,#201563),(#201564,#201565),(#201566,#201567),(#201568,#201569),
(#201570,#201571),(#201572,#201573),(#201574,#201575),(#201576,#201577),
(#201578,#201579),(#201580,#201581),(#201582,#201583),(#201584,#201585),
(#201586,#201587),(#201588,#201589),(#201590,#201591),(#201592,#201593),
(#201594,#201595),(#201596,#201597),(#201598,#201599),(#201600,#201601),
(#201602,#201603),(#201604,#201605),(#201606,#201607),(#201608,#201609),
(#201610,#201611),(#201612,#201613),(#201614,#201615),(#201616,#201617),
(#201618,#201619),(#201620,#201621),(#201622,#201623),(#201624,#201625),
(#201626,#201627),(#201628,#201629),(#201630,#201631),(#201632,#201633),
(#201634,#201635),(#201636,#201637),(#201638,#201639),(#201640,#201641),
(#201642,#201643),(#201644,#201645),(#201646,#201647),(#201648,#201649),
(#201650,#201651),(#201652,#201653),(#201654,#201655),(#201656,#201657),
(#201658,#201659),(#201660,#201661),(#201662,#201663),(#201664,#201665),
(#201666,#201667),(#201668,#201669),(#201670,#201671),(#201672,#201673),
(#201674,#201675),(#201676,#201677),(#201678,#201679),(#201680,#201681),
(#201682,#201683),(#201684,#201685),(#201686,#201687),(#201688,#201689),
(#201690,#201691),(#201692,#201693),(#201694,#201695),(#201696,#201697),
(#201698,#201699),(#201700,#201701),(#201702,#201703),(#201704,#201705),
(#201706,#201707),(#201708,#201709),(#201710,#201711),(#201712,#201713),
(#201714,#201715),(#201716,#201717),(#201718,#201719),(#201720,#201721),
(#201722,#201723),(#201724,#201725),(#201726,#201727),(#201728,#201729),
(#201730,#201731),(#201732,#201733),(#201734,#201735),(#201736,#201737),
(#201738,#201739),(#201740,#201741),(#201742,#201743),(#201744,#201745),
(#201746,#201747),(#201748,#201749),(#201750,#201751),(#201752,#201753),
(#201754,#201755),(#201756,#201757),(#201758,#201759),(#201760,#201761),
(#201762,#201763),(#201764,#201765),(#201766,#201767),(#201768,#201769),
(#201770,#201771),(#201772,#201773),(#201774,#201775),(#201776,#201777),
(#201778,#201779),(#201780,#201781),(#201782,#201783),(#201784,#201785),
(#201786,#201787),(#201788,#201789),(#201790,#201791),(#201792,#201793),
(#201794,#201795),(#201796,#201797),(#201798,#201799),(#201800,#201801),
(#201802,#201803),(#201804,#201805),(#201806,#201807),(#201808,#201809),
(#201810,#201811),(#201812,#201813),(#201814,#201815),(#201816,#201817),
(#201818,#201819),(#201820,#201821),(#201822,#201823),(#201824,#201825),
(#201826,#201827),(#201828,#201829),(#201830,#201831),(#201832,#201833),
(#201834,#201835),(#201836,#201837),(#201838,#201839),(#201840,#201841),
(#201842,#201843),(#201844,#201845),(#201846,#201847),(#201848,#201849),
(#201850,#201851),(#201852,#201853),(#201854,#201855),(#201856,#201857),
(#201858,#201859),(#201860,#201861),(#201862,#201863),(#201864,#201865),
(#201866,#201867),(#201868,#201869),(#201870,#201871),(#201872,#201873),
(#201874,#201875),(#201876,#201877),(#201878,#201879),(#201880,#201881),
(#201882,#201883),(#201884,#201885),(#201886,#201887),(#201888,#201889),
(#201890,#201891),(#201892,#201893),(#201894,#201895),(#201896,#201897),
(#201898,#201899),(#201900,#201901),(#201902,#201903),(#201904,#201905),
(#201906,#201907),(#201908,#201909),(#201910,#201911),(#201912,#201913),
(#201914,#201915),(#201916,#201917),(#201918,#201919),(#201920,#201921),
(#201922,#201923),(#201924,#201925),(#201926,#201927),(#201928,#201929),
(#201930,#201931),(#201932,#201933),(#201934,#201935),(#201936,#201937),
(#201938,#201939),(#201940,#201941),(#201942,#201943),(#201944,#201945),
(#201946,#201947),(#201948,#201949),(#201950,#201951),(#201952,#201953),
(#201954,#201955),(#201956,#201957),(#201958,#201959),(#201960,#201961),
(#201962,#201963),(#201964,#201965),(#201966,#201967),(#201968,#201969),
(#201970,#201971),(#201972,#201973),(#201974,#201975),(#201976,#201977),
(#201978,#201979),(#201980,#201981),(#201982,#201983),(#201984,#201985),
(#201986,#201987),(#201988,#201989),(#201990,#201991),(#201992,#201993),
(#201994,#201995),(#201996,#201997),(#201998,#201999),(#202000,#202001),
(#202002,#202003),(#202004,#202005),(#202006,#202007),(#202008,#202009),
(#202010,#202011),(#202012,#202013),(#202014,#202015),(#202016,#202017),
(#202018,#202019),(#202020,#202021),(#202022,#202023),(#202024,#202025),
(#202026,#202027),(#202028,#202029),(#202030,#202031),(#202032,#202033),
(#202034,#202035),(#202036,#202037),(#202038,#202039),(#202040,#202041),
(#202042,#202043),(#202044,#202045),(#202046,#202047),(#202048,#202049),
(#202050,#202051),(#202052,#202053),(#202054,#202055),(#202056,#202057),
(#202058,#202059),(#202060,#202061)),.UNSPECIFIED.,.F.,.F.,.F.,(6,1,1,1,
1,1,1,1,1,1,1,1,1,1,1,1,1,1,1,1,1,1,1,1,1,1,1,1,1,1,1,1,1,1,1,1,1,1,1,1,
1,1,1,1,1,1,1,1,1,1,1,1,1,1,1,1,1,1,1,1,1,1,1,1,1,1,1,1,1,1,1,1,1,1,1,1,
1,1,1,1,1,1,1,1,1,1,1,1,1,1,1,1,1,1,1,1,1,1,1,1,1,1,1,1,1,1,1,1,1,1,1,1,
1,1,1,1,1,1,1,1,1,1,1,1,1,1,1,1,1,1,1,1,1,1,1,1,1,1,1,1,1,1,1,1,1,1,1,1,
1,1,1,1,1,1,1,1,1,1,1,1,1,1,1,1,1,1,1,1,1,1,1,1,1,1,1,1,1,1,1,1,1,1,1,1,
1,1,1,1,1,1,1,1,1,1,1,1,1,1,1,1,1,1,1,1,1,1,1,1,1,1,1,1,1,1,1,1,1,1,1,1,
1,1,1,1,1,1,1,1,1,1,1,1,1,1,1,1,1,1,1,1,1,1,1,1,1,1,1,1,1,1,1,1,1,1,1,1,
1,1,1,1,1,1,1,1,1,1,1,1,1,1,1,1,1,1,1,1,1,1,1,1,1,1,1,1,1,1,1,1,1,1,1,1,
1,1,1,1,1,1,1,1,1,1,1,1,1,1,1,1,1,1,1,1,1,1,1,1,1,1,1,1,1,1,1,1,1,1,1,1,
1,1,1,1,1,1,1,1,1,1,1,1,1,1,1,1,1,1,1,1,1,1,1,1,1,1,1,1,1,1,1,1,1,1,1,1,
1,1,1,1,1,1,1,1,1,1,1,1,1,1,1,1,1,1,1,1,1,1,1,1,1,1,1,1,1,1,1,1,1,1,1,1,
1,1,1,1,1,1,1,1,1,1,1,1,1,1,1,1,1,1,1,1,1,1,1,1,1,1,1,1,1,1,1,1,1,1,1,1,
1,1,1,1,1,1,1,1,1,1,1,1,1,1,1,1,1,1,1,1,1,1,1,1,1,1,1,1,1,1,1,6),(2,2),
(0.143172103,0.144954128,0.146788991,0.148623853,0.150458716,0.152293578,
0.15412844,0.155963303,0.157798165,0.159633028,0.16146789,0.163302752,0.165137615,
0.166972477,0.168807339,0.170642202,0.172477064,0.174311927,0.176146789,
0.177981651,0.179816514,0.181651376,0.183486239,0.185321101,0.187155963,
0.188990826,0.190825688,0.19266055,0.194495413,0.196330275,0.198165138,
0.2,0.201834862,0.203669725,0.205504587,0.20733945,0.209174312,0.211009174,
0.212844037,0.214678899,0.216513761,0.218348624,0.220183486,0.222018349,
0.223853211,0.225688073,0.227522936,0.229357798,0.231192661,0.233027523,
0.234862385,0.236697248,0.23853211,0.240366972,0.242201835,0.244036697,
0.24587156,0.247706422,0.249541284,0.251376147,0.253211009,0.255045872,
0.256880734,0.258715596,0.260550459,0.262385321,0.264220183,0.266055046,
0.267889908,0.269724771,0.271559633,0.273394495,0.275229358,0.27706422,
0.278899083,0.280733945,0.282568807,0.28440367,0.286238532,0.288073394,
0.289908257,0.291743119,0.293577982,0.295412844,0.297247706,0.299082569,
0.300917431,0.302752294,0.304587156,0.306422018,0.308256881,0.310091743,
0.311926606,0.313761468,0.31559633,0.317431193,0.319266055,0.321100917,
0.32293578,0.324770642,0.326605505,0.328440367,0.330275229,0.332110092,
0.333944954,0.335779817,0.337614679,0.339449541,0.341284404,0.343119266,
0.344954128,0.346788991,0.348623853,0.350458716,0.352293578,0.35412844,
0.355963303,0.357798165,0.359633028,0.36146789,0.363302752,0.365137615,
0.366972477,0.368807339,0.370642202,0.372477064,0.374311927,0.376146789,
0.377981651,0.379816514,0.381651376,0.383486239,0.385321101,0.387155963,
0.388990826,0.390825688,0.39266055,0.394495413,0.396330275,0.398165138,
0.4,0.401834862,0.403669725,0.405504587,0.40733945,0.409174312,0.411009174,
0.412844037,0.414678899,0.416513761,0.418348624,0.420183486,0.422018349,
0.423853211,0.425688073,0.427522936,0.429357798,0.431192661,0.433027523,
0.434862385,0.436697248,0.43853211,0.440366972,0.442201835,0.444036697,
0.44587156,0.447706422,0.449541284,0.451376147,0.453211009,0.455045872,
0.456880734,0.458715596,0.460550459,0.462385321,0.464220183,0.466055046,
0.467889908,0.469724771,0.471559633,0.473394495,0.475229358,0.47706422,
0.478899083,0.480733945,0.482568807,0.48440367,0.486238532,0.488073394,
0.489908257,0.491743119,0.493577982,0.495412844,0.497247706,0.499082569,
0.500917431,0.502752294,0.504587156,0.506422018,0.508256881,0.510091743,
0.511926606,0.513761468,0.51559633,0.517431193,0.519266055,0.521100917,
0.52293578,0.524770642,0.526605505,0.528440367,0.530275229,0.532110092,
0.533944954,0.535779817,0.537614679,0.539449541,0.541284404,0.543119266,
0.544954128,0.546788991,0.548623853,0.550458716,0.552293578,0.55412844,
0.555963303,0.557798165,0.559633028,0.56146789,0.563302752,0.565137615,
0.566972477,0.568807339,0.570642202,0.572477064,0.574311927,0.576146789,
0.577981651,0.579816514,0.581651376,0.583486239,0.585321101,0.587155963,
0.588990826,0.590825688,0.59266055,0.594495413,0.596330275,0.598165138,
0.6,0.601834862,0.603669725,0.605504587,0.60733945,0.609174312,0.611009174,
0.612844037,0.614678899,0.616513761,0.618348624,0.620183486,0.622018349,
0.623853211,0.625688073,0.627522936,0.629357798,0.631192661,0.633027523,
0.634862385,0.636697248,0.63853211,0.640366972,0.642201835,0.644036697,
0.64587156,0.647706422,0.649541284,0.651376147,0.653211009,0.655045872,
0.656880734,0.658715596,0.660550459,0.662385321,0.664220183,0.666055046,
0.667889908,0.669724771,0.671559633,0.673394495,0.675229358,0.67706422,
0.678899083,0.680733945,0.682568807,0.68440367,0.686238532,0.688073394,
0.689908257,0.691743119,0.693577982,0.695412844,0.697247706,0.699082569,
0.700917431,0.702752294,0.704587156,0.706422018,0.708256881,0.710091743,
0.711926606,0.713761468,0.71559633,0.717431193,0.719266055,0.721100917,
0.72293578,0.724770642,0.726605505,0.728440367,0.730275229,0.732110092,
0.733944954,0.735779817,0.737614679,0.739449541,0.741284404,0.743119266,
0.744954128,0.746788991,0.748623853,0.750458716,0.752293578,0.75412844,
0.755963303,0.757798165,0.759633028,0.76146789,0.763302752,0.765137615,
0.766972477,0.768807339,0.770642202,0.772477064,0.774311927,0.776146789,
0.777981651,0.779816514,0.781651376,0.783486239,0.785321101,0.787155963,
0.788990826,0.790825688,0.79266055,0.794495413,0.796330275,0.798165138,
0.8,0.801834862,0.803669725,0.805504587,0.80733945,0.809174312,0.811009174,
0.812844037,0.814678899,0.816513761,0.818348624,0.820183486,0.822018349,
0.823853211,0.825688073,0.827522936,0.829357798,0.831192661,0.833027523,
0.834862385,0.836697248,0.83853211,0.840366972,0.842201835,0.844036697,
0.84587156,0.847706422,0.849541284,0.851376147,0.853211009,0.855045872,
0.856880734,0.858715596,0.860550459,0.862385321,0.864220183,0.866055046,
0.867889908,0.869724771,0.871559633,0.873394495,0.875229358,0.87706422,
0.878899083,0.880733945,0.882568807,0.88440367,0.886238532,0.888073394,
0.889908257,0.891743119,0.893577982,0.895412844,0.897247706,0.899082569,
0.900917431,0.902752294,0.904587156,0.906422018,0.908256881,0.910091743,
0.911926606,0.913761468,0.91559633,0.917431193,0.919266055,0.921100917,
0.92293578,0.924770642,0.926605505,0.928440367,0.930275229,0.932110092,
0.933944954,0.935779817,0.937614679,0.939449541,0.941284404,0.943119266,
0.944954128,0.946788991,0.948623853,0.950458716,0.952293578,0.95412844,
0.955963303,0.957798165,0.959633028,0.96146789,0.963302752,0.965137615,
0.966972477,0.968807339,0.970642202,0.972477064,0.974311927,0.976146789,
0.977981651,0.979816514,0.981651376,0.983486239,0.985321101,0.987155963,
0.988990826,0.990825688,0.99266055,0.994495413,0.996330275,0.998165138,
1.),(0.,0.36),.UNSPECIFIED.);
#6244=B_SPLINE_SURFACE_WITH_KNOTS('',5,1,((#202700,#202701),(#202702,#202703),
(#202704,#202705),(#202706,#202707),(#202708,#202709),(#202710,#202711),
(#202712,#202713),(#202714,#202715),(#202716,#202717),(#202718,#202719),
(#202720,#202721),(#202722,#202723),(#202724,#202725),(#202726,#202727),
(#202728,#202729),(#202730,#202731),(#202732,#202733),(#202734,#202735),
(#202736,#202737),(#202738,#202739),(#202740,#202741),(#202742,#202743),
(#202744,#202745),(#202746,#202747),(#202748,#202749),(#202750,#202751),
(#202752,#202753),(#202754,#202755),(#202756,#202757),(#202758,#202759),
(#202760,#202761),(#202762,#202763),(#202764,#202765),(#202766,#202767),
(#202768,#202769),(#202770,#202771),(#202772,#202773),(#202774,#202775),
(#202776,#202777),(#202778,#202779),(#202780,#202781),(#202782,#202783),
(#202784,#202785),(#202786,#202787),(#202788,#202789),(#202790,#202791),
(#202792,#202793),(#202794,#202795),(#202796,#202797),(#202798,#202799),
(#202800,#202801),(#202802,#202803),(#202804,#202805),(#202806,#202807),
(#202808,#202809),(#202810,#202811),(#202812,#202813),(#202814,#202815),
(#202816,#202817),(#202818,#202819),(#202820,#202821),(#202822,#202823),
(#202824,#202825),(#202826,#202827),(#202828,#202829),(#202830,#202831),
(#202832,#202833),(#202834,#202835),(#202836,#202837),(#202838,#202839),
(#202840,#202841),(#202842,#202843),(#202844,#202845),(#202846,#202847),
(#202848,#202849),(#202850,#202851),(#202852,#202853),(#202854,#202855),
(#202856,#202857),(#202858,#202859),(#202860,#202861),(#202862,#202863),
(#202864,#202865),(#202866,#202867),(#202868,#202869),(#202870,#202871),
(#202872,#202873),(#202874,#202875),(#202876,#202877),(#202878,#202879),
(#202880,#202881),(#202882,#202883),(#202884,#202885),(#202886,#202887),
(#202888,#202889),(#202890,#202891),(#202892,#202893),(#202894,#202895),
(#202896,#202897),(#202898,#202899),(#202900,#202901),(#202902,#202903),
(#202904,#202905),(#202906,#202907),(#202908,#202909),(#202910,#202911),
(#202912,#202913),(#202914,#202915),(#202916,#202917),(#202918,#202919),
(#202920,#202921),(#202922,#202923),(#202924,#202925),(#202926,#202927),
(#202928,#202929),(#202930,#202931),(#202932,#202933),(#202934,#202935),
(#202936,#202937),(#202938,#202939),(#202940,#202941),(#202942,#202943),
(#202944,#202945),(#202946,#202947),(#202948,#202949),(#202950,#202951),
(#202952,#202953),(#202954,#202955),(#202956,#202957),(#202958,#202959),
(#202960,#202961),(#202962,#202963),(#202964,#202965),(#202966,#202967),
(#202968,#202969),(#202970,#202971),(#202972,#202973),(#202974,#202975),
(#202976,#202977),(#202978,#202979),(#202980,#202981),(#202982,#202983),
(#202984,#202985),(#202986,#202987),(#202988,#202989),(#202990,#202991),
(#202992,#202993),(#202994,#202995),(#202996,#202997),(#202998,#202999),
(#203000,#203001),(#203002,#203003),(#203004,#203005),(#203006,#203007),
(#203008,#203009),(#203010,#203011),(#203012,#203013),(#203014,#203015),
(#203016,#203017),(#203018,#203019),(#203020,#203021),(#203022,#203023),
(#203024,#203025),(#203026,#203027),(#203028,#203029),(#203030,#203031),
(#203032,#203033),(#203034,#203035),(#203036,#203037),(#203038,#203039),
(#203040,#203041),(#203042,#203043),(#203044,#203045),(#203046,#203047),
(#203048,#203049),(#203050,#203051),(#203052,#203053),(#203054,#203055),
(#203056,#203057),(#203058,#203059),(#203060,#203061),(#203062,#203063),
(#203064,#203065),(#203066,#203067),(#203068,#203069),(#203070,#203071),
(#203072,#203073),(#203074,#203075),(#203076,#203077),(#203078,#203079),
(#203080,#203081),(#203082,#203083),(#203084,#203085),(#203086,#203087),
(#203088,#203089),(#203090,#203091),(#203092,#203093),(#203094,#203095),
(#203096,#203097),(#203098,#203099),(#203100,#203101),(#203102,#203103),
(#203104,#203105),(#203106,#203107),(#203108,#203109),(#203110,#203111),
(#203112,#203113),(#203114,#203115),(#203116,#203117),(#203118,#203119),
(#203120,#203121),(#203122,#203123),(#203124,#203125),(#203126,#203127),
(#203128,#203129),(#203130,#203131),(#203132,#203133),(#203134,#203135),
(#203136,#203137),(#203138,#203139),(#203140,#203141),(#203142,#203143),
(#203144,#203145),(#203146,#203147),(#203148,#203149),(#203150,#203151),
(#203152,#203153),(#203154,#203155),(#203156,#203157),(#203158,#203159),
(#203160,#203161),(#203162,#203163),(#203164,#203165),(#203166,#203167),
(#203168,#203169),(#203170,#203171),(#203172,#203173),(#203174,#203175),
(#203176,#203177),(#203178,#203179),(#203180,#203181),(#203182,#203183),
(#203184,#203185),(#203186,#203187),(#203188,#203189),(#203190,#203191),
(#203192,#203193),(#203194,#203195),(#203196,#203197),(#203198,#203199),
(#203200,#203201),(#203202,#203203),(#203204,#203205),(#203206,#203207),
(#203208,#203209),(#203210,#203211),(#203212,#203213),(#203214,#203215),
(#203216,#203217),(#203218,#203219),(#203220,#203221),(#203222,#203223),
(#203224,#203225),(#203226,#203227),(#203228,#203229),(#203230,#203231),
(#203232,#203233),(#203234,#203235),(#203236,#203237),(#203238,#203239),
(#203240,#203241),(#203242,#203243),(#203244,#203245),(#203246,#203247),
(#203248,#203249),(#203250,#203251),(#203252,#203253),(#203254,#203255),
(#203256,#203257),(#203258,#203259),(#203260,#203261),(#203262,#203263),
(#203264,#203265),(#203266,#203267),(#203268,#203269),(#203270,#203271),
(#203272,#203273),(#203274,#203275),(#203276,#203277),(#203278,#203279),
(#203280,#203281),(#203282,#203283),(#203284,#203285),(#203286,#203287),
(#203288,#203289),(#203290,#203291),(#203292,#203293),(#203294,#203295),
(#203296,#203297),(#203298,#203299),(#203300,#203301),(#203302,#203303),
(#203304,#203305),(#203306,#203307),(#203308,#203309),(#203310,#203311),
(#203312,#203313),(#203314,#203315),(#203316,#203317),(#203318,#203319),
(#203320,#203321),(#203322,#203323),(#203324,#203325),(#203326,#203327),
(#203328,#203329),(#203330,#203331),(#203332,#203333),(#203334,#203335),
(#203336,#203337),(#203338,#203339),(#203340,#203341),(#203342,#203343),
(#203344,#203345),(#203346,#203347),(#203348,#203349),(#203350,#203351),
(#203352,#203353),(#203354,#203355),(#203356,#203357),(#203358,#203359),
(#203360,#203361),(#203362,#203363),(#203364,#203365),(#203366,#203367),
(#203368,#203369),(#203370,#203371),(#203372,#203373),(#203374,#203375),
(#203376,#203377),(#203378,#203379),(#203380,#203381),(#203382,#203383),
(#203384,#203385),(#203386,#203387),(#203388,#203389),(#203390,#203391),
(#203392,#203393),(#203394,#203395),(#203396,#203397),(#203398,#203399),
(#203400,#203401),(#203402,#203403),(#203404,#203405),(#203406,#203407),
(#203408,#203409),(#203410,#203411),(#203412,#203413),(#203414,#203415),
(#203416,#203417),(#203418,#203419),(#203420,#203421),(#203422,#203423),
(#203424,#203425),(#203426,#203427),(#203428,#203429),(#203430,#203431),
(#203432,#203433),(#203434,#203435),(#203436,#203437),(#203438,#203439),
(#203440,#203441),(#203442,#203443),(#203444,#203445),(#203446,#203447),
(#203448,#203449),(#203450,#203451),(#203452,#203453),(#203454,#203455),
(#203456,#203457),(#203458,#203459),(#203460,#203461),(#203462,#203463),
(#203464,#203465),(#203466,#203467),(#203468,#203469),(#203470,#203471),
(#203472,#203473),(#203474,#203475),(#203476,#203477),(#203478,#203479),
(#203480,#203481),(#203482,#203483),(#203484,#203485),(#203486,#203487),
(#203488,#203489),(#203490,#203491),(#203492,#203493),(#203494,#203495),
(#203496,#203497),(#203498,#203499),(#203500,#203501),(#203502,#203503),
(#203504,#203505),(#203506,#203507),(#203508,#203509),(#203510,#203511),
(#203512,#203513),(#203514,#203515),(#203516,#203517),(#203518,#203519),
(#203520,#203521),(#203522,#203523),(#203524,#203525),(#203526,#203527),
(#203528,#203529),(#203530,#203531),(#203532,#203533),(#203534,#203535),
(#203536,#203537),(#203538,#203539),(#203540,#203541),(#203542,#203543),
(#203544,#203545),(#203546,#203547),(#203548,#203549),(#203550,#203551),
(#203552,#203553),(#203554,#203555),(#203556,#203557),(#203558,#203559),
(#203560,#203561),(#203562,#203563),(#203564,#203565),(#203566,#203567),
(#203568,#203569),(#203570,#203571),(#203572,#203573),(#203574,#203575),
(#203576,#203577),(#203578,#203579),(#203580,#203581),(#203582,#203583),
(#203584,#203585),(#203586,#203587),(#203588,#203589),(#203590,#203591),
(#203592,#203593),(#203594,#203595),(#203596,#203597),(#203598,#203599),
(#203600,#203601),(#203602,#203603),(#203604,#203605),(#203606,#203607),
(#203608,#203609),(#203610,#203611),(#203612,#203613),(#203614,#203615),
(#203616,#203617),(#203618,#203619),(#203620,#203621),(#203622,#203623),
(#203624,#203625),(#203626,#203627),(#203628,#203629),(#203630,#203631),
(#203632,#203633),(#203634,#203635),(#203636,#203637),(#203638,#203639),
(#203640,#203641),(#203642,#203643)),.UNSPECIFIED.,.F.,.F.,.F.,(6,1,1,1,
1,1,1,1,1,1,1,1,1,1,1,1,1,1,1,1,1,1,1,1,1,1,1,1,1,1,1,1,1,1,1,1,1,1,1,1,
1,1,1,1,1,1,1,1,1,1,1,1,1,1,1,1,1,1,1,1,1,1,1,1,1,1,1,1,1,1,1,1,1,1,1,1,
1,1,1,1,1,1,1,1,1,1,1,1,1,1,1,1,1,1,1,1,1,1,1,1,1,1,1,1,1,1,1,1,1,1,1,1,
1,1,1,1,1,1,1,1,1,1,1,1,1,1,1,1,1,1,1,1,1,1,1,1,1,1,1,1,1,1,1,1,1,1,1,1,
1,1,1,1,1,1,1,1,1,1,1,1,1,1,1,1,1,1,1,1,1,1,1,1,1,1,1,1,1,1,1,1,1,1,1,1,
1,1,1,1,1,1,1,1,1,1,1,1,1,1,1,1,1,1,1,1,1,1,1,1,1,1,1,1,1,1,1,1,1,1,1,1,
1,1,1,1,1,1,1,1,1,1,1,1,1,1,1,1,1,1,1,1,1,1,1,1,1,1,1,1,1,1,1,1,1,1,1,1,
1,1,1,1,1,1,1,1,1,1,1,1,1,1,1,1,1,1,1,1,1,1,1,1,1,1,1,1,1,1,1,1,1,1,1,1,
1,1,1,1,1,1,1,1,1,1,1,1,1,1,1,1,1,1,1,1,1,1,1,1,1,1,1,1,1,1,1,1,1,1,1,1,
1,1,1,1,1,1,1,1,1,1,1,1,1,1,1,1,1,1,1,1,1,1,1,1,1,1,1,1,1,1,1,1,1,1,1,1,
1,1,1,1,1,1,1,1,1,1,1,1,1,1,1,1,1,1,1,1,1,1,1,1,1,1,1,1,1,1,1,1,1,1,1,1,
1,1,1,1,1,1,1,1,1,1,1,1,1,1,1,1,1,1,1,1,1,1,1,1,1,1,1,1,1,1,1,1,1,1,1,1,
1,1,1,1,1,1,1,1,1,1,1,1,1,1,1,1,1,1,1,1,1,1,1,1,1,1,1,1,1,1,1,6),(2,2),
(-1.,-0.998165138,-0.996330275,-0.994495413,-0.99266055,-0.990825688,-0.988990826,
-0.987155963,-0.985321101,-0.983486239,-0.981651376,-0.979816514,-0.977981651,
-0.976146789,-0.974311927,-0.972477064,-0.970642202,-0.968807339,-0.966972477,
-0.965137615,-0.963302752,-0.96146789,-0.959633028,-0.957798165,-0.955963303,
-0.95412844,-0.952293578,-0.950458716,-0.948623853,-0.946788991,-0.944954128,
-0.943119266,-0.941284404,-0.939449541,-0.937614679,-0.935779817,-0.933944954,
-0.932110092,-0.930275229,-0.928440367,-0.926605505,-0.924770642,-0.92293578,
-0.921100917,-0.919266055,-0.917431193,-0.91559633,-0.913761468,-0.911926606,
-0.910091743,-0.908256881,-0.906422018,-0.904587156,-0.902752294,-0.900917431,
-0.899082569,-0.897247706,-0.895412844,-0.893577982,-0.891743119,-0.889908257,
-0.888073394,-0.886238532,-0.88440367,-0.882568807,-0.880733945,-0.878899083,
-0.87706422,-0.875229358,-0.873394495,-0.871559633,-0.869724771,-0.867889908,
-0.866055046,-0.864220183,-0.862385321,-0.860550459,-0.858715596,-0.856880734,
-0.855045872,-0.853211009,-0.851376147,-0.849541284,-0.847706422,-0.84587156,
-0.844036697,-0.842201835,-0.840366972,-0.83853211,-0.836697248,-0.834862385,
-0.833027523,-0.831192661,-0.829357798,-0.827522936,-0.825688073,-0.823853211,
-0.822018349,-0.820183486,-0.818348624,-0.816513761,-0.814678899,-0.812844037,
-0.811009174,-0.809174312,-0.80733945,-0.805504587,-0.803669725,-0.801834862,
-0.8,-0.798165138,-0.796330275,-0.794495413,-0.79266055,-0.790825688,-0.788990826,
-0.787155963,-0.785321101,-0.783486239,-0.781651376,-0.779816514,-0.777981651,
-0.776146789,-0.774311927,-0.772477064,-0.770642202,-0.768807339,-0.766972477,
-0.765137615,-0.763302752,-0.76146789,-0.759633028,-0.757798165,-0.755963303,
-0.75412844,-0.752293578,-0.750458716,-0.748623853,-0.746788991,-0.744954128,
-0.743119266,-0.741284404,-0.739449541,-0.737614679,-0.735779817,-0.733944954,
-0.732110092,-0.730275229,-0.728440367,-0.726605505,-0.724770642,-0.72293578,
-0.721100917,-0.719266055,-0.717431193,-0.71559633,-0.713761468,-0.711926606,
-0.710091743,-0.708256881,-0.706422018,-0.704587156,-0.702752294,-0.700917431,
-0.699082569,-0.697247706,-0.695412844,-0.693577982,-0.691743119,-0.689908257,
-0.688073394,-0.686238532,-0.68440367,-0.682568807,-0.680733945,-0.678899083,
-0.67706422,-0.675229358,-0.673394495,-0.671559633,-0.669724771,-0.667889908,
-0.666055046,-0.664220183,-0.662385321,-0.660550459,-0.658715596,-0.656880734,
-0.655045872,-0.653211009,-0.651376147,-0.649541284,-0.647706422,-0.64587156,
-0.644036697,-0.642201835,-0.640366972,-0.63853211,-0.636697248,-0.634862385,
-0.633027523,-0.631192661,-0.629357798,-0.627522936,-0.625688073,-0.623853211,
-0.622018349,-0.620183486,-0.618348624,-0.616513761,-0.614678899,-0.612844037,
-0.611009174,-0.609174312,-0.60733945,-0.605504587,-0.603669725,-0.601834862,
-0.6,-0.598165138,-0.596330275,-0.594495413,-0.59266055,-0.590825688,-0.588990826,
-0.587155963,-0.585321101,-0.583486239,-0.581651376,-0.579816514,-0.577981651,
-0.576146789,-0.574311927,-0.572477064,-0.570642202,-0.568807339,-0.566972477,
-0.565137615,-0.563302752,-0.56146789,-0.559633028,-0.557798165,-0.555963303,
-0.55412844,-0.552293578,-0.550458716,-0.548623853,-0.546788991,-0.544954128,
-0.543119266,-0.541284404,-0.539449541,-0.537614679,-0.535779817,-0.533944954,
-0.532110092,-0.530275229,-0.528440367,-0.526605505,-0.524770642,-0.52293578,
-0.521100917,-0.519266055,-0.517431193,-0.51559633,-0.513761468,-0.511926606,
-0.510091743,-0.508256881,-0.506422018,-0.504587156,-0.502752294,-0.500917431,
-0.499082569,-0.497247706,-0.495412844,-0.493577982,-0.491743119,-0.489908257,
-0.488073394,-0.486238532,-0.48440367,-0.482568807,-0.480733945,-0.478899083,
-0.47706422,-0.475229358,-0.473394495,-0.471559633,-0.469724771,-0.467889908,
-0.466055046,-0.464220183,-0.462385321,-0.460550459,-0.458715596,-0.456880734,
-0.455045872,-0.453211009,-0.451376147,-0.449541284,-0.447706422,-0.44587156,
-0.444036697,-0.442201835,-0.440366972,-0.43853211,-0.436697248,-0.434862385,
-0.433027523,-0.431192661,-0.429357798,-0.427522936,-0.425688073,-0.423853211,
-0.422018349,-0.420183486,-0.418348624,-0.416513761,-0.414678899,-0.412844037,
-0.411009174,-0.409174312,-0.40733945,-0.405504587,-0.403669725,-0.401834862,
-0.4,-0.398165138,-0.396330275,-0.394495413,-0.39266055,-0.390825688,-0.388990826,
-0.387155963,-0.385321101,-0.383486239,-0.381651376,-0.379816514,-0.377981651,
-0.376146789,-0.374311927,-0.372477064,-0.370642202,-0.368807339,-0.366972477,
-0.365137615,-0.363302752,-0.36146789,-0.359633028,-0.357798165,-0.355963303,
-0.35412844,-0.352293578,-0.350458716,-0.348623853,-0.346788991,-0.344954128,
-0.343119266,-0.341284404,-0.339449541,-0.337614679,-0.335779817,-0.333944954,
-0.332110092,-0.330275229,-0.328440367,-0.326605505,-0.324770642,-0.32293578,
-0.321100917,-0.319266055,-0.317431193,-0.31559633,-0.313761468,-0.311926606,
-0.310091743,-0.308256881,-0.306422018,-0.304587156,-0.302752294,-0.300917431,
-0.299082569,-0.297247706,-0.295412844,-0.293577982,-0.291743119,-0.289908257,
-0.288073394,-0.286238532,-0.28440367,-0.282568807,-0.280733945,-0.278899083,
-0.27706422,-0.275229358,-0.273394495,-0.271559633,-0.269724771,-0.267889908,
-0.266055046,-0.264220183,-0.262385321,-0.260550459,-0.258715596,-0.256880734,
-0.255045872,-0.253211009,-0.251376147,-0.249541284,-0.247706422,-0.24587156,
-0.244036697,-0.242201835,-0.240366972,-0.23853211,-0.236697248,-0.234862385,
-0.233027523,-0.231192661,-0.229357798,-0.227522936,-0.225688073,-0.223853211,
-0.222018349,-0.220183486,-0.218348624,-0.216513761,-0.214678899,-0.212844037,
-0.211009174,-0.209174312,-0.20733945,-0.205504587,-0.203669725,-0.201834862,
-0.2,-0.198165138,-0.196330275,-0.194495413,-0.19266055,-0.190825688,-0.188990826,
-0.187155963,-0.185321101,-0.183486239,-0.181651376,-0.179816514,-0.177981651,
-0.176146789,-0.174311927,-0.172477064,-0.170642202,-0.168807339,-0.166972477,
-0.165137615,-0.163302752,-0.16146789,-0.159633028,-0.157798165,-0.155963303,
-0.15412844,-0.152293578,-0.150458716,-0.148623853,-0.146788991,-0.144954128,
-0.143172103),(0.,0.36),.UNSPECIFIED.);
#6245=B_SPLINE_SURFACE_WITH_KNOTS('',5,1,((#204294,#204295),(#204296,#204297),
(#204298,#204299),(#204300,#204301),(#204302,#204303),(#204304,#204305),
(#204306,#204307),(#204308,#204309),(#204310,#204311),(#204312,#204313),
(#204314,#204315),(#204316,#204317),(#204318,#204319),(#204320,#204321),
(#204322,#204323),(#204324,#204325),(#204326,#204327),(#204328,#204329),
(#204330,#204331),(#204332,#204333),(#204334,#204335),(#204336,#204337),
(#204338,#204339),(#204340,#204341),(#204342,#204343),(#204344,#204345),
(#204346,#204347),(#204348,#204349),(#204350,#204351),(#204352,#204353),
(#204354,#204355),(#204356,#204357),(#204358,#204359),(#204360,#204361),
(#204362,#204363),(#204364,#204365),(#204366,#204367),(#204368,#204369),
(#204370,#204371),(#204372,#204373),(#204374,#204375),(#204376,#204377),
(#204378,#204379),(#204380,#204381),(#204382,#204383),(#204384,#204385),
(#204386,#204387),(#204388,#204389),(#204390,#204391),(#204392,#204393),
(#204394,#204395),(#204396,#204397),(#204398,#204399),(#204400,#204401),
(#204402,#204403),(#204404,#204405),(#204406,#204407),(#204408,#204409),
(#204410,#204411),(#204412,#204413),(#204414,#204415),(#204416,#204417),
(#204418,#204419),(#204420,#204421),(#204422,#204423),(#204424,#204425),
(#204426,#204427),(#204428,#204429),(#204430,#204431),(#204432,#204433),
(#204434,#204435),(#204436,#204437),(#204438,#204439),(#204440,#204441),
(#204442,#204443),(#204444,#204445),(#204446,#204447),(#204448,#204449),
(#204450,#204451),(#204452,#204453),(#204454,#204455),(#204456,#204457),
(#204458,#204459),(#204460,#204461),(#204462,#204463),(#204464,#204465),
(#204466,#204467),(#204468,#204469),(#204470,#204471),(#204472,#204473),
(#204474,#204475),(#204476,#204477),(#204478,#204479),(#204480,#204481),
(#204482,#204483),(#204484,#204485),(#204486,#204487),(#204488,#204489),
(#204490,#204491),(#204492,#204493),(#204494,#204495),(#204496,#204497),
(#204498,#204499),(#204500,#204501),(#204502,#204503),(#204504,#204505),
(#204506,#204507),(#204508,#204509),(#204510,#204511),(#204512,#204513),
(#204514,#204515),(#204516,#204517),(#204518,#204519),(#204520,#204521),
(#204522,#204523),(#204524,#204525),(#204526,#204527),(#204528,#204529),
(#204530,#204531),(#204532,#204533),(#204534,#204535),(#204536,#204537),
(#204538,#204539),(#204540,#204541),(#204542,#204543),(#204544,#204545),
(#204546,#204547),(#204548,#204549),(#204550,#204551),(#204552,#204553),
(#204554,#204555),(#204556,#204557),(#204558,#204559),(#204560,#204561),
(#204562,#204563),(#204564,#204565),(#204566,#204567),(#204568,#204569),
(#204570,#204571),(#204572,#204573),(#204574,#204575),(#204576,#204577),
(#204578,#204579),(#204580,#204581),(#204582,#204583),(#204584,#204585),
(#204586,#204587),(#204588,#204589),(#204590,#204591),(#204592,#204593),
(#204594,#204595),(#204596,#204597),(#204598,#204599),(#204600,#204601),
(#204602,#204603),(#204604,#204605),(#204606,#204607),(#204608,#204609),
(#204610,#204611),(#204612,#204613),(#204614,#204615),(#204616,#204617),
(#204618,#204619),(#204620,#204621),(#204622,#204623),(#204624,#204625),
(#204626,#204627),(#204628,#204629),(#204630,#204631),(#204632,#204633),
(#204634,#204635),(#204636,#204637),(#204638,#204639),(#204640,#204641),
(#204642,#204643),(#204644,#204645),(#204646,#204647),(#204648,#204649),
(#204650,#204651),(#204652,#204653),(#204654,#204655),(#204656,#204657),
(#204658,#204659),(#204660,#204661),(#204662,#204663),(#204664,#204665),
(#204666,#204667),(#204668,#204669),(#204670,#204671),(#204672,#204673),
(#204674,#204675),(#204676,#204677),(#204678,#204679),(#204680,#204681),
(#204682,#204683),(#204684,#204685),(#204686,#204687),(#204688,#204689),
(#204690,#204691),(#204692,#204693),(#204694,#204695),(#204696,#204697),
(#204698,#204699),(#204700,#204701),(#204702,#204703),(#204704,#204705),
(#204706,#204707),(#204708,#204709),(#204710,#204711),(#204712,#204713),
(#204714,#204715),(#204716,#204717),(#204718,#204719),(#204720,#204721),
(#204722,#204723),(#204724,#204725),(#204726,#204727),(#204728,#204729),
(#204730,#204731),(#204732,#204733),(#204734,#204735),(#204736,#204737),
(#204738,#204739),(#204740,#204741),(#204742,#204743),(#204744,#204745),
(#204746,#204747),(#204748,#204749),(#204750,#204751),(#204752,#204753),
(#204754,#204755),(#204756,#204757),(#204758,#204759),(#204760,#204761),
(#204762,#204763),(#204764,#204765),(#204766,#204767),(#204768,#204769),
(#204770,#204771),(#204772,#204773),(#204774,#204775),(#204776,#204777),
(#204778,#204779),(#204780,#204781),(#204782,#204783),(#204784,#204785),
(#204786,#204787),(#204788,#204789),(#204790,#204791),(#204792,#204793),
(#204794,#204795),(#204796,#204797),(#204798,#204799),(#204800,#204801),
(#204802,#204803),(#204804,#204805),(#204806,#204807),(#204808,#204809),
(#204810,#204811),(#204812,#204813),(#204814,#204815),(#204816,#204817),
(#204818,#204819),(#204820,#204821),(#204822,#204823),(#204824,#204825),
(#204826,#204827),(#204828,#204829),(#204830,#204831),(#204832,#204833),
(#204834,#204835),(#204836,#204837),(#204838,#204839),(#204840,#204841),
(#204842,#204843),(#204844,#204845),(#204846,#204847),(#204848,#204849),
(#204850,#204851),(#204852,#204853),(#204854,#204855),(#204856,#204857),
(#204858,#204859),(#204860,#204861),(#204862,#204863),(#204864,#204865),
(#204866,#204867),(#204868,#204869),(#204870,#204871),(#204872,#204873),
(#204874,#204875),(#204876,#204877),(#204878,#204879),(#204880,#204881),
(#204882,#204883),(#204884,#204885),(#204886,#204887),(#204888,#204889),
(#204890,#204891),(#204892,#204893),(#204894,#204895),(#204896,#204897),
(#204898,#204899),(#204900,#204901),(#204902,#204903),(#204904,#204905),
(#204906,#204907),(#204908,#204909),(#204910,#204911),(#204912,#204913),
(#204914,#204915),(#204916,#204917),(#204918,#204919),(#204920,#204921),
(#204922,#204923),(#204924,#204925),(#204926,#204927),(#204928,#204929),
(#204930,#204931),(#204932,#204933),(#204934,#204935),(#204936,#204937),
(#204938,#204939),(#204940,#204941),(#204942,#204943),(#204944,#204945),
(#204946,#204947),(#204948,#204949),(#204950,#204951),(#204952,#204953),
(#204954,#204955),(#204956,#204957),(#204958,#204959),(#204960,#204961),
(#204962,#204963),(#204964,#204965),(#204966,#204967),(#204968,#204969),
(#204970,#204971),(#204972,#204973),(#204974,#204975),(#204976,#204977),
(#204978,#204979),(#204980,#204981),(#204982,#204983),(#204984,#204985),
(#204986,#204987),(#204988,#204989),(#204990,#204991),(#204992,#204993),
(#204994,#204995),(#204996,#204997),(#204998,#204999),(#205000,#205001),
(#205002,#205003),(#205004,#205005),(#205006,#205007),(#205008,#205009),
(#205010,#205011),(#205012,#205013),(#205014,#205015),(#205016,#205017),
(#205018,#205019),(#205020,#205021),(#205022,#205023),(#205024,#205025),
(#205026,#205027),(#205028,#205029),(#205030,#205031),(#205032,#205033),
(#205034,#205035),(#205036,#205037),(#205038,#205039),(#205040,#205041),
(#205042,#205043),(#205044,#205045),(#205046,#205047),(#205048,#205049),
(#205050,#205051),(#205052,#205053),(#205054,#205055),(#205056,#205057),
(#205058,#205059),(#205060,#205061),(#205062,#205063),(#205064,#205065),
(#205066,#205067),(#205068,#205069),(#205070,#205071),(#205072,#205073),
(#205074,#205075),(#205076,#205077),(#205078,#205079),(#205080,#205081),
(#205082,#205083),(#205084,#205085),(#205086,#205087),(#205088,#205089),
(#205090,#205091),(#205092,#205093),(#205094,#205095),(#205096,#205097),
(#205098,#205099),(#205100,#205101),(#205102,#205103),(#205104,#205105),
(#205106,#205107),(#205108,#205109),(#205110,#205111),(#205112,#205113),
(#205114,#205115),(#205116,#205117),(#205118,#205119),(#205120,#205121),
(#205122,#205123),(#205124,#205125),(#205126,#205127),(#205128,#205129),
(#205130,#205131),(#205132,#205133),(#205134,#205135),(#205136,#205137),
(#205138,#205139),(#205140,#205141),(#205142,#205143),(#205144,#205145),
(#205146,#205147),(#205148,#205149),(#205150,#205151),(#205152,#205153),
(#205154,#205155),(#205156,#205157),(#205158,#205159),(#205160,#205161),
(#205162,#205163),(#205164,#205165),(#205166,#205167),(#205168,#205169),
(#205170,#205171),(#205172,#205173),(#205174,#205175),(#205176,#205177),
(#205178,#205179),(#205180,#205181),(#205182,#205183),(#205184,#205185),
(#205186,#205187),(#205188,#205189),(#205190,#205191),(#205192,#205193),
(#205194,#205195),(#205196,#205197),(#205198,#205199),(#205200,#205201),
(#205202,#205203),(#205204,#205205),(#205206,#205207),(#205208,#205209),
(#205210,#205211),(#205212,#205213),(#205214,#205215),(#205216,#205217),
(#205218,#205219),(#205220,#205221),(#205222,#205223),(#205224,#205225),
(#205226,#205227),(#205228,#205229),(#205230,#205231),(#205232,#205233),
(#205234,#205235),(#205236,#205237)),.UNSPECIFIED.,.F.,.F.,.F.,(6,1,1,1,
1,1,1,1,1,1,1,1,1,1,1,1,1,1,1,1,1,1,1,1,1,1,1,1,1,1,1,1,1,1,1,1,1,1,1,1,
1,1,1,1,1,1,1,1,1,1,1,1,1,1,1,1,1,1,1,1,1,1,1,1,1,1,1,1,1,1,1,1,1,1,1,1,
1,1,1,1,1,1,1,1,1,1,1,1,1,1,1,1,1,1,1,1,1,1,1,1,1,1,1,1,1,1,1,1,1,1,1,1,
1,1,1,1,1,1,1,1,1,1,1,1,1,1,1,1,1,1,1,1,1,1,1,1,1,1,1,1,1,1,1,1,1,1,1,1,
1,1,1,1,1,1,1,1,1,1,1,1,1,1,1,1,1,1,1,1,1,1,1,1,1,1,1,1,1,1,1,1,1,1,1,1,
1,1,1,1,1,1,1,1,1,1,1,1,1,1,1,1,1,1,1,1,1,1,1,1,1,1,1,1,1,1,1,1,1,1,1,1,
1,1,1,1,1,1,1,1,1,1,1,1,1,1,1,1,1,1,1,1,1,1,1,1,1,1,1,1,1,1,1,1,1,1,1,1,
1,1,1,1,1,1,1,1,1,1,1,1,1,1,1,1,1,1,1,1,1,1,1,1,1,1,1,1,1,1,1,1,1,1,1,1,
1,1,1,1,1,1,1,1,1,1,1,1,1,1,1,1,1,1,1,1,1,1,1,1,1,1,1,1,1,1,1,1,1,1,1,1,
1,1,1,1,1,1,1,1,1,1,1,1,1,1,1,1,1,1,1,1,1,1,1,1,1,1,1,1,1,1,1,1,1,1,1,1,
1,1,1,1,1,1,1,1,1,1,1,1,1,1,1,1,1,1,1,1,1,1,1,1,1,1,1,1,1,1,1,1,1,1,1,1,
1,1,1,1,1,1,1,1,1,1,1,1,1,1,1,1,1,1,1,1,1,1,1,1,1,1,1,1,1,1,1,1,1,1,1,1,
1,1,1,1,1,1,1,1,1,1,1,1,1,1,1,1,1,1,1,1,1,1,1,1,1,1,1,1,1,1,1,6),(2,2),
(-1.,-0.998165138,-0.996330275,-0.994495413,-0.99266055,-0.990825688,-0.988990826,
-0.987155963,-0.985321101,-0.983486239,-0.981651376,-0.979816514,-0.977981651,
-0.976146789,-0.974311927,-0.972477064,-0.970642202,-0.968807339,-0.966972477,
-0.965137615,-0.963302752,-0.96146789,-0.959633028,-0.957798165,-0.955963303,
-0.95412844,-0.952293578,-0.950458716,-0.948623853,-0.946788991,-0.944954128,
-0.943119266,-0.941284404,-0.939449541,-0.937614679,-0.935779817,-0.933944954,
-0.932110092,-0.930275229,-0.928440367,-0.926605505,-0.924770642,-0.92293578,
-0.921100917,-0.919266055,-0.917431193,-0.91559633,-0.913761468,-0.911926606,
-0.910091743,-0.908256881,-0.906422018,-0.904587156,-0.902752294,-0.900917431,
-0.899082569,-0.897247706,-0.895412844,-0.893577982,-0.891743119,-0.889908257,
-0.888073394,-0.886238532,-0.88440367,-0.882568807,-0.880733945,-0.878899083,
-0.87706422,-0.875229358,-0.873394495,-0.871559633,-0.869724771,-0.867889908,
-0.866055046,-0.864220183,-0.862385321,-0.860550459,-0.858715596,-0.856880734,
-0.855045872,-0.853211009,-0.851376147,-0.849541284,-0.847706422,-0.84587156,
-0.844036697,-0.842201835,-0.840366972,-0.83853211,-0.836697248,-0.834862385,
-0.833027523,-0.831192661,-0.829357798,-0.827522936,-0.825688073,-0.823853211,
-0.822018349,-0.820183486,-0.818348624,-0.816513761,-0.814678899,-0.812844037,
-0.811009174,-0.809174312,-0.80733945,-0.805504587,-0.803669725,-0.801834862,
-0.8,-0.798165138,-0.796330275,-0.794495413,-0.79266055,-0.790825688,-0.788990826,
-0.787155963,-0.785321101,-0.783486239,-0.781651376,-0.779816514,-0.777981651,
-0.776146789,-0.774311927,-0.772477064,-0.770642202,-0.768807339,-0.766972477,
-0.765137615,-0.763302752,-0.76146789,-0.759633028,-0.757798165,-0.755963303,
-0.75412844,-0.752293578,-0.750458716,-0.748623853,-0.746788991,-0.744954128,
-0.743119266,-0.741284404,-0.739449541,-0.737614679,-0.735779817,-0.733944954,
-0.732110092,-0.730275229,-0.728440367,-0.726605505,-0.724770642,-0.72293578,
-0.721100917,-0.719266055,-0.717431193,-0.71559633,-0.713761468,-0.711926606,
-0.710091743,-0.708256881,-0.706422018,-0.704587156,-0.702752294,-0.700917431,
-0.699082569,-0.697247706,-0.695412844,-0.693577982,-0.691743119,-0.689908257,
-0.688073394,-0.686238532,-0.68440367,-0.682568807,-0.680733945,-0.678899083,
-0.67706422,-0.675229358,-0.673394495,-0.671559633,-0.669724771,-0.667889908,
-0.666055046,-0.664220183,-0.662385321,-0.660550459,-0.658715596,-0.656880734,
-0.655045872,-0.653211009,-0.651376147,-0.649541284,-0.647706422,-0.64587156,
-0.644036697,-0.642201835,-0.640366972,-0.63853211,-0.636697248,-0.634862385,
-0.633027523,-0.631192661,-0.629357798,-0.627522936,-0.625688073,-0.623853211,
-0.622018349,-0.620183486,-0.618348624,-0.616513761,-0.614678899,-0.612844037,
-0.611009174,-0.609174312,-0.60733945,-0.605504587,-0.603669725,-0.601834862,
-0.6,-0.598165138,-0.596330275,-0.594495413,-0.59266055,-0.590825688,-0.588990826,
-0.587155963,-0.585321101,-0.583486239,-0.581651376,-0.579816514,-0.577981651,
-0.576146789,-0.574311927,-0.572477064,-0.570642202,-0.568807339,-0.566972477,
-0.565137615,-0.563302752,-0.56146789,-0.559633028,-0.557798165,-0.555963303,
-0.55412844,-0.552293578,-0.550458716,-0.548623853,-0.546788991,-0.544954128,
-0.543119266,-0.541284404,-0.539449541,-0.537614679,-0.535779817,-0.533944954,
-0.532110092,-0.530275229,-0.528440367,-0.526605505,-0.524770642,-0.52293578,
-0.521100917,-0.519266055,-0.517431193,-0.51559633,-0.513761468,-0.511926606,
-0.510091743,-0.508256881,-0.506422018,-0.504587156,-0.502752294,-0.500917431,
-0.499082569,-0.497247706,-0.495412844,-0.493577982,-0.491743119,-0.489908257,
-0.488073394,-0.486238532,-0.48440367,-0.482568807,-0.480733945,-0.478899083,
-0.47706422,-0.475229358,-0.473394495,-0.471559633,-0.469724771,-0.467889908,
-0.466055046,-0.464220183,-0.462385321,-0.460550459,-0.458715596,-0.456880734,
-0.455045872,-0.453211009,-0.451376147,-0.449541284,-0.447706422,-0.44587156,
-0.444036697,-0.442201835,-0.440366972,-0.43853211,-0.436697248,-0.434862385,
-0.433027523,-0.431192661,-0.429357798,-0.427522936,-0.425688073,-0.423853211,
-0.422018349,-0.420183486,-0.418348624,-0.416513761,-0.414678899,-0.412844037,
-0.411009174,-0.409174312,-0.40733945,-0.405504587,-0.403669725,-0.401834862,
-0.4,-0.398165138,-0.396330275,-0.394495413,-0.39266055,-0.390825688,-0.388990826,
-0.387155963,-0.385321101,-0.383486239,-0.381651376,-0.379816514,-0.377981651,
-0.376146789,-0.374311927,-0.372477064,-0.370642202,-0.368807339,-0.366972477,
-0.365137615,-0.363302752,-0.36146789,-0.359633028,-0.357798165,-0.355963303,
-0.35412844,-0.352293578,-0.350458716,-0.348623853,-0.346788991,-0.344954128,
-0.343119266,-0.341284404,-0.339449541,-0.337614679,-0.335779817,-0.333944954,
-0.332110092,-0.330275229,-0.328440367,-0.326605505,-0.324770642,-0.32293578,
-0.321100917,-0.319266055,-0.317431193,-0.31559633,-0.313761468,-0.311926606,
-0.310091743,-0.308256881,-0.306422018,-0.304587156,-0.302752294,-0.300917431,
-0.299082569,-0.297247706,-0.295412844,-0.293577982,-0.291743119,-0.289908257,
-0.288073394,-0.286238532,-0.28440367,-0.282568807,-0.280733945,-0.278899083,
-0.27706422,-0.275229358,-0.273394495,-0.271559633,-0.269724771,-0.267889908,
-0.266055046,-0.264220183,-0.262385321,-0.260550459,-0.258715596,-0.256880734,
-0.255045872,-0.253211009,-0.251376147,-0.249541284,-0.247706422,-0.24587156,
-0.244036697,-0.242201835,-0.240366972,-0.23853211,-0.236697248,-0.234862385,
-0.233027523,-0.231192661,-0.229357798,-0.227522936,-0.225688073,-0.223853211,
-0.222018349,-0.220183486,-0.218348624,-0.216513761,-0.214678899,-0.212844037,
-0.211009174,-0.209174312,-0.20733945,-0.205504587,-0.203669725,-0.201834862,
-0.2,-0.198165138,-0.196330275,-0.194495413,-0.19266055,-0.190825688,-0.188990826,
-0.187155963,-0.185321101,-0.183486239,-0.181651376,-0.179816514,-0.177981651,
-0.176146789,-0.174311927,-0.172477064,-0.170642202,-0.168807339,-0.166972477,
-0.165137615,-0.163302752,-0.16146789,-0.159633028,-0.157798165,-0.155963303,
-0.15412844,-0.152293578,-0.150458716,-0.148623853,-0.146788991,-0.144954128,
-0.143172103),(0.,0.36),.UNSPECIFIED.);
#6246=B_SPLINE_SURFACE_WITH_KNOTS('',5,1,((#205867,#205868),(#205869,#205870),
(#205871,#205872),(#205873,#205874),(#205875,#205876),(#205877,#205878),
(#205879,#205880),(#205881,#205882),(#205883,#205884),(#205885,#205886),
(#205887,#205888),(#205889,#205890),(#205891,#205892),(#205893,#205894),
(#205895,#205896),(#205897,#205898),(#205899,#205900),(#205901,#205902),
(#205903,#205904),(#205905,#205906),(#205907,#205908),(#205909,#205910),
(#205911,#205912),(#205913,#205914),(#205915,#205916),(#205917,#205918),
(#205919,#205920),(#205921,#205922),(#205923,#205924),(#205925,#205926),
(#205927,#205928),(#205929,#205930),(#205931,#205932),(#205933,#205934),
(#205935,#205936),(#205937,#205938),(#205939,#205940),(#205941,#205942),
(#205943,#205944),(#205945,#205946),(#205947,#205948),(#205949,#205950),
(#205951,#205952),(#205953,#205954),(#205955,#205956),(#205957,#205958),
(#205959,#205960),(#205961,#205962),(#205963,#205964),(#205965,#205966),
(#205967,#205968),(#205969,#205970),(#205971,#205972),(#205973,#205974),
(#205975,#205976),(#205977,#205978),(#205979,#205980),(#205981,#205982),
(#205983,#205984),(#205985,#205986),(#205987,#205988),(#205989,#205990),
(#205991,#205992),(#205993,#205994),(#205995,#205996),(#205997,#205998),
(#205999,#206000),(#206001,#206002),(#206003,#206004),(#206005,#206006),
(#206007,#206008),(#206009,#206010),(#206011,#206012),(#206013,#206014),
(#206015,#206016),(#206017,#206018),(#206019,#206020),(#206021,#206022),
(#206023,#206024),(#206025,#206026),(#206027,#206028),(#206029,#206030),
(#206031,#206032),(#206033,#206034),(#206035,#206036),(#206037,#206038),
(#206039,#206040),(#206041,#206042),(#206043,#206044),(#206045,#206046),
(#206047,#206048),(#206049,#206050),(#206051,#206052),(#206053,#206054),
(#206055,#206056),(#206057,#206058),(#206059,#206060),(#206061,#206062),
(#206063,#206064),(#206065,#206066),(#206067,#206068),(#206069,#206070),
(#206071,#206072),(#206073,#206074),(#206075,#206076),(#206077,#206078),
(#206079,#206080),(#206081,#206082),(#206083,#206084),(#206085,#206086),
(#206087,#206088),(#206089,#206090),(#206091,#206092),(#206093,#206094),
(#206095,#206096),(#206097,#206098),(#206099,#206100),(#206101,#206102),
(#206103,#206104),(#206105,#206106),(#206107,#206108),(#206109,#206110),
(#206111,#206112),(#206113,#206114),(#206115,#206116),(#206117,#206118),
(#206119,#206120),(#206121,#206122),(#206123,#206124),(#206125,#206126),
(#206127,#206128),(#206129,#206130),(#206131,#206132),(#206133,#206134),
(#206135,#206136),(#206137,#206138),(#206139,#206140),(#206141,#206142),
(#206143,#206144),(#206145,#206146),(#206147,#206148),(#206149,#206150),
(#206151,#206152),(#206153,#206154),(#206155,#206156),(#206157,#206158),
(#206159,#206160),(#206161,#206162),(#206163,#206164),(#206165,#206166),
(#206167,#206168),(#206169,#206170),(#206171,#206172),(#206173,#206174),
(#206175,#206176),(#206177,#206178),(#206179,#206180),(#206181,#206182),
(#206183,#206184),(#206185,#206186),(#206187,#206188),(#206189,#206190),
(#206191,#206192),(#206193,#206194),(#206195,#206196),(#206197,#206198),
(#206199,#206200),(#206201,#206202),(#206203,#206204),(#206205,#206206),
(#206207,#206208),(#206209,#206210),(#206211,#206212),(#206213,#206214),
(#206215,#206216),(#206217,#206218),(#206219,#206220),(#206221,#206222),
(#206223,#206224),(#206225,#206226),(#206227,#206228),(#206229,#206230),
(#206231,#206232),(#206233,#206234),(#206235,#206236),(#206237,#206238),
(#206239,#206240),(#206241,#206242),(#206243,#206244),(#206245,#206246),
(#206247,#206248),(#206249,#206250),(#206251,#206252),(#206253,#206254),
(#206255,#206256),(#206257,#206258),(#206259,#206260),(#206261,#206262),
(#206263,#206264),(#206265,#206266),(#206267,#206268),(#206269,#206270),
(#206271,#206272),(#206273,#206274),(#206275,#206276),(#206277,#206278),
(#206279,#206280),(#206281,#206282),(#206283,#206284),(#206285,#206286),
(#206287,#206288),(#206289,#206290),(#206291,#206292),(#206293,#206294),
(#206295,#206296),(#206297,#206298),(#206299,#206300),(#206301,#206302),
(#206303,#206304),(#206305,#206306),(#206307,#206308),(#206309,#206310),
(#206311,#206312),(#206313,#206314),(#206315,#206316),(#206317,#206318),
(#206319,#206320),(#206321,#206322),(#206323,#206324),(#206325,#206326),
(#206327,#206328),(#206329,#206330),(#206331,#206332),(#206333,#206334),
(#206335,#206336),(#206337,#206338),(#206339,#206340),(#206341,#206342),
(#206343,#206344),(#206345,#206346),(#206347,#206348),(#206349,#206350),
(#206351,#206352),(#206353,#206354),(#206355,#206356),(#206357,#206358),
(#206359,#206360),(#206361,#206362),(#206363,#206364),(#206365,#206366),
(#206367,#206368),(#206369,#206370),(#206371,#206372),(#206373,#206374),
(#206375,#206376),(#206377,#206378),(#206379,#206380),(#206381,#206382),
(#206383,#206384),(#206385,#206386),(#206387,#206388),(#206389,#206390),
(#206391,#206392),(#206393,#206394),(#206395,#206396),(#206397,#206398),
(#206399,#206400),(#206401,#206402),(#206403,#206404),(#206405,#206406),
(#206407,#206408),(#206409,#206410),(#206411,#206412),(#206413,#206414),
(#206415,#206416),(#206417,#206418),(#206419,#206420),(#206421,#206422),
(#206423,#206424),(#206425,#206426),(#206427,#206428),(#206429,#206430),
(#206431,#206432),(#206433,#206434),(#206435,#206436),(#206437,#206438),
(#206439,#206440),(#206441,#206442),(#206443,#206444),(#206445,#206446),
(#206447,#206448),(#206449,#206450),(#206451,#206452),(#206453,#206454),
(#206455,#206456),(#206457,#206458),(#206459,#206460),(#206461,#206462),
(#206463,#206464),(#206465,#206466),(#206467,#206468),(#206469,#206470),
(#206471,#206472),(#206473,#206474),(#206475,#206476),(#206477,#206478),
(#206479,#206480),(#206481,#206482),(#206483,#206484),(#206485,#206486),
(#206487,#206488),(#206489,#206490),(#206491,#206492),(#206493,#206494),
(#206495,#206496),(#206497,#206498),(#206499,#206500),(#206501,#206502),
(#206503,#206504),(#206505,#206506),(#206507,#206508),(#206509,#206510),
(#206511,#206512),(#206513,#206514),(#206515,#206516),(#206517,#206518),
(#206519,#206520),(#206521,#206522),(#206523,#206524),(#206525,#206526),
(#206527,#206528),(#206529,#206530),(#206531,#206532),(#206533,#206534),
(#206535,#206536),(#206537,#206538),(#206539,#206540),(#206541,#206542),
(#206543,#206544),(#206545,#206546),(#206547,#206548),(#206549,#206550),
(#206551,#206552),(#206553,#206554),(#206555,#206556),(#206557,#206558),
(#206559,#206560),(#206561,#206562),(#206563,#206564),(#206565,#206566),
(#206567,#206568),(#206569,#206570),(#206571,#206572),(#206573,#206574),
(#206575,#206576),(#206577,#206578),(#206579,#206580),(#206581,#206582),
(#206583,#206584),(#206585,#206586),(#206587,#206588),(#206589,#206590),
(#206591,#206592),(#206593,#206594),(#206595,#206596),(#206597,#206598),
(#206599,#206600),(#206601,#206602),(#206603,#206604),(#206605,#206606),
(#206607,#206608),(#206609,#206610),(#206611,#206612),(#206613,#206614),
(#206615,#206616),(#206617,#206618),(#206619,#206620),(#206621,#206622),
(#206623,#206624),(#206625,#206626),(#206627,#206628),(#206629,#206630),
(#206631,#206632),(#206633,#206634),(#206635,#206636),(#206637,#206638),
(#206639,#206640),(#206641,#206642),(#206643,#206644),(#206645,#206646),
(#206647,#206648),(#206649,#206650),(#206651,#206652),(#206653,#206654),
(#206655,#206656),(#206657,#206658),(#206659,#206660),(#206661,#206662),
(#206663,#206664),(#206665,#206666),(#206667,#206668),(#206669,#206670),
(#206671,#206672),(#206673,#206674),(#206675,#206676),(#206677,#206678),
(#206679,#206680),(#206681,#206682),(#206683,#206684),(#206685,#206686),
(#206687,#206688),(#206689,#206690),(#206691,#206692),(#206693,#206694),
(#206695,#206696),(#206697,#206698),(#206699,#206700),(#206701,#206702),
(#206703,#206704),(#206705,#206706),(#206707,#206708),(#206709,#206710),
(#206711,#206712),(#206713,#206714),(#206715,#206716),(#206717,#206718),
(#206719,#206720),(#206721,#206722),(#206723,#206724),(#206725,#206726),
(#206727,#206728),(#206729,#206730),(#206731,#206732),(#206733,#206734),
(#206735,#206736),(#206737,#206738),(#206739,#206740),(#206741,#206742),
(#206743,#206744),(#206745,#206746),(#206747,#206748),(#206749,#206750),
(#206751,#206752),(#206753,#206754),(#206755,#206756),(#206757,#206758),
(#206759,#206760),(#206761,#206762),(#206763,#206764),(#206765,#206766),
(#206767,#206768),(#206769,#206770),(#206771,#206772),(#206773,#206774),
(#206775,#206776),(#206777,#206778),(#206779,#206780),(#206781,#206782),
(#206783,#206784),(#206785,#206786),(#206787,#206788),(#206789,#206790),
(#206791,#206792),(#206793,#206794),(#206795,#206796),(#206797,#206798),
(#206799,#206800),(#206801,#206802),(#206803,#206804),(#206805,#206806),
(#206807,#206808),(#206809,#206810)),.UNSPECIFIED.,.F.,.F.,.F.,(6,1,1,1,
1,1,1,1,1,1,1,1,1,1,1,1,1,1,1,1,1,1,1,1,1,1,1,1,1,1,1,1,1,1,1,1,1,1,1,1,
1,1,1,1,1,1,1,1,1,1,1,1,1,1,1,1,1,1,1,1,1,1,1,1,1,1,1,1,1,1,1,1,1,1,1,1,
1,1,1,1,1,1,1,1,1,1,1,1,1,1,1,1,1,1,1,1,1,1,1,1,1,1,1,1,1,1,1,1,1,1,1,1,
1,1,1,1,1,1,1,1,1,1,1,1,1,1,1,1,1,1,1,1,1,1,1,1,1,1,1,1,1,1,1,1,1,1,1,1,
1,1,1,1,1,1,1,1,1,1,1,1,1,1,1,1,1,1,1,1,1,1,1,1,1,1,1,1,1,1,1,1,1,1,1,1,
1,1,1,1,1,1,1,1,1,1,1,1,1,1,1,1,1,1,1,1,1,1,1,1,1,1,1,1,1,1,1,1,1,1,1,1,
1,1,1,1,1,1,1,1,1,1,1,1,1,1,1,1,1,1,1,1,1,1,1,1,1,1,1,1,1,1,1,1,1,1,1,1,
1,1,1,1,1,1,1,1,1,1,1,1,1,1,1,1,1,1,1,1,1,1,1,1,1,1,1,1,1,1,1,1,1,1,1,1,
1,1,1,1,1,1,1,1,1,1,1,1,1,1,1,1,1,1,1,1,1,1,1,1,1,1,1,1,1,1,1,1,1,1,1,1,
1,1,1,1,1,1,1,1,1,1,1,1,1,1,1,1,1,1,1,1,1,1,1,1,1,1,1,1,1,1,1,1,1,1,1,1,
1,1,1,1,1,1,1,1,1,1,1,1,1,1,1,1,1,1,1,1,1,1,1,1,1,1,1,1,1,1,1,1,1,1,1,1,
1,1,1,1,1,1,1,1,1,1,1,1,1,1,1,1,1,1,1,1,1,1,1,1,1,1,1,1,1,1,1,1,1,1,1,1,
1,1,1,1,1,1,1,1,1,1,1,1,1,1,1,1,1,1,1,1,1,1,1,1,1,1,1,1,1,1,1,6),(2,2),
(0.143172103,0.144954128,0.146788991,0.148623853,0.150458716,0.152293578,
0.15412844,0.155963303,0.157798165,0.159633028,0.16146789,0.163302752,0.165137615,
0.166972477,0.168807339,0.170642202,0.172477064,0.174311927,0.176146789,
0.177981651,0.179816514,0.181651376,0.183486239,0.185321101,0.187155963,
0.188990826,0.190825688,0.19266055,0.194495413,0.196330275,0.198165138,
0.2,0.201834862,0.203669725,0.205504587,0.20733945,0.209174312,0.211009174,
0.212844037,0.214678899,0.216513761,0.218348624,0.220183486,0.222018349,
0.223853211,0.225688073,0.227522936,0.229357798,0.231192661,0.233027523,
0.234862385,0.236697248,0.23853211,0.240366972,0.242201835,0.244036697,
0.24587156,0.247706422,0.249541284,0.251376147,0.253211009,0.255045872,
0.256880734,0.258715596,0.260550459,0.262385321,0.264220183,0.266055046,
0.267889908,0.269724771,0.271559633,0.273394495,0.275229358,0.27706422,
0.278899083,0.280733945,0.282568807,0.28440367,0.286238532,0.288073394,
0.289908257,0.291743119,0.293577982,0.295412844,0.297247706,0.299082569,
0.300917431,0.302752294,0.304587156,0.306422018,0.308256881,0.310091743,
0.311926606,0.313761468,0.31559633,0.317431193,0.319266055,0.321100917,
0.32293578,0.324770642,0.326605505,0.328440367,0.330275229,0.332110092,
0.333944954,0.335779817,0.337614679,0.339449541,0.341284404,0.343119266,
0.344954128,0.346788991,0.348623853,0.350458716,0.352293578,0.35412844,
0.355963303,0.357798165,0.359633028,0.36146789,0.363302752,0.365137615,
0.366972477,0.368807339,0.370642202,0.372477064,0.374311927,0.376146789,
0.377981651,0.379816514,0.381651376,0.383486239,0.385321101,0.387155963,
0.388990826,0.390825688,0.39266055,0.394495413,0.396330275,0.398165138,
0.4,0.401834862,0.403669725,0.405504587,0.40733945,0.409174312,0.411009174,
0.412844037,0.414678899,0.416513761,0.418348624,0.420183486,0.422018349,
0.423853211,0.425688073,0.427522936,0.429357798,0.431192661,0.433027523,
0.434862385,0.436697248,0.43853211,0.440366972,0.442201835,0.444036697,
0.44587156,0.447706422,0.449541284,0.451376147,0.453211009,0.455045872,
0.456880734,0.458715596,0.460550459,0.462385321,0.464220183,0.466055046,
0.467889908,0.469724771,0.471559633,0.473394495,0.475229358,0.47706422,
0.478899083,0.480733945,0.482568807,0.48440367,0.486238532,0.488073394,
0.489908257,0.491743119,0.493577982,0.495412844,0.497247706,0.499082569,
0.500917431,0.502752294,0.504587156,0.506422018,0.508256881,0.510091743,
0.511926606,0.513761468,0.51559633,0.517431193,0.519266055,0.521100917,
0.52293578,0.524770642,0.526605505,0.528440367,0.530275229,0.532110092,
0.533944954,0.535779817,0.537614679,0.539449541,0.541284404,0.543119266,
0.544954128,0.546788991,0.548623853,0.550458716,0.552293578,0.55412844,
0.555963303,0.557798165,0.559633028,0.56146789,0.563302752,0.565137615,
0.566972477,0.568807339,0.570642202,0.572477064,0.574311927,0.576146789,
0.577981651,0.579816514,0.581651376,0.583486239,0.585321101,0.587155963,
0.588990826,0.590825688,0.59266055,0.594495413,0.596330275,0.598165138,
0.6,0.601834862,0.603669725,0.605504587,0.60733945,0.609174312,0.611009174,
0.612844037,0.614678899,0.616513761,0.618348624,0.620183486,0.622018349,
0.623853211,0.625688073,0.627522936,0.629357798,0.631192661,0.633027523,
0.634862385,0.636697248,0.63853211,0.640366972,0.642201835,0.644036697,
0.64587156,0.647706422,0.649541284,0.651376147,0.653211009,0.655045872,
0.656880734,0.658715596,0.660550459,0.662385321,0.664220183,0.666055046,
0.667889908,0.669724771,0.671559633,0.673394495,0.675229358,0.67706422,
0.678899083,0.680733945,0.682568807,0.68440367,0.686238532,0.688073394,
0.689908257,0.691743119,0.693577982,0.695412844,0.697247706,0.699082569,
0.700917431,0.702752294,0.704587156,0.706422018,0.708256881,0.710091743,
0.711926606,0.713761468,0.71559633,0.717431193,0.719266055,0.721100917,
0.72293578,0.724770642,0.726605505,0.728440367,0.730275229,0.732110092,
0.733944954,0.735779817,0.737614679,0.739449541,0.741284404,0.743119266,
0.744954128,0.746788991,0.748623853,0.750458716,0.752293578,0.75412844,
0.755963303,0.757798165,0.759633028,0.76146789,0.763302752,0.765137615,
0.766972477,0.768807339,0.770642202,0.772477064,0.774311927,0.776146789,
0.777981651,0.779816514,0.781651376,0.783486239,0.785321101,0.787155963,
0.788990826,0.790825688,0.79266055,0.794495413,0.796330275,0.798165138,
0.8,0.801834862,0.803669725,0.805504587,0.80733945,0.809174312,0.811009174,
0.812844037,0.814678899,0.816513761,0.818348624,0.820183486,0.822018349,
0.823853211,0.825688073,0.827522936,0.829357798,0.831192661,0.833027523,
0.834862385,0.836697248,0.83853211,0.840366972,0.842201835,0.844036697,
0.84587156,0.847706422,0.849541284,0.851376147,0.853211009,0.855045872,
0.856880734,0.858715596,0.860550459,0.862385321,0.864220183,0.866055046,
0.867889908,0.869724771,0.871559633,0.873394495,0.875229358,0.87706422,
0.878899083,0.880733945,0.882568807,0.88440367,0.886238532,0.888073394,
0.889908257,0.891743119,0.893577982,0.895412844,0.897247706,0.899082569,
0.900917431,0.902752294,0.904587156,0.906422018,0.908256881,0.910091743,
0.911926606,0.913761468,0.91559633,0.917431193,0.919266055,0.921100917,
0.92293578,0.924770642,0.926605505,0.928440367,0.930275229,0.932110092,
0.933944954,0.935779817,0.937614679,0.939449541,0.941284404,0.943119266,
0.944954128,0.946788991,0.948623853,0.950458716,0.952293578,0.95412844,
0.955963303,0.957798165,0.959633028,0.96146789,0.963302752,0.965137615,
0.966972477,0.968807339,0.970642202,0.972477064,0.974311927,0.976146789,
0.977981651,0.979816514,0.981651376,0.983486239,0.985321101,0.987155963,
0.988990826,0.990825688,0.99266055,0.994495413,0.996330275,0.998165138,
1.),(0.,0.36),.UNSPECIFIED.);
#6247=B_SPLINE_SURFACE_WITH_KNOTS('',5,1,((#207446,#207447),(#207448,#207449),
(#207450,#207451),(#207452,#207453),(#207454,#207455),(#207456,#207457),
(#207458,#207459),(#207460,#207461),(#207462,#207463),(#207464,#207465),
(#207466,#207467),(#207468,#207469),(#207470,#207471),(#207472,#207473),
(#207474,#207475),(#207476,#207477),(#207478,#207479),(#207480,#207481),
(#207482,#207483),(#207484,#207485),(#207486,#207487),(#207488,#207489),
(#207490,#207491),(#207492,#207493),(#207494,#207495),(#207496,#207497),
(#207498,#207499),(#207500,#207501),(#207502,#207503),(#207504,#207505),
(#207506,#207507),(#207508,#207509),(#207510,#207511),(#207512,#207513),
(#207514,#207515),(#207516,#207517),(#207518,#207519),(#207520,#207521),
(#207522,#207523),(#207524,#207525),(#207526,#207527),(#207528,#207529),
(#207530,#207531),(#207532,#207533),(#207534,#207535),(#207536,#207537),
(#207538,#207539),(#207540,#207541),(#207542,#207543),(#207544,#207545),
(#207546,#207547),(#207548,#207549),(#207550,#207551),(#207552,#207553),
(#207554,#207555),(#207556,#207557),(#207558,#207559),(#207560,#207561),
(#207562,#207563),(#207564,#207565),(#207566,#207567),(#207568,#207569),
(#207570,#207571),(#207572,#207573),(#207574,#207575),(#207576,#207577),
(#207578,#207579),(#207580,#207581),(#207582,#207583),(#207584,#207585),
(#207586,#207587),(#207588,#207589),(#207590,#207591),(#207592,#207593),
(#207594,#207595),(#207596,#207597),(#207598,#207599),(#207600,#207601),
(#207602,#207603),(#207604,#207605),(#207606,#207607),(#207608,#207609),
(#207610,#207611),(#207612,#207613),(#207614,#207615),(#207616,#207617),
(#207618,#207619),(#207620,#207621),(#207622,#207623),(#207624,#207625),
(#207626,#207627),(#207628,#207629),(#207630,#207631),(#207632,#207633),
(#207634,#207635),(#207636,#207637),(#207638,#207639),(#207640,#207641),
(#207642,#207643),(#207644,#207645),(#207646,#207647),(#207648,#207649),
(#207650,#207651),(#207652,#207653),(#207654,#207655),(#207656,#207657),
(#207658,#207659),(#207660,#207661),(#207662,#207663),(#207664,#207665),
(#207666,#207667),(#207668,#207669),(#207670,#207671),(#207672,#207673),
(#207674,#207675),(#207676,#207677),(#207678,#207679),(#207680,#207681),
(#207682,#207683),(#207684,#207685),(#207686,#207687),(#207688,#207689),
(#207690,#207691),(#207692,#207693),(#207694,#207695),(#207696,#207697),
(#207698,#207699),(#207700,#207701),(#207702,#207703),(#207704,#207705),
(#207706,#207707),(#207708,#207709),(#207710,#207711),(#207712,#207713),
(#207714,#207715),(#207716,#207717),(#207718,#207719),(#207720,#207721),
(#207722,#207723),(#207724,#207725),(#207726,#207727),(#207728,#207729),
(#207730,#207731),(#207732,#207733),(#207734,#207735),(#207736,#207737),
(#207738,#207739),(#207740,#207741),(#207742,#207743),(#207744,#207745),
(#207746,#207747),(#207748,#207749),(#207750,#207751),(#207752,#207753),
(#207754,#207755),(#207756,#207757),(#207758,#207759),(#207760,#207761),
(#207762,#207763),(#207764,#207765),(#207766,#207767),(#207768,#207769),
(#207770,#207771),(#207772,#207773),(#207774,#207775),(#207776,#207777),
(#207778,#207779),(#207780,#207781),(#207782,#207783),(#207784,#207785),
(#207786,#207787),(#207788,#207789),(#207790,#207791),(#207792,#207793),
(#207794,#207795),(#207796,#207797),(#207798,#207799),(#207800,#207801),
(#207802,#207803),(#207804,#207805),(#207806,#207807),(#207808,#207809),
(#207810,#207811),(#207812,#207813),(#207814,#207815),(#207816,#207817),
(#207818,#207819),(#207820,#207821),(#207822,#207823),(#207824,#207825),
(#207826,#207827),(#207828,#207829),(#207830,#207831),(#207832,#207833),
(#207834,#207835),(#207836,#207837),(#207838,#207839),(#207840,#207841),
(#207842,#207843),(#207844,#207845),(#207846,#207847),(#207848,#207849),
(#207850,#207851),(#207852,#207853),(#207854,#207855),(#207856,#207857),
(#207858,#207859),(#207860,#207861),(#207862,#207863),(#207864,#207865),
(#207866,#207867),(#207868,#207869),(#207870,#207871),(#207872,#207873),
(#207874,#207875),(#207876,#207877),(#207878,#207879),(#207880,#207881),
(#207882,#207883),(#207884,#207885),(#207886,#207887),(#207888,#207889),
(#207890,#207891),(#207892,#207893),(#207894,#207895),(#207896,#207897),
(#207898,#207899),(#207900,#207901),(#207902,#207903),(#207904,#207905),
(#207906,#207907),(#207908,#207909),(#207910,#207911),(#207912,#207913),
(#207914,#207915),(#207916,#207917),(#207918,#207919),(#207920,#207921),
(#207922,#207923),(#207924,#207925),(#207926,#207927),(#207928,#207929),
(#207930,#207931),(#207932,#207933),(#207934,#207935),(#207936,#207937),
(#207938,#207939),(#207940,#207941),(#207942,#207943),(#207944,#207945),
(#207946,#207947),(#207948,#207949),(#207950,#207951),(#207952,#207953),
(#207954,#207955),(#207956,#207957),(#207958,#207959),(#207960,#207961),
(#207962,#207963),(#207964,#207965),(#207966,#207967),(#207968,#207969),
(#207970,#207971),(#207972,#207973),(#207974,#207975),(#207976,#207977),
(#207978,#207979),(#207980,#207981),(#207982,#207983),(#207984,#207985),
(#207986,#207987),(#207988,#207989),(#207990,#207991),(#207992,#207993),
(#207994,#207995),(#207996,#207997),(#207998,#207999),(#208000,#208001),
(#208002,#208003),(#208004,#208005),(#208006,#208007),(#208008,#208009),
(#208010,#208011),(#208012,#208013),(#208014,#208015),(#208016,#208017),
(#208018,#208019),(#208020,#208021),(#208022,#208023),(#208024,#208025),
(#208026,#208027),(#208028,#208029),(#208030,#208031),(#208032,#208033),
(#208034,#208035),(#208036,#208037),(#208038,#208039),(#208040,#208041),
(#208042,#208043),(#208044,#208045),(#208046,#208047),(#208048,#208049),
(#208050,#208051),(#208052,#208053),(#208054,#208055),(#208056,#208057),
(#208058,#208059),(#208060,#208061),(#208062,#208063),(#208064,#208065),
(#208066,#208067),(#208068,#208069),(#208070,#208071),(#208072,#208073),
(#208074,#208075),(#208076,#208077),(#208078,#208079),(#208080,#208081),
(#208082,#208083),(#208084,#208085),(#208086,#208087),(#208088,#208089),
(#208090,#208091),(#208092,#208093),(#208094,#208095),(#208096,#208097),
(#208098,#208099),(#208100,#208101),(#208102,#208103),(#208104,#208105),
(#208106,#208107),(#208108,#208109),(#208110,#208111),(#208112,#208113),
(#208114,#208115),(#208116,#208117),(#208118,#208119),(#208120,#208121),
(#208122,#208123),(#208124,#208125),(#208126,#208127),(#208128,#208129),
(#208130,#208131),(#208132,#208133),(#208134,#208135),(#208136,#208137),
(#208138,#208139),(#208140,#208141),(#208142,#208143),(#208144,#208145),
(#208146,#208147),(#208148,#208149),(#208150,#208151),(#208152,#208153),
(#208154,#208155),(#208156,#208157),(#208158,#208159),(#208160,#208161),
(#208162,#208163),(#208164,#208165),(#208166,#208167),(#208168,#208169),
(#208170,#208171),(#208172,#208173),(#208174,#208175),(#208176,#208177),
(#208178,#208179),(#208180,#208181),(#208182,#208183),(#208184,#208185),
(#208186,#208187),(#208188,#208189),(#208190,#208191),(#208192,#208193),
(#208194,#208195),(#208196,#208197),(#208198,#208199),(#208200,#208201),
(#208202,#208203),(#208204,#208205),(#208206,#208207),(#208208,#208209),
(#208210,#208211),(#208212,#208213),(#208214,#208215),(#208216,#208217),
(#208218,#208219),(#208220,#208221),(#208222,#208223),(#208224,#208225),
(#208226,#208227),(#208228,#208229),(#208230,#208231),(#208232,#208233),
(#208234,#208235),(#208236,#208237),(#208238,#208239),(#208240,#208241),
(#208242,#208243),(#208244,#208245),(#208246,#208247),(#208248,#208249),
(#208250,#208251),(#208252,#208253),(#208254,#208255),(#208256,#208257),
(#208258,#208259),(#208260,#208261),(#208262,#208263),(#208264,#208265),
(#208266,#208267),(#208268,#208269),(#208270,#208271),(#208272,#208273),
(#208274,#208275),(#208276,#208277),(#208278,#208279),(#208280,#208281),
(#208282,#208283),(#208284,#208285),(#208286,#208287),(#208288,#208289),
(#208290,#208291),(#208292,#208293),(#208294,#208295),(#208296,#208297),
(#208298,#208299),(#208300,#208301),(#208302,#208303),(#208304,#208305),
(#208306,#208307),(#208308,#208309),(#208310,#208311),(#208312,#208313),
(#208314,#208315),(#208316,#208317),(#208318,#208319),(#208320,#208321),
(#208322,#208323),(#208324,#208325),(#208326,#208327),(#208328,#208329),
(#208330,#208331),(#208332,#208333),(#208334,#208335),(#208336,#208337),
(#208338,#208339),(#208340,#208341),(#208342,#208343),(#208344,#208345),
(#208346,#208347),(#208348,#208349),(#208350,#208351),(#208352,#208353),
(#208354,#208355),(#208356,#208357),(#208358,#208359),(#208360,#208361),
(#208362,#208363),(#208364,#208365),(#208366,#208367),(#208368,#208369),
(#208370,#208371),(#208372,#208373),(#208374,#208375),(#208376,#208377),
(#208378,#208379),(#208380,#208381),(#208382,#208383),(#208384,#208385),
(#208386,#208387),(#208388,#208389)),.UNSPECIFIED.,.F.,.F.,.F.,(6,1,1,1,
1,1,1,1,1,1,1,1,1,1,1,1,1,1,1,1,1,1,1,1,1,1,1,1,1,1,1,1,1,1,1,1,1,1,1,1,
1,1,1,1,1,1,1,1,1,1,1,1,1,1,1,1,1,1,1,1,1,1,1,1,1,1,1,1,1,1,1,1,1,1,1,1,
1,1,1,1,1,1,1,1,1,1,1,1,1,1,1,1,1,1,1,1,1,1,1,1,1,1,1,1,1,1,1,1,1,1,1,1,
1,1,1,1,1,1,1,1,1,1,1,1,1,1,1,1,1,1,1,1,1,1,1,1,1,1,1,1,1,1,1,1,1,1,1,1,
1,1,1,1,1,1,1,1,1,1,1,1,1,1,1,1,1,1,1,1,1,1,1,1,1,1,1,1,1,1,1,1,1,1,1,1,
1,1,1,1,1,1,1,1,1,1,1,1,1,1,1,1,1,1,1,1,1,1,1,1,1,1,1,1,1,1,1,1,1,1,1,1,
1,1,1,1,1,1,1,1,1,1,1,1,1,1,1,1,1,1,1,1,1,1,1,1,1,1,1,1,1,1,1,1,1,1,1,1,
1,1,1,1,1,1,1,1,1,1,1,1,1,1,1,1,1,1,1,1,1,1,1,1,1,1,1,1,1,1,1,1,1,1,1,1,
1,1,1,1,1,1,1,1,1,1,1,1,1,1,1,1,1,1,1,1,1,1,1,1,1,1,1,1,1,1,1,1,1,1,1,1,
1,1,1,1,1,1,1,1,1,1,1,1,1,1,1,1,1,1,1,1,1,1,1,1,1,1,1,1,1,1,1,1,1,1,1,1,
1,1,1,1,1,1,1,1,1,1,1,1,1,1,1,1,1,1,1,1,1,1,1,1,1,1,1,1,1,1,1,1,1,1,1,1,
1,1,1,1,1,1,1,1,1,1,1,1,1,1,1,1,1,1,1,1,1,1,1,1,1,1,1,1,1,1,1,1,1,1,1,1,
1,1,1,1,1,1,1,1,1,1,1,1,1,1,1,1,1,1,1,1,1,1,1,1,1,1,1,1,1,1,1,6),(2,2),
(0.143172104,0.144954128,0.146788991,0.148623853,0.150458716,0.152293578,
0.15412844,0.155963303,0.157798165,0.159633028,0.16146789,0.163302752,0.165137615,
0.166972477,0.168807339,0.170642202,0.172477064,0.174311927,0.176146789,
0.177981651,0.179816514,0.181651376,0.183486239,0.185321101,0.187155963,
0.188990826,0.190825688,0.19266055,0.194495413,0.196330275,0.198165138,
0.2,0.201834862,0.203669725,0.205504587,0.20733945,0.209174312,0.211009174,
0.212844037,0.214678899,0.216513761,0.218348624,0.220183486,0.222018349,
0.223853211,0.225688073,0.227522936,0.229357798,0.231192661,0.233027523,
0.234862385,0.236697248,0.23853211,0.240366972,0.242201835,0.244036697,
0.24587156,0.247706422,0.249541284,0.251376147,0.253211009,0.255045872,
0.256880734,0.258715596,0.260550459,0.262385321,0.264220183,0.266055046,
0.267889908,0.269724771,0.271559633,0.273394495,0.275229358,0.27706422,
0.278899083,0.280733945,0.282568807,0.28440367,0.286238532,0.288073394,
0.289908257,0.291743119,0.293577982,0.295412844,0.297247706,0.299082569,
0.300917431,0.302752294,0.304587156,0.306422018,0.308256881,0.310091743,
0.311926606,0.313761468,0.31559633,0.317431193,0.319266055,0.321100917,
0.32293578,0.324770642,0.326605505,0.328440367,0.330275229,0.332110092,
0.333944954,0.335779817,0.337614679,0.339449541,0.341284404,0.343119266,
0.344954128,0.346788991,0.348623853,0.350458716,0.352293578,0.35412844,
0.355963303,0.357798165,0.359633028,0.36146789,0.363302752,0.365137615,
0.366972477,0.368807339,0.370642202,0.372477064,0.374311927,0.376146789,
0.377981651,0.379816514,0.381651376,0.383486239,0.385321101,0.387155963,
0.388990826,0.390825688,0.39266055,0.394495413,0.396330275,0.398165138,
0.4,0.401834862,0.403669725,0.405504587,0.40733945,0.409174312,0.411009174,
0.412844037,0.414678899,0.416513761,0.418348624,0.420183486,0.422018349,
0.423853211,0.425688073,0.427522936,0.429357798,0.431192661,0.433027523,
0.434862385,0.436697248,0.43853211,0.440366972,0.442201835,0.444036697,
0.44587156,0.447706422,0.449541284,0.451376147,0.453211009,0.455045872,
0.456880734,0.458715596,0.460550459,0.462385321,0.464220183,0.466055046,
0.467889908,0.469724771,0.471559633,0.473394495,0.475229358,0.47706422,
0.478899083,0.480733945,0.482568807,0.48440367,0.486238532,0.488073394,
0.489908257,0.491743119,0.493577982,0.495412844,0.497247706,0.499082569,
0.500917431,0.502752294,0.504587156,0.506422018,0.508256881,0.510091743,
0.511926606,0.513761468,0.51559633,0.517431193,0.519266055,0.521100917,
0.52293578,0.524770642,0.526605505,0.528440367,0.530275229,0.532110092,
0.533944954,0.535779817,0.537614679,0.539449541,0.541284404,0.543119266,
0.544954128,0.546788991,0.548623853,0.550458716,0.552293578,0.55412844,
0.555963303,0.557798165,0.559633028,0.56146789,0.563302752,0.565137615,
0.566972477,0.568807339,0.570642202,0.572477064,0.574311927,0.576146789,
0.577981651,0.579816514,0.581651376,0.583486239,0.585321101,0.587155963,
0.588990826,0.590825688,0.59266055,0.594495413,0.596330275,0.598165138,
0.6,0.601834862,0.603669725,0.605504587,0.60733945,0.609174312,0.611009174,
0.612844037,0.614678899,0.616513761,0.618348624,0.620183486,0.622018349,
0.623853211,0.625688073,0.627522936,0.629357798,0.631192661,0.633027523,
0.634862385,0.636697248,0.63853211,0.640366972,0.642201835,0.644036697,
0.64587156,0.647706422,0.649541284,0.651376147,0.653211009,0.655045872,
0.656880734,0.658715596,0.660550459,0.662385321,0.664220183,0.666055046,
0.667889908,0.669724771,0.671559633,0.673394495,0.675229358,0.67706422,
0.678899083,0.680733945,0.682568807,0.68440367,0.686238532,0.688073394,
0.689908257,0.691743119,0.693577982,0.695412844,0.697247706,0.699082569,
0.700917431,0.702752294,0.704587156,0.706422018,0.708256881,0.710091743,
0.711926606,0.713761468,0.71559633,0.717431193,0.719266055,0.721100917,
0.72293578,0.724770642,0.726605505,0.728440367,0.730275229,0.732110092,
0.733944954,0.735779817,0.737614679,0.739449541,0.741284404,0.743119266,
0.744954128,0.746788991,0.748623853,0.750458716,0.752293578,0.75412844,
0.755963303,0.757798165,0.759633028,0.76146789,0.763302752,0.765137615,
0.766972477,0.768807339,0.770642202,0.772477064,0.774311927,0.776146789,
0.777981651,0.779816514,0.781651376,0.783486239,0.785321101,0.787155963,
0.788990826,0.790825688,0.79266055,0.794495413,0.796330275,0.798165138,
0.8,0.801834862,0.803669725,0.805504587,0.80733945,0.809174312,0.811009174,
0.812844037,0.814678899,0.816513761,0.818348624,0.820183486,0.822018349,
0.823853211,0.825688073,0.827522936,0.829357798,0.831192661,0.833027523,
0.834862385,0.836697248,0.83853211,0.840366972,0.842201835,0.844036697,
0.84587156,0.847706422,0.849541284,0.851376147,0.853211009,0.855045872,
0.856880734,0.858715596,0.860550459,0.862385321,0.864220183,0.866055046,
0.867889908,0.869724771,0.871559633,0.873394495,0.875229358,0.87706422,
0.878899083,0.880733945,0.882568807,0.88440367,0.886238532,0.888073394,
0.889908257,0.891743119,0.893577982,0.895412844,0.897247706,0.899082569,
0.900917431,0.902752294,0.904587156,0.906422018,0.908256881,0.910091743,
0.911926606,0.913761468,0.91559633,0.917431193,0.919266055,0.921100917,
0.92293578,0.924770642,0.926605505,0.928440367,0.930275229,0.932110092,
0.933944954,0.935779817,0.937614679,0.939449541,0.941284404,0.943119266,
0.944954128,0.946788991,0.948623853,0.950458716,0.952293578,0.95412844,
0.955963303,0.957798165,0.959633028,0.96146789,0.963302752,0.965137615,
0.966972477,0.968807339,0.970642202,0.972477064,0.974311927,0.976146789,
0.977981651,0.979816514,0.981651376,0.983486239,0.985321101,0.987155963,
0.988990826,0.990825688,0.99266055,0.994495413,0.996330275,0.998165138,
1.),(0.,0.36),.UNSPECIFIED.);
#6248=B_SPLINE_SURFACE_WITH_KNOTS('',5,1,((#209028,#209029),(#209030,#209031),
(#209032,#209033),(#209034,#209035),(#209036,#209037),(#209038,#209039),
(#209040,#209041),(#209042,#209043),(#209044,#209045),(#209046,#209047),
(#209048,#209049),(#209050,#209051),(#209052,#209053),(#209054,#209055),
(#209056,#209057),(#209058,#209059),(#209060,#209061),(#209062,#209063),
(#209064,#209065),(#209066,#209067),(#209068,#209069),(#209070,#209071),
(#209072,#209073),(#209074,#209075),(#209076,#209077),(#209078,#209079),
(#209080,#209081),(#209082,#209083),(#209084,#209085),(#209086,#209087),
(#209088,#209089),(#209090,#209091),(#209092,#209093),(#209094,#209095),
(#209096,#209097),(#209098,#209099),(#209100,#209101),(#209102,#209103),
(#209104,#209105),(#209106,#209107),(#209108,#209109),(#209110,#209111),
(#209112,#209113),(#209114,#209115),(#209116,#209117),(#209118,#209119),
(#209120,#209121),(#209122,#209123),(#209124,#209125),(#209126,#209127),
(#209128,#209129),(#209130,#209131),(#209132,#209133),(#209134,#209135),
(#209136,#209137),(#209138,#209139),(#209140,#209141),(#209142,#209143),
(#209144,#209145),(#209146,#209147),(#209148,#209149),(#209150,#209151),
(#209152,#209153),(#209154,#209155),(#209156,#209157),(#209158,#209159),
(#209160,#209161),(#209162,#209163),(#209164,#209165),(#209166,#209167),
(#209168,#209169),(#209170,#209171),(#209172,#209173),(#209174,#209175),
(#209176,#209177),(#209178,#209179),(#209180,#209181),(#209182,#209183),
(#209184,#209185),(#209186,#209187),(#209188,#209189),(#209190,#209191),
(#209192,#209193),(#209194,#209195),(#209196,#209197),(#209198,#209199),
(#209200,#209201),(#209202,#209203),(#209204,#209205),(#209206,#209207),
(#209208,#209209),(#209210,#209211),(#209212,#209213),(#209214,#209215),
(#209216,#209217),(#209218,#209219),(#209220,#209221),(#209222,#209223),
(#209224,#209225),(#209226,#209227),(#209228,#209229),(#209230,#209231),
(#209232,#209233),(#209234,#209235),(#209236,#209237),(#209238,#209239),
(#209240,#209241),(#209242,#209243),(#209244,#209245),(#209246,#209247),
(#209248,#209249),(#209250,#209251),(#209252,#209253),(#209254,#209255),
(#209256,#209257),(#209258,#209259),(#209260,#209261),(#209262,#209263),
(#209264,#209265),(#209266,#209267),(#209268,#209269),(#209270,#209271),
(#209272,#209273),(#209274,#209275),(#209276,#209277),(#209278,#209279),
(#209280,#209281),(#209282,#209283),(#209284,#209285),(#209286,#209287),
(#209288,#209289),(#209290,#209291),(#209292,#209293),(#209294,#209295),
(#209296,#209297),(#209298,#209299),(#209300,#209301),(#209302,#209303),
(#209304,#209305),(#209306,#209307),(#209308,#209309),(#209310,#209311),
(#209312,#209313),(#209314,#209315),(#209316,#209317),(#209318,#209319),
(#209320,#209321),(#209322,#209323),(#209324,#209325),(#209326,#209327),
(#209328,#209329),(#209330,#209331),(#209332,#209333),(#209334,#209335),
(#209336,#209337),(#209338,#209339),(#209340,#209341),(#209342,#209343),
(#209344,#209345),(#209346,#209347),(#209348,#209349),(#209350,#209351),
(#209352,#209353),(#209354,#209355),(#209356,#209357),(#209358,#209359),
(#209360,#209361),(#209362,#209363),(#209364,#209365),(#209366,#209367),
(#209368,#209369),(#209370,#209371),(#209372,#209373),(#209374,#209375),
(#209376,#209377),(#209378,#209379),(#209380,#209381),(#209382,#209383),
(#209384,#209385),(#209386,#209387),(#209388,#209389),(#209390,#209391),
(#209392,#209393),(#209394,#209395),(#209396,#209397),(#209398,#209399),
(#209400,#209401),(#209402,#209403),(#209404,#209405),(#209406,#209407),
(#209408,#209409),(#209410,#209411),(#209412,#209413),(#209414,#209415),
(#209416,#209417),(#209418,#209419),(#209420,#209421),(#209422,#209423),
(#209424,#209425),(#209426,#209427),(#209428,#209429),(#209430,#209431),
(#209432,#209433),(#209434,#209435),(#209436,#209437),(#209438,#209439),
(#209440,#209441),(#209442,#209443),(#209444,#209445),(#209446,#209447),
(#209448,#209449),(#209450,#209451),(#209452,#209453),(#209454,#209455),
(#209456,#209457),(#209458,#209459),(#209460,#209461),(#209462,#209463),
(#209464,#209465),(#209466,#209467),(#209468,#209469),(#209470,#209471),
(#209472,#209473),(#209474,#209475),(#209476,#209477),(#209478,#209479),
(#209480,#209481),(#209482,#209483),(#209484,#209485),(#209486,#209487),
(#209488,#209489),(#209490,#209491),(#209492,#209493),(#209494,#209495),
(#209496,#209497),(#209498,#209499),(#209500,#209501),(#209502,#209503),
(#209504,#209505),(#209506,#209507),(#209508,#209509),(#209510,#209511),
(#209512,#209513),(#209514,#209515),(#209516,#209517),(#209518,#209519),
(#209520,#209521),(#209522,#209523),(#209524,#209525),(#209526,#209527),
(#209528,#209529),(#209530,#209531),(#209532,#209533),(#209534,#209535),
(#209536,#209537),(#209538,#209539),(#209540,#209541),(#209542,#209543),
(#209544,#209545),(#209546,#209547),(#209548,#209549),(#209550,#209551),
(#209552,#209553),(#209554,#209555),(#209556,#209557),(#209558,#209559),
(#209560,#209561),(#209562,#209563),(#209564,#209565),(#209566,#209567),
(#209568,#209569),(#209570,#209571),(#209572,#209573),(#209574,#209575),
(#209576,#209577),(#209578,#209579),(#209580,#209581),(#209582,#209583),
(#209584,#209585),(#209586,#209587),(#209588,#209589),(#209590,#209591),
(#209592,#209593),(#209594,#209595),(#209596,#209597),(#209598,#209599),
(#209600,#209601),(#209602,#209603),(#209604,#209605),(#209606,#209607),
(#209608,#209609),(#209610,#209611),(#209612,#209613),(#209614,#209615),
(#209616,#209617),(#209618,#209619),(#209620,#209621),(#209622,#209623),
(#209624,#209625),(#209626,#209627),(#209628,#209629),(#209630,#209631),
(#209632,#209633),(#209634,#209635),(#209636,#209637),(#209638,#209639),
(#209640,#209641),(#209642,#209643),(#209644,#209645),(#209646,#209647),
(#209648,#209649),(#209650,#209651),(#209652,#209653),(#209654,#209655),
(#209656,#209657),(#209658,#209659),(#209660,#209661),(#209662,#209663),
(#209664,#209665),(#209666,#209667),(#209668,#209669),(#209670,#209671),
(#209672,#209673),(#209674,#209675),(#209676,#209677),(#209678,#209679),
(#209680,#209681),(#209682,#209683),(#209684,#209685),(#209686,#209687),
(#209688,#209689),(#209690,#209691),(#209692,#209693),(#209694,#209695),
(#209696,#209697),(#209698,#209699),(#209700,#209701),(#209702,#209703),
(#209704,#209705),(#209706,#209707),(#209708,#209709),(#209710,#209711),
(#209712,#209713),(#209714,#209715),(#209716,#209717),(#209718,#209719),
(#209720,#209721),(#209722,#209723),(#209724,#209725),(#209726,#209727),
(#209728,#209729),(#209730,#209731),(#209732,#209733),(#209734,#209735),
(#209736,#209737),(#209738,#209739),(#209740,#209741),(#209742,#209743),
(#209744,#209745),(#209746,#209747),(#209748,#209749),(#209750,#209751),
(#209752,#209753),(#209754,#209755),(#209756,#209757),(#209758,#209759),
(#209760,#209761),(#209762,#209763),(#209764,#209765),(#209766,#209767),
(#209768,#209769),(#209770,#209771),(#209772,#209773),(#209774,#209775),
(#209776,#209777),(#209778,#209779),(#209780,#209781),(#209782,#209783),
(#209784,#209785),(#209786,#209787),(#209788,#209789),(#209790,#209791),
(#209792,#209793),(#209794,#209795),(#209796,#209797),(#209798,#209799),
(#209800,#209801),(#209802,#209803),(#209804,#209805),(#209806,#209807),
(#209808,#209809),(#209810,#209811),(#209812,#209813),(#209814,#209815),
(#209816,#209817),(#209818,#209819),(#209820,#209821),(#209822,#209823),
(#209824,#209825),(#209826,#209827),(#209828,#209829),(#209830,#209831),
(#209832,#209833),(#209834,#209835),(#209836,#209837),(#209838,#209839),
(#209840,#209841),(#209842,#209843),(#209844,#209845),(#209846,#209847),
(#209848,#209849),(#209850,#209851),(#209852,#209853),(#209854,#209855),
(#209856,#209857),(#209858,#209859),(#209860,#209861),(#209862,#209863),
(#209864,#209865),(#209866,#209867),(#209868,#209869),(#209870,#209871),
(#209872,#209873),(#209874,#209875),(#209876,#209877),(#209878,#209879),
(#209880,#209881),(#209882,#209883),(#209884,#209885),(#209886,#209887),
(#209888,#209889),(#209890,#209891),(#209892,#209893),(#209894,#209895),
(#209896,#209897),(#209898,#209899),(#209900,#209901),(#209902,#209903),
(#209904,#209905),(#209906,#209907),(#209908,#209909),(#209910,#209911),
(#209912,#209913),(#209914,#209915),(#209916,#209917),(#209918,#209919),
(#209920,#209921),(#209922,#209923),(#209924,#209925),(#209926,#209927),
(#209928,#209929),(#209930,#209931),(#209932,#209933),(#209934,#209935),
(#209936,#209937),(#209938,#209939),(#209940,#209941),(#209942,#209943),
(#209944,#209945),(#209946,#209947),(#209948,#209949),(#209950,#209951),
(#209952,#209953),(#209954,#209955),(#209956,#209957),(#209958,#209959),
(#209960,#209961),(#209962,#209963),(#209964,#209965),(#209966,#209967),
(#209968,#209969),(#209970,#209971)),.UNSPECIFIED.,.F.,.F.,.F.,(6,1,1,1,
1,1,1,1,1,1,1,1,1,1,1,1,1,1,1,1,1,1,1,1,1,1,1,1,1,1,1,1,1,1,1,1,1,1,1,1,
1,1,1,1,1,1,1,1,1,1,1,1,1,1,1,1,1,1,1,1,1,1,1,1,1,1,1,1,1,1,1,1,1,1,1,1,
1,1,1,1,1,1,1,1,1,1,1,1,1,1,1,1,1,1,1,1,1,1,1,1,1,1,1,1,1,1,1,1,1,1,1,1,
1,1,1,1,1,1,1,1,1,1,1,1,1,1,1,1,1,1,1,1,1,1,1,1,1,1,1,1,1,1,1,1,1,1,1,1,
1,1,1,1,1,1,1,1,1,1,1,1,1,1,1,1,1,1,1,1,1,1,1,1,1,1,1,1,1,1,1,1,1,1,1,1,
1,1,1,1,1,1,1,1,1,1,1,1,1,1,1,1,1,1,1,1,1,1,1,1,1,1,1,1,1,1,1,1,1,1,1,1,
1,1,1,1,1,1,1,1,1,1,1,1,1,1,1,1,1,1,1,1,1,1,1,1,1,1,1,1,1,1,1,1,1,1,1,1,
1,1,1,1,1,1,1,1,1,1,1,1,1,1,1,1,1,1,1,1,1,1,1,1,1,1,1,1,1,1,1,1,1,1,1,1,
1,1,1,1,1,1,1,1,1,1,1,1,1,1,1,1,1,1,1,1,1,1,1,1,1,1,1,1,1,1,1,1,1,1,1,1,
1,1,1,1,1,1,1,1,1,1,1,1,1,1,1,1,1,1,1,1,1,1,1,1,1,1,1,1,1,1,1,1,1,1,1,1,
1,1,1,1,1,1,1,1,1,1,1,1,1,1,1,1,1,1,1,1,1,1,1,1,1,1,1,1,1,1,1,1,1,1,1,1,
1,1,1,1,1,1,1,1,1,1,1,1,1,1,1,1,1,1,1,1,1,1,1,1,1,1,1,1,1,1,1,1,1,1,1,1,
1,1,1,1,1,1,1,1,1,1,1,1,1,1,1,1,1,1,1,1,1,1,1,1,1,1,1,1,1,1,1,6),(2,2),
(-1.,-0.998165138,-0.996330275,-0.994495413,-0.99266055,-0.990825688,-0.988990826,
-0.987155963,-0.985321101,-0.983486239,-0.981651376,-0.979816514,-0.977981651,
-0.976146789,-0.974311927,-0.972477064,-0.970642202,-0.968807339,-0.966972477,
-0.965137615,-0.963302752,-0.96146789,-0.959633028,-0.957798165,-0.955963303,
-0.95412844,-0.952293578,-0.950458716,-0.948623853,-0.946788991,-0.944954128,
-0.943119266,-0.941284404,-0.939449541,-0.937614679,-0.935779817,-0.933944954,
-0.932110092,-0.930275229,-0.928440367,-0.926605505,-0.924770642,-0.92293578,
-0.921100917,-0.919266055,-0.917431193,-0.91559633,-0.913761468,-0.911926606,
-0.910091743,-0.908256881,-0.906422018,-0.904587156,-0.902752294,-0.900917431,
-0.899082569,-0.897247706,-0.895412844,-0.893577982,-0.891743119,-0.889908257,
-0.888073394,-0.886238532,-0.88440367,-0.882568807,-0.880733945,-0.878899083,
-0.87706422,-0.875229358,-0.873394495,-0.871559633,-0.869724771,-0.867889908,
-0.866055046,-0.864220183,-0.862385321,-0.860550459,-0.858715596,-0.856880734,
-0.855045872,-0.853211009,-0.851376147,-0.849541284,-0.847706422,-0.84587156,
-0.844036697,-0.842201835,-0.840366972,-0.83853211,-0.836697248,-0.834862385,
-0.833027523,-0.831192661,-0.829357798,-0.827522936,-0.825688073,-0.823853211,
-0.822018349,-0.820183486,-0.818348624,-0.816513761,-0.814678899,-0.812844037,
-0.811009174,-0.809174312,-0.80733945,-0.805504587,-0.803669725,-0.801834862,
-0.8,-0.798165138,-0.796330275,-0.794495413,-0.79266055,-0.790825688,-0.788990826,
-0.787155963,-0.785321101,-0.783486239,-0.781651376,-0.779816514,-0.777981651,
-0.776146789,-0.774311927,-0.772477064,-0.770642202,-0.768807339,-0.766972477,
-0.765137615,-0.763302752,-0.76146789,-0.759633028,-0.757798165,-0.755963303,
-0.75412844,-0.752293578,-0.750458716,-0.748623853,-0.746788991,-0.744954128,
-0.743119266,-0.741284404,-0.739449541,-0.737614679,-0.735779817,-0.733944954,
-0.732110092,-0.730275229,-0.728440367,-0.726605505,-0.724770642,-0.72293578,
-0.721100917,-0.719266055,-0.717431193,-0.71559633,-0.713761468,-0.711926606,
-0.710091743,-0.708256881,-0.706422018,-0.704587156,-0.702752294,-0.700917431,
-0.699082569,-0.697247706,-0.695412844,-0.693577982,-0.691743119,-0.689908257,
-0.688073394,-0.686238532,-0.68440367,-0.682568807,-0.680733945,-0.678899083,
-0.67706422,-0.675229358,-0.673394495,-0.671559633,-0.669724771,-0.667889908,
-0.666055046,-0.664220183,-0.662385321,-0.660550459,-0.658715596,-0.656880734,
-0.655045872,-0.653211009,-0.651376147,-0.649541284,-0.647706422,-0.64587156,
-0.644036697,-0.642201835,-0.640366972,-0.63853211,-0.636697248,-0.634862385,
-0.633027523,-0.631192661,-0.629357798,-0.627522936,-0.625688073,-0.623853211,
-0.622018349,-0.620183486,-0.618348624,-0.616513761,-0.614678899,-0.612844037,
-0.611009174,-0.609174312,-0.60733945,-0.605504587,-0.603669725,-0.601834862,
-0.6,-0.598165138,-0.596330275,-0.594495413,-0.59266055,-0.590825688,-0.588990826,
-0.587155963,-0.585321101,-0.583486239,-0.581651376,-0.579816514,-0.577981651,
-0.576146789,-0.574311927,-0.572477064,-0.570642202,-0.568807339,-0.566972477,
-0.565137615,-0.563302752,-0.56146789,-0.559633028,-0.557798165,-0.555963303,
-0.55412844,-0.552293578,-0.550458716,-0.548623853,-0.546788991,-0.544954128,
-0.543119266,-0.541284404,-0.539449541,-0.537614679,-0.535779817,-0.533944954,
-0.532110092,-0.530275229,-0.528440367,-0.526605505,-0.524770642,-0.52293578,
-0.521100917,-0.519266055,-0.517431193,-0.51559633,-0.513761468,-0.511926606,
-0.510091743,-0.508256881,-0.506422018,-0.504587156,-0.502752294,-0.500917431,
-0.499082569,-0.497247706,-0.495412844,-0.493577982,-0.491743119,-0.489908257,
-0.488073394,-0.486238532,-0.48440367,-0.482568807,-0.480733945,-0.478899083,
-0.47706422,-0.475229358,-0.473394495,-0.471559633,-0.469724771,-0.467889908,
-0.466055046,-0.464220183,-0.462385321,-0.460550459,-0.458715596,-0.456880734,
-0.455045872,-0.453211009,-0.451376147,-0.449541284,-0.447706422,-0.44587156,
-0.444036697,-0.442201835,-0.440366972,-0.43853211,-0.436697248,-0.434862385,
-0.433027523,-0.431192661,-0.429357798,-0.427522936,-0.425688073,-0.423853211,
-0.422018349,-0.420183486,-0.418348624,-0.416513761,-0.414678899,-0.412844037,
-0.411009174,-0.409174312,-0.40733945,-0.405504587,-0.403669725,-0.401834862,
-0.4,-0.398165138,-0.396330275,-0.394495413,-0.39266055,-0.390825688,-0.388990826,
-0.387155963,-0.385321101,-0.383486239,-0.381651376,-0.379816514,-0.377981651,
-0.376146789,-0.374311927,-0.372477064,-0.370642202,-0.368807339,-0.366972477,
-0.365137615,-0.363302752,-0.36146789,-0.359633028,-0.357798165,-0.355963303,
-0.35412844,-0.352293578,-0.350458716,-0.348623853,-0.346788991,-0.344954128,
-0.343119266,-0.341284404,-0.339449541,-0.337614679,-0.335779817,-0.333944954,
-0.332110092,-0.330275229,-0.328440367,-0.326605505,-0.324770642,-0.32293578,
-0.321100917,-0.319266055,-0.317431193,-0.31559633,-0.313761468,-0.311926606,
-0.310091743,-0.308256881,-0.306422018,-0.304587156,-0.302752294,-0.300917431,
-0.299082569,-0.297247706,-0.295412844,-0.293577982,-0.291743119,-0.289908257,
-0.288073394,-0.286238532,-0.28440367,-0.282568807,-0.280733945,-0.278899083,
-0.27706422,-0.275229358,-0.273394495,-0.271559633,-0.269724771,-0.267889908,
-0.266055046,-0.264220183,-0.262385321,-0.260550459,-0.258715596,-0.256880734,
-0.255045872,-0.253211009,-0.251376147,-0.249541284,-0.247706422,-0.24587156,
-0.244036697,-0.242201835,-0.240366972,-0.23853211,-0.236697248,-0.234862385,
-0.233027523,-0.231192661,-0.229357798,-0.227522936,-0.225688073,-0.223853211,
-0.222018349,-0.220183486,-0.218348624,-0.216513761,-0.214678899,-0.212844037,
-0.211009174,-0.209174312,-0.20733945,-0.205504587,-0.203669725,-0.201834862,
-0.2,-0.198165138,-0.196330275,-0.194495413,-0.19266055,-0.190825688,-0.188990826,
-0.187155963,-0.185321101,-0.183486239,-0.181651376,-0.179816514,-0.177981651,
-0.176146789,-0.174311927,-0.172477064,-0.170642202,-0.168807339,-0.166972477,
-0.165137615,-0.163302752,-0.16146789,-0.159633028,-0.157798165,-0.155963303,
-0.15412844,-0.152293578,-0.150458716,-0.148623853,-0.146788991,-0.144954128,
-0.143172103),(0.,0.36),.UNSPECIFIED.);
#6249=B_SPLINE_SURFACE_WITH_KNOTS('',5,1,((#210625,#210626),(#210627,#210628),
(#210629,#210630),(#210631,#210632),(#210633,#210634),(#210635,#210636),
(#210637,#210638),(#210639,#210640),(#210641,#210642),(#210643,#210644),
(#210645,#210646),(#210647,#210648),(#210649,#210650),(#210651,#210652),
(#210653,#210654),(#210655,#210656),(#210657,#210658),(#210659,#210660),
(#210661,#210662),(#210663,#210664),(#210665,#210666),(#210667,#210668),
(#210669,#210670),(#210671,#210672),(#210673,#210674),(#210675,#210676),
(#210677,#210678),(#210679,#210680),(#210681,#210682),(#210683,#210684),
(#210685,#210686),(#210687,#210688),(#210689,#210690),(#210691,#210692),
(#210693,#210694),(#210695,#210696),(#210697,#210698),(#210699,#210700),
(#210701,#210702),(#210703,#210704),(#210705,#210706),(#210707,#210708),
(#210709,#210710),(#210711,#210712),(#210713,#210714),(#210715,#210716),
(#210717,#210718),(#210719,#210720),(#210721,#210722),(#210723,#210724),
(#210725,#210726),(#210727,#210728),(#210729,#210730),(#210731,#210732),
(#210733,#210734),(#210735,#210736),(#210737,#210738),(#210739,#210740),
(#210741,#210742),(#210743,#210744),(#210745,#210746),(#210747,#210748),
(#210749,#210750),(#210751,#210752),(#210753,#210754),(#210755,#210756),
(#210757,#210758),(#210759,#210760),(#210761,#210762),(#210763,#210764),
(#210765,#210766),(#210767,#210768),(#210769,#210770),(#210771,#210772),
(#210773,#210774),(#210775,#210776),(#210777,#210778),(#210779,#210780),
(#210781,#210782),(#210783,#210784),(#210785,#210786),(#210787,#210788),
(#210789,#210790),(#210791,#210792),(#210793,#210794),(#210795,#210796),
(#210797,#210798),(#210799,#210800),(#210801,#210802),(#210803,#210804),
(#210805,#210806),(#210807,#210808),(#210809,#210810),(#210811,#210812),
(#210813,#210814),(#210815,#210816),(#210817,#210818),(#210819,#210820),
(#210821,#210822),(#210823,#210824),(#210825,#210826),(#210827,#210828),
(#210829,#210830),(#210831,#210832),(#210833,#210834),(#210835,#210836),
(#210837,#210838),(#210839,#210840),(#210841,#210842),(#210843,#210844),
(#210845,#210846),(#210847,#210848),(#210849,#210850),(#210851,#210852),
(#210853,#210854),(#210855,#210856),(#210857,#210858),(#210859,#210860),
(#210861,#210862),(#210863,#210864),(#210865,#210866),(#210867,#210868),
(#210869,#210870),(#210871,#210872),(#210873,#210874),(#210875,#210876),
(#210877,#210878),(#210879,#210880),(#210881,#210882),(#210883,#210884),
(#210885,#210886),(#210887,#210888),(#210889,#210890),(#210891,#210892),
(#210893,#210894),(#210895,#210896),(#210897,#210898),(#210899,#210900),
(#210901,#210902),(#210903,#210904),(#210905,#210906),(#210907,#210908),
(#210909,#210910),(#210911,#210912),(#210913,#210914),(#210915,#210916),
(#210917,#210918),(#210919,#210920),(#210921,#210922),(#210923,#210924),
(#210925,#210926),(#210927,#210928),(#210929,#210930),(#210931,#210932),
(#210933,#210934),(#210935,#210936),(#210937,#210938),(#210939,#210940),
(#210941,#210942),(#210943,#210944),(#210945,#210946),(#210947,#210948),
(#210949,#210950),(#210951,#210952),(#210953,#210954),(#210955,#210956),
(#210957,#210958),(#210959,#210960),(#210961,#210962),(#210963,#210964),
(#210965,#210966),(#210967,#210968),(#210969,#210970),(#210971,#210972),
(#210973,#210974),(#210975,#210976),(#210977,#210978),(#210979,#210980),
(#210981,#210982),(#210983,#210984),(#210985,#210986),(#210987,#210988),
(#210989,#210990),(#210991,#210992),(#210993,#210994),(#210995,#210996),
(#210997,#210998),(#210999,#211000),(#211001,#211002),(#211003,#211004),
(#211005,#211006),(#211007,#211008),(#211009,#211010),(#211011,#211012),
(#211013,#211014),(#211015,#211016),(#211017,#211018),(#211019,#211020),
(#211021,#211022),(#211023,#211024),(#211025,#211026),(#211027,#211028),
(#211029,#211030),(#211031,#211032),(#211033,#211034),(#211035,#211036),
(#211037,#211038),(#211039,#211040),(#211041,#211042),(#211043,#211044),
(#211045,#211046),(#211047,#211048),(#211049,#211050),(#211051,#211052),
(#211053,#211054),(#211055,#211056),(#211057,#211058),(#211059,#211060),
(#211061,#211062),(#211063,#211064),(#211065,#211066),(#211067,#211068),
(#211069,#211070),(#211071,#211072),(#211073,#211074),(#211075,#211076),
(#211077,#211078),(#211079,#211080),(#211081,#211082),(#211083,#211084),
(#211085,#211086),(#211087,#211088),(#211089,#211090),(#211091,#211092),
(#211093,#211094),(#211095,#211096),(#211097,#211098),(#211099,#211100),
(#211101,#211102),(#211103,#211104),(#211105,#211106),(#211107,#211108),
(#211109,#211110),(#211111,#211112),(#211113,#211114),(#211115,#211116),
(#211117,#211118),(#211119,#211120),(#211121,#211122),(#211123,#211124),
(#211125,#211126),(#211127,#211128),(#211129,#211130),(#211131,#211132),
(#211133,#211134),(#211135,#211136),(#211137,#211138),(#211139,#211140),
(#211141,#211142),(#211143,#211144),(#211145,#211146),(#211147,#211148),
(#211149,#211150),(#211151,#211152),(#211153,#211154),(#211155,#211156),
(#211157,#211158),(#211159,#211160),(#211161,#211162),(#211163,#211164),
(#211165,#211166),(#211167,#211168),(#211169,#211170),(#211171,#211172),
(#211173,#211174),(#211175,#211176),(#211177,#211178),(#211179,#211180),
(#211181,#211182),(#211183,#211184),(#211185,#211186),(#211187,#211188),
(#211189,#211190),(#211191,#211192),(#211193,#211194),(#211195,#211196),
(#211197,#211198),(#211199,#211200),(#211201,#211202),(#211203,#211204),
(#211205,#211206),(#211207,#211208),(#211209,#211210),(#211211,#211212),
(#211213,#211214),(#211215,#211216),(#211217,#211218),(#211219,#211220),
(#211221,#211222),(#211223,#211224),(#211225,#211226),(#211227,#211228),
(#211229,#211230),(#211231,#211232),(#211233,#211234),(#211235,#211236),
(#211237,#211238),(#211239,#211240),(#211241,#211242),(#211243,#211244),
(#211245,#211246),(#211247,#211248),(#211249,#211250),(#211251,#211252),
(#211253,#211254),(#211255,#211256),(#211257,#211258),(#211259,#211260),
(#211261,#211262),(#211263,#211264),(#211265,#211266),(#211267,#211268),
(#211269,#211270),(#211271,#211272),(#211273,#211274),(#211275,#211276),
(#211277,#211278),(#211279,#211280),(#211281,#211282),(#211283,#211284),
(#211285,#211286),(#211287,#211288),(#211289,#211290),(#211291,#211292),
(#211293,#211294),(#211295,#211296),(#211297,#211298),(#211299,#211300),
(#211301,#211302),(#211303,#211304),(#211305,#211306),(#211307,#211308),
(#211309,#211310),(#211311,#211312),(#211313,#211314),(#211315,#211316),
(#211317,#211318),(#211319,#211320),(#211321,#211322),(#211323,#211324),
(#211325,#211326),(#211327,#211328),(#211329,#211330),(#211331,#211332),
(#211333,#211334),(#211335,#211336),(#211337,#211338),(#211339,#211340),
(#211341,#211342),(#211343,#211344),(#211345,#211346),(#211347,#211348),
(#211349,#211350),(#211351,#211352),(#211353,#211354),(#211355,#211356),
(#211357,#211358),(#211359,#211360),(#211361,#211362),(#211363,#211364),
(#211365,#211366),(#211367,#211368),(#211369,#211370),(#211371,#211372),
(#211373,#211374),(#211375,#211376),(#211377,#211378),(#211379,#211380),
(#211381,#211382),(#211383,#211384),(#211385,#211386),(#211387,#211388),
(#211389,#211390),(#211391,#211392),(#211393,#211394),(#211395,#211396),
(#211397,#211398),(#211399,#211400),(#211401,#211402),(#211403,#211404),
(#211405,#211406),(#211407,#211408),(#211409,#211410),(#211411,#211412),
(#211413,#211414),(#211415,#211416),(#211417,#211418),(#211419,#211420),
(#211421,#211422),(#211423,#211424),(#211425,#211426),(#211427,#211428),
(#211429,#211430),(#211431,#211432),(#211433,#211434),(#211435,#211436),
(#211437,#211438),(#211439,#211440),(#211441,#211442),(#211443,#211444),
(#211445,#211446),(#211447,#211448),(#211449,#211450),(#211451,#211452),
(#211453,#211454),(#211455,#211456),(#211457,#211458),(#211459,#211460),
(#211461,#211462),(#211463,#211464),(#211465,#211466),(#211467,#211468),
(#211469,#211470),(#211471,#211472),(#211473,#211474),(#211475,#211476),
(#211477,#211478),(#211479,#211480),(#211481,#211482),(#211483,#211484),
(#211485,#211486),(#211487,#211488),(#211489,#211490),(#211491,#211492),
(#211493,#211494),(#211495,#211496),(#211497,#211498),(#211499,#211500),
(#211501,#211502),(#211503,#211504),(#211505,#211506),(#211507,#211508),
(#211509,#211510),(#211511,#211512),(#211513,#211514),(#211515,#211516),
(#211517,#211518),(#211519,#211520),(#211521,#211522),(#211523,#211524),
(#211525,#211526),(#211527,#211528),(#211529,#211530),(#211531,#211532),
(#211533,#211534),(#211535,#211536),(#211537,#211538),(#211539,#211540),
(#211541,#211542),(#211543,#211544),(#211545,#211546),(#211547,#211548),
(#211549,#211550),(#211551,#211552),(#211553,#211554),(#211555,#211556),
(#211557,#211558),(#211559,#211560),(#211561,#211562),(#211563,#211564),
(#211565,#211566),(#211567,#211568)),.UNSPECIFIED.,.F.,.F.,.F.,(6,1,1,1,
1,1,1,1,1,1,1,1,1,1,1,1,1,1,1,1,1,1,1,1,1,1,1,1,1,1,1,1,1,1,1,1,1,1,1,1,
1,1,1,1,1,1,1,1,1,1,1,1,1,1,1,1,1,1,1,1,1,1,1,1,1,1,1,1,1,1,1,1,1,1,1,1,
1,1,1,1,1,1,1,1,1,1,1,1,1,1,1,1,1,1,1,1,1,1,1,1,1,1,1,1,1,1,1,1,1,1,1,1,
1,1,1,1,1,1,1,1,1,1,1,1,1,1,1,1,1,1,1,1,1,1,1,1,1,1,1,1,1,1,1,1,1,1,1,1,
1,1,1,1,1,1,1,1,1,1,1,1,1,1,1,1,1,1,1,1,1,1,1,1,1,1,1,1,1,1,1,1,1,1,1,1,
1,1,1,1,1,1,1,1,1,1,1,1,1,1,1,1,1,1,1,1,1,1,1,1,1,1,1,1,1,1,1,1,1,1,1,1,
1,1,1,1,1,1,1,1,1,1,1,1,1,1,1,1,1,1,1,1,1,1,1,1,1,1,1,1,1,1,1,1,1,1,1,1,
1,1,1,1,1,1,1,1,1,1,1,1,1,1,1,1,1,1,1,1,1,1,1,1,1,1,1,1,1,1,1,1,1,1,1,1,
1,1,1,1,1,1,1,1,1,1,1,1,1,1,1,1,1,1,1,1,1,1,1,1,1,1,1,1,1,1,1,1,1,1,1,1,
1,1,1,1,1,1,1,1,1,1,1,1,1,1,1,1,1,1,1,1,1,1,1,1,1,1,1,1,1,1,1,1,1,1,1,1,
1,1,1,1,1,1,1,1,1,1,1,1,1,1,1,1,1,1,1,1,1,1,1,1,1,1,1,1,1,1,1,1,1,1,1,1,
1,1,1,1,1,1,1,1,1,1,1,1,1,1,1,1,1,1,1,1,1,1,1,1,1,1,1,1,1,1,1,1,1,1,1,1,
1,1,1,1,1,1,1,1,1,1,1,1,1,1,1,1,1,1,1,1,1,1,1,1,1,1,1,1,1,1,1,6),(2,2),
(-1.,-0.998165138,-0.996330275,-0.994495413,-0.99266055,-0.990825688,-0.988990826,
-0.987155963,-0.985321101,-0.983486239,-0.981651376,-0.979816514,-0.977981651,
-0.976146789,-0.974311927,-0.972477064,-0.970642202,-0.968807339,-0.966972477,
-0.965137615,-0.963302752,-0.96146789,-0.959633028,-0.957798165,-0.955963303,
-0.95412844,-0.952293578,-0.950458716,-0.948623853,-0.946788991,-0.944954128,
-0.943119266,-0.941284404,-0.939449541,-0.937614679,-0.935779817,-0.933944954,
-0.932110092,-0.930275229,-0.928440367,-0.926605505,-0.924770642,-0.92293578,
-0.921100917,-0.919266055,-0.917431193,-0.91559633,-0.913761468,-0.911926606,
-0.910091743,-0.908256881,-0.906422018,-0.904587156,-0.902752294,-0.900917431,
-0.899082569,-0.897247706,-0.895412844,-0.893577982,-0.891743119,-0.889908257,
-0.888073394,-0.886238532,-0.88440367,-0.882568807,-0.880733945,-0.878899083,
-0.87706422,-0.875229358,-0.873394495,-0.871559633,-0.869724771,-0.867889908,
-0.866055046,-0.864220183,-0.862385321,-0.860550459,-0.858715596,-0.856880734,
-0.855045872,-0.853211009,-0.851376147,-0.849541284,-0.847706422,-0.84587156,
-0.844036697,-0.842201835,-0.840366972,-0.83853211,-0.836697248,-0.834862385,
-0.833027523,-0.831192661,-0.829357798,-0.827522936,-0.825688073,-0.823853211,
-0.822018349,-0.820183486,-0.818348624,-0.816513761,-0.814678899,-0.812844037,
-0.811009174,-0.809174312,-0.80733945,-0.805504587,-0.803669725,-0.801834862,
-0.8,-0.798165138,-0.796330275,-0.794495413,-0.79266055,-0.790825688,-0.788990826,
-0.787155963,-0.785321101,-0.783486239,-0.781651376,-0.779816514,-0.777981651,
-0.776146789,-0.774311927,-0.772477064,-0.770642202,-0.768807339,-0.766972477,
-0.765137615,-0.763302752,-0.76146789,-0.759633028,-0.757798165,-0.755963303,
-0.75412844,-0.752293578,-0.750458716,-0.748623853,-0.746788991,-0.744954128,
-0.743119266,-0.741284404,-0.739449541,-0.737614679,-0.735779817,-0.733944954,
-0.732110092,-0.730275229,-0.728440367,-0.726605505,-0.724770642,-0.72293578,
-0.721100917,-0.719266055,-0.717431193,-0.71559633,-0.713761468,-0.711926606,
-0.710091743,-0.708256881,-0.706422018,-0.704587156,-0.702752294,-0.700917431,
-0.699082569,-0.697247706,-0.695412844,-0.693577982,-0.691743119,-0.689908257,
-0.688073394,-0.686238532,-0.68440367,-0.682568807,-0.680733945,-0.678899083,
-0.67706422,-0.675229358,-0.673394495,-0.671559633,-0.669724771,-0.667889908,
-0.666055046,-0.664220183,-0.662385321,-0.660550459,-0.658715596,-0.656880734,
-0.655045872,-0.653211009,-0.651376147,-0.649541284,-0.647706422,-0.64587156,
-0.644036697,-0.642201835,-0.640366972,-0.63853211,-0.636697248,-0.634862385,
-0.633027523,-0.631192661,-0.629357798,-0.627522936,-0.625688073,-0.623853211,
-0.622018349,-0.620183486,-0.618348624,-0.616513761,-0.614678899,-0.612844037,
-0.611009174,-0.609174312,-0.60733945,-0.605504587,-0.603669725,-0.601834862,
-0.6,-0.598165138,-0.596330275,-0.594495413,-0.59266055,-0.590825688,-0.588990826,
-0.587155963,-0.585321101,-0.583486239,-0.581651376,-0.579816514,-0.577981651,
-0.576146789,-0.574311927,-0.572477064,-0.570642202,-0.568807339,-0.566972477,
-0.565137615,-0.563302752,-0.56146789,-0.559633028,-0.557798165,-0.555963303,
-0.55412844,-0.552293578,-0.550458716,-0.548623853,-0.546788991,-0.544954128,
-0.543119266,-0.541284404,-0.539449541,-0.537614679,-0.535779817,-0.533944954,
-0.532110092,-0.530275229,-0.528440367,-0.526605505,-0.524770642,-0.52293578,
-0.521100917,-0.519266055,-0.517431193,-0.51559633,-0.513761468,-0.511926606,
-0.510091743,-0.508256881,-0.506422018,-0.504587156,-0.502752294,-0.500917431,
-0.499082569,-0.497247706,-0.495412844,-0.493577982,-0.491743119,-0.489908257,
-0.488073394,-0.486238532,-0.48440367,-0.482568807,-0.480733945,-0.478899083,
-0.47706422,-0.475229358,-0.473394495,-0.471559633,-0.469724771,-0.467889908,
-0.466055046,-0.464220183,-0.462385321,-0.460550459,-0.458715596,-0.456880734,
-0.455045872,-0.453211009,-0.451376147,-0.449541284,-0.447706422,-0.44587156,
-0.444036697,-0.442201835,-0.440366972,-0.43853211,-0.436697248,-0.434862385,
-0.433027523,-0.431192661,-0.429357798,-0.427522936,-0.425688073,-0.423853211,
-0.422018349,-0.420183486,-0.418348624,-0.416513761,-0.414678899,-0.412844037,
-0.411009174,-0.409174312,-0.40733945,-0.405504587,-0.403669725,-0.401834862,
-0.4,-0.398165138,-0.396330275,-0.394495413,-0.39266055,-0.390825688,-0.388990826,
-0.387155963,-0.385321101,-0.383486239,-0.381651376,-0.379816514,-0.377981651,
-0.376146789,-0.374311927,-0.372477064,-0.370642202,-0.368807339,-0.366972477,
-0.365137615,-0.363302752,-0.36146789,-0.359633028,-0.357798165,-0.355963303,
-0.35412844,-0.352293578,-0.350458716,-0.348623853,-0.346788991,-0.344954128,
-0.343119266,-0.341284404,-0.339449541,-0.337614679,-0.335779817,-0.333944954,
-0.332110092,-0.330275229,-0.328440367,-0.326605505,-0.324770642,-0.32293578,
-0.321100917,-0.319266055,-0.317431193,-0.31559633,-0.313761468,-0.311926606,
-0.310091743,-0.308256881,-0.306422018,-0.304587156,-0.302752294,-0.300917431,
-0.299082569,-0.297247706,-0.295412844,-0.293577982,-0.291743119,-0.289908257,
-0.288073394,-0.286238532,-0.28440367,-0.282568807,-0.280733945,-0.278899083,
-0.27706422,-0.275229358,-0.273394495,-0.271559633,-0.269724771,-0.267889908,
-0.266055046,-0.264220183,-0.262385321,-0.260550459,-0.258715596,-0.256880734,
-0.255045872,-0.253211009,-0.251376147,-0.249541284,-0.247706422,-0.24587156,
-0.244036697,-0.242201835,-0.240366972,-0.23853211,-0.236697248,-0.234862385,
-0.233027523,-0.231192661,-0.229357798,-0.227522936,-0.225688073,-0.223853211,
-0.222018349,-0.220183486,-0.218348624,-0.216513761,-0.214678899,-0.212844037,
-0.211009174,-0.209174312,-0.20733945,-0.205504587,-0.203669725,-0.201834862,
-0.2,-0.198165138,-0.196330275,-0.194495413,-0.19266055,-0.190825688,-0.188990826,
-0.187155963,-0.185321101,-0.183486239,-0.181651376,-0.179816514,-0.177981651,
-0.176146789,-0.174311927,-0.172477064,-0.170642202,-0.168807339,-0.166972477,
-0.165137615,-0.163302752,-0.16146789,-0.159633028,-0.157798165,-0.155963303,
-0.15412844,-0.152293578,-0.150458716,-0.148623853,-0.146788991,-0.144954128,
-0.143172103),(0.,0.36),.UNSPECIFIED.);
#6250=B_SPLINE_SURFACE_WITH_KNOTS('',5,1,((#212195,#212196),(#212197,#212198),
(#212199,#212200),(#212201,#212202),(#212203,#212204),(#212205,#212206),
(#212207,#212208),(#212209,#212210),(#212211,#212212),(#212213,#212214),
(#212215,#212216),(#212217,#212218),(#212219,#212220),(#212221,#212222),
(#212223,#212224),(#212225,#212226),(#212227,#212228),(#212229,#212230),
(#212231,#212232),(#212233,#212234),(#212235,#212236),(#212237,#212238),
(#212239,#212240),(#212241,#212242),(#212243,#212244),(#212245,#212246),
(#212247,#212248),(#212249,#212250),(#212251,#212252),(#212253,#212254),
(#212255,#212256),(#212257,#212258),(#212259,#212260),(#212261,#212262),
(#212263,#212264),(#212265,#212266),(#212267,#212268),(#212269,#212270),
(#212271,#212272),(#212273,#212274),(#212275,#212276),(#212277,#212278),
(#212279,#212280),(#212281,#212282),(#212283,#212284),(#212285,#212286),
(#212287,#212288),(#212289,#212290),(#212291,#212292),(#212293,#212294),
(#212295,#212296),(#212297,#212298),(#212299,#212300),(#212301,#212302),
(#212303,#212304),(#212305,#212306),(#212307,#212308),(#212309,#212310),
(#212311,#212312),(#212313,#212314),(#212315,#212316),(#212317,#212318),
(#212319,#212320),(#212321,#212322),(#212323,#212324),(#212325,#212326),
(#212327,#212328),(#212329,#212330),(#212331,#212332),(#212333,#212334),
(#212335,#212336),(#212337,#212338),(#212339,#212340),(#212341,#212342),
(#212343,#212344),(#212345,#212346),(#212347,#212348),(#212349,#212350),
(#212351,#212352),(#212353,#212354),(#212355,#212356),(#212357,#212358),
(#212359,#212360),(#212361,#212362),(#212363,#212364),(#212365,#212366),
(#212367,#212368),(#212369,#212370),(#212371,#212372),(#212373,#212374),
(#212375,#212376),(#212377,#212378),(#212379,#212380),(#212381,#212382),
(#212383,#212384),(#212385,#212386),(#212387,#212388),(#212389,#212390),
(#212391,#212392),(#212393,#212394),(#212395,#212396),(#212397,#212398),
(#212399,#212400),(#212401,#212402),(#212403,#212404),(#212405,#212406),
(#212407,#212408),(#212409,#212410),(#212411,#212412),(#212413,#212414),
(#212415,#212416),(#212417,#212418),(#212419,#212420),(#212421,#212422),
(#212423,#212424),(#212425,#212426),(#212427,#212428),(#212429,#212430),
(#212431,#212432),(#212433,#212434),(#212435,#212436),(#212437,#212438),
(#212439,#212440),(#212441,#212442),(#212443,#212444),(#212445,#212446),
(#212447,#212448),(#212449,#212450),(#212451,#212452),(#212453,#212454),
(#212455,#212456),(#212457,#212458),(#212459,#212460),(#212461,#212462),
(#212463,#212464),(#212465,#212466),(#212467,#212468),(#212469,#212470),
(#212471,#212472),(#212473,#212474),(#212475,#212476),(#212477,#212478),
(#212479,#212480),(#212481,#212482),(#212483,#212484),(#212485,#212486),
(#212487,#212488),(#212489,#212490),(#212491,#212492),(#212493,#212494),
(#212495,#212496),(#212497,#212498),(#212499,#212500),(#212501,#212502),
(#212503,#212504),(#212505,#212506),(#212507,#212508),(#212509,#212510),
(#212511,#212512),(#212513,#212514),(#212515,#212516),(#212517,#212518),
(#212519,#212520),(#212521,#212522),(#212523,#212524),(#212525,#212526),
(#212527,#212528),(#212529,#212530),(#212531,#212532),(#212533,#212534),
(#212535,#212536),(#212537,#212538),(#212539,#212540),(#212541,#212542),
(#212543,#212544),(#212545,#212546),(#212547,#212548),(#212549,#212550),
(#212551,#212552),(#212553,#212554),(#212555,#212556),(#212557,#212558),
(#212559,#212560),(#212561,#212562),(#212563,#212564),(#212565,#212566),
(#212567,#212568),(#212569,#212570),(#212571,#212572),(#212573,#212574),
(#212575,#212576),(#212577,#212578),(#212579,#212580),(#212581,#212582),
(#212583,#212584),(#212585,#212586),(#212587,#212588),(#212589,#212590),
(#212591,#212592),(#212593,#212594),(#212595,#212596),(#212597,#212598),
(#212599,#212600),(#212601,#212602),(#212603,#212604),(#212605,#212606),
(#212607,#212608),(#212609,#212610),(#212611,#212612),(#212613,#212614),
(#212615,#212616),(#212617,#212618),(#212619,#212620),(#212621,#212622),
(#212623,#212624),(#212625,#212626),(#212627,#212628),(#212629,#212630),
(#212631,#212632),(#212633,#212634),(#212635,#212636),(#212637,#212638),
(#212639,#212640),(#212641,#212642),(#212643,#212644),(#212645,#212646),
(#212647,#212648),(#212649,#212650),(#212651,#212652),(#212653,#212654),
(#212655,#212656),(#212657,#212658),(#212659,#212660),(#212661,#212662),
(#212663,#212664),(#212665,#212666),(#212667,#212668),(#212669,#212670),
(#212671,#212672),(#212673,#212674),(#212675,#212676),(#212677,#212678),
(#212679,#212680),(#212681,#212682),(#212683,#212684),(#212685,#212686),
(#212687,#212688),(#212689,#212690),(#212691,#212692),(#212693,#212694),
(#212695,#212696),(#212697,#212698),(#212699,#212700),(#212701,#212702),
(#212703,#212704),(#212705,#212706),(#212707,#212708),(#212709,#212710),
(#212711,#212712),(#212713,#212714),(#212715,#212716),(#212717,#212718),
(#212719,#212720),(#212721,#212722),(#212723,#212724),(#212725,#212726),
(#212727,#212728),(#212729,#212730),(#212731,#212732),(#212733,#212734),
(#212735,#212736),(#212737,#212738),(#212739,#212740),(#212741,#212742),
(#212743,#212744),(#212745,#212746),(#212747,#212748),(#212749,#212750),
(#212751,#212752),(#212753,#212754),(#212755,#212756),(#212757,#212758),
(#212759,#212760),(#212761,#212762),(#212763,#212764),(#212765,#212766),
(#212767,#212768),(#212769,#212770),(#212771,#212772),(#212773,#212774),
(#212775,#212776),(#212777,#212778),(#212779,#212780),(#212781,#212782),
(#212783,#212784),(#212785,#212786),(#212787,#212788),(#212789,#212790),
(#212791,#212792),(#212793,#212794),(#212795,#212796),(#212797,#212798),
(#212799,#212800),(#212801,#212802),(#212803,#212804),(#212805,#212806),
(#212807,#212808),(#212809,#212810),(#212811,#212812),(#212813,#212814),
(#212815,#212816),(#212817,#212818),(#212819,#212820),(#212821,#212822),
(#212823,#212824),(#212825,#212826),(#212827,#212828),(#212829,#212830),
(#212831,#212832),(#212833,#212834),(#212835,#212836),(#212837,#212838),
(#212839,#212840),(#212841,#212842),(#212843,#212844),(#212845,#212846),
(#212847,#212848),(#212849,#212850),(#212851,#212852),(#212853,#212854),
(#212855,#212856),(#212857,#212858),(#212859,#212860),(#212861,#212862),
(#212863,#212864),(#212865,#212866),(#212867,#212868),(#212869,#212870),
(#212871,#212872),(#212873,#212874),(#212875,#212876),(#212877,#212878),
(#212879,#212880),(#212881,#212882),(#212883,#212884),(#212885,#212886),
(#212887,#212888),(#212889,#212890),(#212891,#212892),(#212893,#212894),
(#212895,#212896),(#212897,#212898),(#212899,#212900),(#212901,#212902),
(#212903,#212904),(#212905,#212906),(#212907,#212908),(#212909,#212910),
(#212911,#212912),(#212913,#212914),(#212915,#212916),(#212917,#212918),
(#212919,#212920),(#212921,#212922),(#212923,#212924),(#212925,#212926),
(#212927,#212928),(#212929,#212930),(#212931,#212932),(#212933,#212934),
(#212935,#212936),(#212937,#212938),(#212939,#212940),(#212941,#212942),
(#212943,#212944),(#212945,#212946),(#212947,#212948),(#212949,#212950),
(#212951,#212952),(#212953,#212954),(#212955,#212956),(#212957,#212958),
(#212959,#212960),(#212961,#212962),(#212963,#212964),(#212965,#212966),
(#212967,#212968),(#212969,#212970),(#212971,#212972),(#212973,#212974),
(#212975,#212976),(#212977,#212978),(#212979,#212980),(#212981,#212982),
(#212983,#212984),(#212985,#212986),(#212987,#212988),(#212989,#212990),
(#212991,#212992),(#212993,#212994),(#212995,#212996),(#212997,#212998),
(#212999,#213000),(#213001,#213002),(#213003,#213004),(#213005,#213006),
(#213007,#213008),(#213009,#213010),(#213011,#213012),(#213013,#213014),
(#213015,#213016),(#213017,#213018),(#213019,#213020),(#213021,#213022),
(#213023,#213024),(#213025,#213026),(#213027,#213028),(#213029,#213030),
(#213031,#213032),(#213033,#213034),(#213035,#213036),(#213037,#213038),
(#213039,#213040),(#213041,#213042),(#213043,#213044),(#213045,#213046),
(#213047,#213048),(#213049,#213050),(#213051,#213052),(#213053,#213054),
(#213055,#213056),(#213057,#213058),(#213059,#213060),(#213061,#213062),
(#213063,#213064),(#213065,#213066),(#213067,#213068),(#213069,#213070),
(#213071,#213072),(#213073,#213074),(#213075,#213076),(#213077,#213078),
(#213079,#213080),(#213081,#213082),(#213083,#213084),(#213085,#213086),
(#213087,#213088),(#213089,#213090),(#213091,#213092),(#213093,#213094),
(#213095,#213096),(#213097,#213098),(#213099,#213100),(#213101,#213102),
(#213103,#213104),(#213105,#213106),(#213107,#213108),(#213109,#213110),
(#213111,#213112),(#213113,#213114),(#213115,#213116),(#213117,#213118),
(#213119,#213120),(#213121,#213122),(#213123,#213124),(#213125,#213126),
(#213127,#213128),(#213129,#213130),(#213131,#213132),(#213133,#213134),
(#213135,#213136),(#213137,#213138)),.UNSPECIFIED.,.F.,.F.,.F.,(6,1,1,1,
1,1,1,1,1,1,1,1,1,1,1,1,1,1,1,1,1,1,1,1,1,1,1,1,1,1,1,1,1,1,1,1,1,1,1,1,
1,1,1,1,1,1,1,1,1,1,1,1,1,1,1,1,1,1,1,1,1,1,1,1,1,1,1,1,1,1,1,1,1,1,1,1,
1,1,1,1,1,1,1,1,1,1,1,1,1,1,1,1,1,1,1,1,1,1,1,1,1,1,1,1,1,1,1,1,1,1,1,1,
1,1,1,1,1,1,1,1,1,1,1,1,1,1,1,1,1,1,1,1,1,1,1,1,1,1,1,1,1,1,1,1,1,1,1,1,
1,1,1,1,1,1,1,1,1,1,1,1,1,1,1,1,1,1,1,1,1,1,1,1,1,1,1,1,1,1,1,1,1,1,1,1,
1,1,1,1,1,1,1,1,1,1,1,1,1,1,1,1,1,1,1,1,1,1,1,1,1,1,1,1,1,1,1,1,1,1,1,1,
1,1,1,1,1,1,1,1,1,1,1,1,1,1,1,1,1,1,1,1,1,1,1,1,1,1,1,1,1,1,1,1,1,1,1,1,
1,1,1,1,1,1,1,1,1,1,1,1,1,1,1,1,1,1,1,1,1,1,1,1,1,1,1,1,1,1,1,1,1,1,1,1,
1,1,1,1,1,1,1,1,1,1,1,1,1,1,1,1,1,1,1,1,1,1,1,1,1,1,1,1,1,1,1,1,1,1,1,1,
1,1,1,1,1,1,1,1,1,1,1,1,1,1,1,1,1,1,1,1,1,1,1,1,1,1,1,1,1,1,1,1,1,1,1,1,
1,1,1,1,1,1,1,1,1,1,1,1,1,1,1,1,1,1,1,1,1,1,1,1,1,1,1,1,1,1,1,1,1,1,1,1,
1,1,1,1,1,1,1,1,1,1,1,1,1,1,1,1,1,1,1,1,1,1,1,1,1,1,1,1,1,1,1,1,1,1,1,1,
1,1,1,1,1,1,1,1,1,1,1,1,1,1,1,1,1,1,1,1,1,1,1,1,1,1,1,1,1,1,1,6),(2,2),
(0.143172103,0.144954128,0.146788991,0.148623853,0.150458716,0.152293578,
0.15412844,0.155963303,0.157798165,0.159633028,0.16146789,0.163302752,0.165137615,
0.166972477,0.168807339,0.170642202,0.172477064,0.174311927,0.176146789,
0.177981651,0.179816514,0.181651376,0.183486239,0.185321101,0.187155963,
0.188990826,0.190825688,0.19266055,0.194495413,0.196330275,0.198165138,
0.2,0.201834862,0.203669725,0.205504587,0.20733945,0.209174312,0.211009174,
0.212844037,0.214678899,0.216513761,0.218348624,0.220183486,0.222018349,
0.223853211,0.225688073,0.227522936,0.229357798,0.231192661,0.233027523,
0.234862385,0.236697248,0.23853211,0.240366972,0.242201835,0.244036697,
0.24587156,0.247706422,0.249541284,0.251376147,0.253211009,0.255045872,
0.256880734,0.258715596,0.260550459,0.262385321,0.264220183,0.266055046,
0.267889908,0.269724771,0.271559633,0.273394495,0.275229358,0.27706422,
0.278899083,0.280733945,0.282568807,0.28440367,0.286238532,0.288073394,
0.289908257,0.291743119,0.293577982,0.295412844,0.297247706,0.299082569,
0.300917431,0.302752294,0.304587156,0.306422018,0.308256881,0.310091743,
0.311926606,0.313761468,0.31559633,0.317431193,0.319266055,0.321100917,
0.32293578,0.324770642,0.326605505,0.328440367,0.330275229,0.332110092,
0.333944954,0.335779817,0.337614679,0.339449541,0.341284404,0.343119266,
0.344954128,0.346788991,0.348623853,0.350458716,0.352293578,0.35412844,
0.355963303,0.357798165,0.359633028,0.36146789,0.363302752,0.365137615,
0.366972477,0.368807339,0.370642202,0.372477064,0.374311927,0.376146789,
0.377981651,0.379816514,0.381651376,0.383486239,0.385321101,0.387155963,
0.388990826,0.390825688,0.39266055,0.394495413,0.396330275,0.398165138,
0.4,0.401834862,0.403669725,0.405504587,0.40733945,0.409174312,0.411009174,
0.412844037,0.414678899,0.416513761,0.418348624,0.420183486,0.422018349,
0.423853211,0.425688073,0.427522936,0.429357798,0.431192661,0.433027523,
0.434862385,0.436697248,0.43853211,0.440366972,0.442201835,0.444036697,
0.44587156,0.447706422,0.449541284,0.451376147,0.453211009,0.455045872,
0.456880734,0.458715596,0.460550459,0.462385321,0.464220183,0.466055046,
0.467889908,0.469724771,0.471559633,0.473394495,0.475229358,0.47706422,
0.478899083,0.480733945,0.482568807,0.48440367,0.486238532,0.488073394,
0.489908257,0.491743119,0.493577982,0.495412844,0.497247706,0.499082569,
0.500917431,0.502752294,0.504587156,0.506422018,0.508256881,0.510091743,
0.511926606,0.513761468,0.51559633,0.517431193,0.519266055,0.521100917,
0.52293578,0.524770642,0.526605505,0.528440367,0.530275229,0.532110092,
0.533944954,0.535779817,0.537614679,0.539449541,0.541284404,0.543119266,
0.544954128,0.546788991,0.548623853,0.550458716,0.552293578,0.55412844,
0.555963303,0.557798165,0.559633028,0.56146789,0.563302752,0.565137615,
0.566972477,0.568807339,0.570642202,0.572477064,0.574311927,0.576146789,
0.577981651,0.579816514,0.581651376,0.583486239,0.585321101,0.587155963,
0.588990826,0.590825688,0.59266055,0.594495413,0.596330275,0.598165138,
0.6,0.601834862,0.603669725,0.605504587,0.60733945,0.609174312,0.611009174,
0.612844037,0.614678899,0.616513761,0.618348624,0.620183486,0.622018349,
0.623853211,0.625688073,0.627522936,0.629357798,0.631192661,0.633027523,
0.634862385,0.636697248,0.63853211,0.640366972,0.642201835,0.644036697,
0.64587156,0.647706422,0.649541284,0.651376147,0.653211009,0.655045872,
0.656880734,0.658715596,0.660550459,0.662385321,0.664220183,0.666055046,
0.667889908,0.669724771,0.671559633,0.673394495,0.675229358,0.67706422,
0.678899083,0.680733945,0.682568807,0.68440367,0.686238532,0.688073394,
0.689908257,0.691743119,0.693577982,0.695412844,0.697247706,0.699082569,
0.700917431,0.702752294,0.704587156,0.706422018,0.708256881,0.710091743,
0.711926606,0.713761468,0.71559633,0.717431193,0.719266055,0.721100917,
0.72293578,0.724770642,0.726605505,0.728440367,0.730275229,0.732110092,
0.733944954,0.735779817,0.737614679,0.739449541,0.741284404,0.743119266,
0.744954128,0.746788991,0.748623853,0.750458716,0.752293578,0.75412844,
0.755963303,0.757798165,0.759633028,0.76146789,0.763302752,0.765137615,
0.766972477,0.768807339,0.770642202,0.772477064,0.774311927,0.776146789,
0.777981651,0.779816514,0.781651376,0.783486239,0.785321101,0.787155963,
0.788990826,0.790825688,0.79266055,0.794495413,0.796330275,0.798165138,
0.8,0.801834862,0.803669725,0.805504587,0.80733945,0.809174312,0.811009174,
0.812844037,0.814678899,0.816513761,0.818348624,0.820183486,0.822018349,
0.823853211,0.825688073,0.827522936,0.829357798,0.831192661,0.833027523,
0.834862385,0.836697248,0.83853211,0.840366972,0.842201835,0.844036697,
0.84587156,0.847706422,0.849541284,0.851376147,0.853211009,0.855045872,
0.856880734,0.858715596,0.860550459,0.862385321,0.864220183,0.866055046,
0.867889908,0.869724771,0.871559633,0.873394495,0.875229358,0.87706422,
0.878899083,0.880733945,0.882568807,0.88440367,0.886238532,0.888073394,
0.889908257,0.891743119,0.893577982,0.895412844,0.897247706,0.899082569,
0.900917431,0.902752294,0.904587156,0.906422018,0.908256881,0.910091743,
0.911926606,0.913761468,0.91559633,0.917431193,0.919266055,0.921100917,
0.92293578,0.924770642,0.926605505,0.928440367,0.930275229,0.932110092,
0.933944954,0.935779817,0.937614679,0.939449541,0.941284404,0.943119266,
0.944954128,0.946788991,0.948623853,0.950458716,0.952293578,0.95412844,
0.955963303,0.957798165,0.959633028,0.96146789,0.963302752,0.965137615,
0.966972477,0.968807339,0.970642202,0.972477064,0.974311927,0.976146789,
0.977981651,0.979816514,0.981651376,0.983486239,0.985321101,0.987155963,
0.988990826,0.990825688,0.99266055,0.994495413,0.996330275,0.998165138,
1.),(0.,0.36),.UNSPECIFIED.);
#6251=B_SPLINE_SURFACE_WITH_KNOTS('',5,1,((#213789,#213790),(#213791,#213792),
(#213793,#213794),(#213795,#213796),(#213797,#213798),(#213799,#213800),
(#213801,#213802),(#213803,#213804),(#213805,#213806),(#213807,#213808),
(#213809,#213810),(#213811,#213812),(#213813,#213814),(#213815,#213816),
(#213817,#213818),(#213819,#213820),(#213821,#213822),(#213823,#213824),
(#213825,#213826),(#213827,#213828),(#213829,#213830),(#213831,#213832),
(#213833,#213834),(#213835,#213836),(#213837,#213838),(#213839,#213840),
(#213841,#213842),(#213843,#213844),(#213845,#213846),(#213847,#213848),
(#213849,#213850),(#213851,#213852),(#213853,#213854),(#213855,#213856),
(#213857,#213858),(#213859,#213860),(#213861,#213862),(#213863,#213864),
(#213865,#213866),(#213867,#213868),(#213869,#213870),(#213871,#213872),
(#213873,#213874),(#213875,#213876),(#213877,#213878),(#213879,#213880),
(#213881,#213882),(#213883,#213884),(#213885,#213886),(#213887,#213888),
(#213889,#213890),(#213891,#213892),(#213893,#213894),(#213895,#213896),
(#213897,#213898),(#213899,#213900),(#213901,#213902),(#213903,#213904),
(#213905,#213906),(#213907,#213908),(#213909,#213910),(#213911,#213912),
(#213913,#213914),(#213915,#213916),(#213917,#213918),(#213919,#213920),
(#213921,#213922),(#213923,#213924),(#213925,#213926),(#213927,#213928),
(#213929,#213930),(#213931,#213932),(#213933,#213934),(#213935,#213936),
(#213937,#213938),(#213939,#213940),(#213941,#213942),(#213943,#213944),
(#213945,#213946),(#213947,#213948),(#213949,#213950),(#213951,#213952),
(#213953,#213954),(#213955,#213956),(#213957,#213958),(#213959,#213960),
(#213961,#213962),(#213963,#213964),(#213965,#213966),(#213967,#213968),
(#213969,#213970),(#213971,#213972),(#213973,#213974),(#213975,#213976),
(#213977,#213978),(#213979,#213980),(#213981,#213982),(#213983,#213984),
(#213985,#213986),(#213987,#213988),(#213989,#213990),(#213991,#213992),
(#213993,#213994),(#213995,#213996),(#213997,#213998),(#213999,#214000),
(#214001,#214002),(#214003,#214004),(#214005,#214006),(#214007,#214008),
(#214009,#214010),(#214011,#214012),(#214013,#214014),(#214015,#214016),
(#214017,#214018),(#214019,#214020),(#214021,#214022),(#214023,#214024),
(#214025,#214026),(#214027,#214028),(#214029,#214030),(#214031,#214032),
(#214033,#214034),(#214035,#214036),(#214037,#214038),(#214039,#214040),
(#214041,#214042),(#214043,#214044),(#214045,#214046),(#214047,#214048),
(#214049,#214050),(#214051,#214052),(#214053,#214054),(#214055,#214056),
(#214057,#214058),(#214059,#214060),(#214061,#214062),(#214063,#214064),
(#214065,#214066),(#214067,#214068),(#214069,#214070),(#214071,#214072),
(#214073,#214074),(#214075,#214076),(#214077,#214078),(#214079,#214080),
(#214081,#214082),(#214083,#214084),(#214085,#214086),(#214087,#214088),
(#214089,#214090),(#214091,#214092),(#214093,#214094),(#214095,#214096),
(#214097,#214098),(#214099,#214100),(#214101,#214102),(#214103,#214104),
(#214105,#214106),(#214107,#214108),(#214109,#214110),(#214111,#214112),
(#214113,#214114),(#214115,#214116),(#214117,#214118),(#214119,#214120),
(#214121,#214122),(#214123,#214124),(#214125,#214126),(#214127,#214128),
(#214129,#214130),(#214131,#214132),(#214133,#214134),(#214135,#214136),
(#214137,#214138),(#214139,#214140),(#214141,#214142),(#214143,#214144),
(#214145,#214146),(#214147,#214148),(#214149,#214150),(#214151,#214152),
(#214153,#214154),(#214155,#214156),(#214157,#214158),(#214159,#214160),
(#214161,#214162),(#214163,#214164),(#214165,#214166),(#214167,#214168),
(#214169,#214170),(#214171,#214172),(#214173,#214174),(#214175,#214176),
(#214177,#214178),(#214179,#214180),(#214181,#214182),(#214183,#214184),
(#214185,#214186),(#214187,#214188),(#214189,#214190),(#214191,#214192),
(#214193,#214194),(#214195,#214196),(#214197,#214198),(#214199,#214200),
(#214201,#214202),(#214203,#214204),(#214205,#214206),(#214207,#214208),
(#214209,#214210),(#214211,#214212),(#214213,#214214),(#214215,#214216),
(#214217,#214218),(#214219,#214220),(#214221,#214222),(#214223,#214224),
(#214225,#214226),(#214227,#214228),(#214229,#214230),(#214231,#214232),
(#214233,#214234),(#214235,#214236),(#214237,#214238),(#214239,#214240),
(#214241,#214242),(#214243,#214244),(#214245,#214246),(#214247,#214248),
(#214249,#214250),(#214251,#214252),(#214253,#214254),(#214255,#214256),
(#214257,#214258),(#214259,#214260),(#214261,#214262),(#214263,#214264),
(#214265,#214266),(#214267,#214268),(#214269,#214270),(#214271,#214272),
(#214273,#214274),(#214275,#214276),(#214277,#214278),(#214279,#214280),
(#214281,#214282),(#214283,#214284),(#214285,#214286),(#214287,#214288),
(#214289,#214290),(#214291,#214292),(#214293,#214294),(#214295,#214296),
(#214297,#214298),(#214299,#214300),(#214301,#214302),(#214303,#214304),
(#214305,#214306),(#214307,#214308),(#214309,#214310),(#214311,#214312),
(#214313,#214314),(#214315,#214316),(#214317,#214318),(#214319,#214320),
(#214321,#214322),(#214323,#214324),(#214325,#214326),(#214327,#214328),
(#214329,#214330),(#214331,#214332),(#214333,#214334),(#214335,#214336),
(#214337,#214338),(#214339,#214340),(#214341,#214342),(#214343,#214344),
(#214345,#214346),(#214347,#214348),(#214349,#214350),(#214351,#214352),
(#214353,#214354),(#214355,#214356),(#214357,#214358),(#214359,#214360),
(#214361,#214362),(#214363,#214364),(#214365,#214366),(#214367,#214368),
(#214369,#214370),(#214371,#214372),(#214373,#214374),(#214375,#214376),
(#214377,#214378),(#214379,#214380),(#214381,#214382),(#214383,#214384),
(#214385,#214386),(#214387,#214388),(#214389,#214390),(#214391,#214392),
(#214393,#214394),(#214395,#214396),(#214397,#214398),(#214399,#214400),
(#214401,#214402),(#214403,#214404),(#214405,#214406),(#214407,#214408),
(#214409,#214410),(#214411,#214412),(#214413,#214414),(#214415,#214416),
(#214417,#214418),(#214419,#214420),(#214421,#214422),(#214423,#214424),
(#214425,#214426),(#214427,#214428),(#214429,#214430),(#214431,#214432),
(#214433,#214434),(#214435,#214436),(#214437,#214438),(#214439,#214440),
(#214441,#214442),(#214443,#214444),(#214445,#214446),(#214447,#214448),
(#214449,#214450),(#214451,#214452),(#214453,#214454),(#214455,#214456),
(#214457,#214458),(#214459,#214460),(#214461,#214462),(#214463,#214464),
(#214465,#214466),(#214467,#214468),(#214469,#214470),(#214471,#214472),
(#214473,#214474),(#214475,#214476),(#214477,#214478),(#214479,#214480),
(#214481,#214482),(#214483,#214484),(#214485,#214486),(#214487,#214488),
(#214489,#214490),(#214491,#214492),(#214493,#214494),(#214495,#214496),
(#214497,#214498),(#214499,#214500),(#214501,#214502),(#214503,#214504),
(#214505,#214506),(#214507,#214508),(#214509,#214510),(#214511,#214512),
(#214513,#214514),(#214515,#214516),(#214517,#214518),(#214519,#214520),
(#214521,#214522),(#214523,#214524),(#214525,#214526),(#214527,#214528),
(#214529,#214530),(#214531,#214532),(#214533,#214534),(#214535,#214536),
(#214537,#214538),(#214539,#214540),(#214541,#214542),(#214543,#214544),
(#214545,#214546),(#214547,#214548),(#214549,#214550),(#214551,#214552),
(#214553,#214554),(#214555,#214556),(#214557,#214558),(#214559,#214560),
(#214561,#214562),(#214563,#214564),(#214565,#214566),(#214567,#214568),
(#214569,#214570),(#214571,#214572),(#214573,#214574),(#214575,#214576),
(#214577,#214578),(#214579,#214580),(#214581,#214582),(#214583,#214584),
(#214585,#214586),(#214587,#214588),(#214589,#214590),(#214591,#214592),
(#214593,#214594),(#214595,#214596),(#214597,#214598),(#214599,#214600),
(#214601,#214602),(#214603,#214604),(#214605,#214606),(#214607,#214608),
(#214609,#214610),(#214611,#214612),(#214613,#214614),(#214615,#214616),
(#214617,#214618),(#214619,#214620),(#214621,#214622),(#214623,#214624),
(#214625,#214626),(#214627,#214628),(#214629,#214630),(#214631,#214632),
(#214633,#214634),(#214635,#214636),(#214637,#214638),(#214639,#214640),
(#214641,#214642),(#214643,#214644),(#214645,#214646),(#214647,#214648),
(#214649,#214650),(#214651,#214652),(#214653,#214654),(#214655,#214656),
(#214657,#214658),(#214659,#214660),(#214661,#214662),(#214663,#214664),
(#214665,#214666),(#214667,#214668),(#214669,#214670),(#214671,#214672),
(#214673,#214674),(#214675,#214676),(#214677,#214678),(#214679,#214680),
(#214681,#214682),(#214683,#214684),(#214685,#214686),(#214687,#214688),
(#214689,#214690),(#214691,#214692),(#214693,#214694),(#214695,#214696),
(#214697,#214698),(#214699,#214700),(#214701,#214702),(#214703,#214704),
(#214705,#214706),(#214707,#214708),(#214709,#214710),(#214711,#214712),
(#214713,#214714),(#214715,#214716),(#214717,#214718),(#214719,#214720),
(#214721,#214722),(#214723,#214724),(#214725,#214726),(#214727,#214728),
(#214729,#214730),(#214731,#214732)),.UNSPECIFIED.,.F.,.F.,.F.,(6,1,1,1,
1,1,1,1,1,1,1,1,1,1,1,1,1,1,1,1,1,1,1,1,1,1,1,1,1,1,1,1,1,1,1,1,1,1,1,1,
1,1,1,1,1,1,1,1,1,1,1,1,1,1,1,1,1,1,1,1,1,1,1,1,1,1,1,1,1,1,1,1,1,1,1,1,
1,1,1,1,1,1,1,1,1,1,1,1,1,1,1,1,1,1,1,1,1,1,1,1,1,1,1,1,1,1,1,1,1,1,1,1,
1,1,1,1,1,1,1,1,1,1,1,1,1,1,1,1,1,1,1,1,1,1,1,1,1,1,1,1,1,1,1,1,1,1,1,1,
1,1,1,1,1,1,1,1,1,1,1,1,1,1,1,1,1,1,1,1,1,1,1,1,1,1,1,1,1,1,1,1,1,1,1,1,
1,1,1,1,1,1,1,1,1,1,1,1,1,1,1,1,1,1,1,1,1,1,1,1,1,1,1,1,1,1,1,1,1,1,1,1,
1,1,1,1,1,1,1,1,1,1,1,1,1,1,1,1,1,1,1,1,1,1,1,1,1,1,1,1,1,1,1,1,1,1,1,1,
1,1,1,1,1,1,1,1,1,1,1,1,1,1,1,1,1,1,1,1,1,1,1,1,1,1,1,1,1,1,1,1,1,1,1,1,
1,1,1,1,1,1,1,1,1,1,1,1,1,1,1,1,1,1,1,1,1,1,1,1,1,1,1,1,1,1,1,1,1,1,1,1,
1,1,1,1,1,1,1,1,1,1,1,1,1,1,1,1,1,1,1,1,1,1,1,1,1,1,1,1,1,1,1,1,1,1,1,1,
1,1,1,1,1,1,1,1,1,1,1,1,1,1,1,1,1,1,1,1,1,1,1,1,1,1,1,1,1,1,1,1,1,1,1,1,
1,1,1,1,1,1,1,1,1,1,1,1,1,1,1,1,1,1,1,1,1,1,1,1,1,1,1,1,1,1,1,1,1,1,1,1,
1,1,1,1,1,1,1,1,1,1,1,1,1,1,1,1,1,1,1,1,1,1,1,1,1,1,1,1,1,1,1,6),(2,2),
(0.143172104,0.144954128,0.146788991,0.148623853,0.150458716,0.152293578,
0.15412844,0.155963303,0.157798165,0.159633028,0.16146789,0.163302752,0.165137615,
0.166972477,0.168807339,0.170642202,0.172477064,0.174311927,0.176146789,
0.177981651,0.179816514,0.181651376,0.183486239,0.185321101,0.187155963,
0.188990826,0.190825688,0.19266055,0.194495413,0.196330275,0.198165138,
0.2,0.201834862,0.203669725,0.205504587,0.20733945,0.209174312,0.211009174,
0.212844037,0.214678899,0.216513761,0.218348624,0.220183486,0.222018349,
0.223853211,0.225688073,0.227522936,0.229357798,0.231192661,0.233027523,
0.234862385,0.236697248,0.23853211,0.240366972,0.242201835,0.244036697,
0.24587156,0.247706422,0.249541284,0.251376147,0.253211009,0.255045872,
0.256880734,0.258715596,0.260550459,0.262385321,0.264220183,0.266055046,
0.267889908,0.269724771,0.271559633,0.273394495,0.275229358,0.27706422,
0.278899083,0.280733945,0.282568807,0.28440367,0.286238532,0.288073394,
0.289908257,0.291743119,0.293577982,0.295412844,0.297247706,0.299082569,
0.300917431,0.302752294,0.304587156,0.306422018,0.308256881,0.310091743,
0.311926606,0.313761468,0.31559633,0.317431193,0.319266055,0.321100917,
0.32293578,0.324770642,0.326605505,0.328440367,0.330275229,0.332110092,
0.333944954,0.335779817,0.337614679,0.339449541,0.341284404,0.343119266,
0.344954128,0.346788991,0.348623853,0.350458716,0.352293578,0.35412844,
0.355963303,0.357798165,0.359633028,0.36146789,0.363302752,0.365137615,
0.366972477,0.368807339,0.370642202,0.372477064,0.374311927,0.376146789,
0.377981651,0.379816514,0.381651376,0.383486239,0.385321101,0.387155963,
0.388990826,0.390825688,0.39266055,0.394495413,0.396330275,0.398165138,
0.4,0.401834862,0.403669725,0.405504587,0.40733945,0.409174312,0.411009174,
0.412844037,0.414678899,0.416513761,0.418348624,0.420183486,0.422018349,
0.423853211,0.425688073,0.427522936,0.429357798,0.431192661,0.433027523,
0.434862385,0.436697248,0.43853211,0.440366972,0.442201835,0.444036697,
0.44587156,0.447706422,0.449541284,0.451376147,0.453211009,0.455045872,
0.456880734,0.458715596,0.460550459,0.462385321,0.464220183,0.466055046,
0.467889908,0.469724771,0.471559633,0.473394495,0.475229358,0.47706422,
0.478899083,0.480733945,0.482568807,0.48440367,0.486238532,0.488073394,
0.489908257,0.491743119,0.493577982,0.495412844,0.497247706,0.499082569,
0.500917431,0.502752294,0.504587156,0.506422018,0.508256881,0.510091743,
0.511926606,0.513761468,0.51559633,0.517431193,0.519266055,0.521100917,
0.52293578,0.524770642,0.526605505,0.528440367,0.530275229,0.532110092,
0.533944954,0.535779817,0.537614679,0.539449541,0.541284404,0.543119266,
0.544954128,0.546788991,0.548623853,0.550458716,0.552293578,0.55412844,
0.555963303,0.557798165,0.559633028,0.56146789,0.563302752,0.565137615,
0.566972477,0.568807339,0.570642202,0.572477064,0.574311927,0.576146789,
0.577981651,0.579816514,0.581651376,0.583486239,0.585321101,0.587155963,
0.588990826,0.590825688,0.59266055,0.594495413,0.596330275,0.598165138,
0.6,0.601834862,0.603669725,0.605504587,0.60733945,0.609174312,0.611009174,
0.612844037,0.614678899,0.616513761,0.618348624,0.620183486,0.622018349,
0.623853211,0.625688073,0.627522936,0.629357798,0.631192661,0.633027523,
0.634862385,0.636697248,0.63853211,0.640366972,0.642201835,0.644036697,
0.64587156,0.647706422,0.649541284,0.651376147,0.653211009,0.655045872,
0.656880734,0.658715596,0.660550459,0.662385321,0.664220183,0.666055046,
0.667889908,0.669724771,0.671559633,0.673394495,0.675229358,0.67706422,
0.678899083,0.680733945,0.682568807,0.68440367,0.686238532,0.688073394,
0.689908257,0.691743119,0.693577982,0.695412844,0.697247706,0.699082569,
0.700917431,0.702752294,0.704587156,0.706422018,0.708256881,0.710091743,
0.711926606,0.713761468,0.71559633,0.717431193,0.719266055,0.721100917,
0.72293578,0.724770642,0.726605505,0.728440367,0.730275229,0.732110092,
0.733944954,0.735779817,0.737614679,0.739449541,0.741284404,0.743119266,
0.744954128,0.746788991,0.748623853,0.750458716,0.752293578,0.75412844,
0.755963303,0.757798165,0.759633028,0.76146789,0.763302752,0.765137615,
0.766972477,0.768807339,0.770642202,0.772477064,0.774311927,0.776146789,
0.777981651,0.779816514,0.781651376,0.783486239,0.785321101,0.787155963,
0.788990826,0.790825688,0.79266055,0.794495413,0.796330275,0.798165138,
0.8,0.801834862,0.803669725,0.805504587,0.80733945,0.809174312,0.811009174,
0.812844037,0.814678899,0.816513761,0.818348624,0.820183486,0.822018349,
0.823853211,0.825688073,0.827522936,0.829357798,0.831192661,0.833027523,
0.834862385,0.836697248,0.83853211,0.840366972,0.842201835,0.844036697,
0.84587156,0.847706422,0.849541284,0.851376147,0.853211009,0.855045872,
0.856880734,0.858715596,0.860550459,0.862385321,0.864220183,0.866055046,
0.867889908,0.869724771,0.871559633,0.873394495,0.875229358,0.87706422,
0.878899083,0.880733945,0.882568807,0.88440367,0.886238532,0.888073394,
0.889908257,0.891743119,0.893577982,0.895412844,0.897247706,0.899082569,
0.900917431,0.902752294,0.904587156,0.906422018,0.908256881,0.910091743,
0.911926606,0.913761468,0.91559633,0.917431193,0.919266055,0.921100917,
0.92293578,0.924770642,0.926605505,0.928440367,0.930275229,0.932110092,
0.933944954,0.935779817,0.937614679,0.939449541,0.941284404,0.943119266,
0.944954128,0.946788991,0.948623853,0.950458716,0.952293578,0.95412844,
0.955963303,0.957798165,0.959633028,0.96146789,0.963302752,0.965137615,
0.966972477,0.968807339,0.970642202,0.972477064,0.974311927,0.976146789,
0.977981651,0.979816514,0.981651376,0.983486239,0.985321101,0.987155963,
0.988990826,0.990825688,0.99266055,0.994495413,0.996330275,0.998165138,
1.),(0.,0.36),.UNSPECIFIED.);
#6252=B_SPLINE_SURFACE_WITH_KNOTS('',5,1,((#215365,#215366),(#215367,#215368),
(#215369,#215370),(#215371,#215372),(#215373,#215374),(#215375,#215376),
(#215377,#215378),(#215379,#215380),(#215381,#215382),(#215383,#215384),
(#215385,#215386),(#215387,#215388),(#215389,#215390),(#215391,#215392),
(#215393,#215394),(#215395,#215396),(#215397,#215398),(#215399,#215400),
(#215401,#215402),(#215403,#215404),(#215405,#215406),(#215407,#215408),
(#215409,#215410),(#215411,#215412),(#215413,#215414),(#215415,#215416),
(#215417,#215418),(#215419,#215420),(#215421,#215422),(#215423,#215424),
(#215425,#215426),(#215427,#215428),(#215429,#215430),(#215431,#215432),
(#215433,#215434),(#215435,#215436),(#215437,#215438),(#215439,#215440),
(#215441,#215442),(#215443,#215444),(#215445,#215446),(#215447,#215448),
(#215449,#215450),(#215451,#215452),(#215453,#215454),(#215455,#215456),
(#215457,#215458),(#215459,#215460),(#215461,#215462),(#215463,#215464),
(#215465,#215466),(#215467,#215468),(#215469,#215470),(#215471,#215472),
(#215473,#215474),(#215475,#215476),(#215477,#215478),(#215479,#215480),
(#215481,#215482),(#215483,#215484),(#215485,#215486),(#215487,#215488),
(#215489,#215490),(#215491,#215492),(#215493,#215494),(#215495,#215496),
(#215497,#215498),(#215499,#215500),(#215501,#215502),(#215503,#215504),
(#215505,#215506),(#215507,#215508),(#215509,#215510),(#215511,#215512),
(#215513,#215514),(#215515,#215516),(#215517,#215518),(#215519,#215520),
(#215521,#215522),(#215523,#215524),(#215525,#215526),(#215527,#215528),
(#215529,#215530),(#215531,#215532),(#215533,#215534),(#215535,#215536),
(#215537,#215538),(#215539,#215540),(#215541,#215542),(#215543,#215544),
(#215545,#215546),(#215547,#215548),(#215549,#215550),(#215551,#215552),
(#215553,#215554),(#215555,#215556),(#215557,#215558),(#215559,#215560),
(#215561,#215562),(#215563,#215564),(#215565,#215566),(#215567,#215568),
(#215569,#215570),(#215571,#215572),(#215573,#215574),(#215575,#215576),
(#215577,#215578),(#215579,#215580),(#215581,#215582),(#215583,#215584),
(#215585,#215586),(#215587,#215588),(#215589,#215590),(#215591,#215592),
(#215593,#215594),(#215595,#215596),(#215597,#215598),(#215599,#215600),
(#215601,#215602),(#215603,#215604),(#215605,#215606),(#215607,#215608),
(#215609,#215610),(#215611,#215612),(#215613,#215614),(#215615,#215616),
(#215617,#215618),(#215619,#215620),(#215621,#215622),(#215623,#215624),
(#215625,#215626),(#215627,#215628),(#215629,#215630),(#215631,#215632),
(#215633,#215634),(#215635,#215636),(#215637,#215638),(#215639,#215640),
(#215641,#215642),(#215643,#215644),(#215645,#215646),(#215647,#215648),
(#215649,#215650),(#215651,#215652),(#215653,#215654),(#215655,#215656),
(#215657,#215658),(#215659,#215660),(#215661,#215662),(#215663,#215664),
(#215665,#215666),(#215667,#215668),(#215669,#215670),(#215671,#215672),
(#215673,#215674),(#215675,#215676),(#215677,#215678),(#215679,#215680),
(#215681,#215682),(#215683,#215684),(#215685,#215686),(#215687,#215688),
(#215689,#215690),(#215691,#215692),(#215693,#215694),(#215695,#215696),
(#215697,#215698),(#215699,#215700),(#215701,#215702),(#215703,#215704),
(#215705,#215706),(#215707,#215708),(#215709,#215710),(#215711,#215712),
(#215713,#215714),(#215715,#215716),(#215717,#215718),(#215719,#215720),
(#215721,#215722),(#215723,#215724),(#215725,#215726),(#215727,#215728),
(#215729,#215730),(#215731,#215732),(#215733,#215734),(#215735,#215736),
(#215737,#215738),(#215739,#215740),(#215741,#215742),(#215743,#215744),
(#215745,#215746),(#215747,#215748),(#215749,#215750),(#215751,#215752),
(#215753,#215754),(#215755,#215756),(#215757,#215758),(#215759,#215760),
(#215761,#215762),(#215763,#215764),(#215765,#215766),(#215767,#215768),
(#215769,#215770),(#215771,#215772),(#215773,#215774),(#215775,#215776),
(#215777,#215778),(#215779,#215780),(#215781,#215782),(#215783,#215784),
(#215785,#215786),(#215787,#215788),(#215789,#215790),(#215791,#215792),
(#215793,#215794),(#215795,#215796),(#215797,#215798),(#215799,#215800),
(#215801,#215802),(#215803,#215804),(#215805,#215806),(#215807,#215808),
(#215809,#215810),(#215811,#215812),(#215813,#215814),(#215815,#215816),
(#215817,#215818),(#215819,#215820),(#215821,#215822),(#215823,#215824),
(#215825,#215826),(#215827,#215828),(#215829,#215830),(#215831,#215832),
(#215833,#215834),(#215835,#215836),(#215837,#215838),(#215839,#215840),
(#215841,#215842),(#215843,#215844),(#215845,#215846),(#215847,#215848),
(#215849,#215850),(#215851,#215852),(#215853,#215854),(#215855,#215856),
(#215857,#215858),(#215859,#215860),(#215861,#215862),(#215863,#215864),
(#215865,#215866),(#215867,#215868),(#215869,#215870),(#215871,#215872),
(#215873,#215874),(#215875,#215876),(#215877,#215878),(#215879,#215880),
(#215881,#215882),(#215883,#215884),(#215885,#215886),(#215887,#215888),
(#215889,#215890),(#215891,#215892),(#215893,#215894),(#215895,#215896),
(#215897,#215898),(#215899,#215900),(#215901,#215902),(#215903,#215904),
(#215905,#215906),(#215907,#215908),(#215909,#215910),(#215911,#215912),
(#215913,#215914),(#215915,#215916),(#215917,#215918),(#215919,#215920),
(#215921,#215922),(#215923,#215924),(#215925,#215926),(#215927,#215928),
(#215929,#215930),(#215931,#215932),(#215933,#215934),(#215935,#215936),
(#215937,#215938),(#215939,#215940),(#215941,#215942),(#215943,#215944),
(#215945,#215946),(#215947,#215948),(#215949,#215950),(#215951,#215952),
(#215953,#215954),(#215955,#215956),(#215957,#215958),(#215959,#215960),
(#215961,#215962),(#215963,#215964),(#215965,#215966),(#215967,#215968),
(#215969,#215970),(#215971,#215972),(#215973,#215974),(#215975,#215976),
(#215977,#215978),(#215979,#215980),(#215981,#215982),(#215983,#215984),
(#215985,#215986),(#215987,#215988),(#215989,#215990),(#215991,#215992),
(#215993,#215994),(#215995,#215996),(#215997,#215998),(#215999,#216000),
(#216001,#216002),(#216003,#216004),(#216005,#216006),(#216007,#216008),
(#216009,#216010),(#216011,#216012),(#216013,#216014),(#216015,#216016),
(#216017,#216018),(#216019,#216020),(#216021,#216022),(#216023,#216024),
(#216025,#216026),(#216027,#216028),(#216029,#216030),(#216031,#216032),
(#216033,#216034),(#216035,#216036),(#216037,#216038),(#216039,#216040),
(#216041,#216042),(#216043,#216044),(#216045,#216046),(#216047,#216048),
(#216049,#216050),(#216051,#216052),(#216053,#216054),(#216055,#216056),
(#216057,#216058),(#216059,#216060),(#216061,#216062),(#216063,#216064),
(#216065,#216066),(#216067,#216068),(#216069,#216070),(#216071,#216072),
(#216073,#216074),(#216075,#216076),(#216077,#216078),(#216079,#216080),
(#216081,#216082),(#216083,#216084),(#216085,#216086),(#216087,#216088),
(#216089,#216090),(#216091,#216092),(#216093,#216094),(#216095,#216096),
(#216097,#216098),(#216099,#216100),(#216101,#216102),(#216103,#216104),
(#216105,#216106),(#216107,#216108),(#216109,#216110),(#216111,#216112),
(#216113,#216114),(#216115,#216116),(#216117,#216118),(#216119,#216120),
(#216121,#216122),(#216123,#216124),(#216125,#216126),(#216127,#216128),
(#216129,#216130),(#216131,#216132),(#216133,#216134),(#216135,#216136),
(#216137,#216138),(#216139,#216140),(#216141,#216142),(#216143,#216144),
(#216145,#216146),(#216147,#216148),(#216149,#216150),(#216151,#216152),
(#216153,#216154),(#216155,#216156),(#216157,#216158),(#216159,#216160),
(#216161,#216162),(#216163,#216164),(#216165,#216166),(#216167,#216168),
(#216169,#216170),(#216171,#216172),(#216173,#216174),(#216175,#216176),
(#216177,#216178),(#216179,#216180),(#216181,#216182),(#216183,#216184),
(#216185,#216186),(#216187,#216188),(#216189,#216190),(#216191,#216192),
(#216193,#216194),(#216195,#216196),(#216197,#216198),(#216199,#216200),
(#216201,#216202),(#216203,#216204),(#216205,#216206),(#216207,#216208),
(#216209,#216210),(#216211,#216212),(#216213,#216214),(#216215,#216216),
(#216217,#216218),(#216219,#216220),(#216221,#216222),(#216223,#216224),
(#216225,#216226),(#216227,#216228),(#216229,#216230),(#216231,#216232),
(#216233,#216234),(#216235,#216236),(#216237,#216238),(#216239,#216240),
(#216241,#216242),(#216243,#216244),(#216245,#216246),(#216247,#216248),
(#216249,#216250),(#216251,#216252),(#216253,#216254),(#216255,#216256),
(#216257,#216258),(#216259,#216260),(#216261,#216262),(#216263,#216264),
(#216265,#216266),(#216267,#216268),(#216269,#216270),(#216271,#216272),
(#216273,#216274),(#216275,#216276),(#216277,#216278),(#216279,#216280),
(#216281,#216282),(#216283,#216284),(#216285,#216286),(#216287,#216288),
(#216289,#216290),(#216291,#216292),(#216293,#216294),(#216295,#216296),
(#216297,#216298),(#216299,#216300),(#216301,#216302),(#216303,#216304),
(#216305,#216306),(#216307,#216308)),.UNSPECIFIED.,.F.,.F.,.F.,(6,1,1,1,
1,1,1,1,1,1,1,1,1,1,1,1,1,1,1,1,1,1,1,1,1,1,1,1,1,1,1,1,1,1,1,1,1,1,1,1,
1,1,1,1,1,1,1,1,1,1,1,1,1,1,1,1,1,1,1,1,1,1,1,1,1,1,1,1,1,1,1,1,1,1,1,1,
1,1,1,1,1,1,1,1,1,1,1,1,1,1,1,1,1,1,1,1,1,1,1,1,1,1,1,1,1,1,1,1,1,1,1,1,
1,1,1,1,1,1,1,1,1,1,1,1,1,1,1,1,1,1,1,1,1,1,1,1,1,1,1,1,1,1,1,1,1,1,1,1,
1,1,1,1,1,1,1,1,1,1,1,1,1,1,1,1,1,1,1,1,1,1,1,1,1,1,1,1,1,1,1,1,1,1,1,1,
1,1,1,1,1,1,1,1,1,1,1,1,1,1,1,1,1,1,1,1,1,1,1,1,1,1,1,1,1,1,1,1,1,1,1,1,
1,1,1,1,1,1,1,1,1,1,1,1,1,1,1,1,1,1,1,1,1,1,1,1,1,1,1,1,1,1,1,1,1,1,1,1,
1,1,1,1,1,1,1,1,1,1,1,1,1,1,1,1,1,1,1,1,1,1,1,1,1,1,1,1,1,1,1,1,1,1,1,1,
1,1,1,1,1,1,1,1,1,1,1,1,1,1,1,1,1,1,1,1,1,1,1,1,1,1,1,1,1,1,1,1,1,1,1,1,
1,1,1,1,1,1,1,1,1,1,1,1,1,1,1,1,1,1,1,1,1,1,1,1,1,1,1,1,1,1,1,1,1,1,1,1,
1,1,1,1,1,1,1,1,1,1,1,1,1,1,1,1,1,1,1,1,1,1,1,1,1,1,1,1,1,1,1,1,1,1,1,1,
1,1,1,1,1,1,1,1,1,1,1,1,1,1,1,1,1,1,1,1,1,1,1,1,1,1,1,1,1,1,1,1,1,1,1,1,
1,1,1,1,1,1,1,1,1,1,1,1,1,1,1,1,1,1,1,1,1,1,1,1,1,1,1,1,1,1,1,6),(2,2),
(-1.,-0.998165138,-0.996330275,-0.994495413,-0.99266055,-0.990825688,-0.988990826,
-0.987155963,-0.985321101,-0.983486239,-0.981651376,-0.979816514,-0.977981651,
-0.976146789,-0.974311927,-0.972477064,-0.970642202,-0.968807339,-0.966972477,
-0.965137615,-0.963302752,-0.96146789,-0.959633028,-0.957798165,-0.955963303,
-0.95412844,-0.952293578,-0.950458716,-0.948623853,-0.946788991,-0.944954128,
-0.943119266,-0.941284404,-0.939449541,-0.937614679,-0.935779817,-0.933944954,
-0.932110092,-0.930275229,-0.928440367,-0.926605505,-0.924770642,-0.92293578,
-0.921100917,-0.919266055,-0.917431193,-0.91559633,-0.913761468,-0.911926606,
-0.910091743,-0.908256881,-0.906422018,-0.904587156,-0.902752294,-0.900917431,
-0.899082569,-0.897247706,-0.895412844,-0.893577982,-0.891743119,-0.889908257,
-0.888073394,-0.886238532,-0.88440367,-0.882568807,-0.880733945,-0.878899083,
-0.87706422,-0.875229358,-0.873394495,-0.871559633,-0.869724771,-0.867889908,
-0.866055046,-0.864220183,-0.862385321,-0.860550459,-0.858715596,-0.856880734,
-0.855045872,-0.853211009,-0.851376147,-0.849541284,-0.847706422,-0.84587156,
-0.844036697,-0.842201835,-0.840366972,-0.83853211,-0.836697248,-0.834862385,
-0.833027523,-0.831192661,-0.829357798,-0.827522936,-0.825688073,-0.823853211,
-0.822018349,-0.820183486,-0.818348624,-0.816513761,-0.814678899,-0.812844037,
-0.811009174,-0.809174312,-0.80733945,-0.805504587,-0.803669725,-0.801834862,
-0.8,-0.798165138,-0.796330275,-0.794495413,-0.79266055,-0.790825688,-0.788990826,
-0.787155963,-0.785321101,-0.783486239,-0.781651376,-0.779816514,-0.777981651,
-0.776146789,-0.774311927,-0.772477064,-0.770642202,-0.768807339,-0.766972477,
-0.765137615,-0.763302752,-0.76146789,-0.759633028,-0.757798165,-0.755963303,
-0.75412844,-0.752293578,-0.750458716,-0.748623853,-0.746788991,-0.744954128,
-0.743119266,-0.741284404,-0.739449541,-0.737614679,-0.735779817,-0.733944954,
-0.732110092,-0.730275229,-0.728440367,-0.726605505,-0.724770642,-0.72293578,
-0.721100917,-0.719266055,-0.717431193,-0.71559633,-0.713761468,-0.711926606,
-0.710091743,-0.708256881,-0.706422018,-0.704587156,-0.702752294,-0.700917431,
-0.699082569,-0.697247706,-0.695412844,-0.693577982,-0.691743119,-0.689908257,
-0.688073394,-0.686238532,-0.68440367,-0.682568807,-0.680733945,-0.678899083,
-0.67706422,-0.675229358,-0.673394495,-0.671559633,-0.669724771,-0.667889908,
-0.666055046,-0.664220183,-0.662385321,-0.660550459,-0.658715596,-0.656880734,
-0.655045872,-0.653211009,-0.651376147,-0.649541284,-0.647706422,-0.64587156,
-0.644036697,-0.642201835,-0.640366972,-0.63853211,-0.636697248,-0.634862385,
-0.633027523,-0.631192661,-0.629357798,-0.627522936,-0.625688073,-0.623853211,
-0.622018349,-0.620183486,-0.618348624,-0.616513761,-0.614678899,-0.612844037,
-0.611009174,-0.609174312,-0.60733945,-0.605504587,-0.603669725,-0.601834862,
-0.6,-0.598165138,-0.596330275,-0.594495413,-0.59266055,-0.590825688,-0.588990826,
-0.587155963,-0.585321101,-0.583486239,-0.581651376,-0.579816514,-0.577981651,
-0.576146789,-0.574311927,-0.572477064,-0.570642202,-0.568807339,-0.566972477,
-0.565137615,-0.563302752,-0.56146789,-0.559633028,-0.557798165,-0.555963303,
-0.55412844,-0.552293578,-0.550458716,-0.548623853,-0.546788991,-0.544954128,
-0.543119266,-0.541284404,-0.539449541,-0.537614679,-0.535779817,-0.533944954,
-0.532110092,-0.530275229,-0.528440367,-0.526605505,-0.524770642,-0.52293578,
-0.521100917,-0.519266055,-0.517431193,-0.51559633,-0.513761468,-0.511926606,
-0.510091743,-0.508256881,-0.506422018,-0.504587156,-0.502752294,-0.500917431,
-0.499082569,-0.497247706,-0.495412844,-0.493577982,-0.491743119,-0.489908257,
-0.488073394,-0.486238532,-0.48440367,-0.482568807,-0.480733945,-0.478899083,
-0.47706422,-0.475229358,-0.473394495,-0.471559633,-0.469724771,-0.467889908,
-0.466055046,-0.464220183,-0.462385321,-0.460550459,-0.458715596,-0.456880734,
-0.455045872,-0.453211009,-0.451376147,-0.449541284,-0.447706422,-0.44587156,
-0.444036697,-0.442201835,-0.440366972,-0.43853211,-0.436697248,-0.434862385,
-0.433027523,-0.431192661,-0.429357798,-0.427522936,-0.425688073,-0.423853211,
-0.422018349,-0.420183486,-0.418348624,-0.416513761,-0.414678899,-0.412844037,
-0.411009174,-0.409174312,-0.40733945,-0.405504587,-0.403669725,-0.401834862,
-0.4,-0.398165138,-0.396330275,-0.394495413,-0.39266055,-0.390825688,-0.388990826,
-0.387155963,-0.385321101,-0.383486239,-0.381651376,-0.379816514,-0.377981651,
-0.376146789,-0.374311927,-0.372477064,-0.370642202,-0.368807339,-0.366972477,
-0.365137615,-0.363302752,-0.36146789,-0.359633028,-0.357798165,-0.355963303,
-0.35412844,-0.352293578,-0.350458716,-0.348623853,-0.346788991,-0.344954128,
-0.343119266,-0.341284404,-0.339449541,-0.337614679,-0.335779817,-0.333944954,
-0.332110092,-0.330275229,-0.328440367,-0.326605505,-0.324770642,-0.32293578,
-0.321100917,-0.319266055,-0.317431193,-0.31559633,-0.313761468,-0.311926606,
-0.310091743,-0.308256881,-0.306422018,-0.304587156,-0.302752294,-0.300917431,
-0.299082569,-0.297247706,-0.295412844,-0.293577982,-0.291743119,-0.289908257,
-0.288073394,-0.286238532,-0.28440367,-0.282568807,-0.280733945,-0.278899083,
-0.27706422,-0.275229358,-0.273394495,-0.271559633,-0.269724771,-0.267889908,
-0.266055046,-0.264220183,-0.262385321,-0.260550459,-0.258715596,-0.256880734,
-0.255045872,-0.253211009,-0.251376147,-0.249541284,-0.247706422,-0.24587156,
-0.244036697,-0.242201835,-0.240366972,-0.23853211,-0.236697248,-0.234862385,
-0.233027523,-0.231192661,-0.229357798,-0.227522936,-0.225688073,-0.223853211,
-0.222018349,-0.220183486,-0.218348624,-0.216513761,-0.214678899,-0.212844037,
-0.211009174,-0.209174312,-0.20733945,-0.205504587,-0.203669725,-0.201834862,
-0.2,-0.198165138,-0.196330275,-0.194495413,-0.19266055,-0.190825688,-0.188990826,
-0.187155963,-0.185321101,-0.183486239,-0.181651376,-0.179816514,-0.177981651,
-0.176146789,-0.174311927,-0.172477064,-0.170642202,-0.168807339,-0.166972477,
-0.165137615,-0.163302752,-0.16146789,-0.159633028,-0.157798165,-0.155963303,
-0.15412844,-0.152293578,-0.150458716,-0.148623853,-0.146788991,-0.144954128,
-0.143172104),(0.,0.36),.UNSPECIFIED.);
#6253=B_SPLINE_SURFACE_WITH_KNOTS('',5,1,((#216956,#216957),(#216958,#216959),
(#216960,#216961),(#216962,#216963),(#216964,#216965),(#216966,#216967),
(#216968,#216969),(#216970,#216971),(#216972,#216973),(#216974,#216975),
(#216976,#216977),(#216978,#216979),(#216980,#216981),(#216982,#216983),
(#216984,#216985),(#216986,#216987),(#216988,#216989),(#216990,#216991),
(#216992,#216993),(#216994,#216995),(#216996,#216997),(#216998,#216999),
(#217000,#217001),(#217002,#217003),(#217004,#217005),(#217006,#217007),
(#217008,#217009),(#217010,#217011),(#217012,#217013),(#217014,#217015),
(#217016,#217017),(#217018,#217019),(#217020,#217021),(#217022,#217023),
(#217024,#217025),(#217026,#217027),(#217028,#217029),(#217030,#217031),
(#217032,#217033),(#217034,#217035),(#217036,#217037),(#217038,#217039),
(#217040,#217041),(#217042,#217043),(#217044,#217045),(#217046,#217047),
(#217048,#217049),(#217050,#217051),(#217052,#217053),(#217054,#217055),
(#217056,#217057),(#217058,#217059),(#217060,#217061),(#217062,#217063),
(#217064,#217065),(#217066,#217067),(#217068,#217069),(#217070,#217071),
(#217072,#217073),(#217074,#217075),(#217076,#217077),(#217078,#217079),
(#217080,#217081),(#217082,#217083),(#217084,#217085),(#217086,#217087),
(#217088,#217089),(#217090,#217091),(#217092,#217093),(#217094,#217095),
(#217096,#217097),(#217098,#217099),(#217100,#217101),(#217102,#217103),
(#217104,#217105),(#217106,#217107),(#217108,#217109),(#217110,#217111),
(#217112,#217113),(#217114,#217115),(#217116,#217117),(#217118,#217119),
(#217120,#217121),(#217122,#217123),(#217124,#217125),(#217126,#217127),
(#217128,#217129),(#217130,#217131),(#217132,#217133),(#217134,#217135),
(#217136,#217137),(#217138,#217139),(#217140,#217141),(#217142,#217143),
(#217144,#217145),(#217146,#217147),(#217148,#217149),(#217150,#217151),
(#217152,#217153),(#217154,#217155),(#217156,#217157),(#217158,#217159),
(#217160,#217161),(#217162,#217163),(#217164,#217165),(#217166,#217167),
(#217168,#217169),(#217170,#217171),(#217172,#217173),(#217174,#217175),
(#217176,#217177),(#217178,#217179),(#217180,#217181),(#217182,#217183),
(#217184,#217185),(#217186,#217187),(#217188,#217189),(#217190,#217191),
(#217192,#217193),(#217194,#217195),(#217196,#217197),(#217198,#217199),
(#217200,#217201),(#217202,#217203),(#217204,#217205),(#217206,#217207),
(#217208,#217209),(#217210,#217211),(#217212,#217213),(#217214,#217215),
(#217216,#217217),(#217218,#217219),(#217220,#217221),(#217222,#217223),
(#217224,#217225),(#217226,#217227),(#217228,#217229),(#217230,#217231),
(#217232,#217233),(#217234,#217235),(#217236,#217237),(#217238,#217239),
(#217240,#217241),(#217242,#217243),(#217244,#217245),(#217246,#217247),
(#217248,#217249),(#217250,#217251),(#217252,#217253),(#217254,#217255),
(#217256,#217257),(#217258,#217259),(#217260,#217261),(#217262,#217263),
(#217264,#217265),(#217266,#217267),(#217268,#217269),(#217270,#217271),
(#217272,#217273),(#217274,#217275),(#217276,#217277),(#217278,#217279),
(#217280,#217281),(#217282,#217283),(#217284,#217285),(#217286,#217287),
(#217288,#217289),(#217290,#217291),(#217292,#217293),(#217294,#217295),
(#217296,#217297),(#217298,#217299),(#217300,#217301),(#217302,#217303),
(#217304,#217305),(#217306,#217307),(#217308,#217309),(#217310,#217311),
(#217312,#217313),(#217314,#217315),(#217316,#217317),(#217318,#217319),
(#217320,#217321),(#217322,#217323),(#217324,#217325),(#217326,#217327),
(#217328,#217329),(#217330,#217331),(#217332,#217333),(#217334,#217335),
(#217336,#217337),(#217338,#217339),(#217340,#217341),(#217342,#217343),
(#217344,#217345),(#217346,#217347),(#217348,#217349),(#217350,#217351),
(#217352,#217353),(#217354,#217355),(#217356,#217357),(#217358,#217359),
(#217360,#217361),(#217362,#217363),(#217364,#217365),(#217366,#217367),
(#217368,#217369),(#217370,#217371),(#217372,#217373),(#217374,#217375),
(#217376,#217377),(#217378,#217379),(#217380,#217381),(#217382,#217383),
(#217384,#217385),(#217386,#217387),(#217388,#217389),(#217390,#217391),
(#217392,#217393),(#217394,#217395),(#217396,#217397),(#217398,#217399),
(#217400,#217401),(#217402,#217403),(#217404,#217405),(#217406,#217407),
(#217408,#217409),(#217410,#217411),(#217412,#217413),(#217414,#217415),
(#217416,#217417),(#217418,#217419),(#217420,#217421),(#217422,#217423),
(#217424,#217425),(#217426,#217427),(#217428,#217429),(#217430,#217431),
(#217432,#217433),(#217434,#217435),(#217436,#217437),(#217438,#217439),
(#217440,#217441),(#217442,#217443),(#217444,#217445),(#217446,#217447),
(#217448,#217449),(#217450,#217451),(#217452,#217453),(#217454,#217455),
(#217456,#217457),(#217458,#217459),(#217460,#217461),(#217462,#217463),
(#217464,#217465),(#217466,#217467),(#217468,#217469),(#217470,#217471),
(#217472,#217473),(#217474,#217475),(#217476,#217477),(#217478,#217479),
(#217480,#217481),(#217482,#217483),(#217484,#217485),(#217486,#217487),
(#217488,#217489),(#217490,#217491),(#217492,#217493),(#217494,#217495),
(#217496,#217497),(#217498,#217499),(#217500,#217501),(#217502,#217503),
(#217504,#217505),(#217506,#217507),(#217508,#217509),(#217510,#217511),
(#217512,#217513),(#217514,#217515),(#217516,#217517),(#217518,#217519),
(#217520,#217521),(#217522,#217523),(#217524,#217525),(#217526,#217527),
(#217528,#217529),(#217530,#217531),(#217532,#217533),(#217534,#217535),
(#217536,#217537),(#217538,#217539),(#217540,#217541),(#217542,#217543),
(#217544,#217545),(#217546,#217547),(#217548,#217549),(#217550,#217551),
(#217552,#217553),(#217554,#217555),(#217556,#217557),(#217558,#217559),
(#217560,#217561),(#217562,#217563),(#217564,#217565),(#217566,#217567),
(#217568,#217569),(#217570,#217571),(#217572,#217573),(#217574,#217575),
(#217576,#217577),(#217578,#217579),(#217580,#217581),(#217582,#217583),
(#217584,#217585),(#217586,#217587),(#217588,#217589),(#217590,#217591),
(#217592,#217593),(#217594,#217595),(#217596,#217597),(#217598,#217599),
(#217600,#217601),(#217602,#217603),(#217604,#217605),(#217606,#217607),
(#217608,#217609),(#217610,#217611),(#217612,#217613),(#217614,#217615),
(#217616,#217617),(#217618,#217619),(#217620,#217621),(#217622,#217623),
(#217624,#217625),(#217626,#217627),(#217628,#217629),(#217630,#217631),
(#217632,#217633),(#217634,#217635),(#217636,#217637),(#217638,#217639),
(#217640,#217641),(#217642,#217643),(#217644,#217645),(#217646,#217647),
(#217648,#217649),(#217650,#217651),(#217652,#217653),(#217654,#217655),
(#217656,#217657),(#217658,#217659),(#217660,#217661),(#217662,#217663),
(#217664,#217665),(#217666,#217667),(#217668,#217669),(#217670,#217671),
(#217672,#217673),(#217674,#217675),(#217676,#217677),(#217678,#217679),
(#217680,#217681),(#217682,#217683),(#217684,#217685),(#217686,#217687),
(#217688,#217689),(#217690,#217691),(#217692,#217693),(#217694,#217695),
(#217696,#217697),(#217698,#217699),(#217700,#217701),(#217702,#217703),
(#217704,#217705),(#217706,#217707),(#217708,#217709),(#217710,#217711),
(#217712,#217713),(#217714,#217715),(#217716,#217717),(#217718,#217719),
(#217720,#217721),(#217722,#217723),(#217724,#217725),(#217726,#217727),
(#217728,#217729),(#217730,#217731),(#217732,#217733),(#217734,#217735),
(#217736,#217737),(#217738,#217739),(#217740,#217741),(#217742,#217743),
(#217744,#217745),(#217746,#217747),(#217748,#217749),(#217750,#217751),
(#217752,#217753),(#217754,#217755),(#217756,#217757),(#217758,#217759),
(#217760,#217761),(#217762,#217763),(#217764,#217765),(#217766,#217767),
(#217768,#217769),(#217770,#217771),(#217772,#217773),(#217774,#217775),
(#217776,#217777),(#217778,#217779),(#217780,#217781),(#217782,#217783),
(#217784,#217785),(#217786,#217787),(#217788,#217789),(#217790,#217791),
(#217792,#217793),(#217794,#217795),(#217796,#217797),(#217798,#217799),
(#217800,#217801),(#217802,#217803),(#217804,#217805),(#217806,#217807),
(#217808,#217809),(#217810,#217811),(#217812,#217813),(#217814,#217815),
(#217816,#217817),(#217818,#217819),(#217820,#217821),(#217822,#217823),
(#217824,#217825),(#217826,#217827),(#217828,#217829),(#217830,#217831),
(#217832,#217833),(#217834,#217835),(#217836,#217837),(#217838,#217839),
(#217840,#217841),(#217842,#217843),(#217844,#217845),(#217846,#217847),
(#217848,#217849),(#217850,#217851),(#217852,#217853),(#217854,#217855),
(#217856,#217857),(#217858,#217859),(#217860,#217861),(#217862,#217863),
(#217864,#217865),(#217866,#217867),(#217868,#217869),(#217870,#217871),
(#217872,#217873),(#217874,#217875),(#217876,#217877),(#217878,#217879),
(#217880,#217881),(#217882,#217883),(#217884,#217885),(#217886,#217887),
(#217888,#217889),(#217890,#217891),(#217892,#217893),(#217894,#217895),
(#217896,#217897),(#217898,#217899)),.UNSPECIFIED.,.F.,.F.,.F.,(6,1,1,1,
1,1,1,1,1,1,1,1,1,1,1,1,1,1,1,1,1,1,1,1,1,1,1,1,1,1,1,1,1,1,1,1,1,1,1,1,
1,1,1,1,1,1,1,1,1,1,1,1,1,1,1,1,1,1,1,1,1,1,1,1,1,1,1,1,1,1,1,1,1,1,1,1,
1,1,1,1,1,1,1,1,1,1,1,1,1,1,1,1,1,1,1,1,1,1,1,1,1,1,1,1,1,1,1,1,1,1,1,1,
1,1,1,1,1,1,1,1,1,1,1,1,1,1,1,1,1,1,1,1,1,1,1,1,1,1,1,1,1,1,1,1,1,1,1,1,
1,1,1,1,1,1,1,1,1,1,1,1,1,1,1,1,1,1,1,1,1,1,1,1,1,1,1,1,1,1,1,1,1,1,1,1,
1,1,1,1,1,1,1,1,1,1,1,1,1,1,1,1,1,1,1,1,1,1,1,1,1,1,1,1,1,1,1,1,1,1,1,1,
1,1,1,1,1,1,1,1,1,1,1,1,1,1,1,1,1,1,1,1,1,1,1,1,1,1,1,1,1,1,1,1,1,1,1,1,
1,1,1,1,1,1,1,1,1,1,1,1,1,1,1,1,1,1,1,1,1,1,1,1,1,1,1,1,1,1,1,1,1,1,1,1,
1,1,1,1,1,1,1,1,1,1,1,1,1,1,1,1,1,1,1,1,1,1,1,1,1,1,1,1,1,1,1,1,1,1,1,1,
1,1,1,1,1,1,1,1,1,1,1,1,1,1,1,1,1,1,1,1,1,1,1,1,1,1,1,1,1,1,1,1,1,1,1,1,
1,1,1,1,1,1,1,1,1,1,1,1,1,1,1,1,1,1,1,1,1,1,1,1,1,1,1,1,1,1,1,1,1,1,1,1,
1,1,1,1,1,1,1,1,1,1,1,1,1,1,1,1,1,1,1,1,1,1,1,1,1,1,1,1,1,1,1,1,1,1,1,1,
1,1,1,1,1,1,1,1,1,1,1,1,1,1,1,1,1,1,1,1,1,1,1,1,1,1,1,1,1,1,1,6),(2,2),
(-1.,-0.998165138,-0.996330275,-0.994495413,-0.99266055,-0.990825688,-0.988990826,
-0.987155963,-0.985321101,-0.983486239,-0.981651376,-0.979816514,-0.977981651,
-0.976146789,-0.974311927,-0.972477064,-0.970642202,-0.968807339,-0.966972477,
-0.965137615,-0.963302752,-0.96146789,-0.959633028,-0.957798165,-0.955963303,
-0.95412844,-0.952293578,-0.950458716,-0.948623853,-0.946788991,-0.944954128,
-0.943119266,-0.941284404,-0.939449541,-0.937614679,-0.935779817,-0.933944954,
-0.932110092,-0.930275229,-0.928440367,-0.926605505,-0.924770642,-0.92293578,
-0.921100917,-0.919266055,-0.917431193,-0.91559633,-0.913761468,-0.911926606,
-0.910091743,-0.908256881,-0.906422018,-0.904587156,-0.902752294,-0.900917431,
-0.899082569,-0.897247706,-0.895412844,-0.893577982,-0.891743119,-0.889908257,
-0.888073394,-0.886238532,-0.88440367,-0.882568807,-0.880733945,-0.878899083,
-0.87706422,-0.875229358,-0.873394495,-0.871559633,-0.869724771,-0.867889908,
-0.866055046,-0.864220183,-0.862385321,-0.860550459,-0.858715596,-0.856880734,
-0.855045872,-0.853211009,-0.851376147,-0.849541284,-0.847706422,-0.84587156,
-0.844036697,-0.842201835,-0.840366972,-0.83853211,-0.836697248,-0.834862385,
-0.833027523,-0.831192661,-0.829357798,-0.827522936,-0.825688073,-0.823853211,
-0.822018349,-0.820183486,-0.818348624,-0.816513761,-0.814678899,-0.812844037,
-0.811009174,-0.809174312,-0.80733945,-0.805504587,-0.803669725,-0.801834862,
-0.8,-0.798165138,-0.796330275,-0.794495413,-0.79266055,-0.790825688,-0.788990826,
-0.787155963,-0.785321101,-0.783486239,-0.781651376,-0.779816514,-0.777981651,
-0.776146789,-0.774311927,-0.772477064,-0.770642202,-0.768807339,-0.766972477,
-0.765137615,-0.763302752,-0.76146789,-0.759633028,-0.757798165,-0.755963303,
-0.75412844,-0.752293578,-0.750458716,-0.748623853,-0.746788991,-0.744954128,
-0.743119266,-0.741284404,-0.739449541,-0.737614679,-0.735779817,-0.733944954,
-0.732110092,-0.730275229,-0.728440367,-0.726605505,-0.724770642,-0.72293578,
-0.721100917,-0.719266055,-0.717431193,-0.71559633,-0.713761468,-0.711926606,
-0.710091743,-0.708256881,-0.706422018,-0.704587156,-0.702752294,-0.700917431,
-0.699082569,-0.697247706,-0.695412844,-0.693577982,-0.691743119,-0.689908257,
-0.688073394,-0.686238532,-0.68440367,-0.682568807,-0.680733945,-0.678899083,
-0.67706422,-0.675229358,-0.673394495,-0.671559633,-0.669724771,-0.667889908,
-0.666055046,-0.664220183,-0.662385321,-0.660550459,-0.658715596,-0.656880734,
-0.655045872,-0.653211009,-0.651376147,-0.649541284,-0.647706422,-0.64587156,
-0.644036697,-0.642201835,-0.640366972,-0.63853211,-0.636697248,-0.634862385,
-0.633027523,-0.631192661,-0.629357798,-0.627522936,-0.625688073,-0.623853211,
-0.622018349,-0.620183486,-0.618348624,-0.616513761,-0.614678899,-0.612844037,
-0.611009174,-0.609174312,-0.60733945,-0.605504587,-0.603669725,-0.601834862,
-0.6,-0.598165138,-0.596330275,-0.594495413,-0.59266055,-0.590825688,-0.588990826,
-0.587155963,-0.585321101,-0.583486239,-0.581651376,-0.579816514,-0.577981651,
-0.576146789,-0.574311927,-0.572477064,-0.570642202,-0.568807339,-0.566972477,
-0.565137615,-0.563302752,-0.56146789,-0.559633028,-0.557798165,-0.555963303,
-0.55412844,-0.552293578,-0.550458716,-0.548623853,-0.546788991,-0.544954128,
-0.543119266,-0.541284404,-0.539449541,-0.537614679,-0.535779817,-0.533944954,
-0.532110092,-0.530275229,-0.528440367,-0.526605505,-0.524770642,-0.52293578,
-0.521100917,-0.519266055,-0.517431193,-0.51559633,-0.513761468,-0.511926606,
-0.510091743,-0.508256881,-0.506422018,-0.504587156,-0.502752294,-0.500917431,
-0.499082569,-0.497247706,-0.495412844,-0.493577982,-0.491743119,-0.489908257,
-0.488073394,-0.486238532,-0.48440367,-0.482568807,-0.480733945,-0.478899083,
-0.47706422,-0.475229358,-0.473394495,-0.471559633,-0.469724771,-0.467889908,
-0.466055046,-0.464220183,-0.462385321,-0.460550459,-0.458715596,-0.456880734,
-0.455045872,-0.453211009,-0.451376147,-0.449541284,-0.447706422,-0.44587156,
-0.444036697,-0.442201835,-0.440366972,-0.43853211,-0.436697248,-0.434862385,
-0.433027523,-0.431192661,-0.429357798,-0.427522936,-0.425688073,-0.423853211,
-0.422018349,-0.420183486,-0.418348624,-0.416513761,-0.414678899,-0.412844037,
-0.411009174,-0.409174312,-0.40733945,-0.405504587,-0.403669725,-0.401834862,
-0.4,-0.398165138,-0.396330275,-0.394495413,-0.39266055,-0.390825688,-0.388990826,
-0.387155963,-0.385321101,-0.383486239,-0.381651376,-0.379816514,-0.377981651,
-0.376146789,-0.374311927,-0.372477064,-0.370642202,-0.368807339,-0.366972477,
-0.365137615,-0.363302752,-0.36146789,-0.359633028,-0.357798165,-0.355963303,
-0.35412844,-0.352293578,-0.350458716,-0.348623853,-0.346788991,-0.344954128,
-0.343119266,-0.341284404,-0.339449541,-0.337614679,-0.335779817,-0.333944954,
-0.332110092,-0.330275229,-0.328440367,-0.326605505,-0.324770642,-0.32293578,
-0.321100917,-0.319266055,-0.317431193,-0.31559633,-0.313761468,-0.311926606,
-0.310091743,-0.308256881,-0.306422018,-0.304587156,-0.302752294,-0.300917431,
-0.299082569,-0.297247706,-0.295412844,-0.293577982,-0.291743119,-0.289908257,
-0.288073394,-0.286238532,-0.28440367,-0.282568807,-0.280733945,-0.278899083,
-0.27706422,-0.275229358,-0.273394495,-0.271559633,-0.269724771,-0.267889908,
-0.266055046,-0.264220183,-0.262385321,-0.260550459,-0.258715596,-0.256880734,
-0.255045872,-0.253211009,-0.251376147,-0.249541284,-0.247706422,-0.24587156,
-0.244036697,-0.242201835,-0.240366972,-0.23853211,-0.236697248,-0.234862385,
-0.233027523,-0.231192661,-0.229357798,-0.227522936,-0.225688073,-0.223853211,
-0.222018349,-0.220183486,-0.218348624,-0.216513761,-0.214678899,-0.212844037,
-0.211009174,-0.209174312,-0.20733945,-0.205504587,-0.203669725,-0.201834862,
-0.2,-0.198165138,-0.196330275,-0.194495413,-0.19266055,-0.190825688,-0.188990826,
-0.187155963,-0.185321101,-0.183486239,-0.181651376,-0.179816514,-0.177981651,
-0.176146789,-0.174311927,-0.172477064,-0.170642202,-0.168807339,-0.166972477,
-0.165137615,-0.163302752,-0.16146789,-0.159633028,-0.157798165,-0.155963303,
-0.15412844,-0.152293578,-0.150458716,-0.148623853,-0.146788991,-0.144954128,
-0.143172103),(0.,0.36),.UNSPECIFIED.);
#6254=B_SPLINE_SURFACE_WITH_KNOTS('',5,1,((#218845,#218846),(#218847,#218848),
(#218849,#218850),(#218851,#218852),(#218853,#218854),(#218855,#218856),
(#218857,#218858),(#218859,#218860),(#218861,#218862),(#218863,#218864),
(#218865,#218866),(#218867,#218868),(#218869,#218870),(#218871,#218872),
(#218873,#218874),(#218875,#218876),(#218877,#218878),(#218879,#218880),
(#218881,#218882),(#218883,#218884),(#218885,#218886),(#218887,#218888),
(#218889,#218890),(#218891,#218892),(#218893,#218894),(#218895,#218896),
(#218897,#218898),(#218899,#218900),(#218901,#218902),(#218903,#218904),
(#218905,#218906),(#218907,#218908),(#218909,#218910),(#218911,#218912),
(#218913,#218914),(#218915,#218916),(#218917,#218918),(#218919,#218920),
(#218921,#218922),(#218923,#218924),(#218925,#218926),(#218927,#218928),
(#218929,#218930),(#218931,#218932),(#218933,#218934),(#218935,#218936),
(#218937,#218938),(#218939,#218940),(#218941,#218942),(#218943,#218944),
(#218945,#218946),(#218947,#218948),(#218949,#218950),(#218951,#218952),
(#218953,#218954),(#218955,#218956),(#218957,#218958),(#218959,#218960),
(#218961,#218962),(#218963,#218964),(#218965,#218966),(#218967,#218968),
(#218969,#218970),(#218971,#218972),(#218973,#218974),(#218975,#218976),
(#218977,#218978),(#218979,#218980),(#218981,#218982),(#218983,#218984),
(#218985,#218986),(#218987,#218988),(#218989,#218990),(#218991,#218992),
(#218993,#218994),(#218995,#218996),(#218997,#218998),(#218999,#219000),
(#219001,#219002),(#219003,#219004),(#219005,#219006),(#219007,#219008),
(#219009,#219010),(#219011,#219012),(#219013,#219014),(#219015,#219016),
(#219017,#219018),(#219019,#219020),(#219021,#219022),(#219023,#219024),
(#219025,#219026),(#219027,#219028),(#219029,#219030),(#219031,#219032),
(#219033,#219034),(#219035,#219036),(#219037,#219038),(#219039,#219040),
(#219041,#219042),(#219043,#219044),(#219045,#219046),(#219047,#219048),
(#219049,#219050),(#219051,#219052),(#219053,#219054),(#219055,#219056),
(#219057,#219058),(#219059,#219060),(#219061,#219062),(#219063,#219064),
(#219065,#219066),(#219067,#219068),(#219069,#219070),(#219071,#219072),
(#219073,#219074),(#219075,#219076),(#219077,#219078),(#219079,#219080),
(#219081,#219082),(#219083,#219084),(#219085,#219086),(#219087,#219088),
(#219089,#219090),(#219091,#219092),(#219093,#219094),(#219095,#219096),
(#219097,#219098),(#219099,#219100),(#219101,#219102),(#219103,#219104),
(#219105,#219106),(#219107,#219108),(#219109,#219110),(#219111,#219112),
(#219113,#219114),(#219115,#219116),(#219117,#219118),(#219119,#219120),
(#219121,#219122),(#219123,#219124),(#219125,#219126),(#219127,#219128),
(#219129,#219130),(#219131,#219132),(#219133,#219134),(#219135,#219136),
(#219137,#219138),(#219139,#219140),(#219141,#219142),(#219143,#219144),
(#219145,#219146),(#219147,#219148),(#219149,#219150),(#219151,#219152),
(#219153,#219154),(#219155,#219156),(#219157,#219158),(#219159,#219160),
(#219161,#219162),(#219163,#219164),(#219165,#219166),(#219167,#219168),
(#219169,#219170),(#219171,#219172),(#219173,#219174),(#219175,#219176),
(#219177,#219178),(#219179,#219180),(#219181,#219182),(#219183,#219184),
(#219185,#219186),(#219187,#219188),(#219189,#219190),(#219191,#219192),
(#219193,#219194),(#219195,#219196),(#219197,#219198),(#219199,#219200),
(#219201,#219202),(#219203,#219204),(#219205,#219206),(#219207,#219208),
(#219209,#219210),(#219211,#219212),(#219213,#219214),(#219215,#219216),
(#219217,#219218),(#219219,#219220),(#219221,#219222),(#219223,#219224),
(#219225,#219226),(#219227,#219228),(#219229,#219230),(#219231,#219232),
(#219233,#219234),(#219235,#219236),(#219237,#219238),(#219239,#219240),
(#219241,#219242),(#219243,#219244),(#219245,#219246),(#219247,#219248),
(#219249,#219250),(#219251,#219252),(#219253,#219254),(#219255,#219256),
(#219257,#219258),(#219259,#219260),(#219261,#219262),(#219263,#219264),
(#219265,#219266),(#219267,#219268),(#219269,#219270),(#219271,#219272),
(#219273,#219274),(#219275,#219276),(#219277,#219278),(#219279,#219280),
(#219281,#219282),(#219283,#219284),(#219285,#219286),(#219287,#219288),
(#219289,#219290),(#219291,#219292),(#219293,#219294),(#219295,#219296),
(#219297,#219298),(#219299,#219300),(#219301,#219302),(#219303,#219304),
(#219305,#219306),(#219307,#219308),(#219309,#219310),(#219311,#219312),
(#219313,#219314),(#219315,#219316),(#219317,#219318),(#219319,#219320),
(#219321,#219322),(#219323,#219324),(#219325,#219326),(#219327,#219328),
(#219329,#219330),(#219331,#219332),(#219333,#219334),(#219335,#219336),
(#219337,#219338),(#219339,#219340),(#219341,#219342),(#219343,#219344),
(#219345,#219346),(#219347,#219348),(#219349,#219350),(#219351,#219352),
(#219353,#219354),(#219355,#219356),(#219357,#219358),(#219359,#219360),
(#219361,#219362),(#219363,#219364),(#219365,#219366),(#219367,#219368),
(#219369,#219370),(#219371,#219372),(#219373,#219374),(#219375,#219376),
(#219377,#219378),(#219379,#219380),(#219381,#219382),(#219383,#219384),
(#219385,#219386),(#219387,#219388),(#219389,#219390),(#219391,#219392),
(#219393,#219394),(#219395,#219396),(#219397,#219398),(#219399,#219400),
(#219401,#219402),(#219403,#219404),(#219405,#219406),(#219407,#219408),
(#219409,#219410),(#219411,#219412),(#219413,#219414),(#219415,#219416),
(#219417,#219418),(#219419,#219420),(#219421,#219422),(#219423,#219424),
(#219425,#219426),(#219427,#219428),(#219429,#219430),(#219431,#219432),
(#219433,#219434),(#219435,#219436),(#219437,#219438),(#219439,#219440),
(#219441,#219442),(#219443,#219444),(#219445,#219446),(#219447,#219448),
(#219449,#219450),(#219451,#219452),(#219453,#219454),(#219455,#219456),
(#219457,#219458),(#219459,#219460),(#219461,#219462),(#219463,#219464),
(#219465,#219466),(#219467,#219468),(#219469,#219470),(#219471,#219472),
(#219473,#219474),(#219475,#219476),(#219477,#219478),(#219479,#219480),
(#219481,#219482),(#219483,#219484),(#219485,#219486),(#219487,#219488),
(#219489,#219490),(#219491,#219492),(#219493,#219494),(#219495,#219496),
(#219497,#219498),(#219499,#219500),(#219501,#219502),(#219503,#219504),
(#219505,#219506),(#219507,#219508),(#219509,#219510),(#219511,#219512),
(#219513,#219514),(#219515,#219516),(#219517,#219518),(#219519,#219520),
(#219521,#219522),(#219523,#219524),(#219525,#219526),(#219527,#219528),
(#219529,#219530),(#219531,#219532),(#219533,#219534),(#219535,#219536),
(#219537,#219538),(#219539,#219540),(#219541,#219542),(#219543,#219544),
(#219545,#219546),(#219547,#219548),(#219549,#219550),(#219551,#219552),
(#219553,#219554),(#219555,#219556),(#219557,#219558),(#219559,#219560),
(#219561,#219562),(#219563,#219564),(#219565,#219566),(#219567,#219568),
(#219569,#219570),(#219571,#219572),(#219573,#219574),(#219575,#219576),
(#219577,#219578),(#219579,#219580),(#219581,#219582),(#219583,#219584),
(#219585,#219586),(#219587,#219588),(#219589,#219590),(#219591,#219592),
(#219593,#219594),(#219595,#219596),(#219597,#219598),(#219599,#219600),
(#219601,#219602),(#219603,#219604),(#219605,#219606),(#219607,#219608),
(#219609,#219610),(#219611,#219612),(#219613,#219614),(#219615,#219616),
(#219617,#219618),(#219619,#219620),(#219621,#219622),(#219623,#219624),
(#219625,#219626),(#219627,#219628),(#219629,#219630),(#219631,#219632),
(#219633,#219634),(#219635,#219636),(#219637,#219638),(#219639,#219640),
(#219641,#219642),(#219643,#219644),(#219645,#219646),(#219647,#219648),
(#219649,#219650),(#219651,#219652),(#219653,#219654),(#219655,#219656),
(#219657,#219658),(#219659,#219660),(#219661,#219662),(#219663,#219664),
(#219665,#219666),(#219667,#219668),(#219669,#219670),(#219671,#219672),
(#219673,#219674),(#219675,#219676),(#219677,#219678),(#219679,#219680),
(#219681,#219682),(#219683,#219684),(#219685,#219686),(#219687,#219688),
(#219689,#219690),(#219691,#219692),(#219693,#219694),(#219695,#219696),
(#219697,#219698),(#219699,#219700),(#219701,#219702),(#219703,#219704),
(#219705,#219706),(#219707,#219708),(#219709,#219710),(#219711,#219712),
(#219713,#219714),(#219715,#219716),(#219717,#219718),(#219719,#219720),
(#219721,#219722),(#219723,#219724),(#219725,#219726),(#219727,#219728),
(#219729,#219730),(#219731,#219732),(#219733,#219734),(#219735,#219736),
(#219737,#219738),(#219739,#219740),(#219741,#219742),(#219743,#219744),
(#219745,#219746),(#219747,#219748),(#219749,#219750),(#219751,#219752),
(#219753,#219754),(#219755,#219756),(#219757,#219758),(#219759,#219760),
(#219761,#219762),(#219763,#219764),(#219765,#219766),(#219767,#219768),
(#219769,#219770),(#219771,#219772),(#219773,#219774),(#219775,#219776),
(#219777,#219778),(#219779,#219780),(#219781,#219782),(#219783,#219784),
(#219785,#219786),(#219787,#219788)),.UNSPECIFIED.,.F.,.F.,.F.,(6,1,1,1,
1,1,1,1,1,1,1,1,1,1,1,1,1,1,1,1,1,1,1,1,1,1,1,1,1,1,1,1,1,1,1,1,1,1,1,1,
1,1,1,1,1,1,1,1,1,1,1,1,1,1,1,1,1,1,1,1,1,1,1,1,1,1,1,1,1,1,1,1,1,1,1,1,
1,1,1,1,1,1,1,1,1,1,1,1,1,1,1,1,1,1,1,1,1,1,1,1,1,1,1,1,1,1,1,1,1,1,1,1,
1,1,1,1,1,1,1,1,1,1,1,1,1,1,1,1,1,1,1,1,1,1,1,1,1,1,1,1,1,1,1,1,1,1,1,1,
1,1,1,1,1,1,1,1,1,1,1,1,1,1,1,1,1,1,1,1,1,1,1,1,1,1,1,1,1,1,1,1,1,1,1,1,
1,1,1,1,1,1,1,1,1,1,1,1,1,1,1,1,1,1,1,1,1,1,1,1,1,1,1,1,1,1,1,1,1,1,1,1,
1,1,1,1,1,1,1,1,1,1,1,1,1,1,1,1,1,1,1,1,1,1,1,1,1,1,1,1,1,1,1,1,1,1,1,1,
1,1,1,1,1,1,1,1,1,1,1,1,1,1,1,1,1,1,1,1,1,1,1,1,1,1,1,1,1,1,1,1,1,1,1,1,
1,1,1,1,1,1,1,1,1,1,1,1,1,1,1,1,1,1,1,1,1,1,1,1,1,1,1,1,1,1,1,1,1,1,1,1,
1,1,1,1,1,1,1,1,1,1,1,1,1,1,1,1,1,1,1,1,1,1,1,1,1,1,1,1,1,1,1,1,1,1,1,1,
1,1,1,1,1,1,1,1,1,1,1,1,1,1,1,1,1,1,1,1,1,1,1,1,1,1,1,1,1,1,1,1,1,1,1,1,
1,1,1,1,1,1,1,1,1,1,1,1,1,1,1,1,1,1,1,1,1,1,1,1,1,1,1,1,1,1,1,1,1,1,1,1,
1,1,1,1,1,1,1,1,1,1,1,1,1,1,1,1,1,1,1,1,1,1,1,1,1,1,1,1,1,1,1,6),(2,2),
(0.143172104,0.144954128,0.146788991,0.148623853,0.150458716,0.152293578,
0.15412844,0.155963303,0.157798165,0.159633028,0.16146789,0.163302752,0.165137615,
0.166972477,0.168807339,0.170642202,0.172477064,0.174311927,0.176146789,
0.177981651,0.179816514,0.181651376,0.183486239,0.185321101,0.187155963,
0.188990826,0.190825688,0.19266055,0.194495413,0.196330275,0.198165138,
0.2,0.201834862,0.203669725,0.205504587,0.20733945,0.209174312,0.211009174,
0.212844037,0.214678899,0.216513761,0.218348624,0.220183486,0.222018349,
0.223853211,0.225688073,0.227522936,0.229357798,0.231192661,0.233027523,
0.234862385,0.236697248,0.23853211,0.240366972,0.242201835,0.244036697,
0.24587156,0.247706422,0.249541284,0.251376147,0.253211009,0.255045872,
0.256880734,0.258715596,0.260550459,0.262385321,0.264220183,0.266055046,
0.267889908,0.269724771,0.271559633,0.273394495,0.275229358,0.27706422,
0.278899083,0.280733945,0.282568807,0.28440367,0.286238532,0.288073394,
0.289908257,0.291743119,0.293577982,0.295412844,0.297247706,0.299082569,
0.300917431,0.302752294,0.304587156,0.306422018,0.308256881,0.310091743,
0.311926606,0.313761468,0.31559633,0.317431193,0.319266055,0.321100917,
0.32293578,0.324770642,0.326605505,0.328440367,0.330275229,0.332110092,
0.333944954,0.335779817,0.337614679,0.339449541,0.341284404,0.343119266,
0.344954128,0.346788991,0.348623853,0.350458716,0.352293578,0.35412844,
0.355963303,0.357798165,0.359633028,0.36146789,0.363302752,0.365137615,
0.366972477,0.368807339,0.370642202,0.372477064,0.374311927,0.376146789,
0.377981651,0.379816514,0.381651376,0.383486239,0.385321101,0.387155963,
0.388990826,0.390825688,0.39266055,0.394495413,0.396330275,0.398165138,
0.4,0.401834862,0.403669725,0.405504587,0.40733945,0.409174312,0.411009174,
0.412844037,0.414678899,0.416513761,0.418348624,0.420183486,0.422018349,
0.423853211,0.425688073,0.427522936,0.429357798,0.431192661,0.433027523,
0.434862385,0.436697248,0.43853211,0.440366972,0.442201835,0.444036697,
0.44587156,0.447706422,0.449541284,0.451376147,0.453211009,0.455045872,
0.456880734,0.458715596,0.460550459,0.462385321,0.464220183,0.466055046,
0.467889908,0.469724771,0.471559633,0.473394495,0.475229358,0.47706422,
0.478899083,0.480733945,0.482568807,0.48440367,0.486238532,0.488073394,
0.489908257,0.491743119,0.493577982,0.495412844,0.497247706,0.499082569,
0.500917431,0.502752294,0.504587156,0.506422018,0.508256881,0.510091743,
0.511926606,0.513761468,0.51559633,0.517431193,0.519266055,0.521100917,
0.52293578,0.524770642,0.526605505,0.528440367,0.530275229,0.532110092,
0.533944954,0.535779817,0.537614679,0.539449541,0.541284404,0.543119266,
0.544954128,0.546788991,0.548623853,0.550458716,0.552293578,0.55412844,
0.555963303,0.557798165,0.559633028,0.56146789,0.563302752,0.565137615,
0.566972477,0.568807339,0.570642202,0.572477064,0.574311927,0.576146789,
0.577981651,0.579816514,0.581651376,0.583486239,0.585321101,0.587155963,
0.588990826,0.590825688,0.59266055,0.594495413,0.596330275,0.598165138,
0.6,0.601834862,0.603669725,0.605504587,0.60733945,0.609174312,0.611009174,
0.612844037,0.614678899,0.616513761,0.618348624,0.620183486,0.622018349,
0.623853211,0.625688073,0.627522936,0.629357798,0.631192661,0.633027523,
0.634862385,0.636697248,0.63853211,0.640366972,0.642201835,0.644036697,
0.64587156,0.647706422,0.649541284,0.651376147,0.653211009,0.655045872,
0.656880734,0.658715596,0.660550459,0.662385321,0.664220183,0.666055046,
0.667889908,0.669724771,0.671559633,0.673394495,0.675229358,0.67706422,
0.678899083,0.680733945,0.682568807,0.68440367,0.686238532,0.688073394,
0.689908257,0.691743119,0.693577982,0.695412844,0.697247706,0.699082569,
0.700917431,0.702752294,0.704587156,0.706422018,0.708256881,0.710091743,
0.711926606,0.713761468,0.71559633,0.717431193,0.719266055,0.721100917,
0.72293578,0.724770642,0.726605505,0.728440367,0.730275229,0.732110092,
0.733944954,0.735779817,0.737614679,0.739449541,0.741284404,0.743119266,
0.744954128,0.746788991,0.748623853,0.750458716,0.752293578,0.75412844,
0.755963303,0.757798165,0.759633028,0.76146789,0.763302752,0.765137615,
0.766972477,0.768807339,0.770642202,0.772477064,0.774311927,0.776146789,
0.777981651,0.779816514,0.781651376,0.783486239,0.785321101,0.787155963,
0.788990826,0.790825688,0.79266055,0.794495413,0.796330275,0.798165138,
0.8,0.801834862,0.803669725,0.805504587,0.80733945,0.809174312,0.811009174,
0.812844037,0.814678899,0.816513761,0.818348624,0.820183486,0.822018349,
0.823853211,0.825688073,0.827522936,0.829357798,0.831192661,0.833027523,
0.834862385,0.836697248,0.83853211,0.840366972,0.842201835,0.844036697,
0.84587156,0.847706422,0.849541284,0.851376147,0.853211009,0.855045872,
0.856880734,0.858715596,0.860550459,0.862385321,0.864220183,0.866055046,
0.867889908,0.869724771,0.871559633,0.873394495,0.875229358,0.87706422,
0.878899083,0.880733945,0.882568807,0.88440367,0.886238532,0.888073394,
0.889908257,0.891743119,0.893577982,0.895412844,0.897247706,0.899082569,
0.900917431,0.902752294,0.904587156,0.906422018,0.908256881,0.910091743,
0.911926606,0.913761468,0.91559633,0.917431193,0.919266055,0.921100917,
0.92293578,0.924770642,0.926605505,0.928440367,0.930275229,0.932110092,
0.933944954,0.935779817,0.937614679,0.939449541,0.941284404,0.943119266,
0.944954128,0.946788991,0.948623853,0.950458716,0.952293578,0.95412844,
0.955963303,0.957798165,0.959633028,0.96146789,0.963302752,0.965137615,
0.966972477,0.968807339,0.970642202,0.972477064,0.974311927,0.976146789,
0.977981651,0.979816514,0.981651376,0.983486239,0.985321101,0.987155963,
0.988990826,0.990825688,0.99266055,0.994495413,0.996330275,0.998165138,
1.),(0.,0.36),.UNSPECIFIED.);
#6255=B_SPLINE_SURFACE_WITH_KNOTS('',5,1,((#220421,#220422),(#220423,#220424),
(#220425,#220426),(#220427,#220428),(#220429,#220430),(#220431,#220432),
(#220433,#220434),(#220435,#220436),(#220437,#220438),(#220439,#220440),
(#220441,#220442),(#220443,#220444),(#220445,#220446),(#220447,#220448),
(#220449,#220450),(#220451,#220452),(#220453,#220454),(#220455,#220456),
(#220457,#220458),(#220459,#220460),(#220461,#220462),(#220463,#220464),
(#220465,#220466),(#220467,#220468),(#220469,#220470),(#220471,#220472),
(#220473,#220474),(#220475,#220476),(#220477,#220478),(#220479,#220480),
(#220481,#220482),(#220483,#220484),(#220485,#220486),(#220487,#220488),
(#220489,#220490),(#220491,#220492),(#220493,#220494),(#220495,#220496),
(#220497,#220498),(#220499,#220500),(#220501,#220502),(#220503,#220504),
(#220505,#220506),(#220507,#220508),(#220509,#220510),(#220511,#220512),
(#220513,#220514),(#220515,#220516),(#220517,#220518),(#220519,#220520),
(#220521,#220522),(#220523,#220524),(#220525,#220526),(#220527,#220528),
(#220529,#220530),(#220531,#220532),(#220533,#220534),(#220535,#220536),
(#220537,#220538),(#220539,#220540),(#220541,#220542),(#220543,#220544),
(#220545,#220546),(#220547,#220548),(#220549,#220550),(#220551,#220552),
(#220553,#220554),(#220555,#220556),(#220557,#220558),(#220559,#220560),
(#220561,#220562),(#220563,#220564),(#220565,#220566),(#220567,#220568),
(#220569,#220570),(#220571,#220572),(#220573,#220574),(#220575,#220576),
(#220577,#220578),(#220579,#220580),(#220581,#220582),(#220583,#220584),
(#220585,#220586),(#220587,#220588),(#220589,#220590),(#220591,#220592),
(#220593,#220594),(#220595,#220596),(#220597,#220598),(#220599,#220600),
(#220601,#220602),(#220603,#220604),(#220605,#220606),(#220607,#220608),
(#220609,#220610),(#220611,#220612),(#220613,#220614),(#220615,#220616),
(#220617,#220618),(#220619,#220620),(#220621,#220622),(#220623,#220624),
(#220625,#220626),(#220627,#220628),(#220629,#220630),(#220631,#220632),
(#220633,#220634),(#220635,#220636),(#220637,#220638),(#220639,#220640),
(#220641,#220642),(#220643,#220644),(#220645,#220646),(#220647,#220648),
(#220649,#220650),(#220651,#220652),(#220653,#220654),(#220655,#220656),
(#220657,#220658),(#220659,#220660),(#220661,#220662),(#220663,#220664),
(#220665,#220666),(#220667,#220668),(#220669,#220670),(#220671,#220672),
(#220673,#220674),(#220675,#220676),(#220677,#220678),(#220679,#220680),
(#220681,#220682),(#220683,#220684),(#220685,#220686),(#220687,#220688),
(#220689,#220690),(#220691,#220692),(#220693,#220694),(#220695,#220696),
(#220697,#220698),(#220699,#220700),(#220701,#220702),(#220703,#220704),
(#220705,#220706),(#220707,#220708),(#220709,#220710),(#220711,#220712),
(#220713,#220714),(#220715,#220716),(#220717,#220718),(#220719,#220720),
(#220721,#220722),(#220723,#220724),(#220725,#220726),(#220727,#220728),
(#220729,#220730),(#220731,#220732),(#220733,#220734),(#220735,#220736),
(#220737,#220738),(#220739,#220740),(#220741,#220742),(#220743,#220744),
(#220745,#220746),(#220747,#220748),(#220749,#220750),(#220751,#220752),
(#220753,#220754),(#220755,#220756),(#220757,#220758),(#220759,#220760),
(#220761,#220762),(#220763,#220764),(#220765,#220766),(#220767,#220768),
(#220769,#220770),(#220771,#220772),(#220773,#220774),(#220775,#220776),
(#220777,#220778),(#220779,#220780),(#220781,#220782),(#220783,#220784),
(#220785,#220786),(#220787,#220788),(#220789,#220790),(#220791,#220792),
(#220793,#220794),(#220795,#220796),(#220797,#220798),(#220799,#220800),
(#220801,#220802),(#220803,#220804),(#220805,#220806),(#220807,#220808),
(#220809,#220810),(#220811,#220812),(#220813,#220814),(#220815,#220816),
(#220817,#220818),(#220819,#220820),(#220821,#220822),(#220823,#220824),
(#220825,#220826),(#220827,#220828),(#220829,#220830),(#220831,#220832),
(#220833,#220834),(#220835,#220836),(#220837,#220838),(#220839,#220840),
(#220841,#220842),(#220843,#220844),(#220845,#220846),(#220847,#220848),
(#220849,#220850),(#220851,#220852),(#220853,#220854),(#220855,#220856),
(#220857,#220858),(#220859,#220860),(#220861,#220862),(#220863,#220864),
(#220865,#220866),(#220867,#220868),(#220869,#220870),(#220871,#220872),
(#220873,#220874),(#220875,#220876),(#220877,#220878),(#220879,#220880),
(#220881,#220882),(#220883,#220884),(#220885,#220886),(#220887,#220888),
(#220889,#220890),(#220891,#220892),(#220893,#220894),(#220895,#220896),
(#220897,#220898),(#220899,#220900),(#220901,#220902),(#220903,#220904),
(#220905,#220906),(#220907,#220908),(#220909,#220910),(#220911,#220912),
(#220913,#220914),(#220915,#220916),(#220917,#220918),(#220919,#220920),
(#220921,#220922),(#220923,#220924),(#220925,#220926),(#220927,#220928),
(#220929,#220930),(#220931,#220932),(#220933,#220934),(#220935,#220936),
(#220937,#220938),(#220939,#220940),(#220941,#220942),(#220943,#220944),
(#220945,#220946),(#220947,#220948),(#220949,#220950),(#220951,#220952),
(#220953,#220954),(#220955,#220956),(#220957,#220958),(#220959,#220960),
(#220961,#220962),(#220963,#220964),(#220965,#220966),(#220967,#220968),
(#220969,#220970),(#220971,#220972),(#220973,#220974),(#220975,#220976),
(#220977,#220978),(#220979,#220980),(#220981,#220982),(#220983,#220984),
(#220985,#220986),(#220987,#220988),(#220989,#220990),(#220991,#220992),
(#220993,#220994),(#220995,#220996),(#220997,#220998),(#220999,#221000),
(#221001,#221002),(#221003,#221004),(#221005,#221006),(#221007,#221008),
(#221009,#221010),(#221011,#221012),(#221013,#221014),(#221015,#221016),
(#221017,#221018),(#221019,#221020),(#221021,#221022),(#221023,#221024),
(#221025,#221026),(#221027,#221028),(#221029,#221030),(#221031,#221032),
(#221033,#221034),(#221035,#221036),(#221037,#221038),(#221039,#221040),
(#221041,#221042),(#221043,#221044),(#221045,#221046),(#221047,#221048),
(#221049,#221050),(#221051,#221052),(#221053,#221054),(#221055,#221056),
(#221057,#221058),(#221059,#221060),(#221061,#221062),(#221063,#221064),
(#221065,#221066),(#221067,#221068),(#221069,#221070),(#221071,#221072),
(#221073,#221074),(#221075,#221076),(#221077,#221078),(#221079,#221080),
(#221081,#221082),(#221083,#221084),(#221085,#221086),(#221087,#221088),
(#221089,#221090),(#221091,#221092),(#221093,#221094),(#221095,#221096),
(#221097,#221098),(#221099,#221100),(#221101,#221102),(#221103,#221104),
(#221105,#221106),(#221107,#221108),(#221109,#221110),(#221111,#221112),
(#221113,#221114),(#221115,#221116),(#221117,#221118),(#221119,#221120),
(#221121,#221122),(#221123,#221124),(#221125,#221126),(#221127,#221128),
(#221129,#221130),(#221131,#221132),(#221133,#221134),(#221135,#221136),
(#221137,#221138),(#221139,#221140),(#221141,#221142),(#221143,#221144),
(#221145,#221146),(#221147,#221148),(#221149,#221150),(#221151,#221152),
(#221153,#221154),(#221155,#221156),(#221157,#221158),(#221159,#221160),
(#221161,#221162),(#221163,#221164),(#221165,#221166),(#221167,#221168),
(#221169,#221170),(#221171,#221172),(#221173,#221174),(#221175,#221176),
(#221177,#221178),(#221179,#221180),(#221181,#221182),(#221183,#221184),
(#221185,#221186),(#221187,#221188),(#221189,#221190),(#221191,#221192),
(#221193,#221194),(#221195,#221196),(#221197,#221198),(#221199,#221200),
(#221201,#221202),(#221203,#221204),(#221205,#221206),(#221207,#221208),
(#221209,#221210),(#221211,#221212),(#221213,#221214),(#221215,#221216),
(#221217,#221218),(#221219,#221220),(#221221,#221222),(#221223,#221224),
(#221225,#221226),(#221227,#221228),(#221229,#221230),(#221231,#221232),
(#221233,#221234),(#221235,#221236),(#221237,#221238),(#221239,#221240),
(#221241,#221242),(#221243,#221244),(#221245,#221246),(#221247,#221248),
(#221249,#221250),(#221251,#221252),(#221253,#221254),(#221255,#221256),
(#221257,#221258),(#221259,#221260),(#221261,#221262),(#221263,#221264),
(#221265,#221266),(#221267,#221268),(#221269,#221270),(#221271,#221272),
(#221273,#221274),(#221275,#221276),(#221277,#221278),(#221279,#221280),
(#221281,#221282),(#221283,#221284),(#221285,#221286),(#221287,#221288),
(#221289,#221290),(#221291,#221292),(#221293,#221294),(#221295,#221296),
(#221297,#221298),(#221299,#221300),(#221301,#221302),(#221303,#221304),
(#221305,#221306),(#221307,#221308),(#221309,#221310),(#221311,#221312),
(#221313,#221314),(#221315,#221316),(#221317,#221318),(#221319,#221320),
(#221321,#221322),(#221323,#221324),(#221325,#221326),(#221327,#221328),
(#221329,#221330),(#221331,#221332),(#221333,#221334),(#221335,#221336),
(#221337,#221338),(#221339,#221340),(#221341,#221342),(#221343,#221344),
(#221345,#221346),(#221347,#221348),(#221349,#221350),(#221351,#221352),
(#221353,#221354),(#221355,#221356),(#221357,#221358),(#221359,#221360),
(#221361,#221362),(#221363,#221364)),.UNSPECIFIED.,.F.,.F.,.F.,(6,1,1,1,
1,1,1,1,1,1,1,1,1,1,1,1,1,1,1,1,1,1,1,1,1,1,1,1,1,1,1,1,1,1,1,1,1,1,1,1,
1,1,1,1,1,1,1,1,1,1,1,1,1,1,1,1,1,1,1,1,1,1,1,1,1,1,1,1,1,1,1,1,1,1,1,1,
1,1,1,1,1,1,1,1,1,1,1,1,1,1,1,1,1,1,1,1,1,1,1,1,1,1,1,1,1,1,1,1,1,1,1,1,
1,1,1,1,1,1,1,1,1,1,1,1,1,1,1,1,1,1,1,1,1,1,1,1,1,1,1,1,1,1,1,1,1,1,1,1,
1,1,1,1,1,1,1,1,1,1,1,1,1,1,1,1,1,1,1,1,1,1,1,1,1,1,1,1,1,1,1,1,1,1,1,1,
1,1,1,1,1,1,1,1,1,1,1,1,1,1,1,1,1,1,1,1,1,1,1,1,1,1,1,1,1,1,1,1,1,1,1,1,
1,1,1,1,1,1,1,1,1,1,1,1,1,1,1,1,1,1,1,1,1,1,1,1,1,1,1,1,1,1,1,1,1,1,1,1,
1,1,1,1,1,1,1,1,1,1,1,1,1,1,1,1,1,1,1,1,1,1,1,1,1,1,1,1,1,1,1,1,1,1,1,1,
1,1,1,1,1,1,1,1,1,1,1,1,1,1,1,1,1,1,1,1,1,1,1,1,1,1,1,1,1,1,1,1,1,1,1,1,
1,1,1,1,1,1,1,1,1,1,1,1,1,1,1,1,1,1,1,1,1,1,1,1,1,1,1,1,1,1,1,1,1,1,1,1,
1,1,1,1,1,1,1,1,1,1,1,1,1,1,1,1,1,1,1,1,1,1,1,1,1,1,1,1,1,1,1,1,1,1,1,1,
1,1,1,1,1,1,1,1,1,1,1,1,1,1,1,1,1,1,1,1,1,1,1,1,1,1,1,1,1,1,1,1,1,1,1,1,
1,1,1,1,1,1,1,1,1,1,1,1,1,1,1,1,1,1,1,1,1,1,1,1,1,1,1,1,1,1,1,6),(2,2),
(0.143172103,0.144954128,0.146788991,0.148623853,0.150458716,0.152293578,
0.15412844,0.155963303,0.157798165,0.159633028,0.16146789,0.163302752,0.165137615,
0.166972477,0.168807339,0.170642202,0.172477064,0.174311927,0.176146789,
0.177981651,0.179816514,0.181651376,0.183486239,0.185321101,0.187155963,
0.188990826,0.190825688,0.19266055,0.194495413,0.196330275,0.198165138,
0.2,0.201834862,0.203669725,0.205504587,0.20733945,0.209174312,0.211009174,
0.212844037,0.214678899,0.216513761,0.218348624,0.220183486,0.222018349,
0.223853211,0.225688073,0.227522936,0.229357798,0.231192661,0.233027523,
0.234862385,0.236697248,0.23853211,0.240366972,0.242201835,0.244036697,
0.24587156,0.247706422,0.249541284,0.251376147,0.253211009,0.255045872,
0.256880734,0.258715596,0.260550459,0.262385321,0.264220183,0.266055046,
0.267889908,0.269724771,0.271559633,0.273394495,0.275229358,0.27706422,
0.278899083,0.280733945,0.282568807,0.28440367,0.286238532,0.288073394,
0.289908257,0.291743119,0.293577982,0.295412844,0.297247706,0.299082569,
0.300917431,0.302752294,0.304587156,0.306422018,0.308256881,0.310091743,
0.311926606,0.313761468,0.31559633,0.317431193,0.319266055,0.321100917,
0.32293578,0.324770642,0.326605505,0.328440367,0.330275229,0.332110092,
0.333944954,0.335779817,0.337614679,0.339449541,0.341284404,0.343119266,
0.344954128,0.346788991,0.348623853,0.350458716,0.352293578,0.35412844,
0.355963303,0.357798165,0.359633028,0.36146789,0.363302752,0.365137615,
0.366972477,0.368807339,0.370642202,0.372477064,0.374311927,0.376146789,
0.377981651,0.379816514,0.381651376,0.383486239,0.385321101,0.387155963,
0.388990826,0.390825688,0.39266055,0.394495413,0.396330275,0.398165138,
0.4,0.401834862,0.403669725,0.405504587,0.40733945,0.409174312,0.411009174,
0.412844037,0.414678899,0.416513761,0.418348624,0.420183486,0.422018349,
0.423853211,0.425688073,0.427522936,0.429357798,0.431192661,0.433027523,
0.434862385,0.436697248,0.43853211,0.440366972,0.442201835,0.444036697,
0.44587156,0.447706422,0.449541284,0.451376147,0.453211009,0.455045872,
0.456880734,0.458715596,0.460550459,0.462385321,0.464220183,0.466055046,
0.467889908,0.469724771,0.471559633,0.473394495,0.475229358,0.47706422,
0.478899083,0.480733945,0.482568807,0.48440367,0.486238532,0.488073394,
0.489908257,0.491743119,0.493577982,0.495412844,0.497247706,0.499082569,
0.500917431,0.502752294,0.504587156,0.506422018,0.508256881,0.510091743,
0.511926606,0.513761468,0.51559633,0.517431193,0.519266055,0.521100917,
0.52293578,0.524770642,0.526605505,0.528440367,0.530275229,0.532110092,
0.533944954,0.535779817,0.537614679,0.539449541,0.541284404,0.543119266,
0.544954128,0.546788991,0.548623853,0.550458716,0.552293578,0.55412844,
0.555963303,0.557798165,0.559633028,0.56146789,0.563302752,0.565137615,
0.566972477,0.568807339,0.570642202,0.572477064,0.574311927,0.576146789,
0.577981651,0.579816514,0.581651376,0.583486239,0.585321101,0.587155963,
0.588990826,0.590825688,0.59266055,0.594495413,0.596330275,0.598165138,
0.6,0.601834862,0.603669725,0.605504587,0.60733945,0.609174312,0.611009174,
0.612844037,0.614678899,0.616513761,0.618348624,0.620183486,0.622018349,
0.623853211,0.625688073,0.627522936,0.629357798,0.631192661,0.633027523,
0.634862385,0.636697248,0.63853211,0.640366972,0.642201835,0.644036697,
0.64587156,0.647706422,0.649541284,0.651376147,0.653211009,0.655045872,
0.656880734,0.658715596,0.660550459,0.662385321,0.664220183,0.666055046,
0.667889908,0.669724771,0.671559633,0.673394495,0.675229358,0.67706422,
0.678899083,0.680733945,0.682568807,0.68440367,0.686238532,0.688073394,
0.689908257,0.691743119,0.693577982,0.695412844,0.697247706,0.699082569,
0.700917431,0.702752294,0.704587156,0.706422018,0.708256881,0.710091743,
0.711926606,0.713761468,0.71559633,0.717431193,0.719266055,0.721100917,
0.72293578,0.724770642,0.726605505,0.728440367,0.730275229,0.732110092,
0.733944954,0.735779817,0.737614679,0.739449541,0.741284404,0.743119266,
0.744954128,0.746788991,0.748623853,0.750458716,0.752293578,0.75412844,
0.755963303,0.757798165,0.759633028,0.76146789,0.763302752,0.765137615,
0.766972477,0.768807339,0.770642202,0.772477064,0.774311927,0.776146789,
0.777981651,0.779816514,0.781651376,0.783486239,0.785321101,0.787155963,
0.788990826,0.790825688,0.79266055,0.794495413,0.796330275,0.798165138,
0.8,0.801834862,0.803669725,0.805504587,0.80733945,0.809174312,0.811009174,
0.812844037,0.814678899,0.816513761,0.818348624,0.820183486,0.822018349,
0.823853211,0.825688073,0.827522936,0.829357798,0.831192661,0.833027523,
0.834862385,0.836697248,0.83853211,0.840366972,0.842201835,0.844036697,
0.84587156,0.847706422,0.849541284,0.851376147,0.853211009,0.855045872,
0.856880734,0.858715596,0.860550459,0.862385321,0.864220183,0.866055046,
0.867889908,0.869724771,0.871559633,0.873394495,0.875229358,0.87706422,
0.878899083,0.880733945,0.882568807,0.88440367,0.886238532,0.888073394,
0.889908257,0.891743119,0.893577982,0.895412844,0.897247706,0.899082569,
0.900917431,0.902752294,0.904587156,0.906422018,0.908256881,0.910091743,
0.911926606,0.913761468,0.91559633,0.917431193,0.919266055,0.921100917,
0.92293578,0.924770642,0.926605505,0.928440367,0.930275229,0.932110092,
0.933944954,0.935779817,0.937614679,0.939449541,0.941284404,0.943119266,
0.944954128,0.946788991,0.948623853,0.950458716,0.952293578,0.95412844,
0.955963303,0.957798165,0.959633028,0.96146789,0.963302752,0.965137615,
0.966972477,0.968807339,0.970642202,0.972477064,0.974311927,0.976146789,
0.977981651,0.979816514,0.981651376,0.983486239,0.985321101,0.987155963,
0.988990826,0.990825688,0.99266055,0.994495413,0.996330275,0.998165138,
1.),(0.,0.36),.UNSPECIFIED.);
#6256=B_SPLINE_SURFACE_WITH_KNOTS('',5,1,((#221976,#221977),(#221978,#221979),
(#221980,#221981),(#221982,#221983),(#221984,#221985),(#221986,#221987),
(#221988,#221989),(#221990,#221991),(#221992,#221993),(#221994,#221995),
(#221996,#221997),(#221998,#221999),(#222000,#222001),(#222002,#222003),
(#222004,#222005),(#222006,#222007),(#222008,#222009),(#222010,#222011),
(#222012,#222013),(#222014,#222015),(#222016,#222017),(#222018,#222019),
(#222020,#222021),(#222022,#222023),(#222024,#222025),(#222026,#222027),
(#222028,#222029),(#222030,#222031),(#222032,#222033),(#222034,#222035),
(#222036,#222037),(#222038,#222039),(#222040,#222041),(#222042,#222043),
(#222044,#222045),(#222046,#222047),(#222048,#222049),(#222050,#222051),
(#222052,#222053),(#222054,#222055),(#222056,#222057),(#222058,#222059),
(#222060,#222061),(#222062,#222063),(#222064,#222065),(#222066,#222067),
(#222068,#222069),(#222070,#222071),(#222072,#222073),(#222074,#222075),
(#222076,#222077),(#222078,#222079),(#222080,#222081),(#222082,#222083),
(#222084,#222085),(#222086,#222087),(#222088,#222089),(#222090,#222091),
(#222092,#222093),(#222094,#222095),(#222096,#222097),(#222098,#222099),
(#222100,#222101),(#222102,#222103),(#222104,#222105),(#222106,#222107),
(#222108,#222109),(#222110,#222111),(#222112,#222113),(#222114,#222115),
(#222116,#222117),(#222118,#222119),(#222120,#222121),(#222122,#222123),
(#222124,#222125),(#222126,#222127),(#222128,#222129),(#222130,#222131),
(#222132,#222133),(#222134,#222135),(#222136,#222137),(#222138,#222139),
(#222140,#222141),(#222142,#222143),(#222144,#222145),(#222146,#222147),
(#222148,#222149),(#222150,#222151),(#222152,#222153),(#222154,#222155),
(#222156,#222157),(#222158,#222159),(#222160,#222161),(#222162,#222163),
(#222164,#222165),(#222166,#222167),(#222168,#222169),(#222170,#222171),
(#222172,#222173),(#222174,#222175),(#222176,#222177),(#222178,#222179),
(#222180,#222181),(#222182,#222183),(#222184,#222185),(#222186,#222187),
(#222188,#222189),(#222190,#222191),(#222192,#222193),(#222194,#222195),
(#222196,#222197),(#222198,#222199),(#222200,#222201),(#222202,#222203),
(#222204,#222205),(#222206,#222207),(#222208,#222209),(#222210,#222211),
(#222212,#222213),(#222214,#222215),(#222216,#222217),(#222218,#222219),
(#222220,#222221),(#222222,#222223),(#222224,#222225),(#222226,#222227),
(#222228,#222229),(#222230,#222231),(#222232,#222233),(#222234,#222235),
(#222236,#222237),(#222238,#222239),(#222240,#222241),(#222242,#222243),
(#222244,#222245),(#222246,#222247),(#222248,#222249),(#222250,#222251),
(#222252,#222253),(#222254,#222255),(#222256,#222257),(#222258,#222259),
(#222260,#222261),(#222262,#222263),(#222264,#222265),(#222266,#222267),
(#222268,#222269),(#222270,#222271),(#222272,#222273),(#222274,#222275),
(#222276,#222277),(#222278,#222279),(#222280,#222281),(#222282,#222283),
(#222284,#222285),(#222286,#222287),(#222288,#222289),(#222290,#222291),
(#222292,#222293),(#222294,#222295),(#222296,#222297),(#222298,#222299),
(#222300,#222301),(#222302,#222303),(#222304,#222305),(#222306,#222307),
(#222308,#222309),(#222310,#222311),(#222312,#222313),(#222314,#222315),
(#222316,#222317),(#222318,#222319),(#222320,#222321),(#222322,#222323),
(#222324,#222325),(#222326,#222327),(#222328,#222329),(#222330,#222331),
(#222332,#222333),(#222334,#222335),(#222336,#222337),(#222338,#222339),
(#222340,#222341),(#222342,#222343),(#222344,#222345),(#222346,#222347),
(#222348,#222349),(#222350,#222351),(#222352,#222353),(#222354,#222355),
(#222356,#222357),(#222358,#222359),(#222360,#222361),(#222362,#222363),
(#222364,#222365),(#222366,#222367),(#222368,#222369),(#222370,#222371),
(#222372,#222373),(#222374,#222375),(#222376,#222377),(#222378,#222379),
(#222380,#222381),(#222382,#222383),(#222384,#222385),(#222386,#222387),
(#222388,#222389),(#222390,#222391),(#222392,#222393),(#222394,#222395),
(#222396,#222397),(#222398,#222399),(#222400,#222401),(#222402,#222403),
(#222404,#222405),(#222406,#222407),(#222408,#222409),(#222410,#222411),
(#222412,#222413),(#222414,#222415),(#222416,#222417),(#222418,#222419),
(#222420,#222421),(#222422,#222423),(#222424,#222425),(#222426,#222427),
(#222428,#222429),(#222430,#222431),(#222432,#222433),(#222434,#222435),
(#222436,#222437),(#222438,#222439),(#222440,#222441),(#222442,#222443),
(#222444,#222445),(#222446,#222447),(#222448,#222449),(#222450,#222451),
(#222452,#222453),(#222454,#222455),(#222456,#222457),(#222458,#222459),
(#222460,#222461),(#222462,#222463),(#222464,#222465),(#222466,#222467),
(#222468,#222469),(#222470,#222471),(#222472,#222473),(#222474,#222475),
(#222476,#222477),(#222478,#222479),(#222480,#222481),(#222482,#222483),
(#222484,#222485),(#222486,#222487),(#222488,#222489),(#222490,#222491),
(#222492,#222493),(#222494,#222495),(#222496,#222497),(#222498,#222499),
(#222500,#222501),(#222502,#222503),(#222504,#222505),(#222506,#222507),
(#222508,#222509),(#222510,#222511),(#222512,#222513),(#222514,#222515),
(#222516,#222517),(#222518,#222519),(#222520,#222521),(#222522,#222523),
(#222524,#222525),(#222526,#222527),(#222528,#222529),(#222530,#222531),
(#222532,#222533),(#222534,#222535),(#222536,#222537),(#222538,#222539),
(#222540,#222541),(#222542,#222543),(#222544,#222545),(#222546,#222547),
(#222548,#222549),(#222550,#222551),(#222552,#222553),(#222554,#222555),
(#222556,#222557),(#222558,#222559),(#222560,#222561),(#222562,#222563),
(#222564,#222565),(#222566,#222567),(#222568,#222569),(#222570,#222571),
(#222572,#222573),(#222574,#222575),(#222576,#222577),(#222578,#222579),
(#222580,#222581),(#222582,#222583),(#222584,#222585),(#222586,#222587),
(#222588,#222589),(#222590,#222591),(#222592,#222593),(#222594,#222595),
(#222596,#222597),(#222598,#222599),(#222600,#222601),(#222602,#222603),
(#222604,#222605),(#222606,#222607),(#222608,#222609),(#222610,#222611),
(#222612,#222613),(#222614,#222615),(#222616,#222617),(#222618,#222619),
(#222620,#222621),(#222622,#222623),(#222624,#222625),(#222626,#222627),
(#222628,#222629),(#222630,#222631),(#222632,#222633),(#222634,#222635),
(#222636,#222637),(#222638,#222639),(#222640,#222641),(#222642,#222643),
(#222644,#222645),(#222646,#222647),(#222648,#222649),(#222650,#222651),
(#222652,#222653),(#222654,#222655),(#222656,#222657),(#222658,#222659),
(#222660,#222661),(#222662,#222663),(#222664,#222665),(#222666,#222667),
(#222668,#222669),(#222670,#222671),(#222672,#222673),(#222674,#222675),
(#222676,#222677),(#222678,#222679),(#222680,#222681),(#222682,#222683),
(#222684,#222685),(#222686,#222687),(#222688,#222689),(#222690,#222691),
(#222692,#222693),(#222694,#222695),(#222696,#222697),(#222698,#222699),
(#222700,#222701),(#222702,#222703),(#222704,#222705),(#222706,#222707),
(#222708,#222709),(#222710,#222711),(#222712,#222713),(#222714,#222715),
(#222716,#222717),(#222718,#222719),(#222720,#222721),(#222722,#222723),
(#222724,#222725),(#222726,#222727),(#222728,#222729),(#222730,#222731),
(#222732,#222733),(#222734,#222735),(#222736,#222737),(#222738,#222739),
(#222740,#222741),(#222742,#222743),(#222744,#222745),(#222746,#222747),
(#222748,#222749),(#222750,#222751),(#222752,#222753),(#222754,#222755),
(#222756,#222757),(#222758,#222759),(#222760,#222761),(#222762,#222763),
(#222764,#222765),(#222766,#222767),(#222768,#222769),(#222770,#222771),
(#222772,#222773),(#222774,#222775),(#222776,#222777),(#222778,#222779),
(#222780,#222781),(#222782,#222783),(#222784,#222785),(#222786,#222787),
(#222788,#222789),(#222790,#222791),(#222792,#222793),(#222794,#222795),
(#222796,#222797),(#222798,#222799),(#222800,#222801),(#222802,#222803),
(#222804,#222805),(#222806,#222807),(#222808,#222809),(#222810,#222811),
(#222812,#222813),(#222814,#222815),(#222816,#222817),(#222818,#222819),
(#222820,#222821),(#222822,#222823),(#222824,#222825),(#222826,#222827),
(#222828,#222829),(#222830,#222831),(#222832,#222833),(#222834,#222835),
(#222836,#222837),(#222838,#222839),(#222840,#222841),(#222842,#222843),
(#222844,#222845),(#222846,#222847),(#222848,#222849),(#222850,#222851),
(#222852,#222853),(#222854,#222855),(#222856,#222857),(#222858,#222859),
(#222860,#222861),(#222862,#222863),(#222864,#222865),(#222866,#222867),
(#222868,#222869),(#222870,#222871),(#222872,#222873),(#222874,#222875),
(#222876,#222877),(#222878,#222879),(#222880,#222881),(#222882,#222883),
(#222884,#222885),(#222886,#222887),(#222888,#222889),(#222890,#222891),
(#222892,#222893),(#222894,#222895),(#222896,#222897),(#222898,#222899),
(#222900,#222901),(#222902,#222903),(#222904,#222905),(#222906,#222907),
(#222908,#222909),(#222910,#222911),(#222912,#222913),(#222914,#222915),
(#222916,#222917),(#222918,#222919)),.UNSPECIFIED.,.F.,.F.,.F.,(6,1,1,1,
1,1,1,1,1,1,1,1,1,1,1,1,1,1,1,1,1,1,1,1,1,1,1,1,1,1,1,1,1,1,1,1,1,1,1,1,
1,1,1,1,1,1,1,1,1,1,1,1,1,1,1,1,1,1,1,1,1,1,1,1,1,1,1,1,1,1,1,1,1,1,1,1,
1,1,1,1,1,1,1,1,1,1,1,1,1,1,1,1,1,1,1,1,1,1,1,1,1,1,1,1,1,1,1,1,1,1,1,1,
1,1,1,1,1,1,1,1,1,1,1,1,1,1,1,1,1,1,1,1,1,1,1,1,1,1,1,1,1,1,1,1,1,1,1,1,
1,1,1,1,1,1,1,1,1,1,1,1,1,1,1,1,1,1,1,1,1,1,1,1,1,1,1,1,1,1,1,1,1,1,1,1,
1,1,1,1,1,1,1,1,1,1,1,1,1,1,1,1,1,1,1,1,1,1,1,1,1,1,1,1,1,1,1,1,1,1,1,1,
1,1,1,1,1,1,1,1,1,1,1,1,1,1,1,1,1,1,1,1,1,1,1,1,1,1,1,1,1,1,1,1,1,1,1,1,
1,1,1,1,1,1,1,1,1,1,1,1,1,1,1,1,1,1,1,1,1,1,1,1,1,1,1,1,1,1,1,1,1,1,1,1,
1,1,1,1,1,1,1,1,1,1,1,1,1,1,1,1,1,1,1,1,1,1,1,1,1,1,1,1,1,1,1,1,1,1,1,1,
1,1,1,1,1,1,1,1,1,1,1,1,1,1,1,1,1,1,1,1,1,1,1,1,1,1,1,1,1,1,1,1,1,1,1,1,
1,1,1,1,1,1,1,1,1,1,1,1,1,1,1,1,1,1,1,1,1,1,1,1,1,1,1,1,1,1,1,1,1,1,1,1,
1,1,1,1,1,1,1,1,1,1,1,1,1,1,1,1,1,1,1,1,1,1,1,1,1,1,1,1,1,1,1,1,1,1,1,1,
1,1,1,1,1,1,1,1,1,1,1,1,1,1,1,1,1,1,1,1,1,1,1,1,1,1,1,1,1,1,1,6),(2,2),
(-1.,-0.998165138,-0.996330275,-0.994495413,-0.99266055,-0.990825688,-0.988990826,
-0.987155963,-0.985321101,-0.983486239,-0.981651376,-0.979816514,-0.977981651,
-0.976146789,-0.974311927,-0.972477064,-0.970642202,-0.968807339,-0.966972477,
-0.965137615,-0.963302752,-0.96146789,-0.959633028,-0.957798165,-0.955963303,
-0.95412844,-0.952293578,-0.950458716,-0.948623853,-0.946788991,-0.944954128,
-0.943119266,-0.941284404,-0.939449541,-0.937614679,-0.935779817,-0.933944954,
-0.932110092,-0.930275229,-0.928440367,-0.926605505,-0.924770642,-0.92293578,
-0.921100917,-0.919266055,-0.917431193,-0.91559633,-0.913761468,-0.911926606,
-0.910091743,-0.908256881,-0.906422018,-0.904587156,-0.902752294,-0.900917431,
-0.899082569,-0.897247706,-0.895412844,-0.893577982,-0.891743119,-0.889908257,
-0.888073394,-0.886238532,-0.88440367,-0.882568807,-0.880733945,-0.878899083,
-0.87706422,-0.875229358,-0.873394495,-0.871559633,-0.869724771,-0.867889908,
-0.866055046,-0.864220183,-0.862385321,-0.860550459,-0.858715596,-0.856880734,
-0.855045872,-0.853211009,-0.851376147,-0.849541284,-0.847706422,-0.84587156,
-0.844036697,-0.842201835,-0.840366972,-0.83853211,-0.836697248,-0.834862385,
-0.833027523,-0.831192661,-0.829357798,-0.827522936,-0.825688073,-0.823853211,
-0.822018349,-0.820183486,-0.818348624,-0.816513761,-0.814678899,-0.812844037,
-0.811009174,-0.809174312,-0.80733945,-0.805504587,-0.803669725,-0.801834862,
-0.8,-0.798165138,-0.796330275,-0.794495413,-0.79266055,-0.790825688,-0.788990826,
-0.787155963,-0.785321101,-0.783486239,-0.781651376,-0.779816514,-0.777981651,
-0.776146789,-0.774311927,-0.772477064,-0.770642202,-0.768807339,-0.766972477,
-0.765137615,-0.763302752,-0.76146789,-0.759633028,-0.757798165,-0.755963303,
-0.75412844,-0.752293578,-0.750458716,-0.748623853,-0.746788991,-0.744954128,
-0.743119266,-0.741284404,-0.739449541,-0.737614679,-0.735779817,-0.733944954,
-0.732110092,-0.730275229,-0.728440367,-0.726605505,-0.724770642,-0.72293578,
-0.721100917,-0.719266055,-0.717431193,-0.71559633,-0.713761468,-0.711926606,
-0.710091743,-0.708256881,-0.706422018,-0.704587156,-0.702752294,-0.700917431,
-0.699082569,-0.697247706,-0.695412844,-0.693577982,-0.691743119,-0.689908257,
-0.688073394,-0.686238532,-0.68440367,-0.682568807,-0.680733945,-0.678899083,
-0.67706422,-0.675229358,-0.673394495,-0.671559633,-0.669724771,-0.667889908,
-0.666055046,-0.664220183,-0.662385321,-0.660550459,-0.658715596,-0.656880734,
-0.655045872,-0.653211009,-0.651376147,-0.649541284,-0.647706422,-0.64587156,
-0.644036697,-0.642201835,-0.640366972,-0.63853211,-0.636697248,-0.634862385,
-0.633027523,-0.631192661,-0.629357798,-0.627522936,-0.625688073,-0.623853211,
-0.622018349,-0.620183486,-0.618348624,-0.616513761,-0.614678899,-0.612844037,
-0.611009174,-0.609174312,-0.60733945,-0.605504587,-0.603669725,-0.601834862,
-0.6,-0.598165138,-0.596330275,-0.594495413,-0.59266055,-0.590825688,-0.588990826,
-0.587155963,-0.585321101,-0.583486239,-0.581651376,-0.579816514,-0.577981651,
-0.576146789,-0.574311927,-0.572477064,-0.570642202,-0.568807339,-0.566972477,
-0.565137615,-0.563302752,-0.56146789,-0.559633028,-0.557798165,-0.555963303,
-0.55412844,-0.552293578,-0.550458716,-0.548623853,-0.546788991,-0.544954128,
-0.543119266,-0.541284404,-0.539449541,-0.537614679,-0.535779817,-0.533944954,
-0.532110092,-0.530275229,-0.528440367,-0.526605505,-0.524770642,-0.52293578,
-0.521100917,-0.519266055,-0.517431193,-0.51559633,-0.513761468,-0.511926606,
-0.510091743,-0.508256881,-0.506422018,-0.504587156,-0.502752294,-0.500917431,
-0.499082569,-0.497247706,-0.495412844,-0.493577982,-0.491743119,-0.489908257,
-0.488073394,-0.486238532,-0.48440367,-0.482568807,-0.480733945,-0.478899083,
-0.47706422,-0.475229358,-0.473394495,-0.471559633,-0.469724771,-0.467889908,
-0.466055046,-0.464220183,-0.462385321,-0.460550459,-0.458715596,-0.456880734,
-0.455045872,-0.453211009,-0.451376147,-0.449541284,-0.447706422,-0.44587156,
-0.444036697,-0.442201835,-0.440366972,-0.43853211,-0.436697248,-0.434862385,
-0.433027523,-0.431192661,-0.429357798,-0.427522936,-0.425688073,-0.423853211,
-0.422018349,-0.420183486,-0.418348624,-0.416513761,-0.414678899,-0.412844037,
-0.411009174,-0.409174312,-0.40733945,-0.405504587,-0.403669725,-0.401834862,
-0.4,-0.398165138,-0.396330275,-0.394495413,-0.39266055,-0.390825688,-0.388990826,
-0.387155963,-0.385321101,-0.383486239,-0.381651376,-0.379816514,-0.377981651,
-0.376146789,-0.374311927,-0.372477064,-0.370642202,-0.368807339,-0.366972477,
-0.365137615,-0.363302752,-0.36146789,-0.359633028,-0.357798165,-0.355963303,
-0.35412844,-0.352293578,-0.350458716,-0.348623853,-0.346788991,-0.344954128,
-0.343119266,-0.341284404,-0.339449541,-0.337614679,-0.335779817,-0.333944954,
-0.332110092,-0.330275229,-0.328440367,-0.326605505,-0.324770642,-0.32293578,
-0.321100917,-0.319266055,-0.317431193,-0.31559633,-0.313761468,-0.311926606,
-0.310091743,-0.308256881,-0.306422018,-0.304587156,-0.302752294,-0.300917431,
-0.299082569,-0.297247706,-0.295412844,-0.293577982,-0.291743119,-0.289908257,
-0.288073394,-0.286238532,-0.28440367,-0.282568807,-0.280733945,-0.278899083,
-0.27706422,-0.275229358,-0.273394495,-0.271559633,-0.269724771,-0.267889908,
-0.266055046,-0.264220183,-0.262385321,-0.260550459,-0.258715596,-0.256880734,
-0.255045872,-0.253211009,-0.251376147,-0.249541284,-0.247706422,-0.24587156,
-0.244036697,-0.242201835,-0.240366972,-0.23853211,-0.236697248,-0.234862385,
-0.233027523,-0.231192661,-0.229357798,-0.227522936,-0.225688073,-0.223853211,
-0.222018349,-0.220183486,-0.218348624,-0.216513761,-0.214678899,-0.212844037,
-0.211009174,-0.209174312,-0.20733945,-0.205504587,-0.203669725,-0.201834862,
-0.2,-0.198165138,-0.196330275,-0.194495413,-0.19266055,-0.190825688,-0.188990826,
-0.187155963,-0.185321101,-0.183486239,-0.181651376,-0.179816514,-0.177981651,
-0.176146789,-0.174311927,-0.172477064,-0.170642202,-0.168807339,-0.166972477,
-0.165137615,-0.163302752,-0.16146789,-0.159633028,-0.157798165,-0.155963303,
-0.15412844,-0.152293578,-0.150458716,-0.148623853,-0.146788991,-0.144954128,
-0.143172103),(0.,0.36),.UNSPECIFIED.);
#6257=B_SPLINE_SURFACE_WITH_KNOTS('',5,1,((#223564,#223565),(#223566,#223567),
(#223568,#223569),(#223570,#223571),(#223572,#223573),(#223574,#223575),
(#223576,#223577),(#223578,#223579),(#223580,#223581),(#223582,#223583),
(#223584,#223585),(#223586,#223587),(#223588,#223589),(#223590,#223591),
(#223592,#223593),(#223594,#223595),(#223596,#223597),(#223598,#223599),
(#223600,#223601),(#223602,#223603),(#223604,#223605),(#223606,#223607),
(#223608,#223609),(#223610,#223611),(#223612,#223613),(#223614,#223615),
(#223616,#223617),(#223618,#223619),(#223620,#223621),(#223622,#223623),
(#223624,#223625),(#223626,#223627),(#223628,#223629),(#223630,#223631),
(#223632,#223633),(#223634,#223635),(#223636,#223637),(#223638,#223639),
(#223640,#223641),(#223642,#223643),(#223644,#223645),(#223646,#223647),
(#223648,#223649),(#223650,#223651),(#223652,#223653),(#223654,#223655),
(#223656,#223657),(#223658,#223659),(#223660,#223661),(#223662,#223663),
(#223664,#223665),(#223666,#223667),(#223668,#223669),(#223670,#223671),
(#223672,#223673),(#223674,#223675),(#223676,#223677),(#223678,#223679),
(#223680,#223681),(#223682,#223683),(#223684,#223685),(#223686,#223687),
(#223688,#223689),(#223690,#223691),(#223692,#223693),(#223694,#223695),
(#223696,#223697),(#223698,#223699),(#223700,#223701),(#223702,#223703),
(#223704,#223705),(#223706,#223707),(#223708,#223709),(#223710,#223711),
(#223712,#223713),(#223714,#223715),(#223716,#223717),(#223718,#223719),
(#223720,#223721),(#223722,#223723),(#223724,#223725),(#223726,#223727),
(#223728,#223729),(#223730,#223731),(#223732,#223733),(#223734,#223735),
(#223736,#223737),(#223738,#223739),(#223740,#223741),(#223742,#223743),
(#223744,#223745),(#223746,#223747),(#223748,#223749),(#223750,#223751),
(#223752,#223753),(#223754,#223755),(#223756,#223757),(#223758,#223759),
(#223760,#223761),(#223762,#223763),(#223764,#223765),(#223766,#223767),
(#223768,#223769),(#223770,#223771),(#223772,#223773),(#223774,#223775),
(#223776,#223777),(#223778,#223779),(#223780,#223781),(#223782,#223783),
(#223784,#223785),(#223786,#223787),(#223788,#223789),(#223790,#223791),
(#223792,#223793),(#223794,#223795),(#223796,#223797),(#223798,#223799),
(#223800,#223801),(#223802,#223803),(#223804,#223805),(#223806,#223807),
(#223808,#223809),(#223810,#223811),(#223812,#223813),(#223814,#223815),
(#223816,#223817),(#223818,#223819),(#223820,#223821),(#223822,#223823),
(#223824,#223825),(#223826,#223827),(#223828,#223829),(#223830,#223831),
(#223832,#223833),(#223834,#223835),(#223836,#223837),(#223838,#223839),
(#223840,#223841),(#223842,#223843),(#223844,#223845),(#223846,#223847),
(#223848,#223849),(#223850,#223851),(#223852,#223853),(#223854,#223855),
(#223856,#223857),(#223858,#223859),(#223860,#223861),(#223862,#223863),
(#223864,#223865),(#223866,#223867),(#223868,#223869),(#223870,#223871),
(#223872,#223873),(#223874,#223875),(#223876,#223877),(#223878,#223879),
(#223880,#223881),(#223882,#223883),(#223884,#223885),(#223886,#223887),
(#223888,#223889),(#223890,#223891),(#223892,#223893),(#223894,#223895),
(#223896,#223897),(#223898,#223899),(#223900,#223901),(#223902,#223903),
(#223904,#223905),(#223906,#223907),(#223908,#223909),(#223910,#223911),
(#223912,#223913),(#223914,#223915),(#223916,#223917),(#223918,#223919),
(#223920,#223921),(#223922,#223923),(#223924,#223925),(#223926,#223927),
(#223928,#223929),(#223930,#223931),(#223932,#223933),(#223934,#223935),
(#223936,#223937),(#223938,#223939),(#223940,#223941),(#223942,#223943),
(#223944,#223945),(#223946,#223947),(#223948,#223949),(#223950,#223951),
(#223952,#223953),(#223954,#223955),(#223956,#223957),(#223958,#223959),
(#223960,#223961),(#223962,#223963),(#223964,#223965),(#223966,#223967),
(#223968,#223969),(#223970,#223971),(#223972,#223973),(#223974,#223975),
(#223976,#223977),(#223978,#223979),(#223980,#223981),(#223982,#223983),
(#223984,#223985),(#223986,#223987),(#223988,#223989),(#223990,#223991),
(#223992,#223993),(#223994,#223995),(#223996,#223997),(#223998,#223999),
(#224000,#224001),(#224002,#224003),(#224004,#224005),(#224006,#224007),
(#224008,#224009),(#224010,#224011),(#224012,#224013),(#224014,#224015),
(#224016,#224017),(#224018,#224019),(#224020,#224021),(#224022,#224023),
(#224024,#224025),(#224026,#224027),(#224028,#224029),(#224030,#224031),
(#224032,#224033),(#224034,#224035),(#224036,#224037),(#224038,#224039),
(#224040,#224041),(#224042,#224043),(#224044,#224045),(#224046,#224047),
(#224048,#224049),(#224050,#224051),(#224052,#224053),(#224054,#224055),
(#224056,#224057),(#224058,#224059),(#224060,#224061),(#224062,#224063),
(#224064,#224065),(#224066,#224067),(#224068,#224069),(#224070,#224071),
(#224072,#224073),(#224074,#224075),(#224076,#224077),(#224078,#224079),
(#224080,#224081),(#224082,#224083),(#224084,#224085),(#224086,#224087),
(#224088,#224089),(#224090,#224091),(#224092,#224093),(#224094,#224095),
(#224096,#224097),(#224098,#224099),(#224100,#224101),(#224102,#224103),
(#224104,#224105),(#224106,#224107),(#224108,#224109),(#224110,#224111),
(#224112,#224113),(#224114,#224115),(#224116,#224117),(#224118,#224119),
(#224120,#224121),(#224122,#224123),(#224124,#224125),(#224126,#224127),
(#224128,#224129),(#224130,#224131),(#224132,#224133),(#224134,#224135),
(#224136,#224137),(#224138,#224139),(#224140,#224141),(#224142,#224143),
(#224144,#224145),(#224146,#224147),(#224148,#224149),(#224150,#224151),
(#224152,#224153),(#224154,#224155),(#224156,#224157),(#224158,#224159),
(#224160,#224161),(#224162,#224163),(#224164,#224165),(#224166,#224167),
(#224168,#224169),(#224170,#224171),(#224172,#224173),(#224174,#224175),
(#224176,#224177),(#224178,#224179),(#224180,#224181),(#224182,#224183),
(#224184,#224185),(#224186,#224187),(#224188,#224189),(#224190,#224191),
(#224192,#224193),(#224194,#224195),(#224196,#224197),(#224198,#224199),
(#224200,#224201),(#224202,#224203),(#224204,#224205),(#224206,#224207),
(#224208,#224209),(#224210,#224211),(#224212,#224213),(#224214,#224215),
(#224216,#224217),(#224218,#224219),(#224220,#224221),(#224222,#224223),
(#224224,#224225),(#224226,#224227),(#224228,#224229),(#224230,#224231),
(#224232,#224233),(#224234,#224235),(#224236,#224237),(#224238,#224239),
(#224240,#224241),(#224242,#224243),(#224244,#224245),(#224246,#224247),
(#224248,#224249),(#224250,#224251),(#224252,#224253),(#224254,#224255),
(#224256,#224257),(#224258,#224259),(#224260,#224261),(#224262,#224263),
(#224264,#224265),(#224266,#224267),(#224268,#224269),(#224270,#224271),
(#224272,#224273),(#224274,#224275),(#224276,#224277),(#224278,#224279),
(#224280,#224281),(#224282,#224283),(#224284,#224285),(#224286,#224287),
(#224288,#224289),(#224290,#224291),(#224292,#224293),(#224294,#224295),
(#224296,#224297),(#224298,#224299),(#224300,#224301),(#224302,#224303),
(#224304,#224305),(#224306,#224307),(#224308,#224309),(#224310,#224311),
(#224312,#224313),(#224314,#224315),(#224316,#224317),(#224318,#224319),
(#224320,#224321),(#224322,#224323),(#224324,#224325),(#224326,#224327),
(#224328,#224329),(#224330,#224331),(#224332,#224333),(#224334,#224335),
(#224336,#224337),(#224338,#224339),(#224340,#224341),(#224342,#224343),
(#224344,#224345),(#224346,#224347),(#224348,#224349),(#224350,#224351),
(#224352,#224353),(#224354,#224355),(#224356,#224357),(#224358,#224359),
(#224360,#224361),(#224362,#224363),(#224364,#224365),(#224366,#224367),
(#224368,#224369),(#224370,#224371),(#224372,#224373),(#224374,#224375),
(#224376,#224377),(#224378,#224379),(#224380,#224381),(#224382,#224383),
(#224384,#224385),(#224386,#224387),(#224388,#224389),(#224390,#224391),
(#224392,#224393),(#224394,#224395),(#224396,#224397),(#224398,#224399),
(#224400,#224401),(#224402,#224403),(#224404,#224405),(#224406,#224407),
(#224408,#224409),(#224410,#224411),(#224412,#224413),(#224414,#224415),
(#224416,#224417),(#224418,#224419),(#224420,#224421),(#224422,#224423),
(#224424,#224425),(#224426,#224427),(#224428,#224429),(#224430,#224431),
(#224432,#224433),(#224434,#224435),(#224436,#224437),(#224438,#224439),
(#224440,#224441),(#224442,#224443),(#224444,#224445),(#224446,#224447),
(#224448,#224449),(#224450,#224451),(#224452,#224453),(#224454,#224455),
(#224456,#224457),(#224458,#224459),(#224460,#224461),(#224462,#224463),
(#224464,#224465),(#224466,#224467),(#224468,#224469),(#224470,#224471),
(#224472,#224473),(#224474,#224475),(#224476,#224477),(#224478,#224479),
(#224480,#224481),(#224482,#224483),(#224484,#224485),(#224486,#224487),
(#224488,#224489),(#224490,#224491),(#224492,#224493),(#224494,#224495),
(#224496,#224497),(#224498,#224499),(#224500,#224501),(#224502,#224503),
(#224504,#224505),(#224506,#224507)),.UNSPECIFIED.,.F.,.F.,.F.,(6,1,1,1,
1,1,1,1,1,1,1,1,1,1,1,1,1,1,1,1,1,1,1,1,1,1,1,1,1,1,1,1,1,1,1,1,1,1,1,1,
1,1,1,1,1,1,1,1,1,1,1,1,1,1,1,1,1,1,1,1,1,1,1,1,1,1,1,1,1,1,1,1,1,1,1,1,
1,1,1,1,1,1,1,1,1,1,1,1,1,1,1,1,1,1,1,1,1,1,1,1,1,1,1,1,1,1,1,1,1,1,1,1,
1,1,1,1,1,1,1,1,1,1,1,1,1,1,1,1,1,1,1,1,1,1,1,1,1,1,1,1,1,1,1,1,1,1,1,1,
1,1,1,1,1,1,1,1,1,1,1,1,1,1,1,1,1,1,1,1,1,1,1,1,1,1,1,1,1,1,1,1,1,1,1,1,
1,1,1,1,1,1,1,1,1,1,1,1,1,1,1,1,1,1,1,1,1,1,1,1,1,1,1,1,1,1,1,1,1,1,1,1,
1,1,1,1,1,1,1,1,1,1,1,1,1,1,1,1,1,1,1,1,1,1,1,1,1,1,1,1,1,1,1,1,1,1,1,1,
1,1,1,1,1,1,1,1,1,1,1,1,1,1,1,1,1,1,1,1,1,1,1,1,1,1,1,1,1,1,1,1,1,1,1,1,
1,1,1,1,1,1,1,1,1,1,1,1,1,1,1,1,1,1,1,1,1,1,1,1,1,1,1,1,1,1,1,1,1,1,1,1,
1,1,1,1,1,1,1,1,1,1,1,1,1,1,1,1,1,1,1,1,1,1,1,1,1,1,1,1,1,1,1,1,1,1,1,1,
1,1,1,1,1,1,1,1,1,1,1,1,1,1,1,1,1,1,1,1,1,1,1,1,1,1,1,1,1,1,1,1,1,1,1,1,
1,1,1,1,1,1,1,1,1,1,1,1,1,1,1,1,1,1,1,1,1,1,1,1,1,1,1,1,1,1,1,1,1,1,1,1,
1,1,1,1,1,1,1,1,1,1,1,1,1,1,1,1,1,1,1,1,1,1,1,1,1,1,1,1,1,1,1,6),(2,2),
(-1.,-0.998165138,-0.996330275,-0.994495413,-0.99266055,-0.990825688,-0.988990826,
-0.987155963,-0.985321101,-0.983486239,-0.981651376,-0.979816514,-0.977981651,
-0.976146789,-0.974311927,-0.972477064,-0.970642202,-0.968807339,-0.966972477,
-0.965137615,-0.963302752,-0.96146789,-0.959633028,-0.957798165,-0.955963303,
-0.95412844,-0.952293578,-0.950458716,-0.948623853,-0.946788991,-0.944954128,
-0.943119266,-0.941284404,-0.939449541,-0.937614679,-0.935779817,-0.933944954,
-0.932110092,-0.930275229,-0.928440367,-0.926605505,-0.924770642,-0.92293578,
-0.921100917,-0.919266055,-0.917431193,-0.91559633,-0.913761468,-0.911926606,
-0.910091743,-0.908256881,-0.906422018,-0.904587156,-0.902752294,-0.900917431,
-0.899082569,-0.897247706,-0.895412844,-0.893577982,-0.891743119,-0.889908257,
-0.888073394,-0.886238532,-0.88440367,-0.882568807,-0.880733945,-0.878899083,
-0.87706422,-0.875229358,-0.873394495,-0.871559633,-0.869724771,-0.867889908,
-0.866055046,-0.864220183,-0.862385321,-0.860550459,-0.858715596,-0.856880734,
-0.855045872,-0.853211009,-0.851376147,-0.849541284,-0.847706422,-0.84587156,
-0.844036697,-0.842201835,-0.840366972,-0.83853211,-0.836697248,-0.834862385,
-0.833027523,-0.831192661,-0.829357798,-0.827522936,-0.825688073,-0.823853211,
-0.822018349,-0.820183486,-0.818348624,-0.816513761,-0.814678899,-0.812844037,
-0.811009174,-0.809174312,-0.80733945,-0.805504587,-0.803669725,-0.801834862,
-0.8,-0.798165138,-0.796330275,-0.794495413,-0.79266055,-0.790825688,-0.788990826,
-0.787155963,-0.785321101,-0.783486239,-0.781651376,-0.779816514,-0.777981651,
-0.776146789,-0.774311927,-0.772477064,-0.770642202,-0.768807339,-0.766972477,
-0.765137615,-0.763302752,-0.76146789,-0.759633028,-0.757798165,-0.755963303,
-0.75412844,-0.752293578,-0.750458716,-0.748623853,-0.746788991,-0.744954128,
-0.743119266,-0.741284404,-0.739449541,-0.737614679,-0.735779817,-0.733944954,
-0.732110092,-0.730275229,-0.728440367,-0.726605505,-0.724770642,-0.72293578,
-0.721100917,-0.719266055,-0.717431193,-0.71559633,-0.713761468,-0.711926606,
-0.710091743,-0.708256881,-0.706422018,-0.704587156,-0.702752294,-0.700917431,
-0.699082569,-0.697247706,-0.695412844,-0.693577982,-0.691743119,-0.689908257,
-0.688073394,-0.686238532,-0.68440367,-0.682568807,-0.680733945,-0.678899083,
-0.67706422,-0.675229358,-0.673394495,-0.671559633,-0.669724771,-0.667889908,
-0.666055046,-0.664220183,-0.662385321,-0.660550459,-0.658715596,-0.656880734,
-0.655045872,-0.653211009,-0.651376147,-0.649541284,-0.647706422,-0.64587156,
-0.644036697,-0.642201835,-0.640366972,-0.63853211,-0.636697248,-0.634862385,
-0.633027523,-0.631192661,-0.629357798,-0.627522936,-0.625688073,-0.623853211,
-0.622018349,-0.620183486,-0.618348624,-0.616513761,-0.614678899,-0.612844037,
-0.611009174,-0.609174312,-0.60733945,-0.605504587,-0.603669725,-0.601834862,
-0.6,-0.598165138,-0.596330275,-0.594495413,-0.59266055,-0.590825688,-0.588990826,
-0.587155963,-0.585321101,-0.583486239,-0.581651376,-0.579816514,-0.577981651,
-0.576146789,-0.574311927,-0.572477064,-0.570642202,-0.568807339,-0.566972477,
-0.565137615,-0.563302752,-0.56146789,-0.559633028,-0.557798165,-0.555963303,
-0.55412844,-0.552293578,-0.550458716,-0.548623853,-0.546788991,-0.544954128,
-0.543119266,-0.541284404,-0.539449541,-0.537614679,-0.535779817,-0.533944954,
-0.532110092,-0.530275229,-0.528440367,-0.526605505,-0.524770642,-0.52293578,
-0.521100917,-0.519266055,-0.517431193,-0.51559633,-0.513761468,-0.511926606,
-0.510091743,-0.508256881,-0.506422018,-0.504587156,-0.502752294,-0.500917431,
-0.499082569,-0.497247706,-0.495412844,-0.493577982,-0.491743119,-0.489908257,
-0.488073394,-0.486238532,-0.48440367,-0.482568807,-0.480733945,-0.478899083,
-0.47706422,-0.475229358,-0.473394495,-0.471559633,-0.469724771,-0.467889908,
-0.466055046,-0.464220183,-0.462385321,-0.460550459,-0.458715596,-0.456880734,
-0.455045872,-0.453211009,-0.451376147,-0.449541284,-0.447706422,-0.44587156,
-0.444036697,-0.442201835,-0.440366972,-0.43853211,-0.436697248,-0.434862385,
-0.433027523,-0.431192661,-0.429357798,-0.427522936,-0.425688073,-0.423853211,
-0.422018349,-0.420183486,-0.418348624,-0.416513761,-0.414678899,-0.412844037,
-0.411009174,-0.409174312,-0.40733945,-0.405504587,-0.403669725,-0.401834862,
-0.4,-0.398165138,-0.396330275,-0.394495413,-0.39266055,-0.390825688,-0.388990826,
-0.387155963,-0.385321101,-0.383486239,-0.381651376,-0.379816514,-0.377981651,
-0.376146789,-0.374311927,-0.372477064,-0.370642202,-0.368807339,-0.366972477,
-0.365137615,-0.363302752,-0.36146789,-0.359633028,-0.357798165,-0.355963303,
-0.35412844,-0.352293578,-0.350458716,-0.348623853,-0.346788991,-0.344954128,
-0.343119266,-0.341284404,-0.339449541,-0.337614679,-0.335779817,-0.333944954,
-0.332110092,-0.330275229,-0.328440367,-0.326605505,-0.324770642,-0.32293578,
-0.321100917,-0.319266055,-0.317431193,-0.31559633,-0.313761468,-0.311926606,
-0.310091743,-0.308256881,-0.306422018,-0.304587156,-0.302752294,-0.300917431,
-0.299082569,-0.297247706,-0.295412844,-0.293577982,-0.291743119,-0.289908257,
-0.288073394,-0.286238532,-0.28440367,-0.282568807,-0.280733945,-0.278899083,
-0.27706422,-0.275229358,-0.273394495,-0.271559633,-0.269724771,-0.267889908,
-0.266055046,-0.264220183,-0.262385321,-0.260550459,-0.258715596,-0.256880734,
-0.255045872,-0.253211009,-0.251376147,-0.249541284,-0.247706422,-0.24587156,
-0.244036697,-0.242201835,-0.240366972,-0.23853211,-0.236697248,-0.234862385,
-0.233027523,-0.231192661,-0.229357798,-0.227522936,-0.225688073,-0.223853211,
-0.222018349,-0.220183486,-0.218348624,-0.216513761,-0.214678899,-0.212844037,
-0.211009174,-0.209174312,-0.20733945,-0.205504587,-0.203669725,-0.201834862,
-0.2,-0.198165138,-0.196330275,-0.194495413,-0.19266055,-0.190825688,-0.188990826,
-0.187155963,-0.185321101,-0.183486239,-0.181651376,-0.179816514,-0.177981651,
-0.176146789,-0.174311927,-0.172477064,-0.170642202,-0.168807339,-0.166972477,
-0.165137615,-0.163302752,-0.16146789,-0.159633028,-0.157798165,-0.155963303,
-0.15412844,-0.152293578,-0.150458716,-0.148623853,-0.146788991,-0.144954128,
-0.143172103),(0.,0.36),.UNSPECIFIED.);
#6258=B_SPLINE_SURFACE_WITH_KNOTS('',5,1,((#225453,#225454),(#225455,#225456),
(#225457,#225458),(#225459,#225460),(#225461,#225462),(#225463,#225464),
(#225465,#225466),(#225467,#225468),(#225469,#225470),(#225471,#225472),
(#225473,#225474),(#225475,#225476),(#225477,#225478),(#225479,#225480),
(#225481,#225482),(#225483,#225484),(#225485,#225486),(#225487,#225488),
(#225489,#225490),(#225491,#225492),(#225493,#225494),(#225495,#225496),
(#225497,#225498),(#225499,#225500),(#225501,#225502),(#225503,#225504),
(#225505,#225506),(#225507,#225508),(#225509,#225510),(#225511,#225512),
(#225513,#225514),(#225515,#225516),(#225517,#225518),(#225519,#225520),
(#225521,#225522),(#225523,#225524),(#225525,#225526),(#225527,#225528),
(#225529,#225530),(#225531,#225532),(#225533,#225534),(#225535,#225536),
(#225537,#225538),(#225539,#225540),(#225541,#225542),(#225543,#225544),
(#225545,#225546),(#225547,#225548),(#225549,#225550),(#225551,#225552),
(#225553,#225554),(#225555,#225556),(#225557,#225558),(#225559,#225560),
(#225561,#225562),(#225563,#225564),(#225565,#225566),(#225567,#225568),
(#225569,#225570),(#225571,#225572),(#225573,#225574),(#225575,#225576),
(#225577,#225578),(#225579,#225580),(#225581,#225582),(#225583,#225584),
(#225585,#225586),(#225587,#225588),(#225589,#225590),(#225591,#225592),
(#225593,#225594),(#225595,#225596),(#225597,#225598),(#225599,#225600),
(#225601,#225602),(#225603,#225604),(#225605,#225606),(#225607,#225608),
(#225609,#225610),(#225611,#225612),(#225613,#225614),(#225615,#225616),
(#225617,#225618),(#225619,#225620),(#225621,#225622),(#225623,#225624),
(#225625,#225626),(#225627,#225628),(#225629,#225630),(#225631,#225632),
(#225633,#225634),(#225635,#225636),(#225637,#225638),(#225639,#225640),
(#225641,#225642),(#225643,#225644),(#225645,#225646),(#225647,#225648),
(#225649,#225650),(#225651,#225652),(#225653,#225654),(#225655,#225656),
(#225657,#225658),(#225659,#225660),(#225661,#225662),(#225663,#225664),
(#225665,#225666),(#225667,#225668),(#225669,#225670),(#225671,#225672),
(#225673,#225674),(#225675,#225676),(#225677,#225678),(#225679,#225680),
(#225681,#225682),(#225683,#225684),(#225685,#225686),(#225687,#225688),
(#225689,#225690),(#225691,#225692),(#225693,#225694),(#225695,#225696),
(#225697,#225698),(#225699,#225700),(#225701,#225702),(#225703,#225704),
(#225705,#225706),(#225707,#225708),(#225709,#225710),(#225711,#225712),
(#225713,#225714),(#225715,#225716),(#225717,#225718),(#225719,#225720),
(#225721,#225722),(#225723,#225724),(#225725,#225726),(#225727,#225728),
(#225729,#225730),(#225731,#225732),(#225733,#225734),(#225735,#225736),
(#225737,#225738),(#225739,#225740),(#225741,#225742),(#225743,#225744),
(#225745,#225746),(#225747,#225748),(#225749,#225750),(#225751,#225752),
(#225753,#225754),(#225755,#225756),(#225757,#225758),(#225759,#225760),
(#225761,#225762),(#225763,#225764),(#225765,#225766),(#225767,#225768),
(#225769,#225770),(#225771,#225772),(#225773,#225774),(#225775,#225776),
(#225777,#225778),(#225779,#225780),(#225781,#225782),(#225783,#225784),
(#225785,#225786),(#225787,#225788),(#225789,#225790),(#225791,#225792),
(#225793,#225794),(#225795,#225796),(#225797,#225798),(#225799,#225800),
(#225801,#225802),(#225803,#225804),(#225805,#225806),(#225807,#225808),
(#225809,#225810),(#225811,#225812),(#225813,#225814),(#225815,#225816),
(#225817,#225818),(#225819,#225820),(#225821,#225822),(#225823,#225824),
(#225825,#225826),(#225827,#225828),(#225829,#225830),(#225831,#225832),
(#225833,#225834),(#225835,#225836),(#225837,#225838),(#225839,#225840),
(#225841,#225842),(#225843,#225844),(#225845,#225846),(#225847,#225848),
(#225849,#225850),(#225851,#225852),(#225853,#225854),(#225855,#225856),
(#225857,#225858),(#225859,#225860),(#225861,#225862),(#225863,#225864),
(#225865,#225866),(#225867,#225868),(#225869,#225870),(#225871,#225872),
(#225873,#225874),(#225875,#225876),(#225877,#225878),(#225879,#225880),
(#225881,#225882),(#225883,#225884),(#225885,#225886),(#225887,#225888),
(#225889,#225890),(#225891,#225892),(#225893,#225894),(#225895,#225896),
(#225897,#225898),(#225899,#225900),(#225901,#225902),(#225903,#225904),
(#225905,#225906),(#225907,#225908),(#225909,#225910),(#225911,#225912),
(#225913,#225914),(#225915,#225916),(#225917,#225918),(#225919,#225920),
(#225921,#225922),(#225923,#225924),(#225925,#225926),(#225927,#225928),
(#225929,#225930),(#225931,#225932),(#225933,#225934),(#225935,#225936),
(#225937,#225938),(#225939,#225940),(#225941,#225942),(#225943,#225944),
(#225945,#225946),(#225947,#225948),(#225949,#225950),(#225951,#225952),
(#225953,#225954),(#225955,#225956),(#225957,#225958),(#225959,#225960),
(#225961,#225962),(#225963,#225964),(#225965,#225966),(#225967,#225968),
(#225969,#225970),(#225971,#225972),(#225973,#225974),(#225975,#225976),
(#225977,#225978),(#225979,#225980),(#225981,#225982),(#225983,#225984),
(#225985,#225986),(#225987,#225988),(#225989,#225990),(#225991,#225992),
(#225993,#225994),(#225995,#225996),(#225997,#225998),(#225999,#226000),
(#226001,#226002),(#226003,#226004),(#226005,#226006),(#226007,#226008),
(#226009,#226010),(#226011,#226012),(#226013,#226014),(#226015,#226016),
(#226017,#226018),(#226019,#226020),(#226021,#226022),(#226023,#226024),
(#226025,#226026),(#226027,#226028),(#226029,#226030),(#226031,#226032),
(#226033,#226034),(#226035,#226036),(#226037,#226038),(#226039,#226040),
(#226041,#226042),(#226043,#226044),(#226045,#226046),(#226047,#226048),
(#226049,#226050),(#226051,#226052),(#226053,#226054),(#226055,#226056),
(#226057,#226058),(#226059,#226060),(#226061,#226062),(#226063,#226064),
(#226065,#226066),(#226067,#226068),(#226069,#226070),(#226071,#226072),
(#226073,#226074),(#226075,#226076),(#226077,#226078),(#226079,#226080),
(#226081,#226082),(#226083,#226084),(#226085,#226086),(#226087,#226088),
(#226089,#226090),(#226091,#226092),(#226093,#226094),(#226095,#226096),
(#226097,#226098),(#226099,#226100),(#226101,#226102),(#226103,#226104),
(#226105,#226106),(#226107,#226108),(#226109,#226110),(#226111,#226112),
(#226113,#226114),(#226115,#226116),(#226117,#226118),(#226119,#226120),
(#226121,#226122),(#226123,#226124),(#226125,#226126),(#226127,#226128),
(#226129,#226130),(#226131,#226132),(#226133,#226134),(#226135,#226136),
(#226137,#226138),(#226139,#226140),(#226141,#226142),(#226143,#226144),
(#226145,#226146),(#226147,#226148),(#226149,#226150),(#226151,#226152),
(#226153,#226154),(#226155,#226156),(#226157,#226158),(#226159,#226160),
(#226161,#226162),(#226163,#226164),(#226165,#226166),(#226167,#226168),
(#226169,#226170),(#226171,#226172),(#226173,#226174),(#226175,#226176),
(#226177,#226178),(#226179,#226180),(#226181,#226182),(#226183,#226184),
(#226185,#226186),(#226187,#226188),(#226189,#226190),(#226191,#226192),
(#226193,#226194),(#226195,#226196),(#226197,#226198),(#226199,#226200),
(#226201,#226202),(#226203,#226204),(#226205,#226206),(#226207,#226208),
(#226209,#226210),(#226211,#226212),(#226213,#226214),(#226215,#226216),
(#226217,#226218),(#226219,#226220),(#226221,#226222),(#226223,#226224),
(#226225,#226226),(#226227,#226228),(#226229,#226230),(#226231,#226232),
(#226233,#226234),(#226235,#226236),(#226237,#226238),(#226239,#226240),
(#226241,#226242),(#226243,#226244),(#226245,#226246),(#226247,#226248),
(#226249,#226250),(#226251,#226252),(#226253,#226254),(#226255,#226256),
(#226257,#226258),(#226259,#226260),(#226261,#226262),(#226263,#226264),
(#226265,#226266),(#226267,#226268),(#226269,#226270),(#226271,#226272),
(#226273,#226274),(#226275,#226276),(#226277,#226278),(#226279,#226280),
(#226281,#226282),(#226283,#226284),(#226285,#226286),(#226287,#226288),
(#226289,#226290),(#226291,#226292),(#226293,#226294),(#226295,#226296),
(#226297,#226298),(#226299,#226300),(#226301,#226302),(#226303,#226304),
(#226305,#226306),(#226307,#226308),(#226309,#226310),(#226311,#226312),
(#226313,#226314),(#226315,#226316),(#226317,#226318),(#226319,#226320),
(#226321,#226322),(#226323,#226324),(#226325,#226326),(#226327,#226328),
(#226329,#226330),(#226331,#226332),(#226333,#226334),(#226335,#226336),
(#226337,#226338),(#226339,#226340),(#226341,#226342),(#226343,#226344),
(#226345,#226346),(#226347,#226348),(#226349,#226350),(#226351,#226352),
(#226353,#226354),(#226355,#226356),(#226357,#226358),(#226359,#226360),
(#226361,#226362),(#226363,#226364),(#226365,#226366),(#226367,#226368),
(#226369,#226370),(#226371,#226372),(#226373,#226374),(#226375,#226376),
(#226377,#226378),(#226379,#226380),(#226381,#226382),(#226383,#226384),
(#226385,#226386),(#226387,#226388),(#226389,#226390),(#226391,#226392),
(#226393,#226394),(#226395,#226396)),.UNSPECIFIED.,.F.,.F.,.F.,(6,1,1,1,
1,1,1,1,1,1,1,1,1,1,1,1,1,1,1,1,1,1,1,1,1,1,1,1,1,1,1,1,1,1,1,1,1,1,1,1,
1,1,1,1,1,1,1,1,1,1,1,1,1,1,1,1,1,1,1,1,1,1,1,1,1,1,1,1,1,1,1,1,1,1,1,1,
1,1,1,1,1,1,1,1,1,1,1,1,1,1,1,1,1,1,1,1,1,1,1,1,1,1,1,1,1,1,1,1,1,1,1,1,
1,1,1,1,1,1,1,1,1,1,1,1,1,1,1,1,1,1,1,1,1,1,1,1,1,1,1,1,1,1,1,1,1,1,1,1,
1,1,1,1,1,1,1,1,1,1,1,1,1,1,1,1,1,1,1,1,1,1,1,1,1,1,1,1,1,1,1,1,1,1,1,1,
1,1,1,1,1,1,1,1,1,1,1,1,1,1,1,1,1,1,1,1,1,1,1,1,1,1,1,1,1,1,1,1,1,1,1,1,
1,1,1,1,1,1,1,1,1,1,1,1,1,1,1,1,1,1,1,1,1,1,1,1,1,1,1,1,1,1,1,1,1,1,1,1,
1,1,1,1,1,1,1,1,1,1,1,1,1,1,1,1,1,1,1,1,1,1,1,1,1,1,1,1,1,1,1,1,1,1,1,1,
1,1,1,1,1,1,1,1,1,1,1,1,1,1,1,1,1,1,1,1,1,1,1,1,1,1,1,1,1,1,1,1,1,1,1,1,
1,1,1,1,1,1,1,1,1,1,1,1,1,1,1,1,1,1,1,1,1,1,1,1,1,1,1,1,1,1,1,1,1,1,1,1,
1,1,1,1,1,1,1,1,1,1,1,1,1,1,1,1,1,1,1,1,1,1,1,1,1,1,1,1,1,1,1,1,1,1,1,1,
1,1,1,1,1,1,1,1,1,1,1,1,1,1,1,1,1,1,1,1,1,1,1,1,1,1,1,1,1,1,1,1,1,1,1,1,
1,1,1,1,1,1,1,1,1,1,1,1,1,1,1,1,1,1,1,1,1,1,1,1,1,1,1,1,1,1,1,6),(2,2),
(0.143172104,0.144954128,0.146788991,0.148623853,0.150458716,0.152293578,
0.15412844,0.155963303,0.157798165,0.159633028,0.16146789,0.163302752,0.165137615,
0.166972477,0.168807339,0.170642202,0.172477064,0.174311927,0.176146789,
0.177981651,0.179816514,0.181651376,0.183486239,0.185321101,0.187155963,
0.188990826,0.190825688,0.19266055,0.194495413,0.196330275,0.198165138,
0.2,0.201834862,0.203669725,0.205504587,0.20733945,0.209174312,0.211009174,
0.212844037,0.214678899,0.216513761,0.218348624,0.220183486,0.222018349,
0.223853211,0.225688073,0.227522936,0.229357798,0.231192661,0.233027523,
0.234862385,0.236697248,0.23853211,0.240366972,0.242201835,0.244036697,
0.24587156,0.247706422,0.249541284,0.251376147,0.253211009,0.255045872,
0.256880734,0.258715596,0.260550459,0.262385321,0.264220183,0.266055046,
0.267889908,0.269724771,0.271559633,0.273394495,0.275229358,0.27706422,
0.278899083,0.280733945,0.282568807,0.28440367,0.286238532,0.288073394,
0.289908257,0.291743119,0.293577982,0.295412844,0.297247706,0.299082569,
0.300917431,0.302752294,0.304587156,0.306422018,0.308256881,0.310091743,
0.311926606,0.313761468,0.31559633,0.317431193,0.319266055,0.321100917,
0.32293578,0.324770642,0.326605505,0.328440367,0.330275229,0.332110092,
0.333944954,0.335779817,0.337614679,0.339449541,0.341284404,0.343119266,
0.344954128,0.346788991,0.348623853,0.350458716,0.352293578,0.35412844,
0.355963303,0.357798165,0.359633028,0.36146789,0.363302752,0.365137615,
0.366972477,0.368807339,0.370642202,0.372477064,0.374311927,0.376146789,
0.377981651,0.379816514,0.381651376,0.383486239,0.385321101,0.387155963,
0.388990826,0.390825688,0.39266055,0.394495413,0.396330275,0.398165138,
0.4,0.401834862,0.403669725,0.405504587,0.40733945,0.409174312,0.411009174,
0.412844037,0.414678899,0.416513761,0.418348624,0.420183486,0.422018349,
0.423853211,0.425688073,0.427522936,0.429357798,0.431192661,0.433027523,
0.434862385,0.436697248,0.43853211,0.440366972,0.442201835,0.444036697,
0.44587156,0.447706422,0.449541284,0.451376147,0.453211009,0.455045872,
0.456880734,0.458715596,0.460550459,0.462385321,0.464220183,0.466055046,
0.467889908,0.469724771,0.471559633,0.473394495,0.475229358,0.47706422,
0.478899083,0.480733945,0.482568807,0.48440367,0.486238532,0.488073394,
0.489908257,0.491743119,0.493577982,0.495412844,0.497247706,0.499082569,
0.500917431,0.502752294,0.504587156,0.506422018,0.508256881,0.510091743,
0.511926606,0.513761468,0.51559633,0.517431193,0.519266055,0.521100917,
0.52293578,0.524770642,0.526605505,0.528440367,0.530275229,0.532110092,
0.533944954,0.535779817,0.537614679,0.539449541,0.541284404,0.543119266,
0.544954128,0.546788991,0.548623853,0.550458716,0.552293578,0.55412844,
0.555963303,0.557798165,0.559633028,0.56146789,0.563302752,0.565137615,
0.566972477,0.568807339,0.570642202,0.572477064,0.574311927,0.576146789,
0.577981651,0.579816514,0.581651376,0.583486239,0.585321101,0.587155963,
0.588990826,0.590825688,0.59266055,0.594495413,0.596330275,0.598165138,
0.6,0.601834862,0.603669725,0.605504587,0.60733945,0.609174312,0.611009174,
0.612844037,0.614678899,0.616513761,0.618348624,0.620183486,0.622018349,
0.623853211,0.625688073,0.627522936,0.629357798,0.631192661,0.633027523,
0.634862385,0.636697248,0.63853211,0.640366972,0.642201835,0.644036697,
0.64587156,0.647706422,0.649541284,0.651376147,0.653211009,0.655045872,
0.656880734,0.658715596,0.660550459,0.662385321,0.664220183,0.666055046,
0.667889908,0.669724771,0.671559633,0.673394495,0.675229358,0.67706422,
0.678899083,0.680733945,0.682568807,0.68440367,0.686238532,0.688073394,
0.689908257,0.691743119,0.693577982,0.695412844,0.697247706,0.699082569,
0.700917431,0.702752294,0.704587156,0.706422018,0.708256881,0.710091743,
0.711926606,0.713761468,0.71559633,0.717431193,0.719266055,0.721100917,
0.72293578,0.724770642,0.726605505,0.728440367,0.730275229,0.732110092,
0.733944954,0.735779817,0.737614679,0.739449541,0.741284404,0.743119266,
0.744954128,0.746788991,0.748623853,0.750458716,0.752293578,0.75412844,
0.755963303,0.757798165,0.759633028,0.76146789,0.763302752,0.765137615,
0.766972477,0.768807339,0.770642202,0.772477064,0.774311927,0.776146789,
0.777981651,0.779816514,0.781651376,0.783486239,0.785321101,0.787155963,
0.788990826,0.790825688,0.79266055,0.794495413,0.796330275,0.798165138,
0.8,0.801834862,0.803669725,0.805504587,0.80733945,0.809174312,0.811009174,
0.812844037,0.814678899,0.816513761,0.818348624,0.820183486,0.822018349,
0.823853211,0.825688073,0.827522936,0.829357798,0.831192661,0.833027523,
0.834862385,0.836697248,0.83853211,0.840366972,0.842201835,0.844036697,
0.84587156,0.847706422,0.849541284,0.851376147,0.853211009,0.855045872,
0.856880734,0.858715596,0.860550459,0.862385321,0.864220183,0.866055046,
0.867889908,0.869724771,0.871559633,0.873394495,0.875229358,0.87706422,
0.878899083,0.880733945,0.882568807,0.88440367,0.886238532,0.888073394,
0.889908257,0.891743119,0.893577982,0.895412844,0.897247706,0.899082569,
0.900917431,0.902752294,0.904587156,0.906422018,0.908256881,0.910091743,
0.911926606,0.913761468,0.91559633,0.917431193,0.919266055,0.921100917,
0.92293578,0.924770642,0.926605505,0.928440367,0.930275229,0.932110092,
0.933944954,0.935779817,0.937614679,0.939449541,0.941284404,0.943119266,
0.944954128,0.946788991,0.948623853,0.950458716,0.952293578,0.95412844,
0.955963303,0.957798165,0.959633028,0.96146789,0.963302752,0.965137615,
0.966972477,0.968807339,0.970642202,0.972477064,0.974311927,0.976146789,
0.977981651,0.979816514,0.981651376,0.983486239,0.985321101,0.987155963,
0.988990826,0.990825688,0.99266055,0.994495413,0.996330275,0.998165138,
1.),(0.,0.36),.UNSPECIFIED.);
#6259=B_SPLINE_SURFACE_WITH_KNOTS('',5,1,((#227008,#227009),(#227010,#227011),
(#227012,#227013),(#227014,#227015),(#227016,#227017),(#227018,#227019),
(#227020,#227021),(#227022,#227023),(#227024,#227025),(#227026,#227027),
(#227028,#227029),(#227030,#227031),(#227032,#227033),(#227034,#227035),
(#227036,#227037),(#227038,#227039),(#227040,#227041),(#227042,#227043),
(#227044,#227045),(#227046,#227047),(#227048,#227049),(#227050,#227051),
(#227052,#227053),(#227054,#227055),(#227056,#227057),(#227058,#227059),
(#227060,#227061),(#227062,#227063),(#227064,#227065),(#227066,#227067),
(#227068,#227069),(#227070,#227071),(#227072,#227073),(#227074,#227075),
(#227076,#227077),(#227078,#227079),(#227080,#227081),(#227082,#227083),
(#227084,#227085),(#227086,#227087),(#227088,#227089),(#227090,#227091),
(#227092,#227093),(#227094,#227095),(#227096,#227097),(#227098,#227099),
(#227100,#227101),(#227102,#227103),(#227104,#227105),(#227106,#227107),
(#227108,#227109),(#227110,#227111),(#227112,#227113),(#227114,#227115),
(#227116,#227117),(#227118,#227119),(#227120,#227121),(#227122,#227123),
(#227124,#227125),(#227126,#227127),(#227128,#227129),(#227130,#227131),
(#227132,#227133),(#227134,#227135),(#227136,#227137),(#227138,#227139),
(#227140,#227141),(#227142,#227143),(#227144,#227145),(#227146,#227147),
(#227148,#227149),(#227150,#227151),(#227152,#227153),(#227154,#227155),
(#227156,#227157),(#227158,#227159),(#227160,#227161),(#227162,#227163),
(#227164,#227165),(#227166,#227167),(#227168,#227169),(#227170,#227171),
(#227172,#227173),(#227174,#227175),(#227176,#227177),(#227178,#227179),
(#227180,#227181),(#227182,#227183),(#227184,#227185),(#227186,#227187),
(#227188,#227189),(#227190,#227191),(#227192,#227193),(#227194,#227195),
(#227196,#227197),(#227198,#227199),(#227200,#227201),(#227202,#227203),
(#227204,#227205),(#227206,#227207),(#227208,#227209),(#227210,#227211),
(#227212,#227213),(#227214,#227215),(#227216,#227217),(#227218,#227219),
(#227220,#227221),(#227222,#227223),(#227224,#227225),(#227226,#227227),
(#227228,#227229),(#227230,#227231),(#227232,#227233),(#227234,#227235),
(#227236,#227237),(#227238,#227239),(#227240,#227241),(#227242,#227243),
(#227244,#227245),(#227246,#227247),(#227248,#227249),(#227250,#227251),
(#227252,#227253),(#227254,#227255),(#227256,#227257),(#227258,#227259),
(#227260,#227261),(#227262,#227263),(#227264,#227265),(#227266,#227267),
(#227268,#227269),(#227270,#227271),(#227272,#227273),(#227274,#227275),
(#227276,#227277),(#227278,#227279),(#227280,#227281),(#227282,#227283),
(#227284,#227285),(#227286,#227287),(#227288,#227289),(#227290,#227291),
(#227292,#227293),(#227294,#227295),(#227296,#227297),(#227298,#227299),
(#227300,#227301),(#227302,#227303),(#227304,#227305),(#227306,#227307),
(#227308,#227309),(#227310,#227311),(#227312,#227313),(#227314,#227315),
(#227316,#227317),(#227318,#227319),(#227320,#227321),(#227322,#227323),
(#227324,#227325),(#227326,#227327),(#227328,#227329),(#227330,#227331),
(#227332,#227333),(#227334,#227335),(#227336,#227337),(#227338,#227339),
(#227340,#227341),(#227342,#227343),(#227344,#227345),(#227346,#227347),
(#227348,#227349),(#227350,#227351),(#227352,#227353),(#227354,#227355),
(#227356,#227357),(#227358,#227359),(#227360,#227361),(#227362,#227363),
(#227364,#227365),(#227366,#227367),(#227368,#227369),(#227370,#227371),
(#227372,#227373),(#227374,#227375),(#227376,#227377),(#227378,#227379),
(#227380,#227381),(#227382,#227383),(#227384,#227385),(#227386,#227387),
(#227388,#227389),(#227390,#227391),(#227392,#227393),(#227394,#227395),
(#227396,#227397),(#227398,#227399),(#227400,#227401),(#227402,#227403),
(#227404,#227405),(#227406,#227407),(#227408,#227409),(#227410,#227411),
(#227412,#227413),(#227414,#227415),(#227416,#227417),(#227418,#227419),
(#227420,#227421),(#227422,#227423),(#227424,#227425),(#227426,#227427),
(#227428,#227429),(#227430,#227431),(#227432,#227433),(#227434,#227435),
(#227436,#227437),(#227438,#227439),(#227440,#227441),(#227442,#227443),
(#227444,#227445),(#227446,#227447),(#227448,#227449),(#227450,#227451),
(#227452,#227453),(#227454,#227455),(#227456,#227457),(#227458,#227459),
(#227460,#227461),(#227462,#227463),(#227464,#227465),(#227466,#227467),
(#227468,#227469),(#227470,#227471),(#227472,#227473),(#227474,#227475),
(#227476,#227477),(#227478,#227479),(#227480,#227481),(#227482,#227483),
(#227484,#227485),(#227486,#227487),(#227488,#227489),(#227490,#227491),
(#227492,#227493),(#227494,#227495),(#227496,#227497),(#227498,#227499),
(#227500,#227501),(#227502,#227503),(#227504,#227505),(#227506,#227507),
(#227508,#227509),(#227510,#227511),(#227512,#227513),(#227514,#227515),
(#227516,#227517),(#227518,#227519),(#227520,#227521),(#227522,#227523),
(#227524,#227525),(#227526,#227527),(#227528,#227529),(#227530,#227531),
(#227532,#227533),(#227534,#227535),(#227536,#227537),(#227538,#227539),
(#227540,#227541),(#227542,#227543),(#227544,#227545),(#227546,#227547),
(#227548,#227549),(#227550,#227551),(#227552,#227553),(#227554,#227555),
(#227556,#227557),(#227558,#227559),(#227560,#227561),(#227562,#227563),
(#227564,#227565),(#227566,#227567),(#227568,#227569),(#227570,#227571),
(#227572,#227573),(#227574,#227575),(#227576,#227577),(#227578,#227579),
(#227580,#227581),(#227582,#227583),(#227584,#227585),(#227586,#227587),
(#227588,#227589),(#227590,#227591),(#227592,#227593),(#227594,#227595),
(#227596,#227597),(#227598,#227599),(#227600,#227601),(#227602,#227603),
(#227604,#227605),(#227606,#227607),(#227608,#227609),(#227610,#227611),
(#227612,#227613),(#227614,#227615),(#227616,#227617),(#227618,#227619),
(#227620,#227621),(#227622,#227623),(#227624,#227625),(#227626,#227627),
(#227628,#227629),(#227630,#227631),(#227632,#227633),(#227634,#227635),
(#227636,#227637),(#227638,#227639),(#227640,#227641),(#227642,#227643),
(#227644,#227645),(#227646,#227647),(#227648,#227649),(#227650,#227651),
(#227652,#227653),(#227654,#227655),(#227656,#227657),(#227658,#227659),
(#227660,#227661),(#227662,#227663),(#227664,#227665),(#227666,#227667),
(#227668,#227669),(#227670,#227671),(#227672,#227673),(#227674,#227675),
(#227676,#227677),(#227678,#227679),(#227680,#227681),(#227682,#227683),
(#227684,#227685),(#227686,#227687),(#227688,#227689),(#227690,#227691),
(#227692,#227693),(#227694,#227695),(#227696,#227697),(#227698,#227699),
(#227700,#227701),(#227702,#227703),(#227704,#227705),(#227706,#227707),
(#227708,#227709),(#227710,#227711),(#227712,#227713),(#227714,#227715),
(#227716,#227717),(#227718,#227719),(#227720,#227721),(#227722,#227723),
(#227724,#227725),(#227726,#227727),(#227728,#227729),(#227730,#227731),
(#227732,#227733),(#227734,#227735),(#227736,#227737),(#227738,#227739),
(#227740,#227741),(#227742,#227743),(#227744,#227745),(#227746,#227747),
(#227748,#227749),(#227750,#227751),(#227752,#227753),(#227754,#227755),
(#227756,#227757),(#227758,#227759),(#227760,#227761),(#227762,#227763),
(#227764,#227765),(#227766,#227767),(#227768,#227769),(#227770,#227771),
(#227772,#227773),(#227774,#227775),(#227776,#227777),(#227778,#227779),
(#227780,#227781),(#227782,#227783),(#227784,#227785),(#227786,#227787),
(#227788,#227789),(#227790,#227791),(#227792,#227793),(#227794,#227795),
(#227796,#227797),(#227798,#227799),(#227800,#227801),(#227802,#227803),
(#227804,#227805),(#227806,#227807),(#227808,#227809),(#227810,#227811),
(#227812,#227813),(#227814,#227815),(#227816,#227817),(#227818,#227819),
(#227820,#227821),(#227822,#227823),(#227824,#227825),(#227826,#227827),
(#227828,#227829),(#227830,#227831),(#227832,#227833),(#227834,#227835),
(#227836,#227837),(#227838,#227839),(#227840,#227841),(#227842,#227843),
(#227844,#227845),(#227846,#227847),(#227848,#227849),(#227850,#227851),
(#227852,#227853),(#227854,#227855),(#227856,#227857),(#227858,#227859),
(#227860,#227861),(#227862,#227863),(#227864,#227865),(#227866,#227867),
(#227868,#227869),(#227870,#227871),(#227872,#227873),(#227874,#227875),
(#227876,#227877),(#227878,#227879),(#227880,#227881),(#227882,#227883),
(#227884,#227885),(#227886,#227887),(#227888,#227889),(#227890,#227891),
(#227892,#227893),(#227894,#227895),(#227896,#227897),(#227898,#227899),
(#227900,#227901),(#227902,#227903),(#227904,#227905),(#227906,#227907),
(#227908,#227909),(#227910,#227911),(#227912,#227913),(#227914,#227915),
(#227916,#227917),(#227918,#227919),(#227920,#227921),(#227922,#227923),
(#227924,#227925),(#227926,#227927),(#227928,#227929),(#227930,#227931),
(#227932,#227933),(#227934,#227935),(#227936,#227937),(#227938,#227939),
(#227940,#227941),(#227942,#227943),(#227944,#227945),(#227946,#227947),
(#227948,#227949),(#227950,#227951)),.UNSPECIFIED.,.F.,.F.,.F.,(6,1,1,1,
1,1,1,1,1,1,1,1,1,1,1,1,1,1,1,1,1,1,1,1,1,1,1,1,1,1,1,1,1,1,1,1,1,1,1,1,
1,1,1,1,1,1,1,1,1,1,1,1,1,1,1,1,1,1,1,1,1,1,1,1,1,1,1,1,1,1,1,1,1,1,1,1,
1,1,1,1,1,1,1,1,1,1,1,1,1,1,1,1,1,1,1,1,1,1,1,1,1,1,1,1,1,1,1,1,1,1,1,1,
1,1,1,1,1,1,1,1,1,1,1,1,1,1,1,1,1,1,1,1,1,1,1,1,1,1,1,1,1,1,1,1,1,1,1,1,
1,1,1,1,1,1,1,1,1,1,1,1,1,1,1,1,1,1,1,1,1,1,1,1,1,1,1,1,1,1,1,1,1,1,1,1,
1,1,1,1,1,1,1,1,1,1,1,1,1,1,1,1,1,1,1,1,1,1,1,1,1,1,1,1,1,1,1,1,1,1,1,1,
1,1,1,1,1,1,1,1,1,1,1,1,1,1,1,1,1,1,1,1,1,1,1,1,1,1,1,1,1,1,1,1,1,1,1,1,
1,1,1,1,1,1,1,1,1,1,1,1,1,1,1,1,1,1,1,1,1,1,1,1,1,1,1,1,1,1,1,1,1,1,1,1,
1,1,1,1,1,1,1,1,1,1,1,1,1,1,1,1,1,1,1,1,1,1,1,1,1,1,1,1,1,1,1,1,1,1,1,1,
1,1,1,1,1,1,1,1,1,1,1,1,1,1,1,1,1,1,1,1,1,1,1,1,1,1,1,1,1,1,1,1,1,1,1,1,
1,1,1,1,1,1,1,1,1,1,1,1,1,1,1,1,1,1,1,1,1,1,1,1,1,1,1,1,1,1,1,1,1,1,1,1,
1,1,1,1,1,1,1,1,1,1,1,1,1,1,1,1,1,1,1,1,1,1,1,1,1,1,1,1,1,1,1,1,1,1,1,1,
1,1,1,1,1,1,1,1,1,1,1,1,1,1,1,1,1,1,1,1,1,1,1,1,1,1,1,1,1,1,1,6),(2,2),
(0.143172103,0.144954128,0.146788991,0.148623853,0.150458716,0.152293578,
0.15412844,0.155963303,0.157798165,0.159633028,0.16146789,0.163302752,0.165137615,
0.166972477,0.168807339,0.170642202,0.172477064,0.174311927,0.176146789,
0.177981651,0.179816514,0.181651376,0.183486239,0.185321101,0.187155963,
0.188990826,0.190825688,0.19266055,0.194495413,0.196330275,0.198165138,
0.2,0.201834862,0.203669725,0.205504587,0.20733945,0.209174312,0.211009174,
0.212844037,0.214678899,0.216513761,0.218348624,0.220183486,0.222018349,
0.223853211,0.225688073,0.227522936,0.229357798,0.231192661,0.233027523,
0.234862385,0.236697248,0.23853211,0.240366972,0.242201835,0.244036697,
0.24587156,0.247706422,0.249541284,0.251376147,0.253211009,0.255045872,
0.256880734,0.258715596,0.260550459,0.262385321,0.264220183,0.266055046,
0.267889908,0.269724771,0.271559633,0.273394495,0.275229358,0.27706422,
0.278899083,0.280733945,0.282568807,0.28440367,0.286238532,0.288073394,
0.289908257,0.291743119,0.293577982,0.295412844,0.297247706,0.299082569,
0.300917431,0.302752294,0.304587156,0.306422018,0.308256881,0.310091743,
0.311926606,0.313761468,0.31559633,0.317431193,0.319266055,0.321100917,
0.32293578,0.324770642,0.326605505,0.328440367,0.330275229,0.332110092,
0.333944954,0.335779817,0.337614679,0.339449541,0.341284404,0.343119266,
0.344954128,0.346788991,0.348623853,0.350458716,0.352293578,0.35412844,
0.355963303,0.357798165,0.359633028,0.36146789,0.363302752,0.365137615,
0.366972477,0.368807339,0.370642202,0.372477064,0.374311927,0.376146789,
0.377981651,0.379816514,0.381651376,0.383486239,0.385321101,0.387155963,
0.388990826,0.390825688,0.39266055,0.394495413,0.396330275,0.398165138,
0.4,0.401834862,0.403669725,0.405504587,0.40733945,0.409174312,0.411009174,
0.412844037,0.414678899,0.416513761,0.418348624,0.420183486,0.422018349,
0.423853211,0.425688073,0.427522936,0.429357798,0.431192661,0.433027523,
0.434862385,0.436697248,0.43853211,0.440366972,0.442201835,0.444036697,
0.44587156,0.447706422,0.449541284,0.451376147,0.453211009,0.455045872,
0.456880734,0.458715596,0.460550459,0.462385321,0.464220183,0.466055046,
0.467889908,0.469724771,0.471559633,0.473394495,0.475229358,0.47706422,
0.478899083,0.480733945,0.482568807,0.48440367,0.486238532,0.488073394,
0.489908257,0.491743119,0.493577982,0.495412844,0.497247706,0.499082569,
0.500917431,0.502752294,0.504587156,0.506422018,0.508256881,0.510091743,
0.511926606,0.513761468,0.51559633,0.517431193,0.519266055,0.521100917,
0.52293578,0.524770642,0.526605505,0.528440367,0.530275229,0.532110092,
0.533944954,0.535779817,0.537614679,0.539449541,0.541284404,0.543119266,
0.544954128,0.546788991,0.548623853,0.550458716,0.552293578,0.55412844,
0.555963303,0.557798165,0.559633028,0.56146789,0.563302752,0.565137615,
0.566972477,0.568807339,0.570642202,0.572477064,0.574311927,0.576146789,
0.577981651,0.579816514,0.581651376,0.583486239,0.585321101,0.587155963,
0.588990826,0.590825688,0.59266055,0.594495413,0.596330275,0.598165138,
0.6,0.601834862,0.603669725,0.605504587,0.60733945,0.609174312,0.611009174,
0.612844037,0.614678899,0.616513761,0.618348624,0.620183486,0.622018349,
0.623853211,0.625688073,0.627522936,0.629357798,0.631192661,0.633027523,
0.634862385,0.636697248,0.63853211,0.640366972,0.642201835,0.644036697,
0.64587156,0.647706422,0.649541284,0.651376147,0.653211009,0.655045872,
0.656880734,0.658715596,0.660550459,0.662385321,0.664220183,0.666055046,
0.667889908,0.669724771,0.671559633,0.673394495,0.675229358,0.67706422,
0.678899083,0.680733945,0.682568807,0.68440367,0.686238532,0.688073394,
0.689908257,0.691743119,0.693577982,0.695412844,0.697247706,0.699082569,
0.700917431,0.702752294,0.704587156,0.706422018,0.708256881,0.710091743,
0.711926606,0.713761468,0.71559633,0.717431193,0.719266055,0.721100917,
0.72293578,0.724770642,0.726605505,0.728440367,0.730275229,0.732110092,
0.733944954,0.735779817,0.737614679,0.739449541,0.741284404,0.743119266,
0.744954128,0.746788991,0.748623853,0.750458716,0.752293578,0.75412844,
0.755963303,0.757798165,0.759633028,0.76146789,0.763302752,0.765137615,
0.766972477,0.768807339,0.770642202,0.772477064,0.774311927,0.776146789,
0.777981651,0.779816514,0.781651376,0.783486239,0.785321101,0.787155963,
0.788990826,0.790825688,0.79266055,0.794495413,0.796330275,0.798165138,
0.8,0.801834862,0.803669725,0.805504587,0.80733945,0.809174312,0.811009174,
0.812844037,0.814678899,0.816513761,0.818348624,0.820183486,0.822018349,
0.823853211,0.825688073,0.827522936,0.829357798,0.831192661,0.833027523,
0.834862385,0.836697248,0.83853211,0.840366972,0.842201835,0.844036697,
0.84587156,0.847706422,0.849541284,0.851376147,0.853211009,0.855045872,
0.856880734,0.858715596,0.860550459,0.862385321,0.864220183,0.866055046,
0.867889908,0.869724771,0.871559633,0.873394495,0.875229358,0.87706422,
0.878899083,0.880733945,0.882568807,0.88440367,0.886238532,0.888073394,
0.889908257,0.891743119,0.893577982,0.895412844,0.897247706,0.899082569,
0.900917431,0.902752294,0.904587156,0.906422018,0.908256881,0.910091743,
0.911926606,0.913761468,0.91559633,0.917431193,0.919266055,0.921100917,
0.92293578,0.924770642,0.926605505,0.928440367,0.930275229,0.932110092,
0.933944954,0.935779817,0.937614679,0.939449541,0.941284404,0.943119266,
0.944954128,0.946788991,0.948623853,0.950458716,0.952293578,0.95412844,
0.955963303,0.957798165,0.959633028,0.96146789,0.963302752,0.965137615,
0.966972477,0.968807339,0.970642202,0.972477064,0.974311927,0.976146789,
0.977981651,0.979816514,0.981651376,0.983486239,0.985321101,0.987155963,
0.988990826,0.990825688,0.99266055,0.994495413,0.996330275,0.998165138,
1.),(0.,0.36),.UNSPECIFIED.);
#6260=B_SPLINE_SURFACE_WITH_KNOTS('',5,1,((#228575,#228576),(#228577,#228578),
(#228579,#228580),(#228581,#228582),(#228583,#228584),(#228585,#228586),
(#228587,#228588),(#228589,#228590),(#228591,#228592),(#228593,#228594),
(#228595,#228596),(#228597,#228598),(#228599,#228600),(#228601,#228602),
(#228603,#228604),(#228605,#228606),(#228607,#228608),(#228609,#228610),
(#228611,#228612),(#228613,#228614),(#228615,#228616),(#228617,#228618),
(#228619,#228620),(#228621,#228622),(#228623,#228624),(#228625,#228626),
(#228627,#228628),(#228629,#228630),(#228631,#228632),(#228633,#228634),
(#228635,#228636),(#228637,#228638),(#228639,#228640),(#228641,#228642),
(#228643,#228644),(#228645,#228646),(#228647,#228648),(#228649,#228650),
(#228651,#228652),(#228653,#228654),(#228655,#228656),(#228657,#228658),
(#228659,#228660),(#228661,#228662),(#228663,#228664),(#228665,#228666),
(#228667,#228668),(#228669,#228670),(#228671,#228672),(#228673,#228674),
(#228675,#228676),(#228677,#228678),(#228679,#228680),(#228681,#228682),
(#228683,#228684),(#228685,#228686),(#228687,#228688),(#228689,#228690),
(#228691,#228692),(#228693,#228694),(#228695,#228696),(#228697,#228698),
(#228699,#228700),(#228701,#228702),(#228703,#228704),(#228705,#228706),
(#228707,#228708),(#228709,#228710),(#228711,#228712),(#228713,#228714),
(#228715,#228716),(#228717,#228718),(#228719,#228720),(#228721,#228722),
(#228723,#228724),(#228725,#228726),(#228727,#228728),(#228729,#228730),
(#228731,#228732),(#228733,#228734),(#228735,#228736),(#228737,#228738),
(#228739,#228740),(#228741,#228742),(#228743,#228744),(#228745,#228746),
(#228747,#228748),(#228749,#228750),(#228751,#228752),(#228753,#228754),
(#228755,#228756),(#228757,#228758),(#228759,#228760),(#228761,#228762),
(#228763,#228764),(#228765,#228766),(#228767,#228768),(#228769,#228770),
(#228771,#228772),(#228773,#228774),(#228775,#228776),(#228777,#228778),
(#228779,#228780),(#228781,#228782),(#228783,#228784),(#228785,#228786),
(#228787,#228788),(#228789,#228790),(#228791,#228792),(#228793,#228794),
(#228795,#228796),(#228797,#228798),(#228799,#228800),(#228801,#228802),
(#228803,#228804),(#228805,#228806),(#228807,#228808),(#228809,#228810),
(#228811,#228812),(#228813,#228814),(#228815,#228816),(#228817,#228818),
(#228819,#228820),(#228821,#228822),(#228823,#228824),(#228825,#228826),
(#228827,#228828),(#228829,#228830),(#228831,#228832),(#228833,#228834),
(#228835,#228836),(#228837,#228838),(#228839,#228840),(#228841,#228842),
(#228843,#228844),(#228845,#228846),(#228847,#228848),(#228849,#228850),
(#228851,#228852),(#228853,#228854),(#228855,#228856),(#228857,#228858),
(#228859,#228860),(#228861,#228862),(#228863,#228864),(#228865,#228866),
(#228867,#228868),(#228869,#228870),(#228871,#228872),(#228873,#228874),
(#228875,#228876),(#228877,#228878),(#228879,#228880),(#228881,#228882),
(#228883,#228884),(#228885,#228886),(#228887,#228888),(#228889,#228890),
(#228891,#228892),(#228893,#228894),(#228895,#228896),(#228897,#228898),
(#228899,#228900),(#228901,#228902),(#228903,#228904),(#228905,#228906),
(#228907,#228908),(#228909,#228910),(#228911,#228912),(#228913,#228914),
(#228915,#228916),(#228917,#228918),(#228919,#228920),(#228921,#228922),
(#228923,#228924),(#228925,#228926),(#228927,#228928),(#228929,#228930),
(#228931,#228932),(#228933,#228934),(#228935,#228936),(#228937,#228938),
(#228939,#228940),(#228941,#228942),(#228943,#228944),(#228945,#228946),
(#228947,#228948),(#228949,#228950),(#228951,#228952),(#228953,#228954),
(#228955,#228956),(#228957,#228958),(#228959,#228960),(#228961,#228962),
(#228963,#228964),(#228965,#228966),(#228967,#228968),(#228969,#228970),
(#228971,#228972),(#228973,#228974),(#228975,#228976),(#228977,#228978),
(#228979,#228980),(#228981,#228982),(#228983,#228984),(#228985,#228986),
(#228987,#228988),(#228989,#228990),(#228991,#228992),(#228993,#228994),
(#228995,#228996),(#228997,#228998),(#228999,#229000),(#229001,#229002),
(#229003,#229004),(#229005,#229006),(#229007,#229008),(#229009,#229010),
(#229011,#229012),(#229013,#229014),(#229015,#229016),(#229017,#229018),
(#229019,#229020),(#229021,#229022),(#229023,#229024),(#229025,#229026),
(#229027,#229028),(#229029,#229030),(#229031,#229032),(#229033,#229034),
(#229035,#229036),(#229037,#229038),(#229039,#229040),(#229041,#229042),
(#229043,#229044),(#229045,#229046),(#229047,#229048),(#229049,#229050),
(#229051,#229052),(#229053,#229054),(#229055,#229056),(#229057,#229058),
(#229059,#229060),(#229061,#229062),(#229063,#229064),(#229065,#229066),
(#229067,#229068),(#229069,#229070),(#229071,#229072),(#229073,#229074),
(#229075,#229076),(#229077,#229078),(#229079,#229080),(#229081,#229082),
(#229083,#229084),(#229085,#229086),(#229087,#229088),(#229089,#229090),
(#229091,#229092),(#229093,#229094),(#229095,#229096),(#229097,#229098),
(#229099,#229100),(#229101,#229102),(#229103,#229104),(#229105,#229106),
(#229107,#229108),(#229109,#229110),(#229111,#229112),(#229113,#229114),
(#229115,#229116),(#229117,#229118),(#229119,#229120),(#229121,#229122),
(#229123,#229124),(#229125,#229126),(#229127,#229128),(#229129,#229130),
(#229131,#229132),(#229133,#229134),(#229135,#229136),(#229137,#229138),
(#229139,#229140),(#229141,#229142),(#229143,#229144),(#229145,#229146),
(#229147,#229148),(#229149,#229150),(#229151,#229152),(#229153,#229154),
(#229155,#229156),(#229157,#229158),(#229159,#229160),(#229161,#229162),
(#229163,#229164),(#229165,#229166),(#229167,#229168),(#229169,#229170),
(#229171,#229172),(#229173,#229174),(#229175,#229176),(#229177,#229178),
(#229179,#229180),(#229181,#229182),(#229183,#229184),(#229185,#229186),
(#229187,#229188),(#229189,#229190),(#229191,#229192),(#229193,#229194),
(#229195,#229196),(#229197,#229198),(#229199,#229200),(#229201,#229202),
(#229203,#229204),(#229205,#229206),(#229207,#229208),(#229209,#229210),
(#229211,#229212),(#229213,#229214),(#229215,#229216),(#229217,#229218),
(#229219,#229220),(#229221,#229222),(#229223,#229224),(#229225,#229226),
(#229227,#229228),(#229229,#229230),(#229231,#229232),(#229233,#229234),
(#229235,#229236),(#229237,#229238),(#229239,#229240),(#229241,#229242),
(#229243,#229244),(#229245,#229246),(#229247,#229248),(#229249,#229250),
(#229251,#229252),(#229253,#229254),(#229255,#229256),(#229257,#229258),
(#229259,#229260),(#229261,#229262),(#229263,#229264),(#229265,#229266),
(#229267,#229268),(#229269,#229270),(#229271,#229272),(#229273,#229274),
(#229275,#229276),(#229277,#229278),(#229279,#229280),(#229281,#229282),
(#229283,#229284),(#229285,#229286),(#229287,#229288),(#229289,#229290),
(#229291,#229292),(#229293,#229294),(#229295,#229296),(#229297,#229298),
(#229299,#229300),(#229301,#229302),(#229303,#229304),(#229305,#229306),
(#229307,#229308),(#229309,#229310),(#229311,#229312),(#229313,#229314),
(#229315,#229316),(#229317,#229318),(#229319,#229320),(#229321,#229322),
(#229323,#229324),(#229325,#229326),(#229327,#229328),(#229329,#229330),
(#229331,#229332),(#229333,#229334),(#229335,#229336),(#229337,#229338),
(#229339,#229340),(#229341,#229342),(#229343,#229344),(#229345,#229346),
(#229347,#229348),(#229349,#229350),(#229351,#229352),(#229353,#229354),
(#229355,#229356),(#229357,#229358),(#229359,#229360),(#229361,#229362),
(#229363,#229364),(#229365,#229366),(#229367,#229368),(#229369,#229370),
(#229371,#229372),(#229373,#229374),(#229375,#229376),(#229377,#229378),
(#229379,#229380),(#229381,#229382),(#229383,#229384),(#229385,#229386),
(#229387,#229388),(#229389,#229390),(#229391,#229392),(#229393,#229394),
(#229395,#229396),(#229397,#229398),(#229399,#229400),(#229401,#229402),
(#229403,#229404),(#229405,#229406),(#229407,#229408),(#229409,#229410),
(#229411,#229412),(#229413,#229414),(#229415,#229416),(#229417,#229418),
(#229419,#229420),(#229421,#229422),(#229423,#229424),(#229425,#229426),
(#229427,#229428),(#229429,#229430),(#229431,#229432),(#229433,#229434),
(#229435,#229436),(#229437,#229438),(#229439,#229440),(#229441,#229442),
(#229443,#229444),(#229445,#229446),(#229447,#229448),(#229449,#229450),
(#229451,#229452),(#229453,#229454),(#229455,#229456),(#229457,#229458),
(#229459,#229460),(#229461,#229462),(#229463,#229464),(#229465,#229466),
(#229467,#229468),(#229469,#229470),(#229471,#229472),(#229473,#229474),
(#229475,#229476),(#229477,#229478),(#229479,#229480),(#229481,#229482),
(#229483,#229484),(#229485,#229486),(#229487,#229488),(#229489,#229490),
(#229491,#229492),(#229493,#229494),(#229495,#229496),(#229497,#229498),
(#229499,#229500),(#229501,#229502),(#229503,#229504),(#229505,#229506),
(#229507,#229508),(#229509,#229510),(#229511,#229512),(#229513,#229514),
(#229515,#229516),(#229517,#229518)),.UNSPECIFIED.,.F.,.F.,.F.,(6,1,1,1,
1,1,1,1,1,1,1,1,1,1,1,1,1,1,1,1,1,1,1,1,1,1,1,1,1,1,1,1,1,1,1,1,1,1,1,1,
1,1,1,1,1,1,1,1,1,1,1,1,1,1,1,1,1,1,1,1,1,1,1,1,1,1,1,1,1,1,1,1,1,1,1,1,
1,1,1,1,1,1,1,1,1,1,1,1,1,1,1,1,1,1,1,1,1,1,1,1,1,1,1,1,1,1,1,1,1,1,1,1,
1,1,1,1,1,1,1,1,1,1,1,1,1,1,1,1,1,1,1,1,1,1,1,1,1,1,1,1,1,1,1,1,1,1,1,1,
1,1,1,1,1,1,1,1,1,1,1,1,1,1,1,1,1,1,1,1,1,1,1,1,1,1,1,1,1,1,1,1,1,1,1,1,
1,1,1,1,1,1,1,1,1,1,1,1,1,1,1,1,1,1,1,1,1,1,1,1,1,1,1,1,1,1,1,1,1,1,1,1,
1,1,1,1,1,1,1,1,1,1,1,1,1,1,1,1,1,1,1,1,1,1,1,1,1,1,1,1,1,1,1,1,1,1,1,1,
1,1,1,1,1,1,1,1,1,1,1,1,1,1,1,1,1,1,1,1,1,1,1,1,1,1,1,1,1,1,1,1,1,1,1,1,
1,1,1,1,1,1,1,1,1,1,1,1,1,1,1,1,1,1,1,1,1,1,1,1,1,1,1,1,1,1,1,1,1,1,1,1,
1,1,1,1,1,1,1,1,1,1,1,1,1,1,1,1,1,1,1,1,1,1,1,1,1,1,1,1,1,1,1,1,1,1,1,1,
1,1,1,1,1,1,1,1,1,1,1,1,1,1,1,1,1,1,1,1,1,1,1,1,1,1,1,1,1,1,1,1,1,1,1,1,
1,1,1,1,1,1,1,1,1,1,1,1,1,1,1,1,1,1,1,1,1,1,1,1,1,1,1,1,1,1,1,1,1,1,1,1,
1,1,1,1,1,1,1,1,1,1,1,1,1,1,1,1,1,1,1,1,1,1,1,1,1,1,1,1,1,1,1,6),(2,2),
(-1.,-0.998165138,-0.996330275,-0.994495413,-0.99266055,-0.990825688,-0.988990826,
-0.987155963,-0.985321101,-0.983486239,-0.981651376,-0.979816514,-0.977981651,
-0.976146789,-0.974311927,-0.972477064,-0.970642202,-0.968807339,-0.966972477,
-0.965137615,-0.963302752,-0.96146789,-0.959633028,-0.957798165,-0.955963303,
-0.95412844,-0.952293578,-0.950458716,-0.948623853,-0.946788991,-0.944954128,
-0.943119266,-0.941284404,-0.939449541,-0.937614679,-0.935779817,-0.933944954,
-0.932110092,-0.930275229,-0.928440367,-0.926605505,-0.924770642,-0.92293578,
-0.921100917,-0.919266055,-0.917431193,-0.91559633,-0.913761468,-0.911926606,
-0.910091743,-0.908256881,-0.906422018,-0.904587156,-0.902752294,-0.900917431,
-0.899082569,-0.897247706,-0.895412844,-0.893577982,-0.891743119,-0.889908257,
-0.888073394,-0.886238532,-0.88440367,-0.882568807,-0.880733945,-0.878899083,
-0.87706422,-0.875229358,-0.873394495,-0.871559633,-0.869724771,-0.867889908,
-0.866055046,-0.864220183,-0.862385321,-0.860550459,-0.858715596,-0.856880734,
-0.855045872,-0.853211009,-0.851376147,-0.849541284,-0.847706422,-0.84587156,
-0.844036697,-0.842201835,-0.840366972,-0.83853211,-0.836697248,-0.834862385,
-0.833027523,-0.831192661,-0.829357798,-0.827522936,-0.825688073,-0.823853211,
-0.822018349,-0.820183486,-0.818348624,-0.816513761,-0.814678899,-0.812844037,
-0.811009174,-0.809174312,-0.80733945,-0.805504587,-0.803669725,-0.801834862,
-0.8,-0.798165138,-0.796330275,-0.794495413,-0.79266055,-0.790825688,-0.788990826,
-0.787155963,-0.785321101,-0.783486239,-0.781651376,-0.779816514,-0.777981651,
-0.776146789,-0.774311927,-0.772477064,-0.770642202,-0.768807339,-0.766972477,
-0.765137615,-0.763302752,-0.76146789,-0.759633028,-0.757798165,-0.755963303,
-0.75412844,-0.752293578,-0.750458716,-0.748623853,-0.746788991,-0.744954128,
-0.743119266,-0.741284404,-0.739449541,-0.737614679,-0.735779817,-0.733944954,
-0.732110092,-0.730275229,-0.728440367,-0.726605505,-0.724770642,-0.72293578,
-0.721100917,-0.719266055,-0.717431193,-0.71559633,-0.713761468,-0.711926606,
-0.710091743,-0.708256881,-0.706422018,-0.704587156,-0.702752294,-0.700917431,
-0.699082569,-0.697247706,-0.695412844,-0.693577982,-0.691743119,-0.689908257,
-0.688073394,-0.686238532,-0.68440367,-0.682568807,-0.680733945,-0.678899083,
-0.67706422,-0.675229358,-0.673394495,-0.671559633,-0.669724771,-0.667889908,
-0.666055046,-0.664220183,-0.662385321,-0.660550459,-0.658715596,-0.656880734,
-0.655045872,-0.653211009,-0.651376147,-0.649541284,-0.647706422,-0.64587156,
-0.644036697,-0.642201835,-0.640366972,-0.63853211,-0.636697248,-0.634862385,
-0.633027523,-0.631192661,-0.629357798,-0.627522936,-0.625688073,-0.623853211,
-0.622018349,-0.620183486,-0.618348624,-0.616513761,-0.614678899,-0.612844037,
-0.611009174,-0.609174312,-0.60733945,-0.605504587,-0.603669725,-0.601834862,
-0.6,-0.598165138,-0.596330275,-0.594495413,-0.59266055,-0.590825688,-0.588990826,
-0.587155963,-0.585321101,-0.583486239,-0.581651376,-0.579816514,-0.577981651,
-0.576146789,-0.574311927,-0.572477064,-0.570642202,-0.568807339,-0.566972477,
-0.565137615,-0.563302752,-0.56146789,-0.559633028,-0.557798165,-0.555963303,
-0.55412844,-0.552293578,-0.550458716,-0.548623853,-0.546788991,-0.544954128,
-0.543119266,-0.541284404,-0.539449541,-0.537614679,-0.535779817,-0.533944954,
-0.532110092,-0.530275229,-0.528440367,-0.526605505,-0.524770642,-0.52293578,
-0.521100917,-0.519266055,-0.517431193,-0.51559633,-0.513761468,-0.511926606,
-0.510091743,-0.508256881,-0.506422018,-0.504587156,-0.502752294,-0.500917431,
-0.499082569,-0.497247706,-0.495412844,-0.493577982,-0.491743119,-0.489908257,
-0.488073394,-0.486238532,-0.48440367,-0.482568807,-0.480733945,-0.478899083,
-0.47706422,-0.475229358,-0.473394495,-0.471559633,-0.469724771,-0.467889908,
-0.466055046,-0.464220183,-0.462385321,-0.460550459,-0.458715596,-0.456880734,
-0.455045872,-0.453211009,-0.451376147,-0.449541284,-0.447706422,-0.44587156,
-0.444036697,-0.442201835,-0.440366972,-0.43853211,-0.436697248,-0.434862385,
-0.433027523,-0.431192661,-0.429357798,-0.427522936,-0.425688073,-0.423853211,
-0.422018349,-0.420183486,-0.418348624,-0.416513761,-0.414678899,-0.412844037,
-0.411009174,-0.409174312,-0.40733945,-0.405504587,-0.403669725,-0.401834862,
-0.4,-0.398165138,-0.396330275,-0.394495413,-0.39266055,-0.390825688,-0.388990826,
-0.387155963,-0.385321101,-0.383486239,-0.381651376,-0.379816514,-0.377981651,
-0.376146789,-0.374311927,-0.372477064,-0.370642202,-0.368807339,-0.366972477,
-0.365137615,-0.363302752,-0.36146789,-0.359633028,-0.357798165,-0.355963303,
-0.35412844,-0.352293578,-0.350458716,-0.348623853,-0.346788991,-0.344954128,
-0.343119266,-0.341284404,-0.339449541,-0.337614679,-0.335779817,-0.333944954,
-0.332110092,-0.330275229,-0.328440367,-0.326605505,-0.324770642,-0.32293578,
-0.321100917,-0.319266055,-0.317431193,-0.31559633,-0.313761468,-0.311926606,
-0.310091743,-0.308256881,-0.306422018,-0.304587156,-0.302752294,-0.300917431,
-0.299082569,-0.297247706,-0.295412844,-0.293577982,-0.291743119,-0.289908257,
-0.288073394,-0.286238532,-0.28440367,-0.282568807,-0.280733945,-0.278899083,
-0.27706422,-0.275229358,-0.273394495,-0.271559633,-0.269724771,-0.267889908,
-0.266055046,-0.264220183,-0.262385321,-0.260550459,-0.258715596,-0.256880734,
-0.255045872,-0.253211009,-0.251376147,-0.249541284,-0.247706422,-0.24587156,
-0.244036697,-0.242201835,-0.240366972,-0.23853211,-0.236697248,-0.234862385,
-0.233027523,-0.231192661,-0.229357798,-0.227522936,-0.225688073,-0.223853211,
-0.222018349,-0.220183486,-0.218348624,-0.216513761,-0.214678899,-0.212844037,
-0.211009174,-0.209174312,-0.20733945,-0.205504587,-0.203669725,-0.201834862,
-0.2,-0.198165138,-0.196330275,-0.194495413,-0.19266055,-0.190825688,-0.188990826,
-0.187155963,-0.185321101,-0.183486239,-0.181651376,-0.179816514,-0.177981651,
-0.176146789,-0.174311927,-0.172477064,-0.170642202,-0.168807339,-0.166972477,
-0.165137615,-0.163302752,-0.16146789,-0.159633028,-0.157798165,-0.155963303,
-0.15412844,-0.152293578,-0.150458716,-0.148623853,-0.146788991,-0.144954128,
-0.143172103),(0.,0.36),.UNSPECIFIED.);
#6261=B_SPLINE_SURFACE_WITH_KNOTS('',5,1,((#230148,#230149),(#230150,#230151),
(#230152,#230153),(#230154,#230155),(#230156,#230157),(#230158,#230159),
(#230160,#230161),(#230162,#230163),(#230164,#230165),(#230166,#230167),
(#230168,#230169),(#230170,#230171),(#230172,#230173),(#230174,#230175),
(#230176,#230177),(#230178,#230179),(#230180,#230181),(#230182,#230183),
(#230184,#230185),(#230186,#230187),(#230188,#230189),(#230190,#230191),
(#230192,#230193),(#230194,#230195),(#230196,#230197),(#230198,#230199),
(#230200,#230201),(#230202,#230203),(#230204,#230205),(#230206,#230207),
(#230208,#230209),(#230210,#230211),(#230212,#230213),(#230214,#230215),
(#230216,#230217),(#230218,#230219),(#230220,#230221),(#230222,#230223),
(#230224,#230225),(#230226,#230227),(#230228,#230229),(#230230,#230231),
(#230232,#230233),(#230234,#230235),(#230236,#230237),(#230238,#230239),
(#230240,#230241),(#230242,#230243),(#230244,#230245),(#230246,#230247),
(#230248,#230249),(#230250,#230251),(#230252,#230253),(#230254,#230255),
(#230256,#230257),(#230258,#230259),(#230260,#230261),(#230262,#230263),
(#230264,#230265),(#230266,#230267),(#230268,#230269),(#230270,#230271),
(#230272,#230273),(#230274,#230275),(#230276,#230277),(#230278,#230279),
(#230280,#230281),(#230282,#230283),(#230284,#230285),(#230286,#230287),
(#230288,#230289),(#230290,#230291),(#230292,#230293),(#230294,#230295),
(#230296,#230297),(#230298,#230299),(#230300,#230301),(#230302,#230303),
(#230304,#230305),(#230306,#230307),(#230308,#230309),(#230310,#230311),
(#230312,#230313),(#230314,#230315),(#230316,#230317),(#230318,#230319),
(#230320,#230321),(#230322,#230323),(#230324,#230325),(#230326,#230327),
(#230328,#230329),(#230330,#230331),(#230332,#230333),(#230334,#230335),
(#230336,#230337),(#230338,#230339),(#230340,#230341),(#230342,#230343),
(#230344,#230345),(#230346,#230347),(#230348,#230349),(#230350,#230351),
(#230352,#230353),(#230354,#230355),(#230356,#230357),(#230358,#230359),
(#230360,#230361),(#230362,#230363),(#230364,#230365),(#230366,#230367),
(#230368,#230369),(#230370,#230371),(#230372,#230373),(#230374,#230375),
(#230376,#230377),(#230378,#230379),(#230380,#230381),(#230382,#230383),
(#230384,#230385),(#230386,#230387),(#230388,#230389),(#230390,#230391),
(#230392,#230393),(#230394,#230395),(#230396,#230397),(#230398,#230399),
(#230400,#230401),(#230402,#230403),(#230404,#230405),(#230406,#230407),
(#230408,#230409),(#230410,#230411),(#230412,#230413),(#230414,#230415),
(#230416,#230417),(#230418,#230419),(#230420,#230421),(#230422,#230423),
(#230424,#230425),(#230426,#230427),(#230428,#230429),(#230430,#230431),
(#230432,#230433),(#230434,#230435),(#230436,#230437),(#230438,#230439),
(#230440,#230441),(#230442,#230443),(#230444,#230445),(#230446,#230447),
(#230448,#230449),(#230450,#230451),(#230452,#230453),(#230454,#230455),
(#230456,#230457),(#230458,#230459),(#230460,#230461),(#230462,#230463),
(#230464,#230465),(#230466,#230467),(#230468,#230469),(#230470,#230471),
(#230472,#230473),(#230474,#230475),(#230476,#230477),(#230478,#230479),
(#230480,#230481),(#230482,#230483),(#230484,#230485),(#230486,#230487),
(#230488,#230489),(#230490,#230491),(#230492,#230493),(#230494,#230495),
(#230496,#230497),(#230498,#230499),(#230500,#230501),(#230502,#230503),
(#230504,#230505),(#230506,#230507),(#230508,#230509),(#230510,#230511),
(#230512,#230513),(#230514,#230515),(#230516,#230517),(#230518,#230519),
(#230520,#230521),(#230522,#230523),(#230524,#230525),(#230526,#230527),
(#230528,#230529),(#230530,#230531),(#230532,#230533),(#230534,#230535),
(#230536,#230537),(#230538,#230539),(#230540,#230541),(#230542,#230543),
(#230544,#230545),(#230546,#230547),(#230548,#230549),(#230550,#230551),
(#230552,#230553),(#230554,#230555),(#230556,#230557),(#230558,#230559),
(#230560,#230561),(#230562,#230563),(#230564,#230565),(#230566,#230567),
(#230568,#230569),(#230570,#230571),(#230572,#230573),(#230574,#230575),
(#230576,#230577),(#230578,#230579),(#230580,#230581),(#230582,#230583),
(#230584,#230585),(#230586,#230587),(#230588,#230589),(#230590,#230591),
(#230592,#230593),(#230594,#230595),(#230596,#230597),(#230598,#230599),
(#230600,#230601),(#230602,#230603),(#230604,#230605),(#230606,#230607),
(#230608,#230609),(#230610,#230611),(#230612,#230613),(#230614,#230615),
(#230616,#230617),(#230618,#230619),(#230620,#230621),(#230622,#230623),
(#230624,#230625),(#230626,#230627),(#230628,#230629),(#230630,#230631),
(#230632,#230633),(#230634,#230635),(#230636,#230637),(#230638,#230639),
(#230640,#230641),(#230642,#230643),(#230644,#230645),(#230646,#230647),
(#230648,#230649),(#230650,#230651),(#230652,#230653),(#230654,#230655),
(#230656,#230657),(#230658,#230659),(#230660,#230661),(#230662,#230663),
(#230664,#230665),(#230666,#230667),(#230668,#230669),(#230670,#230671),
(#230672,#230673),(#230674,#230675),(#230676,#230677),(#230678,#230679),
(#230680,#230681),(#230682,#230683),(#230684,#230685),(#230686,#230687),
(#230688,#230689),(#230690,#230691),(#230692,#230693),(#230694,#230695),
(#230696,#230697),(#230698,#230699),(#230700,#230701),(#230702,#230703),
(#230704,#230705),(#230706,#230707),(#230708,#230709),(#230710,#230711),
(#230712,#230713),(#230714,#230715),(#230716,#230717),(#230718,#230719),
(#230720,#230721),(#230722,#230723),(#230724,#230725),(#230726,#230727),
(#230728,#230729),(#230730,#230731),(#230732,#230733),(#230734,#230735),
(#230736,#230737),(#230738,#230739),(#230740,#230741),(#230742,#230743),
(#230744,#230745),(#230746,#230747),(#230748,#230749),(#230750,#230751),
(#230752,#230753),(#230754,#230755),(#230756,#230757),(#230758,#230759),
(#230760,#230761),(#230762,#230763),(#230764,#230765),(#230766,#230767),
(#230768,#230769),(#230770,#230771),(#230772,#230773),(#230774,#230775),
(#230776,#230777),(#230778,#230779),(#230780,#230781),(#230782,#230783),
(#230784,#230785),(#230786,#230787),(#230788,#230789),(#230790,#230791),
(#230792,#230793),(#230794,#230795),(#230796,#230797),(#230798,#230799),
(#230800,#230801),(#230802,#230803),(#230804,#230805),(#230806,#230807),
(#230808,#230809),(#230810,#230811),(#230812,#230813),(#230814,#230815),
(#230816,#230817),(#230818,#230819),(#230820,#230821),(#230822,#230823),
(#230824,#230825),(#230826,#230827),(#230828,#230829),(#230830,#230831),
(#230832,#230833),(#230834,#230835),(#230836,#230837),(#230838,#230839),
(#230840,#230841),(#230842,#230843),(#230844,#230845),(#230846,#230847),
(#230848,#230849),(#230850,#230851),(#230852,#230853),(#230854,#230855),
(#230856,#230857),(#230858,#230859),(#230860,#230861),(#230862,#230863),
(#230864,#230865),(#230866,#230867),(#230868,#230869),(#230870,#230871),
(#230872,#230873),(#230874,#230875),(#230876,#230877),(#230878,#230879),
(#230880,#230881),(#230882,#230883),(#230884,#230885),(#230886,#230887),
(#230888,#230889),(#230890,#230891),(#230892,#230893),(#230894,#230895),
(#230896,#230897),(#230898,#230899),(#230900,#230901),(#230902,#230903),
(#230904,#230905),(#230906,#230907),(#230908,#230909),(#230910,#230911),
(#230912,#230913),(#230914,#230915),(#230916,#230917),(#230918,#230919),
(#230920,#230921),(#230922,#230923),(#230924,#230925),(#230926,#230927),
(#230928,#230929),(#230930,#230931),(#230932,#230933),(#230934,#230935),
(#230936,#230937),(#230938,#230939),(#230940,#230941),(#230942,#230943),
(#230944,#230945),(#230946,#230947),(#230948,#230949),(#230950,#230951),
(#230952,#230953),(#230954,#230955),(#230956,#230957),(#230958,#230959),
(#230960,#230961),(#230962,#230963),(#230964,#230965),(#230966,#230967),
(#230968,#230969),(#230970,#230971),(#230972,#230973),(#230974,#230975),
(#230976,#230977),(#230978,#230979),(#230980,#230981),(#230982,#230983),
(#230984,#230985),(#230986,#230987),(#230988,#230989),(#230990,#230991),
(#230992,#230993),(#230994,#230995),(#230996,#230997),(#230998,#230999),
(#231000,#231001),(#231002,#231003),(#231004,#231005),(#231006,#231007),
(#231008,#231009),(#231010,#231011),(#231012,#231013),(#231014,#231015),
(#231016,#231017),(#231018,#231019),(#231020,#231021),(#231022,#231023),
(#231024,#231025),(#231026,#231027),(#231028,#231029),(#231030,#231031),
(#231032,#231033),(#231034,#231035),(#231036,#231037),(#231038,#231039),
(#231040,#231041),(#231042,#231043),(#231044,#231045),(#231046,#231047),
(#231048,#231049),(#231050,#231051),(#231052,#231053),(#231054,#231055),
(#231056,#231057),(#231058,#231059),(#231060,#231061),(#231062,#231063),
(#231064,#231065),(#231066,#231067),(#231068,#231069),(#231070,#231071),
(#231072,#231073),(#231074,#231075),(#231076,#231077),(#231078,#231079),
(#231080,#231081),(#231082,#231083),(#231084,#231085),(#231086,#231087),
(#231088,#231089),(#231090,#231091)),.UNSPECIFIED.,.F.,.F.,.F.,(6,1,1,1,
1,1,1,1,1,1,1,1,1,1,1,1,1,1,1,1,1,1,1,1,1,1,1,1,1,1,1,1,1,1,1,1,1,1,1,1,
1,1,1,1,1,1,1,1,1,1,1,1,1,1,1,1,1,1,1,1,1,1,1,1,1,1,1,1,1,1,1,1,1,1,1,1,
1,1,1,1,1,1,1,1,1,1,1,1,1,1,1,1,1,1,1,1,1,1,1,1,1,1,1,1,1,1,1,1,1,1,1,1,
1,1,1,1,1,1,1,1,1,1,1,1,1,1,1,1,1,1,1,1,1,1,1,1,1,1,1,1,1,1,1,1,1,1,1,1,
1,1,1,1,1,1,1,1,1,1,1,1,1,1,1,1,1,1,1,1,1,1,1,1,1,1,1,1,1,1,1,1,1,1,1,1,
1,1,1,1,1,1,1,1,1,1,1,1,1,1,1,1,1,1,1,1,1,1,1,1,1,1,1,1,1,1,1,1,1,1,1,1,
1,1,1,1,1,1,1,1,1,1,1,1,1,1,1,1,1,1,1,1,1,1,1,1,1,1,1,1,1,1,1,1,1,1,1,1,
1,1,1,1,1,1,1,1,1,1,1,1,1,1,1,1,1,1,1,1,1,1,1,1,1,1,1,1,1,1,1,1,1,1,1,1,
1,1,1,1,1,1,1,1,1,1,1,1,1,1,1,1,1,1,1,1,1,1,1,1,1,1,1,1,1,1,1,1,1,1,1,1,
1,1,1,1,1,1,1,1,1,1,1,1,1,1,1,1,1,1,1,1,1,1,1,1,1,1,1,1,1,1,1,1,1,1,1,1,
1,1,1,1,1,1,1,1,1,1,1,1,1,1,1,1,1,1,1,1,1,1,1,1,1,1,1,1,1,1,1,1,1,1,1,1,
1,1,1,1,1,1,1,1,1,1,1,1,1,1,1,1,1,1,1,1,1,1,1,1,1,1,1,1,1,1,1,1,1,1,1,1,
1,1,1,1,1,1,1,1,1,1,1,1,1,1,1,1,1,1,1,1,1,1,1,1,1,1,1,1,1,1,1,6),(2,2),
(-1.,-0.998165138,-0.996330275,-0.994495413,-0.99266055,-0.990825688,-0.988990826,
-0.987155963,-0.985321101,-0.983486239,-0.981651376,-0.979816514,-0.977981651,
-0.976146789,-0.974311927,-0.972477064,-0.970642202,-0.968807339,-0.966972477,
-0.965137615,-0.963302752,-0.96146789,-0.959633028,-0.957798165,-0.955963303,
-0.95412844,-0.952293578,-0.950458716,-0.948623853,-0.946788991,-0.944954128,
-0.943119266,-0.941284404,-0.939449541,-0.937614679,-0.935779817,-0.933944954,
-0.932110092,-0.930275229,-0.928440367,-0.926605505,-0.924770642,-0.92293578,
-0.921100917,-0.919266055,-0.917431193,-0.91559633,-0.913761468,-0.911926606,
-0.910091743,-0.908256881,-0.906422018,-0.904587156,-0.902752294,-0.900917431,
-0.899082569,-0.897247706,-0.895412844,-0.893577982,-0.891743119,-0.889908257,
-0.888073394,-0.886238532,-0.88440367,-0.882568807,-0.880733945,-0.878899083,
-0.87706422,-0.875229358,-0.873394495,-0.871559633,-0.869724771,-0.867889908,
-0.866055046,-0.864220183,-0.862385321,-0.860550459,-0.858715596,-0.856880734,
-0.855045872,-0.853211009,-0.851376147,-0.849541284,-0.847706422,-0.84587156,
-0.844036697,-0.842201835,-0.840366972,-0.83853211,-0.836697248,-0.834862385,
-0.833027523,-0.831192661,-0.829357798,-0.827522936,-0.825688073,-0.823853211,
-0.822018349,-0.820183486,-0.818348624,-0.816513761,-0.814678899,-0.812844037,
-0.811009174,-0.809174312,-0.80733945,-0.805504587,-0.803669725,-0.801834862,
-0.8,-0.798165138,-0.796330275,-0.794495413,-0.79266055,-0.790825688,-0.788990826,
-0.787155963,-0.785321101,-0.783486239,-0.781651376,-0.779816514,-0.777981651,
-0.776146789,-0.774311927,-0.772477064,-0.770642202,-0.768807339,-0.766972477,
-0.765137615,-0.763302752,-0.76146789,-0.759633028,-0.757798165,-0.755963303,
-0.75412844,-0.752293578,-0.750458716,-0.748623853,-0.746788991,-0.744954128,
-0.743119266,-0.741284404,-0.739449541,-0.737614679,-0.735779817,-0.733944954,
-0.732110092,-0.730275229,-0.728440367,-0.726605505,-0.724770642,-0.72293578,
-0.721100917,-0.719266055,-0.717431193,-0.71559633,-0.713761468,-0.711926606,
-0.710091743,-0.708256881,-0.706422018,-0.704587156,-0.702752294,-0.700917431,
-0.699082569,-0.697247706,-0.695412844,-0.693577982,-0.691743119,-0.689908257,
-0.688073394,-0.686238532,-0.68440367,-0.682568807,-0.680733945,-0.678899083,
-0.67706422,-0.675229358,-0.673394495,-0.671559633,-0.669724771,-0.667889908,
-0.666055046,-0.664220183,-0.662385321,-0.660550459,-0.658715596,-0.656880734,
-0.655045872,-0.653211009,-0.651376147,-0.649541284,-0.647706422,-0.64587156,
-0.644036697,-0.642201835,-0.640366972,-0.63853211,-0.636697248,-0.634862385,
-0.633027523,-0.631192661,-0.629357798,-0.627522936,-0.625688073,-0.623853211,
-0.622018349,-0.620183486,-0.618348624,-0.616513761,-0.614678899,-0.612844037,
-0.611009174,-0.609174312,-0.60733945,-0.605504587,-0.603669725,-0.601834862,
-0.6,-0.598165138,-0.596330275,-0.594495413,-0.59266055,-0.590825688,-0.588990826,
-0.587155963,-0.585321101,-0.583486239,-0.581651376,-0.579816514,-0.577981651,
-0.576146789,-0.574311927,-0.572477064,-0.570642202,-0.568807339,-0.566972477,
-0.565137615,-0.563302752,-0.56146789,-0.559633028,-0.557798165,-0.555963303,
-0.55412844,-0.552293578,-0.550458716,-0.548623853,-0.546788991,-0.544954128,
-0.543119266,-0.541284404,-0.539449541,-0.537614679,-0.535779817,-0.533944954,
-0.532110092,-0.530275229,-0.528440367,-0.526605505,-0.524770642,-0.52293578,
-0.521100917,-0.519266055,-0.517431193,-0.51559633,-0.513761468,-0.511926606,
-0.510091743,-0.508256881,-0.506422018,-0.504587156,-0.502752294,-0.500917431,
-0.499082569,-0.497247706,-0.495412844,-0.493577982,-0.491743119,-0.489908257,
-0.488073394,-0.486238532,-0.48440367,-0.482568807,-0.480733945,-0.478899083,
-0.47706422,-0.475229358,-0.473394495,-0.471559633,-0.469724771,-0.467889908,
-0.466055046,-0.464220183,-0.462385321,-0.460550459,-0.458715596,-0.456880734,
-0.455045872,-0.453211009,-0.451376147,-0.449541284,-0.447706422,-0.44587156,
-0.444036697,-0.442201835,-0.440366972,-0.43853211,-0.436697248,-0.434862385,
-0.433027523,-0.431192661,-0.429357798,-0.427522936,-0.425688073,-0.423853211,
-0.422018349,-0.420183486,-0.418348624,-0.416513761,-0.414678899,-0.412844037,
-0.411009174,-0.409174312,-0.40733945,-0.405504587,-0.403669725,-0.401834862,
-0.4,-0.398165138,-0.396330275,-0.394495413,-0.39266055,-0.390825688,-0.388990826,
-0.387155963,-0.385321101,-0.383486239,-0.381651376,-0.379816514,-0.377981651,
-0.376146789,-0.374311927,-0.372477064,-0.370642202,-0.368807339,-0.366972477,
-0.365137615,-0.363302752,-0.36146789,-0.359633028,-0.357798165,-0.355963303,
-0.35412844,-0.352293578,-0.350458716,-0.348623853,-0.346788991,-0.344954128,
-0.343119266,-0.341284404,-0.339449541,-0.337614679,-0.335779817,-0.333944954,
-0.332110092,-0.330275229,-0.328440367,-0.326605505,-0.324770642,-0.32293578,
-0.321100917,-0.319266055,-0.317431193,-0.31559633,-0.313761468,-0.311926606,
-0.310091743,-0.308256881,-0.306422018,-0.304587156,-0.302752294,-0.300917431,
-0.299082569,-0.297247706,-0.295412844,-0.293577982,-0.291743119,-0.289908257,
-0.288073394,-0.286238532,-0.28440367,-0.282568807,-0.280733945,-0.278899083,
-0.27706422,-0.275229358,-0.273394495,-0.271559633,-0.269724771,-0.267889908,
-0.266055046,-0.264220183,-0.262385321,-0.260550459,-0.258715596,-0.256880734,
-0.255045872,-0.253211009,-0.251376147,-0.249541284,-0.247706422,-0.24587156,
-0.244036697,-0.242201835,-0.240366972,-0.23853211,-0.236697248,-0.234862385,
-0.233027523,-0.231192661,-0.229357798,-0.227522936,-0.225688073,-0.223853211,
-0.222018349,-0.220183486,-0.218348624,-0.216513761,-0.214678899,-0.212844037,
-0.211009174,-0.209174312,-0.20733945,-0.205504587,-0.203669725,-0.201834862,
-0.2,-0.198165138,-0.196330275,-0.194495413,-0.19266055,-0.190825688,-0.188990826,
-0.187155963,-0.185321101,-0.183486239,-0.181651376,-0.179816514,-0.177981651,
-0.176146789,-0.174311927,-0.172477064,-0.170642202,-0.168807339,-0.166972477,
-0.165137615,-0.163302752,-0.16146789,-0.159633028,-0.157798165,-0.155963303,
-0.15412844,-0.152293578,-0.150458716,-0.148623853,-0.146788991,-0.144954128,
-0.143172104),(0.,0.36),.UNSPECIFIED.);
#6262=B_SPLINE_SURFACE_WITH_KNOTS('',5,1,((#231706,#231707),(#231708,#231709),
(#231710,#231711),(#231712,#231713),(#231714,#231715),(#231716,#231717),
(#231718,#231719),(#231720,#231721),(#231722,#231723),(#231724,#231725),
(#231726,#231727),(#231728,#231729),(#231730,#231731),(#231732,#231733),
(#231734,#231735),(#231736,#231737),(#231738,#231739),(#231740,#231741),
(#231742,#231743),(#231744,#231745),(#231746,#231747),(#231748,#231749),
(#231750,#231751),(#231752,#231753),(#231754,#231755),(#231756,#231757),
(#231758,#231759),(#231760,#231761),(#231762,#231763),(#231764,#231765),
(#231766,#231767),(#231768,#231769),(#231770,#231771),(#231772,#231773),
(#231774,#231775),(#231776,#231777),(#231778,#231779),(#231780,#231781),
(#231782,#231783),(#231784,#231785),(#231786,#231787),(#231788,#231789),
(#231790,#231791),(#231792,#231793),(#231794,#231795),(#231796,#231797),
(#231798,#231799),(#231800,#231801),(#231802,#231803),(#231804,#231805),
(#231806,#231807),(#231808,#231809),(#231810,#231811),(#231812,#231813),
(#231814,#231815),(#231816,#231817),(#231818,#231819),(#231820,#231821),
(#231822,#231823),(#231824,#231825),(#231826,#231827),(#231828,#231829),
(#231830,#231831),(#231832,#231833),(#231834,#231835),(#231836,#231837),
(#231838,#231839),(#231840,#231841),(#231842,#231843),(#231844,#231845),
(#231846,#231847),(#231848,#231849),(#231850,#231851),(#231852,#231853),
(#231854,#231855),(#231856,#231857),(#231858,#231859),(#231860,#231861),
(#231862,#231863),(#231864,#231865),(#231866,#231867),(#231868,#231869),
(#231870,#231871),(#231872,#231873),(#231874,#231875),(#231876,#231877),
(#231878,#231879),(#231880,#231881),(#231882,#231883),(#231884,#231885),
(#231886,#231887),(#231888,#231889),(#231890,#231891),(#231892,#231893),
(#231894,#231895),(#231896,#231897),(#231898,#231899),(#231900,#231901),
(#231902,#231903),(#231904,#231905),(#231906,#231907),(#231908,#231909),
(#231910,#231911),(#231912,#231913),(#231914,#231915),(#231916,#231917),
(#231918,#231919),(#231920,#231921),(#231922,#231923),(#231924,#231925),
(#231926,#231927),(#231928,#231929),(#231930,#231931),(#231932,#231933),
(#231934,#231935),(#231936,#231937),(#231938,#231939),(#231940,#231941),
(#231942,#231943),(#231944,#231945),(#231946,#231947),(#231948,#231949),
(#231950,#231951),(#231952,#231953),(#231954,#231955),(#231956,#231957),
(#231958,#231959),(#231960,#231961),(#231962,#231963),(#231964,#231965),
(#231966,#231967),(#231968,#231969),(#231970,#231971),(#231972,#231973),
(#231974,#231975),(#231976,#231977),(#231978,#231979),(#231980,#231981),
(#231982,#231983),(#231984,#231985),(#231986,#231987),(#231988,#231989),
(#231990,#231991),(#231992,#231993),(#231994,#231995),(#231996,#231997),
(#231998,#231999),(#232000,#232001),(#232002,#232003),(#232004,#232005),
(#232006,#232007),(#232008,#232009),(#232010,#232011),(#232012,#232013),
(#232014,#232015),(#232016,#232017),(#232018,#232019),(#232020,#232021),
(#232022,#232023),(#232024,#232025),(#232026,#232027),(#232028,#232029),
(#232030,#232031),(#232032,#232033),(#232034,#232035),(#232036,#232037),
(#232038,#232039),(#232040,#232041),(#232042,#232043),(#232044,#232045),
(#232046,#232047),(#232048,#232049),(#232050,#232051),(#232052,#232053),
(#232054,#232055),(#232056,#232057),(#232058,#232059),(#232060,#232061),
(#232062,#232063),(#232064,#232065),(#232066,#232067),(#232068,#232069),
(#232070,#232071),(#232072,#232073),(#232074,#232075),(#232076,#232077),
(#232078,#232079),(#232080,#232081),(#232082,#232083),(#232084,#232085),
(#232086,#232087),(#232088,#232089),(#232090,#232091),(#232092,#232093),
(#232094,#232095),(#232096,#232097),(#232098,#232099),(#232100,#232101),
(#232102,#232103),(#232104,#232105),(#232106,#232107),(#232108,#232109),
(#232110,#232111),(#232112,#232113),(#232114,#232115),(#232116,#232117),
(#232118,#232119),(#232120,#232121),(#232122,#232123),(#232124,#232125),
(#232126,#232127),(#232128,#232129),(#232130,#232131),(#232132,#232133),
(#232134,#232135),(#232136,#232137),(#232138,#232139),(#232140,#232141),
(#232142,#232143),(#232144,#232145),(#232146,#232147),(#232148,#232149),
(#232150,#232151),(#232152,#232153),(#232154,#232155),(#232156,#232157),
(#232158,#232159),(#232160,#232161),(#232162,#232163),(#232164,#232165),
(#232166,#232167),(#232168,#232169),(#232170,#232171),(#232172,#232173),
(#232174,#232175),(#232176,#232177),(#232178,#232179),(#232180,#232181),
(#232182,#232183),(#232184,#232185),(#232186,#232187),(#232188,#232189),
(#232190,#232191),(#232192,#232193),(#232194,#232195),(#232196,#232197),
(#232198,#232199),(#232200,#232201),(#232202,#232203),(#232204,#232205),
(#232206,#232207),(#232208,#232209),(#232210,#232211),(#232212,#232213),
(#232214,#232215),(#232216,#232217),(#232218,#232219),(#232220,#232221),
(#232222,#232223),(#232224,#232225),(#232226,#232227),(#232228,#232229),
(#232230,#232231),(#232232,#232233),(#232234,#232235),(#232236,#232237),
(#232238,#232239),(#232240,#232241),(#232242,#232243),(#232244,#232245),
(#232246,#232247),(#232248,#232249),(#232250,#232251),(#232252,#232253),
(#232254,#232255),(#232256,#232257),(#232258,#232259),(#232260,#232261),
(#232262,#232263),(#232264,#232265),(#232266,#232267),(#232268,#232269),
(#232270,#232271),(#232272,#232273),(#232274,#232275),(#232276,#232277),
(#232278,#232279),(#232280,#232281),(#232282,#232283),(#232284,#232285),
(#232286,#232287),(#232288,#232289),(#232290,#232291),(#232292,#232293),
(#232294,#232295),(#232296,#232297),(#232298,#232299),(#232300,#232301),
(#232302,#232303),(#232304,#232305),(#232306,#232307),(#232308,#232309),
(#232310,#232311),(#232312,#232313),(#232314,#232315),(#232316,#232317),
(#232318,#232319),(#232320,#232321),(#232322,#232323),(#232324,#232325),
(#232326,#232327),(#232328,#232329),(#232330,#232331),(#232332,#232333),
(#232334,#232335),(#232336,#232337),(#232338,#232339),(#232340,#232341),
(#232342,#232343),(#232344,#232345),(#232346,#232347),(#232348,#232349),
(#232350,#232351),(#232352,#232353),(#232354,#232355),(#232356,#232357),
(#232358,#232359),(#232360,#232361),(#232362,#232363),(#232364,#232365),
(#232366,#232367),(#232368,#232369),(#232370,#232371),(#232372,#232373),
(#232374,#232375),(#232376,#232377),(#232378,#232379),(#232380,#232381),
(#232382,#232383),(#232384,#232385),(#232386,#232387),(#232388,#232389),
(#232390,#232391),(#232392,#232393),(#232394,#232395),(#232396,#232397),
(#232398,#232399),(#232400,#232401),(#232402,#232403),(#232404,#232405),
(#232406,#232407),(#232408,#232409),(#232410,#232411),(#232412,#232413),
(#232414,#232415),(#232416,#232417),(#232418,#232419),(#232420,#232421),
(#232422,#232423),(#232424,#232425),(#232426,#232427),(#232428,#232429),
(#232430,#232431),(#232432,#232433),(#232434,#232435),(#232436,#232437),
(#232438,#232439),(#232440,#232441),(#232442,#232443),(#232444,#232445),
(#232446,#232447),(#232448,#232449),(#232450,#232451),(#232452,#232453),
(#232454,#232455),(#232456,#232457),(#232458,#232459),(#232460,#232461),
(#232462,#232463),(#232464,#232465),(#232466,#232467),(#232468,#232469),
(#232470,#232471),(#232472,#232473),(#232474,#232475),(#232476,#232477),
(#232478,#232479),(#232480,#232481),(#232482,#232483),(#232484,#232485),
(#232486,#232487),(#232488,#232489),(#232490,#232491),(#232492,#232493),
(#232494,#232495),(#232496,#232497),(#232498,#232499),(#232500,#232501),
(#232502,#232503),(#232504,#232505),(#232506,#232507),(#232508,#232509),
(#232510,#232511),(#232512,#232513),(#232514,#232515),(#232516,#232517),
(#232518,#232519),(#232520,#232521),(#232522,#232523),(#232524,#232525),
(#232526,#232527),(#232528,#232529),(#232530,#232531),(#232532,#232533),
(#232534,#232535),(#232536,#232537),(#232538,#232539),(#232540,#232541),
(#232542,#232543),(#232544,#232545),(#232546,#232547),(#232548,#232549),
(#232550,#232551),(#232552,#232553),(#232554,#232555),(#232556,#232557),
(#232558,#232559),(#232560,#232561),(#232562,#232563),(#232564,#232565),
(#232566,#232567),(#232568,#232569),(#232570,#232571),(#232572,#232573),
(#232574,#232575),(#232576,#232577),(#232578,#232579),(#232580,#232581),
(#232582,#232583),(#232584,#232585),(#232586,#232587),(#232588,#232589),
(#232590,#232591),(#232592,#232593),(#232594,#232595),(#232596,#232597),
(#232598,#232599),(#232600,#232601),(#232602,#232603),(#232604,#232605),
(#232606,#232607),(#232608,#232609),(#232610,#232611),(#232612,#232613),
(#232614,#232615),(#232616,#232617),(#232618,#232619),(#232620,#232621),
(#232622,#232623),(#232624,#232625),(#232626,#232627),(#232628,#232629),
(#232630,#232631),(#232632,#232633),(#232634,#232635),(#232636,#232637),
(#232638,#232639),(#232640,#232641),(#232642,#232643),(#232644,#232645),
(#232646,#232647),(#232648,#232649)),.UNSPECIFIED.,.F.,.F.,.F.,(6,1,1,1,
1,1,1,1,1,1,1,1,1,1,1,1,1,1,1,1,1,1,1,1,1,1,1,1,1,1,1,1,1,1,1,1,1,1,1,1,
1,1,1,1,1,1,1,1,1,1,1,1,1,1,1,1,1,1,1,1,1,1,1,1,1,1,1,1,1,1,1,1,1,1,1,1,
1,1,1,1,1,1,1,1,1,1,1,1,1,1,1,1,1,1,1,1,1,1,1,1,1,1,1,1,1,1,1,1,1,1,1,1,
1,1,1,1,1,1,1,1,1,1,1,1,1,1,1,1,1,1,1,1,1,1,1,1,1,1,1,1,1,1,1,1,1,1,1,1,
1,1,1,1,1,1,1,1,1,1,1,1,1,1,1,1,1,1,1,1,1,1,1,1,1,1,1,1,1,1,1,1,1,1,1,1,
1,1,1,1,1,1,1,1,1,1,1,1,1,1,1,1,1,1,1,1,1,1,1,1,1,1,1,1,1,1,1,1,1,1,1,1,
1,1,1,1,1,1,1,1,1,1,1,1,1,1,1,1,1,1,1,1,1,1,1,1,1,1,1,1,1,1,1,1,1,1,1,1,
1,1,1,1,1,1,1,1,1,1,1,1,1,1,1,1,1,1,1,1,1,1,1,1,1,1,1,1,1,1,1,1,1,1,1,1,
1,1,1,1,1,1,1,1,1,1,1,1,1,1,1,1,1,1,1,1,1,1,1,1,1,1,1,1,1,1,1,1,1,1,1,1,
1,1,1,1,1,1,1,1,1,1,1,1,1,1,1,1,1,1,1,1,1,1,1,1,1,1,1,1,1,1,1,1,1,1,1,1,
1,1,1,1,1,1,1,1,1,1,1,1,1,1,1,1,1,1,1,1,1,1,1,1,1,1,1,1,1,1,1,1,1,1,1,1,
1,1,1,1,1,1,1,1,1,1,1,1,1,1,1,1,1,1,1,1,1,1,1,1,1,1,1,1,1,1,1,1,1,1,1,1,
1,1,1,1,1,1,1,1,1,1,1,1,1,1,1,1,1,1,1,1,1,1,1,1,1,1,1,1,1,1,1,6),(2,2),
(0.143172105,0.144954128,0.146788991,0.148623853,0.150458716,0.152293578,
0.15412844,0.155963303,0.157798165,0.159633028,0.16146789,0.163302752,0.165137615,
0.166972477,0.168807339,0.170642202,0.172477064,0.174311927,0.176146789,
0.177981651,0.179816514,0.181651376,0.183486239,0.185321101,0.187155963,
0.188990826,0.190825688,0.19266055,0.194495413,0.196330275,0.198165138,
0.2,0.201834862,0.203669725,0.205504587,0.20733945,0.209174312,0.211009174,
0.212844037,0.214678899,0.216513761,0.218348624,0.220183486,0.222018349,
0.223853211,0.225688073,0.227522936,0.229357798,0.231192661,0.233027523,
0.234862385,0.236697248,0.23853211,0.240366972,0.242201835,0.244036697,
0.24587156,0.247706422,0.249541284,0.251376147,0.253211009,0.255045872,
0.256880734,0.258715596,0.260550459,0.262385321,0.264220183,0.266055046,
0.267889908,0.269724771,0.271559633,0.273394495,0.275229358,0.27706422,
0.278899083,0.280733945,0.282568807,0.28440367,0.286238532,0.288073394,
0.289908257,0.291743119,0.293577982,0.295412844,0.297247706,0.299082569,
0.300917431,0.302752294,0.304587156,0.306422018,0.308256881,0.310091743,
0.311926606,0.313761468,0.31559633,0.317431193,0.319266055,0.321100917,
0.32293578,0.324770642,0.326605505,0.328440367,0.330275229,0.332110092,
0.333944954,0.335779817,0.337614679,0.339449541,0.341284404,0.343119266,
0.344954128,0.346788991,0.348623853,0.350458716,0.352293578,0.35412844,
0.355963303,0.357798165,0.359633028,0.36146789,0.363302752,0.365137615,
0.366972477,0.368807339,0.370642202,0.372477064,0.374311927,0.376146789,
0.377981651,0.379816514,0.381651376,0.383486239,0.385321101,0.387155963,
0.388990826,0.390825688,0.39266055,0.394495413,0.396330275,0.398165138,
0.4,0.401834862,0.403669725,0.405504587,0.40733945,0.409174312,0.411009174,
0.412844037,0.414678899,0.416513761,0.418348624,0.420183486,0.422018349,
0.423853211,0.425688073,0.427522936,0.429357798,0.431192661,0.433027523,
0.434862385,0.436697248,0.43853211,0.440366972,0.442201835,0.444036697,
0.44587156,0.447706422,0.449541284,0.451376147,0.453211009,0.455045872,
0.456880734,0.458715596,0.460550459,0.462385321,0.464220183,0.466055046,
0.467889908,0.469724771,0.471559633,0.473394495,0.475229358,0.47706422,
0.478899083,0.480733945,0.482568807,0.48440367,0.486238532,0.488073394,
0.489908257,0.491743119,0.493577982,0.495412844,0.497247706,0.499082569,
0.500917431,0.502752294,0.504587156,0.506422018,0.508256881,0.510091743,
0.511926606,0.513761468,0.51559633,0.517431193,0.519266055,0.521100917,
0.52293578,0.524770642,0.526605505,0.528440367,0.530275229,0.532110092,
0.533944954,0.535779817,0.537614679,0.539449541,0.541284404,0.543119266,
0.544954128,0.546788991,0.548623853,0.550458716,0.552293578,0.55412844,
0.555963303,0.557798165,0.559633028,0.56146789,0.563302752,0.565137615,
0.566972477,0.568807339,0.570642202,0.572477064,0.574311927,0.576146789,
0.577981651,0.579816514,0.581651376,0.583486239,0.585321101,0.587155963,
0.588990826,0.590825688,0.59266055,0.594495413,0.596330275,0.598165138,
0.6,0.601834862,0.603669725,0.605504587,0.60733945,0.609174312,0.611009174,
0.612844037,0.614678899,0.616513761,0.618348624,0.620183486,0.622018349,
0.623853211,0.625688073,0.627522936,0.629357798,0.631192661,0.633027523,
0.634862385,0.636697248,0.63853211,0.640366972,0.642201835,0.644036697,
0.64587156,0.647706422,0.649541284,0.651376147,0.653211009,0.655045872,
0.656880734,0.658715596,0.660550459,0.662385321,0.664220183,0.666055046,
0.667889908,0.669724771,0.671559633,0.673394495,0.675229358,0.67706422,
0.678899083,0.680733945,0.682568807,0.68440367,0.686238532,0.688073394,
0.689908257,0.691743119,0.693577982,0.695412844,0.697247706,0.699082569,
0.700917431,0.702752294,0.704587156,0.706422018,0.708256881,0.710091743,
0.711926606,0.713761468,0.71559633,0.717431193,0.719266055,0.721100917,
0.72293578,0.724770642,0.726605505,0.728440367,0.730275229,0.732110092,
0.733944954,0.735779817,0.737614679,0.739449541,0.741284404,0.743119266,
0.744954128,0.746788991,0.748623853,0.750458716,0.752293578,0.75412844,
0.755963303,0.757798165,0.759633028,0.76146789,0.763302752,0.765137615,
0.766972477,0.768807339,0.770642202,0.772477064,0.774311927,0.776146789,
0.777981651,0.779816514,0.781651376,0.783486239,0.785321101,0.787155963,
0.788990826,0.790825688,0.79266055,0.794495413,0.796330275,0.798165138,
0.8,0.801834862,0.803669725,0.805504587,0.80733945,0.809174312,0.811009174,
0.812844037,0.814678899,0.816513761,0.818348624,0.820183486,0.822018349,
0.823853211,0.825688073,0.827522936,0.829357798,0.831192661,0.833027523,
0.834862385,0.836697248,0.83853211,0.840366972,0.842201835,0.844036697,
0.84587156,0.847706422,0.849541284,0.851376147,0.853211009,0.855045872,
0.856880734,0.858715596,0.860550459,0.862385321,0.864220183,0.866055046,
0.867889908,0.869724771,0.871559633,0.873394495,0.875229358,0.87706422,
0.878899083,0.880733945,0.882568807,0.88440367,0.886238532,0.888073394,
0.889908257,0.891743119,0.893577982,0.895412844,0.897247706,0.899082569,
0.900917431,0.902752294,0.904587156,0.906422018,0.908256881,0.910091743,
0.911926606,0.913761468,0.91559633,0.917431193,0.919266055,0.921100917,
0.92293578,0.924770642,0.926605505,0.928440367,0.930275229,0.932110092,
0.933944954,0.935779817,0.937614679,0.939449541,0.941284404,0.943119266,
0.944954128,0.946788991,0.948623853,0.950458716,0.952293578,0.95412844,
0.955963303,0.957798165,0.959633028,0.96146789,0.963302752,0.965137615,
0.966972477,0.968807339,0.970642202,0.972477064,0.974311927,0.976146789,
0.977981651,0.979816514,0.981651376,0.983486239,0.985321101,0.987155963,
0.988990826,0.990825688,0.99266055,0.994495413,0.996330275,0.998165138,
1.),(0.,0.36),.UNSPECIFIED.);
#6263=B_SPLINE_SURFACE_WITH_KNOTS('',5,1,((#233288,#233289),(#233290,#233291),
(#233292,#233293),(#233294,#233295),(#233296,#233297),(#233298,#233299),
(#233300,#233301),(#233302,#233303),(#233304,#233305),(#233306,#233307),
(#233308,#233309),(#233310,#233311),(#233312,#233313),(#233314,#233315),
(#233316,#233317),(#233318,#233319),(#233320,#233321),(#233322,#233323),
(#233324,#233325),(#233326,#233327),(#233328,#233329),(#233330,#233331),
(#233332,#233333),(#233334,#233335),(#233336,#233337),(#233338,#233339),
(#233340,#233341),(#233342,#233343),(#233344,#233345),(#233346,#233347),
(#233348,#233349),(#233350,#233351),(#233352,#233353),(#233354,#233355),
(#233356,#233357),(#233358,#233359),(#233360,#233361),(#233362,#233363),
(#233364,#233365),(#233366,#233367),(#233368,#233369),(#233370,#233371),
(#233372,#233373),(#233374,#233375),(#233376,#233377),(#233378,#233379),
(#233380,#233381),(#233382,#233383),(#233384,#233385),(#233386,#233387),
(#233388,#233389),(#233390,#233391),(#233392,#233393),(#233394,#233395),
(#233396,#233397),(#233398,#233399),(#233400,#233401),(#233402,#233403),
(#233404,#233405),(#233406,#233407),(#233408,#233409),(#233410,#233411),
(#233412,#233413),(#233414,#233415),(#233416,#233417),(#233418,#233419),
(#233420,#233421),(#233422,#233423),(#233424,#233425),(#233426,#233427),
(#233428,#233429),(#233430,#233431),(#233432,#233433),(#233434,#233435),
(#233436,#233437),(#233438,#233439),(#233440,#233441),(#233442,#233443),
(#233444,#233445),(#233446,#233447),(#233448,#233449),(#233450,#233451),
(#233452,#233453),(#233454,#233455),(#233456,#233457),(#233458,#233459),
(#233460,#233461),(#233462,#233463),(#233464,#233465),(#233466,#233467),
(#233468,#233469),(#233470,#233471),(#233472,#233473),(#233474,#233475),
(#233476,#233477),(#233478,#233479),(#233480,#233481),(#233482,#233483),
(#233484,#233485),(#233486,#233487),(#233488,#233489),(#233490,#233491),
(#233492,#233493),(#233494,#233495),(#233496,#233497),(#233498,#233499),
(#233500,#233501),(#233502,#233503),(#233504,#233505),(#233506,#233507),
(#233508,#233509),(#233510,#233511),(#233512,#233513),(#233514,#233515),
(#233516,#233517),(#233518,#233519),(#233520,#233521),(#233522,#233523),
(#233524,#233525),(#233526,#233527),(#233528,#233529),(#233530,#233531),
(#233532,#233533),(#233534,#233535),(#233536,#233537),(#233538,#233539),
(#233540,#233541),(#233542,#233543),(#233544,#233545),(#233546,#233547),
(#233548,#233549),(#233550,#233551),(#233552,#233553),(#233554,#233555),
(#233556,#233557),(#233558,#233559),(#233560,#233561),(#233562,#233563),
(#233564,#233565),(#233566,#233567),(#233568,#233569),(#233570,#233571),
(#233572,#233573),(#233574,#233575),(#233576,#233577),(#233578,#233579),
(#233580,#233581),(#233582,#233583),(#233584,#233585),(#233586,#233587),
(#233588,#233589),(#233590,#233591),(#233592,#233593),(#233594,#233595),
(#233596,#233597),(#233598,#233599),(#233600,#233601),(#233602,#233603),
(#233604,#233605),(#233606,#233607),(#233608,#233609),(#233610,#233611),
(#233612,#233613),(#233614,#233615),(#233616,#233617),(#233618,#233619),
(#233620,#233621),(#233622,#233623),(#233624,#233625),(#233626,#233627),
(#233628,#233629),(#233630,#233631),(#233632,#233633),(#233634,#233635),
(#233636,#233637),(#233638,#233639),(#233640,#233641),(#233642,#233643),
(#233644,#233645),(#233646,#233647),(#233648,#233649),(#233650,#233651),
(#233652,#233653),(#233654,#233655),(#233656,#233657),(#233658,#233659),
(#233660,#233661),(#233662,#233663),(#233664,#233665),(#233666,#233667),
(#233668,#233669),(#233670,#233671),(#233672,#233673),(#233674,#233675),
(#233676,#233677),(#233678,#233679),(#233680,#233681),(#233682,#233683),
(#233684,#233685),(#233686,#233687),(#233688,#233689),(#233690,#233691),
(#233692,#233693),(#233694,#233695),(#233696,#233697),(#233698,#233699),
(#233700,#233701),(#233702,#233703),(#233704,#233705),(#233706,#233707),
(#233708,#233709),(#233710,#233711),(#233712,#233713),(#233714,#233715),
(#233716,#233717),(#233718,#233719),(#233720,#233721),(#233722,#233723),
(#233724,#233725),(#233726,#233727),(#233728,#233729),(#233730,#233731),
(#233732,#233733),(#233734,#233735),(#233736,#233737),(#233738,#233739),
(#233740,#233741),(#233742,#233743),(#233744,#233745),(#233746,#233747),
(#233748,#233749),(#233750,#233751),(#233752,#233753),(#233754,#233755),
(#233756,#233757),(#233758,#233759),(#233760,#233761),(#233762,#233763),
(#233764,#233765),(#233766,#233767),(#233768,#233769),(#233770,#233771),
(#233772,#233773),(#233774,#233775),(#233776,#233777),(#233778,#233779),
(#233780,#233781),(#233782,#233783),(#233784,#233785),(#233786,#233787),
(#233788,#233789),(#233790,#233791),(#233792,#233793),(#233794,#233795),
(#233796,#233797),(#233798,#233799),(#233800,#233801),(#233802,#233803),
(#233804,#233805),(#233806,#233807),(#233808,#233809),(#233810,#233811),
(#233812,#233813),(#233814,#233815),(#233816,#233817),(#233818,#233819),
(#233820,#233821),(#233822,#233823),(#233824,#233825),(#233826,#233827),
(#233828,#233829),(#233830,#233831),(#233832,#233833),(#233834,#233835),
(#233836,#233837),(#233838,#233839),(#233840,#233841),(#233842,#233843),
(#233844,#233845),(#233846,#233847),(#233848,#233849),(#233850,#233851),
(#233852,#233853),(#233854,#233855),(#233856,#233857),(#233858,#233859),
(#233860,#233861),(#233862,#233863),(#233864,#233865),(#233866,#233867),
(#233868,#233869),(#233870,#233871),(#233872,#233873),(#233874,#233875),
(#233876,#233877),(#233878,#233879),(#233880,#233881),(#233882,#233883),
(#233884,#233885),(#233886,#233887),(#233888,#233889),(#233890,#233891),
(#233892,#233893),(#233894,#233895),(#233896,#233897),(#233898,#233899),
(#233900,#233901),(#233902,#233903),(#233904,#233905),(#233906,#233907),
(#233908,#233909),(#233910,#233911),(#233912,#233913),(#233914,#233915),
(#233916,#233917),(#233918,#233919),(#233920,#233921),(#233922,#233923),
(#233924,#233925),(#233926,#233927),(#233928,#233929),(#233930,#233931),
(#233932,#233933),(#233934,#233935),(#233936,#233937),(#233938,#233939),
(#233940,#233941),(#233942,#233943),(#233944,#233945),(#233946,#233947),
(#233948,#233949),(#233950,#233951),(#233952,#233953),(#233954,#233955),
(#233956,#233957),(#233958,#233959),(#233960,#233961),(#233962,#233963),
(#233964,#233965),(#233966,#233967),(#233968,#233969),(#233970,#233971),
(#233972,#233973),(#233974,#233975),(#233976,#233977),(#233978,#233979),
(#233980,#233981),(#233982,#233983),(#233984,#233985),(#233986,#233987),
(#233988,#233989),(#233990,#233991),(#233992,#233993),(#233994,#233995),
(#233996,#233997),(#233998,#233999),(#234000,#234001),(#234002,#234003),
(#234004,#234005),(#234006,#234007),(#234008,#234009),(#234010,#234011),
(#234012,#234013),(#234014,#234015),(#234016,#234017),(#234018,#234019),
(#234020,#234021),(#234022,#234023),(#234024,#234025),(#234026,#234027),
(#234028,#234029),(#234030,#234031),(#234032,#234033),(#234034,#234035),
(#234036,#234037),(#234038,#234039),(#234040,#234041),(#234042,#234043),
(#234044,#234045),(#234046,#234047),(#234048,#234049),(#234050,#234051),
(#234052,#234053),(#234054,#234055),(#234056,#234057),(#234058,#234059),
(#234060,#234061),(#234062,#234063),(#234064,#234065),(#234066,#234067),
(#234068,#234069),(#234070,#234071),(#234072,#234073),(#234074,#234075),
(#234076,#234077),(#234078,#234079),(#234080,#234081),(#234082,#234083),
(#234084,#234085),(#234086,#234087),(#234088,#234089),(#234090,#234091),
(#234092,#234093),(#234094,#234095),(#234096,#234097),(#234098,#234099),
(#234100,#234101),(#234102,#234103),(#234104,#234105),(#234106,#234107),
(#234108,#234109),(#234110,#234111),(#234112,#234113),(#234114,#234115),
(#234116,#234117),(#234118,#234119),(#234120,#234121),(#234122,#234123),
(#234124,#234125),(#234126,#234127),(#234128,#234129),(#234130,#234131),
(#234132,#234133),(#234134,#234135),(#234136,#234137),(#234138,#234139),
(#234140,#234141),(#234142,#234143),(#234144,#234145),(#234146,#234147),
(#234148,#234149),(#234150,#234151),(#234152,#234153),(#234154,#234155),
(#234156,#234157),(#234158,#234159),(#234160,#234161),(#234162,#234163),
(#234164,#234165),(#234166,#234167),(#234168,#234169),(#234170,#234171),
(#234172,#234173),(#234174,#234175),(#234176,#234177),(#234178,#234179),
(#234180,#234181),(#234182,#234183),(#234184,#234185),(#234186,#234187),
(#234188,#234189),(#234190,#234191),(#234192,#234193),(#234194,#234195),
(#234196,#234197),(#234198,#234199),(#234200,#234201),(#234202,#234203),
(#234204,#234205),(#234206,#234207),(#234208,#234209),(#234210,#234211),
(#234212,#234213),(#234214,#234215),(#234216,#234217),(#234218,#234219),
(#234220,#234221),(#234222,#234223),(#234224,#234225),(#234226,#234227),
(#234228,#234229),(#234230,#234231)),.UNSPECIFIED.,.F.,.F.,.F.,(6,1,1,1,
1,1,1,1,1,1,1,1,1,1,1,1,1,1,1,1,1,1,1,1,1,1,1,1,1,1,1,1,1,1,1,1,1,1,1,1,
1,1,1,1,1,1,1,1,1,1,1,1,1,1,1,1,1,1,1,1,1,1,1,1,1,1,1,1,1,1,1,1,1,1,1,1,
1,1,1,1,1,1,1,1,1,1,1,1,1,1,1,1,1,1,1,1,1,1,1,1,1,1,1,1,1,1,1,1,1,1,1,1,
1,1,1,1,1,1,1,1,1,1,1,1,1,1,1,1,1,1,1,1,1,1,1,1,1,1,1,1,1,1,1,1,1,1,1,1,
1,1,1,1,1,1,1,1,1,1,1,1,1,1,1,1,1,1,1,1,1,1,1,1,1,1,1,1,1,1,1,1,1,1,1,1,
1,1,1,1,1,1,1,1,1,1,1,1,1,1,1,1,1,1,1,1,1,1,1,1,1,1,1,1,1,1,1,1,1,1,1,1,
1,1,1,1,1,1,1,1,1,1,1,1,1,1,1,1,1,1,1,1,1,1,1,1,1,1,1,1,1,1,1,1,1,1,1,1,
1,1,1,1,1,1,1,1,1,1,1,1,1,1,1,1,1,1,1,1,1,1,1,1,1,1,1,1,1,1,1,1,1,1,1,1,
1,1,1,1,1,1,1,1,1,1,1,1,1,1,1,1,1,1,1,1,1,1,1,1,1,1,1,1,1,1,1,1,1,1,1,1,
1,1,1,1,1,1,1,1,1,1,1,1,1,1,1,1,1,1,1,1,1,1,1,1,1,1,1,1,1,1,1,1,1,1,1,1,
1,1,1,1,1,1,1,1,1,1,1,1,1,1,1,1,1,1,1,1,1,1,1,1,1,1,1,1,1,1,1,1,1,1,1,1,
1,1,1,1,1,1,1,1,1,1,1,1,1,1,1,1,1,1,1,1,1,1,1,1,1,1,1,1,1,1,1,1,1,1,1,1,
1,1,1,1,1,1,1,1,1,1,1,1,1,1,1,1,1,1,1,1,1,1,1,1,1,1,1,1,1,1,1,6),(2,2),
(0.143172104,0.144954128,0.146788991,0.148623853,0.150458716,0.152293578,
0.15412844,0.155963303,0.157798165,0.159633028,0.16146789,0.163302752,0.165137615,
0.166972477,0.168807339,0.170642202,0.172477064,0.174311927,0.176146789,
0.177981651,0.179816514,0.181651376,0.183486239,0.185321101,0.187155963,
0.188990826,0.190825688,0.19266055,0.194495413,0.196330275,0.198165138,
0.2,0.201834862,0.203669725,0.205504587,0.20733945,0.209174312,0.211009174,
0.212844037,0.214678899,0.216513761,0.218348624,0.220183486,0.222018349,
0.223853211,0.225688073,0.227522936,0.229357798,0.231192661,0.233027523,
0.234862385,0.236697248,0.23853211,0.240366972,0.242201835,0.244036697,
0.24587156,0.247706422,0.249541284,0.251376147,0.253211009,0.255045872,
0.256880734,0.258715596,0.260550459,0.262385321,0.264220183,0.266055046,
0.267889908,0.269724771,0.271559633,0.273394495,0.275229358,0.27706422,
0.278899083,0.280733945,0.282568807,0.28440367,0.286238532,0.288073394,
0.289908257,0.291743119,0.293577982,0.295412844,0.297247706,0.299082569,
0.300917431,0.302752294,0.304587156,0.306422018,0.308256881,0.310091743,
0.311926606,0.313761468,0.31559633,0.317431193,0.319266055,0.321100917,
0.32293578,0.324770642,0.326605505,0.328440367,0.330275229,0.332110092,
0.333944954,0.335779817,0.337614679,0.339449541,0.341284404,0.343119266,
0.344954128,0.346788991,0.348623853,0.350458716,0.352293578,0.35412844,
0.355963303,0.357798165,0.359633028,0.36146789,0.363302752,0.365137615,
0.366972477,0.368807339,0.370642202,0.372477064,0.374311927,0.376146789,
0.377981651,0.379816514,0.381651376,0.383486239,0.385321101,0.387155963,
0.388990826,0.390825688,0.39266055,0.394495413,0.396330275,0.398165138,
0.4,0.401834862,0.403669725,0.405504587,0.40733945,0.409174312,0.411009174,
0.412844037,0.414678899,0.416513761,0.418348624,0.420183486,0.422018349,
0.423853211,0.425688073,0.427522936,0.429357798,0.431192661,0.433027523,
0.434862385,0.436697248,0.43853211,0.440366972,0.442201835,0.444036697,
0.44587156,0.447706422,0.449541284,0.451376147,0.453211009,0.455045872,
0.456880734,0.458715596,0.460550459,0.462385321,0.464220183,0.466055046,
0.467889908,0.469724771,0.471559633,0.473394495,0.475229358,0.47706422,
0.478899083,0.480733945,0.482568807,0.48440367,0.486238532,0.488073394,
0.489908257,0.491743119,0.493577982,0.495412844,0.497247706,0.499082569,
0.500917431,0.502752294,0.504587156,0.506422018,0.508256881,0.510091743,
0.511926606,0.513761468,0.51559633,0.517431193,0.519266055,0.521100917,
0.52293578,0.524770642,0.526605505,0.528440367,0.530275229,0.532110092,
0.533944954,0.535779817,0.537614679,0.539449541,0.541284404,0.543119266,
0.544954128,0.546788991,0.548623853,0.550458716,0.552293578,0.55412844,
0.555963303,0.557798165,0.559633028,0.56146789,0.563302752,0.565137615,
0.566972477,0.568807339,0.570642202,0.572477064,0.574311927,0.576146789,
0.577981651,0.579816514,0.581651376,0.583486239,0.585321101,0.587155963,
0.588990826,0.590825688,0.59266055,0.594495413,0.596330275,0.598165138,
0.6,0.601834862,0.603669725,0.605504587,0.60733945,0.609174312,0.611009174,
0.612844037,0.614678899,0.616513761,0.618348624,0.620183486,0.622018349,
0.623853211,0.625688073,0.627522936,0.629357798,0.631192661,0.633027523,
0.634862385,0.636697248,0.63853211,0.640366972,0.642201835,0.644036697,
0.64587156,0.647706422,0.649541284,0.651376147,0.653211009,0.655045872,
0.656880734,0.658715596,0.660550459,0.662385321,0.664220183,0.666055046,
0.667889908,0.669724771,0.671559633,0.673394495,0.675229358,0.67706422,
0.678899083,0.680733945,0.682568807,0.68440367,0.686238532,0.688073394,
0.689908257,0.691743119,0.693577982,0.695412844,0.697247706,0.699082569,
0.700917431,0.702752294,0.704587156,0.706422018,0.708256881,0.710091743,
0.711926606,0.713761468,0.71559633,0.717431193,0.719266055,0.721100917,
0.72293578,0.724770642,0.726605505,0.728440367,0.730275229,0.732110092,
0.733944954,0.735779817,0.737614679,0.739449541,0.741284404,0.743119266,
0.744954128,0.746788991,0.748623853,0.750458716,0.752293578,0.75412844,
0.755963303,0.757798165,0.759633028,0.76146789,0.763302752,0.765137615,
0.766972477,0.768807339,0.770642202,0.772477064,0.774311927,0.776146789,
0.777981651,0.779816514,0.781651376,0.783486239,0.785321101,0.787155963,
0.788990826,0.790825688,0.79266055,0.794495413,0.796330275,0.798165138,
0.8,0.801834862,0.803669725,0.805504587,0.80733945,0.809174312,0.811009174,
0.812844037,0.814678899,0.816513761,0.818348624,0.820183486,0.822018349,
0.823853211,0.825688073,0.827522936,0.829357798,0.831192661,0.833027523,
0.834862385,0.836697248,0.83853211,0.840366972,0.842201835,0.844036697,
0.84587156,0.847706422,0.849541284,0.851376147,0.853211009,0.855045872,
0.856880734,0.858715596,0.860550459,0.862385321,0.864220183,0.866055046,
0.867889908,0.869724771,0.871559633,0.873394495,0.875229358,0.87706422,
0.878899083,0.880733945,0.882568807,0.88440367,0.886238532,0.888073394,
0.889908257,0.891743119,0.893577982,0.895412844,0.897247706,0.899082569,
0.900917431,0.902752294,0.904587156,0.906422018,0.908256881,0.910091743,
0.911926606,0.913761468,0.91559633,0.917431193,0.919266055,0.921100917,
0.92293578,0.924770642,0.926605505,0.928440367,0.930275229,0.932110092,
0.933944954,0.935779817,0.937614679,0.939449541,0.941284404,0.943119266,
0.944954128,0.946788991,0.948623853,0.950458716,0.952293578,0.95412844,
0.955963303,0.957798165,0.959633028,0.96146789,0.963302752,0.965137615,
0.966972477,0.968807339,0.970642202,0.972477064,0.974311927,0.976146789,
0.977981651,0.979816514,0.981651376,0.983486239,0.985321101,0.987155963,
0.988990826,0.990825688,0.99266055,0.994495413,0.996330275,0.998165138,
1.),(0.,0.36),.UNSPECIFIED.);
#6264=B_SPLINE_SURFACE_WITH_KNOTS('',5,1,((#234870,#234871),(#234872,#234873),
(#234874,#234875),(#234876,#234877),(#234878,#234879),(#234880,#234881),
(#234882,#234883),(#234884,#234885),(#234886,#234887),(#234888,#234889),
(#234890,#234891),(#234892,#234893),(#234894,#234895),(#234896,#234897),
(#234898,#234899),(#234900,#234901),(#234902,#234903),(#234904,#234905),
(#234906,#234907),(#234908,#234909),(#234910,#234911),(#234912,#234913),
(#234914,#234915),(#234916,#234917),(#234918,#234919),(#234920,#234921),
(#234922,#234923),(#234924,#234925),(#234926,#234927),(#234928,#234929),
(#234930,#234931),(#234932,#234933),(#234934,#234935),(#234936,#234937),
(#234938,#234939),(#234940,#234941),(#234942,#234943),(#234944,#234945),
(#234946,#234947),(#234948,#234949),(#234950,#234951),(#234952,#234953),
(#234954,#234955),(#234956,#234957),(#234958,#234959),(#234960,#234961),
(#234962,#234963),(#234964,#234965),(#234966,#234967),(#234968,#234969),
(#234970,#234971),(#234972,#234973),(#234974,#234975),(#234976,#234977),
(#234978,#234979),(#234980,#234981),(#234982,#234983),(#234984,#234985),
(#234986,#234987),(#234988,#234989),(#234990,#234991),(#234992,#234993),
(#234994,#234995),(#234996,#234997),(#234998,#234999),(#235000,#235001),
(#235002,#235003),(#235004,#235005),(#235006,#235007),(#235008,#235009),
(#235010,#235011),(#235012,#235013),(#235014,#235015),(#235016,#235017),
(#235018,#235019),(#235020,#235021),(#235022,#235023),(#235024,#235025),
(#235026,#235027),(#235028,#235029),(#235030,#235031),(#235032,#235033),
(#235034,#235035),(#235036,#235037),(#235038,#235039),(#235040,#235041),
(#235042,#235043),(#235044,#235045),(#235046,#235047),(#235048,#235049),
(#235050,#235051),(#235052,#235053),(#235054,#235055),(#235056,#235057),
(#235058,#235059),(#235060,#235061),(#235062,#235063),(#235064,#235065),
(#235066,#235067),(#235068,#235069),(#235070,#235071),(#235072,#235073),
(#235074,#235075),(#235076,#235077),(#235078,#235079),(#235080,#235081),
(#235082,#235083),(#235084,#235085),(#235086,#235087),(#235088,#235089),
(#235090,#235091),(#235092,#235093),(#235094,#235095),(#235096,#235097),
(#235098,#235099),(#235100,#235101),(#235102,#235103),(#235104,#235105),
(#235106,#235107),(#235108,#235109),(#235110,#235111),(#235112,#235113),
(#235114,#235115),(#235116,#235117),(#235118,#235119),(#235120,#235121),
(#235122,#235123),(#235124,#235125),(#235126,#235127),(#235128,#235129),
(#235130,#235131),(#235132,#235133),(#235134,#235135),(#235136,#235137),
(#235138,#235139),(#235140,#235141),(#235142,#235143),(#235144,#235145),
(#235146,#235147),(#235148,#235149),(#235150,#235151),(#235152,#235153),
(#235154,#235155),(#235156,#235157),(#235158,#235159),(#235160,#235161),
(#235162,#235163),(#235164,#235165),(#235166,#235167),(#235168,#235169),
(#235170,#235171),(#235172,#235173),(#235174,#235175),(#235176,#235177),
(#235178,#235179),(#235180,#235181),(#235182,#235183),(#235184,#235185),
(#235186,#235187),(#235188,#235189),(#235190,#235191),(#235192,#235193),
(#235194,#235195),(#235196,#235197),(#235198,#235199),(#235200,#235201),
(#235202,#235203),(#235204,#235205),(#235206,#235207),(#235208,#235209),
(#235210,#235211),(#235212,#235213),(#235214,#235215),(#235216,#235217),
(#235218,#235219),(#235220,#235221),(#235222,#235223),(#235224,#235225),
(#235226,#235227),(#235228,#235229),(#235230,#235231),(#235232,#235233),
(#235234,#235235),(#235236,#235237),(#235238,#235239),(#235240,#235241),
(#235242,#235243),(#235244,#235245),(#235246,#235247),(#235248,#235249),
(#235250,#235251),(#235252,#235253),(#235254,#235255),(#235256,#235257),
(#235258,#235259),(#235260,#235261),(#235262,#235263),(#235264,#235265),
(#235266,#235267),(#235268,#235269),(#235270,#235271),(#235272,#235273),
(#235274,#235275),(#235276,#235277),(#235278,#235279),(#235280,#235281),
(#235282,#235283),(#235284,#235285),(#235286,#235287),(#235288,#235289),
(#235290,#235291),(#235292,#235293),(#235294,#235295),(#235296,#235297),
(#235298,#235299),(#235300,#235301),(#235302,#235303),(#235304,#235305),
(#235306,#235307),(#235308,#235309),(#235310,#235311),(#235312,#235313),
(#235314,#235315),(#235316,#235317),(#235318,#235319),(#235320,#235321),
(#235322,#235323),(#235324,#235325),(#235326,#235327),(#235328,#235329),
(#235330,#235331),(#235332,#235333),(#235334,#235335),(#235336,#235337),
(#235338,#235339),(#235340,#235341),(#235342,#235343),(#235344,#235345),
(#235346,#235347),(#235348,#235349),(#235350,#235351),(#235352,#235353),
(#235354,#235355),(#235356,#235357),(#235358,#235359),(#235360,#235361),
(#235362,#235363),(#235364,#235365),(#235366,#235367),(#235368,#235369),
(#235370,#235371),(#235372,#235373),(#235374,#235375),(#235376,#235377),
(#235378,#235379),(#235380,#235381),(#235382,#235383),(#235384,#235385),
(#235386,#235387),(#235388,#235389),(#235390,#235391),(#235392,#235393),
(#235394,#235395),(#235396,#235397),(#235398,#235399),(#235400,#235401),
(#235402,#235403),(#235404,#235405),(#235406,#235407),(#235408,#235409),
(#235410,#235411),(#235412,#235413),(#235414,#235415),(#235416,#235417),
(#235418,#235419),(#235420,#235421),(#235422,#235423),(#235424,#235425),
(#235426,#235427),(#235428,#235429),(#235430,#235431),(#235432,#235433),
(#235434,#235435),(#235436,#235437),(#235438,#235439),(#235440,#235441),
(#235442,#235443),(#235444,#235445),(#235446,#235447),(#235448,#235449),
(#235450,#235451),(#235452,#235453),(#235454,#235455),(#235456,#235457),
(#235458,#235459),(#235460,#235461),(#235462,#235463),(#235464,#235465),
(#235466,#235467),(#235468,#235469),(#235470,#235471),(#235472,#235473),
(#235474,#235475),(#235476,#235477),(#235478,#235479),(#235480,#235481),
(#235482,#235483),(#235484,#235485),(#235486,#235487),(#235488,#235489),
(#235490,#235491),(#235492,#235493),(#235494,#235495),(#235496,#235497),
(#235498,#235499),(#235500,#235501),(#235502,#235503),(#235504,#235505),
(#235506,#235507),(#235508,#235509),(#235510,#235511),(#235512,#235513),
(#235514,#235515),(#235516,#235517),(#235518,#235519),(#235520,#235521),
(#235522,#235523),(#235524,#235525),(#235526,#235527),(#235528,#235529),
(#235530,#235531),(#235532,#235533),(#235534,#235535),(#235536,#235537),
(#235538,#235539),(#235540,#235541),(#235542,#235543),(#235544,#235545),
(#235546,#235547),(#235548,#235549),(#235550,#235551),(#235552,#235553),
(#235554,#235555),(#235556,#235557),(#235558,#235559),(#235560,#235561),
(#235562,#235563),(#235564,#235565),(#235566,#235567),(#235568,#235569),
(#235570,#235571),(#235572,#235573),(#235574,#235575),(#235576,#235577),
(#235578,#235579),(#235580,#235581),(#235582,#235583),(#235584,#235585),
(#235586,#235587),(#235588,#235589),(#235590,#235591),(#235592,#235593),
(#235594,#235595),(#235596,#235597),(#235598,#235599),(#235600,#235601),
(#235602,#235603),(#235604,#235605),(#235606,#235607),(#235608,#235609),
(#235610,#235611),(#235612,#235613),(#235614,#235615),(#235616,#235617),
(#235618,#235619),(#235620,#235621),(#235622,#235623),(#235624,#235625),
(#235626,#235627),(#235628,#235629),(#235630,#235631),(#235632,#235633),
(#235634,#235635),(#235636,#235637),(#235638,#235639),(#235640,#235641),
(#235642,#235643),(#235644,#235645),(#235646,#235647),(#235648,#235649),
(#235650,#235651),(#235652,#235653),(#235654,#235655),(#235656,#235657),
(#235658,#235659),(#235660,#235661),(#235662,#235663),(#235664,#235665),
(#235666,#235667),(#235668,#235669),(#235670,#235671),(#235672,#235673),
(#235674,#235675),(#235676,#235677),(#235678,#235679),(#235680,#235681),
(#235682,#235683),(#235684,#235685),(#235686,#235687),(#235688,#235689),
(#235690,#235691),(#235692,#235693),(#235694,#235695),(#235696,#235697),
(#235698,#235699),(#235700,#235701),(#235702,#235703),(#235704,#235705),
(#235706,#235707),(#235708,#235709),(#235710,#235711),(#235712,#235713),
(#235714,#235715),(#235716,#235717),(#235718,#235719),(#235720,#235721),
(#235722,#235723),(#235724,#235725),(#235726,#235727),(#235728,#235729),
(#235730,#235731),(#235732,#235733),(#235734,#235735),(#235736,#235737),
(#235738,#235739),(#235740,#235741),(#235742,#235743),(#235744,#235745),
(#235746,#235747),(#235748,#235749),(#235750,#235751),(#235752,#235753),
(#235754,#235755),(#235756,#235757),(#235758,#235759),(#235760,#235761),
(#235762,#235763),(#235764,#235765),(#235766,#235767),(#235768,#235769),
(#235770,#235771),(#235772,#235773),(#235774,#235775),(#235776,#235777),
(#235778,#235779),(#235780,#235781),(#235782,#235783),(#235784,#235785),
(#235786,#235787),(#235788,#235789),(#235790,#235791),(#235792,#235793),
(#235794,#235795),(#235796,#235797),(#235798,#235799),(#235800,#235801),
(#235802,#235803),(#235804,#235805),(#235806,#235807),(#235808,#235809),
(#235810,#235811),(#235812,#235813)),.UNSPECIFIED.,.F.,.F.,.F.,(6,1,1,1,
1,1,1,1,1,1,1,1,1,1,1,1,1,1,1,1,1,1,1,1,1,1,1,1,1,1,1,1,1,1,1,1,1,1,1,1,
1,1,1,1,1,1,1,1,1,1,1,1,1,1,1,1,1,1,1,1,1,1,1,1,1,1,1,1,1,1,1,1,1,1,1,1,
1,1,1,1,1,1,1,1,1,1,1,1,1,1,1,1,1,1,1,1,1,1,1,1,1,1,1,1,1,1,1,1,1,1,1,1,
1,1,1,1,1,1,1,1,1,1,1,1,1,1,1,1,1,1,1,1,1,1,1,1,1,1,1,1,1,1,1,1,1,1,1,1,
1,1,1,1,1,1,1,1,1,1,1,1,1,1,1,1,1,1,1,1,1,1,1,1,1,1,1,1,1,1,1,1,1,1,1,1,
1,1,1,1,1,1,1,1,1,1,1,1,1,1,1,1,1,1,1,1,1,1,1,1,1,1,1,1,1,1,1,1,1,1,1,1,
1,1,1,1,1,1,1,1,1,1,1,1,1,1,1,1,1,1,1,1,1,1,1,1,1,1,1,1,1,1,1,1,1,1,1,1,
1,1,1,1,1,1,1,1,1,1,1,1,1,1,1,1,1,1,1,1,1,1,1,1,1,1,1,1,1,1,1,1,1,1,1,1,
1,1,1,1,1,1,1,1,1,1,1,1,1,1,1,1,1,1,1,1,1,1,1,1,1,1,1,1,1,1,1,1,1,1,1,1,
1,1,1,1,1,1,1,1,1,1,1,1,1,1,1,1,1,1,1,1,1,1,1,1,1,1,1,1,1,1,1,1,1,1,1,1,
1,1,1,1,1,1,1,1,1,1,1,1,1,1,1,1,1,1,1,1,1,1,1,1,1,1,1,1,1,1,1,1,1,1,1,1,
1,1,1,1,1,1,1,1,1,1,1,1,1,1,1,1,1,1,1,1,1,1,1,1,1,1,1,1,1,1,1,1,1,1,1,1,
1,1,1,1,1,1,1,1,1,1,1,1,1,1,1,1,1,1,1,1,1,1,1,1,1,1,1,1,1,1,1,6),(2,2),
(-1.,-0.998165138,-0.996330275,-0.994495413,-0.99266055,-0.990825688,-0.988990826,
-0.987155963,-0.985321101,-0.983486239,-0.981651376,-0.979816514,-0.977981651,
-0.976146789,-0.974311927,-0.972477064,-0.970642202,-0.968807339,-0.966972477,
-0.965137615,-0.963302752,-0.96146789,-0.959633028,-0.957798165,-0.955963303,
-0.95412844,-0.952293578,-0.950458716,-0.948623853,-0.946788991,-0.944954128,
-0.943119266,-0.941284404,-0.939449541,-0.937614679,-0.935779817,-0.933944954,
-0.932110092,-0.930275229,-0.928440367,-0.926605505,-0.924770642,-0.92293578,
-0.921100917,-0.919266055,-0.917431193,-0.91559633,-0.913761468,-0.911926606,
-0.910091743,-0.908256881,-0.906422018,-0.904587156,-0.902752294,-0.900917431,
-0.899082569,-0.897247706,-0.895412844,-0.893577982,-0.891743119,-0.889908257,
-0.888073394,-0.886238532,-0.88440367,-0.882568807,-0.880733945,-0.878899083,
-0.87706422,-0.875229358,-0.873394495,-0.871559633,-0.869724771,-0.867889908,
-0.866055046,-0.864220183,-0.862385321,-0.860550459,-0.858715596,-0.856880734,
-0.855045872,-0.853211009,-0.851376147,-0.849541284,-0.847706422,-0.84587156,
-0.844036697,-0.842201835,-0.840366972,-0.83853211,-0.836697248,-0.834862385,
-0.833027523,-0.831192661,-0.829357798,-0.827522936,-0.825688073,-0.823853211,
-0.822018349,-0.820183486,-0.818348624,-0.816513761,-0.814678899,-0.812844037,
-0.811009174,-0.809174312,-0.80733945,-0.805504587,-0.803669725,-0.801834862,
-0.8,-0.798165138,-0.796330275,-0.794495413,-0.79266055,-0.790825688,-0.788990826,
-0.787155963,-0.785321101,-0.783486239,-0.781651376,-0.779816514,-0.777981651,
-0.776146789,-0.774311927,-0.772477064,-0.770642202,-0.768807339,-0.766972477,
-0.765137615,-0.763302752,-0.76146789,-0.759633028,-0.757798165,-0.755963303,
-0.75412844,-0.752293578,-0.750458716,-0.748623853,-0.746788991,-0.744954128,
-0.743119266,-0.741284404,-0.739449541,-0.737614679,-0.735779817,-0.733944954,
-0.732110092,-0.730275229,-0.728440367,-0.726605505,-0.724770642,-0.72293578,
-0.721100917,-0.719266055,-0.717431193,-0.71559633,-0.713761468,-0.711926606,
-0.710091743,-0.708256881,-0.706422018,-0.704587156,-0.702752294,-0.700917431,
-0.699082569,-0.697247706,-0.695412844,-0.693577982,-0.691743119,-0.689908257,
-0.688073394,-0.686238532,-0.68440367,-0.682568807,-0.680733945,-0.678899083,
-0.67706422,-0.675229358,-0.673394495,-0.671559633,-0.669724771,-0.667889908,
-0.666055046,-0.664220183,-0.662385321,-0.660550459,-0.658715596,-0.656880734,
-0.655045872,-0.653211009,-0.651376147,-0.649541284,-0.647706422,-0.64587156,
-0.644036697,-0.642201835,-0.640366972,-0.63853211,-0.636697248,-0.634862385,
-0.633027523,-0.631192661,-0.629357798,-0.627522936,-0.625688073,-0.623853211,
-0.622018349,-0.620183486,-0.618348624,-0.616513761,-0.614678899,-0.612844037,
-0.611009174,-0.609174312,-0.60733945,-0.605504587,-0.603669725,-0.601834862,
-0.6,-0.598165138,-0.596330275,-0.594495413,-0.59266055,-0.590825688,-0.588990826,
-0.587155963,-0.585321101,-0.583486239,-0.581651376,-0.579816514,-0.577981651,
-0.576146789,-0.574311927,-0.572477064,-0.570642202,-0.568807339,-0.566972477,
-0.565137615,-0.563302752,-0.56146789,-0.559633028,-0.557798165,-0.555963303,
-0.55412844,-0.552293578,-0.550458716,-0.548623853,-0.546788991,-0.544954128,
-0.543119266,-0.541284404,-0.539449541,-0.537614679,-0.535779817,-0.533944954,
-0.532110092,-0.530275229,-0.528440367,-0.526605505,-0.524770642,-0.52293578,
-0.521100917,-0.519266055,-0.517431193,-0.51559633,-0.513761468,-0.511926606,
-0.510091743,-0.508256881,-0.506422018,-0.504587156,-0.502752294,-0.500917431,
-0.499082569,-0.497247706,-0.495412844,-0.493577982,-0.491743119,-0.489908257,
-0.488073394,-0.486238532,-0.48440367,-0.482568807,-0.480733945,-0.478899083,
-0.47706422,-0.475229358,-0.473394495,-0.471559633,-0.469724771,-0.467889908,
-0.466055046,-0.464220183,-0.462385321,-0.460550459,-0.458715596,-0.456880734,
-0.455045872,-0.453211009,-0.451376147,-0.449541284,-0.447706422,-0.44587156,
-0.444036697,-0.442201835,-0.440366972,-0.43853211,-0.436697248,-0.434862385,
-0.433027523,-0.431192661,-0.429357798,-0.427522936,-0.425688073,-0.423853211,
-0.422018349,-0.420183486,-0.418348624,-0.416513761,-0.414678899,-0.412844037,
-0.411009174,-0.409174312,-0.40733945,-0.405504587,-0.403669725,-0.401834862,
-0.4,-0.398165138,-0.396330275,-0.394495413,-0.39266055,-0.390825688,-0.388990826,
-0.387155963,-0.385321101,-0.383486239,-0.381651376,-0.379816514,-0.377981651,
-0.376146789,-0.374311927,-0.372477064,-0.370642202,-0.368807339,-0.366972477,
-0.365137615,-0.363302752,-0.36146789,-0.359633028,-0.357798165,-0.355963303,
-0.35412844,-0.352293578,-0.350458716,-0.348623853,-0.346788991,-0.344954128,
-0.343119266,-0.341284404,-0.339449541,-0.337614679,-0.335779817,-0.333944954,
-0.332110092,-0.330275229,-0.328440367,-0.326605505,-0.324770642,-0.32293578,
-0.321100917,-0.319266055,-0.317431193,-0.31559633,-0.313761468,-0.311926606,
-0.310091743,-0.308256881,-0.306422018,-0.304587156,-0.302752294,-0.300917431,
-0.299082569,-0.297247706,-0.295412844,-0.293577982,-0.291743119,-0.289908257,
-0.288073394,-0.286238532,-0.28440367,-0.282568807,-0.280733945,-0.278899083,
-0.27706422,-0.275229358,-0.273394495,-0.271559633,-0.269724771,-0.267889908,
-0.266055046,-0.264220183,-0.262385321,-0.260550459,-0.258715596,-0.256880734,
-0.255045872,-0.253211009,-0.251376147,-0.249541284,-0.247706422,-0.24587156,
-0.244036697,-0.242201835,-0.240366972,-0.23853211,-0.236697248,-0.234862385,
-0.233027523,-0.231192661,-0.229357798,-0.227522936,-0.225688073,-0.223853211,
-0.222018349,-0.220183486,-0.218348624,-0.216513761,-0.214678899,-0.212844037,
-0.211009174,-0.209174312,-0.20733945,-0.205504587,-0.203669725,-0.201834862,
-0.2,-0.198165138,-0.196330275,-0.194495413,-0.19266055,-0.190825688,-0.188990826,
-0.187155963,-0.185321101,-0.183486239,-0.181651376,-0.179816514,-0.177981651,
-0.176146789,-0.174311927,-0.172477064,-0.170642202,-0.168807339,-0.166972477,
-0.165137615,-0.163302752,-0.16146789,-0.159633028,-0.157798165,-0.155963303,
-0.15412844,-0.152293578,-0.150458716,-0.148623853,-0.146788991,-0.144954128,
-0.143172104),(0.,0.36),.UNSPECIFIED.);
#6265=B_SPLINE_SURFACE_WITH_KNOTS('',5,1,((#236446,#236447),(#236448,#236449),
(#236450,#236451),(#236452,#236453),(#236454,#236455),(#236456,#236457),
(#236458,#236459),(#236460,#236461),(#236462,#236463),(#236464,#236465),
(#236466,#236467),(#236468,#236469),(#236470,#236471),(#236472,#236473),
(#236474,#236475),(#236476,#236477),(#236478,#236479),(#236480,#236481),
(#236482,#236483),(#236484,#236485),(#236486,#236487),(#236488,#236489),
(#236490,#236491),(#236492,#236493),(#236494,#236495),(#236496,#236497),
(#236498,#236499),(#236500,#236501),(#236502,#236503),(#236504,#236505),
(#236506,#236507),(#236508,#236509),(#236510,#236511),(#236512,#236513),
(#236514,#236515),(#236516,#236517),(#236518,#236519),(#236520,#236521),
(#236522,#236523),(#236524,#236525),(#236526,#236527),(#236528,#236529),
(#236530,#236531),(#236532,#236533),(#236534,#236535),(#236536,#236537),
(#236538,#236539),(#236540,#236541),(#236542,#236543),(#236544,#236545),
(#236546,#236547),(#236548,#236549),(#236550,#236551),(#236552,#236553),
(#236554,#236555),(#236556,#236557),(#236558,#236559),(#236560,#236561),
(#236562,#236563),(#236564,#236565),(#236566,#236567),(#236568,#236569),
(#236570,#236571),(#236572,#236573),(#236574,#236575),(#236576,#236577),
(#236578,#236579),(#236580,#236581),(#236582,#236583),(#236584,#236585),
(#236586,#236587),(#236588,#236589),(#236590,#236591),(#236592,#236593),
(#236594,#236595),(#236596,#236597),(#236598,#236599),(#236600,#236601),
(#236602,#236603),(#236604,#236605),(#236606,#236607),(#236608,#236609),
(#236610,#236611),(#236612,#236613),(#236614,#236615),(#236616,#236617),
(#236618,#236619),(#236620,#236621),(#236622,#236623),(#236624,#236625),
(#236626,#236627),(#236628,#236629),(#236630,#236631),(#236632,#236633),
(#236634,#236635),(#236636,#236637),(#236638,#236639),(#236640,#236641),
(#236642,#236643),(#236644,#236645),(#236646,#236647),(#236648,#236649),
(#236650,#236651),(#236652,#236653),(#236654,#236655),(#236656,#236657),
(#236658,#236659),(#236660,#236661),(#236662,#236663),(#236664,#236665),
(#236666,#236667),(#236668,#236669),(#236670,#236671),(#236672,#236673),
(#236674,#236675),(#236676,#236677),(#236678,#236679),(#236680,#236681),
(#236682,#236683),(#236684,#236685),(#236686,#236687),(#236688,#236689),
(#236690,#236691),(#236692,#236693),(#236694,#236695),(#236696,#236697),
(#236698,#236699),(#236700,#236701),(#236702,#236703),(#236704,#236705),
(#236706,#236707),(#236708,#236709),(#236710,#236711),(#236712,#236713),
(#236714,#236715),(#236716,#236717),(#236718,#236719),(#236720,#236721),
(#236722,#236723),(#236724,#236725),(#236726,#236727),(#236728,#236729),
(#236730,#236731),(#236732,#236733),(#236734,#236735),(#236736,#236737),
(#236738,#236739),(#236740,#236741),(#236742,#236743),(#236744,#236745),
(#236746,#236747),(#236748,#236749),(#236750,#236751),(#236752,#236753),
(#236754,#236755),(#236756,#236757),(#236758,#236759),(#236760,#236761),
(#236762,#236763),(#236764,#236765),(#236766,#236767),(#236768,#236769),
(#236770,#236771),(#236772,#236773),(#236774,#236775),(#236776,#236777),
(#236778,#236779),(#236780,#236781),(#236782,#236783),(#236784,#236785),
(#236786,#236787),(#236788,#236789),(#236790,#236791),(#236792,#236793),
(#236794,#236795),(#236796,#236797),(#236798,#236799),(#236800,#236801),
(#236802,#236803),(#236804,#236805),(#236806,#236807),(#236808,#236809),
(#236810,#236811),(#236812,#236813),(#236814,#236815),(#236816,#236817),
(#236818,#236819),(#236820,#236821),(#236822,#236823),(#236824,#236825),
(#236826,#236827),(#236828,#236829),(#236830,#236831),(#236832,#236833),
(#236834,#236835),(#236836,#236837),(#236838,#236839),(#236840,#236841),
(#236842,#236843),(#236844,#236845),(#236846,#236847),(#236848,#236849),
(#236850,#236851),(#236852,#236853),(#236854,#236855),(#236856,#236857),
(#236858,#236859),(#236860,#236861),(#236862,#236863),(#236864,#236865),
(#236866,#236867),(#236868,#236869),(#236870,#236871),(#236872,#236873),
(#236874,#236875),(#236876,#236877),(#236878,#236879),(#236880,#236881),
(#236882,#236883),(#236884,#236885),(#236886,#236887),(#236888,#236889),
(#236890,#236891),(#236892,#236893),(#236894,#236895),(#236896,#236897),
(#236898,#236899),(#236900,#236901),(#236902,#236903),(#236904,#236905),
(#236906,#236907),(#236908,#236909),(#236910,#236911),(#236912,#236913),
(#236914,#236915),(#236916,#236917),(#236918,#236919),(#236920,#236921),
(#236922,#236923),(#236924,#236925),(#236926,#236927),(#236928,#236929),
(#236930,#236931),(#236932,#236933),(#236934,#236935),(#236936,#236937),
(#236938,#236939),(#236940,#236941),(#236942,#236943),(#236944,#236945),
(#236946,#236947),(#236948,#236949),(#236950,#236951),(#236952,#236953),
(#236954,#236955),(#236956,#236957),(#236958,#236959),(#236960,#236961),
(#236962,#236963),(#236964,#236965),(#236966,#236967),(#236968,#236969),
(#236970,#236971),(#236972,#236973),(#236974,#236975),(#236976,#236977),
(#236978,#236979),(#236980,#236981),(#236982,#236983),(#236984,#236985),
(#236986,#236987),(#236988,#236989),(#236990,#236991),(#236992,#236993),
(#236994,#236995),(#236996,#236997),(#236998,#236999),(#237000,#237001),
(#237002,#237003),(#237004,#237005),(#237006,#237007),(#237008,#237009),
(#237010,#237011),(#237012,#237013),(#237014,#237015),(#237016,#237017),
(#237018,#237019),(#237020,#237021),(#237022,#237023),(#237024,#237025),
(#237026,#237027),(#237028,#237029),(#237030,#237031),(#237032,#237033),
(#237034,#237035),(#237036,#237037),(#237038,#237039),(#237040,#237041),
(#237042,#237043),(#237044,#237045),(#237046,#237047),(#237048,#237049),
(#237050,#237051),(#237052,#237053),(#237054,#237055),(#237056,#237057),
(#237058,#237059),(#237060,#237061),(#237062,#237063),(#237064,#237065),
(#237066,#237067),(#237068,#237069),(#237070,#237071),(#237072,#237073),
(#237074,#237075),(#237076,#237077),(#237078,#237079),(#237080,#237081),
(#237082,#237083),(#237084,#237085),(#237086,#237087),(#237088,#237089),
(#237090,#237091),(#237092,#237093),(#237094,#237095),(#237096,#237097),
(#237098,#237099),(#237100,#237101),(#237102,#237103),(#237104,#237105),
(#237106,#237107),(#237108,#237109),(#237110,#237111),(#237112,#237113),
(#237114,#237115),(#237116,#237117),(#237118,#237119),(#237120,#237121),
(#237122,#237123),(#237124,#237125),(#237126,#237127),(#237128,#237129),
(#237130,#237131),(#237132,#237133),(#237134,#237135),(#237136,#237137),
(#237138,#237139),(#237140,#237141),(#237142,#237143),(#237144,#237145),
(#237146,#237147),(#237148,#237149),(#237150,#237151),(#237152,#237153),
(#237154,#237155),(#237156,#237157),(#237158,#237159),(#237160,#237161),
(#237162,#237163),(#237164,#237165),(#237166,#237167),(#237168,#237169),
(#237170,#237171),(#237172,#237173),(#237174,#237175),(#237176,#237177),
(#237178,#237179),(#237180,#237181),(#237182,#237183),(#237184,#237185),
(#237186,#237187),(#237188,#237189),(#237190,#237191),(#237192,#237193),
(#237194,#237195),(#237196,#237197),(#237198,#237199),(#237200,#237201),
(#237202,#237203),(#237204,#237205),(#237206,#237207),(#237208,#237209),
(#237210,#237211),(#237212,#237213),(#237214,#237215),(#237216,#237217),
(#237218,#237219),(#237220,#237221),(#237222,#237223),(#237224,#237225),
(#237226,#237227),(#237228,#237229),(#237230,#237231),(#237232,#237233),
(#237234,#237235),(#237236,#237237),(#237238,#237239),(#237240,#237241),
(#237242,#237243),(#237244,#237245),(#237246,#237247),(#237248,#237249),
(#237250,#237251),(#237252,#237253),(#237254,#237255),(#237256,#237257),
(#237258,#237259),(#237260,#237261),(#237262,#237263),(#237264,#237265),
(#237266,#237267),(#237268,#237269),(#237270,#237271),(#237272,#237273),
(#237274,#237275),(#237276,#237277),(#237278,#237279),(#237280,#237281),
(#237282,#237283),(#237284,#237285),(#237286,#237287),(#237288,#237289),
(#237290,#237291),(#237292,#237293),(#237294,#237295),(#237296,#237297),
(#237298,#237299),(#237300,#237301),(#237302,#237303),(#237304,#237305),
(#237306,#237307),(#237308,#237309),(#237310,#237311),(#237312,#237313),
(#237314,#237315),(#237316,#237317),(#237318,#237319),(#237320,#237321),
(#237322,#237323),(#237324,#237325),(#237326,#237327),(#237328,#237329),
(#237330,#237331),(#237332,#237333),(#237334,#237335),(#237336,#237337),
(#237338,#237339),(#237340,#237341),(#237342,#237343),(#237344,#237345),
(#237346,#237347),(#237348,#237349),(#237350,#237351),(#237352,#237353),
(#237354,#237355),(#237356,#237357),(#237358,#237359),(#237360,#237361),
(#237362,#237363),(#237364,#237365),(#237366,#237367),(#237368,#237369),
(#237370,#237371),(#237372,#237373),(#237374,#237375),(#237376,#237377),
(#237378,#237379),(#237380,#237381),(#237382,#237383),(#237384,#237385),
(#237386,#237387),(#237388,#237389)),.UNSPECIFIED.,.F.,.F.,.F.,(6,1,1,1,
1,1,1,1,1,1,1,1,1,1,1,1,1,1,1,1,1,1,1,1,1,1,1,1,1,1,1,1,1,1,1,1,1,1,1,1,
1,1,1,1,1,1,1,1,1,1,1,1,1,1,1,1,1,1,1,1,1,1,1,1,1,1,1,1,1,1,1,1,1,1,1,1,
1,1,1,1,1,1,1,1,1,1,1,1,1,1,1,1,1,1,1,1,1,1,1,1,1,1,1,1,1,1,1,1,1,1,1,1,
1,1,1,1,1,1,1,1,1,1,1,1,1,1,1,1,1,1,1,1,1,1,1,1,1,1,1,1,1,1,1,1,1,1,1,1,
1,1,1,1,1,1,1,1,1,1,1,1,1,1,1,1,1,1,1,1,1,1,1,1,1,1,1,1,1,1,1,1,1,1,1,1,
1,1,1,1,1,1,1,1,1,1,1,1,1,1,1,1,1,1,1,1,1,1,1,1,1,1,1,1,1,1,1,1,1,1,1,1,
1,1,1,1,1,1,1,1,1,1,1,1,1,1,1,1,1,1,1,1,1,1,1,1,1,1,1,1,1,1,1,1,1,1,1,1,
1,1,1,1,1,1,1,1,1,1,1,1,1,1,1,1,1,1,1,1,1,1,1,1,1,1,1,1,1,1,1,1,1,1,1,1,
1,1,1,1,1,1,1,1,1,1,1,1,1,1,1,1,1,1,1,1,1,1,1,1,1,1,1,1,1,1,1,1,1,1,1,1,
1,1,1,1,1,1,1,1,1,1,1,1,1,1,1,1,1,1,1,1,1,1,1,1,1,1,1,1,1,1,1,1,1,1,1,1,
1,1,1,1,1,1,1,1,1,1,1,1,1,1,1,1,1,1,1,1,1,1,1,1,1,1,1,1,1,1,1,1,1,1,1,1,
1,1,1,1,1,1,1,1,1,1,1,1,1,1,1,1,1,1,1,1,1,1,1,1,1,1,1,1,1,1,1,1,1,1,1,1,
1,1,1,1,1,1,1,1,1,1,1,1,1,1,1,1,1,1,1,1,1,1,1,1,1,1,1,1,1,1,1,6),(2,2),
(-1.,-0.998165138,-0.996330275,-0.994495413,-0.99266055,-0.990825688,-0.988990826,
-0.987155963,-0.985321101,-0.983486239,-0.981651376,-0.979816514,-0.977981651,
-0.976146789,-0.974311927,-0.972477064,-0.970642202,-0.968807339,-0.966972477,
-0.965137615,-0.963302752,-0.96146789,-0.959633028,-0.957798165,-0.955963303,
-0.95412844,-0.952293578,-0.950458716,-0.948623853,-0.946788991,-0.944954128,
-0.943119266,-0.941284404,-0.939449541,-0.937614679,-0.935779817,-0.933944954,
-0.932110092,-0.930275229,-0.928440367,-0.926605505,-0.924770642,-0.92293578,
-0.921100917,-0.919266055,-0.917431193,-0.91559633,-0.913761468,-0.911926606,
-0.910091743,-0.908256881,-0.906422018,-0.904587156,-0.902752294,-0.900917431,
-0.899082569,-0.897247706,-0.895412844,-0.893577982,-0.891743119,-0.889908257,
-0.888073394,-0.886238532,-0.88440367,-0.882568807,-0.880733945,-0.878899083,
-0.87706422,-0.875229358,-0.873394495,-0.871559633,-0.869724771,-0.867889908,
-0.866055046,-0.864220183,-0.862385321,-0.860550459,-0.858715596,-0.856880734,
-0.855045872,-0.853211009,-0.851376147,-0.849541284,-0.847706422,-0.84587156,
-0.844036697,-0.842201835,-0.840366972,-0.83853211,-0.836697248,-0.834862385,
-0.833027523,-0.831192661,-0.829357798,-0.827522936,-0.825688073,-0.823853211,
-0.822018349,-0.820183486,-0.818348624,-0.816513761,-0.814678899,-0.812844037,
-0.811009174,-0.809174312,-0.80733945,-0.805504587,-0.803669725,-0.801834862,
-0.8,-0.798165138,-0.796330275,-0.794495413,-0.79266055,-0.790825688,-0.788990826,
-0.787155963,-0.785321101,-0.783486239,-0.781651376,-0.779816514,-0.777981651,
-0.776146789,-0.774311927,-0.772477064,-0.770642202,-0.768807339,-0.766972477,
-0.765137615,-0.763302752,-0.76146789,-0.759633028,-0.757798165,-0.755963303,
-0.75412844,-0.752293578,-0.750458716,-0.748623853,-0.746788991,-0.744954128,
-0.743119266,-0.741284404,-0.739449541,-0.737614679,-0.735779817,-0.733944954,
-0.732110092,-0.730275229,-0.728440367,-0.726605505,-0.724770642,-0.72293578,
-0.721100917,-0.719266055,-0.717431193,-0.71559633,-0.713761468,-0.711926606,
-0.710091743,-0.708256881,-0.706422018,-0.704587156,-0.702752294,-0.700917431,
-0.699082569,-0.697247706,-0.695412844,-0.693577982,-0.691743119,-0.689908257,
-0.688073394,-0.686238532,-0.68440367,-0.682568807,-0.680733945,-0.678899083,
-0.67706422,-0.675229358,-0.673394495,-0.671559633,-0.669724771,-0.667889908,
-0.666055046,-0.664220183,-0.662385321,-0.660550459,-0.658715596,-0.656880734,
-0.655045872,-0.653211009,-0.651376147,-0.649541284,-0.647706422,-0.64587156,
-0.644036697,-0.642201835,-0.640366972,-0.63853211,-0.636697248,-0.634862385,
-0.633027523,-0.631192661,-0.629357798,-0.627522936,-0.625688073,-0.623853211,
-0.622018349,-0.620183486,-0.618348624,-0.616513761,-0.614678899,-0.612844037,
-0.611009174,-0.609174312,-0.60733945,-0.605504587,-0.603669725,-0.601834862,
-0.6,-0.598165138,-0.596330275,-0.594495413,-0.59266055,-0.590825688,-0.588990826,
-0.587155963,-0.585321101,-0.583486239,-0.581651376,-0.579816514,-0.577981651,
-0.576146789,-0.574311927,-0.572477064,-0.570642202,-0.568807339,-0.566972477,
-0.565137615,-0.563302752,-0.56146789,-0.559633028,-0.557798165,-0.555963303,
-0.55412844,-0.552293578,-0.550458716,-0.548623853,-0.546788991,-0.544954128,
-0.543119266,-0.541284404,-0.539449541,-0.537614679,-0.535779817,-0.533944954,
-0.532110092,-0.530275229,-0.528440367,-0.526605505,-0.524770642,-0.52293578,
-0.521100917,-0.519266055,-0.517431193,-0.51559633,-0.513761468,-0.511926606,
-0.510091743,-0.508256881,-0.506422018,-0.504587156,-0.502752294,-0.500917431,
-0.499082569,-0.497247706,-0.495412844,-0.493577982,-0.491743119,-0.489908257,
-0.488073394,-0.486238532,-0.48440367,-0.482568807,-0.480733945,-0.478899083,
-0.47706422,-0.475229358,-0.473394495,-0.471559633,-0.469724771,-0.467889908,
-0.466055046,-0.464220183,-0.462385321,-0.460550459,-0.458715596,-0.456880734,
-0.455045872,-0.453211009,-0.451376147,-0.449541284,-0.447706422,-0.44587156,
-0.444036697,-0.442201835,-0.440366972,-0.43853211,-0.436697248,-0.434862385,
-0.433027523,-0.431192661,-0.429357798,-0.427522936,-0.425688073,-0.423853211,
-0.422018349,-0.420183486,-0.418348624,-0.416513761,-0.414678899,-0.412844037,
-0.411009174,-0.409174312,-0.40733945,-0.405504587,-0.403669725,-0.401834862,
-0.4,-0.398165138,-0.396330275,-0.394495413,-0.39266055,-0.390825688,-0.388990826,
-0.387155963,-0.385321101,-0.383486239,-0.381651376,-0.379816514,-0.377981651,
-0.376146789,-0.374311927,-0.372477064,-0.370642202,-0.368807339,-0.366972477,
-0.365137615,-0.363302752,-0.36146789,-0.359633028,-0.357798165,-0.355963303,
-0.35412844,-0.352293578,-0.350458716,-0.348623853,-0.346788991,-0.344954128,
-0.343119266,-0.341284404,-0.339449541,-0.337614679,-0.335779817,-0.333944954,
-0.332110092,-0.330275229,-0.328440367,-0.326605505,-0.324770642,-0.32293578,
-0.321100917,-0.319266055,-0.317431193,-0.31559633,-0.313761468,-0.311926606,
-0.310091743,-0.308256881,-0.306422018,-0.304587156,-0.302752294,-0.300917431,
-0.299082569,-0.297247706,-0.295412844,-0.293577982,-0.291743119,-0.289908257,
-0.288073394,-0.286238532,-0.28440367,-0.282568807,-0.280733945,-0.278899083,
-0.27706422,-0.275229358,-0.273394495,-0.271559633,-0.269724771,-0.267889908,
-0.266055046,-0.264220183,-0.262385321,-0.260550459,-0.258715596,-0.256880734,
-0.255045872,-0.253211009,-0.251376147,-0.249541284,-0.247706422,-0.24587156,
-0.244036697,-0.242201835,-0.240366972,-0.23853211,-0.236697248,-0.234862385,
-0.233027523,-0.231192661,-0.229357798,-0.227522936,-0.225688073,-0.223853211,
-0.222018349,-0.220183486,-0.218348624,-0.216513761,-0.214678899,-0.212844037,
-0.211009174,-0.209174312,-0.20733945,-0.205504587,-0.203669725,-0.201834862,
-0.2,-0.198165138,-0.196330275,-0.194495413,-0.19266055,-0.190825688,-0.188990826,
-0.187155963,-0.185321101,-0.183486239,-0.181651376,-0.179816514,-0.177981651,
-0.176146789,-0.174311927,-0.172477064,-0.170642202,-0.168807339,-0.166972477,
-0.165137615,-0.163302752,-0.16146789,-0.159633028,-0.157798165,-0.155963303,
-0.15412844,-0.152293578,-0.150458716,-0.148623853,-0.146788991,-0.144954128,
-0.143172103),(0.,0.36),.UNSPECIFIED.);
#6266=B_SPLINE_SURFACE_WITH_KNOTS('',5,1,((#238022,#238023),(#238024,#238025),
(#238026,#238027),(#238028,#238029),(#238030,#238031),(#238032,#238033),
(#238034,#238035),(#238036,#238037),(#238038,#238039),(#238040,#238041),
(#238042,#238043),(#238044,#238045),(#238046,#238047),(#238048,#238049),
(#238050,#238051),(#238052,#238053),(#238054,#238055),(#238056,#238057),
(#238058,#238059),(#238060,#238061),(#238062,#238063),(#238064,#238065),
(#238066,#238067),(#238068,#238069),(#238070,#238071),(#238072,#238073),
(#238074,#238075),(#238076,#238077),(#238078,#238079),(#238080,#238081),
(#238082,#238083),(#238084,#238085),(#238086,#238087),(#238088,#238089),
(#238090,#238091),(#238092,#238093),(#238094,#238095),(#238096,#238097),
(#238098,#238099),(#238100,#238101),(#238102,#238103),(#238104,#238105),
(#238106,#238107),(#238108,#238109),(#238110,#238111),(#238112,#238113),
(#238114,#238115),(#238116,#238117),(#238118,#238119),(#238120,#238121),
(#238122,#238123),(#238124,#238125),(#238126,#238127),(#238128,#238129),
(#238130,#238131),(#238132,#238133),(#238134,#238135),(#238136,#238137),
(#238138,#238139),(#238140,#238141),(#238142,#238143),(#238144,#238145),
(#238146,#238147),(#238148,#238149),(#238150,#238151),(#238152,#238153),
(#238154,#238155),(#238156,#238157),(#238158,#238159),(#238160,#238161),
(#238162,#238163),(#238164,#238165),(#238166,#238167),(#238168,#238169),
(#238170,#238171),(#238172,#238173),(#238174,#238175),(#238176,#238177),
(#238178,#238179),(#238180,#238181),(#238182,#238183),(#238184,#238185),
(#238186,#238187),(#238188,#238189),(#238190,#238191),(#238192,#238193),
(#238194,#238195),(#238196,#238197),(#238198,#238199),(#238200,#238201),
(#238202,#238203),(#238204,#238205),(#238206,#238207),(#238208,#238209),
(#238210,#238211),(#238212,#238213),(#238214,#238215),(#238216,#238217),
(#238218,#238219),(#238220,#238221),(#238222,#238223),(#238224,#238225),
(#238226,#238227),(#238228,#238229),(#238230,#238231),(#238232,#238233),
(#238234,#238235),(#238236,#238237),(#238238,#238239),(#238240,#238241),
(#238242,#238243),(#238244,#238245),(#238246,#238247),(#238248,#238249),
(#238250,#238251),(#238252,#238253),(#238254,#238255),(#238256,#238257),
(#238258,#238259),(#238260,#238261),(#238262,#238263),(#238264,#238265),
(#238266,#238267),(#238268,#238269),(#238270,#238271),(#238272,#238273),
(#238274,#238275),(#238276,#238277),(#238278,#238279),(#238280,#238281),
(#238282,#238283),(#238284,#238285),(#238286,#238287),(#238288,#238289),
(#238290,#238291),(#238292,#238293),(#238294,#238295),(#238296,#238297),
(#238298,#238299),(#238300,#238301),(#238302,#238303),(#238304,#238305),
(#238306,#238307),(#238308,#238309),(#238310,#238311),(#238312,#238313),
(#238314,#238315),(#238316,#238317),(#238318,#238319),(#238320,#238321),
(#238322,#238323),(#238324,#238325),(#238326,#238327),(#238328,#238329),
(#238330,#238331),(#238332,#238333),(#238334,#238335),(#238336,#238337),
(#238338,#238339),(#238340,#238341),(#238342,#238343),(#238344,#238345),
(#238346,#238347),(#238348,#238349),(#238350,#238351),(#238352,#238353),
(#238354,#238355),(#238356,#238357),(#238358,#238359),(#238360,#238361),
(#238362,#238363),(#238364,#238365),(#238366,#238367),(#238368,#238369),
(#238370,#238371),(#238372,#238373),(#238374,#238375),(#238376,#238377),
(#238378,#238379),(#238380,#238381),(#238382,#238383),(#238384,#238385),
(#238386,#238387),(#238388,#238389),(#238390,#238391),(#238392,#238393),
(#238394,#238395),(#238396,#238397),(#238398,#238399),(#238400,#238401),
(#238402,#238403),(#238404,#238405),(#238406,#238407),(#238408,#238409),
(#238410,#238411),(#238412,#238413),(#238414,#238415),(#238416,#238417),
(#238418,#238419),(#238420,#238421),(#238422,#238423),(#238424,#238425),
(#238426,#238427),(#238428,#238429),(#238430,#238431),(#238432,#238433),
(#238434,#238435),(#238436,#238437),(#238438,#238439),(#238440,#238441),
(#238442,#238443),(#238444,#238445),(#238446,#238447),(#238448,#238449),
(#238450,#238451),(#238452,#238453),(#238454,#238455),(#238456,#238457),
(#238458,#238459),(#238460,#238461),(#238462,#238463),(#238464,#238465),
(#238466,#238467),(#238468,#238469),(#238470,#238471),(#238472,#238473),
(#238474,#238475),(#238476,#238477),(#238478,#238479),(#238480,#238481),
(#238482,#238483),(#238484,#238485),(#238486,#238487),(#238488,#238489),
(#238490,#238491),(#238492,#238493),(#238494,#238495),(#238496,#238497),
(#238498,#238499),(#238500,#238501),(#238502,#238503),(#238504,#238505),
(#238506,#238507),(#238508,#238509),(#238510,#238511),(#238512,#238513),
(#238514,#238515),(#238516,#238517),(#238518,#238519),(#238520,#238521),
(#238522,#238523),(#238524,#238525),(#238526,#238527),(#238528,#238529),
(#238530,#238531),(#238532,#238533),(#238534,#238535),(#238536,#238537),
(#238538,#238539),(#238540,#238541),(#238542,#238543),(#238544,#238545),
(#238546,#238547),(#238548,#238549),(#238550,#238551),(#238552,#238553),
(#238554,#238555),(#238556,#238557),(#238558,#238559),(#238560,#238561),
(#238562,#238563),(#238564,#238565),(#238566,#238567),(#238568,#238569),
(#238570,#238571),(#238572,#238573),(#238574,#238575),(#238576,#238577),
(#238578,#238579),(#238580,#238581),(#238582,#238583),(#238584,#238585),
(#238586,#238587),(#238588,#238589),(#238590,#238591),(#238592,#238593),
(#238594,#238595),(#238596,#238597),(#238598,#238599),(#238600,#238601),
(#238602,#238603),(#238604,#238605),(#238606,#238607),(#238608,#238609),
(#238610,#238611),(#238612,#238613),(#238614,#238615),(#238616,#238617),
(#238618,#238619),(#238620,#238621),(#238622,#238623),(#238624,#238625),
(#238626,#238627),(#238628,#238629),(#238630,#238631),(#238632,#238633),
(#238634,#238635),(#238636,#238637),(#238638,#238639),(#238640,#238641),
(#238642,#238643),(#238644,#238645),(#238646,#238647),(#238648,#238649),
(#238650,#238651),(#238652,#238653),(#238654,#238655),(#238656,#238657),
(#238658,#238659),(#238660,#238661),(#238662,#238663),(#238664,#238665),
(#238666,#238667),(#238668,#238669),(#238670,#238671),(#238672,#238673),
(#238674,#238675),(#238676,#238677),(#238678,#238679),(#238680,#238681),
(#238682,#238683),(#238684,#238685),(#238686,#238687),(#238688,#238689),
(#238690,#238691),(#238692,#238693),(#238694,#238695),(#238696,#238697),
(#238698,#238699),(#238700,#238701),(#238702,#238703),(#238704,#238705),
(#238706,#238707),(#238708,#238709),(#238710,#238711),(#238712,#238713),
(#238714,#238715),(#238716,#238717),(#238718,#238719),(#238720,#238721),
(#238722,#238723),(#238724,#238725),(#238726,#238727),(#238728,#238729),
(#238730,#238731),(#238732,#238733),(#238734,#238735),(#238736,#238737),
(#238738,#238739),(#238740,#238741),(#238742,#238743),(#238744,#238745),
(#238746,#238747),(#238748,#238749),(#238750,#238751),(#238752,#238753),
(#238754,#238755),(#238756,#238757),(#238758,#238759),(#238760,#238761),
(#238762,#238763),(#238764,#238765),(#238766,#238767),(#238768,#238769),
(#238770,#238771),(#238772,#238773),(#238774,#238775),(#238776,#238777),
(#238778,#238779),(#238780,#238781),(#238782,#238783),(#238784,#238785),
(#238786,#238787),(#238788,#238789),(#238790,#238791),(#238792,#238793),
(#238794,#238795),(#238796,#238797),(#238798,#238799),(#238800,#238801),
(#238802,#238803),(#238804,#238805),(#238806,#238807),(#238808,#238809),
(#238810,#238811),(#238812,#238813),(#238814,#238815),(#238816,#238817),
(#238818,#238819),(#238820,#238821),(#238822,#238823),(#238824,#238825),
(#238826,#238827),(#238828,#238829),(#238830,#238831),(#238832,#238833),
(#238834,#238835),(#238836,#238837),(#238838,#238839),(#238840,#238841),
(#238842,#238843),(#238844,#238845),(#238846,#238847),(#238848,#238849),
(#238850,#238851),(#238852,#238853),(#238854,#238855),(#238856,#238857),
(#238858,#238859),(#238860,#238861),(#238862,#238863),(#238864,#238865),
(#238866,#238867),(#238868,#238869),(#238870,#238871),(#238872,#238873),
(#238874,#238875),(#238876,#238877),(#238878,#238879),(#238880,#238881),
(#238882,#238883),(#238884,#238885),(#238886,#238887),(#238888,#238889),
(#238890,#238891),(#238892,#238893),(#238894,#238895),(#238896,#238897),
(#238898,#238899),(#238900,#238901),(#238902,#238903),(#238904,#238905),
(#238906,#238907),(#238908,#238909),(#238910,#238911),(#238912,#238913),
(#238914,#238915),(#238916,#238917),(#238918,#238919),(#238920,#238921),
(#238922,#238923),(#238924,#238925),(#238926,#238927),(#238928,#238929),
(#238930,#238931),(#238932,#238933),(#238934,#238935),(#238936,#238937),
(#238938,#238939),(#238940,#238941),(#238942,#238943),(#238944,#238945),
(#238946,#238947),(#238948,#238949),(#238950,#238951),(#238952,#238953),
(#238954,#238955),(#238956,#238957),(#238958,#238959),(#238960,#238961),
(#238962,#238963),(#238964,#238965)),.UNSPECIFIED.,.F.,.F.,.F.,(6,1,1,1,
1,1,1,1,1,1,1,1,1,1,1,1,1,1,1,1,1,1,1,1,1,1,1,1,1,1,1,1,1,1,1,1,1,1,1,1,
1,1,1,1,1,1,1,1,1,1,1,1,1,1,1,1,1,1,1,1,1,1,1,1,1,1,1,1,1,1,1,1,1,1,1,1,
1,1,1,1,1,1,1,1,1,1,1,1,1,1,1,1,1,1,1,1,1,1,1,1,1,1,1,1,1,1,1,1,1,1,1,1,
1,1,1,1,1,1,1,1,1,1,1,1,1,1,1,1,1,1,1,1,1,1,1,1,1,1,1,1,1,1,1,1,1,1,1,1,
1,1,1,1,1,1,1,1,1,1,1,1,1,1,1,1,1,1,1,1,1,1,1,1,1,1,1,1,1,1,1,1,1,1,1,1,
1,1,1,1,1,1,1,1,1,1,1,1,1,1,1,1,1,1,1,1,1,1,1,1,1,1,1,1,1,1,1,1,1,1,1,1,
1,1,1,1,1,1,1,1,1,1,1,1,1,1,1,1,1,1,1,1,1,1,1,1,1,1,1,1,1,1,1,1,1,1,1,1,
1,1,1,1,1,1,1,1,1,1,1,1,1,1,1,1,1,1,1,1,1,1,1,1,1,1,1,1,1,1,1,1,1,1,1,1,
1,1,1,1,1,1,1,1,1,1,1,1,1,1,1,1,1,1,1,1,1,1,1,1,1,1,1,1,1,1,1,1,1,1,1,1,
1,1,1,1,1,1,1,1,1,1,1,1,1,1,1,1,1,1,1,1,1,1,1,1,1,1,1,1,1,1,1,1,1,1,1,1,
1,1,1,1,1,1,1,1,1,1,1,1,1,1,1,1,1,1,1,1,1,1,1,1,1,1,1,1,1,1,1,1,1,1,1,1,
1,1,1,1,1,1,1,1,1,1,1,1,1,1,1,1,1,1,1,1,1,1,1,1,1,1,1,1,1,1,1,1,1,1,1,1,
1,1,1,1,1,1,1,1,1,1,1,1,1,1,1,1,1,1,1,1,1,1,1,1,1,1,1,1,1,1,1,6),(2,2),
(0.143172104,0.144954128,0.146788991,0.148623853,0.150458716,0.152293578,
0.15412844,0.155963303,0.157798165,0.159633028,0.16146789,0.163302752,0.165137615,
0.166972477,0.168807339,0.170642202,0.172477064,0.174311927,0.176146789,
0.177981651,0.179816514,0.181651376,0.183486239,0.185321101,0.187155963,
0.188990826,0.190825688,0.19266055,0.194495413,0.196330275,0.198165138,
0.2,0.201834862,0.203669725,0.205504587,0.20733945,0.209174312,0.211009174,
0.212844037,0.214678899,0.216513761,0.218348624,0.220183486,0.222018349,
0.223853211,0.225688073,0.227522936,0.229357798,0.231192661,0.233027523,
0.234862385,0.236697248,0.23853211,0.240366972,0.242201835,0.244036697,
0.24587156,0.247706422,0.249541284,0.251376147,0.253211009,0.255045872,
0.256880734,0.258715596,0.260550459,0.262385321,0.264220183,0.266055046,
0.267889908,0.269724771,0.271559633,0.273394495,0.275229358,0.27706422,
0.278899083,0.280733945,0.282568807,0.28440367,0.286238532,0.288073394,
0.289908257,0.291743119,0.293577982,0.295412844,0.297247706,0.299082569,
0.300917431,0.302752294,0.304587156,0.306422018,0.308256881,0.310091743,
0.311926606,0.313761468,0.31559633,0.317431193,0.319266055,0.321100917,
0.32293578,0.324770642,0.326605505,0.328440367,0.330275229,0.332110092,
0.333944954,0.335779817,0.337614679,0.339449541,0.341284404,0.343119266,
0.344954128,0.346788991,0.348623853,0.350458716,0.352293578,0.35412844,
0.355963303,0.357798165,0.359633028,0.36146789,0.363302752,0.365137615,
0.366972477,0.368807339,0.370642202,0.372477064,0.374311927,0.376146789,
0.377981651,0.379816514,0.381651376,0.383486239,0.385321101,0.387155963,
0.388990826,0.390825688,0.39266055,0.394495413,0.396330275,0.398165138,
0.4,0.401834862,0.403669725,0.405504587,0.40733945,0.409174312,0.411009174,
0.412844037,0.414678899,0.416513761,0.418348624,0.420183486,0.422018349,
0.423853211,0.425688073,0.427522936,0.429357798,0.431192661,0.433027523,
0.434862385,0.436697248,0.43853211,0.440366972,0.442201835,0.444036697,
0.44587156,0.447706422,0.449541284,0.451376147,0.453211009,0.455045872,
0.456880734,0.458715596,0.460550459,0.462385321,0.464220183,0.466055046,
0.467889908,0.469724771,0.471559633,0.473394495,0.475229358,0.47706422,
0.478899083,0.480733945,0.482568807,0.48440367,0.486238532,0.488073394,
0.489908257,0.491743119,0.493577982,0.495412844,0.497247706,0.499082569,
0.500917431,0.502752294,0.504587156,0.506422018,0.508256881,0.510091743,
0.511926606,0.513761468,0.51559633,0.517431193,0.519266055,0.521100917,
0.52293578,0.524770642,0.526605505,0.528440367,0.530275229,0.532110092,
0.533944954,0.535779817,0.537614679,0.539449541,0.541284404,0.543119266,
0.544954128,0.546788991,0.548623853,0.550458716,0.552293578,0.55412844,
0.555963303,0.557798165,0.559633028,0.56146789,0.563302752,0.565137615,
0.566972477,0.568807339,0.570642202,0.572477064,0.574311927,0.576146789,
0.577981651,0.579816514,0.581651376,0.583486239,0.585321101,0.587155963,
0.588990826,0.590825688,0.59266055,0.594495413,0.596330275,0.598165138,
0.6,0.601834862,0.603669725,0.605504587,0.60733945,0.609174312,0.611009174,
0.612844037,0.614678899,0.616513761,0.618348624,0.620183486,0.622018349,
0.623853211,0.625688073,0.627522936,0.629357798,0.631192661,0.633027523,
0.634862385,0.636697248,0.63853211,0.640366972,0.642201835,0.644036697,
0.64587156,0.647706422,0.649541284,0.651376147,0.653211009,0.655045872,
0.656880734,0.658715596,0.660550459,0.662385321,0.664220183,0.666055046,
0.667889908,0.669724771,0.671559633,0.673394495,0.675229358,0.67706422,
0.678899083,0.680733945,0.682568807,0.68440367,0.686238532,0.688073394,
0.689908257,0.691743119,0.693577982,0.695412844,0.697247706,0.699082569,
0.700917431,0.702752294,0.704587156,0.706422018,0.708256881,0.710091743,
0.711926606,0.713761468,0.71559633,0.717431193,0.719266055,0.721100917,
0.72293578,0.724770642,0.726605505,0.728440367,0.730275229,0.732110092,
0.733944954,0.735779817,0.737614679,0.739449541,0.741284404,0.743119266,
0.744954128,0.746788991,0.748623853,0.750458716,0.752293578,0.75412844,
0.755963303,0.757798165,0.759633028,0.76146789,0.763302752,0.765137615,
0.766972477,0.768807339,0.770642202,0.772477064,0.774311927,0.776146789,
0.777981651,0.779816514,0.781651376,0.783486239,0.785321101,0.787155963,
0.788990826,0.790825688,0.79266055,0.794495413,0.796330275,0.798165138,
0.8,0.801834862,0.803669725,0.805504587,0.80733945,0.809174312,0.811009174,
0.812844037,0.814678899,0.816513761,0.818348624,0.820183486,0.822018349,
0.823853211,0.825688073,0.827522936,0.829357798,0.831192661,0.833027523,
0.834862385,0.836697248,0.83853211,0.840366972,0.842201835,0.844036697,
0.84587156,0.847706422,0.849541284,0.851376147,0.853211009,0.855045872,
0.856880734,0.858715596,0.860550459,0.862385321,0.864220183,0.866055046,
0.867889908,0.869724771,0.871559633,0.873394495,0.875229358,0.87706422,
0.878899083,0.880733945,0.882568807,0.88440367,0.886238532,0.888073394,
0.889908257,0.891743119,0.893577982,0.895412844,0.897247706,0.899082569,
0.900917431,0.902752294,0.904587156,0.906422018,0.908256881,0.910091743,
0.911926606,0.913761468,0.91559633,0.917431193,0.919266055,0.921100917,
0.92293578,0.924770642,0.926605505,0.928440367,0.930275229,0.932110092,
0.933944954,0.935779817,0.937614679,0.939449541,0.941284404,0.943119266,
0.944954128,0.946788991,0.948623853,0.950458716,0.952293578,0.95412844,
0.955963303,0.957798165,0.959633028,0.96146789,0.963302752,0.965137615,
0.966972477,0.968807339,0.970642202,0.972477064,0.974311927,0.976146789,
0.977981651,0.979816514,0.981651376,0.983486239,0.985321101,0.987155963,
0.988990826,0.990825688,0.99266055,0.994495413,0.996330275,0.998165138,
1.),(0.,0.36),.UNSPECIFIED.);
#6267=B_SPLINE_SURFACE_WITH_KNOTS('',5,1,((#239616,#239617),(#239618,#239619),
(#239620,#239621),(#239622,#239623),(#239624,#239625),(#239626,#239627),
(#239628,#239629),(#239630,#239631),(#239632,#239633),(#239634,#239635),
(#239636,#239637),(#239638,#239639),(#239640,#239641),(#239642,#239643),
(#239644,#239645),(#239646,#239647),(#239648,#239649),(#239650,#239651),
(#239652,#239653),(#239654,#239655),(#239656,#239657),(#239658,#239659),
(#239660,#239661),(#239662,#239663),(#239664,#239665),(#239666,#239667),
(#239668,#239669),(#239670,#239671),(#239672,#239673),(#239674,#239675),
(#239676,#239677),(#239678,#239679),(#239680,#239681),(#239682,#239683),
(#239684,#239685),(#239686,#239687),(#239688,#239689),(#239690,#239691),
(#239692,#239693),(#239694,#239695),(#239696,#239697),(#239698,#239699),
(#239700,#239701),(#239702,#239703),(#239704,#239705),(#239706,#239707),
(#239708,#239709),(#239710,#239711),(#239712,#239713),(#239714,#239715),
(#239716,#239717),(#239718,#239719),(#239720,#239721),(#239722,#239723),
(#239724,#239725),(#239726,#239727),(#239728,#239729),(#239730,#239731),
(#239732,#239733),(#239734,#239735),(#239736,#239737),(#239738,#239739),
(#239740,#239741),(#239742,#239743),(#239744,#239745),(#239746,#239747),
(#239748,#239749),(#239750,#239751),(#239752,#239753),(#239754,#239755),
(#239756,#239757),(#239758,#239759),(#239760,#239761),(#239762,#239763),
(#239764,#239765),(#239766,#239767),(#239768,#239769),(#239770,#239771),
(#239772,#239773),(#239774,#239775),(#239776,#239777),(#239778,#239779),
(#239780,#239781),(#239782,#239783),(#239784,#239785),(#239786,#239787),
(#239788,#239789),(#239790,#239791),(#239792,#239793),(#239794,#239795),
(#239796,#239797),(#239798,#239799),(#239800,#239801),(#239802,#239803),
(#239804,#239805),(#239806,#239807),(#239808,#239809),(#239810,#239811),
(#239812,#239813),(#239814,#239815),(#239816,#239817),(#239818,#239819),
(#239820,#239821),(#239822,#239823),(#239824,#239825),(#239826,#239827),
(#239828,#239829),(#239830,#239831),(#239832,#239833),(#239834,#239835),
(#239836,#239837),(#239838,#239839),(#239840,#239841),(#239842,#239843),
(#239844,#239845),(#239846,#239847),(#239848,#239849),(#239850,#239851),
(#239852,#239853),(#239854,#239855),(#239856,#239857),(#239858,#239859),
(#239860,#239861),(#239862,#239863),(#239864,#239865),(#239866,#239867),
(#239868,#239869),(#239870,#239871),(#239872,#239873),(#239874,#239875),
(#239876,#239877),(#239878,#239879),(#239880,#239881),(#239882,#239883),
(#239884,#239885),(#239886,#239887),(#239888,#239889),(#239890,#239891),
(#239892,#239893),(#239894,#239895),(#239896,#239897),(#239898,#239899),
(#239900,#239901),(#239902,#239903),(#239904,#239905),(#239906,#239907),
(#239908,#239909),(#239910,#239911),(#239912,#239913),(#239914,#239915),
(#239916,#239917),(#239918,#239919),(#239920,#239921),(#239922,#239923),
(#239924,#239925),(#239926,#239927),(#239928,#239929),(#239930,#239931),
(#239932,#239933),(#239934,#239935),(#239936,#239937),(#239938,#239939),
(#239940,#239941),(#239942,#239943),(#239944,#239945),(#239946,#239947),
(#239948,#239949),(#239950,#239951),(#239952,#239953),(#239954,#239955),
(#239956,#239957),(#239958,#239959),(#239960,#239961),(#239962,#239963),
(#239964,#239965),(#239966,#239967),(#239968,#239969),(#239970,#239971),
(#239972,#239973),(#239974,#239975),(#239976,#239977),(#239978,#239979),
(#239980,#239981),(#239982,#239983),(#239984,#239985),(#239986,#239987),
(#239988,#239989),(#239990,#239991),(#239992,#239993),(#239994,#239995),
(#239996,#239997),(#239998,#239999),(#240000,#240001),(#240002,#240003),
(#240004,#240005),(#240006,#240007),(#240008,#240009),(#240010,#240011),
(#240012,#240013),(#240014,#240015),(#240016,#240017),(#240018,#240019),
(#240020,#240021),(#240022,#240023),(#240024,#240025),(#240026,#240027),
(#240028,#240029),(#240030,#240031),(#240032,#240033),(#240034,#240035),
(#240036,#240037),(#240038,#240039),(#240040,#240041),(#240042,#240043),
(#240044,#240045),(#240046,#240047),(#240048,#240049),(#240050,#240051),
(#240052,#240053),(#240054,#240055),(#240056,#240057),(#240058,#240059),
(#240060,#240061),(#240062,#240063),(#240064,#240065),(#240066,#240067),
(#240068,#240069),(#240070,#240071),(#240072,#240073),(#240074,#240075),
(#240076,#240077),(#240078,#240079),(#240080,#240081),(#240082,#240083),
(#240084,#240085),(#240086,#240087),(#240088,#240089),(#240090,#240091),
(#240092,#240093),(#240094,#240095),(#240096,#240097),(#240098,#240099),
(#240100,#240101),(#240102,#240103),(#240104,#240105),(#240106,#240107),
(#240108,#240109),(#240110,#240111),(#240112,#240113),(#240114,#240115),
(#240116,#240117),(#240118,#240119),(#240120,#240121),(#240122,#240123),
(#240124,#240125),(#240126,#240127),(#240128,#240129),(#240130,#240131),
(#240132,#240133),(#240134,#240135),(#240136,#240137),(#240138,#240139),
(#240140,#240141),(#240142,#240143),(#240144,#240145),(#240146,#240147),
(#240148,#240149),(#240150,#240151),(#240152,#240153),(#240154,#240155),
(#240156,#240157),(#240158,#240159),(#240160,#240161),(#240162,#240163),
(#240164,#240165),(#240166,#240167),(#240168,#240169),(#240170,#240171),
(#240172,#240173),(#240174,#240175),(#240176,#240177),(#240178,#240179),
(#240180,#240181),(#240182,#240183),(#240184,#240185),(#240186,#240187),
(#240188,#240189),(#240190,#240191),(#240192,#240193),(#240194,#240195),
(#240196,#240197),(#240198,#240199),(#240200,#240201),(#240202,#240203),
(#240204,#240205),(#240206,#240207),(#240208,#240209),(#240210,#240211),
(#240212,#240213),(#240214,#240215),(#240216,#240217),(#240218,#240219),
(#240220,#240221),(#240222,#240223),(#240224,#240225),(#240226,#240227),
(#240228,#240229),(#240230,#240231),(#240232,#240233),(#240234,#240235),
(#240236,#240237),(#240238,#240239),(#240240,#240241),(#240242,#240243),
(#240244,#240245),(#240246,#240247),(#240248,#240249),(#240250,#240251),
(#240252,#240253),(#240254,#240255),(#240256,#240257),(#240258,#240259),
(#240260,#240261),(#240262,#240263),(#240264,#240265),(#240266,#240267),
(#240268,#240269),(#240270,#240271),(#240272,#240273),(#240274,#240275),
(#240276,#240277),(#240278,#240279),(#240280,#240281),(#240282,#240283),
(#240284,#240285),(#240286,#240287),(#240288,#240289),(#240290,#240291),
(#240292,#240293),(#240294,#240295),(#240296,#240297),(#240298,#240299),
(#240300,#240301),(#240302,#240303),(#240304,#240305),(#240306,#240307),
(#240308,#240309),(#240310,#240311),(#240312,#240313),(#240314,#240315),
(#240316,#240317),(#240318,#240319),(#240320,#240321),(#240322,#240323),
(#240324,#240325),(#240326,#240327),(#240328,#240329),(#240330,#240331),
(#240332,#240333),(#240334,#240335),(#240336,#240337),(#240338,#240339),
(#240340,#240341),(#240342,#240343),(#240344,#240345),(#240346,#240347),
(#240348,#240349),(#240350,#240351),(#240352,#240353),(#240354,#240355),
(#240356,#240357),(#240358,#240359),(#240360,#240361),(#240362,#240363),
(#240364,#240365),(#240366,#240367),(#240368,#240369),(#240370,#240371),
(#240372,#240373),(#240374,#240375),(#240376,#240377),(#240378,#240379),
(#240380,#240381),(#240382,#240383),(#240384,#240385),(#240386,#240387),
(#240388,#240389),(#240390,#240391),(#240392,#240393),(#240394,#240395),
(#240396,#240397),(#240398,#240399),(#240400,#240401),(#240402,#240403),
(#240404,#240405),(#240406,#240407),(#240408,#240409),(#240410,#240411),
(#240412,#240413),(#240414,#240415),(#240416,#240417),(#240418,#240419),
(#240420,#240421),(#240422,#240423),(#240424,#240425),(#240426,#240427),
(#240428,#240429),(#240430,#240431),(#240432,#240433),(#240434,#240435),
(#240436,#240437),(#240438,#240439),(#240440,#240441),(#240442,#240443),
(#240444,#240445),(#240446,#240447),(#240448,#240449),(#240450,#240451),
(#240452,#240453),(#240454,#240455),(#240456,#240457),(#240458,#240459),
(#240460,#240461),(#240462,#240463),(#240464,#240465),(#240466,#240467),
(#240468,#240469),(#240470,#240471),(#240472,#240473),(#240474,#240475),
(#240476,#240477),(#240478,#240479),(#240480,#240481),(#240482,#240483),
(#240484,#240485),(#240486,#240487),(#240488,#240489),(#240490,#240491),
(#240492,#240493),(#240494,#240495),(#240496,#240497),(#240498,#240499),
(#240500,#240501),(#240502,#240503),(#240504,#240505),(#240506,#240507),
(#240508,#240509),(#240510,#240511),(#240512,#240513),(#240514,#240515),
(#240516,#240517),(#240518,#240519),(#240520,#240521),(#240522,#240523),
(#240524,#240525),(#240526,#240527),(#240528,#240529),(#240530,#240531),
(#240532,#240533),(#240534,#240535),(#240536,#240537),(#240538,#240539),
(#240540,#240541),(#240542,#240543),(#240544,#240545),(#240546,#240547),
(#240548,#240549),(#240550,#240551),(#240552,#240553),(#240554,#240555),
(#240556,#240557),(#240558,#240559)),.UNSPECIFIED.,.F.,.F.,.F.,(6,1,1,1,
1,1,1,1,1,1,1,1,1,1,1,1,1,1,1,1,1,1,1,1,1,1,1,1,1,1,1,1,1,1,1,1,1,1,1,1,
1,1,1,1,1,1,1,1,1,1,1,1,1,1,1,1,1,1,1,1,1,1,1,1,1,1,1,1,1,1,1,1,1,1,1,1,
1,1,1,1,1,1,1,1,1,1,1,1,1,1,1,1,1,1,1,1,1,1,1,1,1,1,1,1,1,1,1,1,1,1,1,1,
1,1,1,1,1,1,1,1,1,1,1,1,1,1,1,1,1,1,1,1,1,1,1,1,1,1,1,1,1,1,1,1,1,1,1,1,
1,1,1,1,1,1,1,1,1,1,1,1,1,1,1,1,1,1,1,1,1,1,1,1,1,1,1,1,1,1,1,1,1,1,1,1,
1,1,1,1,1,1,1,1,1,1,1,1,1,1,1,1,1,1,1,1,1,1,1,1,1,1,1,1,1,1,1,1,1,1,1,1,
1,1,1,1,1,1,1,1,1,1,1,1,1,1,1,1,1,1,1,1,1,1,1,1,1,1,1,1,1,1,1,1,1,1,1,1,
1,1,1,1,1,1,1,1,1,1,1,1,1,1,1,1,1,1,1,1,1,1,1,1,1,1,1,1,1,1,1,1,1,1,1,1,
1,1,1,1,1,1,1,1,1,1,1,1,1,1,1,1,1,1,1,1,1,1,1,1,1,1,1,1,1,1,1,1,1,1,1,1,
1,1,1,1,1,1,1,1,1,1,1,1,1,1,1,1,1,1,1,1,1,1,1,1,1,1,1,1,1,1,1,1,1,1,1,1,
1,1,1,1,1,1,1,1,1,1,1,1,1,1,1,1,1,1,1,1,1,1,1,1,1,1,1,1,1,1,1,1,1,1,1,1,
1,1,1,1,1,1,1,1,1,1,1,1,1,1,1,1,1,1,1,1,1,1,1,1,1,1,1,1,1,1,1,1,1,1,1,1,
1,1,1,1,1,1,1,1,1,1,1,1,1,1,1,1,1,1,1,1,1,1,1,1,1,1,1,1,1,1,1,6),(2,2),
(0.143172103,0.144954128,0.146788991,0.148623853,0.150458716,0.152293578,
0.15412844,0.155963303,0.157798165,0.159633028,0.16146789,0.163302752,0.165137615,
0.166972477,0.168807339,0.170642202,0.172477064,0.174311927,0.176146789,
0.177981651,0.179816514,0.181651376,0.183486239,0.185321101,0.187155963,
0.188990826,0.190825688,0.19266055,0.194495413,0.196330275,0.198165138,
0.2,0.201834862,0.203669725,0.205504587,0.20733945,0.209174312,0.211009174,
0.212844037,0.214678899,0.216513761,0.218348624,0.220183486,0.222018349,
0.223853211,0.225688073,0.227522936,0.229357798,0.231192661,0.233027523,
0.234862385,0.236697248,0.23853211,0.240366972,0.242201835,0.244036697,
0.24587156,0.247706422,0.249541284,0.251376147,0.253211009,0.255045872,
0.256880734,0.258715596,0.260550459,0.262385321,0.264220183,0.266055046,
0.267889908,0.269724771,0.271559633,0.273394495,0.275229358,0.27706422,
0.278899083,0.280733945,0.282568807,0.28440367,0.286238532,0.288073394,
0.289908257,0.291743119,0.293577982,0.295412844,0.297247706,0.299082569,
0.300917431,0.302752294,0.304587156,0.306422018,0.308256881,0.310091743,
0.311926606,0.313761468,0.31559633,0.317431193,0.319266055,0.321100917,
0.32293578,0.324770642,0.326605505,0.328440367,0.330275229,0.332110092,
0.333944954,0.335779817,0.337614679,0.339449541,0.341284404,0.343119266,
0.344954128,0.346788991,0.348623853,0.350458716,0.352293578,0.35412844,
0.355963303,0.357798165,0.359633028,0.36146789,0.363302752,0.365137615,
0.366972477,0.368807339,0.370642202,0.372477064,0.374311927,0.376146789,
0.377981651,0.379816514,0.381651376,0.383486239,0.385321101,0.387155963,
0.388990826,0.390825688,0.39266055,0.394495413,0.396330275,0.398165138,
0.4,0.401834862,0.403669725,0.405504587,0.40733945,0.409174312,0.411009174,
0.412844037,0.414678899,0.416513761,0.418348624,0.420183486,0.422018349,
0.423853211,0.425688073,0.427522936,0.429357798,0.431192661,0.433027523,
0.434862385,0.436697248,0.43853211,0.440366972,0.442201835,0.444036697,
0.44587156,0.447706422,0.449541284,0.451376147,0.453211009,0.455045872,
0.456880734,0.458715596,0.460550459,0.462385321,0.464220183,0.466055046,
0.467889908,0.469724771,0.471559633,0.473394495,0.475229358,0.47706422,
0.478899083,0.480733945,0.482568807,0.48440367,0.486238532,0.488073394,
0.489908257,0.491743119,0.493577982,0.495412844,0.497247706,0.499082569,
0.500917431,0.502752294,0.504587156,0.506422018,0.508256881,0.510091743,
0.511926606,0.513761468,0.51559633,0.517431193,0.519266055,0.521100917,
0.52293578,0.524770642,0.526605505,0.528440367,0.530275229,0.532110092,
0.533944954,0.535779817,0.537614679,0.539449541,0.541284404,0.543119266,
0.544954128,0.546788991,0.548623853,0.550458716,0.552293578,0.55412844,
0.555963303,0.557798165,0.559633028,0.56146789,0.563302752,0.565137615,
0.566972477,0.568807339,0.570642202,0.572477064,0.574311927,0.576146789,
0.577981651,0.579816514,0.581651376,0.583486239,0.585321101,0.587155963,
0.588990826,0.590825688,0.59266055,0.594495413,0.596330275,0.598165138,
0.6,0.601834862,0.603669725,0.605504587,0.60733945,0.609174312,0.611009174,
0.612844037,0.614678899,0.616513761,0.618348624,0.620183486,0.622018349,
0.623853211,0.625688073,0.627522936,0.629357798,0.631192661,0.633027523,
0.634862385,0.636697248,0.63853211,0.640366972,0.642201835,0.644036697,
0.64587156,0.647706422,0.649541284,0.651376147,0.653211009,0.655045872,
0.656880734,0.658715596,0.660550459,0.662385321,0.664220183,0.666055046,
0.667889908,0.669724771,0.671559633,0.673394495,0.675229358,0.67706422,
0.678899083,0.680733945,0.682568807,0.68440367,0.686238532,0.688073394,
0.689908257,0.691743119,0.693577982,0.695412844,0.697247706,0.699082569,
0.700917431,0.702752294,0.704587156,0.706422018,0.708256881,0.710091743,
0.711926606,0.713761468,0.71559633,0.717431193,0.719266055,0.721100917,
0.72293578,0.724770642,0.726605505,0.728440367,0.730275229,0.732110092,
0.733944954,0.735779817,0.737614679,0.739449541,0.741284404,0.743119266,
0.744954128,0.746788991,0.748623853,0.750458716,0.752293578,0.75412844,
0.755963303,0.757798165,0.759633028,0.76146789,0.763302752,0.765137615,
0.766972477,0.768807339,0.770642202,0.772477064,0.774311927,0.776146789,
0.777981651,0.779816514,0.781651376,0.783486239,0.785321101,0.787155963,
0.788990826,0.790825688,0.79266055,0.794495413,0.796330275,0.798165138,
0.8,0.801834862,0.803669725,0.805504587,0.80733945,0.809174312,0.811009174,
0.812844037,0.814678899,0.816513761,0.818348624,0.820183486,0.822018349,
0.823853211,0.825688073,0.827522936,0.829357798,0.831192661,0.833027523,
0.834862385,0.836697248,0.83853211,0.840366972,0.842201835,0.844036697,
0.84587156,0.847706422,0.849541284,0.851376147,0.853211009,0.855045872,
0.856880734,0.858715596,0.860550459,0.862385321,0.864220183,0.866055046,
0.867889908,0.869724771,0.871559633,0.873394495,0.875229358,0.87706422,
0.878899083,0.880733945,0.882568807,0.88440367,0.886238532,0.888073394,
0.889908257,0.891743119,0.893577982,0.895412844,0.897247706,0.899082569,
0.900917431,0.902752294,0.904587156,0.906422018,0.908256881,0.910091743,
0.911926606,0.913761468,0.91559633,0.917431193,0.919266055,0.921100917,
0.92293578,0.924770642,0.926605505,0.928440367,0.930275229,0.932110092,
0.933944954,0.935779817,0.937614679,0.939449541,0.941284404,0.943119266,
0.944954128,0.946788991,0.948623853,0.950458716,0.952293578,0.95412844,
0.955963303,0.957798165,0.959633028,0.96146789,0.963302752,0.965137615,
0.966972477,0.968807339,0.970642202,0.972477064,0.974311927,0.976146789,
0.977981651,0.979816514,0.981651376,0.983486239,0.985321101,0.987155963,
0.988990826,0.990825688,0.99266055,0.994495413,0.996330275,0.998165138,
1.),(0.,0.36),.UNSPECIFIED.);
#6268=B_SPLINE_SURFACE_WITH_KNOTS('',5,1,((#241192,#241193),(#241194,#241195),
(#241196,#241197),(#241198,#241199),(#241200,#241201),(#241202,#241203),
(#241204,#241205),(#241206,#241207),(#241208,#241209),(#241210,#241211),
(#241212,#241213),(#241214,#241215),(#241216,#241217),(#241218,#241219),
(#241220,#241221),(#241222,#241223),(#241224,#241225),(#241226,#241227),
(#241228,#241229),(#241230,#241231),(#241232,#241233),(#241234,#241235),
(#241236,#241237),(#241238,#241239),(#241240,#241241),(#241242,#241243),
(#241244,#241245),(#241246,#241247),(#241248,#241249),(#241250,#241251),
(#241252,#241253),(#241254,#241255),(#241256,#241257),(#241258,#241259),
(#241260,#241261),(#241262,#241263),(#241264,#241265),(#241266,#241267),
(#241268,#241269),(#241270,#241271),(#241272,#241273),(#241274,#241275),
(#241276,#241277),(#241278,#241279),(#241280,#241281),(#241282,#241283),
(#241284,#241285),(#241286,#241287),(#241288,#241289),(#241290,#241291),
(#241292,#241293),(#241294,#241295),(#241296,#241297),(#241298,#241299),
(#241300,#241301),(#241302,#241303),(#241304,#241305),(#241306,#241307),
(#241308,#241309),(#241310,#241311),(#241312,#241313),(#241314,#241315),
(#241316,#241317),(#241318,#241319),(#241320,#241321),(#241322,#241323),
(#241324,#241325),(#241326,#241327),(#241328,#241329),(#241330,#241331),
(#241332,#241333),(#241334,#241335),(#241336,#241337),(#241338,#241339),
(#241340,#241341),(#241342,#241343),(#241344,#241345),(#241346,#241347),
(#241348,#241349),(#241350,#241351),(#241352,#241353),(#241354,#241355),
(#241356,#241357),(#241358,#241359),(#241360,#241361),(#241362,#241363),
(#241364,#241365),(#241366,#241367),(#241368,#241369),(#241370,#241371),
(#241372,#241373),(#241374,#241375),(#241376,#241377),(#241378,#241379),
(#241380,#241381),(#241382,#241383),(#241384,#241385),(#241386,#241387),
(#241388,#241389),(#241390,#241391),(#241392,#241393),(#241394,#241395),
(#241396,#241397),(#241398,#241399),(#241400,#241401),(#241402,#241403),
(#241404,#241405),(#241406,#241407),(#241408,#241409),(#241410,#241411),
(#241412,#241413),(#241414,#241415),(#241416,#241417),(#241418,#241419),
(#241420,#241421),(#241422,#241423),(#241424,#241425),(#241426,#241427),
(#241428,#241429),(#241430,#241431),(#241432,#241433),(#241434,#241435),
(#241436,#241437),(#241438,#241439),(#241440,#241441),(#241442,#241443),
(#241444,#241445),(#241446,#241447),(#241448,#241449),(#241450,#241451),
(#241452,#241453),(#241454,#241455),(#241456,#241457),(#241458,#241459),
(#241460,#241461),(#241462,#241463),(#241464,#241465),(#241466,#241467),
(#241468,#241469),(#241470,#241471),(#241472,#241473),(#241474,#241475),
(#241476,#241477),(#241478,#241479),(#241480,#241481),(#241482,#241483),
(#241484,#241485),(#241486,#241487),(#241488,#241489),(#241490,#241491),
(#241492,#241493),(#241494,#241495),(#241496,#241497),(#241498,#241499),
(#241500,#241501),(#241502,#241503),(#241504,#241505),(#241506,#241507),
(#241508,#241509),(#241510,#241511),(#241512,#241513),(#241514,#241515),
(#241516,#241517),(#241518,#241519),(#241520,#241521),(#241522,#241523),
(#241524,#241525),(#241526,#241527),(#241528,#241529),(#241530,#241531),
(#241532,#241533),(#241534,#241535),(#241536,#241537),(#241538,#241539),
(#241540,#241541),(#241542,#241543),(#241544,#241545),(#241546,#241547),
(#241548,#241549),(#241550,#241551),(#241552,#241553),(#241554,#241555),
(#241556,#241557),(#241558,#241559),(#241560,#241561),(#241562,#241563),
(#241564,#241565),(#241566,#241567),(#241568,#241569),(#241570,#241571),
(#241572,#241573),(#241574,#241575),(#241576,#241577),(#241578,#241579),
(#241580,#241581),(#241582,#241583),(#241584,#241585),(#241586,#241587),
(#241588,#241589),(#241590,#241591),(#241592,#241593),(#241594,#241595),
(#241596,#241597),(#241598,#241599),(#241600,#241601),(#241602,#241603),
(#241604,#241605),(#241606,#241607),(#241608,#241609),(#241610,#241611),
(#241612,#241613),(#241614,#241615),(#241616,#241617),(#241618,#241619),
(#241620,#241621),(#241622,#241623),(#241624,#241625),(#241626,#241627),
(#241628,#241629),(#241630,#241631),(#241632,#241633),(#241634,#241635),
(#241636,#241637),(#241638,#241639),(#241640,#241641),(#241642,#241643),
(#241644,#241645),(#241646,#241647),(#241648,#241649),(#241650,#241651),
(#241652,#241653),(#241654,#241655),(#241656,#241657),(#241658,#241659),
(#241660,#241661),(#241662,#241663),(#241664,#241665),(#241666,#241667),
(#241668,#241669),(#241670,#241671),(#241672,#241673),(#241674,#241675),
(#241676,#241677),(#241678,#241679),(#241680,#241681),(#241682,#241683),
(#241684,#241685),(#241686,#241687),(#241688,#241689),(#241690,#241691),
(#241692,#241693),(#241694,#241695),(#241696,#241697),(#241698,#241699),
(#241700,#241701),(#241702,#241703),(#241704,#241705),(#241706,#241707),
(#241708,#241709),(#241710,#241711),(#241712,#241713),(#241714,#241715),
(#241716,#241717),(#241718,#241719),(#241720,#241721),(#241722,#241723),
(#241724,#241725),(#241726,#241727),(#241728,#241729),(#241730,#241731),
(#241732,#241733),(#241734,#241735),(#241736,#241737),(#241738,#241739),
(#241740,#241741),(#241742,#241743),(#241744,#241745),(#241746,#241747),
(#241748,#241749),(#241750,#241751),(#241752,#241753),(#241754,#241755),
(#241756,#241757),(#241758,#241759),(#241760,#241761),(#241762,#241763),
(#241764,#241765),(#241766,#241767),(#241768,#241769),(#241770,#241771),
(#241772,#241773),(#241774,#241775),(#241776,#241777),(#241778,#241779),
(#241780,#241781),(#241782,#241783),(#241784,#241785),(#241786,#241787),
(#241788,#241789),(#241790,#241791),(#241792,#241793),(#241794,#241795),
(#241796,#241797),(#241798,#241799),(#241800,#241801),(#241802,#241803),
(#241804,#241805),(#241806,#241807),(#241808,#241809),(#241810,#241811),
(#241812,#241813),(#241814,#241815),(#241816,#241817),(#241818,#241819),
(#241820,#241821),(#241822,#241823),(#241824,#241825),(#241826,#241827),
(#241828,#241829),(#241830,#241831),(#241832,#241833),(#241834,#241835),
(#241836,#241837),(#241838,#241839),(#241840,#241841),(#241842,#241843),
(#241844,#241845),(#241846,#241847),(#241848,#241849),(#241850,#241851),
(#241852,#241853),(#241854,#241855),(#241856,#241857),(#241858,#241859),
(#241860,#241861),(#241862,#241863),(#241864,#241865),(#241866,#241867),
(#241868,#241869),(#241870,#241871),(#241872,#241873),(#241874,#241875),
(#241876,#241877),(#241878,#241879),(#241880,#241881),(#241882,#241883),
(#241884,#241885),(#241886,#241887),(#241888,#241889),(#241890,#241891),
(#241892,#241893),(#241894,#241895),(#241896,#241897),(#241898,#241899),
(#241900,#241901),(#241902,#241903),(#241904,#241905),(#241906,#241907),
(#241908,#241909),(#241910,#241911),(#241912,#241913),(#241914,#241915),
(#241916,#241917),(#241918,#241919),(#241920,#241921),(#241922,#241923),
(#241924,#241925),(#241926,#241927),(#241928,#241929),(#241930,#241931),
(#241932,#241933),(#241934,#241935),(#241936,#241937),(#241938,#241939),
(#241940,#241941),(#241942,#241943),(#241944,#241945),(#241946,#241947),
(#241948,#241949),(#241950,#241951),(#241952,#241953),(#241954,#241955),
(#241956,#241957),(#241958,#241959),(#241960,#241961),(#241962,#241963),
(#241964,#241965),(#241966,#241967),(#241968,#241969),(#241970,#241971),
(#241972,#241973),(#241974,#241975),(#241976,#241977),(#241978,#241979),
(#241980,#241981),(#241982,#241983),(#241984,#241985),(#241986,#241987),
(#241988,#241989),(#241990,#241991),(#241992,#241993),(#241994,#241995),
(#241996,#241997),(#241998,#241999),(#242000,#242001),(#242002,#242003),
(#242004,#242005),(#242006,#242007),(#242008,#242009),(#242010,#242011),
(#242012,#242013),(#242014,#242015),(#242016,#242017),(#242018,#242019),
(#242020,#242021),(#242022,#242023),(#242024,#242025),(#242026,#242027),
(#242028,#242029),(#242030,#242031),(#242032,#242033),(#242034,#242035),
(#242036,#242037),(#242038,#242039),(#242040,#242041),(#242042,#242043),
(#242044,#242045),(#242046,#242047),(#242048,#242049),(#242050,#242051),
(#242052,#242053),(#242054,#242055),(#242056,#242057),(#242058,#242059),
(#242060,#242061),(#242062,#242063),(#242064,#242065),(#242066,#242067),
(#242068,#242069),(#242070,#242071),(#242072,#242073),(#242074,#242075),
(#242076,#242077),(#242078,#242079),(#242080,#242081),(#242082,#242083),
(#242084,#242085),(#242086,#242087),(#242088,#242089),(#242090,#242091),
(#242092,#242093),(#242094,#242095),(#242096,#242097),(#242098,#242099),
(#242100,#242101),(#242102,#242103),(#242104,#242105),(#242106,#242107),
(#242108,#242109),(#242110,#242111),(#242112,#242113),(#242114,#242115),
(#242116,#242117),(#242118,#242119),(#242120,#242121),(#242122,#242123),
(#242124,#242125),(#242126,#242127),(#242128,#242129),(#242130,#242131),
(#242132,#242133),(#242134,#242135)),.UNSPECIFIED.,.F.,.F.,.F.,(6,1,1,1,
1,1,1,1,1,1,1,1,1,1,1,1,1,1,1,1,1,1,1,1,1,1,1,1,1,1,1,1,1,1,1,1,1,1,1,1,
1,1,1,1,1,1,1,1,1,1,1,1,1,1,1,1,1,1,1,1,1,1,1,1,1,1,1,1,1,1,1,1,1,1,1,1,
1,1,1,1,1,1,1,1,1,1,1,1,1,1,1,1,1,1,1,1,1,1,1,1,1,1,1,1,1,1,1,1,1,1,1,1,
1,1,1,1,1,1,1,1,1,1,1,1,1,1,1,1,1,1,1,1,1,1,1,1,1,1,1,1,1,1,1,1,1,1,1,1,
1,1,1,1,1,1,1,1,1,1,1,1,1,1,1,1,1,1,1,1,1,1,1,1,1,1,1,1,1,1,1,1,1,1,1,1,
1,1,1,1,1,1,1,1,1,1,1,1,1,1,1,1,1,1,1,1,1,1,1,1,1,1,1,1,1,1,1,1,1,1,1,1,
1,1,1,1,1,1,1,1,1,1,1,1,1,1,1,1,1,1,1,1,1,1,1,1,1,1,1,1,1,1,1,1,1,1,1,1,
1,1,1,1,1,1,1,1,1,1,1,1,1,1,1,1,1,1,1,1,1,1,1,1,1,1,1,1,1,1,1,1,1,1,1,1,
1,1,1,1,1,1,1,1,1,1,1,1,1,1,1,1,1,1,1,1,1,1,1,1,1,1,1,1,1,1,1,1,1,1,1,1,
1,1,1,1,1,1,1,1,1,1,1,1,1,1,1,1,1,1,1,1,1,1,1,1,1,1,1,1,1,1,1,1,1,1,1,1,
1,1,1,1,1,1,1,1,1,1,1,1,1,1,1,1,1,1,1,1,1,1,1,1,1,1,1,1,1,1,1,1,1,1,1,1,
1,1,1,1,1,1,1,1,1,1,1,1,1,1,1,1,1,1,1,1,1,1,1,1,1,1,1,1,1,1,1,1,1,1,1,1,
1,1,1,1,1,1,1,1,1,1,1,1,1,1,1,1,1,1,1,1,1,1,1,1,1,1,1,1,1,1,1,6),(2,2),
(-1.,-0.998165138,-0.996330275,-0.994495413,-0.99266055,-0.990825688,-0.988990826,
-0.987155963,-0.985321101,-0.983486239,-0.981651376,-0.979816514,-0.977981651,
-0.976146789,-0.974311927,-0.972477064,-0.970642202,-0.968807339,-0.966972477,
-0.965137615,-0.963302752,-0.96146789,-0.959633028,-0.957798165,-0.955963303,
-0.95412844,-0.952293578,-0.950458716,-0.948623853,-0.946788991,-0.944954128,
-0.943119266,-0.941284404,-0.939449541,-0.937614679,-0.935779817,-0.933944954,
-0.932110092,-0.930275229,-0.928440367,-0.926605505,-0.924770642,-0.92293578,
-0.921100917,-0.919266055,-0.917431193,-0.91559633,-0.913761468,-0.911926606,
-0.910091743,-0.908256881,-0.906422018,-0.904587156,-0.902752294,-0.900917431,
-0.899082569,-0.897247706,-0.895412844,-0.893577982,-0.891743119,-0.889908257,
-0.888073394,-0.886238532,-0.88440367,-0.882568807,-0.880733945,-0.878899083,
-0.87706422,-0.875229358,-0.873394495,-0.871559633,-0.869724771,-0.867889908,
-0.866055046,-0.864220183,-0.862385321,-0.860550459,-0.858715596,-0.856880734,
-0.855045872,-0.853211009,-0.851376147,-0.849541284,-0.847706422,-0.84587156,
-0.844036697,-0.842201835,-0.840366972,-0.83853211,-0.836697248,-0.834862385,
-0.833027523,-0.831192661,-0.829357798,-0.827522936,-0.825688073,-0.823853211,
-0.822018349,-0.820183486,-0.818348624,-0.816513761,-0.814678899,-0.812844037,
-0.811009174,-0.809174312,-0.80733945,-0.805504587,-0.803669725,-0.801834862,
-0.8,-0.798165138,-0.796330275,-0.794495413,-0.79266055,-0.790825688,-0.788990826,
-0.787155963,-0.785321101,-0.783486239,-0.781651376,-0.779816514,-0.777981651,
-0.776146789,-0.774311927,-0.772477064,-0.770642202,-0.768807339,-0.766972477,
-0.765137615,-0.763302752,-0.76146789,-0.759633028,-0.757798165,-0.755963303,
-0.75412844,-0.752293578,-0.750458716,-0.748623853,-0.746788991,-0.744954128,
-0.743119266,-0.741284404,-0.739449541,-0.737614679,-0.735779817,-0.733944954,
-0.732110092,-0.730275229,-0.728440367,-0.726605505,-0.724770642,-0.72293578,
-0.721100917,-0.719266055,-0.717431193,-0.71559633,-0.713761468,-0.711926606,
-0.710091743,-0.708256881,-0.706422018,-0.704587156,-0.702752294,-0.700917431,
-0.699082569,-0.697247706,-0.695412844,-0.693577982,-0.691743119,-0.689908257,
-0.688073394,-0.686238532,-0.68440367,-0.682568807,-0.680733945,-0.678899083,
-0.67706422,-0.675229358,-0.673394495,-0.671559633,-0.669724771,-0.667889908,
-0.666055046,-0.664220183,-0.662385321,-0.660550459,-0.658715596,-0.656880734,
-0.655045872,-0.653211009,-0.651376147,-0.649541284,-0.647706422,-0.64587156,
-0.644036697,-0.642201835,-0.640366972,-0.63853211,-0.636697248,-0.634862385,
-0.633027523,-0.631192661,-0.629357798,-0.627522936,-0.625688073,-0.623853211,
-0.622018349,-0.620183486,-0.618348624,-0.616513761,-0.614678899,-0.612844037,
-0.611009174,-0.609174312,-0.60733945,-0.605504587,-0.603669725,-0.601834862,
-0.6,-0.598165138,-0.596330275,-0.594495413,-0.59266055,-0.590825688,-0.588990826,
-0.587155963,-0.585321101,-0.583486239,-0.581651376,-0.579816514,-0.577981651,
-0.576146789,-0.574311927,-0.572477064,-0.570642202,-0.568807339,-0.566972477,
-0.565137615,-0.563302752,-0.56146789,-0.559633028,-0.557798165,-0.555963303,
-0.55412844,-0.552293578,-0.550458716,-0.548623853,-0.546788991,-0.544954128,
-0.543119266,-0.541284404,-0.539449541,-0.537614679,-0.535779817,-0.533944954,
-0.532110092,-0.530275229,-0.528440367,-0.526605505,-0.524770642,-0.52293578,
-0.521100917,-0.519266055,-0.517431193,-0.51559633,-0.513761468,-0.511926606,
-0.510091743,-0.508256881,-0.506422018,-0.504587156,-0.502752294,-0.500917431,
-0.499082569,-0.497247706,-0.495412844,-0.493577982,-0.491743119,-0.489908257,
-0.488073394,-0.486238532,-0.48440367,-0.482568807,-0.480733945,-0.478899083,
-0.47706422,-0.475229358,-0.473394495,-0.471559633,-0.469724771,-0.467889908,
-0.466055046,-0.464220183,-0.462385321,-0.460550459,-0.458715596,-0.456880734,
-0.455045872,-0.453211009,-0.451376147,-0.449541284,-0.447706422,-0.44587156,
-0.444036697,-0.442201835,-0.440366972,-0.43853211,-0.436697248,-0.434862385,
-0.433027523,-0.431192661,-0.429357798,-0.427522936,-0.425688073,-0.423853211,
-0.422018349,-0.420183486,-0.418348624,-0.416513761,-0.414678899,-0.412844037,
-0.411009174,-0.409174312,-0.40733945,-0.405504587,-0.403669725,-0.401834862,
-0.4,-0.398165138,-0.396330275,-0.394495413,-0.39266055,-0.390825688,-0.388990826,
-0.387155963,-0.385321101,-0.383486239,-0.381651376,-0.379816514,-0.377981651,
-0.376146789,-0.374311927,-0.372477064,-0.370642202,-0.368807339,-0.366972477,
-0.365137615,-0.363302752,-0.36146789,-0.359633028,-0.357798165,-0.355963303,
-0.35412844,-0.352293578,-0.350458716,-0.348623853,-0.346788991,-0.344954128,
-0.343119266,-0.341284404,-0.339449541,-0.337614679,-0.335779817,-0.333944954,
-0.332110092,-0.330275229,-0.328440367,-0.326605505,-0.324770642,-0.32293578,
-0.321100917,-0.319266055,-0.317431193,-0.31559633,-0.313761468,-0.311926606,
-0.310091743,-0.308256881,-0.306422018,-0.304587156,-0.302752294,-0.300917431,
-0.299082569,-0.297247706,-0.295412844,-0.293577982,-0.291743119,-0.289908257,
-0.288073394,-0.286238532,-0.28440367,-0.282568807,-0.280733945,-0.278899083,
-0.27706422,-0.275229358,-0.273394495,-0.271559633,-0.269724771,-0.267889908,
-0.266055046,-0.264220183,-0.262385321,-0.260550459,-0.258715596,-0.256880734,
-0.255045872,-0.253211009,-0.251376147,-0.249541284,-0.247706422,-0.24587156,
-0.244036697,-0.242201835,-0.240366972,-0.23853211,-0.236697248,-0.234862385,
-0.233027523,-0.231192661,-0.229357798,-0.227522936,-0.225688073,-0.223853211,
-0.222018349,-0.220183486,-0.218348624,-0.216513761,-0.214678899,-0.212844037,
-0.211009174,-0.209174312,-0.20733945,-0.205504587,-0.203669725,-0.201834862,
-0.2,-0.198165138,-0.196330275,-0.194495413,-0.19266055,-0.190825688,-0.188990826,
-0.187155963,-0.185321101,-0.183486239,-0.181651376,-0.179816514,-0.177981651,
-0.176146789,-0.174311927,-0.172477064,-0.170642202,-0.168807339,-0.166972477,
-0.165137615,-0.163302752,-0.16146789,-0.159633028,-0.157798165,-0.155963303,
-0.15412844,-0.152293578,-0.150458716,-0.148623853,-0.146788991,-0.144954128,
-0.143172103),(0.,0.36),.UNSPECIFIED.);
#6269=B_SPLINE_SURFACE_WITH_KNOTS('',5,1,((#242783,#242784),(#242785,#242786),
(#242787,#242788),(#242789,#242790),(#242791,#242792),(#242793,#242794),
(#242795,#242796),(#242797,#242798),(#242799,#242800),(#242801,#242802),
(#242803,#242804),(#242805,#242806),(#242807,#242808),(#242809,#242810),
(#242811,#242812),(#242813,#242814),(#242815,#242816),(#242817,#242818),
(#242819,#242820),(#242821,#242822),(#242823,#242824),(#242825,#242826),
(#242827,#242828),(#242829,#242830),(#242831,#242832),(#242833,#242834),
(#242835,#242836),(#242837,#242838),(#242839,#242840),(#242841,#242842),
(#242843,#242844),(#242845,#242846),(#242847,#242848),(#242849,#242850),
(#242851,#242852),(#242853,#242854),(#242855,#242856),(#242857,#242858),
(#242859,#242860),(#242861,#242862),(#242863,#242864),(#242865,#242866),
(#242867,#242868),(#242869,#242870),(#242871,#242872),(#242873,#242874),
(#242875,#242876),(#242877,#242878),(#242879,#242880),(#242881,#242882),
(#242883,#242884),(#242885,#242886),(#242887,#242888),(#242889,#242890),
(#242891,#242892),(#242893,#242894),(#242895,#242896),(#242897,#242898),
(#242899,#242900),(#242901,#242902),(#242903,#242904),(#242905,#242906),
(#242907,#242908),(#242909,#242910),(#242911,#242912),(#242913,#242914),
(#242915,#242916),(#242917,#242918),(#242919,#242920),(#242921,#242922),
(#242923,#242924),(#242925,#242926),(#242927,#242928),(#242929,#242930),
(#242931,#242932),(#242933,#242934),(#242935,#242936),(#242937,#242938),
(#242939,#242940),(#242941,#242942),(#242943,#242944),(#242945,#242946),
(#242947,#242948),(#242949,#242950),(#242951,#242952),(#242953,#242954),
(#242955,#242956),(#242957,#242958),(#242959,#242960),(#242961,#242962),
(#242963,#242964),(#242965,#242966),(#242967,#242968),(#242969,#242970),
(#242971,#242972),(#242973,#242974),(#242975,#242976),(#242977,#242978),
(#242979,#242980),(#242981,#242982),(#242983,#242984),(#242985,#242986),
(#242987,#242988),(#242989,#242990),(#242991,#242992),(#242993,#242994),
(#242995,#242996),(#242997,#242998),(#242999,#243000),(#243001,#243002),
(#243003,#243004),(#243005,#243006),(#243007,#243008),(#243009,#243010),
(#243011,#243012),(#243013,#243014),(#243015,#243016),(#243017,#243018),
(#243019,#243020),(#243021,#243022),(#243023,#243024),(#243025,#243026),
(#243027,#243028),(#243029,#243030),(#243031,#243032),(#243033,#243034),
(#243035,#243036),(#243037,#243038),(#243039,#243040),(#243041,#243042),
(#243043,#243044),(#243045,#243046),(#243047,#243048),(#243049,#243050),
(#243051,#243052),(#243053,#243054),(#243055,#243056),(#243057,#243058),
(#243059,#243060),(#243061,#243062),(#243063,#243064),(#243065,#243066),
(#243067,#243068),(#243069,#243070),(#243071,#243072),(#243073,#243074),
(#243075,#243076),(#243077,#243078),(#243079,#243080),(#243081,#243082),
(#243083,#243084),(#243085,#243086),(#243087,#243088),(#243089,#243090),
(#243091,#243092),(#243093,#243094),(#243095,#243096),(#243097,#243098),
(#243099,#243100),(#243101,#243102),(#243103,#243104),(#243105,#243106),
(#243107,#243108),(#243109,#243110),(#243111,#243112),(#243113,#243114),
(#243115,#243116),(#243117,#243118),(#243119,#243120),(#243121,#243122),
(#243123,#243124),(#243125,#243126),(#243127,#243128),(#243129,#243130),
(#243131,#243132),(#243133,#243134),(#243135,#243136),(#243137,#243138),
(#243139,#243140),(#243141,#243142),(#243143,#243144),(#243145,#243146),
(#243147,#243148),(#243149,#243150),(#243151,#243152),(#243153,#243154),
(#243155,#243156),(#243157,#243158),(#243159,#243160),(#243161,#243162),
(#243163,#243164),(#243165,#243166),(#243167,#243168),(#243169,#243170),
(#243171,#243172),(#243173,#243174),(#243175,#243176),(#243177,#243178),
(#243179,#243180),(#243181,#243182),(#243183,#243184),(#243185,#243186),
(#243187,#243188),(#243189,#243190),(#243191,#243192),(#243193,#243194),
(#243195,#243196),(#243197,#243198),(#243199,#243200),(#243201,#243202),
(#243203,#243204),(#243205,#243206),(#243207,#243208),(#243209,#243210),
(#243211,#243212),(#243213,#243214),(#243215,#243216),(#243217,#243218),
(#243219,#243220),(#243221,#243222),(#243223,#243224),(#243225,#243226),
(#243227,#243228),(#243229,#243230),(#243231,#243232),(#243233,#243234),
(#243235,#243236),(#243237,#243238),(#243239,#243240),(#243241,#243242),
(#243243,#243244),(#243245,#243246),(#243247,#243248),(#243249,#243250),
(#243251,#243252),(#243253,#243254),(#243255,#243256),(#243257,#243258),
(#243259,#243260),(#243261,#243262),(#243263,#243264),(#243265,#243266),
(#243267,#243268),(#243269,#243270),(#243271,#243272),(#243273,#243274),
(#243275,#243276),(#243277,#243278),(#243279,#243280),(#243281,#243282),
(#243283,#243284),(#243285,#243286),(#243287,#243288),(#243289,#243290),
(#243291,#243292),(#243293,#243294),(#243295,#243296),(#243297,#243298),
(#243299,#243300),(#243301,#243302),(#243303,#243304),(#243305,#243306),
(#243307,#243308),(#243309,#243310),(#243311,#243312),(#243313,#243314),
(#243315,#243316),(#243317,#243318),(#243319,#243320),(#243321,#243322),
(#243323,#243324),(#243325,#243326),(#243327,#243328),(#243329,#243330),
(#243331,#243332),(#243333,#243334),(#243335,#243336),(#243337,#243338),
(#243339,#243340),(#243341,#243342),(#243343,#243344),(#243345,#243346),
(#243347,#243348),(#243349,#243350),(#243351,#243352),(#243353,#243354),
(#243355,#243356),(#243357,#243358),(#243359,#243360),(#243361,#243362),
(#243363,#243364),(#243365,#243366),(#243367,#243368),(#243369,#243370),
(#243371,#243372),(#243373,#243374),(#243375,#243376),(#243377,#243378),
(#243379,#243380),(#243381,#243382),(#243383,#243384),(#243385,#243386),
(#243387,#243388),(#243389,#243390),(#243391,#243392),(#243393,#243394),
(#243395,#243396),(#243397,#243398),(#243399,#243400),(#243401,#243402),
(#243403,#243404),(#243405,#243406),(#243407,#243408),(#243409,#243410),
(#243411,#243412),(#243413,#243414),(#243415,#243416),(#243417,#243418),
(#243419,#243420),(#243421,#243422),(#243423,#243424),(#243425,#243426),
(#243427,#243428),(#243429,#243430),(#243431,#243432),(#243433,#243434),
(#243435,#243436),(#243437,#243438),(#243439,#243440),(#243441,#243442),
(#243443,#243444),(#243445,#243446),(#243447,#243448),(#243449,#243450),
(#243451,#243452),(#243453,#243454),(#243455,#243456),(#243457,#243458),
(#243459,#243460),(#243461,#243462),(#243463,#243464),(#243465,#243466),
(#243467,#243468),(#243469,#243470),(#243471,#243472),(#243473,#243474),
(#243475,#243476),(#243477,#243478),(#243479,#243480),(#243481,#243482),
(#243483,#243484),(#243485,#243486),(#243487,#243488),(#243489,#243490),
(#243491,#243492),(#243493,#243494),(#243495,#243496),(#243497,#243498),
(#243499,#243500),(#243501,#243502),(#243503,#243504),(#243505,#243506),
(#243507,#243508),(#243509,#243510),(#243511,#243512),(#243513,#243514),
(#243515,#243516),(#243517,#243518),(#243519,#243520),(#243521,#243522),
(#243523,#243524),(#243525,#243526),(#243527,#243528),(#243529,#243530),
(#243531,#243532),(#243533,#243534),(#243535,#243536),(#243537,#243538),
(#243539,#243540),(#243541,#243542),(#243543,#243544),(#243545,#243546),
(#243547,#243548),(#243549,#243550),(#243551,#243552),(#243553,#243554),
(#243555,#243556),(#243557,#243558),(#243559,#243560),(#243561,#243562),
(#243563,#243564),(#243565,#243566),(#243567,#243568),(#243569,#243570),
(#243571,#243572),(#243573,#243574),(#243575,#243576),(#243577,#243578),
(#243579,#243580),(#243581,#243582),(#243583,#243584),(#243585,#243586),
(#243587,#243588),(#243589,#243590),(#243591,#243592),(#243593,#243594),
(#243595,#243596),(#243597,#243598),(#243599,#243600),(#243601,#243602),
(#243603,#243604),(#243605,#243606),(#243607,#243608),(#243609,#243610),
(#243611,#243612),(#243613,#243614),(#243615,#243616),(#243617,#243618),
(#243619,#243620),(#243621,#243622),(#243623,#243624),(#243625,#243626),
(#243627,#243628),(#243629,#243630),(#243631,#243632),(#243633,#243634),
(#243635,#243636),(#243637,#243638),(#243639,#243640),(#243641,#243642),
(#243643,#243644),(#243645,#243646),(#243647,#243648),(#243649,#243650),
(#243651,#243652),(#243653,#243654),(#243655,#243656),(#243657,#243658),
(#243659,#243660),(#243661,#243662),(#243663,#243664),(#243665,#243666),
(#243667,#243668),(#243669,#243670),(#243671,#243672),(#243673,#243674),
(#243675,#243676),(#243677,#243678),(#243679,#243680),(#243681,#243682),
(#243683,#243684),(#243685,#243686),(#243687,#243688),(#243689,#243690),
(#243691,#243692),(#243693,#243694),(#243695,#243696),(#243697,#243698),
(#243699,#243700),(#243701,#243702),(#243703,#243704),(#243705,#243706),
(#243707,#243708),(#243709,#243710),(#243711,#243712),(#243713,#243714),
(#243715,#243716),(#243717,#243718),(#243719,#243720),(#243721,#243722),
(#243723,#243724),(#243725,#243726)),.UNSPECIFIED.,.F.,.F.,.F.,(6,1,1,1,
1,1,1,1,1,1,1,1,1,1,1,1,1,1,1,1,1,1,1,1,1,1,1,1,1,1,1,1,1,1,1,1,1,1,1,1,
1,1,1,1,1,1,1,1,1,1,1,1,1,1,1,1,1,1,1,1,1,1,1,1,1,1,1,1,1,1,1,1,1,1,1,1,
1,1,1,1,1,1,1,1,1,1,1,1,1,1,1,1,1,1,1,1,1,1,1,1,1,1,1,1,1,1,1,1,1,1,1,1,
1,1,1,1,1,1,1,1,1,1,1,1,1,1,1,1,1,1,1,1,1,1,1,1,1,1,1,1,1,1,1,1,1,1,1,1,
1,1,1,1,1,1,1,1,1,1,1,1,1,1,1,1,1,1,1,1,1,1,1,1,1,1,1,1,1,1,1,1,1,1,1,1,
1,1,1,1,1,1,1,1,1,1,1,1,1,1,1,1,1,1,1,1,1,1,1,1,1,1,1,1,1,1,1,1,1,1,1,1,
1,1,1,1,1,1,1,1,1,1,1,1,1,1,1,1,1,1,1,1,1,1,1,1,1,1,1,1,1,1,1,1,1,1,1,1,
1,1,1,1,1,1,1,1,1,1,1,1,1,1,1,1,1,1,1,1,1,1,1,1,1,1,1,1,1,1,1,1,1,1,1,1,
1,1,1,1,1,1,1,1,1,1,1,1,1,1,1,1,1,1,1,1,1,1,1,1,1,1,1,1,1,1,1,1,1,1,1,1,
1,1,1,1,1,1,1,1,1,1,1,1,1,1,1,1,1,1,1,1,1,1,1,1,1,1,1,1,1,1,1,1,1,1,1,1,
1,1,1,1,1,1,1,1,1,1,1,1,1,1,1,1,1,1,1,1,1,1,1,1,1,1,1,1,1,1,1,1,1,1,1,1,
1,1,1,1,1,1,1,1,1,1,1,1,1,1,1,1,1,1,1,1,1,1,1,1,1,1,1,1,1,1,1,1,1,1,1,1,
1,1,1,1,1,1,1,1,1,1,1,1,1,1,1,1,1,1,1,1,1,1,1,1,1,1,1,1,1,1,1,6),(2,2),
(-1.,-0.998165138,-0.996330275,-0.994495413,-0.99266055,-0.990825688,-0.988990826,
-0.987155963,-0.985321101,-0.983486239,-0.981651376,-0.979816514,-0.977981651,
-0.976146789,-0.974311927,-0.972477064,-0.970642202,-0.968807339,-0.966972477,
-0.965137615,-0.963302752,-0.96146789,-0.959633028,-0.957798165,-0.955963303,
-0.95412844,-0.952293578,-0.950458716,-0.948623853,-0.946788991,-0.944954128,
-0.943119266,-0.941284404,-0.939449541,-0.937614679,-0.935779817,-0.933944954,
-0.932110092,-0.930275229,-0.928440367,-0.926605505,-0.924770642,-0.92293578,
-0.921100917,-0.919266055,-0.917431193,-0.91559633,-0.913761468,-0.911926606,
-0.910091743,-0.908256881,-0.906422018,-0.904587156,-0.902752294,-0.900917431,
-0.899082569,-0.897247706,-0.895412844,-0.893577982,-0.891743119,-0.889908257,
-0.888073394,-0.886238532,-0.88440367,-0.882568807,-0.880733945,-0.878899083,
-0.87706422,-0.875229358,-0.873394495,-0.871559633,-0.869724771,-0.867889908,
-0.866055046,-0.864220183,-0.862385321,-0.860550459,-0.858715596,-0.856880734,
-0.855045872,-0.853211009,-0.851376147,-0.849541284,-0.847706422,-0.84587156,
-0.844036697,-0.842201835,-0.840366972,-0.83853211,-0.836697248,-0.834862385,
-0.833027523,-0.831192661,-0.829357798,-0.827522936,-0.825688073,-0.823853211,
-0.822018349,-0.820183486,-0.818348624,-0.816513761,-0.814678899,-0.812844037,
-0.811009174,-0.809174312,-0.80733945,-0.805504587,-0.803669725,-0.801834862,
-0.8,-0.798165138,-0.796330275,-0.794495413,-0.79266055,-0.790825688,-0.788990826,
-0.787155963,-0.785321101,-0.783486239,-0.781651376,-0.779816514,-0.777981651,
-0.776146789,-0.774311927,-0.772477064,-0.770642202,-0.768807339,-0.766972477,
-0.765137615,-0.763302752,-0.76146789,-0.759633028,-0.757798165,-0.755963303,
-0.75412844,-0.752293578,-0.750458716,-0.748623853,-0.746788991,-0.744954128,
-0.743119266,-0.741284404,-0.739449541,-0.737614679,-0.735779817,-0.733944954,
-0.732110092,-0.730275229,-0.728440367,-0.726605505,-0.724770642,-0.72293578,
-0.721100917,-0.719266055,-0.717431193,-0.71559633,-0.713761468,-0.711926606,
-0.710091743,-0.708256881,-0.706422018,-0.704587156,-0.702752294,-0.700917431,
-0.699082569,-0.697247706,-0.695412844,-0.693577982,-0.691743119,-0.689908257,
-0.688073394,-0.686238532,-0.68440367,-0.682568807,-0.680733945,-0.678899083,
-0.67706422,-0.675229358,-0.673394495,-0.671559633,-0.669724771,-0.667889908,
-0.666055046,-0.664220183,-0.662385321,-0.660550459,-0.658715596,-0.656880734,
-0.655045872,-0.653211009,-0.651376147,-0.649541284,-0.647706422,-0.64587156,
-0.644036697,-0.642201835,-0.640366972,-0.63853211,-0.636697248,-0.634862385,
-0.633027523,-0.631192661,-0.629357798,-0.627522936,-0.625688073,-0.623853211,
-0.622018349,-0.620183486,-0.618348624,-0.616513761,-0.614678899,-0.612844037,
-0.611009174,-0.609174312,-0.60733945,-0.605504587,-0.603669725,-0.601834862,
-0.6,-0.598165138,-0.596330275,-0.594495413,-0.59266055,-0.590825688,-0.588990826,
-0.587155963,-0.585321101,-0.583486239,-0.581651376,-0.579816514,-0.577981651,
-0.576146789,-0.574311927,-0.572477064,-0.570642202,-0.568807339,-0.566972477,
-0.565137615,-0.563302752,-0.56146789,-0.559633028,-0.557798165,-0.555963303,
-0.55412844,-0.552293578,-0.550458716,-0.548623853,-0.546788991,-0.544954128,
-0.543119266,-0.541284404,-0.539449541,-0.537614679,-0.535779817,-0.533944954,
-0.532110092,-0.530275229,-0.528440367,-0.526605505,-0.524770642,-0.52293578,
-0.521100917,-0.519266055,-0.517431193,-0.51559633,-0.513761468,-0.511926606,
-0.510091743,-0.508256881,-0.506422018,-0.504587156,-0.502752294,-0.500917431,
-0.499082569,-0.497247706,-0.495412844,-0.493577982,-0.491743119,-0.489908257,
-0.488073394,-0.486238532,-0.48440367,-0.482568807,-0.480733945,-0.478899083,
-0.47706422,-0.475229358,-0.473394495,-0.471559633,-0.469724771,-0.467889908,
-0.466055046,-0.464220183,-0.462385321,-0.460550459,-0.458715596,-0.456880734,
-0.455045872,-0.453211009,-0.451376147,-0.449541284,-0.447706422,-0.44587156,
-0.444036697,-0.442201835,-0.440366972,-0.43853211,-0.436697248,-0.434862385,
-0.433027523,-0.431192661,-0.429357798,-0.427522936,-0.425688073,-0.423853211,
-0.422018349,-0.420183486,-0.418348624,-0.416513761,-0.414678899,-0.412844037,
-0.411009174,-0.409174312,-0.40733945,-0.405504587,-0.403669725,-0.401834862,
-0.4,-0.398165138,-0.396330275,-0.394495413,-0.39266055,-0.390825688,-0.388990826,
-0.387155963,-0.385321101,-0.383486239,-0.381651376,-0.379816514,-0.377981651,
-0.376146789,-0.374311927,-0.372477064,-0.370642202,-0.368807339,-0.366972477,
-0.365137615,-0.363302752,-0.36146789,-0.359633028,-0.357798165,-0.355963303,
-0.35412844,-0.352293578,-0.350458716,-0.348623853,-0.346788991,-0.344954128,
-0.343119266,-0.341284404,-0.339449541,-0.337614679,-0.335779817,-0.333944954,
-0.332110092,-0.330275229,-0.328440367,-0.326605505,-0.324770642,-0.32293578,
-0.321100917,-0.319266055,-0.317431193,-0.31559633,-0.313761468,-0.311926606,
-0.310091743,-0.308256881,-0.306422018,-0.304587156,-0.302752294,-0.300917431,
-0.299082569,-0.297247706,-0.295412844,-0.293577982,-0.291743119,-0.289908257,
-0.288073394,-0.286238532,-0.28440367,-0.282568807,-0.280733945,-0.278899083,
-0.27706422,-0.275229358,-0.273394495,-0.271559633,-0.269724771,-0.267889908,
-0.266055046,-0.264220183,-0.262385321,-0.260550459,-0.258715596,-0.256880734,
-0.255045872,-0.253211009,-0.251376147,-0.249541284,-0.247706422,-0.24587156,
-0.244036697,-0.242201835,-0.240366972,-0.23853211,-0.236697248,-0.234862385,
-0.233027523,-0.231192661,-0.229357798,-0.227522936,-0.225688073,-0.223853211,
-0.222018349,-0.220183486,-0.218348624,-0.216513761,-0.214678899,-0.212844037,
-0.211009174,-0.209174312,-0.20733945,-0.205504587,-0.203669725,-0.201834862,
-0.2,-0.198165138,-0.196330275,-0.194495413,-0.19266055,-0.190825688,-0.188990826,
-0.187155963,-0.185321101,-0.183486239,-0.181651376,-0.179816514,-0.177981651,
-0.176146789,-0.174311927,-0.172477064,-0.170642202,-0.168807339,-0.166972477,
-0.165137615,-0.163302752,-0.16146789,-0.159633028,-0.157798165,-0.155963303,
-0.15412844,-0.152293578,-0.150458716,-0.148623853,-0.146788991,-0.144954128,
-0.143172103),(0.,0.36),.UNSPECIFIED.);
#6270=B_SPLINE_SURFACE_WITH_KNOTS('',5,1,((#244362,#244363),(#244364,#244365),
(#244366,#244367),(#244368,#244369),(#244370,#244371),(#244372,#244373),
(#244374,#244375),(#244376,#244377),(#244378,#244379),(#244380,#244381),
(#244382,#244383),(#244384,#244385),(#244386,#244387),(#244388,#244389),
(#244390,#244391),(#244392,#244393),(#244394,#244395),(#244396,#244397),
(#244398,#244399),(#244400,#244401),(#244402,#244403),(#244404,#244405),
(#244406,#244407),(#244408,#244409),(#244410,#244411),(#244412,#244413),
(#244414,#244415),(#244416,#244417),(#244418,#244419),(#244420,#244421),
(#244422,#244423),(#244424,#244425),(#244426,#244427),(#244428,#244429),
(#244430,#244431),(#244432,#244433),(#244434,#244435),(#244436,#244437),
(#244438,#244439),(#244440,#244441),(#244442,#244443),(#244444,#244445),
(#244446,#244447),(#244448,#244449),(#244450,#244451),(#244452,#244453),
(#244454,#244455),(#244456,#244457),(#244458,#244459),(#244460,#244461),
(#244462,#244463),(#244464,#244465),(#244466,#244467),(#244468,#244469),
(#244470,#244471),(#244472,#244473),(#244474,#244475),(#244476,#244477),
(#244478,#244479),(#244480,#244481),(#244482,#244483),(#244484,#244485),
(#244486,#244487),(#244488,#244489),(#244490,#244491),(#244492,#244493),
(#244494,#244495),(#244496,#244497),(#244498,#244499),(#244500,#244501),
(#244502,#244503),(#244504,#244505),(#244506,#244507),(#244508,#244509),
(#244510,#244511),(#244512,#244513),(#244514,#244515),(#244516,#244517),
(#244518,#244519),(#244520,#244521),(#244522,#244523),(#244524,#244525),
(#244526,#244527),(#244528,#244529),(#244530,#244531),(#244532,#244533),
(#244534,#244535),(#244536,#244537),(#244538,#244539),(#244540,#244541),
(#244542,#244543),(#244544,#244545),(#244546,#244547),(#244548,#244549),
(#244550,#244551),(#244552,#244553),(#244554,#244555),(#244556,#244557),
(#244558,#244559),(#244560,#244561),(#244562,#244563),(#244564,#244565),
(#244566,#244567),(#244568,#244569),(#244570,#244571),(#244572,#244573),
(#244574,#244575),(#244576,#244577),(#244578,#244579),(#244580,#244581),
(#244582,#244583),(#244584,#244585),(#244586,#244587),(#244588,#244589),
(#244590,#244591),(#244592,#244593),(#244594,#244595),(#244596,#244597),
(#244598,#244599),(#244600,#244601),(#244602,#244603),(#244604,#244605),
(#244606,#244607),(#244608,#244609),(#244610,#244611),(#244612,#244613),
(#244614,#244615),(#244616,#244617),(#244618,#244619),(#244620,#244621),
(#244622,#244623),(#244624,#244625),(#244626,#244627),(#244628,#244629),
(#244630,#244631),(#244632,#244633),(#244634,#244635),(#244636,#244637),
(#244638,#244639),(#244640,#244641),(#244642,#244643),(#244644,#244645),
(#244646,#244647),(#244648,#244649),(#244650,#244651),(#244652,#244653),
(#244654,#244655),(#244656,#244657),(#244658,#244659),(#244660,#244661),
(#244662,#244663),(#244664,#244665),(#244666,#244667),(#244668,#244669),
(#244670,#244671),(#244672,#244673),(#244674,#244675),(#244676,#244677),
(#244678,#244679),(#244680,#244681),(#244682,#244683),(#244684,#244685),
(#244686,#244687),(#244688,#244689),(#244690,#244691),(#244692,#244693),
(#244694,#244695),(#244696,#244697),(#244698,#244699),(#244700,#244701),
(#244702,#244703),(#244704,#244705),(#244706,#244707),(#244708,#244709),
(#244710,#244711),(#244712,#244713),(#244714,#244715),(#244716,#244717),
(#244718,#244719),(#244720,#244721),(#244722,#244723),(#244724,#244725),
(#244726,#244727),(#244728,#244729),(#244730,#244731),(#244732,#244733),
(#244734,#244735),(#244736,#244737),(#244738,#244739),(#244740,#244741),
(#244742,#244743),(#244744,#244745),(#244746,#244747),(#244748,#244749),
(#244750,#244751),(#244752,#244753),(#244754,#244755),(#244756,#244757),
(#244758,#244759),(#244760,#244761),(#244762,#244763),(#244764,#244765),
(#244766,#244767),(#244768,#244769),(#244770,#244771),(#244772,#244773),
(#244774,#244775),(#244776,#244777),(#244778,#244779),(#244780,#244781),
(#244782,#244783),(#244784,#244785),(#244786,#244787),(#244788,#244789),
(#244790,#244791),(#244792,#244793),(#244794,#244795),(#244796,#244797),
(#244798,#244799),(#244800,#244801),(#244802,#244803),(#244804,#244805),
(#244806,#244807),(#244808,#244809),(#244810,#244811),(#244812,#244813),
(#244814,#244815),(#244816,#244817),(#244818,#244819),(#244820,#244821),
(#244822,#244823),(#244824,#244825),(#244826,#244827),(#244828,#244829),
(#244830,#244831),(#244832,#244833),(#244834,#244835),(#244836,#244837),
(#244838,#244839),(#244840,#244841),(#244842,#244843),(#244844,#244845),
(#244846,#244847),(#244848,#244849),(#244850,#244851),(#244852,#244853),
(#244854,#244855),(#244856,#244857),(#244858,#244859),(#244860,#244861),
(#244862,#244863),(#244864,#244865),(#244866,#244867),(#244868,#244869),
(#244870,#244871),(#244872,#244873),(#244874,#244875),(#244876,#244877),
(#244878,#244879),(#244880,#244881),(#244882,#244883),(#244884,#244885),
(#244886,#244887),(#244888,#244889),(#244890,#244891),(#244892,#244893),
(#244894,#244895),(#244896,#244897),(#244898,#244899),(#244900,#244901),
(#244902,#244903),(#244904,#244905),(#244906,#244907),(#244908,#244909),
(#244910,#244911),(#244912,#244913),(#244914,#244915),(#244916,#244917),
(#244918,#244919),(#244920,#244921),(#244922,#244923),(#244924,#244925),
(#244926,#244927),(#244928,#244929),(#244930,#244931),(#244932,#244933),
(#244934,#244935),(#244936,#244937),(#244938,#244939),(#244940,#244941),
(#244942,#244943),(#244944,#244945),(#244946,#244947),(#244948,#244949),
(#244950,#244951),(#244952,#244953),(#244954,#244955),(#244956,#244957),
(#244958,#244959),(#244960,#244961),(#244962,#244963),(#244964,#244965),
(#244966,#244967),(#244968,#244969),(#244970,#244971),(#244972,#244973),
(#244974,#244975),(#244976,#244977),(#244978,#244979),(#244980,#244981),
(#244982,#244983),(#244984,#244985),(#244986,#244987),(#244988,#244989),
(#244990,#244991),(#244992,#244993),(#244994,#244995),(#244996,#244997),
(#244998,#244999),(#245000,#245001),(#245002,#245003),(#245004,#245005),
(#245006,#245007),(#245008,#245009),(#245010,#245011),(#245012,#245013),
(#245014,#245015),(#245016,#245017),(#245018,#245019),(#245020,#245021),
(#245022,#245023),(#245024,#245025),(#245026,#245027),(#245028,#245029),
(#245030,#245031),(#245032,#245033),(#245034,#245035),(#245036,#245037),
(#245038,#245039),(#245040,#245041),(#245042,#245043),(#245044,#245045),
(#245046,#245047),(#245048,#245049),(#245050,#245051),(#245052,#245053),
(#245054,#245055),(#245056,#245057),(#245058,#245059),(#245060,#245061),
(#245062,#245063),(#245064,#245065),(#245066,#245067),(#245068,#245069),
(#245070,#245071),(#245072,#245073),(#245074,#245075),(#245076,#245077),
(#245078,#245079),(#245080,#245081),(#245082,#245083),(#245084,#245085),
(#245086,#245087),(#245088,#245089),(#245090,#245091),(#245092,#245093),
(#245094,#245095),(#245096,#245097),(#245098,#245099),(#245100,#245101),
(#245102,#245103),(#245104,#245105),(#245106,#245107),(#245108,#245109),
(#245110,#245111),(#245112,#245113),(#245114,#245115),(#245116,#245117),
(#245118,#245119),(#245120,#245121),(#245122,#245123),(#245124,#245125),
(#245126,#245127),(#245128,#245129),(#245130,#245131),(#245132,#245133),
(#245134,#245135),(#245136,#245137),(#245138,#245139),(#245140,#245141),
(#245142,#245143),(#245144,#245145),(#245146,#245147),(#245148,#245149),
(#245150,#245151),(#245152,#245153),(#245154,#245155),(#245156,#245157),
(#245158,#245159),(#245160,#245161),(#245162,#245163),(#245164,#245165),
(#245166,#245167),(#245168,#245169),(#245170,#245171),(#245172,#245173),
(#245174,#245175),(#245176,#245177),(#245178,#245179),(#245180,#245181),
(#245182,#245183),(#245184,#245185),(#245186,#245187),(#245188,#245189),
(#245190,#245191),(#245192,#245193),(#245194,#245195),(#245196,#245197),
(#245198,#245199),(#245200,#245201),(#245202,#245203),(#245204,#245205),
(#245206,#245207),(#245208,#245209),(#245210,#245211),(#245212,#245213),
(#245214,#245215),(#245216,#245217),(#245218,#245219),(#245220,#245221),
(#245222,#245223),(#245224,#245225),(#245226,#245227),(#245228,#245229),
(#245230,#245231),(#245232,#245233),(#245234,#245235),(#245236,#245237),
(#245238,#245239),(#245240,#245241),(#245242,#245243),(#245244,#245245),
(#245246,#245247),(#245248,#245249),(#245250,#245251),(#245252,#245253),
(#245254,#245255),(#245256,#245257),(#245258,#245259),(#245260,#245261),
(#245262,#245263),(#245264,#245265),(#245266,#245267),(#245268,#245269),
(#245270,#245271),(#245272,#245273),(#245274,#245275),(#245276,#245277),
(#245278,#245279),(#245280,#245281),(#245282,#245283),(#245284,#245285),
(#245286,#245287),(#245288,#245289),(#245290,#245291),(#245292,#245293),
(#245294,#245295),(#245296,#245297),(#245298,#245299),(#245300,#245301),
(#245302,#245303),(#245304,#245305)),.UNSPECIFIED.,.F.,.F.,.F.,(6,1,1,1,
1,1,1,1,1,1,1,1,1,1,1,1,1,1,1,1,1,1,1,1,1,1,1,1,1,1,1,1,1,1,1,1,1,1,1,1,
1,1,1,1,1,1,1,1,1,1,1,1,1,1,1,1,1,1,1,1,1,1,1,1,1,1,1,1,1,1,1,1,1,1,1,1,
1,1,1,1,1,1,1,1,1,1,1,1,1,1,1,1,1,1,1,1,1,1,1,1,1,1,1,1,1,1,1,1,1,1,1,1,
1,1,1,1,1,1,1,1,1,1,1,1,1,1,1,1,1,1,1,1,1,1,1,1,1,1,1,1,1,1,1,1,1,1,1,1,
1,1,1,1,1,1,1,1,1,1,1,1,1,1,1,1,1,1,1,1,1,1,1,1,1,1,1,1,1,1,1,1,1,1,1,1,
1,1,1,1,1,1,1,1,1,1,1,1,1,1,1,1,1,1,1,1,1,1,1,1,1,1,1,1,1,1,1,1,1,1,1,1,
1,1,1,1,1,1,1,1,1,1,1,1,1,1,1,1,1,1,1,1,1,1,1,1,1,1,1,1,1,1,1,1,1,1,1,1,
1,1,1,1,1,1,1,1,1,1,1,1,1,1,1,1,1,1,1,1,1,1,1,1,1,1,1,1,1,1,1,1,1,1,1,1,
1,1,1,1,1,1,1,1,1,1,1,1,1,1,1,1,1,1,1,1,1,1,1,1,1,1,1,1,1,1,1,1,1,1,1,1,
1,1,1,1,1,1,1,1,1,1,1,1,1,1,1,1,1,1,1,1,1,1,1,1,1,1,1,1,1,1,1,1,1,1,1,1,
1,1,1,1,1,1,1,1,1,1,1,1,1,1,1,1,1,1,1,1,1,1,1,1,1,1,1,1,1,1,1,1,1,1,1,1,
1,1,1,1,1,1,1,1,1,1,1,1,1,1,1,1,1,1,1,1,1,1,1,1,1,1,1,1,1,1,1,1,1,1,1,1,
1,1,1,1,1,1,1,1,1,1,1,1,1,1,1,1,1,1,1,1,1,1,1,1,1,1,1,1,1,1,1,6),(2,2),
(0.143172104,0.144954128,0.146788991,0.148623853,0.150458716,0.152293578,
0.15412844,0.155963303,0.157798165,0.159633028,0.16146789,0.163302752,0.165137615,
0.166972477,0.168807339,0.170642202,0.172477064,0.174311927,0.176146789,
0.177981651,0.179816514,0.181651376,0.183486239,0.185321101,0.187155963,
0.188990826,0.190825688,0.19266055,0.194495413,0.196330275,0.198165138,
0.2,0.201834862,0.203669725,0.205504587,0.20733945,0.209174312,0.211009174,
0.212844037,0.214678899,0.216513761,0.218348624,0.220183486,0.222018349,
0.223853211,0.225688073,0.227522936,0.229357798,0.231192661,0.233027523,
0.234862385,0.236697248,0.23853211,0.240366972,0.242201835,0.244036697,
0.24587156,0.247706422,0.249541284,0.251376147,0.253211009,0.255045872,
0.256880734,0.258715596,0.260550459,0.262385321,0.264220183,0.266055046,
0.267889908,0.269724771,0.271559633,0.273394495,0.275229358,0.27706422,
0.278899083,0.280733945,0.282568807,0.28440367,0.286238532,0.288073394,
0.289908257,0.291743119,0.293577982,0.295412844,0.297247706,0.299082569,
0.300917431,0.302752294,0.304587156,0.306422018,0.308256881,0.310091743,
0.311926606,0.313761468,0.31559633,0.317431193,0.319266055,0.321100917,
0.32293578,0.324770642,0.326605505,0.328440367,0.330275229,0.332110092,
0.333944954,0.335779817,0.337614679,0.339449541,0.341284404,0.343119266,
0.344954128,0.346788991,0.348623853,0.350458716,0.352293578,0.35412844,
0.355963303,0.357798165,0.359633028,0.36146789,0.363302752,0.365137615,
0.366972477,0.368807339,0.370642202,0.372477064,0.374311927,0.376146789,
0.377981651,0.379816514,0.381651376,0.383486239,0.385321101,0.387155963,
0.388990826,0.390825688,0.39266055,0.394495413,0.396330275,0.398165138,
0.4,0.401834862,0.403669725,0.405504587,0.40733945,0.409174312,0.411009174,
0.412844037,0.414678899,0.416513761,0.418348624,0.420183486,0.422018349,
0.423853211,0.425688073,0.427522936,0.429357798,0.431192661,0.433027523,
0.434862385,0.436697248,0.43853211,0.440366972,0.442201835,0.444036697,
0.44587156,0.447706422,0.449541284,0.451376147,0.453211009,0.455045872,
0.456880734,0.458715596,0.460550459,0.462385321,0.464220183,0.466055046,
0.467889908,0.469724771,0.471559633,0.473394495,0.475229358,0.47706422,
0.478899083,0.480733945,0.482568807,0.48440367,0.486238532,0.488073394,
0.489908257,0.491743119,0.493577982,0.495412844,0.497247706,0.499082569,
0.500917431,0.502752294,0.504587156,0.506422018,0.508256881,0.510091743,
0.511926606,0.513761468,0.51559633,0.517431193,0.519266055,0.521100917,
0.52293578,0.524770642,0.526605505,0.528440367,0.530275229,0.532110092,
0.533944954,0.535779817,0.537614679,0.539449541,0.541284404,0.543119266,
0.544954128,0.546788991,0.548623853,0.550458716,0.552293578,0.55412844,
0.555963303,0.557798165,0.559633028,0.56146789,0.563302752,0.565137615,
0.566972477,0.568807339,0.570642202,0.572477064,0.574311927,0.576146789,
0.577981651,0.579816514,0.581651376,0.583486239,0.585321101,0.587155963,
0.588990826,0.590825688,0.59266055,0.594495413,0.596330275,0.598165138,
0.6,0.601834862,0.603669725,0.605504587,0.60733945,0.609174312,0.611009174,
0.612844037,0.614678899,0.616513761,0.618348624,0.620183486,0.622018349,
0.623853211,0.625688073,0.627522936,0.629357798,0.631192661,0.633027523,
0.634862385,0.636697248,0.63853211,0.640366972,0.642201835,0.644036697,
0.64587156,0.647706422,0.649541284,0.651376147,0.653211009,0.655045872,
0.656880734,0.658715596,0.660550459,0.662385321,0.664220183,0.666055046,
0.667889908,0.669724771,0.671559633,0.673394495,0.675229358,0.67706422,
0.678899083,0.680733945,0.682568807,0.68440367,0.686238532,0.688073394,
0.689908257,0.691743119,0.693577982,0.695412844,0.697247706,0.699082569,
0.700917431,0.702752294,0.704587156,0.706422018,0.708256881,0.710091743,
0.711926606,0.713761468,0.71559633,0.717431193,0.719266055,0.721100917,
0.72293578,0.724770642,0.726605505,0.728440367,0.730275229,0.732110092,
0.733944954,0.735779817,0.737614679,0.739449541,0.741284404,0.743119266,
0.744954128,0.746788991,0.748623853,0.750458716,0.752293578,0.75412844,
0.755963303,0.757798165,0.759633028,0.76146789,0.763302752,0.765137615,
0.766972477,0.768807339,0.770642202,0.772477064,0.774311927,0.776146789,
0.777981651,0.779816514,0.781651376,0.783486239,0.785321101,0.787155963,
0.788990826,0.790825688,0.79266055,0.794495413,0.796330275,0.798165138,
0.8,0.801834862,0.803669725,0.805504587,0.80733945,0.809174312,0.811009174,
0.812844037,0.814678899,0.816513761,0.818348624,0.820183486,0.822018349,
0.823853211,0.825688073,0.827522936,0.829357798,0.831192661,0.833027523,
0.834862385,0.836697248,0.83853211,0.840366972,0.842201835,0.844036697,
0.84587156,0.847706422,0.849541284,0.851376147,0.853211009,0.855045872,
0.856880734,0.858715596,0.860550459,0.862385321,0.864220183,0.866055046,
0.867889908,0.869724771,0.871559633,0.873394495,0.875229358,0.87706422,
0.878899083,0.880733945,0.882568807,0.88440367,0.886238532,0.888073394,
0.889908257,0.891743119,0.893577982,0.895412844,0.897247706,0.899082569,
0.900917431,0.902752294,0.904587156,0.906422018,0.908256881,0.910091743,
0.911926606,0.913761468,0.91559633,0.917431193,0.919266055,0.921100917,
0.92293578,0.924770642,0.926605505,0.928440367,0.930275229,0.932110092,
0.933944954,0.935779817,0.937614679,0.939449541,0.941284404,0.943119266,
0.944954128,0.946788991,0.948623853,0.950458716,0.952293578,0.95412844,
0.955963303,0.957798165,0.959633028,0.96146789,0.963302752,0.965137615,
0.966972477,0.968807339,0.970642202,0.972477064,0.974311927,0.976146789,
0.977981651,0.979816514,0.981651376,0.983486239,0.985321101,0.987155963,
0.988990826,0.990825688,0.99266055,0.994495413,0.996330275,0.998165138,
1.),(0.,0.36),.UNSPECIFIED.);
#6271=B_SPLINE_SURFACE_WITH_KNOTS('',5,1,((#246265,#246266),(#246267,#246268),
(#246269,#246270),(#246271,#246272),(#246273,#246274),(#246275,#246276),
(#246277,#246278),(#246279,#246280),(#246281,#246282),(#246283,#246284),
(#246285,#246286),(#246287,#246288),(#246289,#246290),(#246291,#246292),
(#246293,#246294),(#246295,#246296),(#246297,#246298),(#246299,#246300),
(#246301,#246302),(#246303,#246304),(#246305,#246306),(#246307,#246308),
(#246309,#246310),(#246311,#246312),(#246313,#246314),(#246315,#246316),
(#246317,#246318),(#246319,#246320),(#246321,#246322),(#246323,#246324),
(#246325,#246326),(#246327,#246328),(#246329,#246330),(#246331,#246332),
(#246333,#246334),(#246335,#246336),(#246337,#246338),(#246339,#246340),
(#246341,#246342),(#246343,#246344),(#246345,#246346),(#246347,#246348),
(#246349,#246350),(#246351,#246352),(#246353,#246354),(#246355,#246356),
(#246357,#246358),(#246359,#246360),(#246361,#246362),(#246363,#246364),
(#246365,#246366),(#246367,#246368),(#246369,#246370),(#246371,#246372),
(#246373,#246374),(#246375,#246376),(#246377,#246378),(#246379,#246380),
(#246381,#246382),(#246383,#246384),(#246385,#246386),(#246387,#246388),
(#246389,#246390),(#246391,#246392),(#246393,#246394),(#246395,#246396),
(#246397,#246398),(#246399,#246400),(#246401,#246402),(#246403,#246404),
(#246405,#246406),(#246407,#246408),(#246409,#246410),(#246411,#246412),
(#246413,#246414),(#246415,#246416),(#246417,#246418),(#246419,#246420),
(#246421,#246422),(#246423,#246424),(#246425,#246426),(#246427,#246428),
(#246429,#246430),(#246431,#246432),(#246433,#246434),(#246435,#246436),
(#246437,#246438),(#246439,#246440),(#246441,#246442),(#246443,#246444),
(#246445,#246446),(#246447,#246448),(#246449,#246450),(#246451,#246452),
(#246453,#246454),(#246455,#246456),(#246457,#246458),(#246459,#246460),
(#246461,#246462),(#246463,#246464),(#246465,#246466),(#246467,#246468),
(#246469,#246470),(#246471,#246472),(#246473,#246474),(#246475,#246476),
(#246477,#246478),(#246479,#246480),(#246481,#246482),(#246483,#246484),
(#246485,#246486),(#246487,#246488),(#246489,#246490),(#246491,#246492),
(#246493,#246494),(#246495,#246496),(#246497,#246498),(#246499,#246500),
(#246501,#246502),(#246503,#246504),(#246505,#246506),(#246507,#246508),
(#246509,#246510),(#246511,#246512),(#246513,#246514),(#246515,#246516),
(#246517,#246518),(#246519,#246520),(#246521,#246522),(#246523,#246524),
(#246525,#246526),(#246527,#246528),(#246529,#246530),(#246531,#246532),
(#246533,#246534),(#246535,#246536),(#246537,#246538),(#246539,#246540),
(#246541,#246542),(#246543,#246544),(#246545,#246546),(#246547,#246548),
(#246549,#246550),(#246551,#246552),(#246553,#246554),(#246555,#246556),
(#246557,#246558),(#246559,#246560),(#246561,#246562),(#246563,#246564),
(#246565,#246566),(#246567,#246568),(#246569,#246570),(#246571,#246572),
(#246573,#246574),(#246575,#246576),(#246577,#246578),(#246579,#246580),
(#246581,#246582),(#246583,#246584),(#246585,#246586),(#246587,#246588),
(#246589,#246590),(#246591,#246592),(#246593,#246594),(#246595,#246596),
(#246597,#246598),(#246599,#246600),(#246601,#246602),(#246603,#246604),
(#246605,#246606),(#246607,#246608),(#246609,#246610),(#246611,#246612),
(#246613,#246614),(#246615,#246616),(#246617,#246618),(#246619,#246620),
(#246621,#246622),(#246623,#246624),(#246625,#246626),(#246627,#246628),
(#246629,#246630),(#246631,#246632),(#246633,#246634),(#246635,#246636),
(#246637,#246638),(#246639,#246640),(#246641,#246642),(#246643,#246644),
(#246645,#246646),(#246647,#246648),(#246649,#246650),(#246651,#246652),
(#246653,#246654),(#246655,#246656),(#246657,#246658),(#246659,#246660),
(#246661,#246662),(#246663,#246664),(#246665,#246666),(#246667,#246668),
(#246669,#246670),(#246671,#246672),(#246673,#246674),(#246675,#246676),
(#246677,#246678),(#246679,#246680),(#246681,#246682),(#246683,#246684),
(#246685,#246686),(#246687,#246688),(#246689,#246690),(#246691,#246692),
(#246693,#246694),(#246695,#246696),(#246697,#246698),(#246699,#246700),
(#246701,#246702),(#246703,#246704),(#246705,#246706),(#246707,#246708),
(#246709,#246710),(#246711,#246712),(#246713,#246714),(#246715,#246716),
(#246717,#246718),(#246719,#246720),(#246721,#246722),(#246723,#246724),
(#246725,#246726),(#246727,#246728),(#246729,#246730),(#246731,#246732),
(#246733,#246734),(#246735,#246736),(#246737,#246738),(#246739,#246740),
(#246741,#246742),(#246743,#246744),(#246745,#246746),(#246747,#246748),
(#246749,#246750),(#246751,#246752),(#246753,#246754),(#246755,#246756),
(#246757,#246758),(#246759,#246760),(#246761,#246762),(#246763,#246764),
(#246765,#246766),(#246767,#246768),(#246769,#246770),(#246771,#246772),
(#246773,#246774),(#246775,#246776),(#246777,#246778),(#246779,#246780),
(#246781,#246782),(#246783,#246784),(#246785,#246786),(#246787,#246788),
(#246789,#246790),(#246791,#246792),(#246793,#246794),(#246795,#246796),
(#246797,#246798),(#246799,#246800),(#246801,#246802),(#246803,#246804),
(#246805,#246806),(#246807,#246808),(#246809,#246810),(#246811,#246812),
(#246813,#246814),(#246815,#246816),(#246817,#246818),(#246819,#246820),
(#246821,#246822),(#246823,#246824),(#246825,#246826),(#246827,#246828),
(#246829,#246830),(#246831,#246832),(#246833,#246834),(#246835,#246836),
(#246837,#246838),(#246839,#246840),(#246841,#246842),(#246843,#246844),
(#246845,#246846),(#246847,#246848),(#246849,#246850),(#246851,#246852),
(#246853,#246854),(#246855,#246856),(#246857,#246858),(#246859,#246860),
(#246861,#246862),(#246863,#246864),(#246865,#246866),(#246867,#246868),
(#246869,#246870),(#246871,#246872),(#246873,#246874),(#246875,#246876),
(#246877,#246878),(#246879,#246880),(#246881,#246882),(#246883,#246884),
(#246885,#246886),(#246887,#246888),(#246889,#246890),(#246891,#246892),
(#246893,#246894),(#246895,#246896),(#246897,#246898),(#246899,#246900),
(#246901,#246902),(#246903,#246904),(#246905,#246906),(#246907,#246908),
(#246909,#246910),(#246911,#246912),(#246913,#246914),(#246915,#246916),
(#246917,#246918),(#246919,#246920),(#246921,#246922),(#246923,#246924),
(#246925,#246926),(#246927,#246928),(#246929,#246930),(#246931,#246932),
(#246933,#246934),(#246935,#246936),(#246937,#246938),(#246939,#246940),
(#246941,#246942),(#246943,#246944),(#246945,#246946),(#246947,#246948),
(#246949,#246950),(#246951,#246952),(#246953,#246954),(#246955,#246956),
(#246957,#246958),(#246959,#246960),(#246961,#246962),(#246963,#246964),
(#246965,#246966),(#246967,#246968),(#246969,#246970),(#246971,#246972),
(#246973,#246974),(#246975,#246976),(#246977,#246978),(#246979,#246980),
(#246981,#246982),(#246983,#246984),(#246985,#246986),(#246987,#246988),
(#246989,#246990),(#246991,#246992),(#246993,#246994),(#246995,#246996),
(#246997,#246998),(#246999,#247000),(#247001,#247002),(#247003,#247004),
(#247005,#247006),(#247007,#247008),(#247009,#247010),(#247011,#247012),
(#247013,#247014),(#247015,#247016),(#247017,#247018),(#247019,#247020),
(#247021,#247022),(#247023,#247024),(#247025,#247026),(#247027,#247028),
(#247029,#247030),(#247031,#247032),(#247033,#247034),(#247035,#247036),
(#247037,#247038),(#247039,#247040),(#247041,#247042),(#247043,#247044),
(#247045,#247046),(#247047,#247048),(#247049,#247050),(#247051,#247052),
(#247053,#247054),(#247055,#247056),(#247057,#247058),(#247059,#247060),
(#247061,#247062),(#247063,#247064),(#247065,#247066),(#247067,#247068),
(#247069,#247070),(#247071,#247072),(#247073,#247074),(#247075,#247076),
(#247077,#247078),(#247079,#247080),(#247081,#247082),(#247083,#247084),
(#247085,#247086),(#247087,#247088),(#247089,#247090),(#247091,#247092),
(#247093,#247094),(#247095,#247096),(#247097,#247098),(#247099,#247100),
(#247101,#247102),(#247103,#247104),(#247105,#247106),(#247107,#247108),
(#247109,#247110),(#247111,#247112),(#247113,#247114),(#247115,#247116),
(#247117,#247118),(#247119,#247120),(#247121,#247122),(#247123,#247124),
(#247125,#247126),(#247127,#247128),(#247129,#247130),(#247131,#247132),
(#247133,#247134),(#247135,#247136),(#247137,#247138),(#247139,#247140),
(#247141,#247142),(#247143,#247144),(#247145,#247146),(#247147,#247148),
(#247149,#247150),(#247151,#247152),(#247153,#247154),(#247155,#247156),
(#247157,#247158),(#247159,#247160),(#247161,#247162),(#247163,#247164),
(#247165,#247166),(#247167,#247168),(#247169,#247170),(#247171,#247172),
(#247173,#247174),(#247175,#247176),(#247177,#247178),(#247179,#247180),
(#247181,#247182),(#247183,#247184),(#247185,#247186),(#247187,#247188),
(#247189,#247190),(#247191,#247192),(#247193,#247194),(#247195,#247196),
(#247197,#247198),(#247199,#247200),(#247201,#247202),(#247203,#247204),
(#247205,#247206),(#247207,#247208)),.UNSPECIFIED.,.F.,.F.,.F.,(6,1,1,1,
1,1,1,1,1,1,1,1,1,1,1,1,1,1,1,1,1,1,1,1,1,1,1,1,1,1,1,1,1,1,1,1,1,1,1,1,
1,1,1,1,1,1,1,1,1,1,1,1,1,1,1,1,1,1,1,1,1,1,1,1,1,1,1,1,1,1,1,1,1,1,1,1,
1,1,1,1,1,1,1,1,1,1,1,1,1,1,1,1,1,1,1,1,1,1,1,1,1,1,1,1,1,1,1,1,1,1,1,1,
1,1,1,1,1,1,1,1,1,1,1,1,1,1,1,1,1,1,1,1,1,1,1,1,1,1,1,1,1,1,1,1,1,1,1,1,
1,1,1,1,1,1,1,1,1,1,1,1,1,1,1,1,1,1,1,1,1,1,1,1,1,1,1,1,1,1,1,1,1,1,1,1,
1,1,1,1,1,1,1,1,1,1,1,1,1,1,1,1,1,1,1,1,1,1,1,1,1,1,1,1,1,1,1,1,1,1,1,1,
1,1,1,1,1,1,1,1,1,1,1,1,1,1,1,1,1,1,1,1,1,1,1,1,1,1,1,1,1,1,1,1,1,1,1,1,
1,1,1,1,1,1,1,1,1,1,1,1,1,1,1,1,1,1,1,1,1,1,1,1,1,1,1,1,1,1,1,1,1,1,1,1,
1,1,1,1,1,1,1,1,1,1,1,1,1,1,1,1,1,1,1,1,1,1,1,1,1,1,1,1,1,1,1,1,1,1,1,1,
1,1,1,1,1,1,1,1,1,1,1,1,1,1,1,1,1,1,1,1,1,1,1,1,1,1,1,1,1,1,1,1,1,1,1,1,
1,1,1,1,1,1,1,1,1,1,1,1,1,1,1,1,1,1,1,1,1,1,1,1,1,1,1,1,1,1,1,1,1,1,1,1,
1,1,1,1,1,1,1,1,1,1,1,1,1,1,1,1,1,1,1,1,1,1,1,1,1,1,1,1,1,1,1,1,1,1,1,1,
1,1,1,1,1,1,1,1,1,1,1,1,1,1,1,1,1,1,1,1,1,1,1,1,1,1,1,1,1,1,1,6),(2,2),
(0.143172103,0.144954128,0.146788991,0.148623853,0.150458716,0.152293578,
0.15412844,0.155963303,0.157798165,0.159633028,0.16146789,0.163302752,0.165137615,
0.166972477,0.168807339,0.170642202,0.172477064,0.174311927,0.176146789,
0.177981651,0.179816514,0.181651376,0.183486239,0.185321101,0.187155963,
0.188990826,0.190825688,0.19266055,0.194495413,0.196330275,0.198165138,
0.2,0.201834862,0.203669725,0.205504587,0.20733945,0.209174312,0.211009174,
0.212844037,0.214678899,0.216513761,0.218348624,0.220183486,0.222018349,
0.223853211,0.225688073,0.227522936,0.229357798,0.231192661,0.233027523,
0.234862385,0.236697248,0.23853211,0.240366972,0.242201835,0.244036697,
0.24587156,0.247706422,0.249541284,0.251376147,0.253211009,0.255045872,
0.256880734,0.258715596,0.260550459,0.262385321,0.264220183,0.266055046,
0.267889908,0.269724771,0.271559633,0.273394495,0.275229358,0.27706422,
0.278899083,0.280733945,0.282568807,0.28440367,0.286238532,0.288073394,
0.289908257,0.291743119,0.293577982,0.295412844,0.297247706,0.299082569,
0.300917431,0.302752294,0.304587156,0.306422018,0.308256881,0.310091743,
0.311926606,0.313761468,0.31559633,0.317431193,0.319266055,0.321100917,
0.32293578,0.324770642,0.326605505,0.328440367,0.330275229,0.332110092,
0.333944954,0.335779817,0.337614679,0.339449541,0.341284404,0.343119266,
0.344954128,0.346788991,0.348623853,0.350458716,0.352293578,0.35412844,
0.355963303,0.357798165,0.359633028,0.36146789,0.363302752,0.365137615,
0.366972477,0.368807339,0.370642202,0.372477064,0.374311927,0.376146789,
0.377981651,0.379816514,0.381651376,0.383486239,0.385321101,0.387155963,
0.388990826,0.390825688,0.39266055,0.394495413,0.396330275,0.398165138,
0.4,0.401834862,0.403669725,0.405504587,0.40733945,0.409174312,0.411009174,
0.412844037,0.414678899,0.416513761,0.418348624,0.420183486,0.422018349,
0.423853211,0.425688073,0.427522936,0.429357798,0.431192661,0.433027523,
0.434862385,0.436697248,0.43853211,0.440366972,0.442201835,0.444036697,
0.44587156,0.447706422,0.449541284,0.451376147,0.453211009,0.455045872,
0.456880734,0.458715596,0.460550459,0.462385321,0.464220183,0.466055046,
0.467889908,0.469724771,0.471559633,0.473394495,0.475229358,0.47706422,
0.478899083,0.480733945,0.482568807,0.48440367,0.486238532,0.488073394,
0.489908257,0.491743119,0.493577982,0.495412844,0.497247706,0.499082569,
0.500917431,0.502752294,0.504587156,0.506422018,0.508256881,0.510091743,
0.511926606,0.513761468,0.51559633,0.517431193,0.519266055,0.521100917,
0.52293578,0.524770642,0.526605505,0.528440367,0.530275229,0.532110092,
0.533944954,0.535779817,0.537614679,0.539449541,0.541284404,0.543119266,
0.544954128,0.546788991,0.548623853,0.550458716,0.552293578,0.55412844,
0.555963303,0.557798165,0.559633028,0.56146789,0.563302752,0.565137615,
0.566972477,0.568807339,0.570642202,0.572477064,0.574311927,0.576146789,
0.577981651,0.579816514,0.581651376,0.583486239,0.585321101,0.587155963,
0.588990826,0.590825688,0.59266055,0.594495413,0.596330275,0.598165138,
0.6,0.601834862,0.603669725,0.605504587,0.60733945,0.609174312,0.611009174,
0.612844037,0.614678899,0.616513761,0.618348624,0.620183486,0.622018349,
0.623853211,0.625688073,0.627522936,0.629357798,0.631192661,0.633027523,
0.634862385,0.636697248,0.63853211,0.640366972,0.642201835,0.644036697,
0.64587156,0.647706422,0.649541284,0.651376147,0.653211009,0.655045872,
0.656880734,0.658715596,0.660550459,0.662385321,0.664220183,0.666055046,
0.667889908,0.669724771,0.671559633,0.673394495,0.675229358,0.67706422,
0.678899083,0.680733945,0.682568807,0.68440367,0.686238532,0.688073394,
0.689908257,0.691743119,0.693577982,0.695412844,0.697247706,0.699082569,
0.700917431,0.702752294,0.704587156,0.706422018,0.708256881,0.710091743,
0.711926606,0.713761468,0.71559633,0.717431193,0.719266055,0.721100917,
0.72293578,0.724770642,0.726605505,0.728440367,0.730275229,0.732110092,
0.733944954,0.735779817,0.737614679,0.739449541,0.741284404,0.743119266,
0.744954128,0.746788991,0.748623853,0.750458716,0.752293578,0.75412844,
0.755963303,0.757798165,0.759633028,0.76146789,0.763302752,0.765137615,
0.766972477,0.768807339,0.770642202,0.772477064,0.774311927,0.776146789,
0.777981651,0.779816514,0.781651376,0.783486239,0.785321101,0.787155963,
0.788990826,0.790825688,0.79266055,0.794495413,0.796330275,0.798165138,
0.8,0.801834862,0.803669725,0.805504587,0.80733945,0.809174312,0.811009174,
0.812844037,0.814678899,0.816513761,0.818348624,0.820183486,0.822018349,
0.823853211,0.825688073,0.827522936,0.829357798,0.831192661,0.833027523,
0.834862385,0.836697248,0.83853211,0.840366972,0.842201835,0.844036697,
0.84587156,0.847706422,0.849541284,0.851376147,0.853211009,0.855045872,
0.856880734,0.858715596,0.860550459,0.862385321,0.864220183,0.866055046,
0.867889908,0.869724771,0.871559633,0.873394495,0.875229358,0.87706422,
0.878899083,0.880733945,0.882568807,0.88440367,0.886238532,0.888073394,
0.889908257,0.891743119,0.893577982,0.895412844,0.897247706,0.899082569,
0.900917431,0.902752294,0.904587156,0.906422018,0.908256881,0.910091743,
0.911926606,0.913761468,0.91559633,0.917431193,0.919266055,0.921100917,
0.92293578,0.924770642,0.926605505,0.928440367,0.930275229,0.932110092,
0.933944954,0.935779817,0.937614679,0.939449541,0.941284404,0.943119266,
0.944954128,0.946788991,0.948623853,0.950458716,0.952293578,0.95412844,
0.955963303,0.957798165,0.959633028,0.96146789,0.963302752,0.965137615,
0.966972477,0.968807339,0.970642202,0.972477064,0.974311927,0.976146789,
0.977981651,0.979816514,0.981651376,0.983486239,0.985321101,0.987155963,
0.988990826,0.990825688,0.99266055,0.994495413,0.996330275,0.998165138,
1.),(0.,0.36),.UNSPECIFIED.);
#6272=B_SPLINE_SURFACE_WITH_KNOTS('',5,1,((#247844,#247845),(#247846,#247847),
(#247848,#247849),(#247850,#247851),(#247852,#247853),(#247854,#247855),
(#247856,#247857),(#247858,#247859),(#247860,#247861),(#247862,#247863),
(#247864,#247865),(#247866,#247867),(#247868,#247869),(#247870,#247871),
(#247872,#247873),(#247874,#247875),(#247876,#247877),(#247878,#247879),
(#247880,#247881),(#247882,#247883),(#247884,#247885),(#247886,#247887),
(#247888,#247889),(#247890,#247891),(#247892,#247893),(#247894,#247895),
(#247896,#247897),(#247898,#247899),(#247900,#247901),(#247902,#247903),
(#247904,#247905),(#247906,#247907),(#247908,#247909),(#247910,#247911),
(#247912,#247913),(#247914,#247915),(#247916,#247917),(#247918,#247919),
(#247920,#247921),(#247922,#247923),(#247924,#247925),(#247926,#247927),
(#247928,#247929),(#247930,#247931),(#247932,#247933),(#247934,#247935),
(#247936,#247937),(#247938,#247939),(#247940,#247941),(#247942,#247943),
(#247944,#247945),(#247946,#247947),(#247948,#247949),(#247950,#247951),
(#247952,#247953),(#247954,#247955),(#247956,#247957),(#247958,#247959),
(#247960,#247961),(#247962,#247963),(#247964,#247965),(#247966,#247967),
(#247968,#247969),(#247970,#247971),(#247972,#247973),(#247974,#247975),
(#247976,#247977),(#247978,#247979),(#247980,#247981),(#247982,#247983),
(#247984,#247985),(#247986,#247987),(#247988,#247989),(#247990,#247991),
(#247992,#247993),(#247994,#247995),(#247996,#247997),(#247998,#247999),
(#248000,#248001),(#248002,#248003),(#248004,#248005),(#248006,#248007),
(#248008,#248009),(#248010,#248011),(#248012,#248013),(#248014,#248015),
(#248016,#248017),(#248018,#248019),(#248020,#248021),(#248022,#248023),
(#248024,#248025),(#248026,#248027),(#248028,#248029),(#248030,#248031),
(#248032,#248033),(#248034,#248035),(#248036,#248037),(#248038,#248039),
(#248040,#248041),(#248042,#248043),(#248044,#248045),(#248046,#248047),
(#248048,#248049),(#248050,#248051),(#248052,#248053),(#248054,#248055),
(#248056,#248057),(#248058,#248059),(#248060,#248061),(#248062,#248063),
(#248064,#248065),(#248066,#248067),(#248068,#248069),(#248070,#248071),
(#248072,#248073),(#248074,#248075),(#248076,#248077),(#248078,#248079),
(#248080,#248081),(#248082,#248083),(#248084,#248085),(#248086,#248087),
(#248088,#248089),(#248090,#248091),(#248092,#248093),(#248094,#248095),
(#248096,#248097),(#248098,#248099),(#248100,#248101),(#248102,#248103),
(#248104,#248105),(#248106,#248107),(#248108,#248109),(#248110,#248111),
(#248112,#248113),(#248114,#248115),(#248116,#248117),(#248118,#248119),
(#248120,#248121),(#248122,#248123),(#248124,#248125),(#248126,#248127),
(#248128,#248129),(#248130,#248131),(#248132,#248133),(#248134,#248135),
(#248136,#248137),(#248138,#248139),(#248140,#248141),(#248142,#248143),
(#248144,#248145),(#248146,#248147),(#248148,#248149),(#248150,#248151),
(#248152,#248153),(#248154,#248155),(#248156,#248157),(#248158,#248159),
(#248160,#248161),(#248162,#248163),(#248164,#248165),(#248166,#248167),
(#248168,#248169),(#248170,#248171),(#248172,#248173),(#248174,#248175),
(#248176,#248177),(#248178,#248179),(#248180,#248181),(#248182,#248183),
(#248184,#248185),(#248186,#248187),(#248188,#248189),(#248190,#248191),
(#248192,#248193),(#248194,#248195),(#248196,#248197),(#248198,#248199),
(#248200,#248201),(#248202,#248203),(#248204,#248205),(#248206,#248207),
(#248208,#248209),(#248210,#248211),(#248212,#248213),(#248214,#248215),
(#248216,#248217),(#248218,#248219),(#248220,#248221),(#248222,#248223),
(#248224,#248225),(#248226,#248227),(#248228,#248229),(#248230,#248231),
(#248232,#248233),(#248234,#248235),(#248236,#248237),(#248238,#248239),
(#248240,#248241),(#248242,#248243),(#248244,#248245),(#248246,#248247),
(#248248,#248249),(#248250,#248251),(#248252,#248253),(#248254,#248255),
(#248256,#248257),(#248258,#248259),(#248260,#248261),(#248262,#248263),
(#248264,#248265),(#248266,#248267),(#248268,#248269),(#248270,#248271),
(#248272,#248273),(#248274,#248275),(#248276,#248277),(#248278,#248279),
(#248280,#248281),(#248282,#248283),(#248284,#248285),(#248286,#248287),
(#248288,#248289),(#248290,#248291),(#248292,#248293),(#248294,#248295),
(#248296,#248297),(#248298,#248299),(#248300,#248301),(#248302,#248303),
(#248304,#248305),(#248306,#248307),(#248308,#248309),(#248310,#248311),
(#248312,#248313),(#248314,#248315),(#248316,#248317),(#248318,#248319),
(#248320,#248321),(#248322,#248323),(#248324,#248325),(#248326,#248327),
(#248328,#248329),(#248330,#248331),(#248332,#248333),(#248334,#248335),
(#248336,#248337),(#248338,#248339),(#248340,#248341),(#248342,#248343),
(#248344,#248345),(#248346,#248347),(#248348,#248349),(#248350,#248351),
(#248352,#248353),(#248354,#248355),(#248356,#248357),(#248358,#248359),
(#248360,#248361),(#248362,#248363),(#248364,#248365),(#248366,#248367),
(#248368,#248369),(#248370,#248371),(#248372,#248373),(#248374,#248375),
(#248376,#248377),(#248378,#248379),(#248380,#248381),(#248382,#248383),
(#248384,#248385),(#248386,#248387),(#248388,#248389),(#248390,#248391),
(#248392,#248393),(#248394,#248395),(#248396,#248397),(#248398,#248399),
(#248400,#248401),(#248402,#248403),(#248404,#248405),(#248406,#248407),
(#248408,#248409),(#248410,#248411),(#248412,#248413),(#248414,#248415),
(#248416,#248417),(#248418,#248419),(#248420,#248421),(#248422,#248423),
(#248424,#248425),(#248426,#248427),(#248428,#248429),(#248430,#248431),
(#248432,#248433),(#248434,#248435),(#248436,#248437),(#248438,#248439),
(#248440,#248441),(#248442,#248443),(#248444,#248445),(#248446,#248447),
(#248448,#248449),(#248450,#248451),(#248452,#248453),(#248454,#248455),
(#248456,#248457),(#248458,#248459),(#248460,#248461),(#248462,#248463),
(#248464,#248465),(#248466,#248467),(#248468,#248469),(#248470,#248471),
(#248472,#248473),(#248474,#248475),(#248476,#248477),(#248478,#248479),
(#248480,#248481),(#248482,#248483),(#248484,#248485),(#248486,#248487),
(#248488,#248489),(#248490,#248491),(#248492,#248493),(#248494,#248495),
(#248496,#248497),(#248498,#248499),(#248500,#248501),(#248502,#248503),
(#248504,#248505),(#248506,#248507),(#248508,#248509),(#248510,#248511),
(#248512,#248513),(#248514,#248515),(#248516,#248517),(#248518,#248519),
(#248520,#248521),(#248522,#248523),(#248524,#248525),(#248526,#248527),
(#248528,#248529),(#248530,#248531),(#248532,#248533),(#248534,#248535),
(#248536,#248537),(#248538,#248539),(#248540,#248541),(#248542,#248543),
(#248544,#248545),(#248546,#248547),(#248548,#248549),(#248550,#248551),
(#248552,#248553),(#248554,#248555),(#248556,#248557),(#248558,#248559),
(#248560,#248561),(#248562,#248563),(#248564,#248565),(#248566,#248567),
(#248568,#248569),(#248570,#248571),(#248572,#248573),(#248574,#248575),
(#248576,#248577),(#248578,#248579),(#248580,#248581),(#248582,#248583),
(#248584,#248585),(#248586,#248587),(#248588,#248589),(#248590,#248591),
(#248592,#248593),(#248594,#248595),(#248596,#248597),(#248598,#248599),
(#248600,#248601),(#248602,#248603),(#248604,#248605),(#248606,#248607),
(#248608,#248609),(#248610,#248611),(#248612,#248613),(#248614,#248615),
(#248616,#248617),(#248618,#248619),(#248620,#248621),(#248622,#248623),
(#248624,#248625),(#248626,#248627),(#248628,#248629),(#248630,#248631),
(#248632,#248633),(#248634,#248635),(#248636,#248637),(#248638,#248639),
(#248640,#248641),(#248642,#248643),(#248644,#248645),(#248646,#248647),
(#248648,#248649),(#248650,#248651),(#248652,#248653),(#248654,#248655),
(#248656,#248657),(#248658,#248659),(#248660,#248661),(#248662,#248663),
(#248664,#248665),(#248666,#248667),(#248668,#248669),(#248670,#248671),
(#248672,#248673),(#248674,#248675),(#248676,#248677),(#248678,#248679),
(#248680,#248681),(#248682,#248683),(#248684,#248685),(#248686,#248687),
(#248688,#248689),(#248690,#248691),(#248692,#248693),(#248694,#248695),
(#248696,#248697),(#248698,#248699),(#248700,#248701),(#248702,#248703),
(#248704,#248705),(#248706,#248707),(#248708,#248709),(#248710,#248711),
(#248712,#248713),(#248714,#248715),(#248716,#248717),(#248718,#248719),
(#248720,#248721),(#248722,#248723),(#248724,#248725),(#248726,#248727),
(#248728,#248729),(#248730,#248731),(#248732,#248733),(#248734,#248735),
(#248736,#248737),(#248738,#248739),(#248740,#248741),(#248742,#248743),
(#248744,#248745),(#248746,#248747),(#248748,#248749),(#248750,#248751),
(#248752,#248753),(#248754,#248755),(#248756,#248757),(#248758,#248759),
(#248760,#248761),(#248762,#248763),(#248764,#248765),(#248766,#248767),
(#248768,#248769),(#248770,#248771),(#248772,#248773),(#248774,#248775),
(#248776,#248777),(#248778,#248779),(#248780,#248781),(#248782,#248783),
(#248784,#248785),(#248786,#248787)),.UNSPECIFIED.,.F.,.F.,.F.,(6,1,1,1,
1,1,1,1,1,1,1,1,1,1,1,1,1,1,1,1,1,1,1,1,1,1,1,1,1,1,1,1,1,1,1,1,1,1,1,1,
1,1,1,1,1,1,1,1,1,1,1,1,1,1,1,1,1,1,1,1,1,1,1,1,1,1,1,1,1,1,1,1,1,1,1,1,
1,1,1,1,1,1,1,1,1,1,1,1,1,1,1,1,1,1,1,1,1,1,1,1,1,1,1,1,1,1,1,1,1,1,1,1,
1,1,1,1,1,1,1,1,1,1,1,1,1,1,1,1,1,1,1,1,1,1,1,1,1,1,1,1,1,1,1,1,1,1,1,1,
1,1,1,1,1,1,1,1,1,1,1,1,1,1,1,1,1,1,1,1,1,1,1,1,1,1,1,1,1,1,1,1,1,1,1,1,
1,1,1,1,1,1,1,1,1,1,1,1,1,1,1,1,1,1,1,1,1,1,1,1,1,1,1,1,1,1,1,1,1,1,1,1,
1,1,1,1,1,1,1,1,1,1,1,1,1,1,1,1,1,1,1,1,1,1,1,1,1,1,1,1,1,1,1,1,1,1,1,1,
1,1,1,1,1,1,1,1,1,1,1,1,1,1,1,1,1,1,1,1,1,1,1,1,1,1,1,1,1,1,1,1,1,1,1,1,
1,1,1,1,1,1,1,1,1,1,1,1,1,1,1,1,1,1,1,1,1,1,1,1,1,1,1,1,1,1,1,1,1,1,1,1,
1,1,1,1,1,1,1,1,1,1,1,1,1,1,1,1,1,1,1,1,1,1,1,1,1,1,1,1,1,1,1,1,1,1,1,1,
1,1,1,1,1,1,1,1,1,1,1,1,1,1,1,1,1,1,1,1,1,1,1,1,1,1,1,1,1,1,1,1,1,1,1,1,
1,1,1,1,1,1,1,1,1,1,1,1,1,1,1,1,1,1,1,1,1,1,1,1,1,1,1,1,1,1,1,1,1,1,1,1,
1,1,1,1,1,1,1,1,1,1,1,1,1,1,1,1,1,1,1,1,1,1,1,1,1,1,1,1,1,1,1,6),(2,2),
(-1.,-0.998165138,-0.996330275,-0.994495413,-0.99266055,-0.990825688,-0.988990826,
-0.987155963,-0.985321101,-0.983486239,-0.981651376,-0.979816514,-0.977981651,
-0.976146789,-0.974311927,-0.972477064,-0.970642202,-0.968807339,-0.966972477,
-0.965137615,-0.963302752,-0.96146789,-0.959633028,-0.957798165,-0.955963303,
-0.95412844,-0.952293578,-0.950458716,-0.948623853,-0.946788991,-0.944954128,
-0.943119266,-0.941284404,-0.939449541,-0.937614679,-0.935779817,-0.933944954,
-0.932110092,-0.930275229,-0.928440367,-0.926605505,-0.924770642,-0.92293578,
-0.921100917,-0.919266055,-0.917431193,-0.91559633,-0.913761468,-0.911926606,
-0.910091743,-0.908256881,-0.906422018,-0.904587156,-0.902752294,-0.900917431,
-0.899082569,-0.897247706,-0.895412844,-0.893577982,-0.891743119,-0.889908257,
-0.888073394,-0.886238532,-0.88440367,-0.882568807,-0.880733945,-0.878899083,
-0.87706422,-0.875229358,-0.873394495,-0.871559633,-0.869724771,-0.867889908,
-0.866055046,-0.864220183,-0.862385321,-0.860550459,-0.858715596,-0.856880734,
-0.855045872,-0.853211009,-0.851376147,-0.849541284,-0.847706422,-0.84587156,
-0.844036697,-0.842201835,-0.840366972,-0.83853211,-0.836697248,-0.834862385,
-0.833027523,-0.831192661,-0.829357798,-0.827522936,-0.825688073,-0.823853211,
-0.822018349,-0.820183486,-0.818348624,-0.816513761,-0.814678899,-0.812844037,
-0.811009174,-0.809174312,-0.80733945,-0.805504587,-0.803669725,-0.801834862,
-0.8,-0.798165138,-0.796330275,-0.794495413,-0.79266055,-0.790825688,-0.788990826,
-0.787155963,-0.785321101,-0.783486239,-0.781651376,-0.779816514,-0.777981651,
-0.776146789,-0.774311927,-0.772477064,-0.770642202,-0.768807339,-0.766972477,
-0.765137615,-0.763302752,-0.76146789,-0.759633028,-0.757798165,-0.755963303,
-0.75412844,-0.752293578,-0.750458716,-0.748623853,-0.746788991,-0.744954128,
-0.743119266,-0.741284404,-0.739449541,-0.737614679,-0.735779817,-0.733944954,
-0.732110092,-0.730275229,-0.728440367,-0.726605505,-0.724770642,-0.72293578,
-0.721100917,-0.719266055,-0.717431193,-0.71559633,-0.713761468,-0.711926606,
-0.710091743,-0.708256881,-0.706422018,-0.704587156,-0.702752294,-0.700917431,
-0.699082569,-0.697247706,-0.695412844,-0.693577982,-0.691743119,-0.689908257,
-0.688073394,-0.686238532,-0.68440367,-0.682568807,-0.680733945,-0.678899083,
-0.67706422,-0.675229358,-0.673394495,-0.671559633,-0.669724771,-0.667889908,
-0.666055046,-0.664220183,-0.662385321,-0.660550459,-0.658715596,-0.656880734,
-0.655045872,-0.653211009,-0.651376147,-0.649541284,-0.647706422,-0.64587156,
-0.644036697,-0.642201835,-0.640366972,-0.63853211,-0.636697248,-0.634862385,
-0.633027523,-0.631192661,-0.629357798,-0.627522936,-0.625688073,-0.623853211,
-0.622018349,-0.620183486,-0.618348624,-0.616513761,-0.614678899,-0.612844037,
-0.611009174,-0.609174312,-0.60733945,-0.605504587,-0.603669725,-0.601834862,
-0.6,-0.598165138,-0.596330275,-0.594495413,-0.59266055,-0.590825688,-0.588990826,
-0.587155963,-0.585321101,-0.583486239,-0.581651376,-0.579816514,-0.577981651,
-0.576146789,-0.574311927,-0.572477064,-0.570642202,-0.568807339,-0.566972477,
-0.565137615,-0.563302752,-0.56146789,-0.559633028,-0.557798165,-0.555963303,
-0.55412844,-0.552293578,-0.550458716,-0.548623853,-0.546788991,-0.544954128,
-0.543119266,-0.541284404,-0.539449541,-0.537614679,-0.535779817,-0.533944954,
-0.532110092,-0.530275229,-0.528440367,-0.526605505,-0.524770642,-0.52293578,
-0.521100917,-0.519266055,-0.517431193,-0.51559633,-0.513761468,-0.511926606,
-0.510091743,-0.508256881,-0.506422018,-0.504587156,-0.502752294,-0.500917431,
-0.499082569,-0.497247706,-0.495412844,-0.493577982,-0.491743119,-0.489908257,
-0.488073394,-0.486238532,-0.48440367,-0.482568807,-0.480733945,-0.478899083,
-0.47706422,-0.475229358,-0.473394495,-0.471559633,-0.469724771,-0.467889908,
-0.466055046,-0.464220183,-0.462385321,-0.460550459,-0.458715596,-0.456880734,
-0.455045872,-0.453211009,-0.451376147,-0.449541284,-0.447706422,-0.44587156,
-0.444036697,-0.442201835,-0.440366972,-0.43853211,-0.436697248,-0.434862385,
-0.433027523,-0.431192661,-0.429357798,-0.427522936,-0.425688073,-0.423853211,
-0.422018349,-0.420183486,-0.418348624,-0.416513761,-0.414678899,-0.412844037,
-0.411009174,-0.409174312,-0.40733945,-0.405504587,-0.403669725,-0.401834862,
-0.4,-0.398165138,-0.396330275,-0.394495413,-0.39266055,-0.390825688,-0.388990826,
-0.387155963,-0.385321101,-0.383486239,-0.381651376,-0.379816514,-0.377981651,
-0.376146789,-0.374311927,-0.372477064,-0.370642202,-0.368807339,-0.366972477,
-0.365137615,-0.363302752,-0.36146789,-0.359633028,-0.357798165,-0.355963303,
-0.35412844,-0.352293578,-0.350458716,-0.348623853,-0.346788991,-0.344954128,
-0.343119266,-0.341284404,-0.339449541,-0.337614679,-0.335779817,-0.333944954,
-0.332110092,-0.330275229,-0.328440367,-0.326605505,-0.324770642,-0.32293578,
-0.321100917,-0.319266055,-0.317431193,-0.31559633,-0.313761468,-0.311926606,
-0.310091743,-0.308256881,-0.306422018,-0.304587156,-0.302752294,-0.300917431,
-0.299082569,-0.297247706,-0.295412844,-0.293577982,-0.291743119,-0.289908257,
-0.288073394,-0.286238532,-0.28440367,-0.282568807,-0.280733945,-0.278899083,
-0.27706422,-0.275229358,-0.273394495,-0.271559633,-0.269724771,-0.267889908,
-0.266055046,-0.264220183,-0.262385321,-0.260550459,-0.258715596,-0.256880734,
-0.255045872,-0.253211009,-0.251376147,-0.249541284,-0.247706422,-0.24587156,
-0.244036697,-0.242201835,-0.240366972,-0.23853211,-0.236697248,-0.234862385,
-0.233027523,-0.231192661,-0.229357798,-0.227522936,-0.225688073,-0.223853211,
-0.222018349,-0.220183486,-0.218348624,-0.216513761,-0.214678899,-0.212844037,
-0.211009174,-0.209174312,-0.20733945,-0.205504587,-0.203669725,-0.201834862,
-0.2,-0.198165138,-0.196330275,-0.194495413,-0.19266055,-0.190825688,-0.188990826,
-0.187155963,-0.185321101,-0.183486239,-0.181651376,-0.179816514,-0.177981651,
-0.176146789,-0.174311927,-0.172477064,-0.170642202,-0.168807339,-0.166972477,
-0.165137615,-0.163302752,-0.16146789,-0.159633028,-0.157798165,-0.155963303,
-0.15412844,-0.152293578,-0.150458716,-0.148623853,-0.146788991,-0.144954128,
-0.143172103),(0.,0.36),.UNSPECIFIED.);
#6273=B_SPLINE_SURFACE_WITH_KNOTS('',5,1,((#249438,#249439),(#249440,#249441),
(#249442,#249443),(#249444,#249445),(#249446,#249447),(#249448,#249449),
(#249450,#249451),(#249452,#249453),(#249454,#249455),(#249456,#249457),
(#249458,#249459),(#249460,#249461),(#249462,#249463),(#249464,#249465),
(#249466,#249467),(#249468,#249469),(#249470,#249471),(#249472,#249473),
(#249474,#249475),(#249476,#249477),(#249478,#249479),(#249480,#249481),
(#249482,#249483),(#249484,#249485),(#249486,#249487),(#249488,#249489),
(#249490,#249491),(#249492,#249493),(#249494,#249495),(#249496,#249497),
(#249498,#249499),(#249500,#249501),(#249502,#249503),(#249504,#249505),
(#249506,#249507),(#249508,#249509),(#249510,#249511),(#249512,#249513),
(#249514,#249515),(#249516,#249517),(#249518,#249519),(#249520,#249521),
(#249522,#249523),(#249524,#249525),(#249526,#249527),(#249528,#249529),
(#249530,#249531),(#249532,#249533),(#249534,#249535),(#249536,#249537),
(#249538,#249539),(#249540,#249541),(#249542,#249543),(#249544,#249545),
(#249546,#249547),(#249548,#249549),(#249550,#249551),(#249552,#249553),
(#249554,#249555),(#249556,#249557),(#249558,#249559),(#249560,#249561),
(#249562,#249563),(#249564,#249565),(#249566,#249567),(#249568,#249569),
(#249570,#249571),(#249572,#249573),(#249574,#249575),(#249576,#249577),
(#249578,#249579),(#249580,#249581),(#249582,#249583),(#249584,#249585),
(#249586,#249587),(#249588,#249589),(#249590,#249591),(#249592,#249593),
(#249594,#249595),(#249596,#249597),(#249598,#249599),(#249600,#249601),
(#249602,#249603),(#249604,#249605),(#249606,#249607),(#249608,#249609),
(#249610,#249611),(#249612,#249613),(#249614,#249615),(#249616,#249617),
(#249618,#249619),(#249620,#249621),(#249622,#249623),(#249624,#249625),
(#249626,#249627),(#249628,#249629),(#249630,#249631),(#249632,#249633),
(#249634,#249635),(#249636,#249637),(#249638,#249639),(#249640,#249641),
(#249642,#249643),(#249644,#249645),(#249646,#249647),(#249648,#249649),
(#249650,#249651),(#249652,#249653),(#249654,#249655),(#249656,#249657),
(#249658,#249659),(#249660,#249661),(#249662,#249663),(#249664,#249665),
(#249666,#249667),(#249668,#249669),(#249670,#249671),(#249672,#249673),
(#249674,#249675),(#249676,#249677),(#249678,#249679),(#249680,#249681),
(#249682,#249683),(#249684,#249685),(#249686,#249687),(#249688,#249689),
(#249690,#249691),(#249692,#249693),(#249694,#249695),(#249696,#249697),
(#249698,#249699),(#249700,#249701),(#249702,#249703),(#249704,#249705),
(#249706,#249707),(#249708,#249709),(#249710,#249711),(#249712,#249713),
(#249714,#249715),(#249716,#249717),(#249718,#249719),(#249720,#249721),
(#249722,#249723),(#249724,#249725),(#249726,#249727),(#249728,#249729),
(#249730,#249731),(#249732,#249733),(#249734,#249735),(#249736,#249737),
(#249738,#249739),(#249740,#249741),(#249742,#249743),(#249744,#249745),
(#249746,#249747),(#249748,#249749),(#249750,#249751),(#249752,#249753),
(#249754,#249755),(#249756,#249757),(#249758,#249759),(#249760,#249761),
(#249762,#249763),(#249764,#249765),(#249766,#249767),(#249768,#249769),
(#249770,#249771),(#249772,#249773),(#249774,#249775),(#249776,#249777),
(#249778,#249779),(#249780,#249781),(#249782,#249783),(#249784,#249785),
(#249786,#249787),(#249788,#249789),(#249790,#249791),(#249792,#249793),
(#249794,#249795),(#249796,#249797),(#249798,#249799),(#249800,#249801),
(#249802,#249803),(#249804,#249805),(#249806,#249807),(#249808,#249809),
(#249810,#249811),(#249812,#249813),(#249814,#249815),(#249816,#249817),
(#249818,#249819),(#249820,#249821),(#249822,#249823),(#249824,#249825),
(#249826,#249827),(#249828,#249829),(#249830,#249831),(#249832,#249833),
(#249834,#249835),(#249836,#249837),(#249838,#249839),(#249840,#249841),
(#249842,#249843),(#249844,#249845),(#249846,#249847),(#249848,#249849),
(#249850,#249851),(#249852,#249853),(#249854,#249855),(#249856,#249857),
(#249858,#249859),(#249860,#249861),(#249862,#249863),(#249864,#249865),
(#249866,#249867),(#249868,#249869),(#249870,#249871),(#249872,#249873),
(#249874,#249875),(#249876,#249877),(#249878,#249879),(#249880,#249881),
(#249882,#249883),(#249884,#249885),(#249886,#249887),(#249888,#249889),
(#249890,#249891),(#249892,#249893),(#249894,#249895),(#249896,#249897),
(#249898,#249899),(#249900,#249901),(#249902,#249903),(#249904,#249905),
(#249906,#249907),(#249908,#249909),(#249910,#249911),(#249912,#249913),
(#249914,#249915),(#249916,#249917),(#249918,#249919),(#249920,#249921),
(#249922,#249923),(#249924,#249925),(#249926,#249927),(#249928,#249929),
(#249930,#249931),(#249932,#249933),(#249934,#249935),(#249936,#249937),
(#249938,#249939),(#249940,#249941),(#249942,#249943),(#249944,#249945),
(#249946,#249947),(#249948,#249949),(#249950,#249951),(#249952,#249953),
(#249954,#249955),(#249956,#249957),(#249958,#249959),(#249960,#249961),
(#249962,#249963),(#249964,#249965),(#249966,#249967),(#249968,#249969),
(#249970,#249971),(#249972,#249973),(#249974,#249975),(#249976,#249977),
(#249978,#249979),(#249980,#249981),(#249982,#249983),(#249984,#249985),
(#249986,#249987),(#249988,#249989),(#249990,#249991),(#249992,#249993),
(#249994,#249995),(#249996,#249997),(#249998,#249999),(#250000,#250001),
(#250002,#250003),(#250004,#250005),(#250006,#250007),(#250008,#250009),
(#250010,#250011),(#250012,#250013),(#250014,#250015),(#250016,#250017),
(#250018,#250019),(#250020,#250021),(#250022,#250023),(#250024,#250025),
(#250026,#250027),(#250028,#250029),(#250030,#250031),(#250032,#250033),
(#250034,#250035),(#250036,#250037),(#250038,#250039),(#250040,#250041),
(#250042,#250043),(#250044,#250045),(#250046,#250047),(#250048,#250049),
(#250050,#250051),(#250052,#250053),(#250054,#250055),(#250056,#250057),
(#250058,#250059),(#250060,#250061),(#250062,#250063),(#250064,#250065),
(#250066,#250067),(#250068,#250069),(#250070,#250071),(#250072,#250073),
(#250074,#250075),(#250076,#250077),(#250078,#250079),(#250080,#250081),
(#250082,#250083),(#250084,#250085),(#250086,#250087),(#250088,#250089),
(#250090,#250091),(#250092,#250093),(#250094,#250095),(#250096,#250097),
(#250098,#250099),(#250100,#250101),(#250102,#250103),(#250104,#250105),
(#250106,#250107),(#250108,#250109),(#250110,#250111),(#250112,#250113),
(#250114,#250115),(#250116,#250117),(#250118,#250119),(#250120,#250121),
(#250122,#250123),(#250124,#250125),(#250126,#250127),(#250128,#250129),
(#250130,#250131),(#250132,#250133),(#250134,#250135),(#250136,#250137),
(#250138,#250139),(#250140,#250141),(#250142,#250143),(#250144,#250145),
(#250146,#250147),(#250148,#250149),(#250150,#250151),(#250152,#250153),
(#250154,#250155),(#250156,#250157),(#250158,#250159),(#250160,#250161),
(#250162,#250163),(#250164,#250165),(#250166,#250167),(#250168,#250169),
(#250170,#250171),(#250172,#250173),(#250174,#250175),(#250176,#250177),
(#250178,#250179),(#250180,#250181),(#250182,#250183),(#250184,#250185),
(#250186,#250187),(#250188,#250189),(#250190,#250191),(#250192,#250193),
(#250194,#250195),(#250196,#250197),(#250198,#250199),(#250200,#250201),
(#250202,#250203),(#250204,#250205),(#250206,#250207),(#250208,#250209),
(#250210,#250211),(#250212,#250213),(#250214,#250215),(#250216,#250217),
(#250218,#250219),(#250220,#250221),(#250222,#250223),(#250224,#250225),
(#250226,#250227),(#250228,#250229),(#250230,#250231),(#250232,#250233),
(#250234,#250235),(#250236,#250237),(#250238,#250239),(#250240,#250241),
(#250242,#250243),(#250244,#250245),(#250246,#250247),(#250248,#250249),
(#250250,#250251),(#250252,#250253),(#250254,#250255),(#250256,#250257),
(#250258,#250259),(#250260,#250261),(#250262,#250263),(#250264,#250265),
(#250266,#250267),(#250268,#250269),(#250270,#250271),(#250272,#250273),
(#250274,#250275),(#250276,#250277),(#250278,#250279),(#250280,#250281),
(#250282,#250283),(#250284,#250285),(#250286,#250287),(#250288,#250289),
(#250290,#250291),(#250292,#250293),(#250294,#250295),(#250296,#250297),
(#250298,#250299),(#250300,#250301),(#250302,#250303),(#250304,#250305),
(#250306,#250307),(#250308,#250309),(#250310,#250311),(#250312,#250313),
(#250314,#250315),(#250316,#250317),(#250318,#250319),(#250320,#250321),
(#250322,#250323),(#250324,#250325),(#250326,#250327),(#250328,#250329),
(#250330,#250331),(#250332,#250333),(#250334,#250335),(#250336,#250337),
(#250338,#250339),(#250340,#250341),(#250342,#250343),(#250344,#250345),
(#250346,#250347),(#250348,#250349),(#250350,#250351),(#250352,#250353),
(#250354,#250355),(#250356,#250357),(#250358,#250359),(#250360,#250361),
(#250362,#250363),(#250364,#250365),(#250366,#250367),(#250368,#250369),
(#250370,#250371),(#250372,#250373),(#250374,#250375),(#250376,#250377),
(#250378,#250379),(#250380,#250381)),.UNSPECIFIED.,.F.,.F.,.F.,(6,1,1,1,
1,1,1,1,1,1,1,1,1,1,1,1,1,1,1,1,1,1,1,1,1,1,1,1,1,1,1,1,1,1,1,1,1,1,1,1,
1,1,1,1,1,1,1,1,1,1,1,1,1,1,1,1,1,1,1,1,1,1,1,1,1,1,1,1,1,1,1,1,1,1,1,1,
1,1,1,1,1,1,1,1,1,1,1,1,1,1,1,1,1,1,1,1,1,1,1,1,1,1,1,1,1,1,1,1,1,1,1,1,
1,1,1,1,1,1,1,1,1,1,1,1,1,1,1,1,1,1,1,1,1,1,1,1,1,1,1,1,1,1,1,1,1,1,1,1,
1,1,1,1,1,1,1,1,1,1,1,1,1,1,1,1,1,1,1,1,1,1,1,1,1,1,1,1,1,1,1,1,1,1,1,1,
1,1,1,1,1,1,1,1,1,1,1,1,1,1,1,1,1,1,1,1,1,1,1,1,1,1,1,1,1,1,1,1,1,1,1,1,
1,1,1,1,1,1,1,1,1,1,1,1,1,1,1,1,1,1,1,1,1,1,1,1,1,1,1,1,1,1,1,1,1,1,1,1,
1,1,1,1,1,1,1,1,1,1,1,1,1,1,1,1,1,1,1,1,1,1,1,1,1,1,1,1,1,1,1,1,1,1,1,1,
1,1,1,1,1,1,1,1,1,1,1,1,1,1,1,1,1,1,1,1,1,1,1,1,1,1,1,1,1,1,1,1,1,1,1,1,
1,1,1,1,1,1,1,1,1,1,1,1,1,1,1,1,1,1,1,1,1,1,1,1,1,1,1,1,1,1,1,1,1,1,1,1,
1,1,1,1,1,1,1,1,1,1,1,1,1,1,1,1,1,1,1,1,1,1,1,1,1,1,1,1,1,1,1,1,1,1,1,1,
1,1,1,1,1,1,1,1,1,1,1,1,1,1,1,1,1,1,1,1,1,1,1,1,1,1,1,1,1,1,1,1,1,1,1,1,
1,1,1,1,1,1,1,1,1,1,1,1,1,1,1,1,1,1,1,1,1,1,1,1,1,1,1,1,1,1,1,6),(2,2),
(-1.,-0.998165138,-0.996330275,-0.994495413,-0.99266055,-0.990825688,-0.988990826,
-0.987155963,-0.985321101,-0.983486239,-0.981651376,-0.979816514,-0.977981651,
-0.976146789,-0.974311927,-0.972477064,-0.970642202,-0.968807339,-0.966972477,
-0.965137615,-0.963302752,-0.96146789,-0.959633028,-0.957798165,-0.955963303,
-0.95412844,-0.952293578,-0.950458716,-0.948623853,-0.946788991,-0.944954128,
-0.943119266,-0.941284404,-0.939449541,-0.937614679,-0.935779817,-0.933944954,
-0.932110092,-0.930275229,-0.928440367,-0.926605505,-0.924770642,-0.92293578,
-0.921100917,-0.919266055,-0.917431193,-0.91559633,-0.913761468,-0.911926606,
-0.910091743,-0.908256881,-0.906422018,-0.904587156,-0.902752294,-0.900917431,
-0.899082569,-0.897247706,-0.895412844,-0.893577982,-0.891743119,-0.889908257,
-0.888073394,-0.886238532,-0.88440367,-0.882568807,-0.880733945,-0.878899083,
-0.87706422,-0.875229358,-0.873394495,-0.871559633,-0.869724771,-0.867889908,
-0.866055046,-0.864220183,-0.862385321,-0.860550459,-0.858715596,-0.856880734,
-0.855045872,-0.853211009,-0.851376147,-0.849541284,-0.847706422,-0.84587156,
-0.844036697,-0.842201835,-0.840366972,-0.83853211,-0.836697248,-0.834862385,
-0.833027523,-0.831192661,-0.829357798,-0.827522936,-0.825688073,-0.823853211,
-0.822018349,-0.820183486,-0.818348624,-0.816513761,-0.814678899,-0.812844037,
-0.811009174,-0.809174312,-0.80733945,-0.805504587,-0.803669725,-0.801834862,
-0.8,-0.798165138,-0.796330275,-0.794495413,-0.79266055,-0.790825688,-0.788990826,
-0.787155963,-0.785321101,-0.783486239,-0.781651376,-0.779816514,-0.777981651,
-0.776146789,-0.774311927,-0.772477064,-0.770642202,-0.768807339,-0.766972477,
-0.765137615,-0.763302752,-0.76146789,-0.759633028,-0.757798165,-0.755963303,
-0.75412844,-0.752293578,-0.750458716,-0.748623853,-0.746788991,-0.744954128,
-0.743119266,-0.741284404,-0.739449541,-0.737614679,-0.735779817,-0.733944954,
-0.732110092,-0.730275229,-0.728440367,-0.726605505,-0.724770642,-0.72293578,
-0.721100917,-0.719266055,-0.717431193,-0.71559633,-0.713761468,-0.711926606,
-0.710091743,-0.708256881,-0.706422018,-0.704587156,-0.702752294,-0.700917431,
-0.699082569,-0.697247706,-0.695412844,-0.693577982,-0.691743119,-0.689908257,
-0.688073394,-0.686238532,-0.68440367,-0.682568807,-0.680733945,-0.678899083,
-0.67706422,-0.675229358,-0.673394495,-0.671559633,-0.669724771,-0.667889908,
-0.666055046,-0.664220183,-0.662385321,-0.660550459,-0.658715596,-0.656880734,
-0.655045872,-0.653211009,-0.651376147,-0.649541284,-0.647706422,-0.64587156,
-0.644036697,-0.642201835,-0.640366972,-0.63853211,-0.636697248,-0.634862385,
-0.633027523,-0.631192661,-0.629357798,-0.627522936,-0.625688073,-0.623853211,
-0.622018349,-0.620183486,-0.618348624,-0.616513761,-0.614678899,-0.612844037,
-0.611009174,-0.609174312,-0.60733945,-0.605504587,-0.603669725,-0.601834862,
-0.6,-0.598165138,-0.596330275,-0.594495413,-0.59266055,-0.590825688,-0.588990826,
-0.587155963,-0.585321101,-0.583486239,-0.581651376,-0.579816514,-0.577981651,
-0.576146789,-0.574311927,-0.572477064,-0.570642202,-0.568807339,-0.566972477,
-0.565137615,-0.563302752,-0.56146789,-0.559633028,-0.557798165,-0.555963303,
-0.55412844,-0.552293578,-0.550458716,-0.548623853,-0.546788991,-0.544954128,
-0.543119266,-0.541284404,-0.539449541,-0.537614679,-0.535779817,-0.533944954,
-0.532110092,-0.530275229,-0.528440367,-0.526605505,-0.524770642,-0.52293578,
-0.521100917,-0.519266055,-0.517431193,-0.51559633,-0.513761468,-0.511926606,
-0.510091743,-0.508256881,-0.506422018,-0.504587156,-0.502752294,-0.500917431,
-0.499082569,-0.497247706,-0.495412844,-0.493577982,-0.491743119,-0.489908257,
-0.488073394,-0.486238532,-0.48440367,-0.482568807,-0.480733945,-0.478899083,
-0.47706422,-0.475229358,-0.473394495,-0.471559633,-0.469724771,-0.467889908,
-0.466055046,-0.464220183,-0.462385321,-0.460550459,-0.458715596,-0.456880734,
-0.455045872,-0.453211009,-0.451376147,-0.449541284,-0.447706422,-0.44587156,
-0.444036697,-0.442201835,-0.440366972,-0.43853211,-0.436697248,-0.434862385,
-0.433027523,-0.431192661,-0.429357798,-0.427522936,-0.425688073,-0.423853211,
-0.422018349,-0.420183486,-0.418348624,-0.416513761,-0.414678899,-0.412844037,
-0.411009174,-0.409174312,-0.40733945,-0.405504587,-0.403669725,-0.401834862,
-0.4,-0.398165138,-0.396330275,-0.394495413,-0.39266055,-0.390825688,-0.388990826,
-0.387155963,-0.385321101,-0.383486239,-0.381651376,-0.379816514,-0.377981651,
-0.376146789,-0.374311927,-0.372477064,-0.370642202,-0.368807339,-0.366972477,
-0.365137615,-0.363302752,-0.36146789,-0.359633028,-0.357798165,-0.355963303,
-0.35412844,-0.352293578,-0.350458716,-0.348623853,-0.346788991,-0.344954128,
-0.343119266,-0.341284404,-0.339449541,-0.337614679,-0.335779817,-0.333944954,
-0.332110092,-0.330275229,-0.328440367,-0.326605505,-0.324770642,-0.32293578,
-0.321100917,-0.319266055,-0.317431193,-0.31559633,-0.313761468,-0.311926606,
-0.310091743,-0.308256881,-0.306422018,-0.304587156,-0.302752294,-0.300917431,
-0.299082569,-0.297247706,-0.295412844,-0.293577982,-0.291743119,-0.289908257,
-0.288073394,-0.286238532,-0.28440367,-0.282568807,-0.280733945,-0.278899083,
-0.27706422,-0.275229358,-0.273394495,-0.271559633,-0.269724771,-0.267889908,
-0.266055046,-0.264220183,-0.262385321,-0.260550459,-0.258715596,-0.256880734,
-0.255045872,-0.253211009,-0.251376147,-0.249541284,-0.247706422,-0.24587156,
-0.244036697,-0.242201835,-0.240366972,-0.23853211,-0.236697248,-0.234862385,
-0.233027523,-0.231192661,-0.229357798,-0.227522936,-0.225688073,-0.223853211,
-0.222018349,-0.220183486,-0.218348624,-0.216513761,-0.214678899,-0.212844037,
-0.211009174,-0.209174312,-0.20733945,-0.205504587,-0.203669725,-0.201834862,
-0.2,-0.198165138,-0.196330275,-0.194495413,-0.19266055,-0.190825688,-0.188990826,
-0.187155963,-0.185321101,-0.183486239,-0.181651376,-0.179816514,-0.177981651,
-0.176146789,-0.174311927,-0.172477064,-0.170642202,-0.168807339,-0.166972477,
-0.165137615,-0.163302752,-0.16146789,-0.159633028,-0.157798165,-0.155963303,
-0.15412844,-0.152293578,-0.150458716,-0.148623853,-0.146788991,-0.144954128,
-0.143172103),(0.,0.36),.UNSPECIFIED.);
#6274=B_SPLINE_SURFACE_WITH_KNOTS('',5,1,((#251023,#251024),(#251025,#251026),
(#251027,#251028),(#251029,#251030),(#251031,#251032),(#251033,#251034),
(#251035,#251036),(#251037,#251038),(#251039,#251040),(#251041,#251042),
(#251043,#251044),(#251045,#251046),(#251047,#251048),(#251049,#251050),
(#251051,#251052),(#251053,#251054),(#251055,#251056),(#251057,#251058),
(#251059,#251060),(#251061,#251062),(#251063,#251064),(#251065,#251066),
(#251067,#251068),(#251069,#251070),(#251071,#251072),(#251073,#251074),
(#251075,#251076),(#251077,#251078),(#251079,#251080),(#251081,#251082),
(#251083,#251084),(#251085,#251086),(#251087,#251088),(#251089,#251090),
(#251091,#251092),(#251093,#251094),(#251095,#251096),(#251097,#251098),
(#251099,#251100),(#251101,#251102),(#251103,#251104),(#251105,#251106),
(#251107,#251108),(#251109,#251110),(#251111,#251112),(#251113,#251114),
(#251115,#251116),(#251117,#251118),(#251119,#251120),(#251121,#251122),
(#251123,#251124),(#251125,#251126),(#251127,#251128),(#251129,#251130),
(#251131,#251132),(#251133,#251134),(#251135,#251136),(#251137,#251138),
(#251139,#251140),(#251141,#251142),(#251143,#251144),(#251145,#251146),
(#251147,#251148),(#251149,#251150),(#251151,#251152),(#251153,#251154),
(#251155,#251156),(#251157,#251158),(#251159,#251160),(#251161,#251162),
(#251163,#251164),(#251165,#251166),(#251167,#251168),(#251169,#251170),
(#251171,#251172),(#251173,#251174),(#251175,#251176),(#251177,#251178),
(#251179,#251180),(#251181,#251182),(#251183,#251184),(#251185,#251186),
(#251187,#251188),(#251189,#251190),(#251191,#251192),(#251193,#251194),
(#251195,#251196),(#251197,#251198),(#251199,#251200),(#251201,#251202),
(#251203,#251204),(#251205,#251206),(#251207,#251208),(#251209,#251210),
(#251211,#251212),(#251213,#251214),(#251215,#251216),(#251217,#251218),
(#251219,#251220),(#251221,#251222),(#251223,#251224),(#251225,#251226),
(#251227,#251228),(#251229,#251230),(#251231,#251232),(#251233,#251234),
(#251235,#251236),(#251237,#251238),(#251239,#251240),(#251241,#251242),
(#251243,#251244),(#251245,#251246),(#251247,#251248),(#251249,#251250),
(#251251,#251252),(#251253,#251254),(#251255,#251256),(#251257,#251258),
(#251259,#251260),(#251261,#251262),(#251263,#251264),(#251265,#251266),
(#251267,#251268),(#251269,#251270),(#251271,#251272),(#251273,#251274),
(#251275,#251276),(#251277,#251278),(#251279,#251280),(#251281,#251282),
(#251283,#251284),(#251285,#251286),(#251287,#251288),(#251289,#251290),
(#251291,#251292),(#251293,#251294),(#251295,#251296),(#251297,#251298),
(#251299,#251300),(#251301,#251302),(#251303,#251304),(#251305,#251306),
(#251307,#251308),(#251309,#251310),(#251311,#251312),(#251313,#251314),
(#251315,#251316),(#251317,#251318),(#251319,#251320),(#251321,#251322),
(#251323,#251324),(#251325,#251326),(#251327,#251328),(#251329,#251330),
(#251331,#251332),(#251333,#251334),(#251335,#251336),(#251337,#251338),
(#251339,#251340),(#251341,#251342),(#251343,#251344),(#251345,#251346),
(#251347,#251348),(#251349,#251350),(#251351,#251352),(#251353,#251354),
(#251355,#251356),(#251357,#251358),(#251359,#251360),(#251361,#251362),
(#251363,#251364),(#251365,#251366),(#251367,#251368),(#251369,#251370),
(#251371,#251372),(#251373,#251374),(#251375,#251376),(#251377,#251378),
(#251379,#251380),(#251381,#251382),(#251383,#251384),(#251385,#251386),
(#251387,#251388),(#251389,#251390),(#251391,#251392),(#251393,#251394),
(#251395,#251396),(#251397,#251398),(#251399,#251400),(#251401,#251402),
(#251403,#251404),(#251405,#251406),(#251407,#251408),(#251409,#251410),
(#251411,#251412),(#251413,#251414),(#251415,#251416),(#251417,#251418),
(#251419,#251420),(#251421,#251422),(#251423,#251424),(#251425,#251426),
(#251427,#251428),(#251429,#251430),(#251431,#251432),(#251433,#251434),
(#251435,#251436),(#251437,#251438),(#251439,#251440),(#251441,#251442),
(#251443,#251444),(#251445,#251446),(#251447,#251448),(#251449,#251450),
(#251451,#251452),(#251453,#251454),(#251455,#251456),(#251457,#251458),
(#251459,#251460),(#251461,#251462),(#251463,#251464),(#251465,#251466),
(#251467,#251468),(#251469,#251470),(#251471,#251472),(#251473,#251474),
(#251475,#251476),(#251477,#251478),(#251479,#251480),(#251481,#251482),
(#251483,#251484),(#251485,#251486),(#251487,#251488),(#251489,#251490),
(#251491,#251492),(#251493,#251494),(#251495,#251496),(#251497,#251498),
(#251499,#251500),(#251501,#251502),(#251503,#251504),(#251505,#251506),
(#251507,#251508),(#251509,#251510),(#251511,#251512),(#251513,#251514),
(#251515,#251516),(#251517,#251518),(#251519,#251520),(#251521,#251522),
(#251523,#251524),(#251525,#251526),(#251527,#251528),(#251529,#251530),
(#251531,#251532),(#251533,#251534),(#251535,#251536),(#251537,#251538),
(#251539,#251540),(#251541,#251542),(#251543,#251544),(#251545,#251546),
(#251547,#251548),(#251549,#251550),(#251551,#251552),(#251553,#251554),
(#251555,#251556),(#251557,#251558),(#251559,#251560),(#251561,#251562),
(#251563,#251564),(#251565,#251566),(#251567,#251568),(#251569,#251570),
(#251571,#251572),(#251573,#251574),(#251575,#251576),(#251577,#251578),
(#251579,#251580),(#251581,#251582),(#251583,#251584),(#251585,#251586),
(#251587,#251588),(#251589,#251590),(#251591,#251592),(#251593,#251594),
(#251595,#251596),(#251597,#251598),(#251599,#251600),(#251601,#251602),
(#251603,#251604),(#251605,#251606),(#251607,#251608),(#251609,#251610),
(#251611,#251612),(#251613,#251614),(#251615,#251616),(#251617,#251618),
(#251619,#251620),(#251621,#251622),(#251623,#251624),(#251625,#251626),
(#251627,#251628),(#251629,#251630),(#251631,#251632),(#251633,#251634),
(#251635,#251636),(#251637,#251638),(#251639,#251640),(#251641,#251642),
(#251643,#251644),(#251645,#251646),(#251647,#251648),(#251649,#251650),
(#251651,#251652),(#251653,#251654),(#251655,#251656),(#251657,#251658),
(#251659,#251660),(#251661,#251662),(#251663,#251664),(#251665,#251666),
(#251667,#251668),(#251669,#251670),(#251671,#251672),(#251673,#251674),
(#251675,#251676),(#251677,#251678),(#251679,#251680),(#251681,#251682),
(#251683,#251684),(#251685,#251686),(#251687,#251688),(#251689,#251690),
(#251691,#251692),(#251693,#251694),(#251695,#251696),(#251697,#251698),
(#251699,#251700),(#251701,#251702),(#251703,#251704),(#251705,#251706),
(#251707,#251708),(#251709,#251710),(#251711,#251712),(#251713,#251714),
(#251715,#251716),(#251717,#251718),(#251719,#251720),(#251721,#251722),
(#251723,#251724),(#251725,#251726),(#251727,#251728),(#251729,#251730),
(#251731,#251732),(#251733,#251734),(#251735,#251736),(#251737,#251738),
(#251739,#251740),(#251741,#251742),(#251743,#251744),(#251745,#251746),
(#251747,#251748),(#251749,#251750),(#251751,#251752),(#251753,#251754),
(#251755,#251756),(#251757,#251758),(#251759,#251760),(#251761,#251762),
(#251763,#251764),(#251765,#251766),(#251767,#251768),(#251769,#251770),
(#251771,#251772),(#251773,#251774),(#251775,#251776),(#251777,#251778),
(#251779,#251780),(#251781,#251782),(#251783,#251784),(#251785,#251786),
(#251787,#251788),(#251789,#251790),(#251791,#251792),(#251793,#251794),
(#251795,#251796),(#251797,#251798),(#251799,#251800),(#251801,#251802),
(#251803,#251804),(#251805,#251806),(#251807,#251808),(#251809,#251810),
(#251811,#251812),(#251813,#251814),(#251815,#251816),(#251817,#251818),
(#251819,#251820),(#251821,#251822),(#251823,#251824),(#251825,#251826),
(#251827,#251828),(#251829,#251830),(#251831,#251832),(#251833,#251834),
(#251835,#251836),(#251837,#251838),(#251839,#251840),(#251841,#251842),
(#251843,#251844),(#251845,#251846),(#251847,#251848),(#251849,#251850),
(#251851,#251852),(#251853,#251854),(#251855,#251856),(#251857,#251858),
(#251859,#251860),(#251861,#251862),(#251863,#251864),(#251865,#251866),
(#251867,#251868),(#251869,#251870),(#251871,#251872),(#251873,#251874),
(#251875,#251876),(#251877,#251878),(#251879,#251880),(#251881,#251882),
(#251883,#251884),(#251885,#251886),(#251887,#251888),(#251889,#251890),
(#251891,#251892),(#251893,#251894),(#251895,#251896),(#251897,#251898),
(#251899,#251900),(#251901,#251902),(#251903,#251904),(#251905,#251906),
(#251907,#251908),(#251909,#251910),(#251911,#251912),(#251913,#251914),
(#251915,#251916),(#251917,#251918),(#251919,#251920),(#251921,#251922),
(#251923,#251924),(#251925,#251926),(#251927,#251928),(#251929,#251930),
(#251931,#251932),(#251933,#251934),(#251935,#251936),(#251937,#251938),
(#251939,#251940),(#251941,#251942),(#251943,#251944),(#251945,#251946),
(#251947,#251948),(#251949,#251950),(#251951,#251952),(#251953,#251954),
(#251955,#251956),(#251957,#251958),(#251959,#251960),(#251961,#251962),
(#251963,#251964),(#251965,#251966)),.UNSPECIFIED.,.F.,.F.,.F.,(6,1,1,1,
1,1,1,1,1,1,1,1,1,1,1,1,1,1,1,1,1,1,1,1,1,1,1,1,1,1,1,1,1,1,1,1,1,1,1,1,
1,1,1,1,1,1,1,1,1,1,1,1,1,1,1,1,1,1,1,1,1,1,1,1,1,1,1,1,1,1,1,1,1,1,1,1,
1,1,1,1,1,1,1,1,1,1,1,1,1,1,1,1,1,1,1,1,1,1,1,1,1,1,1,1,1,1,1,1,1,1,1,1,
1,1,1,1,1,1,1,1,1,1,1,1,1,1,1,1,1,1,1,1,1,1,1,1,1,1,1,1,1,1,1,1,1,1,1,1,
1,1,1,1,1,1,1,1,1,1,1,1,1,1,1,1,1,1,1,1,1,1,1,1,1,1,1,1,1,1,1,1,1,1,1,1,
1,1,1,1,1,1,1,1,1,1,1,1,1,1,1,1,1,1,1,1,1,1,1,1,1,1,1,1,1,1,1,1,1,1,1,1,
1,1,1,1,1,1,1,1,1,1,1,1,1,1,1,1,1,1,1,1,1,1,1,1,1,1,1,1,1,1,1,1,1,1,1,1,
1,1,1,1,1,1,1,1,1,1,1,1,1,1,1,1,1,1,1,1,1,1,1,1,1,1,1,1,1,1,1,1,1,1,1,1,
1,1,1,1,1,1,1,1,1,1,1,1,1,1,1,1,1,1,1,1,1,1,1,1,1,1,1,1,1,1,1,1,1,1,1,1,
1,1,1,1,1,1,1,1,1,1,1,1,1,1,1,1,1,1,1,1,1,1,1,1,1,1,1,1,1,1,1,1,1,1,1,1,
1,1,1,1,1,1,1,1,1,1,1,1,1,1,1,1,1,1,1,1,1,1,1,1,1,1,1,1,1,1,1,1,1,1,1,1,
1,1,1,1,1,1,1,1,1,1,1,1,1,1,1,1,1,1,1,1,1,1,1,1,1,1,1,1,1,1,1,1,1,1,1,1,
1,1,1,1,1,1,1,1,1,1,1,1,1,1,1,1,1,1,1,1,1,1,1,1,1,1,1,1,1,1,1,6),(2,2),
(0.143172104,0.144954128,0.146788991,0.148623853,0.150458716,0.152293578,
0.15412844,0.155963303,0.157798165,0.159633028,0.16146789,0.163302752,0.165137615,
0.166972477,0.168807339,0.170642202,0.172477064,0.174311927,0.176146789,
0.177981651,0.179816514,0.181651376,0.183486239,0.185321101,0.187155963,
0.188990826,0.190825688,0.19266055,0.194495413,0.196330275,0.198165138,
0.2,0.201834862,0.203669725,0.205504587,0.20733945,0.209174312,0.211009174,
0.212844037,0.214678899,0.216513761,0.218348624,0.220183486,0.222018349,
0.223853211,0.225688073,0.227522936,0.229357798,0.231192661,0.233027523,
0.234862385,0.236697248,0.23853211,0.240366972,0.242201835,0.244036697,
0.24587156,0.247706422,0.249541284,0.251376147,0.253211009,0.255045872,
0.256880734,0.258715596,0.260550459,0.262385321,0.264220183,0.266055046,
0.267889908,0.269724771,0.271559633,0.273394495,0.275229358,0.27706422,
0.278899083,0.280733945,0.282568807,0.28440367,0.286238532,0.288073394,
0.289908257,0.291743119,0.293577982,0.295412844,0.297247706,0.299082569,
0.300917431,0.302752294,0.304587156,0.306422018,0.308256881,0.310091743,
0.311926606,0.313761468,0.31559633,0.317431193,0.319266055,0.321100917,
0.32293578,0.324770642,0.326605505,0.328440367,0.330275229,0.332110092,
0.333944954,0.335779817,0.337614679,0.339449541,0.341284404,0.343119266,
0.344954128,0.346788991,0.348623853,0.350458716,0.352293578,0.35412844,
0.355963303,0.357798165,0.359633028,0.36146789,0.363302752,0.365137615,
0.366972477,0.368807339,0.370642202,0.372477064,0.374311927,0.376146789,
0.377981651,0.379816514,0.381651376,0.383486239,0.385321101,0.387155963,
0.388990826,0.390825688,0.39266055,0.394495413,0.396330275,0.398165138,
0.4,0.401834862,0.403669725,0.405504587,0.40733945,0.409174312,0.411009174,
0.412844037,0.414678899,0.416513761,0.418348624,0.420183486,0.422018349,
0.423853211,0.425688073,0.427522936,0.429357798,0.431192661,0.433027523,
0.434862385,0.436697248,0.43853211,0.440366972,0.442201835,0.444036697,
0.44587156,0.447706422,0.449541284,0.451376147,0.453211009,0.455045872,
0.456880734,0.458715596,0.460550459,0.462385321,0.464220183,0.466055046,
0.467889908,0.469724771,0.471559633,0.473394495,0.475229358,0.47706422,
0.478899083,0.480733945,0.482568807,0.48440367,0.486238532,0.488073394,
0.489908257,0.491743119,0.493577982,0.495412844,0.497247706,0.499082569,
0.500917431,0.502752294,0.504587156,0.506422018,0.508256881,0.510091743,
0.511926606,0.513761468,0.51559633,0.517431193,0.519266055,0.521100917,
0.52293578,0.524770642,0.526605505,0.528440367,0.530275229,0.532110092,
0.533944954,0.535779817,0.537614679,0.539449541,0.541284404,0.543119266,
0.544954128,0.546788991,0.548623853,0.550458716,0.552293578,0.55412844,
0.555963303,0.557798165,0.559633028,0.56146789,0.563302752,0.565137615,
0.566972477,0.568807339,0.570642202,0.572477064,0.574311927,0.576146789,
0.577981651,0.579816514,0.581651376,0.583486239,0.585321101,0.587155963,
0.588990826,0.590825688,0.59266055,0.594495413,0.596330275,0.598165138,
0.6,0.601834862,0.603669725,0.605504587,0.60733945,0.609174312,0.611009174,
0.612844037,0.614678899,0.616513761,0.618348624,0.620183486,0.622018349,
0.623853211,0.625688073,0.627522936,0.629357798,0.631192661,0.633027523,
0.634862385,0.636697248,0.63853211,0.640366972,0.642201835,0.644036697,
0.64587156,0.647706422,0.649541284,0.651376147,0.653211009,0.655045872,
0.656880734,0.658715596,0.660550459,0.662385321,0.664220183,0.666055046,
0.667889908,0.669724771,0.671559633,0.673394495,0.675229358,0.67706422,
0.678899083,0.680733945,0.682568807,0.68440367,0.686238532,0.688073394,
0.689908257,0.691743119,0.693577982,0.695412844,0.697247706,0.699082569,
0.700917431,0.702752294,0.704587156,0.706422018,0.708256881,0.710091743,
0.711926606,0.713761468,0.71559633,0.717431193,0.719266055,0.721100917,
0.72293578,0.724770642,0.726605505,0.728440367,0.730275229,0.732110092,
0.733944954,0.735779817,0.737614679,0.739449541,0.741284404,0.743119266,
0.744954128,0.746788991,0.748623853,0.750458716,0.752293578,0.75412844,
0.755963303,0.757798165,0.759633028,0.76146789,0.763302752,0.765137615,
0.766972477,0.768807339,0.770642202,0.772477064,0.774311927,0.776146789,
0.777981651,0.779816514,0.781651376,0.783486239,0.785321101,0.787155963,
0.788990826,0.790825688,0.79266055,0.794495413,0.796330275,0.798165138,
0.8,0.801834862,0.803669725,0.805504587,0.80733945,0.809174312,0.811009174,
0.812844037,0.814678899,0.816513761,0.818348624,0.820183486,0.822018349,
0.823853211,0.825688073,0.827522936,0.829357798,0.831192661,0.833027523,
0.834862385,0.836697248,0.83853211,0.840366972,0.842201835,0.844036697,
0.84587156,0.847706422,0.849541284,0.851376147,0.853211009,0.855045872,
0.856880734,0.858715596,0.860550459,0.862385321,0.864220183,0.866055046,
0.867889908,0.869724771,0.871559633,0.873394495,0.875229358,0.87706422,
0.878899083,0.880733945,0.882568807,0.88440367,0.886238532,0.888073394,
0.889908257,0.891743119,0.893577982,0.895412844,0.897247706,0.899082569,
0.900917431,0.902752294,0.904587156,0.906422018,0.908256881,0.910091743,
0.911926606,0.913761468,0.91559633,0.917431193,0.919266055,0.921100917,
0.92293578,0.924770642,0.926605505,0.928440367,0.930275229,0.932110092,
0.933944954,0.935779817,0.937614679,0.939449541,0.941284404,0.943119266,
0.944954128,0.946788991,0.948623853,0.950458716,0.952293578,0.95412844,
0.955963303,0.957798165,0.959633028,0.96146789,0.963302752,0.965137615,
0.966972477,0.968807339,0.970642202,0.972477064,0.974311927,0.976146789,
0.977981651,0.979816514,0.981651376,0.983486239,0.985321101,0.987155963,
0.988990826,0.990825688,0.99266055,0.994495413,0.996330275,0.998165138,
1.),(0.,0.36),.UNSPECIFIED.);
#6275=B_SPLINE_SURFACE_WITH_KNOTS('',5,1,((#252611,#252612),(#252613,#252614),
(#252615,#252616),(#252617,#252618),(#252619,#252620),(#252621,#252622),
(#252623,#252624),(#252625,#252626),(#252627,#252628),(#252629,#252630),
(#252631,#252632),(#252633,#252634),(#252635,#252636),(#252637,#252638),
(#252639,#252640),(#252641,#252642),(#252643,#252644),(#252645,#252646),
(#252647,#252648),(#252649,#252650),(#252651,#252652),(#252653,#252654),
(#252655,#252656),(#252657,#252658),(#252659,#252660),(#252661,#252662),
(#252663,#252664),(#252665,#252666),(#252667,#252668),(#252669,#252670),
(#252671,#252672),(#252673,#252674),(#252675,#252676),(#252677,#252678),
(#252679,#252680),(#252681,#252682),(#252683,#252684),(#252685,#252686),
(#252687,#252688),(#252689,#252690),(#252691,#252692),(#252693,#252694),
(#252695,#252696),(#252697,#252698),(#252699,#252700),(#252701,#252702),
(#252703,#252704),(#252705,#252706),(#252707,#252708),(#252709,#252710),
(#252711,#252712),(#252713,#252714),(#252715,#252716),(#252717,#252718),
(#252719,#252720),(#252721,#252722),(#252723,#252724),(#252725,#252726),
(#252727,#252728),(#252729,#252730),(#252731,#252732),(#252733,#252734),
(#252735,#252736),(#252737,#252738),(#252739,#252740),(#252741,#252742),
(#252743,#252744),(#252745,#252746),(#252747,#252748),(#252749,#252750),
(#252751,#252752),(#252753,#252754),(#252755,#252756),(#252757,#252758),
(#252759,#252760),(#252761,#252762),(#252763,#252764),(#252765,#252766),
(#252767,#252768),(#252769,#252770),(#252771,#252772),(#252773,#252774),
(#252775,#252776),(#252777,#252778),(#252779,#252780),(#252781,#252782),
(#252783,#252784),(#252785,#252786),(#252787,#252788),(#252789,#252790),
(#252791,#252792),(#252793,#252794),(#252795,#252796),(#252797,#252798),
(#252799,#252800),(#252801,#252802),(#252803,#252804),(#252805,#252806),
(#252807,#252808),(#252809,#252810),(#252811,#252812),(#252813,#252814),
(#252815,#252816),(#252817,#252818),(#252819,#252820),(#252821,#252822),
(#252823,#252824),(#252825,#252826),(#252827,#252828),(#252829,#252830),
(#252831,#252832),(#252833,#252834),(#252835,#252836),(#252837,#252838),
(#252839,#252840),(#252841,#252842),(#252843,#252844),(#252845,#252846),
(#252847,#252848),(#252849,#252850),(#252851,#252852),(#252853,#252854),
(#252855,#252856),(#252857,#252858),(#252859,#252860),(#252861,#252862),
(#252863,#252864),(#252865,#252866),(#252867,#252868),(#252869,#252870),
(#252871,#252872),(#252873,#252874),(#252875,#252876),(#252877,#252878),
(#252879,#252880),(#252881,#252882),(#252883,#252884),(#252885,#252886),
(#252887,#252888),(#252889,#252890),(#252891,#252892),(#252893,#252894),
(#252895,#252896),(#252897,#252898),(#252899,#252900),(#252901,#252902),
(#252903,#252904),(#252905,#252906),(#252907,#252908),(#252909,#252910),
(#252911,#252912),(#252913,#252914),(#252915,#252916),(#252917,#252918),
(#252919,#252920),(#252921,#252922),(#252923,#252924),(#252925,#252926),
(#252927,#252928),(#252929,#252930),(#252931,#252932),(#252933,#252934),
(#252935,#252936),(#252937,#252938),(#252939,#252940),(#252941,#252942),
(#252943,#252944),(#252945,#252946),(#252947,#252948),(#252949,#252950),
(#252951,#252952),(#252953,#252954),(#252955,#252956),(#252957,#252958),
(#252959,#252960),(#252961,#252962),(#252963,#252964),(#252965,#252966),
(#252967,#252968),(#252969,#252970),(#252971,#252972),(#252973,#252974),
(#252975,#252976),(#252977,#252978),(#252979,#252980),(#252981,#252982),
(#252983,#252984),(#252985,#252986),(#252987,#252988),(#252989,#252990),
(#252991,#252992),(#252993,#252994),(#252995,#252996),(#252997,#252998),
(#252999,#253000),(#253001,#253002),(#253003,#253004),(#253005,#253006),
(#253007,#253008),(#253009,#253010),(#253011,#253012),(#253013,#253014),
(#253015,#253016),(#253017,#253018),(#253019,#253020),(#253021,#253022),
(#253023,#253024),(#253025,#253026),(#253027,#253028),(#253029,#253030),
(#253031,#253032),(#253033,#253034),(#253035,#253036),(#253037,#253038),
(#253039,#253040),(#253041,#253042),(#253043,#253044),(#253045,#253046),
(#253047,#253048),(#253049,#253050),(#253051,#253052),(#253053,#253054),
(#253055,#253056),(#253057,#253058),(#253059,#253060),(#253061,#253062),
(#253063,#253064),(#253065,#253066),(#253067,#253068),(#253069,#253070),
(#253071,#253072),(#253073,#253074),(#253075,#253076),(#253077,#253078),
(#253079,#253080),(#253081,#253082),(#253083,#253084),(#253085,#253086),
(#253087,#253088),(#253089,#253090),(#253091,#253092),(#253093,#253094),
(#253095,#253096),(#253097,#253098),(#253099,#253100),(#253101,#253102),
(#253103,#253104),(#253105,#253106),(#253107,#253108),(#253109,#253110),
(#253111,#253112),(#253113,#253114),(#253115,#253116),(#253117,#253118),
(#253119,#253120),(#253121,#253122),(#253123,#253124),(#253125,#253126),
(#253127,#253128),(#253129,#253130),(#253131,#253132),(#253133,#253134),
(#253135,#253136),(#253137,#253138),(#253139,#253140),(#253141,#253142),
(#253143,#253144),(#253145,#253146),(#253147,#253148),(#253149,#253150),
(#253151,#253152),(#253153,#253154),(#253155,#253156),(#253157,#253158),
(#253159,#253160),(#253161,#253162),(#253163,#253164),(#253165,#253166),
(#253167,#253168),(#253169,#253170),(#253171,#253172),(#253173,#253174),
(#253175,#253176),(#253177,#253178),(#253179,#253180),(#253181,#253182),
(#253183,#253184),(#253185,#253186),(#253187,#253188),(#253189,#253190),
(#253191,#253192),(#253193,#253194),(#253195,#253196),(#253197,#253198),
(#253199,#253200),(#253201,#253202),(#253203,#253204),(#253205,#253206),
(#253207,#253208),(#253209,#253210),(#253211,#253212),(#253213,#253214),
(#253215,#253216),(#253217,#253218),(#253219,#253220),(#253221,#253222),
(#253223,#253224),(#253225,#253226),(#253227,#253228),(#253229,#253230),
(#253231,#253232),(#253233,#253234),(#253235,#253236),(#253237,#253238),
(#253239,#253240),(#253241,#253242),(#253243,#253244),(#253245,#253246),
(#253247,#253248),(#253249,#253250),(#253251,#253252),(#253253,#253254),
(#253255,#253256),(#253257,#253258),(#253259,#253260),(#253261,#253262),
(#253263,#253264),(#253265,#253266),(#253267,#253268),(#253269,#253270),
(#253271,#253272),(#253273,#253274),(#253275,#253276),(#253277,#253278),
(#253279,#253280),(#253281,#253282),(#253283,#253284),(#253285,#253286),
(#253287,#253288),(#253289,#253290),(#253291,#253292),(#253293,#253294),
(#253295,#253296),(#253297,#253298),(#253299,#253300),(#253301,#253302),
(#253303,#253304),(#253305,#253306),(#253307,#253308),(#253309,#253310),
(#253311,#253312),(#253313,#253314),(#253315,#253316),(#253317,#253318),
(#253319,#253320),(#253321,#253322),(#253323,#253324),(#253325,#253326),
(#253327,#253328),(#253329,#253330),(#253331,#253332),(#253333,#253334),
(#253335,#253336),(#253337,#253338),(#253339,#253340),(#253341,#253342),
(#253343,#253344),(#253345,#253346),(#253347,#253348),(#253349,#253350),
(#253351,#253352),(#253353,#253354),(#253355,#253356),(#253357,#253358),
(#253359,#253360),(#253361,#253362),(#253363,#253364),(#253365,#253366),
(#253367,#253368),(#253369,#253370),(#253371,#253372),(#253373,#253374),
(#253375,#253376),(#253377,#253378),(#253379,#253380),(#253381,#253382),
(#253383,#253384),(#253385,#253386),(#253387,#253388),(#253389,#253390),
(#253391,#253392),(#253393,#253394),(#253395,#253396),(#253397,#253398),
(#253399,#253400),(#253401,#253402),(#253403,#253404),(#253405,#253406),
(#253407,#253408),(#253409,#253410),(#253411,#253412),(#253413,#253414),
(#253415,#253416),(#253417,#253418),(#253419,#253420),(#253421,#253422),
(#253423,#253424),(#253425,#253426),(#253427,#253428),(#253429,#253430),
(#253431,#253432),(#253433,#253434),(#253435,#253436),(#253437,#253438),
(#253439,#253440),(#253441,#253442),(#253443,#253444),(#253445,#253446),
(#253447,#253448),(#253449,#253450),(#253451,#253452),(#253453,#253454),
(#253455,#253456),(#253457,#253458),(#253459,#253460),(#253461,#253462),
(#253463,#253464),(#253465,#253466),(#253467,#253468),(#253469,#253470),
(#253471,#253472),(#253473,#253474),(#253475,#253476),(#253477,#253478),
(#253479,#253480),(#253481,#253482),(#253483,#253484),(#253485,#253486),
(#253487,#253488),(#253489,#253490),(#253491,#253492),(#253493,#253494),
(#253495,#253496),(#253497,#253498),(#253499,#253500),(#253501,#253502),
(#253503,#253504),(#253505,#253506),(#253507,#253508),(#253509,#253510),
(#253511,#253512),(#253513,#253514),(#253515,#253516),(#253517,#253518),
(#253519,#253520),(#253521,#253522),(#253523,#253524),(#253525,#253526),
(#253527,#253528),(#253529,#253530),(#253531,#253532),(#253533,#253534),
(#253535,#253536),(#253537,#253538),(#253539,#253540),(#253541,#253542),
(#253543,#253544),(#253545,#253546),(#253547,#253548),(#253549,#253550),
(#253551,#253552),(#253553,#253554)),.UNSPECIFIED.,.F.,.F.,.F.,(6,1,1,1,
1,1,1,1,1,1,1,1,1,1,1,1,1,1,1,1,1,1,1,1,1,1,1,1,1,1,1,1,1,1,1,1,1,1,1,1,
1,1,1,1,1,1,1,1,1,1,1,1,1,1,1,1,1,1,1,1,1,1,1,1,1,1,1,1,1,1,1,1,1,1,1,1,
1,1,1,1,1,1,1,1,1,1,1,1,1,1,1,1,1,1,1,1,1,1,1,1,1,1,1,1,1,1,1,1,1,1,1,1,
1,1,1,1,1,1,1,1,1,1,1,1,1,1,1,1,1,1,1,1,1,1,1,1,1,1,1,1,1,1,1,1,1,1,1,1,
1,1,1,1,1,1,1,1,1,1,1,1,1,1,1,1,1,1,1,1,1,1,1,1,1,1,1,1,1,1,1,1,1,1,1,1,
1,1,1,1,1,1,1,1,1,1,1,1,1,1,1,1,1,1,1,1,1,1,1,1,1,1,1,1,1,1,1,1,1,1,1,1,
1,1,1,1,1,1,1,1,1,1,1,1,1,1,1,1,1,1,1,1,1,1,1,1,1,1,1,1,1,1,1,1,1,1,1,1,
1,1,1,1,1,1,1,1,1,1,1,1,1,1,1,1,1,1,1,1,1,1,1,1,1,1,1,1,1,1,1,1,1,1,1,1,
1,1,1,1,1,1,1,1,1,1,1,1,1,1,1,1,1,1,1,1,1,1,1,1,1,1,1,1,1,1,1,1,1,1,1,1,
1,1,1,1,1,1,1,1,1,1,1,1,1,1,1,1,1,1,1,1,1,1,1,1,1,1,1,1,1,1,1,1,1,1,1,1,
1,1,1,1,1,1,1,1,1,1,1,1,1,1,1,1,1,1,1,1,1,1,1,1,1,1,1,1,1,1,1,1,1,1,1,1,
1,1,1,1,1,1,1,1,1,1,1,1,1,1,1,1,1,1,1,1,1,1,1,1,1,1,1,1,1,1,1,1,1,1,1,1,
1,1,1,1,1,1,1,1,1,1,1,1,1,1,1,1,1,1,1,1,1,1,1,1,1,1,1,1,1,1,1,6),(2,2),
(0.143172103,0.144954128,0.146788991,0.148623853,0.150458716,0.152293578,
0.15412844,0.155963303,0.157798165,0.159633028,0.16146789,0.163302752,0.165137615,
0.166972477,0.168807339,0.170642202,0.172477064,0.174311927,0.176146789,
0.177981651,0.179816514,0.181651376,0.183486239,0.185321101,0.187155963,
0.188990826,0.190825688,0.19266055,0.194495413,0.196330275,0.198165138,
0.2,0.201834862,0.203669725,0.205504587,0.20733945,0.209174312,0.211009174,
0.212844037,0.214678899,0.216513761,0.218348624,0.220183486,0.222018349,
0.223853211,0.225688073,0.227522936,0.229357798,0.231192661,0.233027523,
0.234862385,0.236697248,0.23853211,0.240366972,0.242201835,0.244036697,
0.24587156,0.247706422,0.249541284,0.251376147,0.253211009,0.255045872,
0.256880734,0.258715596,0.260550459,0.262385321,0.264220183,0.266055046,
0.267889908,0.269724771,0.271559633,0.273394495,0.275229358,0.27706422,
0.278899083,0.280733945,0.282568807,0.28440367,0.286238532,0.288073394,
0.289908257,0.291743119,0.293577982,0.295412844,0.297247706,0.299082569,
0.300917431,0.302752294,0.304587156,0.306422018,0.308256881,0.310091743,
0.311926606,0.313761468,0.31559633,0.317431193,0.319266055,0.321100917,
0.32293578,0.324770642,0.326605505,0.328440367,0.330275229,0.332110092,
0.333944954,0.335779817,0.337614679,0.339449541,0.341284404,0.343119266,
0.344954128,0.346788991,0.348623853,0.350458716,0.352293578,0.35412844,
0.355963303,0.357798165,0.359633028,0.36146789,0.363302752,0.365137615,
0.366972477,0.368807339,0.370642202,0.372477064,0.374311927,0.376146789,
0.377981651,0.379816514,0.381651376,0.383486239,0.385321101,0.387155963,
0.388990826,0.390825688,0.39266055,0.394495413,0.396330275,0.398165138,
0.4,0.401834862,0.403669725,0.405504587,0.40733945,0.409174312,0.411009174,
0.412844037,0.414678899,0.416513761,0.418348624,0.420183486,0.422018349,
0.423853211,0.425688073,0.427522936,0.429357798,0.431192661,0.433027523,
0.434862385,0.436697248,0.43853211,0.440366972,0.442201835,0.444036697,
0.44587156,0.447706422,0.449541284,0.451376147,0.453211009,0.455045872,
0.456880734,0.458715596,0.460550459,0.462385321,0.464220183,0.466055046,
0.467889908,0.469724771,0.471559633,0.473394495,0.475229358,0.47706422,
0.478899083,0.480733945,0.482568807,0.48440367,0.486238532,0.488073394,
0.489908257,0.491743119,0.493577982,0.495412844,0.497247706,0.499082569,
0.500917431,0.502752294,0.504587156,0.506422018,0.508256881,0.510091743,
0.511926606,0.513761468,0.51559633,0.517431193,0.519266055,0.521100917,
0.52293578,0.524770642,0.526605505,0.528440367,0.530275229,0.532110092,
0.533944954,0.535779817,0.537614679,0.539449541,0.541284404,0.543119266,
0.544954128,0.546788991,0.548623853,0.550458716,0.552293578,0.55412844,
0.555963303,0.557798165,0.559633028,0.56146789,0.563302752,0.565137615,
0.566972477,0.568807339,0.570642202,0.572477064,0.574311927,0.576146789,
0.577981651,0.579816514,0.581651376,0.583486239,0.585321101,0.587155963,
0.588990826,0.590825688,0.59266055,0.594495413,0.596330275,0.598165138,
0.6,0.601834862,0.603669725,0.605504587,0.60733945,0.609174312,0.611009174,
0.612844037,0.614678899,0.616513761,0.618348624,0.620183486,0.622018349,
0.623853211,0.625688073,0.627522936,0.629357798,0.631192661,0.633027523,
0.634862385,0.636697248,0.63853211,0.640366972,0.642201835,0.644036697,
0.64587156,0.647706422,0.649541284,0.651376147,0.653211009,0.655045872,
0.656880734,0.658715596,0.660550459,0.662385321,0.664220183,0.666055046,
0.667889908,0.669724771,0.671559633,0.673394495,0.675229358,0.67706422,
0.678899083,0.680733945,0.682568807,0.68440367,0.686238532,0.688073394,
0.689908257,0.691743119,0.693577982,0.695412844,0.697247706,0.699082569,
0.700917431,0.702752294,0.704587156,0.706422018,0.708256881,0.710091743,
0.711926606,0.713761468,0.71559633,0.717431193,0.719266055,0.721100917,
0.72293578,0.724770642,0.726605505,0.728440367,0.730275229,0.732110092,
0.733944954,0.735779817,0.737614679,0.739449541,0.741284404,0.743119266,
0.744954128,0.746788991,0.748623853,0.750458716,0.752293578,0.75412844,
0.755963303,0.757798165,0.759633028,0.76146789,0.763302752,0.765137615,
0.766972477,0.768807339,0.770642202,0.772477064,0.774311927,0.776146789,
0.777981651,0.779816514,0.781651376,0.783486239,0.785321101,0.787155963,
0.788990826,0.790825688,0.79266055,0.794495413,0.796330275,0.798165138,
0.8,0.801834862,0.803669725,0.805504587,0.80733945,0.809174312,0.811009174,
0.812844037,0.814678899,0.816513761,0.818348624,0.820183486,0.822018349,
0.823853211,0.825688073,0.827522936,0.829357798,0.831192661,0.833027523,
0.834862385,0.836697248,0.83853211,0.840366972,0.842201835,0.844036697,
0.84587156,0.847706422,0.849541284,0.851376147,0.853211009,0.855045872,
0.856880734,0.858715596,0.860550459,0.862385321,0.864220183,0.866055046,
0.867889908,0.869724771,0.871559633,0.873394495,0.875229358,0.87706422,
0.878899083,0.880733945,0.882568807,0.88440367,0.886238532,0.888073394,
0.889908257,0.891743119,0.893577982,0.895412844,0.897247706,0.899082569,
0.900917431,0.902752294,0.904587156,0.906422018,0.908256881,0.910091743,
0.911926606,0.913761468,0.91559633,0.917431193,0.919266055,0.921100917,
0.92293578,0.924770642,0.926605505,0.928440367,0.930275229,0.932110092,
0.933944954,0.935779817,0.937614679,0.939449541,0.941284404,0.943119266,
0.944954128,0.946788991,0.948623853,0.950458716,0.952293578,0.95412844,
0.955963303,0.957798165,0.959633028,0.96146789,0.963302752,0.965137615,
0.966972477,0.968807339,0.970642202,0.972477064,0.974311927,0.976146789,
0.977981651,0.979816514,0.981651376,0.983486239,0.985321101,0.987155963,
0.988990826,0.990825688,0.99266055,0.994495413,0.996330275,0.998165138,
1.),(0.,0.36),.UNSPECIFIED.);
#6276=B_SPLINE_SURFACE_WITH_KNOTS('',5,1,((#254166,#254167),(#254168,#254169),
(#254170,#254171),(#254172,#254173),(#254174,#254175),(#254176,#254177),
(#254178,#254179),(#254180,#254181),(#254182,#254183),(#254184,#254185),
(#254186,#254187),(#254188,#254189),(#254190,#254191),(#254192,#254193),
(#254194,#254195),(#254196,#254197),(#254198,#254199),(#254200,#254201),
(#254202,#254203),(#254204,#254205),(#254206,#254207),(#254208,#254209),
(#254210,#254211),(#254212,#254213),(#254214,#254215),(#254216,#254217),
(#254218,#254219),(#254220,#254221),(#254222,#254223),(#254224,#254225),
(#254226,#254227),(#254228,#254229),(#254230,#254231),(#254232,#254233),
(#254234,#254235),(#254236,#254237),(#254238,#254239),(#254240,#254241),
(#254242,#254243),(#254244,#254245),(#254246,#254247),(#254248,#254249),
(#254250,#254251),(#254252,#254253),(#254254,#254255),(#254256,#254257),
(#254258,#254259),(#254260,#254261),(#254262,#254263),(#254264,#254265),
(#254266,#254267),(#254268,#254269),(#254270,#254271),(#254272,#254273),
(#254274,#254275),(#254276,#254277),(#254278,#254279),(#254280,#254281),
(#254282,#254283),(#254284,#254285),(#254286,#254287),(#254288,#254289),
(#254290,#254291),(#254292,#254293),(#254294,#254295),(#254296,#254297),
(#254298,#254299),(#254300,#254301),(#254302,#254303),(#254304,#254305),
(#254306,#254307),(#254308,#254309),(#254310,#254311),(#254312,#254313),
(#254314,#254315),(#254316,#254317),(#254318,#254319),(#254320,#254321),
(#254322,#254323),(#254324,#254325),(#254326,#254327),(#254328,#254329),
(#254330,#254331),(#254332,#254333),(#254334,#254335),(#254336,#254337),
(#254338,#254339),(#254340,#254341),(#254342,#254343),(#254344,#254345),
(#254346,#254347),(#254348,#254349),(#254350,#254351),(#254352,#254353),
(#254354,#254355),(#254356,#254357),(#254358,#254359),(#254360,#254361),
(#254362,#254363),(#254364,#254365),(#254366,#254367),(#254368,#254369),
(#254370,#254371),(#254372,#254373),(#254374,#254375),(#254376,#254377),
(#254378,#254379),(#254380,#254381),(#254382,#254383),(#254384,#254385),
(#254386,#254387),(#254388,#254389),(#254390,#254391),(#254392,#254393),
(#254394,#254395),(#254396,#254397),(#254398,#254399),(#254400,#254401),
(#254402,#254403),(#254404,#254405),(#254406,#254407),(#254408,#254409),
(#254410,#254411),(#254412,#254413),(#254414,#254415),(#254416,#254417),
(#254418,#254419),(#254420,#254421),(#254422,#254423),(#254424,#254425),
(#254426,#254427),(#254428,#254429),(#254430,#254431),(#254432,#254433),
(#254434,#254435),(#254436,#254437),(#254438,#254439),(#254440,#254441),
(#254442,#254443),(#254444,#254445),(#254446,#254447),(#254448,#254449),
(#254450,#254451),(#254452,#254453),(#254454,#254455),(#254456,#254457),
(#254458,#254459),(#254460,#254461),(#254462,#254463),(#254464,#254465),
(#254466,#254467),(#254468,#254469),(#254470,#254471),(#254472,#254473),
(#254474,#254475),(#254476,#254477),(#254478,#254479),(#254480,#254481),
(#254482,#254483),(#254484,#254485),(#254486,#254487),(#254488,#254489),
(#254490,#254491),(#254492,#254493),(#254494,#254495),(#254496,#254497),
(#254498,#254499),(#254500,#254501),(#254502,#254503),(#254504,#254505),
(#254506,#254507),(#254508,#254509),(#254510,#254511),(#254512,#254513),
(#254514,#254515),(#254516,#254517),(#254518,#254519),(#254520,#254521),
(#254522,#254523),(#254524,#254525),(#254526,#254527),(#254528,#254529),
(#254530,#254531),(#254532,#254533),(#254534,#254535),(#254536,#254537),
(#254538,#254539),(#254540,#254541),(#254542,#254543),(#254544,#254545),
(#254546,#254547),(#254548,#254549),(#254550,#254551),(#254552,#254553),
(#254554,#254555),(#254556,#254557),(#254558,#254559),(#254560,#254561),
(#254562,#254563),(#254564,#254565),(#254566,#254567),(#254568,#254569),
(#254570,#254571),(#254572,#254573),(#254574,#254575),(#254576,#254577),
(#254578,#254579),(#254580,#254581),(#254582,#254583),(#254584,#254585),
(#254586,#254587),(#254588,#254589),(#254590,#254591),(#254592,#254593),
(#254594,#254595),(#254596,#254597),(#254598,#254599),(#254600,#254601),
(#254602,#254603),(#254604,#254605),(#254606,#254607),(#254608,#254609),
(#254610,#254611),(#254612,#254613),(#254614,#254615),(#254616,#254617),
(#254618,#254619),(#254620,#254621),(#254622,#254623),(#254624,#254625),
(#254626,#254627),(#254628,#254629),(#254630,#254631),(#254632,#254633),
(#254634,#254635),(#254636,#254637),(#254638,#254639),(#254640,#254641),
(#254642,#254643),(#254644,#254645),(#254646,#254647),(#254648,#254649),
(#254650,#254651),(#254652,#254653),(#254654,#254655),(#254656,#254657),
(#254658,#254659),(#254660,#254661),(#254662,#254663),(#254664,#254665),
(#254666,#254667),(#254668,#254669),(#254670,#254671),(#254672,#254673),
(#254674,#254675),(#254676,#254677),(#254678,#254679),(#254680,#254681),
(#254682,#254683),(#254684,#254685),(#254686,#254687),(#254688,#254689),
(#254690,#254691),(#254692,#254693),(#254694,#254695),(#254696,#254697),
(#254698,#254699),(#254700,#254701),(#254702,#254703),(#254704,#254705),
(#254706,#254707),(#254708,#254709),(#254710,#254711),(#254712,#254713),
(#254714,#254715),(#254716,#254717),(#254718,#254719),(#254720,#254721),
(#254722,#254723),(#254724,#254725),(#254726,#254727),(#254728,#254729),
(#254730,#254731),(#254732,#254733),(#254734,#254735),(#254736,#254737),
(#254738,#254739),(#254740,#254741),(#254742,#254743),(#254744,#254745),
(#254746,#254747),(#254748,#254749),(#254750,#254751),(#254752,#254753),
(#254754,#254755),(#254756,#254757),(#254758,#254759),(#254760,#254761),
(#254762,#254763),(#254764,#254765),(#254766,#254767),(#254768,#254769),
(#254770,#254771),(#254772,#254773),(#254774,#254775),(#254776,#254777),
(#254778,#254779),(#254780,#254781),(#254782,#254783),(#254784,#254785),
(#254786,#254787),(#254788,#254789),(#254790,#254791),(#254792,#254793),
(#254794,#254795),(#254796,#254797),(#254798,#254799),(#254800,#254801),
(#254802,#254803),(#254804,#254805),(#254806,#254807),(#254808,#254809),
(#254810,#254811),(#254812,#254813),(#254814,#254815),(#254816,#254817),
(#254818,#254819),(#254820,#254821),(#254822,#254823),(#254824,#254825),
(#254826,#254827),(#254828,#254829),(#254830,#254831),(#254832,#254833),
(#254834,#254835),(#254836,#254837),(#254838,#254839),(#254840,#254841),
(#254842,#254843),(#254844,#254845),(#254846,#254847),(#254848,#254849),
(#254850,#254851),(#254852,#254853),(#254854,#254855),(#254856,#254857),
(#254858,#254859),(#254860,#254861),(#254862,#254863),(#254864,#254865),
(#254866,#254867),(#254868,#254869),(#254870,#254871),(#254872,#254873),
(#254874,#254875),(#254876,#254877),(#254878,#254879),(#254880,#254881),
(#254882,#254883),(#254884,#254885),(#254886,#254887),(#254888,#254889),
(#254890,#254891),(#254892,#254893),(#254894,#254895),(#254896,#254897),
(#254898,#254899),(#254900,#254901),(#254902,#254903),(#254904,#254905),
(#254906,#254907),(#254908,#254909),(#254910,#254911),(#254912,#254913),
(#254914,#254915),(#254916,#254917),(#254918,#254919),(#254920,#254921),
(#254922,#254923),(#254924,#254925),(#254926,#254927),(#254928,#254929),
(#254930,#254931),(#254932,#254933),(#254934,#254935),(#254936,#254937),
(#254938,#254939),(#254940,#254941),(#254942,#254943),(#254944,#254945),
(#254946,#254947),(#254948,#254949),(#254950,#254951),(#254952,#254953),
(#254954,#254955),(#254956,#254957),(#254958,#254959),(#254960,#254961),
(#254962,#254963),(#254964,#254965),(#254966,#254967),(#254968,#254969),
(#254970,#254971),(#254972,#254973),(#254974,#254975),(#254976,#254977),
(#254978,#254979),(#254980,#254981),(#254982,#254983),(#254984,#254985),
(#254986,#254987),(#254988,#254989),(#254990,#254991),(#254992,#254993),
(#254994,#254995),(#254996,#254997),(#254998,#254999),(#255000,#255001),
(#255002,#255003),(#255004,#255005),(#255006,#255007),(#255008,#255009),
(#255010,#255011),(#255012,#255013),(#255014,#255015),(#255016,#255017),
(#255018,#255019),(#255020,#255021),(#255022,#255023),(#255024,#255025),
(#255026,#255027),(#255028,#255029),(#255030,#255031),(#255032,#255033),
(#255034,#255035),(#255036,#255037),(#255038,#255039),(#255040,#255041),
(#255042,#255043),(#255044,#255045),(#255046,#255047),(#255048,#255049),
(#255050,#255051),(#255052,#255053),(#255054,#255055),(#255056,#255057),
(#255058,#255059),(#255060,#255061),(#255062,#255063),(#255064,#255065),
(#255066,#255067),(#255068,#255069),(#255070,#255071),(#255072,#255073),
(#255074,#255075),(#255076,#255077),(#255078,#255079),(#255080,#255081),
(#255082,#255083),(#255084,#255085),(#255086,#255087),(#255088,#255089),
(#255090,#255091),(#255092,#255093),(#255094,#255095),(#255096,#255097),
(#255098,#255099),(#255100,#255101),(#255102,#255103),(#255104,#255105),
(#255106,#255107),(#255108,#255109)),.UNSPECIFIED.,.F.,.F.,.F.,(6,1,1,1,
1,1,1,1,1,1,1,1,1,1,1,1,1,1,1,1,1,1,1,1,1,1,1,1,1,1,1,1,1,1,1,1,1,1,1,1,
1,1,1,1,1,1,1,1,1,1,1,1,1,1,1,1,1,1,1,1,1,1,1,1,1,1,1,1,1,1,1,1,1,1,1,1,
1,1,1,1,1,1,1,1,1,1,1,1,1,1,1,1,1,1,1,1,1,1,1,1,1,1,1,1,1,1,1,1,1,1,1,1,
1,1,1,1,1,1,1,1,1,1,1,1,1,1,1,1,1,1,1,1,1,1,1,1,1,1,1,1,1,1,1,1,1,1,1,1,
1,1,1,1,1,1,1,1,1,1,1,1,1,1,1,1,1,1,1,1,1,1,1,1,1,1,1,1,1,1,1,1,1,1,1,1,
1,1,1,1,1,1,1,1,1,1,1,1,1,1,1,1,1,1,1,1,1,1,1,1,1,1,1,1,1,1,1,1,1,1,1,1,
1,1,1,1,1,1,1,1,1,1,1,1,1,1,1,1,1,1,1,1,1,1,1,1,1,1,1,1,1,1,1,1,1,1,1,1,
1,1,1,1,1,1,1,1,1,1,1,1,1,1,1,1,1,1,1,1,1,1,1,1,1,1,1,1,1,1,1,1,1,1,1,1,
1,1,1,1,1,1,1,1,1,1,1,1,1,1,1,1,1,1,1,1,1,1,1,1,1,1,1,1,1,1,1,1,1,1,1,1,
1,1,1,1,1,1,1,1,1,1,1,1,1,1,1,1,1,1,1,1,1,1,1,1,1,1,1,1,1,1,1,1,1,1,1,1,
1,1,1,1,1,1,1,1,1,1,1,1,1,1,1,1,1,1,1,1,1,1,1,1,1,1,1,1,1,1,1,1,1,1,1,1,
1,1,1,1,1,1,1,1,1,1,1,1,1,1,1,1,1,1,1,1,1,1,1,1,1,1,1,1,1,1,1,1,1,1,1,1,
1,1,1,1,1,1,1,1,1,1,1,1,1,1,1,1,1,1,1,1,1,1,1,1,1,1,1,1,1,1,1,6),(2,2),
(-1.,-0.998165138,-0.996330275,-0.994495413,-0.99266055,-0.990825688,-0.988990826,
-0.987155963,-0.985321101,-0.983486239,-0.981651376,-0.979816514,-0.977981651,
-0.976146789,-0.974311927,-0.972477064,-0.970642202,-0.968807339,-0.966972477,
-0.965137615,-0.963302752,-0.96146789,-0.959633028,-0.957798165,-0.955963303,
-0.95412844,-0.952293578,-0.950458716,-0.948623853,-0.946788991,-0.944954128,
-0.943119266,-0.941284404,-0.939449541,-0.937614679,-0.935779817,-0.933944954,
-0.932110092,-0.930275229,-0.928440367,-0.926605505,-0.924770642,-0.92293578,
-0.921100917,-0.919266055,-0.917431193,-0.91559633,-0.913761468,-0.911926606,
-0.910091743,-0.908256881,-0.906422018,-0.904587156,-0.902752294,-0.900917431,
-0.899082569,-0.897247706,-0.895412844,-0.893577982,-0.891743119,-0.889908257,
-0.888073394,-0.886238532,-0.88440367,-0.882568807,-0.880733945,-0.878899083,
-0.87706422,-0.875229358,-0.873394495,-0.871559633,-0.869724771,-0.867889908,
-0.866055046,-0.864220183,-0.862385321,-0.860550459,-0.858715596,-0.856880734,
-0.855045872,-0.853211009,-0.851376147,-0.849541284,-0.847706422,-0.84587156,
-0.844036697,-0.842201835,-0.840366972,-0.83853211,-0.836697248,-0.834862385,
-0.833027523,-0.831192661,-0.829357798,-0.827522936,-0.825688073,-0.823853211,
-0.822018349,-0.820183486,-0.818348624,-0.816513761,-0.814678899,-0.812844037,
-0.811009174,-0.809174312,-0.80733945,-0.805504587,-0.803669725,-0.801834862,
-0.8,-0.798165138,-0.796330275,-0.794495413,-0.79266055,-0.790825688,-0.788990826,
-0.787155963,-0.785321101,-0.783486239,-0.781651376,-0.779816514,-0.777981651,
-0.776146789,-0.774311927,-0.772477064,-0.770642202,-0.768807339,-0.766972477,
-0.765137615,-0.763302752,-0.76146789,-0.759633028,-0.757798165,-0.755963303,
-0.75412844,-0.752293578,-0.750458716,-0.748623853,-0.746788991,-0.744954128,
-0.743119266,-0.741284404,-0.739449541,-0.737614679,-0.735779817,-0.733944954,
-0.732110092,-0.730275229,-0.728440367,-0.726605505,-0.724770642,-0.72293578,
-0.721100917,-0.719266055,-0.717431193,-0.71559633,-0.713761468,-0.711926606,
-0.710091743,-0.708256881,-0.706422018,-0.704587156,-0.702752294,-0.700917431,
-0.699082569,-0.697247706,-0.695412844,-0.693577982,-0.691743119,-0.689908257,
-0.688073394,-0.686238532,-0.68440367,-0.682568807,-0.680733945,-0.678899083,
-0.67706422,-0.675229358,-0.673394495,-0.671559633,-0.669724771,-0.667889908,
-0.666055046,-0.664220183,-0.662385321,-0.660550459,-0.658715596,-0.656880734,
-0.655045872,-0.653211009,-0.651376147,-0.649541284,-0.647706422,-0.64587156,
-0.644036697,-0.642201835,-0.640366972,-0.63853211,-0.636697248,-0.634862385,
-0.633027523,-0.631192661,-0.629357798,-0.627522936,-0.625688073,-0.623853211,
-0.622018349,-0.620183486,-0.618348624,-0.616513761,-0.614678899,-0.612844037,
-0.611009174,-0.609174312,-0.60733945,-0.605504587,-0.603669725,-0.601834862,
-0.6,-0.598165138,-0.596330275,-0.594495413,-0.59266055,-0.590825688,-0.588990826,
-0.587155963,-0.585321101,-0.583486239,-0.581651376,-0.579816514,-0.577981651,
-0.576146789,-0.574311927,-0.572477064,-0.570642202,-0.568807339,-0.566972477,
-0.565137615,-0.563302752,-0.56146789,-0.559633028,-0.557798165,-0.555963303,
-0.55412844,-0.552293578,-0.550458716,-0.548623853,-0.546788991,-0.544954128,
-0.543119266,-0.541284404,-0.539449541,-0.537614679,-0.535779817,-0.533944954,
-0.532110092,-0.530275229,-0.528440367,-0.526605505,-0.524770642,-0.52293578,
-0.521100917,-0.519266055,-0.517431193,-0.51559633,-0.513761468,-0.511926606,
-0.510091743,-0.508256881,-0.506422018,-0.504587156,-0.502752294,-0.500917431,
-0.499082569,-0.497247706,-0.495412844,-0.493577982,-0.491743119,-0.489908257,
-0.488073394,-0.486238532,-0.48440367,-0.482568807,-0.480733945,-0.478899083,
-0.47706422,-0.475229358,-0.473394495,-0.471559633,-0.469724771,-0.467889908,
-0.466055046,-0.464220183,-0.462385321,-0.460550459,-0.458715596,-0.456880734,
-0.455045872,-0.453211009,-0.451376147,-0.449541284,-0.447706422,-0.44587156,
-0.444036697,-0.442201835,-0.440366972,-0.43853211,-0.436697248,-0.434862385,
-0.433027523,-0.431192661,-0.429357798,-0.427522936,-0.425688073,-0.423853211,
-0.422018349,-0.420183486,-0.418348624,-0.416513761,-0.414678899,-0.412844037,
-0.411009174,-0.409174312,-0.40733945,-0.405504587,-0.403669725,-0.401834862,
-0.4,-0.398165138,-0.396330275,-0.394495413,-0.39266055,-0.390825688,-0.388990826,
-0.387155963,-0.385321101,-0.383486239,-0.381651376,-0.379816514,-0.377981651,
-0.376146789,-0.374311927,-0.372477064,-0.370642202,-0.368807339,-0.366972477,
-0.365137615,-0.363302752,-0.36146789,-0.359633028,-0.357798165,-0.355963303,
-0.35412844,-0.352293578,-0.350458716,-0.348623853,-0.346788991,-0.344954128,
-0.343119266,-0.341284404,-0.339449541,-0.337614679,-0.335779817,-0.333944954,
-0.332110092,-0.330275229,-0.328440367,-0.326605505,-0.324770642,-0.32293578,
-0.321100917,-0.319266055,-0.317431193,-0.31559633,-0.313761468,-0.311926606,
-0.310091743,-0.308256881,-0.306422018,-0.304587156,-0.302752294,-0.300917431,
-0.299082569,-0.297247706,-0.295412844,-0.293577982,-0.291743119,-0.289908257,
-0.288073394,-0.286238532,-0.28440367,-0.282568807,-0.280733945,-0.278899083,
-0.27706422,-0.275229358,-0.273394495,-0.271559633,-0.269724771,-0.267889908,
-0.266055046,-0.264220183,-0.262385321,-0.260550459,-0.258715596,-0.256880734,
-0.255045872,-0.253211009,-0.251376147,-0.249541284,-0.247706422,-0.24587156,
-0.244036697,-0.242201835,-0.240366972,-0.23853211,-0.236697248,-0.234862385,
-0.233027523,-0.231192661,-0.229357798,-0.227522936,-0.225688073,-0.223853211,
-0.222018349,-0.220183486,-0.218348624,-0.216513761,-0.214678899,-0.212844037,
-0.211009174,-0.209174312,-0.20733945,-0.205504587,-0.203669725,-0.201834862,
-0.2,-0.198165138,-0.196330275,-0.194495413,-0.19266055,-0.190825688,-0.188990826,
-0.187155963,-0.185321101,-0.183486239,-0.181651376,-0.179816514,-0.177981651,
-0.176146789,-0.174311927,-0.172477064,-0.170642202,-0.168807339,-0.166972477,
-0.165137615,-0.163302752,-0.16146789,-0.159633028,-0.157798165,-0.155963303,
-0.15412844,-0.152293578,-0.150458716,-0.148623853,-0.146788991,-0.144954128,
-0.143172103),(0.,0.36),.UNSPECIFIED.);
#6277=B_SPLINE_SURFACE_WITH_KNOTS('',5,1,((#255763,#255764),(#255765,#255766),
(#255767,#255768),(#255769,#255770),(#255771,#255772),(#255773,#255774),
(#255775,#255776),(#255777,#255778),(#255779,#255780),(#255781,#255782),
(#255783,#255784),(#255785,#255786),(#255787,#255788),(#255789,#255790),
(#255791,#255792),(#255793,#255794),(#255795,#255796),(#255797,#255798),
(#255799,#255800),(#255801,#255802),(#255803,#255804),(#255805,#255806),
(#255807,#255808),(#255809,#255810),(#255811,#255812),(#255813,#255814),
(#255815,#255816),(#255817,#255818),(#255819,#255820),(#255821,#255822),
(#255823,#255824),(#255825,#255826),(#255827,#255828),(#255829,#255830),
(#255831,#255832),(#255833,#255834),(#255835,#255836),(#255837,#255838),
(#255839,#255840),(#255841,#255842),(#255843,#255844),(#255845,#255846),
(#255847,#255848),(#255849,#255850),(#255851,#255852),(#255853,#255854),
(#255855,#255856),(#255857,#255858),(#255859,#255860),(#255861,#255862),
(#255863,#255864),(#255865,#255866),(#255867,#255868),(#255869,#255870),
(#255871,#255872),(#255873,#255874),(#255875,#255876),(#255877,#255878),
(#255879,#255880),(#255881,#255882),(#255883,#255884),(#255885,#255886),
(#255887,#255888),(#255889,#255890),(#255891,#255892),(#255893,#255894),
(#255895,#255896),(#255897,#255898),(#255899,#255900),(#255901,#255902),
(#255903,#255904),(#255905,#255906),(#255907,#255908),(#255909,#255910),
(#255911,#255912),(#255913,#255914),(#255915,#255916),(#255917,#255918),
(#255919,#255920),(#255921,#255922),(#255923,#255924),(#255925,#255926),
(#255927,#255928),(#255929,#255930),(#255931,#255932),(#255933,#255934),
(#255935,#255936),(#255937,#255938),(#255939,#255940),(#255941,#255942),
(#255943,#255944),(#255945,#255946),(#255947,#255948),(#255949,#255950),
(#255951,#255952),(#255953,#255954),(#255955,#255956),(#255957,#255958),
(#255959,#255960),(#255961,#255962),(#255963,#255964),(#255965,#255966),
(#255967,#255968),(#255969,#255970),(#255971,#255972),(#255973,#255974),
(#255975,#255976),(#255977,#255978),(#255979,#255980),(#255981,#255982),
(#255983,#255984),(#255985,#255986),(#255987,#255988),(#255989,#255990),
(#255991,#255992),(#255993,#255994),(#255995,#255996),(#255997,#255998),
(#255999,#256000),(#256001,#256002),(#256003,#256004),(#256005,#256006),
(#256007,#256008),(#256009,#256010),(#256011,#256012),(#256013,#256014),
(#256015,#256016),(#256017,#256018),(#256019,#256020),(#256021,#256022),
(#256023,#256024),(#256025,#256026),(#256027,#256028),(#256029,#256030),
(#256031,#256032),(#256033,#256034),(#256035,#256036),(#256037,#256038),
(#256039,#256040),(#256041,#256042),(#256043,#256044),(#256045,#256046),
(#256047,#256048),(#256049,#256050),(#256051,#256052),(#256053,#256054),
(#256055,#256056),(#256057,#256058),(#256059,#256060),(#256061,#256062),
(#256063,#256064),(#256065,#256066),(#256067,#256068),(#256069,#256070),
(#256071,#256072),(#256073,#256074),(#256075,#256076),(#256077,#256078),
(#256079,#256080),(#256081,#256082),(#256083,#256084),(#256085,#256086),
(#256087,#256088),(#256089,#256090),(#256091,#256092),(#256093,#256094),
(#256095,#256096),(#256097,#256098),(#256099,#256100),(#256101,#256102),
(#256103,#256104),(#256105,#256106),(#256107,#256108),(#256109,#256110),
(#256111,#256112),(#256113,#256114),(#256115,#256116),(#256117,#256118),
(#256119,#256120),(#256121,#256122),(#256123,#256124),(#256125,#256126),
(#256127,#256128),(#256129,#256130),(#256131,#256132),(#256133,#256134),
(#256135,#256136),(#256137,#256138),(#256139,#256140),(#256141,#256142),
(#256143,#256144),(#256145,#256146),(#256147,#256148),(#256149,#256150),
(#256151,#256152),(#256153,#256154),(#256155,#256156),(#256157,#256158),
(#256159,#256160),(#256161,#256162),(#256163,#256164),(#256165,#256166),
(#256167,#256168),(#256169,#256170),(#256171,#256172),(#256173,#256174),
(#256175,#256176),(#256177,#256178),(#256179,#256180),(#256181,#256182),
(#256183,#256184),(#256185,#256186),(#256187,#256188),(#256189,#256190),
(#256191,#256192),(#256193,#256194),(#256195,#256196),(#256197,#256198),
(#256199,#256200),(#256201,#256202),(#256203,#256204),(#256205,#256206),
(#256207,#256208),(#256209,#256210),(#256211,#256212),(#256213,#256214),
(#256215,#256216),(#256217,#256218),(#256219,#256220),(#256221,#256222),
(#256223,#256224),(#256225,#256226),(#256227,#256228),(#256229,#256230),
(#256231,#256232),(#256233,#256234),(#256235,#256236),(#256237,#256238),
(#256239,#256240),(#256241,#256242),(#256243,#256244),(#256245,#256246),
(#256247,#256248),(#256249,#256250),(#256251,#256252),(#256253,#256254),
(#256255,#256256),(#256257,#256258),(#256259,#256260),(#256261,#256262),
(#256263,#256264),(#256265,#256266),(#256267,#256268),(#256269,#256270),
(#256271,#256272),(#256273,#256274),(#256275,#256276),(#256277,#256278),
(#256279,#256280),(#256281,#256282),(#256283,#256284),(#256285,#256286),
(#256287,#256288),(#256289,#256290),(#256291,#256292),(#256293,#256294),
(#256295,#256296),(#256297,#256298),(#256299,#256300),(#256301,#256302),
(#256303,#256304),(#256305,#256306),(#256307,#256308),(#256309,#256310),
(#256311,#256312),(#256313,#256314),(#256315,#256316),(#256317,#256318),
(#256319,#256320),(#256321,#256322),(#256323,#256324),(#256325,#256326),
(#256327,#256328),(#256329,#256330),(#256331,#256332),(#256333,#256334),
(#256335,#256336),(#256337,#256338),(#256339,#256340),(#256341,#256342),
(#256343,#256344),(#256345,#256346),(#256347,#256348),(#256349,#256350),
(#256351,#256352),(#256353,#256354),(#256355,#256356),(#256357,#256358),
(#256359,#256360),(#256361,#256362),(#256363,#256364),(#256365,#256366),
(#256367,#256368),(#256369,#256370),(#256371,#256372),(#256373,#256374),
(#256375,#256376),(#256377,#256378),(#256379,#256380),(#256381,#256382),
(#256383,#256384),(#256385,#256386),(#256387,#256388),(#256389,#256390),
(#256391,#256392),(#256393,#256394),(#256395,#256396),(#256397,#256398),
(#256399,#256400),(#256401,#256402),(#256403,#256404),(#256405,#256406),
(#256407,#256408),(#256409,#256410),(#256411,#256412),(#256413,#256414),
(#256415,#256416),(#256417,#256418),(#256419,#256420),(#256421,#256422),
(#256423,#256424),(#256425,#256426),(#256427,#256428),(#256429,#256430),
(#256431,#256432),(#256433,#256434),(#256435,#256436),(#256437,#256438),
(#256439,#256440),(#256441,#256442),(#256443,#256444),(#256445,#256446),
(#256447,#256448),(#256449,#256450),(#256451,#256452),(#256453,#256454),
(#256455,#256456),(#256457,#256458),(#256459,#256460),(#256461,#256462),
(#256463,#256464),(#256465,#256466),(#256467,#256468),(#256469,#256470),
(#256471,#256472),(#256473,#256474),(#256475,#256476),(#256477,#256478),
(#256479,#256480),(#256481,#256482),(#256483,#256484),(#256485,#256486),
(#256487,#256488),(#256489,#256490),(#256491,#256492),(#256493,#256494),
(#256495,#256496),(#256497,#256498),(#256499,#256500),(#256501,#256502),
(#256503,#256504),(#256505,#256506),(#256507,#256508),(#256509,#256510),
(#256511,#256512),(#256513,#256514),(#256515,#256516),(#256517,#256518),
(#256519,#256520),(#256521,#256522),(#256523,#256524),(#256525,#256526),
(#256527,#256528),(#256529,#256530),(#256531,#256532),(#256533,#256534),
(#256535,#256536),(#256537,#256538),(#256539,#256540),(#256541,#256542),
(#256543,#256544),(#256545,#256546),(#256547,#256548),(#256549,#256550),
(#256551,#256552),(#256553,#256554),(#256555,#256556),(#256557,#256558),
(#256559,#256560),(#256561,#256562),(#256563,#256564),(#256565,#256566),
(#256567,#256568),(#256569,#256570),(#256571,#256572),(#256573,#256574),
(#256575,#256576),(#256577,#256578),(#256579,#256580),(#256581,#256582),
(#256583,#256584),(#256585,#256586),(#256587,#256588),(#256589,#256590),
(#256591,#256592),(#256593,#256594),(#256595,#256596),(#256597,#256598),
(#256599,#256600),(#256601,#256602),(#256603,#256604),(#256605,#256606),
(#256607,#256608),(#256609,#256610),(#256611,#256612),(#256613,#256614),
(#256615,#256616),(#256617,#256618),(#256619,#256620),(#256621,#256622),
(#256623,#256624),(#256625,#256626),(#256627,#256628),(#256629,#256630),
(#256631,#256632),(#256633,#256634),(#256635,#256636),(#256637,#256638),
(#256639,#256640),(#256641,#256642),(#256643,#256644),(#256645,#256646),
(#256647,#256648),(#256649,#256650),(#256651,#256652),(#256653,#256654),
(#256655,#256656),(#256657,#256658),(#256659,#256660),(#256661,#256662),
(#256663,#256664),(#256665,#256666),(#256667,#256668),(#256669,#256670),
(#256671,#256672),(#256673,#256674),(#256675,#256676),(#256677,#256678),
(#256679,#256680),(#256681,#256682),(#256683,#256684),(#256685,#256686),
(#256687,#256688),(#256689,#256690),(#256691,#256692),(#256693,#256694),
(#256695,#256696),(#256697,#256698),(#256699,#256700),(#256701,#256702),
(#256703,#256704),(#256705,#256706)),.UNSPECIFIED.,.F.,.F.,.F.,(6,1,1,1,
1,1,1,1,1,1,1,1,1,1,1,1,1,1,1,1,1,1,1,1,1,1,1,1,1,1,1,1,1,1,1,1,1,1,1,1,
1,1,1,1,1,1,1,1,1,1,1,1,1,1,1,1,1,1,1,1,1,1,1,1,1,1,1,1,1,1,1,1,1,1,1,1,
1,1,1,1,1,1,1,1,1,1,1,1,1,1,1,1,1,1,1,1,1,1,1,1,1,1,1,1,1,1,1,1,1,1,1,1,
1,1,1,1,1,1,1,1,1,1,1,1,1,1,1,1,1,1,1,1,1,1,1,1,1,1,1,1,1,1,1,1,1,1,1,1,
1,1,1,1,1,1,1,1,1,1,1,1,1,1,1,1,1,1,1,1,1,1,1,1,1,1,1,1,1,1,1,1,1,1,1,1,
1,1,1,1,1,1,1,1,1,1,1,1,1,1,1,1,1,1,1,1,1,1,1,1,1,1,1,1,1,1,1,1,1,1,1,1,
1,1,1,1,1,1,1,1,1,1,1,1,1,1,1,1,1,1,1,1,1,1,1,1,1,1,1,1,1,1,1,1,1,1,1,1,
1,1,1,1,1,1,1,1,1,1,1,1,1,1,1,1,1,1,1,1,1,1,1,1,1,1,1,1,1,1,1,1,1,1,1,1,
1,1,1,1,1,1,1,1,1,1,1,1,1,1,1,1,1,1,1,1,1,1,1,1,1,1,1,1,1,1,1,1,1,1,1,1,
1,1,1,1,1,1,1,1,1,1,1,1,1,1,1,1,1,1,1,1,1,1,1,1,1,1,1,1,1,1,1,1,1,1,1,1,
1,1,1,1,1,1,1,1,1,1,1,1,1,1,1,1,1,1,1,1,1,1,1,1,1,1,1,1,1,1,1,1,1,1,1,1,
1,1,1,1,1,1,1,1,1,1,1,1,1,1,1,1,1,1,1,1,1,1,1,1,1,1,1,1,1,1,1,1,1,1,1,1,
1,1,1,1,1,1,1,1,1,1,1,1,1,1,1,1,1,1,1,1,1,1,1,1,1,1,1,1,1,1,1,6),(2,2),
(-1.,-0.998165138,-0.996330275,-0.994495413,-0.99266055,-0.990825688,-0.988990826,
-0.987155963,-0.985321101,-0.983486239,-0.981651376,-0.979816514,-0.977981651,
-0.976146789,-0.974311927,-0.972477064,-0.970642202,-0.968807339,-0.966972477,
-0.965137615,-0.963302752,-0.96146789,-0.959633028,-0.957798165,-0.955963303,
-0.95412844,-0.952293578,-0.950458716,-0.948623853,-0.946788991,-0.944954128,
-0.943119266,-0.941284404,-0.939449541,-0.937614679,-0.935779817,-0.933944954,
-0.932110092,-0.930275229,-0.928440367,-0.926605505,-0.924770642,-0.92293578,
-0.921100917,-0.919266055,-0.917431193,-0.91559633,-0.913761468,-0.911926606,
-0.910091743,-0.908256881,-0.906422018,-0.904587156,-0.902752294,-0.900917431,
-0.899082569,-0.897247706,-0.895412844,-0.893577982,-0.891743119,-0.889908257,
-0.888073394,-0.886238532,-0.88440367,-0.882568807,-0.880733945,-0.878899083,
-0.87706422,-0.875229358,-0.873394495,-0.871559633,-0.869724771,-0.867889908,
-0.866055046,-0.864220183,-0.862385321,-0.860550459,-0.858715596,-0.856880734,
-0.855045872,-0.853211009,-0.851376147,-0.849541284,-0.847706422,-0.84587156,
-0.844036697,-0.842201835,-0.840366972,-0.83853211,-0.836697248,-0.834862385,
-0.833027523,-0.831192661,-0.829357798,-0.827522936,-0.825688073,-0.823853211,
-0.822018349,-0.820183486,-0.818348624,-0.816513761,-0.814678899,-0.812844037,
-0.811009174,-0.809174312,-0.80733945,-0.805504587,-0.803669725,-0.801834862,
-0.8,-0.798165138,-0.796330275,-0.794495413,-0.79266055,-0.790825688,-0.788990826,
-0.787155963,-0.785321101,-0.783486239,-0.781651376,-0.779816514,-0.777981651,
-0.776146789,-0.774311927,-0.772477064,-0.770642202,-0.768807339,-0.766972477,
-0.765137615,-0.763302752,-0.76146789,-0.759633028,-0.757798165,-0.755963303,
-0.75412844,-0.752293578,-0.750458716,-0.748623853,-0.746788991,-0.744954128,
-0.743119266,-0.741284404,-0.739449541,-0.737614679,-0.735779817,-0.733944954,
-0.732110092,-0.730275229,-0.728440367,-0.726605505,-0.724770642,-0.72293578,
-0.721100917,-0.719266055,-0.717431193,-0.71559633,-0.713761468,-0.711926606,
-0.710091743,-0.708256881,-0.706422018,-0.704587156,-0.702752294,-0.700917431,
-0.699082569,-0.697247706,-0.695412844,-0.693577982,-0.691743119,-0.689908257,
-0.688073394,-0.686238532,-0.68440367,-0.682568807,-0.680733945,-0.678899083,
-0.67706422,-0.675229358,-0.673394495,-0.671559633,-0.669724771,-0.667889908,
-0.666055046,-0.664220183,-0.662385321,-0.660550459,-0.658715596,-0.656880734,
-0.655045872,-0.653211009,-0.651376147,-0.649541284,-0.647706422,-0.64587156,
-0.644036697,-0.642201835,-0.640366972,-0.63853211,-0.636697248,-0.634862385,
-0.633027523,-0.631192661,-0.629357798,-0.627522936,-0.625688073,-0.623853211,
-0.622018349,-0.620183486,-0.618348624,-0.616513761,-0.614678899,-0.612844037,
-0.611009174,-0.609174312,-0.60733945,-0.605504587,-0.603669725,-0.601834862,
-0.6,-0.598165138,-0.596330275,-0.594495413,-0.59266055,-0.590825688,-0.588990826,
-0.587155963,-0.585321101,-0.583486239,-0.581651376,-0.579816514,-0.577981651,
-0.576146789,-0.574311927,-0.572477064,-0.570642202,-0.568807339,-0.566972477,
-0.565137615,-0.563302752,-0.56146789,-0.559633028,-0.557798165,-0.555963303,
-0.55412844,-0.552293578,-0.550458716,-0.548623853,-0.546788991,-0.544954128,
-0.543119266,-0.541284404,-0.539449541,-0.537614679,-0.535779817,-0.533944954,
-0.532110092,-0.530275229,-0.528440367,-0.526605505,-0.524770642,-0.52293578,
-0.521100917,-0.519266055,-0.517431193,-0.51559633,-0.513761468,-0.511926606,
-0.510091743,-0.508256881,-0.506422018,-0.504587156,-0.502752294,-0.500917431,
-0.499082569,-0.497247706,-0.495412844,-0.493577982,-0.491743119,-0.489908257,
-0.488073394,-0.486238532,-0.48440367,-0.482568807,-0.480733945,-0.478899083,
-0.47706422,-0.475229358,-0.473394495,-0.471559633,-0.469724771,-0.467889908,
-0.466055046,-0.464220183,-0.462385321,-0.460550459,-0.458715596,-0.456880734,
-0.455045872,-0.453211009,-0.451376147,-0.449541284,-0.447706422,-0.44587156,
-0.444036697,-0.442201835,-0.440366972,-0.43853211,-0.436697248,-0.434862385,
-0.433027523,-0.431192661,-0.429357798,-0.427522936,-0.425688073,-0.423853211,
-0.422018349,-0.420183486,-0.418348624,-0.416513761,-0.414678899,-0.412844037,
-0.411009174,-0.409174312,-0.40733945,-0.405504587,-0.403669725,-0.401834862,
-0.4,-0.398165138,-0.396330275,-0.394495413,-0.39266055,-0.390825688,-0.388990826,
-0.387155963,-0.385321101,-0.383486239,-0.381651376,-0.379816514,-0.377981651,
-0.376146789,-0.374311927,-0.372477064,-0.370642202,-0.368807339,-0.366972477,
-0.365137615,-0.363302752,-0.36146789,-0.359633028,-0.357798165,-0.355963303,
-0.35412844,-0.352293578,-0.350458716,-0.348623853,-0.346788991,-0.344954128,
-0.343119266,-0.341284404,-0.339449541,-0.337614679,-0.335779817,-0.333944954,
-0.332110092,-0.330275229,-0.328440367,-0.326605505,-0.324770642,-0.32293578,
-0.321100917,-0.319266055,-0.317431193,-0.31559633,-0.313761468,-0.311926606,
-0.310091743,-0.308256881,-0.306422018,-0.304587156,-0.302752294,-0.300917431,
-0.299082569,-0.297247706,-0.295412844,-0.293577982,-0.291743119,-0.289908257,
-0.288073394,-0.286238532,-0.28440367,-0.282568807,-0.280733945,-0.278899083,
-0.27706422,-0.275229358,-0.273394495,-0.271559633,-0.269724771,-0.267889908,
-0.266055046,-0.264220183,-0.262385321,-0.260550459,-0.258715596,-0.256880734,
-0.255045872,-0.253211009,-0.251376147,-0.249541284,-0.247706422,-0.24587156,
-0.244036697,-0.242201835,-0.240366972,-0.23853211,-0.236697248,-0.234862385,
-0.233027523,-0.231192661,-0.229357798,-0.227522936,-0.225688073,-0.223853211,
-0.222018349,-0.220183486,-0.218348624,-0.216513761,-0.214678899,-0.212844037,
-0.211009174,-0.209174312,-0.20733945,-0.205504587,-0.203669725,-0.201834862,
-0.2,-0.198165138,-0.196330275,-0.194495413,-0.19266055,-0.190825688,-0.188990826,
-0.187155963,-0.185321101,-0.183486239,-0.181651376,-0.179816514,-0.177981651,
-0.176146789,-0.174311927,-0.172477064,-0.170642202,-0.168807339,-0.166972477,
-0.165137615,-0.163302752,-0.16146789,-0.159633028,-0.157798165,-0.155963303,
-0.15412844,-0.152293578,-0.150458716,-0.148623853,-0.146788991,-0.144954128,
-0.143172103),(0.,0.36),.UNSPECIFIED.);
#6278=B_SPLINE_SURFACE_WITH_KNOTS('',5,1,((#257339,#257340),(#257341,#257342),
(#257343,#257344),(#257345,#257346),(#257347,#257348),(#257349,#257350),
(#257351,#257352),(#257353,#257354),(#257355,#257356),(#257357,#257358),
(#257359,#257360),(#257361,#257362),(#257363,#257364),(#257365,#257366),
(#257367,#257368),(#257369,#257370),(#257371,#257372),(#257373,#257374),
(#257375,#257376),(#257377,#257378),(#257379,#257380),(#257381,#257382),
(#257383,#257384),(#257385,#257386),(#257387,#257388),(#257389,#257390),
(#257391,#257392),(#257393,#257394),(#257395,#257396),(#257397,#257398),
(#257399,#257400),(#257401,#257402),(#257403,#257404),(#257405,#257406),
(#257407,#257408),(#257409,#257410),(#257411,#257412),(#257413,#257414),
(#257415,#257416),(#257417,#257418),(#257419,#257420),(#257421,#257422),
(#257423,#257424),(#257425,#257426),(#257427,#257428),(#257429,#257430),
(#257431,#257432),(#257433,#257434),(#257435,#257436),(#257437,#257438),
(#257439,#257440),(#257441,#257442),(#257443,#257444),(#257445,#257446),
(#257447,#257448),(#257449,#257450),(#257451,#257452),(#257453,#257454),
(#257455,#257456),(#257457,#257458),(#257459,#257460),(#257461,#257462),
(#257463,#257464),(#257465,#257466),(#257467,#257468),(#257469,#257470),
(#257471,#257472),(#257473,#257474),(#257475,#257476),(#257477,#257478),
(#257479,#257480),(#257481,#257482),(#257483,#257484),(#257485,#257486),
(#257487,#257488),(#257489,#257490),(#257491,#257492),(#257493,#257494),
(#257495,#257496),(#257497,#257498),(#257499,#257500),(#257501,#257502),
(#257503,#257504),(#257505,#257506),(#257507,#257508),(#257509,#257510),
(#257511,#257512),(#257513,#257514),(#257515,#257516),(#257517,#257518),
(#257519,#257520),(#257521,#257522),(#257523,#257524),(#257525,#257526),
(#257527,#257528),(#257529,#257530),(#257531,#257532),(#257533,#257534),
(#257535,#257536),(#257537,#257538),(#257539,#257540),(#257541,#257542),
(#257543,#257544),(#257545,#257546),(#257547,#257548),(#257549,#257550),
(#257551,#257552),(#257553,#257554),(#257555,#257556),(#257557,#257558),
(#257559,#257560),(#257561,#257562),(#257563,#257564),(#257565,#257566),
(#257567,#257568),(#257569,#257570),(#257571,#257572),(#257573,#257574),
(#257575,#257576),(#257577,#257578),(#257579,#257580),(#257581,#257582),
(#257583,#257584),(#257585,#257586),(#257587,#257588),(#257589,#257590),
(#257591,#257592),(#257593,#257594),(#257595,#257596),(#257597,#257598),
(#257599,#257600),(#257601,#257602),(#257603,#257604),(#257605,#257606),
(#257607,#257608),(#257609,#257610),(#257611,#257612),(#257613,#257614),
(#257615,#257616),(#257617,#257618),(#257619,#257620),(#257621,#257622),
(#257623,#257624),(#257625,#257626),(#257627,#257628),(#257629,#257630),
(#257631,#257632),(#257633,#257634),(#257635,#257636),(#257637,#257638),
(#257639,#257640),(#257641,#257642),(#257643,#257644),(#257645,#257646),
(#257647,#257648),(#257649,#257650),(#257651,#257652),(#257653,#257654),
(#257655,#257656),(#257657,#257658),(#257659,#257660),(#257661,#257662),
(#257663,#257664),(#257665,#257666),(#257667,#257668),(#257669,#257670),
(#257671,#257672),(#257673,#257674),(#257675,#257676),(#257677,#257678),
(#257679,#257680),(#257681,#257682),(#257683,#257684),(#257685,#257686),
(#257687,#257688),(#257689,#257690),(#257691,#257692),(#257693,#257694),
(#257695,#257696),(#257697,#257698),(#257699,#257700),(#257701,#257702),
(#257703,#257704),(#257705,#257706),(#257707,#257708),(#257709,#257710),
(#257711,#257712),(#257713,#257714),(#257715,#257716),(#257717,#257718),
(#257719,#257720),(#257721,#257722),(#257723,#257724),(#257725,#257726),
(#257727,#257728),(#257729,#257730),(#257731,#257732),(#257733,#257734),
(#257735,#257736),(#257737,#257738),(#257739,#257740),(#257741,#257742),
(#257743,#257744),(#257745,#257746),(#257747,#257748),(#257749,#257750),
(#257751,#257752),(#257753,#257754),(#257755,#257756),(#257757,#257758),
(#257759,#257760),(#257761,#257762),(#257763,#257764),(#257765,#257766),
(#257767,#257768),(#257769,#257770),(#257771,#257772),(#257773,#257774),
(#257775,#257776),(#257777,#257778),(#257779,#257780),(#257781,#257782),
(#257783,#257784),(#257785,#257786),(#257787,#257788),(#257789,#257790),
(#257791,#257792),(#257793,#257794),(#257795,#257796),(#257797,#257798),
(#257799,#257800),(#257801,#257802),(#257803,#257804),(#257805,#257806),
(#257807,#257808),(#257809,#257810),(#257811,#257812),(#257813,#257814),
(#257815,#257816),(#257817,#257818),(#257819,#257820),(#257821,#257822),
(#257823,#257824),(#257825,#257826),(#257827,#257828),(#257829,#257830),
(#257831,#257832),(#257833,#257834),(#257835,#257836),(#257837,#257838),
(#257839,#257840),(#257841,#257842),(#257843,#257844),(#257845,#257846),
(#257847,#257848),(#257849,#257850),(#257851,#257852),(#257853,#257854),
(#257855,#257856),(#257857,#257858),(#257859,#257860),(#257861,#257862),
(#257863,#257864),(#257865,#257866),(#257867,#257868),(#257869,#257870),
(#257871,#257872),(#257873,#257874),(#257875,#257876),(#257877,#257878),
(#257879,#257880),(#257881,#257882),(#257883,#257884),(#257885,#257886),
(#257887,#257888),(#257889,#257890),(#257891,#257892),(#257893,#257894),
(#257895,#257896),(#257897,#257898),(#257899,#257900),(#257901,#257902),
(#257903,#257904),(#257905,#257906),(#257907,#257908),(#257909,#257910),
(#257911,#257912),(#257913,#257914),(#257915,#257916),(#257917,#257918),
(#257919,#257920),(#257921,#257922),(#257923,#257924),(#257925,#257926),
(#257927,#257928),(#257929,#257930),(#257931,#257932),(#257933,#257934),
(#257935,#257936),(#257937,#257938),(#257939,#257940),(#257941,#257942),
(#257943,#257944),(#257945,#257946),(#257947,#257948),(#257949,#257950),
(#257951,#257952),(#257953,#257954),(#257955,#257956),(#257957,#257958),
(#257959,#257960),(#257961,#257962),(#257963,#257964),(#257965,#257966),
(#257967,#257968),(#257969,#257970),(#257971,#257972),(#257973,#257974),
(#257975,#257976),(#257977,#257978),(#257979,#257980),(#257981,#257982),
(#257983,#257984),(#257985,#257986),(#257987,#257988),(#257989,#257990),
(#257991,#257992),(#257993,#257994),(#257995,#257996),(#257997,#257998),
(#257999,#258000),(#258001,#258002),(#258003,#258004),(#258005,#258006),
(#258007,#258008),(#258009,#258010),(#258011,#258012),(#258013,#258014),
(#258015,#258016),(#258017,#258018),(#258019,#258020),(#258021,#258022),
(#258023,#258024),(#258025,#258026),(#258027,#258028),(#258029,#258030),
(#258031,#258032),(#258033,#258034),(#258035,#258036),(#258037,#258038),
(#258039,#258040),(#258041,#258042),(#258043,#258044),(#258045,#258046),
(#258047,#258048),(#258049,#258050),(#258051,#258052),(#258053,#258054),
(#258055,#258056),(#258057,#258058),(#258059,#258060),(#258061,#258062),
(#258063,#258064),(#258065,#258066),(#258067,#258068),(#258069,#258070),
(#258071,#258072),(#258073,#258074),(#258075,#258076),(#258077,#258078),
(#258079,#258080),(#258081,#258082),(#258083,#258084),(#258085,#258086),
(#258087,#258088),(#258089,#258090),(#258091,#258092),(#258093,#258094),
(#258095,#258096),(#258097,#258098),(#258099,#258100),(#258101,#258102),
(#258103,#258104),(#258105,#258106),(#258107,#258108),(#258109,#258110),
(#258111,#258112),(#258113,#258114),(#258115,#258116),(#258117,#258118),
(#258119,#258120),(#258121,#258122),(#258123,#258124),(#258125,#258126),
(#258127,#258128),(#258129,#258130),(#258131,#258132),(#258133,#258134),
(#258135,#258136),(#258137,#258138),(#258139,#258140),(#258141,#258142),
(#258143,#258144),(#258145,#258146),(#258147,#258148),(#258149,#258150),
(#258151,#258152),(#258153,#258154),(#258155,#258156),(#258157,#258158),
(#258159,#258160),(#258161,#258162),(#258163,#258164),(#258165,#258166),
(#258167,#258168),(#258169,#258170),(#258171,#258172),(#258173,#258174),
(#258175,#258176),(#258177,#258178),(#258179,#258180),(#258181,#258182),
(#258183,#258184),(#258185,#258186),(#258187,#258188),(#258189,#258190),
(#258191,#258192),(#258193,#258194),(#258195,#258196),(#258197,#258198),
(#258199,#258200),(#258201,#258202),(#258203,#258204),(#258205,#258206),
(#258207,#258208),(#258209,#258210),(#258211,#258212),(#258213,#258214),
(#258215,#258216),(#258217,#258218),(#258219,#258220),(#258221,#258222),
(#258223,#258224),(#258225,#258226),(#258227,#258228),(#258229,#258230),
(#258231,#258232),(#258233,#258234),(#258235,#258236),(#258237,#258238),
(#258239,#258240),(#258241,#258242),(#258243,#258244),(#258245,#258246),
(#258247,#258248),(#258249,#258250),(#258251,#258252),(#258253,#258254),
(#258255,#258256),(#258257,#258258),(#258259,#258260),(#258261,#258262),
(#258263,#258264),(#258265,#258266),(#258267,#258268),(#258269,#258270),
(#258271,#258272),(#258273,#258274),(#258275,#258276),(#258277,#258278),
(#258279,#258280),(#258281,#258282)),.UNSPECIFIED.,.F.,.F.,.F.,(6,1,1,1,
1,1,1,1,1,1,1,1,1,1,1,1,1,1,1,1,1,1,1,1,1,1,1,1,1,1,1,1,1,1,1,1,1,1,1,1,
1,1,1,1,1,1,1,1,1,1,1,1,1,1,1,1,1,1,1,1,1,1,1,1,1,1,1,1,1,1,1,1,1,1,1,1,
1,1,1,1,1,1,1,1,1,1,1,1,1,1,1,1,1,1,1,1,1,1,1,1,1,1,1,1,1,1,1,1,1,1,1,1,
1,1,1,1,1,1,1,1,1,1,1,1,1,1,1,1,1,1,1,1,1,1,1,1,1,1,1,1,1,1,1,1,1,1,1,1,
1,1,1,1,1,1,1,1,1,1,1,1,1,1,1,1,1,1,1,1,1,1,1,1,1,1,1,1,1,1,1,1,1,1,1,1,
1,1,1,1,1,1,1,1,1,1,1,1,1,1,1,1,1,1,1,1,1,1,1,1,1,1,1,1,1,1,1,1,1,1,1,1,
1,1,1,1,1,1,1,1,1,1,1,1,1,1,1,1,1,1,1,1,1,1,1,1,1,1,1,1,1,1,1,1,1,1,1,1,
1,1,1,1,1,1,1,1,1,1,1,1,1,1,1,1,1,1,1,1,1,1,1,1,1,1,1,1,1,1,1,1,1,1,1,1,
1,1,1,1,1,1,1,1,1,1,1,1,1,1,1,1,1,1,1,1,1,1,1,1,1,1,1,1,1,1,1,1,1,1,1,1,
1,1,1,1,1,1,1,1,1,1,1,1,1,1,1,1,1,1,1,1,1,1,1,1,1,1,1,1,1,1,1,1,1,1,1,1,
1,1,1,1,1,1,1,1,1,1,1,1,1,1,1,1,1,1,1,1,1,1,1,1,1,1,1,1,1,1,1,1,1,1,1,1,
1,1,1,1,1,1,1,1,1,1,1,1,1,1,1,1,1,1,1,1,1,1,1,1,1,1,1,1,1,1,1,1,1,1,1,1,
1,1,1,1,1,1,1,1,1,1,1,1,1,1,1,1,1,1,1,1,1,1,1,1,1,1,1,1,1,1,1,6),(2,2),
(0.143172104,0.144954128,0.146788991,0.148623853,0.150458716,0.152293578,
0.15412844,0.155963303,0.157798165,0.159633028,0.16146789,0.163302752,0.165137615,
0.166972477,0.168807339,0.170642202,0.172477064,0.174311927,0.176146789,
0.177981651,0.179816514,0.181651376,0.183486239,0.185321101,0.187155963,
0.188990826,0.190825688,0.19266055,0.194495413,0.196330275,0.198165138,
0.2,0.201834862,0.203669725,0.205504587,0.20733945,0.209174312,0.211009174,
0.212844037,0.214678899,0.216513761,0.218348624,0.220183486,0.222018349,
0.223853211,0.225688073,0.227522936,0.229357798,0.231192661,0.233027523,
0.234862385,0.236697248,0.23853211,0.240366972,0.242201835,0.244036697,
0.24587156,0.247706422,0.249541284,0.251376147,0.253211009,0.255045872,
0.256880734,0.258715596,0.260550459,0.262385321,0.264220183,0.266055046,
0.267889908,0.269724771,0.271559633,0.273394495,0.275229358,0.27706422,
0.278899083,0.280733945,0.282568807,0.28440367,0.286238532,0.288073394,
0.289908257,0.291743119,0.293577982,0.295412844,0.297247706,0.299082569,
0.300917431,0.302752294,0.304587156,0.306422018,0.308256881,0.310091743,
0.311926606,0.313761468,0.31559633,0.317431193,0.319266055,0.321100917,
0.32293578,0.324770642,0.326605505,0.328440367,0.330275229,0.332110092,
0.333944954,0.335779817,0.337614679,0.339449541,0.341284404,0.343119266,
0.344954128,0.346788991,0.348623853,0.350458716,0.352293578,0.35412844,
0.355963303,0.357798165,0.359633028,0.36146789,0.363302752,0.365137615,
0.366972477,0.368807339,0.370642202,0.372477064,0.374311927,0.376146789,
0.377981651,0.379816514,0.381651376,0.383486239,0.385321101,0.387155963,
0.388990826,0.390825688,0.39266055,0.394495413,0.396330275,0.398165138,
0.4,0.401834862,0.403669725,0.405504587,0.40733945,0.409174312,0.411009174,
0.412844037,0.414678899,0.416513761,0.418348624,0.420183486,0.422018349,
0.423853211,0.425688073,0.427522936,0.429357798,0.431192661,0.433027523,
0.434862385,0.436697248,0.43853211,0.440366972,0.442201835,0.444036697,
0.44587156,0.447706422,0.449541284,0.451376147,0.453211009,0.455045872,
0.456880734,0.458715596,0.460550459,0.462385321,0.464220183,0.466055046,
0.467889908,0.469724771,0.471559633,0.473394495,0.475229358,0.47706422,
0.478899083,0.480733945,0.482568807,0.48440367,0.486238532,0.488073394,
0.489908257,0.491743119,0.493577982,0.495412844,0.497247706,0.499082569,
0.500917431,0.502752294,0.504587156,0.506422018,0.508256881,0.510091743,
0.511926606,0.513761468,0.51559633,0.517431193,0.519266055,0.521100917,
0.52293578,0.524770642,0.526605505,0.528440367,0.530275229,0.532110092,
0.533944954,0.535779817,0.537614679,0.539449541,0.541284404,0.543119266,
0.544954128,0.546788991,0.548623853,0.550458716,0.552293578,0.55412844,
0.555963303,0.557798165,0.559633028,0.56146789,0.563302752,0.565137615,
0.566972477,0.568807339,0.570642202,0.572477064,0.574311927,0.576146789,
0.577981651,0.579816514,0.581651376,0.583486239,0.585321101,0.587155963,
0.588990826,0.590825688,0.59266055,0.594495413,0.596330275,0.598165138,
0.6,0.601834862,0.603669725,0.605504587,0.60733945,0.609174312,0.611009174,
0.612844037,0.614678899,0.616513761,0.618348624,0.620183486,0.622018349,
0.623853211,0.625688073,0.627522936,0.629357798,0.631192661,0.633027523,
0.634862385,0.636697248,0.63853211,0.640366972,0.642201835,0.644036697,
0.64587156,0.647706422,0.649541284,0.651376147,0.653211009,0.655045872,
0.656880734,0.658715596,0.660550459,0.662385321,0.664220183,0.666055046,
0.667889908,0.669724771,0.671559633,0.673394495,0.675229358,0.67706422,
0.678899083,0.680733945,0.682568807,0.68440367,0.686238532,0.688073394,
0.689908257,0.691743119,0.693577982,0.695412844,0.697247706,0.699082569,
0.700917431,0.702752294,0.704587156,0.706422018,0.708256881,0.710091743,
0.711926606,0.713761468,0.71559633,0.717431193,0.719266055,0.721100917,
0.72293578,0.724770642,0.726605505,0.728440367,0.730275229,0.732110092,
0.733944954,0.735779817,0.737614679,0.739449541,0.741284404,0.743119266,
0.744954128,0.746788991,0.748623853,0.750458716,0.752293578,0.75412844,
0.755963303,0.757798165,0.759633028,0.76146789,0.763302752,0.765137615,
0.766972477,0.768807339,0.770642202,0.772477064,0.774311927,0.776146789,
0.777981651,0.779816514,0.781651376,0.783486239,0.785321101,0.787155963,
0.788990826,0.790825688,0.79266055,0.794495413,0.796330275,0.798165138,
0.8,0.801834862,0.803669725,0.805504587,0.80733945,0.809174312,0.811009174,
0.812844037,0.814678899,0.816513761,0.818348624,0.820183486,0.822018349,
0.823853211,0.825688073,0.827522936,0.829357798,0.831192661,0.833027523,
0.834862385,0.836697248,0.83853211,0.840366972,0.842201835,0.844036697,
0.84587156,0.847706422,0.849541284,0.851376147,0.853211009,0.855045872,
0.856880734,0.858715596,0.860550459,0.862385321,0.864220183,0.866055046,
0.867889908,0.869724771,0.871559633,0.873394495,0.875229358,0.87706422,
0.878899083,0.880733945,0.882568807,0.88440367,0.886238532,0.888073394,
0.889908257,0.891743119,0.893577982,0.895412844,0.897247706,0.899082569,
0.900917431,0.902752294,0.904587156,0.906422018,0.908256881,0.910091743,
0.911926606,0.913761468,0.91559633,0.917431193,0.919266055,0.921100917,
0.92293578,0.924770642,0.926605505,0.928440367,0.930275229,0.932110092,
0.933944954,0.935779817,0.937614679,0.939449541,0.941284404,0.943119266,
0.944954128,0.946788991,0.948623853,0.950458716,0.952293578,0.95412844,
0.955963303,0.957798165,0.959633028,0.96146789,0.963302752,0.965137615,
0.966972477,0.968807339,0.970642202,0.972477064,0.974311927,0.976146789,
0.977981651,0.979816514,0.981651376,0.983486239,0.985321101,0.987155963,
0.988990826,0.990825688,0.99266055,0.994495413,0.996330275,0.998165138,
1.),(0.,0.36),.UNSPECIFIED.);
#6279=B_SPLINE_SURFACE_WITH_KNOTS('',5,1,((#258912,#258913),(#258914,#258915),
(#258916,#258917),(#258918,#258919),(#258920,#258921),(#258922,#258923),
(#258924,#258925),(#258926,#258927),(#258928,#258929),(#258930,#258931),
(#258932,#258933),(#258934,#258935),(#258936,#258937),(#258938,#258939),
(#258940,#258941),(#258942,#258943),(#258944,#258945),(#258946,#258947),
(#258948,#258949),(#258950,#258951),(#258952,#258953),(#258954,#258955),
(#258956,#258957),(#258958,#258959),(#258960,#258961),(#258962,#258963),
(#258964,#258965),(#258966,#258967),(#258968,#258969),(#258970,#258971),
(#258972,#258973),(#258974,#258975),(#258976,#258977),(#258978,#258979),
(#258980,#258981),(#258982,#258983),(#258984,#258985),(#258986,#258987),
(#258988,#258989),(#258990,#258991),(#258992,#258993),(#258994,#258995),
(#258996,#258997),(#258998,#258999),(#259000,#259001),(#259002,#259003),
(#259004,#259005),(#259006,#259007),(#259008,#259009),(#259010,#259011),
(#259012,#259013),(#259014,#259015),(#259016,#259017),(#259018,#259019),
(#259020,#259021),(#259022,#259023),(#259024,#259025),(#259026,#259027),
(#259028,#259029),(#259030,#259031),(#259032,#259033),(#259034,#259035),
(#259036,#259037),(#259038,#259039),(#259040,#259041),(#259042,#259043),
(#259044,#259045),(#259046,#259047),(#259048,#259049),(#259050,#259051),
(#259052,#259053),(#259054,#259055),(#259056,#259057),(#259058,#259059),
(#259060,#259061),(#259062,#259063),(#259064,#259065),(#259066,#259067),
(#259068,#259069),(#259070,#259071),(#259072,#259073),(#259074,#259075),
(#259076,#259077),(#259078,#259079),(#259080,#259081),(#259082,#259083),
(#259084,#259085),(#259086,#259087),(#259088,#259089),(#259090,#259091),
(#259092,#259093),(#259094,#259095),(#259096,#259097),(#259098,#259099),
(#259100,#259101),(#259102,#259103),(#259104,#259105),(#259106,#259107),
(#259108,#259109),(#259110,#259111),(#259112,#259113),(#259114,#259115),
(#259116,#259117),(#259118,#259119),(#259120,#259121),(#259122,#259123),
(#259124,#259125),(#259126,#259127),(#259128,#259129),(#259130,#259131),
(#259132,#259133),(#259134,#259135),(#259136,#259137),(#259138,#259139),
(#259140,#259141),(#259142,#259143),(#259144,#259145),(#259146,#259147),
(#259148,#259149),(#259150,#259151),(#259152,#259153),(#259154,#259155),
(#259156,#259157),(#259158,#259159),(#259160,#259161),(#259162,#259163),
(#259164,#259165),(#259166,#259167),(#259168,#259169),(#259170,#259171),
(#259172,#259173),(#259174,#259175),(#259176,#259177),(#259178,#259179),
(#259180,#259181),(#259182,#259183),(#259184,#259185),(#259186,#259187),
(#259188,#259189),(#259190,#259191),(#259192,#259193),(#259194,#259195),
(#259196,#259197),(#259198,#259199),(#259200,#259201),(#259202,#259203),
(#259204,#259205),(#259206,#259207),(#259208,#259209),(#259210,#259211),
(#259212,#259213),(#259214,#259215),(#259216,#259217),(#259218,#259219),
(#259220,#259221),(#259222,#259223),(#259224,#259225),(#259226,#259227),
(#259228,#259229),(#259230,#259231),(#259232,#259233),(#259234,#259235),
(#259236,#259237),(#259238,#259239),(#259240,#259241),(#259242,#259243),
(#259244,#259245),(#259246,#259247),(#259248,#259249),(#259250,#259251),
(#259252,#259253),(#259254,#259255),(#259256,#259257),(#259258,#259259),
(#259260,#259261),(#259262,#259263),(#259264,#259265),(#259266,#259267),
(#259268,#259269),(#259270,#259271),(#259272,#259273),(#259274,#259275),
(#259276,#259277),(#259278,#259279),(#259280,#259281),(#259282,#259283),
(#259284,#259285),(#259286,#259287),(#259288,#259289),(#259290,#259291),
(#259292,#259293),(#259294,#259295),(#259296,#259297),(#259298,#259299),
(#259300,#259301),(#259302,#259303),(#259304,#259305),(#259306,#259307),
(#259308,#259309),(#259310,#259311),(#259312,#259313),(#259314,#259315),
(#259316,#259317),(#259318,#259319),(#259320,#259321),(#259322,#259323),
(#259324,#259325),(#259326,#259327),(#259328,#259329),(#259330,#259331),
(#259332,#259333),(#259334,#259335),(#259336,#259337),(#259338,#259339),
(#259340,#259341),(#259342,#259343),(#259344,#259345),(#259346,#259347),
(#259348,#259349),(#259350,#259351),(#259352,#259353),(#259354,#259355),
(#259356,#259357),(#259358,#259359),(#259360,#259361),(#259362,#259363),
(#259364,#259365),(#259366,#259367),(#259368,#259369),(#259370,#259371),
(#259372,#259373),(#259374,#259375),(#259376,#259377),(#259378,#259379),
(#259380,#259381),(#259382,#259383),(#259384,#259385),(#259386,#259387),
(#259388,#259389),(#259390,#259391),(#259392,#259393),(#259394,#259395),
(#259396,#259397),(#259398,#259399),(#259400,#259401),(#259402,#259403),
(#259404,#259405),(#259406,#259407),(#259408,#259409),(#259410,#259411),
(#259412,#259413),(#259414,#259415),(#259416,#259417),(#259418,#259419),
(#259420,#259421),(#259422,#259423),(#259424,#259425),(#259426,#259427),
(#259428,#259429),(#259430,#259431),(#259432,#259433),(#259434,#259435),
(#259436,#259437),(#259438,#259439),(#259440,#259441),(#259442,#259443),
(#259444,#259445),(#259446,#259447),(#259448,#259449),(#259450,#259451),
(#259452,#259453),(#259454,#259455),(#259456,#259457),(#259458,#259459),
(#259460,#259461),(#259462,#259463),(#259464,#259465),(#259466,#259467),
(#259468,#259469),(#259470,#259471),(#259472,#259473),(#259474,#259475),
(#259476,#259477),(#259478,#259479),(#259480,#259481),(#259482,#259483),
(#259484,#259485),(#259486,#259487),(#259488,#259489),(#259490,#259491),
(#259492,#259493),(#259494,#259495),(#259496,#259497),(#259498,#259499),
(#259500,#259501),(#259502,#259503),(#259504,#259505),(#259506,#259507),
(#259508,#259509),(#259510,#259511),(#259512,#259513),(#259514,#259515),
(#259516,#259517),(#259518,#259519),(#259520,#259521),(#259522,#259523),
(#259524,#259525),(#259526,#259527),(#259528,#259529),(#259530,#259531),
(#259532,#259533),(#259534,#259535),(#259536,#259537),(#259538,#259539),
(#259540,#259541),(#259542,#259543),(#259544,#259545),(#259546,#259547),
(#259548,#259549),(#259550,#259551),(#259552,#259553),(#259554,#259555),
(#259556,#259557),(#259558,#259559),(#259560,#259561),(#259562,#259563),
(#259564,#259565),(#259566,#259567),(#259568,#259569),(#259570,#259571),
(#259572,#259573),(#259574,#259575),(#259576,#259577),(#259578,#259579),
(#259580,#259581),(#259582,#259583),(#259584,#259585),(#259586,#259587),
(#259588,#259589),(#259590,#259591),(#259592,#259593),(#259594,#259595),
(#259596,#259597),(#259598,#259599),(#259600,#259601),(#259602,#259603),
(#259604,#259605),(#259606,#259607),(#259608,#259609),(#259610,#259611),
(#259612,#259613),(#259614,#259615),(#259616,#259617),(#259618,#259619),
(#259620,#259621),(#259622,#259623),(#259624,#259625),(#259626,#259627),
(#259628,#259629),(#259630,#259631),(#259632,#259633),(#259634,#259635),
(#259636,#259637),(#259638,#259639),(#259640,#259641),(#259642,#259643),
(#259644,#259645),(#259646,#259647),(#259648,#259649),(#259650,#259651),
(#259652,#259653),(#259654,#259655),(#259656,#259657),(#259658,#259659),
(#259660,#259661),(#259662,#259663),(#259664,#259665),(#259666,#259667),
(#259668,#259669),(#259670,#259671),(#259672,#259673),(#259674,#259675),
(#259676,#259677),(#259678,#259679),(#259680,#259681),(#259682,#259683),
(#259684,#259685),(#259686,#259687),(#259688,#259689),(#259690,#259691),
(#259692,#259693),(#259694,#259695),(#259696,#259697),(#259698,#259699),
(#259700,#259701),(#259702,#259703),(#259704,#259705),(#259706,#259707),
(#259708,#259709),(#259710,#259711),(#259712,#259713),(#259714,#259715),
(#259716,#259717),(#259718,#259719),(#259720,#259721),(#259722,#259723),
(#259724,#259725),(#259726,#259727),(#259728,#259729),(#259730,#259731),
(#259732,#259733),(#259734,#259735),(#259736,#259737),(#259738,#259739),
(#259740,#259741),(#259742,#259743),(#259744,#259745),(#259746,#259747),
(#259748,#259749),(#259750,#259751),(#259752,#259753),(#259754,#259755),
(#259756,#259757),(#259758,#259759),(#259760,#259761),(#259762,#259763),
(#259764,#259765),(#259766,#259767),(#259768,#259769),(#259770,#259771),
(#259772,#259773),(#259774,#259775),(#259776,#259777),(#259778,#259779),
(#259780,#259781),(#259782,#259783),(#259784,#259785),(#259786,#259787),
(#259788,#259789),(#259790,#259791),(#259792,#259793),(#259794,#259795),
(#259796,#259797),(#259798,#259799),(#259800,#259801),(#259802,#259803),
(#259804,#259805),(#259806,#259807),(#259808,#259809),(#259810,#259811),
(#259812,#259813),(#259814,#259815),(#259816,#259817),(#259818,#259819),
(#259820,#259821),(#259822,#259823),(#259824,#259825),(#259826,#259827),
(#259828,#259829),(#259830,#259831),(#259832,#259833),(#259834,#259835),
(#259836,#259837),(#259838,#259839),(#259840,#259841),(#259842,#259843),
(#259844,#259845),(#259846,#259847),(#259848,#259849),(#259850,#259851),
(#259852,#259853),(#259854,#259855)),.UNSPECIFIED.,.F.,.F.,.F.,(6,1,1,1,
1,1,1,1,1,1,1,1,1,1,1,1,1,1,1,1,1,1,1,1,1,1,1,1,1,1,1,1,1,1,1,1,1,1,1,1,
1,1,1,1,1,1,1,1,1,1,1,1,1,1,1,1,1,1,1,1,1,1,1,1,1,1,1,1,1,1,1,1,1,1,1,1,
1,1,1,1,1,1,1,1,1,1,1,1,1,1,1,1,1,1,1,1,1,1,1,1,1,1,1,1,1,1,1,1,1,1,1,1,
1,1,1,1,1,1,1,1,1,1,1,1,1,1,1,1,1,1,1,1,1,1,1,1,1,1,1,1,1,1,1,1,1,1,1,1,
1,1,1,1,1,1,1,1,1,1,1,1,1,1,1,1,1,1,1,1,1,1,1,1,1,1,1,1,1,1,1,1,1,1,1,1,
1,1,1,1,1,1,1,1,1,1,1,1,1,1,1,1,1,1,1,1,1,1,1,1,1,1,1,1,1,1,1,1,1,1,1,1,
1,1,1,1,1,1,1,1,1,1,1,1,1,1,1,1,1,1,1,1,1,1,1,1,1,1,1,1,1,1,1,1,1,1,1,1,
1,1,1,1,1,1,1,1,1,1,1,1,1,1,1,1,1,1,1,1,1,1,1,1,1,1,1,1,1,1,1,1,1,1,1,1,
1,1,1,1,1,1,1,1,1,1,1,1,1,1,1,1,1,1,1,1,1,1,1,1,1,1,1,1,1,1,1,1,1,1,1,1,
1,1,1,1,1,1,1,1,1,1,1,1,1,1,1,1,1,1,1,1,1,1,1,1,1,1,1,1,1,1,1,1,1,1,1,1,
1,1,1,1,1,1,1,1,1,1,1,1,1,1,1,1,1,1,1,1,1,1,1,1,1,1,1,1,1,1,1,1,1,1,1,1,
1,1,1,1,1,1,1,1,1,1,1,1,1,1,1,1,1,1,1,1,1,1,1,1,1,1,1,1,1,1,1,1,1,1,1,1,
1,1,1,1,1,1,1,1,1,1,1,1,1,1,1,1,1,1,1,1,1,1,1,1,1,1,1,1,1,1,1,6),(2,2),
(0.143172104,0.144954128,0.146788991,0.148623853,0.150458716,0.152293578,
0.15412844,0.155963303,0.157798165,0.159633028,0.16146789,0.163302752,0.165137615,
0.166972477,0.168807339,0.170642202,0.172477064,0.174311927,0.176146789,
0.177981651,0.179816514,0.181651376,0.183486239,0.185321101,0.187155963,
0.188990826,0.190825688,0.19266055,0.194495413,0.196330275,0.198165138,
0.2,0.201834862,0.203669725,0.205504587,0.20733945,0.209174312,0.211009174,
0.212844037,0.214678899,0.216513761,0.218348624,0.220183486,0.222018349,
0.223853211,0.225688073,0.227522936,0.229357798,0.231192661,0.233027523,
0.234862385,0.236697248,0.23853211,0.240366972,0.242201835,0.244036697,
0.24587156,0.247706422,0.249541284,0.251376147,0.253211009,0.255045872,
0.256880734,0.258715596,0.260550459,0.262385321,0.264220183,0.266055046,
0.267889908,0.269724771,0.271559633,0.273394495,0.275229358,0.27706422,
0.278899083,0.280733945,0.282568807,0.28440367,0.286238532,0.288073394,
0.289908257,0.291743119,0.293577982,0.295412844,0.297247706,0.299082569,
0.300917431,0.302752294,0.304587156,0.306422018,0.308256881,0.310091743,
0.311926606,0.313761468,0.31559633,0.317431193,0.319266055,0.321100917,
0.32293578,0.324770642,0.326605505,0.328440367,0.330275229,0.332110092,
0.333944954,0.335779817,0.337614679,0.339449541,0.341284404,0.343119266,
0.344954128,0.346788991,0.348623853,0.350458716,0.352293578,0.35412844,
0.355963303,0.357798165,0.359633028,0.36146789,0.363302752,0.365137615,
0.366972477,0.368807339,0.370642202,0.372477064,0.374311927,0.376146789,
0.377981651,0.379816514,0.381651376,0.383486239,0.385321101,0.387155963,
0.388990826,0.390825688,0.39266055,0.394495413,0.396330275,0.398165138,
0.4,0.401834862,0.403669725,0.405504587,0.40733945,0.409174312,0.411009174,
0.412844037,0.414678899,0.416513761,0.418348624,0.420183486,0.422018349,
0.423853211,0.425688073,0.427522936,0.429357798,0.431192661,0.433027523,
0.434862385,0.436697248,0.43853211,0.440366972,0.442201835,0.444036697,
0.44587156,0.447706422,0.449541284,0.451376147,0.453211009,0.455045872,
0.456880734,0.458715596,0.460550459,0.462385321,0.464220183,0.466055046,
0.467889908,0.469724771,0.471559633,0.473394495,0.475229358,0.47706422,
0.478899083,0.480733945,0.482568807,0.48440367,0.486238532,0.488073394,
0.489908257,0.491743119,0.493577982,0.495412844,0.497247706,0.499082569,
0.500917431,0.502752294,0.504587156,0.506422018,0.508256881,0.510091743,
0.511926606,0.513761468,0.51559633,0.517431193,0.519266055,0.521100917,
0.52293578,0.524770642,0.526605505,0.528440367,0.530275229,0.532110092,
0.533944954,0.535779817,0.537614679,0.539449541,0.541284404,0.543119266,
0.544954128,0.546788991,0.548623853,0.550458716,0.552293578,0.55412844,
0.555963303,0.557798165,0.559633028,0.56146789,0.563302752,0.565137615,
0.566972477,0.568807339,0.570642202,0.572477064,0.574311927,0.576146789,
0.577981651,0.579816514,0.581651376,0.583486239,0.585321101,0.587155963,
0.588990826,0.590825688,0.59266055,0.594495413,0.596330275,0.598165138,
0.6,0.601834862,0.603669725,0.605504587,0.60733945,0.609174312,0.611009174,
0.612844037,0.614678899,0.616513761,0.618348624,0.620183486,0.622018349,
0.623853211,0.625688073,0.627522936,0.629357798,0.631192661,0.633027523,
0.634862385,0.636697248,0.63853211,0.640366972,0.642201835,0.644036697,
0.64587156,0.647706422,0.649541284,0.651376147,0.653211009,0.655045872,
0.656880734,0.658715596,0.660550459,0.662385321,0.664220183,0.666055046,
0.667889908,0.669724771,0.671559633,0.673394495,0.675229358,0.67706422,
0.678899083,0.680733945,0.682568807,0.68440367,0.686238532,0.688073394,
0.689908257,0.691743119,0.693577982,0.695412844,0.697247706,0.699082569,
0.700917431,0.702752294,0.704587156,0.706422018,0.708256881,0.710091743,
0.711926606,0.713761468,0.71559633,0.717431193,0.719266055,0.721100917,
0.72293578,0.724770642,0.726605505,0.728440367,0.730275229,0.732110092,
0.733944954,0.735779817,0.737614679,0.739449541,0.741284404,0.743119266,
0.744954128,0.746788991,0.748623853,0.750458716,0.752293578,0.75412844,
0.755963303,0.757798165,0.759633028,0.76146789,0.763302752,0.765137615,
0.766972477,0.768807339,0.770642202,0.772477064,0.774311927,0.776146789,
0.777981651,0.779816514,0.781651376,0.783486239,0.785321101,0.787155963,
0.788990826,0.790825688,0.79266055,0.794495413,0.796330275,0.798165138,
0.8,0.801834862,0.803669725,0.805504587,0.80733945,0.809174312,0.811009174,
0.812844037,0.814678899,0.816513761,0.818348624,0.820183486,0.822018349,
0.823853211,0.825688073,0.827522936,0.829357798,0.831192661,0.833027523,
0.834862385,0.836697248,0.83853211,0.840366972,0.842201835,0.844036697,
0.84587156,0.847706422,0.849541284,0.851376147,0.853211009,0.855045872,
0.856880734,0.858715596,0.860550459,0.862385321,0.864220183,0.866055046,
0.867889908,0.869724771,0.871559633,0.873394495,0.875229358,0.87706422,
0.878899083,0.880733945,0.882568807,0.88440367,0.886238532,0.888073394,
0.889908257,0.891743119,0.893577982,0.895412844,0.897247706,0.899082569,
0.900917431,0.902752294,0.904587156,0.906422018,0.908256881,0.910091743,
0.911926606,0.913761468,0.91559633,0.917431193,0.919266055,0.921100917,
0.92293578,0.924770642,0.926605505,0.928440367,0.930275229,0.932110092,
0.933944954,0.935779817,0.937614679,0.939449541,0.941284404,0.943119266,
0.944954128,0.946788991,0.948623853,0.950458716,0.952293578,0.95412844,
0.955963303,0.957798165,0.959633028,0.96146789,0.963302752,0.965137615,
0.966972477,0.968807339,0.970642202,0.972477064,0.974311927,0.976146789,
0.977981651,0.979816514,0.981651376,0.983486239,0.985321101,0.987155963,
0.988990826,0.990825688,0.99266055,0.994495413,0.996330275,0.998165138,
1.),(0.,0.36),.UNSPECIFIED.);
#6280=B_SPLINE_SURFACE_WITH_KNOTS('',5,1,((#260798,#260799),(#260800,#260801),
(#260802,#260803),(#260804,#260805),(#260806,#260807),(#260808,#260809),
(#260810,#260811),(#260812,#260813),(#260814,#260815),(#260816,#260817),
(#260818,#260819),(#260820,#260821),(#260822,#260823),(#260824,#260825),
(#260826,#260827),(#260828,#260829),(#260830,#260831),(#260832,#260833),
(#260834,#260835),(#260836,#260837),(#260838,#260839),(#260840,#260841),
(#260842,#260843),(#260844,#260845),(#260846,#260847),(#260848,#260849),
(#260850,#260851),(#260852,#260853),(#260854,#260855),(#260856,#260857),
(#260858,#260859),(#260860,#260861),(#260862,#260863),(#260864,#260865),
(#260866,#260867),(#260868,#260869),(#260870,#260871),(#260872,#260873),
(#260874,#260875),(#260876,#260877),(#260878,#260879),(#260880,#260881),
(#260882,#260883),(#260884,#260885),(#260886,#260887),(#260888,#260889),
(#260890,#260891),(#260892,#260893),(#260894,#260895),(#260896,#260897),
(#260898,#260899),(#260900,#260901),(#260902,#260903),(#260904,#260905),
(#260906,#260907),(#260908,#260909),(#260910,#260911),(#260912,#260913),
(#260914,#260915),(#260916,#260917),(#260918,#260919),(#260920,#260921),
(#260922,#260923),(#260924,#260925),(#260926,#260927),(#260928,#260929),
(#260930,#260931),(#260932,#260933),(#260934,#260935),(#260936,#260937),
(#260938,#260939),(#260940,#260941),(#260942,#260943),(#260944,#260945),
(#260946,#260947),(#260948,#260949),(#260950,#260951),(#260952,#260953),
(#260954,#260955),(#260956,#260957),(#260958,#260959),(#260960,#260961),
(#260962,#260963),(#260964,#260965),(#260966,#260967),(#260968,#260969),
(#260970,#260971),(#260972,#260973),(#260974,#260975),(#260976,#260977),
(#260978,#260979),(#260980,#260981),(#260982,#260983),(#260984,#260985),
(#260986,#260987),(#260988,#260989),(#260990,#260991),(#260992,#260993),
(#260994,#260995),(#260996,#260997),(#260998,#260999),(#261000,#261001),
(#261002,#261003),(#261004,#261005),(#261006,#261007),(#261008,#261009),
(#261010,#261011),(#261012,#261013),(#261014,#261015),(#261016,#261017),
(#261018,#261019),(#261020,#261021),(#261022,#261023),(#261024,#261025),
(#261026,#261027),(#261028,#261029),(#261030,#261031),(#261032,#261033),
(#261034,#261035),(#261036,#261037),(#261038,#261039),(#261040,#261041),
(#261042,#261043),(#261044,#261045),(#261046,#261047),(#261048,#261049),
(#261050,#261051),(#261052,#261053),(#261054,#261055),(#261056,#261057),
(#261058,#261059),(#261060,#261061),(#261062,#261063),(#261064,#261065),
(#261066,#261067),(#261068,#261069),(#261070,#261071),(#261072,#261073),
(#261074,#261075),(#261076,#261077),(#261078,#261079),(#261080,#261081),
(#261082,#261083),(#261084,#261085),(#261086,#261087),(#261088,#261089),
(#261090,#261091),(#261092,#261093),(#261094,#261095),(#261096,#261097),
(#261098,#261099),(#261100,#261101),(#261102,#261103),(#261104,#261105),
(#261106,#261107),(#261108,#261109),(#261110,#261111),(#261112,#261113),
(#261114,#261115),(#261116,#261117),(#261118,#261119),(#261120,#261121),
(#261122,#261123),(#261124,#261125),(#261126,#261127),(#261128,#261129),
(#261130,#261131),(#261132,#261133),(#261134,#261135),(#261136,#261137),
(#261138,#261139),(#261140,#261141),(#261142,#261143),(#261144,#261145),
(#261146,#261147),(#261148,#261149),(#261150,#261151),(#261152,#261153),
(#261154,#261155),(#261156,#261157),(#261158,#261159),(#261160,#261161),
(#261162,#261163),(#261164,#261165),(#261166,#261167),(#261168,#261169),
(#261170,#261171),(#261172,#261173),(#261174,#261175),(#261176,#261177),
(#261178,#261179),(#261180,#261181),(#261182,#261183),(#261184,#261185),
(#261186,#261187),(#261188,#261189),(#261190,#261191),(#261192,#261193),
(#261194,#261195),(#261196,#261197),(#261198,#261199),(#261200,#261201),
(#261202,#261203),(#261204,#261205),(#261206,#261207),(#261208,#261209),
(#261210,#261211),(#261212,#261213),(#261214,#261215),(#261216,#261217),
(#261218,#261219),(#261220,#261221),(#261222,#261223),(#261224,#261225),
(#261226,#261227),(#261228,#261229),(#261230,#261231),(#261232,#261233),
(#261234,#261235),(#261236,#261237),(#261238,#261239),(#261240,#261241),
(#261242,#261243),(#261244,#261245),(#261246,#261247),(#261248,#261249),
(#261250,#261251),(#261252,#261253),(#261254,#261255),(#261256,#261257),
(#261258,#261259),(#261260,#261261),(#261262,#261263),(#261264,#261265),
(#261266,#261267),(#261268,#261269),(#261270,#261271),(#261272,#261273),
(#261274,#261275),(#261276,#261277),(#261278,#261279),(#261280,#261281),
(#261282,#261283),(#261284,#261285),(#261286,#261287),(#261288,#261289),
(#261290,#261291),(#261292,#261293),(#261294,#261295),(#261296,#261297),
(#261298,#261299),(#261300,#261301),(#261302,#261303),(#261304,#261305),
(#261306,#261307),(#261308,#261309),(#261310,#261311),(#261312,#261313),
(#261314,#261315),(#261316,#261317),(#261318,#261319),(#261320,#261321),
(#261322,#261323),(#261324,#261325),(#261326,#261327),(#261328,#261329),
(#261330,#261331),(#261332,#261333),(#261334,#261335),(#261336,#261337),
(#261338,#261339),(#261340,#261341),(#261342,#261343),(#261344,#261345),
(#261346,#261347),(#261348,#261349),(#261350,#261351),(#261352,#261353),
(#261354,#261355),(#261356,#261357),(#261358,#261359),(#261360,#261361),
(#261362,#261363),(#261364,#261365),(#261366,#261367),(#261368,#261369),
(#261370,#261371),(#261372,#261373),(#261374,#261375),(#261376,#261377),
(#261378,#261379),(#261380,#261381),(#261382,#261383),(#261384,#261385),
(#261386,#261387),(#261388,#261389),(#261390,#261391),(#261392,#261393),
(#261394,#261395),(#261396,#261397),(#261398,#261399),(#261400,#261401),
(#261402,#261403),(#261404,#261405),(#261406,#261407),(#261408,#261409),
(#261410,#261411),(#261412,#261413),(#261414,#261415),(#261416,#261417),
(#261418,#261419),(#261420,#261421),(#261422,#261423),(#261424,#261425),
(#261426,#261427),(#261428,#261429),(#261430,#261431),(#261432,#261433),
(#261434,#261435),(#261436,#261437),(#261438,#261439),(#261440,#261441),
(#261442,#261443),(#261444,#261445),(#261446,#261447),(#261448,#261449),
(#261450,#261451),(#261452,#261453),(#261454,#261455),(#261456,#261457),
(#261458,#261459),(#261460,#261461),(#261462,#261463),(#261464,#261465),
(#261466,#261467),(#261468,#261469),(#261470,#261471),(#261472,#261473),
(#261474,#261475),(#261476,#261477),(#261478,#261479),(#261480,#261481),
(#261482,#261483),(#261484,#261485),(#261486,#261487),(#261488,#261489),
(#261490,#261491),(#261492,#261493),(#261494,#261495),(#261496,#261497),
(#261498,#261499),(#261500,#261501),(#261502,#261503),(#261504,#261505),
(#261506,#261507),(#261508,#261509),(#261510,#261511),(#261512,#261513),
(#261514,#261515),(#261516,#261517),(#261518,#261519),(#261520,#261521),
(#261522,#261523),(#261524,#261525),(#261526,#261527),(#261528,#261529),
(#261530,#261531),(#261532,#261533),(#261534,#261535),(#261536,#261537),
(#261538,#261539),(#261540,#261541),(#261542,#261543),(#261544,#261545),
(#261546,#261547),(#261548,#261549),(#261550,#261551),(#261552,#261553),
(#261554,#261555),(#261556,#261557),(#261558,#261559),(#261560,#261561),
(#261562,#261563),(#261564,#261565),(#261566,#261567),(#261568,#261569),
(#261570,#261571),(#261572,#261573),(#261574,#261575),(#261576,#261577),
(#261578,#261579),(#261580,#261581),(#261582,#261583),(#261584,#261585),
(#261586,#261587),(#261588,#261589),(#261590,#261591),(#261592,#261593),
(#261594,#261595),(#261596,#261597),(#261598,#261599),(#261600,#261601),
(#261602,#261603),(#261604,#261605),(#261606,#261607),(#261608,#261609),
(#261610,#261611),(#261612,#261613),(#261614,#261615),(#261616,#261617),
(#261618,#261619),(#261620,#261621),(#261622,#261623),(#261624,#261625),
(#261626,#261627),(#261628,#261629),(#261630,#261631),(#261632,#261633),
(#261634,#261635),(#261636,#261637),(#261638,#261639),(#261640,#261641),
(#261642,#261643),(#261644,#261645),(#261646,#261647),(#261648,#261649),
(#261650,#261651),(#261652,#261653),(#261654,#261655),(#261656,#261657),
(#261658,#261659),(#261660,#261661),(#261662,#261663),(#261664,#261665),
(#261666,#261667),(#261668,#261669),(#261670,#261671),(#261672,#261673),
(#261674,#261675),(#261676,#261677),(#261678,#261679),(#261680,#261681),
(#261682,#261683),(#261684,#261685),(#261686,#261687),(#261688,#261689),
(#261690,#261691),(#261692,#261693),(#261694,#261695),(#261696,#261697),
(#261698,#261699),(#261700,#261701),(#261702,#261703),(#261704,#261705),
(#261706,#261707),(#261708,#261709),(#261710,#261711),(#261712,#261713),
(#261714,#261715),(#261716,#261717),(#261718,#261719),(#261720,#261721),
(#261722,#261723),(#261724,#261725),(#261726,#261727),(#261728,#261729),
(#261730,#261731),(#261732,#261733),(#261734,#261735),(#261736,#261737),
(#261738,#261739),(#261740,#261741)),.UNSPECIFIED.,.F.,.F.,.F.,(6,1,1,1,
1,1,1,1,1,1,1,1,1,1,1,1,1,1,1,1,1,1,1,1,1,1,1,1,1,1,1,1,1,1,1,1,1,1,1,1,
1,1,1,1,1,1,1,1,1,1,1,1,1,1,1,1,1,1,1,1,1,1,1,1,1,1,1,1,1,1,1,1,1,1,1,1,
1,1,1,1,1,1,1,1,1,1,1,1,1,1,1,1,1,1,1,1,1,1,1,1,1,1,1,1,1,1,1,1,1,1,1,1,
1,1,1,1,1,1,1,1,1,1,1,1,1,1,1,1,1,1,1,1,1,1,1,1,1,1,1,1,1,1,1,1,1,1,1,1,
1,1,1,1,1,1,1,1,1,1,1,1,1,1,1,1,1,1,1,1,1,1,1,1,1,1,1,1,1,1,1,1,1,1,1,1,
1,1,1,1,1,1,1,1,1,1,1,1,1,1,1,1,1,1,1,1,1,1,1,1,1,1,1,1,1,1,1,1,1,1,1,1,
1,1,1,1,1,1,1,1,1,1,1,1,1,1,1,1,1,1,1,1,1,1,1,1,1,1,1,1,1,1,1,1,1,1,1,1,
1,1,1,1,1,1,1,1,1,1,1,1,1,1,1,1,1,1,1,1,1,1,1,1,1,1,1,1,1,1,1,1,1,1,1,1,
1,1,1,1,1,1,1,1,1,1,1,1,1,1,1,1,1,1,1,1,1,1,1,1,1,1,1,1,1,1,1,1,1,1,1,1,
1,1,1,1,1,1,1,1,1,1,1,1,1,1,1,1,1,1,1,1,1,1,1,1,1,1,1,1,1,1,1,1,1,1,1,1,
1,1,1,1,1,1,1,1,1,1,1,1,1,1,1,1,1,1,1,1,1,1,1,1,1,1,1,1,1,1,1,1,1,1,1,1,
1,1,1,1,1,1,1,1,1,1,1,1,1,1,1,1,1,1,1,1,1,1,1,1,1,1,1,1,1,1,1,1,1,1,1,1,
1,1,1,1,1,1,1,1,1,1,1,1,1,1,1,1,1,1,1,1,1,1,1,1,1,1,1,1,1,1,1,6),(2,2),
(-1.,-0.998165138,-0.996330275,-0.994495413,-0.99266055,-0.990825688,-0.988990826,
-0.987155963,-0.985321101,-0.983486239,-0.981651376,-0.979816514,-0.977981651,
-0.976146789,-0.974311927,-0.972477064,-0.970642202,-0.968807339,-0.966972477,
-0.965137615,-0.963302752,-0.96146789,-0.959633028,-0.957798165,-0.955963303,
-0.95412844,-0.952293578,-0.950458716,-0.948623853,-0.946788991,-0.944954128,
-0.943119266,-0.941284404,-0.939449541,-0.937614679,-0.935779817,-0.933944954,
-0.932110092,-0.930275229,-0.928440367,-0.926605505,-0.924770642,-0.92293578,
-0.921100917,-0.919266055,-0.917431193,-0.91559633,-0.913761468,-0.911926606,
-0.910091743,-0.908256881,-0.906422018,-0.904587156,-0.902752294,-0.900917431,
-0.899082569,-0.897247706,-0.895412844,-0.893577982,-0.891743119,-0.889908257,
-0.888073394,-0.886238532,-0.88440367,-0.882568807,-0.880733945,-0.878899083,
-0.87706422,-0.875229358,-0.873394495,-0.871559633,-0.869724771,-0.867889908,
-0.866055046,-0.864220183,-0.862385321,-0.860550459,-0.858715596,-0.856880734,
-0.855045872,-0.853211009,-0.851376147,-0.849541284,-0.847706422,-0.84587156,
-0.844036697,-0.842201835,-0.840366972,-0.83853211,-0.836697248,-0.834862385,
-0.833027523,-0.831192661,-0.829357798,-0.827522936,-0.825688073,-0.823853211,
-0.822018349,-0.820183486,-0.818348624,-0.816513761,-0.814678899,-0.812844037,
-0.811009174,-0.809174312,-0.80733945,-0.805504587,-0.803669725,-0.801834862,
-0.8,-0.798165138,-0.796330275,-0.794495413,-0.79266055,-0.790825688,-0.788990826,
-0.787155963,-0.785321101,-0.783486239,-0.781651376,-0.779816514,-0.777981651,
-0.776146789,-0.774311927,-0.772477064,-0.770642202,-0.768807339,-0.766972477,
-0.765137615,-0.763302752,-0.76146789,-0.759633028,-0.757798165,-0.755963303,
-0.75412844,-0.752293578,-0.750458716,-0.748623853,-0.746788991,-0.744954128,
-0.743119266,-0.741284404,-0.739449541,-0.737614679,-0.735779817,-0.733944954,
-0.732110092,-0.730275229,-0.728440367,-0.726605505,-0.724770642,-0.72293578,
-0.721100917,-0.719266055,-0.717431193,-0.71559633,-0.713761468,-0.711926606,
-0.710091743,-0.708256881,-0.706422018,-0.704587156,-0.702752294,-0.700917431,
-0.699082569,-0.697247706,-0.695412844,-0.693577982,-0.691743119,-0.689908257,
-0.688073394,-0.686238532,-0.68440367,-0.682568807,-0.680733945,-0.678899083,
-0.67706422,-0.675229358,-0.673394495,-0.671559633,-0.669724771,-0.667889908,
-0.666055046,-0.664220183,-0.662385321,-0.660550459,-0.658715596,-0.656880734,
-0.655045872,-0.653211009,-0.651376147,-0.649541284,-0.647706422,-0.64587156,
-0.644036697,-0.642201835,-0.640366972,-0.63853211,-0.636697248,-0.634862385,
-0.633027523,-0.631192661,-0.629357798,-0.627522936,-0.625688073,-0.623853211,
-0.622018349,-0.620183486,-0.618348624,-0.616513761,-0.614678899,-0.612844037,
-0.611009174,-0.609174312,-0.60733945,-0.605504587,-0.603669725,-0.601834862,
-0.6,-0.598165138,-0.596330275,-0.594495413,-0.59266055,-0.590825688,-0.588990826,
-0.587155963,-0.585321101,-0.583486239,-0.581651376,-0.579816514,-0.577981651,
-0.576146789,-0.574311927,-0.572477064,-0.570642202,-0.568807339,-0.566972477,
-0.565137615,-0.563302752,-0.56146789,-0.559633028,-0.557798165,-0.555963303,
-0.55412844,-0.552293578,-0.550458716,-0.548623853,-0.546788991,-0.544954128,
-0.543119266,-0.541284404,-0.539449541,-0.537614679,-0.535779817,-0.533944954,
-0.532110092,-0.530275229,-0.528440367,-0.526605505,-0.524770642,-0.52293578,
-0.521100917,-0.519266055,-0.517431193,-0.51559633,-0.513761468,-0.511926606,
-0.510091743,-0.508256881,-0.506422018,-0.504587156,-0.502752294,-0.500917431,
-0.499082569,-0.497247706,-0.495412844,-0.493577982,-0.491743119,-0.489908257,
-0.488073394,-0.486238532,-0.48440367,-0.482568807,-0.480733945,-0.478899083,
-0.47706422,-0.475229358,-0.473394495,-0.471559633,-0.469724771,-0.467889908,
-0.466055046,-0.464220183,-0.462385321,-0.460550459,-0.458715596,-0.456880734,
-0.455045872,-0.453211009,-0.451376147,-0.449541284,-0.447706422,-0.44587156,
-0.444036697,-0.442201835,-0.440366972,-0.43853211,-0.436697248,-0.434862385,
-0.433027523,-0.431192661,-0.429357798,-0.427522936,-0.425688073,-0.423853211,
-0.422018349,-0.420183486,-0.418348624,-0.416513761,-0.414678899,-0.412844037,
-0.411009174,-0.409174312,-0.40733945,-0.405504587,-0.403669725,-0.401834862,
-0.4,-0.398165138,-0.396330275,-0.394495413,-0.39266055,-0.390825688,-0.388990826,
-0.387155963,-0.385321101,-0.383486239,-0.381651376,-0.379816514,-0.377981651,
-0.376146789,-0.374311927,-0.372477064,-0.370642202,-0.368807339,-0.366972477,
-0.365137615,-0.363302752,-0.36146789,-0.359633028,-0.357798165,-0.355963303,
-0.35412844,-0.352293578,-0.350458716,-0.348623853,-0.346788991,-0.344954128,
-0.343119266,-0.341284404,-0.339449541,-0.337614679,-0.335779817,-0.333944954,
-0.332110092,-0.330275229,-0.328440367,-0.326605505,-0.324770642,-0.32293578,
-0.321100917,-0.319266055,-0.317431193,-0.31559633,-0.313761468,-0.311926606,
-0.310091743,-0.308256881,-0.306422018,-0.304587156,-0.302752294,-0.300917431,
-0.299082569,-0.297247706,-0.295412844,-0.293577982,-0.291743119,-0.289908257,
-0.288073394,-0.286238532,-0.28440367,-0.282568807,-0.280733945,-0.278899083,
-0.27706422,-0.275229358,-0.273394495,-0.271559633,-0.269724771,-0.267889908,
-0.266055046,-0.264220183,-0.262385321,-0.260550459,-0.258715596,-0.256880734,
-0.255045872,-0.253211009,-0.251376147,-0.249541284,-0.247706422,-0.24587156,
-0.244036697,-0.242201835,-0.240366972,-0.23853211,-0.236697248,-0.234862385,
-0.233027523,-0.231192661,-0.229357798,-0.227522936,-0.225688073,-0.223853211,
-0.222018349,-0.220183486,-0.218348624,-0.216513761,-0.214678899,-0.212844037,
-0.211009174,-0.209174312,-0.20733945,-0.205504587,-0.203669725,-0.201834862,
-0.2,-0.198165138,-0.196330275,-0.194495413,-0.19266055,-0.190825688,-0.188990826,
-0.187155963,-0.185321101,-0.183486239,-0.181651376,-0.179816514,-0.177981651,
-0.176146789,-0.174311927,-0.172477064,-0.170642202,-0.168807339,-0.166972477,
-0.165137615,-0.163302752,-0.16146789,-0.159633028,-0.157798165,-0.155963303,
-0.15412844,-0.152293578,-0.150458716,-0.148623853,-0.146788991,-0.144954128,
-0.143172103),(0.,0.36),.UNSPECIFIED.);
#6281=B_SPLINE_SURFACE_WITH_KNOTS('',5,1,((#262704,#262705),(#262706,#262707),
(#262708,#262709),(#262710,#262711),(#262712,#262713),(#262714,#262715),
(#262716,#262717),(#262718,#262719),(#262720,#262721),(#262722,#262723),
(#262724,#262725),(#262726,#262727),(#262728,#262729),(#262730,#262731),
(#262732,#262733),(#262734,#262735),(#262736,#262737),(#262738,#262739),
(#262740,#262741),(#262742,#262743),(#262744,#262745),(#262746,#262747),
(#262748,#262749),(#262750,#262751),(#262752,#262753),(#262754,#262755),
(#262756,#262757),(#262758,#262759),(#262760,#262761),(#262762,#262763),
(#262764,#262765),(#262766,#262767),(#262768,#262769),(#262770,#262771),
(#262772,#262773),(#262774,#262775),(#262776,#262777),(#262778,#262779),
(#262780,#262781),(#262782,#262783),(#262784,#262785),(#262786,#262787),
(#262788,#262789),(#262790,#262791),(#262792,#262793),(#262794,#262795),
(#262796,#262797),(#262798,#262799),(#262800,#262801),(#262802,#262803),
(#262804,#262805),(#262806,#262807),(#262808,#262809),(#262810,#262811),
(#262812,#262813),(#262814,#262815),(#262816,#262817),(#262818,#262819),
(#262820,#262821),(#262822,#262823),(#262824,#262825),(#262826,#262827),
(#262828,#262829),(#262830,#262831),(#262832,#262833),(#262834,#262835),
(#262836,#262837),(#262838,#262839),(#262840,#262841),(#262842,#262843),
(#262844,#262845),(#262846,#262847),(#262848,#262849),(#262850,#262851),
(#262852,#262853),(#262854,#262855),(#262856,#262857),(#262858,#262859),
(#262860,#262861),(#262862,#262863),(#262864,#262865),(#262866,#262867),
(#262868,#262869),(#262870,#262871),(#262872,#262873),(#262874,#262875),
(#262876,#262877),(#262878,#262879),(#262880,#262881),(#262882,#262883),
(#262884,#262885),(#262886,#262887),(#262888,#262889),(#262890,#262891),
(#262892,#262893),(#262894,#262895),(#262896,#262897),(#262898,#262899),
(#262900,#262901),(#262902,#262903),(#262904,#262905),(#262906,#262907),
(#262908,#262909),(#262910,#262911),(#262912,#262913),(#262914,#262915),
(#262916,#262917),(#262918,#262919),(#262920,#262921),(#262922,#262923),
(#262924,#262925),(#262926,#262927),(#262928,#262929),(#262930,#262931),
(#262932,#262933),(#262934,#262935),(#262936,#262937),(#262938,#262939),
(#262940,#262941),(#262942,#262943),(#262944,#262945),(#262946,#262947),
(#262948,#262949),(#262950,#262951),(#262952,#262953),(#262954,#262955),
(#262956,#262957),(#262958,#262959),(#262960,#262961),(#262962,#262963),
(#262964,#262965),(#262966,#262967),(#262968,#262969),(#262970,#262971),
(#262972,#262973),(#262974,#262975),(#262976,#262977),(#262978,#262979),
(#262980,#262981),(#262982,#262983),(#262984,#262985),(#262986,#262987),
(#262988,#262989),(#262990,#262991),(#262992,#262993),(#262994,#262995),
(#262996,#262997),(#262998,#262999),(#263000,#263001),(#263002,#263003),
(#263004,#263005),(#263006,#263007),(#263008,#263009),(#263010,#263011),
(#263012,#263013),(#263014,#263015),(#263016,#263017),(#263018,#263019),
(#263020,#263021),(#263022,#263023),(#263024,#263025),(#263026,#263027),
(#263028,#263029),(#263030,#263031),(#263032,#263033),(#263034,#263035),
(#263036,#263037),(#263038,#263039),(#263040,#263041),(#263042,#263043),
(#263044,#263045),(#263046,#263047),(#263048,#263049),(#263050,#263051),
(#263052,#263053),(#263054,#263055),(#263056,#263057),(#263058,#263059),
(#263060,#263061),(#263062,#263063),(#263064,#263065),(#263066,#263067),
(#263068,#263069),(#263070,#263071),(#263072,#263073),(#263074,#263075),
(#263076,#263077),(#263078,#263079),(#263080,#263081),(#263082,#263083),
(#263084,#263085),(#263086,#263087),(#263088,#263089),(#263090,#263091),
(#263092,#263093),(#263094,#263095),(#263096,#263097),(#263098,#263099),
(#263100,#263101),(#263102,#263103),(#263104,#263105),(#263106,#263107),
(#263108,#263109),(#263110,#263111),(#263112,#263113),(#263114,#263115),
(#263116,#263117),(#263118,#263119),(#263120,#263121),(#263122,#263123),
(#263124,#263125),(#263126,#263127),(#263128,#263129),(#263130,#263131),
(#263132,#263133),(#263134,#263135),(#263136,#263137),(#263138,#263139),
(#263140,#263141),(#263142,#263143),(#263144,#263145),(#263146,#263147),
(#263148,#263149),(#263150,#263151),(#263152,#263153),(#263154,#263155),
(#263156,#263157),(#263158,#263159),(#263160,#263161),(#263162,#263163),
(#263164,#263165),(#263166,#263167),(#263168,#263169),(#263170,#263171),
(#263172,#263173),(#263174,#263175),(#263176,#263177),(#263178,#263179),
(#263180,#263181),(#263182,#263183),(#263184,#263185),(#263186,#263187),
(#263188,#263189),(#263190,#263191),(#263192,#263193),(#263194,#263195),
(#263196,#263197),(#263198,#263199),(#263200,#263201),(#263202,#263203),
(#263204,#263205),(#263206,#263207),(#263208,#263209),(#263210,#263211),
(#263212,#263213),(#263214,#263215),(#263216,#263217),(#263218,#263219),
(#263220,#263221),(#263222,#263223),(#263224,#263225),(#263226,#263227),
(#263228,#263229),(#263230,#263231),(#263232,#263233),(#263234,#263235),
(#263236,#263237),(#263238,#263239),(#263240,#263241),(#263242,#263243),
(#263244,#263245),(#263246,#263247),(#263248,#263249),(#263250,#263251),
(#263252,#263253),(#263254,#263255),(#263256,#263257),(#263258,#263259),
(#263260,#263261),(#263262,#263263),(#263264,#263265),(#263266,#263267),
(#263268,#263269),(#263270,#263271),(#263272,#263273),(#263274,#263275),
(#263276,#263277),(#263278,#263279),(#263280,#263281),(#263282,#263283),
(#263284,#263285),(#263286,#263287),(#263288,#263289),(#263290,#263291),
(#263292,#263293),(#263294,#263295),(#263296,#263297),(#263298,#263299),
(#263300,#263301),(#263302,#263303),(#263304,#263305),(#263306,#263307),
(#263308,#263309),(#263310,#263311),(#263312,#263313),(#263314,#263315),
(#263316,#263317),(#263318,#263319),(#263320,#263321),(#263322,#263323),
(#263324,#263325),(#263326,#263327),(#263328,#263329),(#263330,#263331),
(#263332,#263333),(#263334,#263335),(#263336,#263337),(#263338,#263339),
(#263340,#263341),(#263342,#263343),(#263344,#263345),(#263346,#263347),
(#263348,#263349),(#263350,#263351),(#263352,#263353),(#263354,#263355),
(#263356,#263357),(#263358,#263359),(#263360,#263361),(#263362,#263363),
(#263364,#263365),(#263366,#263367),(#263368,#263369),(#263370,#263371),
(#263372,#263373),(#263374,#263375),(#263376,#263377),(#263378,#263379),
(#263380,#263381),(#263382,#263383),(#263384,#263385),(#263386,#263387),
(#263388,#263389),(#263390,#263391),(#263392,#263393),(#263394,#263395),
(#263396,#263397),(#263398,#263399),(#263400,#263401),(#263402,#263403),
(#263404,#263405),(#263406,#263407),(#263408,#263409),(#263410,#263411),
(#263412,#263413),(#263414,#263415),(#263416,#263417),(#263418,#263419),
(#263420,#263421),(#263422,#263423),(#263424,#263425),(#263426,#263427),
(#263428,#263429),(#263430,#263431),(#263432,#263433),(#263434,#263435),
(#263436,#263437),(#263438,#263439),(#263440,#263441),(#263442,#263443),
(#263444,#263445),(#263446,#263447),(#263448,#263449),(#263450,#263451),
(#263452,#263453),(#263454,#263455),(#263456,#263457),(#263458,#263459),
(#263460,#263461),(#263462,#263463),(#263464,#263465),(#263466,#263467),
(#263468,#263469),(#263470,#263471),(#263472,#263473),(#263474,#263475),
(#263476,#263477),(#263478,#263479),(#263480,#263481),(#263482,#263483),
(#263484,#263485),(#263486,#263487),(#263488,#263489),(#263490,#263491),
(#263492,#263493),(#263494,#263495),(#263496,#263497),(#263498,#263499),
(#263500,#263501),(#263502,#263503),(#263504,#263505),(#263506,#263507),
(#263508,#263509),(#263510,#263511),(#263512,#263513),(#263514,#263515),
(#263516,#263517),(#263518,#263519),(#263520,#263521),(#263522,#263523),
(#263524,#263525),(#263526,#263527),(#263528,#263529),(#263530,#263531),
(#263532,#263533),(#263534,#263535),(#263536,#263537),(#263538,#263539),
(#263540,#263541),(#263542,#263543),(#263544,#263545),(#263546,#263547),
(#263548,#263549),(#263550,#263551),(#263552,#263553),(#263554,#263555),
(#263556,#263557),(#263558,#263559),(#263560,#263561),(#263562,#263563),
(#263564,#263565),(#263566,#263567),(#263568,#263569),(#263570,#263571),
(#263572,#263573),(#263574,#263575),(#263576,#263577),(#263578,#263579),
(#263580,#263581),(#263582,#263583),(#263584,#263585),(#263586,#263587),
(#263588,#263589),(#263590,#263591),(#263592,#263593),(#263594,#263595),
(#263596,#263597),(#263598,#263599),(#263600,#263601),(#263602,#263603),
(#263604,#263605),(#263606,#263607),(#263608,#263609),(#263610,#263611),
(#263612,#263613),(#263614,#263615),(#263616,#263617),(#263618,#263619),
(#263620,#263621),(#263622,#263623),(#263624,#263625),(#263626,#263627),
(#263628,#263629),(#263630,#263631),(#263632,#263633),(#263634,#263635),
(#263636,#263637),(#263638,#263639),(#263640,#263641),(#263642,#263643),
(#263644,#263645),(#263646,#263647)),.UNSPECIFIED.,.F.,.F.,.F.,(6,1,1,1,
1,1,1,1,1,1,1,1,1,1,1,1,1,1,1,1,1,1,1,1,1,1,1,1,1,1,1,1,1,1,1,1,1,1,1,1,
1,1,1,1,1,1,1,1,1,1,1,1,1,1,1,1,1,1,1,1,1,1,1,1,1,1,1,1,1,1,1,1,1,1,1,1,
1,1,1,1,1,1,1,1,1,1,1,1,1,1,1,1,1,1,1,1,1,1,1,1,1,1,1,1,1,1,1,1,1,1,1,1,
1,1,1,1,1,1,1,1,1,1,1,1,1,1,1,1,1,1,1,1,1,1,1,1,1,1,1,1,1,1,1,1,1,1,1,1,
1,1,1,1,1,1,1,1,1,1,1,1,1,1,1,1,1,1,1,1,1,1,1,1,1,1,1,1,1,1,1,1,1,1,1,1,
1,1,1,1,1,1,1,1,1,1,1,1,1,1,1,1,1,1,1,1,1,1,1,1,1,1,1,1,1,1,1,1,1,1,1,1,
1,1,1,1,1,1,1,1,1,1,1,1,1,1,1,1,1,1,1,1,1,1,1,1,1,1,1,1,1,1,1,1,1,1,1,1,
1,1,1,1,1,1,1,1,1,1,1,1,1,1,1,1,1,1,1,1,1,1,1,1,1,1,1,1,1,1,1,1,1,1,1,1,
1,1,1,1,1,1,1,1,1,1,1,1,1,1,1,1,1,1,1,1,1,1,1,1,1,1,1,1,1,1,1,1,1,1,1,1,
1,1,1,1,1,1,1,1,1,1,1,1,1,1,1,1,1,1,1,1,1,1,1,1,1,1,1,1,1,1,1,1,1,1,1,1,
1,1,1,1,1,1,1,1,1,1,1,1,1,1,1,1,1,1,1,1,1,1,1,1,1,1,1,1,1,1,1,1,1,1,1,1,
1,1,1,1,1,1,1,1,1,1,1,1,1,1,1,1,1,1,1,1,1,1,1,1,1,1,1,1,1,1,1,1,1,1,1,1,
1,1,1,1,1,1,1,1,1,1,1,1,1,1,1,1,1,1,1,1,1,1,1,1,1,1,1,1,1,1,1,6),(2,2),
(-1.,-0.998165138,-0.996330275,-0.994495413,-0.99266055,-0.990825688,-0.988990826,
-0.987155963,-0.985321101,-0.983486239,-0.981651376,-0.979816514,-0.977981651,
-0.976146789,-0.974311927,-0.972477064,-0.970642202,-0.968807339,-0.966972477,
-0.965137615,-0.963302752,-0.96146789,-0.959633028,-0.957798165,-0.955963303,
-0.95412844,-0.952293578,-0.950458716,-0.948623853,-0.946788991,-0.944954128,
-0.943119266,-0.941284404,-0.939449541,-0.937614679,-0.935779817,-0.933944954,
-0.932110092,-0.930275229,-0.928440367,-0.926605505,-0.924770642,-0.92293578,
-0.921100917,-0.919266055,-0.917431193,-0.91559633,-0.913761468,-0.911926606,
-0.910091743,-0.908256881,-0.906422018,-0.904587156,-0.902752294,-0.900917431,
-0.899082569,-0.897247706,-0.895412844,-0.893577982,-0.891743119,-0.889908257,
-0.888073394,-0.886238532,-0.88440367,-0.882568807,-0.880733945,-0.878899083,
-0.87706422,-0.875229358,-0.873394495,-0.871559633,-0.869724771,-0.867889908,
-0.866055046,-0.864220183,-0.862385321,-0.860550459,-0.858715596,-0.856880734,
-0.855045872,-0.853211009,-0.851376147,-0.849541284,-0.847706422,-0.84587156,
-0.844036697,-0.842201835,-0.840366972,-0.83853211,-0.836697248,-0.834862385,
-0.833027523,-0.831192661,-0.829357798,-0.827522936,-0.825688073,-0.823853211,
-0.822018349,-0.820183486,-0.818348624,-0.816513761,-0.814678899,-0.812844037,
-0.811009174,-0.809174312,-0.80733945,-0.805504587,-0.803669725,-0.801834862,
-0.8,-0.798165138,-0.796330275,-0.794495413,-0.79266055,-0.790825688,-0.788990826,
-0.787155963,-0.785321101,-0.783486239,-0.781651376,-0.779816514,-0.777981651,
-0.776146789,-0.774311927,-0.772477064,-0.770642202,-0.768807339,-0.766972477,
-0.765137615,-0.763302752,-0.76146789,-0.759633028,-0.757798165,-0.755963303,
-0.75412844,-0.752293578,-0.750458716,-0.748623853,-0.746788991,-0.744954128,
-0.743119266,-0.741284404,-0.739449541,-0.737614679,-0.735779817,-0.733944954,
-0.732110092,-0.730275229,-0.728440367,-0.726605505,-0.724770642,-0.72293578,
-0.721100917,-0.719266055,-0.717431193,-0.71559633,-0.713761468,-0.711926606,
-0.710091743,-0.708256881,-0.706422018,-0.704587156,-0.702752294,-0.700917431,
-0.699082569,-0.697247706,-0.695412844,-0.693577982,-0.691743119,-0.689908257,
-0.688073394,-0.686238532,-0.68440367,-0.682568807,-0.680733945,-0.678899083,
-0.67706422,-0.675229358,-0.673394495,-0.671559633,-0.669724771,-0.667889908,
-0.666055046,-0.664220183,-0.662385321,-0.660550459,-0.658715596,-0.656880734,
-0.655045872,-0.653211009,-0.651376147,-0.649541284,-0.647706422,-0.64587156,
-0.644036697,-0.642201835,-0.640366972,-0.63853211,-0.636697248,-0.634862385,
-0.633027523,-0.631192661,-0.629357798,-0.627522936,-0.625688073,-0.623853211,
-0.622018349,-0.620183486,-0.618348624,-0.616513761,-0.614678899,-0.612844037,
-0.611009174,-0.609174312,-0.60733945,-0.605504587,-0.603669725,-0.601834862,
-0.6,-0.598165138,-0.596330275,-0.594495413,-0.59266055,-0.590825688,-0.588990826,
-0.587155963,-0.585321101,-0.583486239,-0.581651376,-0.579816514,-0.577981651,
-0.576146789,-0.574311927,-0.572477064,-0.570642202,-0.568807339,-0.566972477,
-0.565137615,-0.563302752,-0.56146789,-0.559633028,-0.557798165,-0.555963303,
-0.55412844,-0.552293578,-0.550458716,-0.548623853,-0.546788991,-0.544954128,
-0.543119266,-0.541284404,-0.539449541,-0.537614679,-0.535779817,-0.533944954,
-0.532110092,-0.530275229,-0.528440367,-0.526605505,-0.524770642,-0.52293578,
-0.521100917,-0.519266055,-0.517431193,-0.51559633,-0.513761468,-0.511926606,
-0.510091743,-0.508256881,-0.506422018,-0.504587156,-0.502752294,-0.500917431,
-0.499082569,-0.497247706,-0.495412844,-0.493577982,-0.491743119,-0.489908257,
-0.488073394,-0.486238532,-0.48440367,-0.482568807,-0.480733945,-0.478899083,
-0.47706422,-0.475229358,-0.473394495,-0.471559633,-0.469724771,-0.467889908,
-0.466055046,-0.464220183,-0.462385321,-0.460550459,-0.458715596,-0.456880734,
-0.455045872,-0.453211009,-0.451376147,-0.449541284,-0.447706422,-0.44587156,
-0.444036697,-0.442201835,-0.440366972,-0.43853211,-0.436697248,-0.434862385,
-0.433027523,-0.431192661,-0.429357798,-0.427522936,-0.425688073,-0.423853211,
-0.422018349,-0.420183486,-0.418348624,-0.416513761,-0.414678899,-0.412844037,
-0.411009174,-0.409174312,-0.40733945,-0.405504587,-0.403669725,-0.401834862,
-0.4,-0.398165138,-0.396330275,-0.394495413,-0.39266055,-0.390825688,-0.388990826,
-0.387155963,-0.385321101,-0.383486239,-0.381651376,-0.379816514,-0.377981651,
-0.376146789,-0.374311927,-0.372477064,-0.370642202,-0.368807339,-0.366972477,
-0.365137615,-0.363302752,-0.36146789,-0.359633028,-0.357798165,-0.355963303,
-0.35412844,-0.352293578,-0.350458716,-0.348623853,-0.346788991,-0.344954128,
-0.343119266,-0.341284404,-0.339449541,-0.337614679,-0.335779817,-0.333944954,
-0.332110092,-0.330275229,-0.328440367,-0.326605505,-0.324770642,-0.32293578,
-0.321100917,-0.319266055,-0.317431193,-0.31559633,-0.313761468,-0.311926606,
-0.310091743,-0.308256881,-0.306422018,-0.304587156,-0.302752294,-0.300917431,
-0.299082569,-0.297247706,-0.295412844,-0.293577982,-0.291743119,-0.289908257,
-0.288073394,-0.286238532,-0.28440367,-0.282568807,-0.280733945,-0.278899083,
-0.27706422,-0.275229358,-0.273394495,-0.271559633,-0.269724771,-0.267889908,
-0.266055046,-0.264220183,-0.262385321,-0.260550459,-0.258715596,-0.256880734,
-0.255045872,-0.253211009,-0.251376147,-0.249541284,-0.247706422,-0.24587156,
-0.244036697,-0.242201835,-0.240366972,-0.23853211,-0.236697248,-0.234862385,
-0.233027523,-0.231192661,-0.229357798,-0.227522936,-0.225688073,-0.223853211,
-0.222018349,-0.220183486,-0.218348624,-0.216513761,-0.214678899,-0.212844037,
-0.211009174,-0.209174312,-0.20733945,-0.205504587,-0.203669725,-0.201834862,
-0.2,-0.198165138,-0.196330275,-0.194495413,-0.19266055,-0.190825688,-0.188990826,
-0.187155963,-0.185321101,-0.183486239,-0.181651376,-0.179816514,-0.177981651,
-0.176146789,-0.174311927,-0.172477064,-0.170642202,-0.168807339,-0.166972477,
-0.165137615,-0.163302752,-0.16146789,-0.159633028,-0.157798165,-0.155963303,
-0.15412844,-0.152293578,-0.150458716,-0.148623853,-0.146788991,-0.144954128,
-0.143172103),(0.,0.36),.UNSPECIFIED.);
#6282=B_SPLINE_SURFACE_WITH_KNOTS('',5,1,((#264259,#264260),(#264261,#264262),
(#264263,#264264),(#264265,#264266),(#264267,#264268),(#264269,#264270),
(#264271,#264272),(#264273,#264274),(#264275,#264276),(#264277,#264278),
(#264279,#264280),(#264281,#264282),(#264283,#264284),(#264285,#264286),
(#264287,#264288),(#264289,#264290),(#264291,#264292),(#264293,#264294),
(#264295,#264296),(#264297,#264298),(#264299,#264300),(#264301,#264302),
(#264303,#264304),(#264305,#264306),(#264307,#264308),(#264309,#264310),
(#264311,#264312),(#264313,#264314),(#264315,#264316),(#264317,#264318),
(#264319,#264320),(#264321,#264322),(#264323,#264324),(#264325,#264326),
(#264327,#264328),(#264329,#264330),(#264331,#264332),(#264333,#264334),
(#264335,#264336),(#264337,#264338),(#264339,#264340),(#264341,#264342),
(#264343,#264344),(#264345,#264346),(#264347,#264348),(#264349,#264350),
(#264351,#264352),(#264353,#264354),(#264355,#264356),(#264357,#264358),
(#264359,#264360),(#264361,#264362),(#264363,#264364),(#264365,#264366),
(#264367,#264368),(#264369,#264370),(#264371,#264372),(#264373,#264374),
(#264375,#264376),(#264377,#264378),(#264379,#264380),(#264381,#264382),
(#264383,#264384),(#264385,#264386),(#264387,#264388),(#264389,#264390),
(#264391,#264392),(#264393,#264394),(#264395,#264396),(#264397,#264398),
(#264399,#264400),(#264401,#264402),(#264403,#264404),(#264405,#264406),
(#264407,#264408),(#264409,#264410),(#264411,#264412),(#264413,#264414),
(#264415,#264416),(#264417,#264418),(#264419,#264420),(#264421,#264422),
(#264423,#264424),(#264425,#264426),(#264427,#264428),(#264429,#264430),
(#264431,#264432),(#264433,#264434),(#264435,#264436),(#264437,#264438),
(#264439,#264440),(#264441,#264442),(#264443,#264444),(#264445,#264446),
(#264447,#264448),(#264449,#264450),(#264451,#264452),(#264453,#264454),
(#264455,#264456),(#264457,#264458),(#264459,#264460),(#264461,#264462),
(#264463,#264464),(#264465,#264466),(#264467,#264468),(#264469,#264470),
(#264471,#264472),(#264473,#264474),(#264475,#264476),(#264477,#264478),
(#264479,#264480),(#264481,#264482),(#264483,#264484),(#264485,#264486),
(#264487,#264488),(#264489,#264490),(#264491,#264492),(#264493,#264494),
(#264495,#264496),(#264497,#264498),(#264499,#264500),(#264501,#264502),
(#264503,#264504),(#264505,#264506),(#264507,#264508),(#264509,#264510),
(#264511,#264512),(#264513,#264514),(#264515,#264516),(#264517,#264518),
(#264519,#264520),(#264521,#264522),(#264523,#264524),(#264525,#264526),
(#264527,#264528),(#264529,#264530),(#264531,#264532),(#264533,#264534),
(#264535,#264536),(#264537,#264538),(#264539,#264540),(#264541,#264542),
(#264543,#264544),(#264545,#264546),(#264547,#264548),(#264549,#264550),
(#264551,#264552),(#264553,#264554),(#264555,#264556),(#264557,#264558),
(#264559,#264560),(#264561,#264562),(#264563,#264564),(#264565,#264566),
(#264567,#264568),(#264569,#264570),(#264571,#264572),(#264573,#264574),
(#264575,#264576),(#264577,#264578),(#264579,#264580),(#264581,#264582),
(#264583,#264584),(#264585,#264586),(#264587,#264588),(#264589,#264590),
(#264591,#264592),(#264593,#264594),(#264595,#264596),(#264597,#264598),
(#264599,#264600),(#264601,#264602),(#264603,#264604),(#264605,#264606),
(#264607,#264608),(#264609,#264610),(#264611,#264612),(#264613,#264614),
(#264615,#264616),(#264617,#264618),(#264619,#264620),(#264621,#264622),
(#264623,#264624),(#264625,#264626),(#264627,#264628),(#264629,#264630),
(#264631,#264632),(#264633,#264634),(#264635,#264636),(#264637,#264638),
(#264639,#264640),(#264641,#264642),(#264643,#264644),(#264645,#264646),
(#264647,#264648),(#264649,#264650),(#264651,#264652),(#264653,#264654),
(#264655,#264656),(#264657,#264658),(#264659,#264660),(#264661,#264662),
(#264663,#264664),(#264665,#264666),(#264667,#264668),(#264669,#264670),
(#264671,#264672),(#264673,#264674),(#264675,#264676),(#264677,#264678),
(#264679,#264680),(#264681,#264682),(#264683,#264684),(#264685,#264686),
(#264687,#264688),(#264689,#264690),(#264691,#264692),(#264693,#264694),
(#264695,#264696),(#264697,#264698),(#264699,#264700),(#264701,#264702),
(#264703,#264704),(#264705,#264706),(#264707,#264708),(#264709,#264710),
(#264711,#264712),(#264713,#264714),(#264715,#264716),(#264717,#264718),
(#264719,#264720),(#264721,#264722),(#264723,#264724),(#264725,#264726),
(#264727,#264728),(#264729,#264730),(#264731,#264732),(#264733,#264734),
(#264735,#264736),(#264737,#264738),(#264739,#264740),(#264741,#264742),
(#264743,#264744),(#264745,#264746),(#264747,#264748),(#264749,#264750),
(#264751,#264752),(#264753,#264754),(#264755,#264756),(#264757,#264758),
(#264759,#264760),(#264761,#264762),(#264763,#264764),(#264765,#264766),
(#264767,#264768),(#264769,#264770),(#264771,#264772),(#264773,#264774),
(#264775,#264776),(#264777,#264778),(#264779,#264780),(#264781,#264782),
(#264783,#264784),(#264785,#264786),(#264787,#264788),(#264789,#264790),
(#264791,#264792),(#264793,#264794),(#264795,#264796),(#264797,#264798),
(#264799,#264800),(#264801,#264802),(#264803,#264804),(#264805,#264806),
(#264807,#264808),(#264809,#264810),(#264811,#264812),(#264813,#264814),
(#264815,#264816),(#264817,#264818),(#264819,#264820),(#264821,#264822),
(#264823,#264824),(#264825,#264826),(#264827,#264828),(#264829,#264830),
(#264831,#264832),(#264833,#264834),(#264835,#264836),(#264837,#264838),
(#264839,#264840),(#264841,#264842),(#264843,#264844),(#264845,#264846),
(#264847,#264848),(#264849,#264850),(#264851,#264852),(#264853,#264854),
(#264855,#264856),(#264857,#264858),(#264859,#264860),(#264861,#264862),
(#264863,#264864),(#264865,#264866),(#264867,#264868),(#264869,#264870),
(#264871,#264872),(#264873,#264874),(#264875,#264876),(#264877,#264878),
(#264879,#264880),(#264881,#264882),(#264883,#264884),(#264885,#264886),
(#264887,#264888),(#264889,#264890),(#264891,#264892),(#264893,#264894),
(#264895,#264896),(#264897,#264898),(#264899,#264900),(#264901,#264902),
(#264903,#264904),(#264905,#264906),(#264907,#264908),(#264909,#264910),
(#264911,#264912),(#264913,#264914),(#264915,#264916),(#264917,#264918),
(#264919,#264920),(#264921,#264922),(#264923,#264924),(#264925,#264926),
(#264927,#264928),(#264929,#264930),(#264931,#264932),(#264933,#264934),
(#264935,#264936),(#264937,#264938),(#264939,#264940),(#264941,#264942),
(#264943,#264944),(#264945,#264946),(#264947,#264948),(#264949,#264950),
(#264951,#264952),(#264953,#264954),(#264955,#264956),(#264957,#264958),
(#264959,#264960),(#264961,#264962),(#264963,#264964),(#264965,#264966),
(#264967,#264968),(#264969,#264970),(#264971,#264972),(#264973,#264974),
(#264975,#264976),(#264977,#264978),(#264979,#264980),(#264981,#264982),
(#264983,#264984),(#264985,#264986),(#264987,#264988),(#264989,#264990),
(#264991,#264992),(#264993,#264994),(#264995,#264996),(#264997,#264998),
(#264999,#265000),(#265001,#265002),(#265003,#265004),(#265005,#265006),
(#265007,#265008),(#265009,#265010),(#265011,#265012),(#265013,#265014),
(#265015,#265016),(#265017,#265018),(#265019,#265020),(#265021,#265022),
(#265023,#265024),(#265025,#265026),(#265027,#265028),(#265029,#265030),
(#265031,#265032),(#265033,#265034),(#265035,#265036),(#265037,#265038),
(#265039,#265040),(#265041,#265042),(#265043,#265044),(#265045,#265046),
(#265047,#265048),(#265049,#265050),(#265051,#265052),(#265053,#265054),
(#265055,#265056),(#265057,#265058),(#265059,#265060),(#265061,#265062),
(#265063,#265064),(#265065,#265066),(#265067,#265068),(#265069,#265070),
(#265071,#265072),(#265073,#265074),(#265075,#265076),(#265077,#265078),
(#265079,#265080),(#265081,#265082),(#265083,#265084),(#265085,#265086),
(#265087,#265088),(#265089,#265090),(#265091,#265092),(#265093,#265094),
(#265095,#265096),(#265097,#265098),(#265099,#265100),(#265101,#265102),
(#265103,#265104),(#265105,#265106),(#265107,#265108),(#265109,#265110),
(#265111,#265112),(#265113,#265114),(#265115,#265116),(#265117,#265118),
(#265119,#265120),(#265121,#265122),(#265123,#265124),(#265125,#265126),
(#265127,#265128),(#265129,#265130),(#265131,#265132),(#265133,#265134),
(#265135,#265136),(#265137,#265138),(#265139,#265140),(#265141,#265142),
(#265143,#265144),(#265145,#265146),(#265147,#265148),(#265149,#265150),
(#265151,#265152),(#265153,#265154),(#265155,#265156),(#265157,#265158),
(#265159,#265160),(#265161,#265162),(#265163,#265164),(#265165,#265166),
(#265167,#265168),(#265169,#265170),(#265171,#265172),(#265173,#265174),
(#265175,#265176),(#265177,#265178),(#265179,#265180),(#265181,#265182),
(#265183,#265184),(#265185,#265186),(#265187,#265188),(#265189,#265190),
(#265191,#265192),(#265193,#265194),(#265195,#265196),(#265197,#265198),
(#265199,#265200),(#265201,#265202)),.UNSPECIFIED.,.F.,.F.,.F.,(6,1,1,1,
1,1,1,1,1,1,1,1,1,1,1,1,1,1,1,1,1,1,1,1,1,1,1,1,1,1,1,1,1,1,1,1,1,1,1,1,
1,1,1,1,1,1,1,1,1,1,1,1,1,1,1,1,1,1,1,1,1,1,1,1,1,1,1,1,1,1,1,1,1,1,1,1,
1,1,1,1,1,1,1,1,1,1,1,1,1,1,1,1,1,1,1,1,1,1,1,1,1,1,1,1,1,1,1,1,1,1,1,1,
1,1,1,1,1,1,1,1,1,1,1,1,1,1,1,1,1,1,1,1,1,1,1,1,1,1,1,1,1,1,1,1,1,1,1,1,
1,1,1,1,1,1,1,1,1,1,1,1,1,1,1,1,1,1,1,1,1,1,1,1,1,1,1,1,1,1,1,1,1,1,1,1,
1,1,1,1,1,1,1,1,1,1,1,1,1,1,1,1,1,1,1,1,1,1,1,1,1,1,1,1,1,1,1,1,1,1,1,1,
1,1,1,1,1,1,1,1,1,1,1,1,1,1,1,1,1,1,1,1,1,1,1,1,1,1,1,1,1,1,1,1,1,1,1,1,
1,1,1,1,1,1,1,1,1,1,1,1,1,1,1,1,1,1,1,1,1,1,1,1,1,1,1,1,1,1,1,1,1,1,1,1,
1,1,1,1,1,1,1,1,1,1,1,1,1,1,1,1,1,1,1,1,1,1,1,1,1,1,1,1,1,1,1,1,1,1,1,1,
1,1,1,1,1,1,1,1,1,1,1,1,1,1,1,1,1,1,1,1,1,1,1,1,1,1,1,1,1,1,1,1,1,1,1,1,
1,1,1,1,1,1,1,1,1,1,1,1,1,1,1,1,1,1,1,1,1,1,1,1,1,1,1,1,1,1,1,1,1,1,1,1,
1,1,1,1,1,1,1,1,1,1,1,1,1,1,1,1,1,1,1,1,1,1,1,1,1,1,1,1,1,1,1,1,1,1,1,1,
1,1,1,1,1,1,1,1,1,1,1,1,1,1,1,1,1,1,1,1,1,1,1,1,1,1,1,1,1,1,1,6),(2,2),
(0.143172103,0.144954128,0.146788991,0.148623853,0.150458716,0.152293578,
0.15412844,0.155963303,0.157798165,0.159633028,0.16146789,0.163302752,0.165137615,
0.166972477,0.168807339,0.170642202,0.172477064,0.174311927,0.176146789,
0.177981651,0.179816514,0.181651376,0.183486239,0.185321101,0.187155963,
0.188990826,0.190825688,0.19266055,0.194495413,0.196330275,0.198165138,
0.2,0.201834862,0.203669725,0.205504587,0.20733945,0.209174312,0.211009174,
0.212844037,0.214678899,0.216513761,0.218348624,0.220183486,0.222018349,
0.223853211,0.225688073,0.227522936,0.229357798,0.231192661,0.233027523,
0.234862385,0.236697248,0.23853211,0.240366972,0.242201835,0.244036697,
0.24587156,0.247706422,0.249541284,0.251376147,0.253211009,0.255045872,
0.256880734,0.258715596,0.260550459,0.262385321,0.264220183,0.266055046,
0.267889908,0.269724771,0.271559633,0.273394495,0.275229358,0.27706422,
0.278899083,0.280733945,0.282568807,0.28440367,0.286238532,0.288073394,
0.289908257,0.291743119,0.293577982,0.295412844,0.297247706,0.299082569,
0.300917431,0.302752294,0.304587156,0.306422018,0.308256881,0.310091743,
0.311926606,0.313761468,0.31559633,0.317431193,0.319266055,0.321100917,
0.32293578,0.324770642,0.326605505,0.328440367,0.330275229,0.332110092,
0.333944954,0.335779817,0.337614679,0.339449541,0.341284404,0.343119266,
0.344954128,0.346788991,0.348623853,0.350458716,0.352293578,0.35412844,
0.355963303,0.357798165,0.359633028,0.36146789,0.363302752,0.365137615,
0.366972477,0.368807339,0.370642202,0.372477064,0.374311927,0.376146789,
0.377981651,0.379816514,0.381651376,0.383486239,0.385321101,0.387155963,
0.388990826,0.390825688,0.39266055,0.394495413,0.396330275,0.398165138,
0.4,0.401834862,0.403669725,0.405504587,0.40733945,0.409174312,0.411009174,
0.412844037,0.414678899,0.416513761,0.418348624,0.420183486,0.422018349,
0.423853211,0.425688073,0.427522936,0.429357798,0.431192661,0.433027523,
0.434862385,0.436697248,0.43853211,0.440366972,0.442201835,0.444036697,
0.44587156,0.447706422,0.449541284,0.451376147,0.453211009,0.455045872,
0.456880734,0.458715596,0.460550459,0.462385321,0.464220183,0.466055046,
0.467889908,0.469724771,0.471559633,0.473394495,0.475229358,0.47706422,
0.478899083,0.480733945,0.482568807,0.48440367,0.486238532,0.488073394,
0.489908257,0.491743119,0.493577982,0.495412844,0.497247706,0.499082569,
0.500917431,0.502752294,0.504587156,0.506422018,0.508256881,0.510091743,
0.511926606,0.513761468,0.51559633,0.517431193,0.519266055,0.521100917,
0.52293578,0.524770642,0.526605505,0.528440367,0.530275229,0.532110092,
0.533944954,0.535779817,0.537614679,0.539449541,0.541284404,0.543119266,
0.544954128,0.546788991,0.548623853,0.550458716,0.552293578,0.55412844,
0.555963303,0.557798165,0.559633028,0.56146789,0.563302752,0.565137615,
0.566972477,0.568807339,0.570642202,0.572477064,0.574311927,0.576146789,
0.577981651,0.579816514,0.581651376,0.583486239,0.585321101,0.587155963,
0.588990826,0.590825688,0.59266055,0.594495413,0.596330275,0.598165138,
0.6,0.601834862,0.603669725,0.605504587,0.60733945,0.609174312,0.611009174,
0.612844037,0.614678899,0.616513761,0.618348624,0.620183486,0.622018349,
0.623853211,0.625688073,0.627522936,0.629357798,0.631192661,0.633027523,
0.634862385,0.636697248,0.63853211,0.640366972,0.642201835,0.644036697,
0.64587156,0.647706422,0.649541284,0.651376147,0.653211009,0.655045872,
0.656880734,0.658715596,0.660550459,0.662385321,0.664220183,0.666055046,
0.667889908,0.669724771,0.671559633,0.673394495,0.675229358,0.67706422,
0.678899083,0.680733945,0.682568807,0.68440367,0.686238532,0.688073394,
0.689908257,0.691743119,0.693577982,0.695412844,0.697247706,0.699082569,
0.700917431,0.702752294,0.704587156,0.706422018,0.708256881,0.710091743,
0.711926606,0.713761468,0.71559633,0.717431193,0.719266055,0.721100917,
0.72293578,0.724770642,0.726605505,0.728440367,0.730275229,0.732110092,
0.733944954,0.735779817,0.737614679,0.739449541,0.741284404,0.743119266,
0.744954128,0.746788991,0.748623853,0.750458716,0.752293578,0.75412844,
0.755963303,0.757798165,0.759633028,0.76146789,0.763302752,0.765137615,
0.766972477,0.768807339,0.770642202,0.772477064,0.774311927,0.776146789,
0.777981651,0.779816514,0.781651376,0.783486239,0.785321101,0.787155963,
0.788990826,0.790825688,0.79266055,0.794495413,0.796330275,0.798165138,
0.8,0.801834862,0.803669725,0.805504587,0.80733945,0.809174312,0.811009174,
0.812844037,0.814678899,0.816513761,0.818348624,0.820183486,0.822018349,
0.823853211,0.825688073,0.827522936,0.829357798,0.831192661,0.833027523,
0.834862385,0.836697248,0.83853211,0.840366972,0.842201835,0.844036697,
0.84587156,0.847706422,0.849541284,0.851376147,0.853211009,0.855045872,
0.856880734,0.858715596,0.860550459,0.862385321,0.864220183,0.866055046,
0.867889908,0.869724771,0.871559633,0.873394495,0.875229358,0.87706422,
0.878899083,0.880733945,0.882568807,0.88440367,0.886238532,0.888073394,
0.889908257,0.891743119,0.893577982,0.895412844,0.897247706,0.899082569,
0.900917431,0.902752294,0.904587156,0.906422018,0.908256881,0.910091743,
0.911926606,0.913761468,0.91559633,0.917431193,0.919266055,0.921100917,
0.92293578,0.924770642,0.926605505,0.928440367,0.930275229,0.932110092,
0.933944954,0.935779817,0.937614679,0.939449541,0.941284404,0.943119266,
0.944954128,0.946788991,0.948623853,0.950458716,0.952293578,0.95412844,
0.955963303,0.957798165,0.959633028,0.96146789,0.963302752,0.965137615,
0.966972477,0.968807339,0.970642202,0.972477064,0.974311927,0.976146789,
0.977981651,0.979816514,0.981651376,0.983486239,0.985321101,0.987155963,
0.988990826,0.990825688,0.99266055,0.994495413,0.996330275,0.998165138,
1.),(0.,0.36),.UNSPECIFIED.);
#6283=B_SPLINE_SURFACE_WITH_KNOTS('',5,1,((#266158,#266159),(#266160,#266161),
(#266162,#266163),(#266164,#266165),(#266166,#266167),(#266168,#266169),
(#266170,#266171),(#266172,#266173),(#266174,#266175),(#266176,#266177),
(#266178,#266179),(#266180,#266181),(#266182,#266183),(#266184,#266185),
(#266186,#266187),(#266188,#266189),(#266190,#266191),(#266192,#266193),
(#266194,#266195),(#266196,#266197),(#266198,#266199),(#266200,#266201),
(#266202,#266203),(#266204,#266205),(#266206,#266207),(#266208,#266209),
(#266210,#266211),(#266212,#266213),(#266214,#266215),(#266216,#266217),
(#266218,#266219),(#266220,#266221),(#266222,#266223),(#266224,#266225),
(#266226,#266227),(#266228,#266229),(#266230,#266231),(#266232,#266233),
(#266234,#266235),(#266236,#266237),(#266238,#266239),(#266240,#266241),
(#266242,#266243),(#266244,#266245),(#266246,#266247),(#266248,#266249),
(#266250,#266251),(#266252,#266253),(#266254,#266255),(#266256,#266257),
(#266258,#266259),(#266260,#266261),(#266262,#266263),(#266264,#266265),
(#266266,#266267),(#266268,#266269),(#266270,#266271),(#266272,#266273),
(#266274,#266275),(#266276,#266277),(#266278,#266279),(#266280,#266281),
(#266282,#266283),(#266284,#266285),(#266286,#266287),(#266288,#266289),
(#266290,#266291),(#266292,#266293),(#266294,#266295),(#266296,#266297),
(#266298,#266299),(#266300,#266301),(#266302,#266303),(#266304,#266305),
(#266306,#266307),(#266308,#266309),(#266310,#266311),(#266312,#266313),
(#266314,#266315),(#266316,#266317),(#266318,#266319),(#266320,#266321),
(#266322,#266323),(#266324,#266325),(#266326,#266327),(#266328,#266329),
(#266330,#266331),(#266332,#266333),(#266334,#266335),(#266336,#266337),
(#266338,#266339),(#266340,#266341),(#266342,#266343),(#266344,#266345),
(#266346,#266347),(#266348,#266349),(#266350,#266351),(#266352,#266353),
(#266354,#266355),(#266356,#266357),(#266358,#266359),(#266360,#266361),
(#266362,#266363),(#266364,#266365),(#266366,#266367),(#266368,#266369),
(#266370,#266371),(#266372,#266373),(#266374,#266375),(#266376,#266377),
(#266378,#266379),(#266380,#266381),(#266382,#266383),(#266384,#266385),
(#266386,#266387),(#266388,#266389),(#266390,#266391),(#266392,#266393),
(#266394,#266395),(#266396,#266397),(#266398,#266399),(#266400,#266401),
(#266402,#266403),(#266404,#266405),(#266406,#266407),(#266408,#266409),
(#266410,#266411),(#266412,#266413),(#266414,#266415),(#266416,#266417),
(#266418,#266419),(#266420,#266421),(#266422,#266423),(#266424,#266425),
(#266426,#266427),(#266428,#266429),(#266430,#266431),(#266432,#266433),
(#266434,#266435),(#266436,#266437),(#266438,#266439),(#266440,#266441),
(#266442,#266443),(#266444,#266445),(#266446,#266447),(#266448,#266449),
(#266450,#266451),(#266452,#266453),(#266454,#266455),(#266456,#266457),
(#266458,#266459),(#266460,#266461),(#266462,#266463),(#266464,#266465),
(#266466,#266467),(#266468,#266469),(#266470,#266471),(#266472,#266473),
(#266474,#266475),(#266476,#266477),(#266478,#266479),(#266480,#266481),
(#266482,#266483),(#266484,#266485),(#266486,#266487),(#266488,#266489),
(#266490,#266491),(#266492,#266493),(#266494,#266495),(#266496,#266497),
(#266498,#266499),(#266500,#266501),(#266502,#266503),(#266504,#266505),
(#266506,#266507),(#266508,#266509),(#266510,#266511),(#266512,#266513),
(#266514,#266515),(#266516,#266517),(#266518,#266519),(#266520,#266521),
(#266522,#266523),(#266524,#266525),(#266526,#266527),(#266528,#266529),
(#266530,#266531),(#266532,#266533),(#266534,#266535),(#266536,#266537),
(#266538,#266539),(#266540,#266541),(#266542,#266543),(#266544,#266545),
(#266546,#266547),(#266548,#266549),(#266550,#266551),(#266552,#266553),
(#266554,#266555),(#266556,#266557),(#266558,#266559),(#266560,#266561),
(#266562,#266563),(#266564,#266565),(#266566,#266567),(#266568,#266569),
(#266570,#266571),(#266572,#266573),(#266574,#266575),(#266576,#266577),
(#266578,#266579),(#266580,#266581),(#266582,#266583),(#266584,#266585),
(#266586,#266587),(#266588,#266589),(#266590,#266591),(#266592,#266593),
(#266594,#266595),(#266596,#266597),(#266598,#266599),(#266600,#266601),
(#266602,#266603),(#266604,#266605),(#266606,#266607),(#266608,#266609),
(#266610,#266611),(#266612,#266613),(#266614,#266615),(#266616,#266617),
(#266618,#266619),(#266620,#266621),(#266622,#266623),(#266624,#266625),
(#266626,#266627),(#266628,#266629),(#266630,#266631),(#266632,#266633),
(#266634,#266635),(#266636,#266637),(#266638,#266639),(#266640,#266641),
(#266642,#266643),(#266644,#266645),(#266646,#266647),(#266648,#266649),
(#266650,#266651),(#266652,#266653),(#266654,#266655),(#266656,#266657),
(#266658,#266659),(#266660,#266661),(#266662,#266663),(#266664,#266665),
(#266666,#266667),(#266668,#266669),(#266670,#266671),(#266672,#266673),
(#266674,#266675),(#266676,#266677),(#266678,#266679),(#266680,#266681),
(#266682,#266683),(#266684,#266685),(#266686,#266687),(#266688,#266689),
(#266690,#266691),(#266692,#266693),(#266694,#266695),(#266696,#266697),
(#266698,#266699),(#266700,#266701),(#266702,#266703),(#266704,#266705),
(#266706,#266707),(#266708,#266709),(#266710,#266711),(#266712,#266713),
(#266714,#266715),(#266716,#266717),(#266718,#266719),(#266720,#266721),
(#266722,#266723),(#266724,#266725),(#266726,#266727),(#266728,#266729),
(#266730,#266731),(#266732,#266733),(#266734,#266735),(#266736,#266737),
(#266738,#266739),(#266740,#266741),(#266742,#266743),(#266744,#266745),
(#266746,#266747),(#266748,#266749),(#266750,#266751),(#266752,#266753),
(#266754,#266755),(#266756,#266757),(#266758,#266759),(#266760,#266761),
(#266762,#266763),(#266764,#266765),(#266766,#266767),(#266768,#266769),
(#266770,#266771),(#266772,#266773),(#266774,#266775),(#266776,#266777),
(#266778,#266779),(#266780,#266781),(#266782,#266783),(#266784,#266785),
(#266786,#266787),(#266788,#266789),(#266790,#266791),(#266792,#266793),
(#266794,#266795),(#266796,#266797),(#266798,#266799),(#266800,#266801),
(#266802,#266803),(#266804,#266805),(#266806,#266807),(#266808,#266809),
(#266810,#266811),(#266812,#266813),(#266814,#266815),(#266816,#266817),
(#266818,#266819),(#266820,#266821),(#266822,#266823),(#266824,#266825),
(#266826,#266827),(#266828,#266829),(#266830,#266831),(#266832,#266833),
(#266834,#266835),(#266836,#266837),(#266838,#266839),(#266840,#266841),
(#266842,#266843),(#266844,#266845),(#266846,#266847),(#266848,#266849),
(#266850,#266851),(#266852,#266853),(#266854,#266855),(#266856,#266857),
(#266858,#266859),(#266860,#266861),(#266862,#266863),(#266864,#266865),
(#266866,#266867),(#266868,#266869),(#266870,#266871),(#266872,#266873),
(#266874,#266875),(#266876,#266877),(#266878,#266879),(#266880,#266881),
(#266882,#266883),(#266884,#266885),(#266886,#266887),(#266888,#266889),
(#266890,#266891),(#266892,#266893),(#266894,#266895),(#266896,#266897),
(#266898,#266899),(#266900,#266901),(#266902,#266903),(#266904,#266905),
(#266906,#266907),(#266908,#266909),(#266910,#266911),(#266912,#266913),
(#266914,#266915),(#266916,#266917),(#266918,#266919),(#266920,#266921),
(#266922,#266923),(#266924,#266925),(#266926,#266927),(#266928,#266929),
(#266930,#266931),(#266932,#266933),(#266934,#266935),(#266936,#266937),
(#266938,#266939),(#266940,#266941),(#266942,#266943),(#266944,#266945),
(#266946,#266947),(#266948,#266949),(#266950,#266951),(#266952,#266953),
(#266954,#266955),(#266956,#266957),(#266958,#266959),(#266960,#266961),
(#266962,#266963),(#266964,#266965),(#266966,#266967),(#266968,#266969),
(#266970,#266971),(#266972,#266973),(#266974,#266975),(#266976,#266977),
(#266978,#266979),(#266980,#266981),(#266982,#266983),(#266984,#266985),
(#266986,#266987),(#266988,#266989),(#266990,#266991),(#266992,#266993),
(#266994,#266995),(#266996,#266997),(#266998,#266999),(#267000,#267001),
(#267002,#267003),(#267004,#267005),(#267006,#267007),(#267008,#267009),
(#267010,#267011),(#267012,#267013),(#267014,#267015),(#267016,#267017),
(#267018,#267019),(#267020,#267021),(#267022,#267023),(#267024,#267025),
(#267026,#267027),(#267028,#267029),(#267030,#267031),(#267032,#267033),
(#267034,#267035),(#267036,#267037),(#267038,#267039),(#267040,#267041),
(#267042,#267043),(#267044,#267045),(#267046,#267047),(#267048,#267049),
(#267050,#267051),(#267052,#267053),(#267054,#267055),(#267056,#267057),
(#267058,#267059),(#267060,#267061),(#267062,#267063),(#267064,#267065),
(#267066,#267067),(#267068,#267069),(#267070,#267071),(#267072,#267073),
(#267074,#267075),(#267076,#267077),(#267078,#267079),(#267080,#267081),
(#267082,#267083),(#267084,#267085),(#267086,#267087),(#267088,#267089),
(#267090,#267091),(#267092,#267093),(#267094,#267095),(#267096,#267097),
(#267098,#267099),(#267100,#267101)),.UNSPECIFIED.,.F.,.F.,.F.,(6,1,1,1,
1,1,1,1,1,1,1,1,1,1,1,1,1,1,1,1,1,1,1,1,1,1,1,1,1,1,1,1,1,1,1,1,1,1,1,1,
1,1,1,1,1,1,1,1,1,1,1,1,1,1,1,1,1,1,1,1,1,1,1,1,1,1,1,1,1,1,1,1,1,1,1,1,
1,1,1,1,1,1,1,1,1,1,1,1,1,1,1,1,1,1,1,1,1,1,1,1,1,1,1,1,1,1,1,1,1,1,1,1,
1,1,1,1,1,1,1,1,1,1,1,1,1,1,1,1,1,1,1,1,1,1,1,1,1,1,1,1,1,1,1,1,1,1,1,1,
1,1,1,1,1,1,1,1,1,1,1,1,1,1,1,1,1,1,1,1,1,1,1,1,1,1,1,1,1,1,1,1,1,1,1,1,
1,1,1,1,1,1,1,1,1,1,1,1,1,1,1,1,1,1,1,1,1,1,1,1,1,1,1,1,1,1,1,1,1,1,1,1,
1,1,1,1,1,1,1,1,1,1,1,1,1,1,1,1,1,1,1,1,1,1,1,1,1,1,1,1,1,1,1,1,1,1,1,1,
1,1,1,1,1,1,1,1,1,1,1,1,1,1,1,1,1,1,1,1,1,1,1,1,1,1,1,1,1,1,1,1,1,1,1,1,
1,1,1,1,1,1,1,1,1,1,1,1,1,1,1,1,1,1,1,1,1,1,1,1,1,1,1,1,1,1,1,1,1,1,1,1,
1,1,1,1,1,1,1,1,1,1,1,1,1,1,1,1,1,1,1,1,1,1,1,1,1,1,1,1,1,1,1,1,1,1,1,1,
1,1,1,1,1,1,1,1,1,1,1,1,1,1,1,1,1,1,1,1,1,1,1,1,1,1,1,1,1,1,1,1,1,1,1,1,
1,1,1,1,1,1,1,1,1,1,1,1,1,1,1,1,1,1,1,1,1,1,1,1,1,1,1,1,1,1,1,1,1,1,1,1,
1,1,1,1,1,1,1,1,1,1,1,1,1,1,1,1,1,1,1,1,1,1,1,1,1,1,1,1,1,1,1,6),(2,2),
(0.143172103,0.144954128,0.146788991,0.148623853,0.150458716,0.152293578,
0.15412844,0.155963303,0.157798165,0.159633028,0.16146789,0.163302752,0.165137615,
0.166972477,0.168807339,0.170642202,0.172477064,0.174311927,0.176146789,
0.177981651,0.179816514,0.181651376,0.183486239,0.185321101,0.187155963,
0.188990826,0.190825688,0.19266055,0.194495413,0.196330275,0.198165138,
0.2,0.201834862,0.203669725,0.205504587,0.20733945,0.209174312,0.211009174,
0.212844037,0.214678899,0.216513761,0.218348624,0.220183486,0.222018349,
0.223853211,0.225688073,0.227522936,0.229357798,0.231192661,0.233027523,
0.234862385,0.236697248,0.23853211,0.240366972,0.242201835,0.244036697,
0.24587156,0.247706422,0.249541284,0.251376147,0.253211009,0.255045872,
0.256880734,0.258715596,0.260550459,0.262385321,0.264220183,0.266055046,
0.267889908,0.269724771,0.271559633,0.273394495,0.275229358,0.27706422,
0.278899083,0.280733945,0.282568807,0.28440367,0.286238532,0.288073394,
0.289908257,0.291743119,0.293577982,0.295412844,0.297247706,0.299082569,
0.300917431,0.302752294,0.304587156,0.306422018,0.308256881,0.310091743,
0.311926606,0.313761468,0.31559633,0.317431193,0.319266055,0.321100917,
0.32293578,0.324770642,0.326605505,0.328440367,0.330275229,0.332110092,
0.333944954,0.335779817,0.337614679,0.339449541,0.341284404,0.343119266,
0.344954128,0.346788991,0.348623853,0.350458716,0.352293578,0.35412844,
0.355963303,0.357798165,0.359633028,0.36146789,0.363302752,0.365137615,
0.366972477,0.368807339,0.370642202,0.372477064,0.374311927,0.376146789,
0.377981651,0.379816514,0.381651376,0.383486239,0.385321101,0.387155963,
0.388990826,0.390825688,0.39266055,0.394495413,0.396330275,0.398165138,
0.4,0.401834862,0.403669725,0.405504587,0.40733945,0.409174312,0.411009174,
0.412844037,0.414678899,0.416513761,0.418348624,0.420183486,0.422018349,
0.423853211,0.425688073,0.427522936,0.429357798,0.431192661,0.433027523,
0.434862385,0.436697248,0.43853211,0.440366972,0.442201835,0.444036697,
0.44587156,0.447706422,0.449541284,0.451376147,0.453211009,0.455045872,
0.456880734,0.458715596,0.460550459,0.462385321,0.464220183,0.466055046,
0.467889908,0.469724771,0.471559633,0.473394495,0.475229358,0.47706422,
0.478899083,0.480733945,0.482568807,0.48440367,0.486238532,0.488073394,
0.489908257,0.491743119,0.493577982,0.495412844,0.497247706,0.499082569,
0.500917431,0.502752294,0.504587156,0.506422018,0.508256881,0.510091743,
0.511926606,0.513761468,0.51559633,0.517431193,0.519266055,0.521100917,
0.52293578,0.524770642,0.526605505,0.528440367,0.530275229,0.532110092,
0.533944954,0.535779817,0.537614679,0.539449541,0.541284404,0.543119266,
0.544954128,0.546788991,0.548623853,0.550458716,0.552293578,0.55412844,
0.555963303,0.557798165,0.559633028,0.56146789,0.563302752,0.565137615,
0.566972477,0.568807339,0.570642202,0.572477064,0.574311927,0.576146789,
0.577981651,0.579816514,0.581651376,0.583486239,0.585321101,0.587155963,
0.588990826,0.590825688,0.59266055,0.594495413,0.596330275,0.598165138,
0.6,0.601834862,0.603669725,0.605504587,0.60733945,0.609174312,0.611009174,
0.612844037,0.614678899,0.616513761,0.618348624,0.620183486,0.622018349,
0.623853211,0.625688073,0.627522936,0.629357798,0.631192661,0.633027523,
0.634862385,0.636697248,0.63853211,0.640366972,0.642201835,0.644036697,
0.64587156,0.647706422,0.649541284,0.651376147,0.653211009,0.655045872,
0.656880734,0.658715596,0.660550459,0.662385321,0.664220183,0.666055046,
0.667889908,0.669724771,0.671559633,0.673394495,0.675229358,0.67706422,
0.678899083,0.680733945,0.682568807,0.68440367,0.686238532,0.688073394,
0.689908257,0.691743119,0.693577982,0.695412844,0.697247706,0.699082569,
0.700917431,0.702752294,0.704587156,0.706422018,0.708256881,0.710091743,
0.711926606,0.713761468,0.71559633,0.717431193,0.719266055,0.721100917,
0.72293578,0.724770642,0.726605505,0.728440367,0.730275229,0.732110092,
0.733944954,0.735779817,0.737614679,0.739449541,0.741284404,0.743119266,
0.744954128,0.746788991,0.748623853,0.750458716,0.752293578,0.75412844,
0.755963303,0.757798165,0.759633028,0.76146789,0.763302752,0.765137615,
0.766972477,0.768807339,0.770642202,0.772477064,0.774311927,0.776146789,
0.777981651,0.779816514,0.781651376,0.783486239,0.785321101,0.787155963,
0.788990826,0.790825688,0.79266055,0.794495413,0.796330275,0.798165138,
0.8,0.801834862,0.803669725,0.805504587,0.80733945,0.809174312,0.811009174,
0.812844037,0.814678899,0.816513761,0.818348624,0.820183486,0.822018349,
0.823853211,0.825688073,0.827522936,0.829357798,0.831192661,0.833027523,
0.834862385,0.836697248,0.83853211,0.840366972,0.842201835,0.844036697,
0.84587156,0.847706422,0.849541284,0.851376147,0.853211009,0.855045872,
0.856880734,0.858715596,0.860550459,0.862385321,0.864220183,0.866055046,
0.867889908,0.869724771,0.871559633,0.873394495,0.875229358,0.87706422,
0.878899083,0.880733945,0.882568807,0.88440367,0.886238532,0.888073394,
0.889908257,0.891743119,0.893577982,0.895412844,0.897247706,0.899082569,
0.900917431,0.902752294,0.904587156,0.906422018,0.908256881,0.910091743,
0.911926606,0.913761468,0.91559633,0.917431193,0.919266055,0.921100917,
0.92293578,0.924770642,0.926605505,0.928440367,0.930275229,0.932110092,
0.933944954,0.935779817,0.937614679,0.939449541,0.941284404,0.943119266,
0.944954128,0.946788991,0.948623853,0.950458716,0.952293578,0.95412844,
0.955963303,0.957798165,0.959633028,0.96146789,0.963302752,0.965137615,
0.966972477,0.968807339,0.970642202,0.972477064,0.974311927,0.976146789,
0.977981651,0.979816514,0.981651376,0.983486239,0.985321101,0.987155963,
0.988990826,0.990825688,0.99266055,0.994495413,0.996330275,0.998165138,
1.),(0.,0.36),.UNSPECIFIED.);
#6284=B_SPLINE_SURFACE_WITH_KNOTS('',5,1,((#267743,#267744),(#267745,#267746),
(#267747,#267748),(#267749,#267750),(#267751,#267752),(#267753,#267754),
(#267755,#267756),(#267757,#267758),(#267759,#267760),(#267761,#267762),
(#267763,#267764),(#267765,#267766),(#267767,#267768),(#267769,#267770),
(#267771,#267772),(#267773,#267774),(#267775,#267776),(#267777,#267778),
(#267779,#267780),(#267781,#267782),(#267783,#267784),(#267785,#267786),
(#267787,#267788),(#267789,#267790),(#267791,#267792),(#267793,#267794),
(#267795,#267796),(#267797,#267798),(#267799,#267800),(#267801,#267802),
(#267803,#267804),(#267805,#267806),(#267807,#267808),(#267809,#267810),
(#267811,#267812),(#267813,#267814),(#267815,#267816),(#267817,#267818),
(#267819,#267820),(#267821,#267822),(#267823,#267824),(#267825,#267826),
(#267827,#267828),(#267829,#267830),(#267831,#267832),(#267833,#267834),
(#267835,#267836),(#267837,#267838),(#267839,#267840),(#267841,#267842),
(#267843,#267844),(#267845,#267846),(#267847,#267848),(#267849,#267850),
(#267851,#267852),(#267853,#267854),(#267855,#267856),(#267857,#267858),
(#267859,#267860),(#267861,#267862),(#267863,#267864),(#267865,#267866),
(#267867,#267868),(#267869,#267870),(#267871,#267872),(#267873,#267874),
(#267875,#267876),(#267877,#267878),(#267879,#267880),(#267881,#267882),
(#267883,#267884),(#267885,#267886),(#267887,#267888),(#267889,#267890),
(#267891,#267892),(#267893,#267894),(#267895,#267896),(#267897,#267898),
(#267899,#267900),(#267901,#267902),(#267903,#267904),(#267905,#267906),
(#267907,#267908),(#267909,#267910),(#267911,#267912),(#267913,#267914),
(#267915,#267916),(#267917,#267918),(#267919,#267920),(#267921,#267922),
(#267923,#267924),(#267925,#267926),(#267927,#267928),(#267929,#267930),
(#267931,#267932),(#267933,#267934),(#267935,#267936),(#267937,#267938),
(#267939,#267940),(#267941,#267942),(#267943,#267944),(#267945,#267946),
(#267947,#267948),(#267949,#267950),(#267951,#267952),(#267953,#267954),
(#267955,#267956),(#267957,#267958),(#267959,#267960),(#267961,#267962),
(#267963,#267964),(#267965,#267966),(#267967,#267968),(#267969,#267970),
(#267971,#267972),(#267973,#267974),(#267975,#267976),(#267977,#267978),
(#267979,#267980),(#267981,#267982),(#267983,#267984),(#267985,#267986),
(#267987,#267988),(#267989,#267990),(#267991,#267992),(#267993,#267994),
(#267995,#267996),(#267997,#267998),(#267999,#268000),(#268001,#268002),
(#268003,#268004),(#268005,#268006),(#268007,#268008),(#268009,#268010),
(#268011,#268012),(#268013,#268014),(#268015,#268016),(#268017,#268018),
(#268019,#268020),(#268021,#268022),(#268023,#268024),(#268025,#268026),
(#268027,#268028),(#268029,#268030),(#268031,#268032),(#268033,#268034),
(#268035,#268036),(#268037,#268038),(#268039,#268040),(#268041,#268042),
(#268043,#268044),(#268045,#268046),(#268047,#268048),(#268049,#268050),
(#268051,#268052),(#268053,#268054),(#268055,#268056),(#268057,#268058),
(#268059,#268060),(#268061,#268062),(#268063,#268064),(#268065,#268066),
(#268067,#268068),(#268069,#268070),(#268071,#268072),(#268073,#268074),
(#268075,#268076),(#268077,#268078),(#268079,#268080),(#268081,#268082),
(#268083,#268084),(#268085,#268086),(#268087,#268088),(#268089,#268090),
(#268091,#268092),(#268093,#268094),(#268095,#268096),(#268097,#268098),
(#268099,#268100),(#268101,#268102),(#268103,#268104),(#268105,#268106),
(#268107,#268108),(#268109,#268110),(#268111,#268112),(#268113,#268114),
(#268115,#268116),(#268117,#268118),(#268119,#268120),(#268121,#268122),
(#268123,#268124),(#268125,#268126),(#268127,#268128),(#268129,#268130),
(#268131,#268132),(#268133,#268134),(#268135,#268136),(#268137,#268138),
(#268139,#268140),(#268141,#268142),(#268143,#268144),(#268145,#268146),
(#268147,#268148),(#268149,#268150),(#268151,#268152),(#268153,#268154),
(#268155,#268156),(#268157,#268158),(#268159,#268160),(#268161,#268162),
(#268163,#268164),(#268165,#268166),(#268167,#268168),(#268169,#268170),
(#268171,#268172),(#268173,#268174),(#268175,#268176),(#268177,#268178),
(#268179,#268180),(#268181,#268182),(#268183,#268184),(#268185,#268186),
(#268187,#268188),(#268189,#268190),(#268191,#268192),(#268193,#268194),
(#268195,#268196),(#268197,#268198),(#268199,#268200),(#268201,#268202),
(#268203,#268204),(#268205,#268206),(#268207,#268208),(#268209,#268210),
(#268211,#268212),(#268213,#268214),(#268215,#268216),(#268217,#268218),
(#268219,#268220),(#268221,#268222),(#268223,#268224),(#268225,#268226),
(#268227,#268228),(#268229,#268230),(#268231,#268232),(#268233,#268234),
(#268235,#268236),(#268237,#268238),(#268239,#268240),(#268241,#268242),
(#268243,#268244),(#268245,#268246),(#268247,#268248),(#268249,#268250),
(#268251,#268252),(#268253,#268254),(#268255,#268256),(#268257,#268258),
(#268259,#268260),(#268261,#268262),(#268263,#268264),(#268265,#268266),
(#268267,#268268),(#268269,#268270),(#268271,#268272),(#268273,#268274),
(#268275,#268276),(#268277,#268278),(#268279,#268280),(#268281,#268282),
(#268283,#268284),(#268285,#268286),(#268287,#268288),(#268289,#268290),
(#268291,#268292),(#268293,#268294),(#268295,#268296),(#268297,#268298),
(#268299,#268300),(#268301,#268302),(#268303,#268304),(#268305,#268306),
(#268307,#268308),(#268309,#268310),(#268311,#268312),(#268313,#268314),
(#268315,#268316),(#268317,#268318),(#268319,#268320),(#268321,#268322),
(#268323,#268324),(#268325,#268326),(#268327,#268328),(#268329,#268330),
(#268331,#268332),(#268333,#268334),(#268335,#268336),(#268337,#268338),
(#268339,#268340),(#268341,#268342),(#268343,#268344),(#268345,#268346),
(#268347,#268348),(#268349,#268350),(#268351,#268352),(#268353,#268354),
(#268355,#268356),(#268357,#268358),(#268359,#268360),(#268361,#268362),
(#268363,#268364),(#268365,#268366),(#268367,#268368),(#268369,#268370),
(#268371,#268372),(#268373,#268374),(#268375,#268376),(#268377,#268378),
(#268379,#268380),(#268381,#268382),(#268383,#268384),(#268385,#268386),
(#268387,#268388),(#268389,#268390),(#268391,#268392),(#268393,#268394),
(#268395,#268396),(#268397,#268398),(#268399,#268400),(#268401,#268402),
(#268403,#268404),(#268405,#268406),(#268407,#268408),(#268409,#268410),
(#268411,#268412),(#268413,#268414),(#268415,#268416),(#268417,#268418),
(#268419,#268420),(#268421,#268422),(#268423,#268424),(#268425,#268426),
(#268427,#268428),(#268429,#268430),(#268431,#268432),(#268433,#268434),
(#268435,#268436),(#268437,#268438),(#268439,#268440),(#268441,#268442),
(#268443,#268444),(#268445,#268446),(#268447,#268448),(#268449,#268450),
(#268451,#268452),(#268453,#268454),(#268455,#268456),(#268457,#268458),
(#268459,#268460),(#268461,#268462),(#268463,#268464),(#268465,#268466),
(#268467,#268468),(#268469,#268470),(#268471,#268472),(#268473,#268474),
(#268475,#268476),(#268477,#268478),(#268479,#268480),(#268481,#268482),
(#268483,#268484),(#268485,#268486),(#268487,#268488),(#268489,#268490),
(#268491,#268492),(#268493,#268494),(#268495,#268496),(#268497,#268498),
(#268499,#268500),(#268501,#268502),(#268503,#268504),(#268505,#268506),
(#268507,#268508),(#268509,#268510),(#268511,#268512),(#268513,#268514),
(#268515,#268516),(#268517,#268518),(#268519,#268520),(#268521,#268522),
(#268523,#268524),(#268525,#268526),(#268527,#268528),(#268529,#268530),
(#268531,#268532),(#268533,#268534),(#268535,#268536),(#268537,#268538),
(#268539,#268540),(#268541,#268542),(#268543,#268544),(#268545,#268546),
(#268547,#268548),(#268549,#268550),(#268551,#268552),(#268553,#268554),
(#268555,#268556),(#268557,#268558),(#268559,#268560),(#268561,#268562),
(#268563,#268564),(#268565,#268566),(#268567,#268568),(#268569,#268570),
(#268571,#268572),(#268573,#268574),(#268575,#268576),(#268577,#268578),
(#268579,#268580),(#268581,#268582),(#268583,#268584),(#268585,#268586),
(#268587,#268588),(#268589,#268590),(#268591,#268592),(#268593,#268594),
(#268595,#268596),(#268597,#268598),(#268599,#268600),(#268601,#268602),
(#268603,#268604),(#268605,#268606),(#268607,#268608),(#268609,#268610),
(#268611,#268612),(#268613,#268614),(#268615,#268616),(#268617,#268618),
(#268619,#268620),(#268621,#268622),(#268623,#268624),(#268625,#268626),
(#268627,#268628),(#268629,#268630),(#268631,#268632),(#268633,#268634),
(#268635,#268636),(#268637,#268638),(#268639,#268640),(#268641,#268642),
(#268643,#268644),(#268645,#268646),(#268647,#268648),(#268649,#268650),
(#268651,#268652),(#268653,#268654),(#268655,#268656),(#268657,#268658),
(#268659,#268660),(#268661,#268662),(#268663,#268664),(#268665,#268666),
(#268667,#268668),(#268669,#268670),(#268671,#268672),(#268673,#268674),
(#268675,#268676),(#268677,#268678),(#268679,#268680),(#268681,#268682),
(#268683,#268684),(#268685,#268686)),.UNSPECIFIED.,.F.,.F.,.F.,(6,1,1,1,
1,1,1,1,1,1,1,1,1,1,1,1,1,1,1,1,1,1,1,1,1,1,1,1,1,1,1,1,1,1,1,1,1,1,1,1,
1,1,1,1,1,1,1,1,1,1,1,1,1,1,1,1,1,1,1,1,1,1,1,1,1,1,1,1,1,1,1,1,1,1,1,1,
1,1,1,1,1,1,1,1,1,1,1,1,1,1,1,1,1,1,1,1,1,1,1,1,1,1,1,1,1,1,1,1,1,1,1,1,
1,1,1,1,1,1,1,1,1,1,1,1,1,1,1,1,1,1,1,1,1,1,1,1,1,1,1,1,1,1,1,1,1,1,1,1,
1,1,1,1,1,1,1,1,1,1,1,1,1,1,1,1,1,1,1,1,1,1,1,1,1,1,1,1,1,1,1,1,1,1,1,1,
1,1,1,1,1,1,1,1,1,1,1,1,1,1,1,1,1,1,1,1,1,1,1,1,1,1,1,1,1,1,1,1,1,1,1,1,
1,1,1,1,1,1,1,1,1,1,1,1,1,1,1,1,1,1,1,1,1,1,1,1,1,1,1,1,1,1,1,1,1,1,1,1,
1,1,1,1,1,1,1,1,1,1,1,1,1,1,1,1,1,1,1,1,1,1,1,1,1,1,1,1,1,1,1,1,1,1,1,1,
1,1,1,1,1,1,1,1,1,1,1,1,1,1,1,1,1,1,1,1,1,1,1,1,1,1,1,1,1,1,1,1,1,1,1,1,
1,1,1,1,1,1,1,1,1,1,1,1,1,1,1,1,1,1,1,1,1,1,1,1,1,1,1,1,1,1,1,1,1,1,1,1,
1,1,1,1,1,1,1,1,1,1,1,1,1,1,1,1,1,1,1,1,1,1,1,1,1,1,1,1,1,1,1,1,1,1,1,1,
1,1,1,1,1,1,1,1,1,1,1,1,1,1,1,1,1,1,1,1,1,1,1,1,1,1,1,1,1,1,1,1,1,1,1,1,
1,1,1,1,1,1,1,1,1,1,1,1,1,1,1,1,1,1,1,1,1,1,1,1,1,1,1,1,1,1,1,6),(2,2),
(-1.,-0.998165138,-0.996330275,-0.994495413,-0.99266055,-0.990825688,-0.988990826,
-0.987155963,-0.985321101,-0.983486239,-0.981651376,-0.979816514,-0.977981651,
-0.976146789,-0.974311927,-0.972477064,-0.970642202,-0.968807339,-0.966972477,
-0.965137615,-0.963302752,-0.96146789,-0.959633028,-0.957798165,-0.955963303,
-0.95412844,-0.952293578,-0.950458716,-0.948623853,-0.946788991,-0.944954128,
-0.943119266,-0.941284404,-0.939449541,-0.937614679,-0.935779817,-0.933944954,
-0.932110092,-0.930275229,-0.928440367,-0.926605505,-0.924770642,-0.92293578,
-0.921100917,-0.919266055,-0.917431193,-0.91559633,-0.913761468,-0.911926606,
-0.910091743,-0.908256881,-0.906422018,-0.904587156,-0.902752294,-0.900917431,
-0.899082569,-0.897247706,-0.895412844,-0.893577982,-0.891743119,-0.889908257,
-0.888073394,-0.886238532,-0.88440367,-0.882568807,-0.880733945,-0.878899083,
-0.87706422,-0.875229358,-0.873394495,-0.871559633,-0.869724771,-0.867889908,
-0.866055046,-0.864220183,-0.862385321,-0.860550459,-0.858715596,-0.856880734,
-0.855045872,-0.853211009,-0.851376147,-0.849541284,-0.847706422,-0.84587156,
-0.844036697,-0.842201835,-0.840366972,-0.83853211,-0.836697248,-0.834862385,
-0.833027523,-0.831192661,-0.829357798,-0.827522936,-0.825688073,-0.823853211,
-0.822018349,-0.820183486,-0.818348624,-0.816513761,-0.814678899,-0.812844037,
-0.811009174,-0.809174312,-0.80733945,-0.805504587,-0.803669725,-0.801834862,
-0.8,-0.798165138,-0.796330275,-0.794495413,-0.79266055,-0.790825688,-0.788990826,
-0.787155963,-0.785321101,-0.783486239,-0.781651376,-0.779816514,-0.777981651,
-0.776146789,-0.774311927,-0.772477064,-0.770642202,-0.768807339,-0.766972477,
-0.765137615,-0.763302752,-0.76146789,-0.759633028,-0.757798165,-0.755963303,
-0.75412844,-0.752293578,-0.750458716,-0.748623853,-0.746788991,-0.744954128,
-0.743119266,-0.741284404,-0.739449541,-0.737614679,-0.735779817,-0.733944954,
-0.732110092,-0.730275229,-0.728440367,-0.726605505,-0.724770642,-0.72293578,
-0.721100917,-0.719266055,-0.717431193,-0.71559633,-0.713761468,-0.711926606,
-0.710091743,-0.708256881,-0.706422018,-0.704587156,-0.702752294,-0.700917431,
-0.699082569,-0.697247706,-0.695412844,-0.693577982,-0.691743119,-0.689908257,
-0.688073394,-0.686238532,-0.68440367,-0.682568807,-0.680733945,-0.678899083,
-0.67706422,-0.675229358,-0.673394495,-0.671559633,-0.669724771,-0.667889908,
-0.666055046,-0.664220183,-0.662385321,-0.660550459,-0.658715596,-0.656880734,
-0.655045872,-0.653211009,-0.651376147,-0.649541284,-0.647706422,-0.64587156,
-0.644036697,-0.642201835,-0.640366972,-0.63853211,-0.636697248,-0.634862385,
-0.633027523,-0.631192661,-0.629357798,-0.627522936,-0.625688073,-0.623853211,
-0.622018349,-0.620183486,-0.618348624,-0.616513761,-0.614678899,-0.612844037,
-0.611009174,-0.609174312,-0.60733945,-0.605504587,-0.603669725,-0.601834862,
-0.6,-0.598165138,-0.596330275,-0.594495413,-0.59266055,-0.590825688,-0.588990826,
-0.587155963,-0.585321101,-0.583486239,-0.581651376,-0.579816514,-0.577981651,
-0.576146789,-0.574311927,-0.572477064,-0.570642202,-0.568807339,-0.566972477,
-0.565137615,-0.563302752,-0.56146789,-0.559633028,-0.557798165,-0.555963303,
-0.55412844,-0.552293578,-0.550458716,-0.548623853,-0.546788991,-0.544954128,
-0.543119266,-0.541284404,-0.539449541,-0.537614679,-0.535779817,-0.533944954,
-0.532110092,-0.530275229,-0.528440367,-0.526605505,-0.524770642,-0.52293578,
-0.521100917,-0.519266055,-0.517431193,-0.51559633,-0.513761468,-0.511926606,
-0.510091743,-0.508256881,-0.506422018,-0.504587156,-0.502752294,-0.500917431,
-0.499082569,-0.497247706,-0.495412844,-0.493577982,-0.491743119,-0.489908257,
-0.488073394,-0.486238532,-0.48440367,-0.482568807,-0.480733945,-0.478899083,
-0.47706422,-0.475229358,-0.473394495,-0.471559633,-0.469724771,-0.467889908,
-0.466055046,-0.464220183,-0.462385321,-0.460550459,-0.458715596,-0.456880734,
-0.455045872,-0.453211009,-0.451376147,-0.449541284,-0.447706422,-0.44587156,
-0.444036697,-0.442201835,-0.440366972,-0.43853211,-0.436697248,-0.434862385,
-0.433027523,-0.431192661,-0.429357798,-0.427522936,-0.425688073,-0.423853211,
-0.422018349,-0.420183486,-0.418348624,-0.416513761,-0.414678899,-0.412844037,
-0.411009174,-0.409174312,-0.40733945,-0.405504587,-0.403669725,-0.401834862,
-0.4,-0.398165138,-0.396330275,-0.394495413,-0.39266055,-0.390825688,-0.388990826,
-0.387155963,-0.385321101,-0.383486239,-0.381651376,-0.379816514,-0.377981651,
-0.376146789,-0.374311927,-0.372477064,-0.370642202,-0.368807339,-0.366972477,
-0.365137615,-0.363302752,-0.36146789,-0.359633028,-0.357798165,-0.355963303,
-0.35412844,-0.352293578,-0.350458716,-0.348623853,-0.346788991,-0.344954128,
-0.343119266,-0.341284404,-0.339449541,-0.337614679,-0.335779817,-0.333944954,
-0.332110092,-0.330275229,-0.328440367,-0.326605505,-0.324770642,-0.32293578,
-0.321100917,-0.319266055,-0.317431193,-0.31559633,-0.313761468,-0.311926606,
-0.310091743,-0.308256881,-0.306422018,-0.304587156,-0.302752294,-0.300917431,
-0.299082569,-0.297247706,-0.295412844,-0.293577982,-0.291743119,-0.289908257,
-0.288073394,-0.286238532,-0.28440367,-0.282568807,-0.280733945,-0.278899083,
-0.27706422,-0.275229358,-0.273394495,-0.271559633,-0.269724771,-0.267889908,
-0.266055046,-0.264220183,-0.262385321,-0.260550459,-0.258715596,-0.256880734,
-0.255045872,-0.253211009,-0.251376147,-0.249541284,-0.247706422,-0.24587156,
-0.244036697,-0.242201835,-0.240366972,-0.23853211,-0.236697248,-0.234862385,
-0.233027523,-0.231192661,-0.229357798,-0.227522936,-0.225688073,-0.223853211,
-0.222018349,-0.220183486,-0.218348624,-0.216513761,-0.214678899,-0.212844037,
-0.211009174,-0.209174312,-0.20733945,-0.205504587,-0.203669725,-0.201834862,
-0.2,-0.198165138,-0.196330275,-0.194495413,-0.19266055,-0.190825688,-0.188990826,
-0.187155963,-0.185321101,-0.183486239,-0.181651376,-0.179816514,-0.177981651,
-0.176146789,-0.174311927,-0.172477064,-0.170642202,-0.168807339,-0.166972477,
-0.165137615,-0.163302752,-0.16146789,-0.159633028,-0.157798165,-0.155963303,
-0.15412844,-0.152293578,-0.150458716,-0.148623853,-0.146788991,-0.144954128,
-0.143172103),(0.,0.36),.UNSPECIFIED.);
#6285=B_SPLINE_SURFACE_WITH_KNOTS('',5,1,((#269647,#269648),(#269649,#269650),
(#269651,#269652),(#269653,#269654),(#269655,#269656),(#269657,#269658),
(#269659,#269660),(#269661,#269662),(#269663,#269664),(#269665,#269666),
(#269667,#269668),(#269669,#269670),(#269671,#269672),(#269673,#269674),
(#269675,#269676),(#269677,#269678),(#269679,#269680),(#269681,#269682),
(#269683,#269684),(#269685,#269686),(#269687,#269688),(#269689,#269690),
(#269691,#269692),(#269693,#269694),(#269695,#269696),(#269697,#269698),
(#269699,#269700),(#269701,#269702),(#269703,#269704),(#269705,#269706),
(#269707,#269708),(#269709,#269710),(#269711,#269712),(#269713,#269714),
(#269715,#269716),(#269717,#269718),(#269719,#269720),(#269721,#269722),
(#269723,#269724),(#269725,#269726),(#269727,#269728),(#269729,#269730),
(#269731,#269732),(#269733,#269734),(#269735,#269736),(#269737,#269738),
(#269739,#269740),(#269741,#269742),(#269743,#269744),(#269745,#269746),
(#269747,#269748),(#269749,#269750),(#269751,#269752),(#269753,#269754),
(#269755,#269756),(#269757,#269758),(#269759,#269760),(#269761,#269762),
(#269763,#269764),(#269765,#269766),(#269767,#269768),(#269769,#269770),
(#269771,#269772),(#269773,#269774),(#269775,#269776),(#269777,#269778),
(#269779,#269780),(#269781,#269782),(#269783,#269784),(#269785,#269786),
(#269787,#269788),(#269789,#269790),(#269791,#269792),(#269793,#269794),
(#269795,#269796),(#269797,#269798),(#269799,#269800),(#269801,#269802),
(#269803,#269804),(#269805,#269806),(#269807,#269808),(#269809,#269810),
(#269811,#269812),(#269813,#269814),(#269815,#269816),(#269817,#269818),
(#269819,#269820),(#269821,#269822),(#269823,#269824),(#269825,#269826),
(#269827,#269828),(#269829,#269830),(#269831,#269832),(#269833,#269834),
(#269835,#269836),(#269837,#269838),(#269839,#269840),(#269841,#269842),
(#269843,#269844),(#269845,#269846),(#269847,#269848),(#269849,#269850),
(#269851,#269852),(#269853,#269854),(#269855,#269856),(#269857,#269858),
(#269859,#269860),(#269861,#269862),(#269863,#269864),(#269865,#269866),
(#269867,#269868),(#269869,#269870),(#269871,#269872),(#269873,#269874),
(#269875,#269876),(#269877,#269878),(#269879,#269880),(#269881,#269882),
(#269883,#269884),(#269885,#269886),(#269887,#269888),(#269889,#269890),
(#269891,#269892),(#269893,#269894),(#269895,#269896),(#269897,#269898),
(#269899,#269900),(#269901,#269902),(#269903,#269904),(#269905,#269906),
(#269907,#269908),(#269909,#269910),(#269911,#269912),(#269913,#269914),
(#269915,#269916),(#269917,#269918),(#269919,#269920),(#269921,#269922),
(#269923,#269924),(#269925,#269926),(#269927,#269928),(#269929,#269930),
(#269931,#269932),(#269933,#269934),(#269935,#269936),(#269937,#269938),
(#269939,#269940),(#269941,#269942),(#269943,#269944),(#269945,#269946),
(#269947,#269948),(#269949,#269950),(#269951,#269952),(#269953,#269954),
(#269955,#269956),(#269957,#269958),(#269959,#269960),(#269961,#269962),
(#269963,#269964),(#269965,#269966),(#269967,#269968),(#269969,#269970),
(#269971,#269972),(#269973,#269974),(#269975,#269976),(#269977,#269978),
(#269979,#269980),(#269981,#269982),(#269983,#269984),(#269985,#269986),
(#269987,#269988),(#269989,#269990),(#269991,#269992),(#269993,#269994),
(#269995,#269996),(#269997,#269998),(#269999,#270000),(#270001,#270002),
(#270003,#270004),(#270005,#270006),(#270007,#270008),(#270009,#270010),
(#270011,#270012),(#270013,#270014),(#270015,#270016),(#270017,#270018),
(#270019,#270020),(#270021,#270022),(#270023,#270024),(#270025,#270026),
(#270027,#270028),(#270029,#270030),(#270031,#270032),(#270033,#270034),
(#270035,#270036),(#270037,#270038),(#270039,#270040),(#270041,#270042),
(#270043,#270044),(#270045,#270046),(#270047,#270048),(#270049,#270050),
(#270051,#270052),(#270053,#270054),(#270055,#270056),(#270057,#270058),
(#270059,#270060),(#270061,#270062),(#270063,#270064),(#270065,#270066),
(#270067,#270068),(#270069,#270070),(#270071,#270072),(#270073,#270074),
(#270075,#270076),(#270077,#270078),(#270079,#270080),(#270081,#270082),
(#270083,#270084),(#270085,#270086),(#270087,#270088),(#270089,#270090),
(#270091,#270092),(#270093,#270094),(#270095,#270096),(#270097,#270098),
(#270099,#270100),(#270101,#270102),(#270103,#270104),(#270105,#270106),
(#270107,#270108),(#270109,#270110),(#270111,#270112),(#270113,#270114),
(#270115,#270116),(#270117,#270118),(#270119,#270120),(#270121,#270122),
(#270123,#270124),(#270125,#270126),(#270127,#270128),(#270129,#270130),
(#270131,#270132),(#270133,#270134),(#270135,#270136),(#270137,#270138),
(#270139,#270140),(#270141,#270142),(#270143,#270144),(#270145,#270146),
(#270147,#270148),(#270149,#270150),(#270151,#270152),(#270153,#270154),
(#270155,#270156),(#270157,#270158),(#270159,#270160),(#270161,#270162),
(#270163,#270164),(#270165,#270166),(#270167,#270168),(#270169,#270170),
(#270171,#270172),(#270173,#270174),(#270175,#270176),(#270177,#270178),
(#270179,#270180),(#270181,#270182),(#270183,#270184),(#270185,#270186),
(#270187,#270188),(#270189,#270190),(#270191,#270192),(#270193,#270194),
(#270195,#270196),(#270197,#270198),(#270199,#270200),(#270201,#270202),
(#270203,#270204),(#270205,#270206),(#270207,#270208),(#270209,#270210),
(#270211,#270212),(#270213,#270214),(#270215,#270216),(#270217,#270218),
(#270219,#270220),(#270221,#270222),(#270223,#270224),(#270225,#270226),
(#270227,#270228),(#270229,#270230),(#270231,#270232),(#270233,#270234),
(#270235,#270236),(#270237,#270238),(#270239,#270240),(#270241,#270242),
(#270243,#270244),(#270245,#270246),(#270247,#270248),(#270249,#270250),
(#270251,#270252),(#270253,#270254),(#270255,#270256),(#270257,#270258),
(#270259,#270260),(#270261,#270262),(#270263,#270264),(#270265,#270266),
(#270267,#270268),(#270269,#270270),(#270271,#270272),(#270273,#270274),
(#270275,#270276),(#270277,#270278),(#270279,#270280),(#270281,#270282),
(#270283,#270284),(#270285,#270286),(#270287,#270288),(#270289,#270290),
(#270291,#270292),(#270293,#270294),(#270295,#270296),(#270297,#270298),
(#270299,#270300),(#270301,#270302),(#270303,#270304),(#270305,#270306),
(#270307,#270308),(#270309,#270310),(#270311,#270312),(#270313,#270314),
(#270315,#270316),(#270317,#270318),(#270319,#270320),(#270321,#270322),
(#270323,#270324),(#270325,#270326),(#270327,#270328),(#270329,#270330),
(#270331,#270332),(#270333,#270334),(#270335,#270336),(#270337,#270338),
(#270339,#270340),(#270341,#270342),(#270343,#270344),(#270345,#270346),
(#270347,#270348),(#270349,#270350),(#270351,#270352),(#270353,#270354),
(#270355,#270356),(#270357,#270358),(#270359,#270360),(#270361,#270362),
(#270363,#270364),(#270365,#270366),(#270367,#270368),(#270369,#270370),
(#270371,#270372),(#270373,#270374),(#270375,#270376),(#270377,#270378),
(#270379,#270380),(#270381,#270382),(#270383,#270384),(#270385,#270386),
(#270387,#270388),(#270389,#270390),(#270391,#270392),(#270393,#270394),
(#270395,#270396),(#270397,#270398),(#270399,#270400),(#270401,#270402),
(#270403,#270404),(#270405,#270406),(#270407,#270408),(#270409,#270410),
(#270411,#270412),(#270413,#270414),(#270415,#270416),(#270417,#270418),
(#270419,#270420),(#270421,#270422),(#270423,#270424),(#270425,#270426),
(#270427,#270428),(#270429,#270430),(#270431,#270432),(#270433,#270434),
(#270435,#270436),(#270437,#270438),(#270439,#270440),(#270441,#270442),
(#270443,#270444),(#270445,#270446),(#270447,#270448),(#270449,#270450),
(#270451,#270452),(#270453,#270454),(#270455,#270456),(#270457,#270458),
(#270459,#270460),(#270461,#270462),(#270463,#270464),(#270465,#270466),
(#270467,#270468),(#270469,#270470),(#270471,#270472),(#270473,#270474),
(#270475,#270476),(#270477,#270478),(#270479,#270480),(#270481,#270482),
(#270483,#270484),(#270485,#270486),(#270487,#270488),(#270489,#270490),
(#270491,#270492),(#270493,#270494),(#270495,#270496),(#270497,#270498),
(#270499,#270500),(#270501,#270502),(#270503,#270504),(#270505,#270506),
(#270507,#270508),(#270509,#270510),(#270511,#270512),(#270513,#270514),
(#270515,#270516),(#270517,#270518),(#270519,#270520),(#270521,#270522),
(#270523,#270524),(#270525,#270526),(#270527,#270528),(#270529,#270530),
(#270531,#270532),(#270533,#270534),(#270535,#270536),(#270537,#270538),
(#270539,#270540),(#270541,#270542),(#270543,#270544),(#270545,#270546),
(#270547,#270548),(#270549,#270550),(#270551,#270552),(#270553,#270554),
(#270555,#270556),(#270557,#270558),(#270559,#270560),(#270561,#270562),
(#270563,#270564),(#270565,#270566),(#270567,#270568),(#270569,#270570),
(#270571,#270572),(#270573,#270574),(#270575,#270576),(#270577,#270578),
(#270579,#270580),(#270581,#270582),(#270583,#270584),(#270585,#270586),
(#270587,#270588),(#270589,#270590)),.UNSPECIFIED.,.F.,.F.,.F.,(6,1,1,1,
1,1,1,1,1,1,1,1,1,1,1,1,1,1,1,1,1,1,1,1,1,1,1,1,1,1,1,1,1,1,1,1,1,1,1,1,
1,1,1,1,1,1,1,1,1,1,1,1,1,1,1,1,1,1,1,1,1,1,1,1,1,1,1,1,1,1,1,1,1,1,1,1,
1,1,1,1,1,1,1,1,1,1,1,1,1,1,1,1,1,1,1,1,1,1,1,1,1,1,1,1,1,1,1,1,1,1,1,1,
1,1,1,1,1,1,1,1,1,1,1,1,1,1,1,1,1,1,1,1,1,1,1,1,1,1,1,1,1,1,1,1,1,1,1,1,
1,1,1,1,1,1,1,1,1,1,1,1,1,1,1,1,1,1,1,1,1,1,1,1,1,1,1,1,1,1,1,1,1,1,1,1,
1,1,1,1,1,1,1,1,1,1,1,1,1,1,1,1,1,1,1,1,1,1,1,1,1,1,1,1,1,1,1,1,1,1,1,1,
1,1,1,1,1,1,1,1,1,1,1,1,1,1,1,1,1,1,1,1,1,1,1,1,1,1,1,1,1,1,1,1,1,1,1,1,
1,1,1,1,1,1,1,1,1,1,1,1,1,1,1,1,1,1,1,1,1,1,1,1,1,1,1,1,1,1,1,1,1,1,1,1,
1,1,1,1,1,1,1,1,1,1,1,1,1,1,1,1,1,1,1,1,1,1,1,1,1,1,1,1,1,1,1,1,1,1,1,1,
1,1,1,1,1,1,1,1,1,1,1,1,1,1,1,1,1,1,1,1,1,1,1,1,1,1,1,1,1,1,1,1,1,1,1,1,
1,1,1,1,1,1,1,1,1,1,1,1,1,1,1,1,1,1,1,1,1,1,1,1,1,1,1,1,1,1,1,1,1,1,1,1,
1,1,1,1,1,1,1,1,1,1,1,1,1,1,1,1,1,1,1,1,1,1,1,1,1,1,1,1,1,1,1,1,1,1,1,1,
1,1,1,1,1,1,1,1,1,1,1,1,1,1,1,1,1,1,1,1,1,1,1,1,1,1,1,1,1,1,1,6),(2,2),
(-1.,-0.998165138,-0.996330275,-0.994495413,-0.99266055,-0.990825688,-0.988990826,
-0.987155963,-0.985321101,-0.983486239,-0.981651376,-0.979816514,-0.977981651,
-0.976146789,-0.974311927,-0.972477064,-0.970642202,-0.968807339,-0.966972477,
-0.965137615,-0.963302752,-0.96146789,-0.959633028,-0.957798165,-0.955963303,
-0.95412844,-0.952293578,-0.950458716,-0.948623853,-0.946788991,-0.944954128,
-0.943119266,-0.941284404,-0.939449541,-0.937614679,-0.935779817,-0.933944954,
-0.932110092,-0.930275229,-0.928440367,-0.926605505,-0.924770642,-0.92293578,
-0.921100917,-0.919266055,-0.917431193,-0.91559633,-0.913761468,-0.911926606,
-0.910091743,-0.908256881,-0.906422018,-0.904587156,-0.902752294,-0.900917431,
-0.899082569,-0.897247706,-0.895412844,-0.893577982,-0.891743119,-0.889908257,
-0.888073394,-0.886238532,-0.88440367,-0.882568807,-0.880733945,-0.878899083,
-0.87706422,-0.875229358,-0.873394495,-0.871559633,-0.869724771,-0.867889908,
-0.866055046,-0.864220183,-0.862385321,-0.860550459,-0.858715596,-0.856880734,
-0.855045872,-0.853211009,-0.851376147,-0.849541284,-0.847706422,-0.84587156,
-0.844036697,-0.842201835,-0.840366972,-0.83853211,-0.836697248,-0.834862385,
-0.833027523,-0.831192661,-0.829357798,-0.827522936,-0.825688073,-0.823853211,
-0.822018349,-0.820183486,-0.818348624,-0.816513761,-0.814678899,-0.812844037,
-0.811009174,-0.809174312,-0.80733945,-0.805504587,-0.803669725,-0.801834862,
-0.8,-0.798165138,-0.796330275,-0.794495413,-0.79266055,-0.790825688,-0.788990826,
-0.787155963,-0.785321101,-0.783486239,-0.781651376,-0.779816514,-0.777981651,
-0.776146789,-0.774311927,-0.772477064,-0.770642202,-0.768807339,-0.766972477,
-0.765137615,-0.763302752,-0.76146789,-0.759633028,-0.757798165,-0.755963303,
-0.75412844,-0.752293578,-0.750458716,-0.748623853,-0.746788991,-0.744954128,
-0.743119266,-0.741284404,-0.739449541,-0.737614679,-0.735779817,-0.733944954,
-0.732110092,-0.730275229,-0.728440367,-0.726605505,-0.724770642,-0.72293578,
-0.721100917,-0.719266055,-0.717431193,-0.71559633,-0.713761468,-0.711926606,
-0.710091743,-0.708256881,-0.706422018,-0.704587156,-0.702752294,-0.700917431,
-0.699082569,-0.697247706,-0.695412844,-0.693577982,-0.691743119,-0.689908257,
-0.688073394,-0.686238532,-0.68440367,-0.682568807,-0.680733945,-0.678899083,
-0.67706422,-0.675229358,-0.673394495,-0.671559633,-0.669724771,-0.667889908,
-0.666055046,-0.664220183,-0.662385321,-0.660550459,-0.658715596,-0.656880734,
-0.655045872,-0.653211009,-0.651376147,-0.649541284,-0.647706422,-0.64587156,
-0.644036697,-0.642201835,-0.640366972,-0.63853211,-0.636697248,-0.634862385,
-0.633027523,-0.631192661,-0.629357798,-0.627522936,-0.625688073,-0.623853211,
-0.622018349,-0.620183486,-0.618348624,-0.616513761,-0.614678899,-0.612844037,
-0.611009174,-0.609174312,-0.60733945,-0.605504587,-0.603669725,-0.601834862,
-0.6,-0.598165138,-0.596330275,-0.594495413,-0.59266055,-0.590825688,-0.588990826,
-0.587155963,-0.585321101,-0.583486239,-0.581651376,-0.579816514,-0.577981651,
-0.576146789,-0.574311927,-0.572477064,-0.570642202,-0.568807339,-0.566972477,
-0.565137615,-0.563302752,-0.56146789,-0.559633028,-0.557798165,-0.555963303,
-0.55412844,-0.552293578,-0.550458716,-0.548623853,-0.546788991,-0.544954128,
-0.543119266,-0.541284404,-0.539449541,-0.537614679,-0.535779817,-0.533944954,
-0.532110092,-0.530275229,-0.528440367,-0.526605505,-0.524770642,-0.52293578,
-0.521100917,-0.519266055,-0.517431193,-0.51559633,-0.513761468,-0.511926606,
-0.510091743,-0.508256881,-0.506422018,-0.504587156,-0.502752294,-0.500917431,
-0.499082569,-0.497247706,-0.495412844,-0.493577982,-0.491743119,-0.489908257,
-0.488073394,-0.486238532,-0.48440367,-0.482568807,-0.480733945,-0.478899083,
-0.47706422,-0.475229358,-0.473394495,-0.471559633,-0.469724771,-0.467889908,
-0.466055046,-0.464220183,-0.462385321,-0.460550459,-0.458715596,-0.456880734,
-0.455045872,-0.453211009,-0.451376147,-0.449541284,-0.447706422,-0.44587156,
-0.444036697,-0.442201835,-0.440366972,-0.43853211,-0.436697248,-0.434862385,
-0.433027523,-0.431192661,-0.429357798,-0.427522936,-0.425688073,-0.423853211,
-0.422018349,-0.420183486,-0.418348624,-0.416513761,-0.414678899,-0.412844037,
-0.411009174,-0.409174312,-0.40733945,-0.405504587,-0.403669725,-0.401834862,
-0.4,-0.398165138,-0.396330275,-0.394495413,-0.39266055,-0.390825688,-0.388990826,
-0.387155963,-0.385321101,-0.383486239,-0.381651376,-0.379816514,-0.377981651,
-0.376146789,-0.374311927,-0.372477064,-0.370642202,-0.368807339,-0.366972477,
-0.365137615,-0.363302752,-0.36146789,-0.359633028,-0.357798165,-0.355963303,
-0.35412844,-0.352293578,-0.350458716,-0.348623853,-0.346788991,-0.344954128,
-0.343119266,-0.341284404,-0.339449541,-0.337614679,-0.335779817,-0.333944954,
-0.332110092,-0.330275229,-0.328440367,-0.326605505,-0.324770642,-0.32293578,
-0.321100917,-0.319266055,-0.317431193,-0.31559633,-0.313761468,-0.311926606,
-0.310091743,-0.308256881,-0.306422018,-0.304587156,-0.302752294,-0.300917431,
-0.299082569,-0.297247706,-0.295412844,-0.293577982,-0.291743119,-0.289908257,
-0.288073394,-0.286238532,-0.28440367,-0.282568807,-0.280733945,-0.278899083,
-0.27706422,-0.275229358,-0.273394495,-0.271559633,-0.269724771,-0.267889908,
-0.266055046,-0.264220183,-0.262385321,-0.260550459,-0.258715596,-0.256880734,
-0.255045872,-0.253211009,-0.251376147,-0.249541284,-0.247706422,-0.24587156,
-0.244036697,-0.242201835,-0.240366972,-0.23853211,-0.236697248,-0.234862385,
-0.233027523,-0.231192661,-0.229357798,-0.227522936,-0.225688073,-0.223853211,
-0.222018349,-0.220183486,-0.218348624,-0.216513761,-0.214678899,-0.212844037,
-0.211009174,-0.209174312,-0.20733945,-0.205504587,-0.203669725,-0.201834862,
-0.2,-0.198165138,-0.196330275,-0.194495413,-0.19266055,-0.190825688,-0.188990826,
-0.187155963,-0.185321101,-0.183486239,-0.181651376,-0.179816514,-0.177981651,
-0.176146789,-0.174311927,-0.172477064,-0.170642202,-0.168807339,-0.166972477,
-0.165137615,-0.163302752,-0.16146789,-0.159633028,-0.157798165,-0.155963303,
-0.15412844,-0.152293578,-0.150458716,-0.148623853,-0.146788991,-0.144954128,
-0.143172103),(0.,0.36),.UNSPECIFIED.);
#6286=B_SPLINE_SURFACE_WITH_KNOTS('',5,1,((#271235,#271236),(#271237,#271238),
(#271239,#271240),(#271241,#271242),(#271243,#271244),(#271245,#271246),
(#271247,#271248),(#271249,#271250),(#271251,#271252),(#271253,#271254),
(#271255,#271256),(#271257,#271258),(#271259,#271260),(#271261,#271262),
(#271263,#271264),(#271265,#271266),(#271267,#271268),(#271269,#271270),
(#271271,#271272),(#271273,#271274),(#271275,#271276),(#271277,#271278),
(#271279,#271280),(#271281,#271282),(#271283,#271284),(#271285,#271286),
(#271287,#271288),(#271289,#271290),(#271291,#271292),(#271293,#271294),
(#271295,#271296),(#271297,#271298),(#271299,#271300),(#271301,#271302),
(#271303,#271304),(#271305,#271306),(#271307,#271308),(#271309,#271310),
(#271311,#271312),(#271313,#271314),(#271315,#271316),(#271317,#271318),
(#271319,#271320),(#271321,#271322),(#271323,#271324),(#271325,#271326),
(#271327,#271328),(#271329,#271330),(#271331,#271332),(#271333,#271334),
(#271335,#271336),(#271337,#271338),(#271339,#271340),(#271341,#271342),
(#271343,#271344),(#271345,#271346),(#271347,#271348),(#271349,#271350),
(#271351,#271352),(#271353,#271354),(#271355,#271356),(#271357,#271358),
(#271359,#271360),(#271361,#271362),(#271363,#271364),(#271365,#271366),
(#271367,#271368),(#271369,#271370),(#271371,#271372),(#271373,#271374),
(#271375,#271376),(#271377,#271378),(#271379,#271380),(#271381,#271382),
(#271383,#271384),(#271385,#271386),(#271387,#271388),(#271389,#271390),
(#271391,#271392),(#271393,#271394),(#271395,#271396),(#271397,#271398),
(#271399,#271400),(#271401,#271402),(#271403,#271404),(#271405,#271406),
(#271407,#271408),(#271409,#271410),(#271411,#271412),(#271413,#271414),
(#271415,#271416),(#271417,#271418),(#271419,#271420),(#271421,#271422),
(#271423,#271424),(#271425,#271426),(#271427,#271428),(#271429,#271430),
(#271431,#271432),(#271433,#271434),(#271435,#271436),(#271437,#271438),
(#271439,#271440),(#271441,#271442),(#271443,#271444),(#271445,#271446),
(#271447,#271448),(#271449,#271450),(#271451,#271452),(#271453,#271454),
(#271455,#271456),(#271457,#271458),(#271459,#271460),(#271461,#271462),
(#271463,#271464),(#271465,#271466),(#271467,#271468),(#271469,#271470),
(#271471,#271472),(#271473,#271474),(#271475,#271476),(#271477,#271478),
(#271479,#271480),(#271481,#271482),(#271483,#271484),(#271485,#271486),
(#271487,#271488),(#271489,#271490),(#271491,#271492),(#271493,#271494),
(#271495,#271496),(#271497,#271498),(#271499,#271500),(#271501,#271502),
(#271503,#271504),(#271505,#271506),(#271507,#271508),(#271509,#271510),
(#271511,#271512),(#271513,#271514),(#271515,#271516),(#271517,#271518),
(#271519,#271520),(#271521,#271522),(#271523,#271524),(#271525,#271526),
(#271527,#271528),(#271529,#271530),(#271531,#271532),(#271533,#271534),
(#271535,#271536),(#271537,#271538),(#271539,#271540),(#271541,#271542),
(#271543,#271544),(#271545,#271546),(#271547,#271548),(#271549,#271550),
(#271551,#271552),(#271553,#271554),(#271555,#271556),(#271557,#271558),
(#271559,#271560),(#271561,#271562),(#271563,#271564),(#271565,#271566),
(#271567,#271568),(#271569,#271570),(#271571,#271572),(#271573,#271574),
(#271575,#271576),(#271577,#271578),(#271579,#271580),(#271581,#271582),
(#271583,#271584),(#271585,#271586),(#271587,#271588),(#271589,#271590),
(#271591,#271592),(#271593,#271594),(#271595,#271596),(#271597,#271598),
(#271599,#271600),(#271601,#271602),(#271603,#271604),(#271605,#271606),
(#271607,#271608),(#271609,#271610),(#271611,#271612),(#271613,#271614),
(#271615,#271616),(#271617,#271618),(#271619,#271620),(#271621,#271622),
(#271623,#271624),(#271625,#271626),(#271627,#271628),(#271629,#271630),
(#271631,#271632),(#271633,#271634),(#271635,#271636),(#271637,#271638),
(#271639,#271640),(#271641,#271642),(#271643,#271644),(#271645,#271646),
(#271647,#271648),(#271649,#271650),(#271651,#271652),(#271653,#271654),
(#271655,#271656),(#271657,#271658),(#271659,#271660),(#271661,#271662),
(#271663,#271664),(#271665,#271666),(#271667,#271668),(#271669,#271670),
(#271671,#271672),(#271673,#271674),(#271675,#271676),(#271677,#271678),
(#271679,#271680),(#271681,#271682),(#271683,#271684),(#271685,#271686),
(#271687,#271688),(#271689,#271690),(#271691,#271692),(#271693,#271694),
(#271695,#271696),(#271697,#271698),(#271699,#271700),(#271701,#271702),
(#271703,#271704),(#271705,#271706),(#271707,#271708),(#271709,#271710),
(#271711,#271712),(#271713,#271714),(#271715,#271716),(#271717,#271718),
(#271719,#271720),(#271721,#271722),(#271723,#271724),(#271725,#271726),
(#271727,#271728),(#271729,#271730),(#271731,#271732),(#271733,#271734),
(#271735,#271736),(#271737,#271738),(#271739,#271740),(#271741,#271742),
(#271743,#271744),(#271745,#271746),(#271747,#271748),(#271749,#271750),
(#271751,#271752),(#271753,#271754),(#271755,#271756),(#271757,#271758),
(#271759,#271760),(#271761,#271762),(#271763,#271764),(#271765,#271766),
(#271767,#271768),(#271769,#271770),(#271771,#271772),(#271773,#271774),
(#271775,#271776),(#271777,#271778),(#271779,#271780),(#271781,#271782),
(#271783,#271784),(#271785,#271786),(#271787,#271788),(#271789,#271790),
(#271791,#271792),(#271793,#271794),(#271795,#271796),(#271797,#271798),
(#271799,#271800),(#271801,#271802),(#271803,#271804),(#271805,#271806),
(#271807,#271808),(#271809,#271810),(#271811,#271812),(#271813,#271814),
(#271815,#271816),(#271817,#271818),(#271819,#271820),(#271821,#271822),
(#271823,#271824),(#271825,#271826),(#271827,#271828),(#271829,#271830),
(#271831,#271832),(#271833,#271834),(#271835,#271836),(#271837,#271838),
(#271839,#271840),(#271841,#271842),(#271843,#271844),(#271845,#271846),
(#271847,#271848),(#271849,#271850),(#271851,#271852),(#271853,#271854),
(#271855,#271856),(#271857,#271858),(#271859,#271860),(#271861,#271862),
(#271863,#271864),(#271865,#271866),(#271867,#271868),(#271869,#271870),
(#271871,#271872),(#271873,#271874),(#271875,#271876),(#271877,#271878),
(#271879,#271880),(#271881,#271882),(#271883,#271884),(#271885,#271886),
(#271887,#271888),(#271889,#271890),(#271891,#271892),(#271893,#271894),
(#271895,#271896),(#271897,#271898),(#271899,#271900),(#271901,#271902),
(#271903,#271904),(#271905,#271906),(#271907,#271908),(#271909,#271910),
(#271911,#271912),(#271913,#271914),(#271915,#271916),(#271917,#271918),
(#271919,#271920),(#271921,#271922),(#271923,#271924),(#271925,#271926),
(#271927,#271928),(#271929,#271930),(#271931,#271932),(#271933,#271934),
(#271935,#271936),(#271937,#271938),(#271939,#271940),(#271941,#271942),
(#271943,#271944),(#271945,#271946),(#271947,#271948),(#271949,#271950),
(#271951,#271952),(#271953,#271954),(#271955,#271956),(#271957,#271958),
(#271959,#271960),(#271961,#271962),(#271963,#271964),(#271965,#271966),
(#271967,#271968),(#271969,#271970),(#271971,#271972),(#271973,#271974),
(#271975,#271976),(#271977,#271978),(#271979,#271980),(#271981,#271982),
(#271983,#271984),(#271985,#271986),(#271987,#271988),(#271989,#271990),
(#271991,#271992),(#271993,#271994),(#271995,#271996),(#271997,#271998),
(#271999,#272000),(#272001,#272002),(#272003,#272004),(#272005,#272006),
(#272007,#272008),(#272009,#272010),(#272011,#272012),(#272013,#272014),
(#272015,#272016),(#272017,#272018),(#272019,#272020),(#272021,#272022),
(#272023,#272024),(#272025,#272026),(#272027,#272028),(#272029,#272030),
(#272031,#272032),(#272033,#272034),(#272035,#272036),(#272037,#272038),
(#272039,#272040),(#272041,#272042),(#272043,#272044),(#272045,#272046),
(#272047,#272048),(#272049,#272050),(#272051,#272052),(#272053,#272054),
(#272055,#272056),(#272057,#272058),(#272059,#272060),(#272061,#272062),
(#272063,#272064),(#272065,#272066),(#272067,#272068),(#272069,#272070),
(#272071,#272072),(#272073,#272074),(#272075,#272076),(#272077,#272078),
(#272079,#272080),(#272081,#272082),(#272083,#272084),(#272085,#272086),
(#272087,#272088),(#272089,#272090),(#272091,#272092),(#272093,#272094),
(#272095,#272096),(#272097,#272098),(#272099,#272100),(#272101,#272102),
(#272103,#272104),(#272105,#272106),(#272107,#272108),(#272109,#272110),
(#272111,#272112),(#272113,#272114),(#272115,#272116),(#272117,#272118),
(#272119,#272120),(#272121,#272122),(#272123,#272124),(#272125,#272126),
(#272127,#272128),(#272129,#272130),(#272131,#272132),(#272133,#272134),
(#272135,#272136),(#272137,#272138),(#272139,#272140),(#272141,#272142),
(#272143,#272144),(#272145,#272146),(#272147,#272148),(#272149,#272150),
(#272151,#272152),(#272153,#272154),(#272155,#272156),(#272157,#272158),
(#272159,#272160),(#272161,#272162),(#272163,#272164),(#272165,#272166),
(#272167,#272168),(#272169,#272170),(#272171,#272172),(#272173,#272174),
(#272175,#272176),(#272177,#272178)),.UNSPECIFIED.,.F.,.F.,.F.,(6,1,1,1,
1,1,1,1,1,1,1,1,1,1,1,1,1,1,1,1,1,1,1,1,1,1,1,1,1,1,1,1,1,1,1,1,1,1,1,1,
1,1,1,1,1,1,1,1,1,1,1,1,1,1,1,1,1,1,1,1,1,1,1,1,1,1,1,1,1,1,1,1,1,1,1,1,
1,1,1,1,1,1,1,1,1,1,1,1,1,1,1,1,1,1,1,1,1,1,1,1,1,1,1,1,1,1,1,1,1,1,1,1,
1,1,1,1,1,1,1,1,1,1,1,1,1,1,1,1,1,1,1,1,1,1,1,1,1,1,1,1,1,1,1,1,1,1,1,1,
1,1,1,1,1,1,1,1,1,1,1,1,1,1,1,1,1,1,1,1,1,1,1,1,1,1,1,1,1,1,1,1,1,1,1,1,
1,1,1,1,1,1,1,1,1,1,1,1,1,1,1,1,1,1,1,1,1,1,1,1,1,1,1,1,1,1,1,1,1,1,1,1,
1,1,1,1,1,1,1,1,1,1,1,1,1,1,1,1,1,1,1,1,1,1,1,1,1,1,1,1,1,1,1,1,1,1,1,1,
1,1,1,1,1,1,1,1,1,1,1,1,1,1,1,1,1,1,1,1,1,1,1,1,1,1,1,1,1,1,1,1,1,1,1,1,
1,1,1,1,1,1,1,1,1,1,1,1,1,1,1,1,1,1,1,1,1,1,1,1,1,1,1,1,1,1,1,1,1,1,1,1,
1,1,1,1,1,1,1,1,1,1,1,1,1,1,1,1,1,1,1,1,1,1,1,1,1,1,1,1,1,1,1,1,1,1,1,1,
1,1,1,1,1,1,1,1,1,1,1,1,1,1,1,1,1,1,1,1,1,1,1,1,1,1,1,1,1,1,1,1,1,1,1,1,
1,1,1,1,1,1,1,1,1,1,1,1,1,1,1,1,1,1,1,1,1,1,1,1,1,1,1,1,1,1,1,1,1,1,1,1,
1,1,1,1,1,1,1,1,1,1,1,1,1,1,1,1,1,1,1,1,1,1,1,1,1,1,1,1,1,1,1,6),(2,2),
(0.143172103,0.144954128,0.146788991,0.148623853,0.150458716,0.152293578,
0.15412844,0.155963303,0.157798165,0.159633028,0.16146789,0.163302752,0.165137615,
0.166972477,0.168807339,0.170642202,0.172477064,0.174311927,0.176146789,
0.177981651,0.179816514,0.181651376,0.183486239,0.185321101,0.187155963,
0.188990826,0.190825688,0.19266055,0.194495413,0.196330275,0.198165138,
0.2,0.201834862,0.203669725,0.205504587,0.20733945,0.209174312,0.211009174,
0.212844037,0.214678899,0.216513761,0.218348624,0.220183486,0.222018349,
0.223853211,0.225688073,0.227522936,0.229357798,0.231192661,0.233027523,
0.234862385,0.236697248,0.23853211,0.240366972,0.242201835,0.244036697,
0.24587156,0.247706422,0.249541284,0.251376147,0.253211009,0.255045872,
0.256880734,0.258715596,0.260550459,0.262385321,0.264220183,0.266055046,
0.267889908,0.269724771,0.271559633,0.273394495,0.275229358,0.27706422,
0.278899083,0.280733945,0.282568807,0.28440367,0.286238532,0.288073394,
0.289908257,0.291743119,0.293577982,0.295412844,0.297247706,0.299082569,
0.300917431,0.302752294,0.304587156,0.306422018,0.308256881,0.310091743,
0.311926606,0.313761468,0.31559633,0.317431193,0.319266055,0.321100917,
0.32293578,0.324770642,0.326605505,0.328440367,0.330275229,0.332110092,
0.333944954,0.335779817,0.337614679,0.339449541,0.341284404,0.343119266,
0.344954128,0.346788991,0.348623853,0.350458716,0.352293578,0.35412844,
0.355963303,0.357798165,0.359633028,0.36146789,0.363302752,0.365137615,
0.366972477,0.368807339,0.370642202,0.372477064,0.374311927,0.376146789,
0.377981651,0.379816514,0.381651376,0.383486239,0.385321101,0.387155963,
0.388990826,0.390825688,0.39266055,0.394495413,0.396330275,0.398165138,
0.4,0.401834862,0.403669725,0.405504587,0.40733945,0.409174312,0.411009174,
0.412844037,0.414678899,0.416513761,0.418348624,0.420183486,0.422018349,
0.423853211,0.425688073,0.427522936,0.429357798,0.431192661,0.433027523,
0.434862385,0.436697248,0.43853211,0.440366972,0.442201835,0.444036697,
0.44587156,0.447706422,0.449541284,0.451376147,0.453211009,0.455045872,
0.456880734,0.458715596,0.460550459,0.462385321,0.464220183,0.466055046,
0.467889908,0.469724771,0.471559633,0.473394495,0.475229358,0.47706422,
0.478899083,0.480733945,0.482568807,0.48440367,0.486238532,0.488073394,
0.489908257,0.491743119,0.493577982,0.495412844,0.497247706,0.499082569,
0.500917431,0.502752294,0.504587156,0.506422018,0.508256881,0.510091743,
0.511926606,0.513761468,0.51559633,0.517431193,0.519266055,0.521100917,
0.52293578,0.524770642,0.526605505,0.528440367,0.530275229,0.532110092,
0.533944954,0.535779817,0.537614679,0.539449541,0.541284404,0.543119266,
0.544954128,0.546788991,0.548623853,0.550458716,0.552293578,0.55412844,
0.555963303,0.557798165,0.559633028,0.56146789,0.563302752,0.565137615,
0.566972477,0.568807339,0.570642202,0.572477064,0.574311927,0.576146789,
0.577981651,0.579816514,0.581651376,0.583486239,0.585321101,0.587155963,
0.588990826,0.590825688,0.59266055,0.594495413,0.596330275,0.598165138,
0.6,0.601834862,0.603669725,0.605504587,0.60733945,0.609174312,0.611009174,
0.612844037,0.614678899,0.616513761,0.618348624,0.620183486,0.622018349,
0.623853211,0.625688073,0.627522936,0.629357798,0.631192661,0.633027523,
0.634862385,0.636697248,0.63853211,0.640366972,0.642201835,0.644036697,
0.64587156,0.647706422,0.649541284,0.651376147,0.653211009,0.655045872,
0.656880734,0.658715596,0.660550459,0.662385321,0.664220183,0.666055046,
0.667889908,0.669724771,0.671559633,0.673394495,0.675229358,0.67706422,
0.678899083,0.680733945,0.682568807,0.68440367,0.686238532,0.688073394,
0.689908257,0.691743119,0.693577982,0.695412844,0.697247706,0.699082569,
0.700917431,0.702752294,0.704587156,0.706422018,0.708256881,0.710091743,
0.711926606,0.713761468,0.71559633,0.717431193,0.719266055,0.721100917,
0.72293578,0.724770642,0.726605505,0.728440367,0.730275229,0.732110092,
0.733944954,0.735779817,0.737614679,0.739449541,0.741284404,0.743119266,
0.744954128,0.746788991,0.748623853,0.750458716,0.752293578,0.75412844,
0.755963303,0.757798165,0.759633028,0.76146789,0.763302752,0.765137615,
0.766972477,0.768807339,0.770642202,0.772477064,0.774311927,0.776146789,
0.777981651,0.779816514,0.781651376,0.783486239,0.785321101,0.787155963,
0.788990826,0.790825688,0.79266055,0.794495413,0.796330275,0.798165138,
0.8,0.801834862,0.803669725,0.805504587,0.80733945,0.809174312,0.811009174,
0.812844037,0.814678899,0.816513761,0.818348624,0.820183486,0.822018349,
0.823853211,0.825688073,0.827522936,0.829357798,0.831192661,0.833027523,
0.834862385,0.836697248,0.83853211,0.840366972,0.842201835,0.844036697,
0.84587156,0.847706422,0.849541284,0.851376147,0.853211009,0.855045872,
0.856880734,0.858715596,0.860550459,0.862385321,0.864220183,0.866055046,
0.867889908,0.869724771,0.871559633,0.873394495,0.875229358,0.87706422,
0.878899083,0.880733945,0.882568807,0.88440367,0.886238532,0.888073394,
0.889908257,0.891743119,0.893577982,0.895412844,0.897247706,0.899082569,
0.900917431,0.902752294,0.904587156,0.906422018,0.908256881,0.910091743,
0.911926606,0.913761468,0.91559633,0.917431193,0.919266055,0.921100917,
0.92293578,0.924770642,0.926605505,0.928440367,0.930275229,0.932110092,
0.933944954,0.935779817,0.937614679,0.939449541,0.941284404,0.943119266,
0.944954128,0.946788991,0.948623853,0.950458716,0.952293578,0.95412844,
0.955963303,0.957798165,0.959633028,0.96146789,0.963302752,0.965137615,
0.966972477,0.968807339,0.970642202,0.972477064,0.974311927,0.976146789,
0.977981651,0.979816514,0.981651376,0.983486239,0.985321101,0.987155963,
0.988990826,0.990825688,0.99266055,0.994495413,0.996330275,0.998165138,
1.),(0.,0.36),.UNSPECIFIED.);
#6287=B_SPLINE_SURFACE_WITH_KNOTS('',5,1,((#272844,#272845),(#272846,#272847),
(#272848,#272849),(#272850,#272851),(#272852,#272853),(#272854,#272855),
(#272856,#272857),(#272858,#272859),(#272860,#272861),(#272862,#272863),
(#272864,#272865),(#272866,#272867),(#272868,#272869),(#272870,#272871),
(#272872,#272873),(#272874,#272875),(#272876,#272877),(#272878,#272879),
(#272880,#272881),(#272882,#272883),(#272884,#272885),(#272886,#272887),
(#272888,#272889),(#272890,#272891),(#272892,#272893),(#272894,#272895),
(#272896,#272897),(#272898,#272899),(#272900,#272901),(#272902,#272903),
(#272904,#272905),(#272906,#272907),(#272908,#272909),(#272910,#272911),
(#272912,#272913),(#272914,#272915),(#272916,#272917),(#272918,#272919),
(#272920,#272921),(#272922,#272923),(#272924,#272925),(#272926,#272927),
(#272928,#272929),(#272930,#272931),(#272932,#272933),(#272934,#272935),
(#272936,#272937),(#272938,#272939),(#272940,#272941),(#272942,#272943),
(#272944,#272945),(#272946,#272947),(#272948,#272949),(#272950,#272951),
(#272952,#272953),(#272954,#272955),(#272956,#272957),(#272958,#272959),
(#272960,#272961),(#272962,#272963),(#272964,#272965),(#272966,#272967),
(#272968,#272969),(#272970,#272971),(#272972,#272973),(#272974,#272975),
(#272976,#272977),(#272978,#272979),(#272980,#272981),(#272982,#272983),
(#272984,#272985),(#272986,#272987),(#272988,#272989),(#272990,#272991),
(#272992,#272993),(#272994,#272995),(#272996,#272997),(#272998,#272999),
(#273000,#273001),(#273002,#273003),(#273004,#273005),(#273006,#273007),
(#273008,#273009),(#273010,#273011),(#273012,#273013),(#273014,#273015),
(#273016,#273017),(#273018,#273019),(#273020,#273021),(#273022,#273023),
(#273024,#273025),(#273026,#273027),(#273028,#273029),(#273030,#273031),
(#273032,#273033),(#273034,#273035),(#273036,#273037),(#273038,#273039),
(#273040,#273041),(#273042,#273043),(#273044,#273045),(#273046,#273047),
(#273048,#273049),(#273050,#273051),(#273052,#273053),(#273054,#273055),
(#273056,#273057),(#273058,#273059),(#273060,#273061),(#273062,#273063),
(#273064,#273065),(#273066,#273067),(#273068,#273069),(#273070,#273071),
(#273072,#273073),(#273074,#273075),(#273076,#273077),(#273078,#273079),
(#273080,#273081),(#273082,#273083),(#273084,#273085),(#273086,#273087),
(#273088,#273089),(#273090,#273091),(#273092,#273093),(#273094,#273095),
(#273096,#273097),(#273098,#273099),(#273100,#273101),(#273102,#273103),
(#273104,#273105),(#273106,#273107),(#273108,#273109),(#273110,#273111),
(#273112,#273113),(#273114,#273115),(#273116,#273117),(#273118,#273119),
(#273120,#273121),(#273122,#273123),(#273124,#273125),(#273126,#273127),
(#273128,#273129),(#273130,#273131),(#273132,#273133),(#273134,#273135),
(#273136,#273137),(#273138,#273139),(#273140,#273141),(#273142,#273143),
(#273144,#273145),(#273146,#273147),(#273148,#273149),(#273150,#273151),
(#273152,#273153),(#273154,#273155),(#273156,#273157),(#273158,#273159),
(#273160,#273161),(#273162,#273163),(#273164,#273165),(#273166,#273167),
(#273168,#273169),(#273170,#273171),(#273172,#273173),(#273174,#273175),
(#273176,#273177),(#273178,#273179),(#273180,#273181),(#273182,#273183),
(#273184,#273185),(#273186,#273187),(#273188,#273189),(#273190,#273191),
(#273192,#273193),(#273194,#273195),(#273196,#273197),(#273198,#273199),
(#273200,#273201),(#273202,#273203),(#273204,#273205),(#273206,#273207),
(#273208,#273209),(#273210,#273211),(#273212,#273213),(#273214,#273215),
(#273216,#273217),(#273218,#273219),(#273220,#273221),(#273222,#273223),
(#273224,#273225),(#273226,#273227),(#273228,#273229),(#273230,#273231),
(#273232,#273233),(#273234,#273235),(#273236,#273237),(#273238,#273239),
(#273240,#273241),(#273242,#273243),(#273244,#273245),(#273246,#273247),
(#273248,#273249),(#273250,#273251),(#273252,#273253),(#273254,#273255),
(#273256,#273257),(#273258,#273259),(#273260,#273261),(#273262,#273263),
(#273264,#273265),(#273266,#273267),(#273268,#273269),(#273270,#273271),
(#273272,#273273),(#273274,#273275),(#273276,#273277),(#273278,#273279),
(#273280,#273281),(#273282,#273283),(#273284,#273285),(#273286,#273287),
(#273288,#273289),(#273290,#273291),(#273292,#273293),(#273294,#273295),
(#273296,#273297),(#273298,#273299),(#273300,#273301),(#273302,#273303),
(#273304,#273305),(#273306,#273307),(#273308,#273309),(#273310,#273311),
(#273312,#273313),(#273314,#273315),(#273316,#273317),(#273318,#273319),
(#273320,#273321),(#273322,#273323),(#273324,#273325),(#273326,#273327),
(#273328,#273329),(#273330,#273331),(#273332,#273333),(#273334,#273335),
(#273336,#273337),(#273338,#273339),(#273340,#273341),(#273342,#273343),
(#273344,#273345),(#273346,#273347),(#273348,#273349),(#273350,#273351),
(#273352,#273353),(#273354,#273355),(#273356,#273357),(#273358,#273359),
(#273360,#273361),(#273362,#273363),(#273364,#273365),(#273366,#273367),
(#273368,#273369),(#273370,#273371),(#273372,#273373),(#273374,#273375),
(#273376,#273377),(#273378,#273379),(#273380,#273381),(#273382,#273383),
(#273384,#273385),(#273386,#273387),(#273388,#273389),(#273390,#273391),
(#273392,#273393),(#273394,#273395),(#273396,#273397),(#273398,#273399),
(#273400,#273401),(#273402,#273403),(#273404,#273405),(#273406,#273407),
(#273408,#273409),(#273410,#273411),(#273412,#273413),(#273414,#273415),
(#273416,#273417),(#273418,#273419),(#273420,#273421),(#273422,#273423),
(#273424,#273425),(#273426,#273427),(#273428,#273429),(#273430,#273431),
(#273432,#273433),(#273434,#273435),(#273436,#273437),(#273438,#273439),
(#273440,#273441),(#273442,#273443),(#273444,#273445),(#273446,#273447),
(#273448,#273449),(#273450,#273451),(#273452,#273453),(#273454,#273455),
(#273456,#273457),(#273458,#273459),(#273460,#273461),(#273462,#273463),
(#273464,#273465),(#273466,#273467),(#273468,#273469),(#273470,#273471),
(#273472,#273473),(#273474,#273475),(#273476,#273477),(#273478,#273479),
(#273480,#273481),(#273482,#273483),(#273484,#273485),(#273486,#273487),
(#273488,#273489),(#273490,#273491),(#273492,#273493),(#273494,#273495),
(#273496,#273497),(#273498,#273499),(#273500,#273501),(#273502,#273503),
(#273504,#273505),(#273506,#273507),(#273508,#273509),(#273510,#273511),
(#273512,#273513),(#273514,#273515),(#273516,#273517),(#273518,#273519),
(#273520,#273521),(#273522,#273523),(#273524,#273525),(#273526,#273527),
(#273528,#273529),(#273530,#273531),(#273532,#273533),(#273534,#273535),
(#273536,#273537),(#273538,#273539),(#273540,#273541),(#273542,#273543),
(#273544,#273545),(#273546,#273547),(#273548,#273549),(#273550,#273551),
(#273552,#273553),(#273554,#273555),(#273556,#273557),(#273558,#273559),
(#273560,#273561),(#273562,#273563),(#273564,#273565),(#273566,#273567),
(#273568,#273569),(#273570,#273571),(#273572,#273573),(#273574,#273575),
(#273576,#273577),(#273578,#273579),(#273580,#273581),(#273582,#273583),
(#273584,#273585),(#273586,#273587),(#273588,#273589),(#273590,#273591),
(#273592,#273593),(#273594,#273595),(#273596,#273597),(#273598,#273599),
(#273600,#273601),(#273602,#273603),(#273604,#273605),(#273606,#273607),
(#273608,#273609),(#273610,#273611),(#273612,#273613),(#273614,#273615),
(#273616,#273617),(#273618,#273619),(#273620,#273621),(#273622,#273623),
(#273624,#273625),(#273626,#273627),(#273628,#273629),(#273630,#273631),
(#273632,#273633),(#273634,#273635),(#273636,#273637),(#273638,#273639),
(#273640,#273641),(#273642,#273643),(#273644,#273645),(#273646,#273647),
(#273648,#273649),(#273650,#273651),(#273652,#273653),(#273654,#273655),
(#273656,#273657),(#273658,#273659),(#273660,#273661),(#273662,#273663),
(#273664,#273665),(#273666,#273667),(#273668,#273669),(#273670,#273671),
(#273672,#273673),(#273674,#273675),(#273676,#273677),(#273678,#273679),
(#273680,#273681),(#273682,#273683),(#273684,#273685),(#273686,#273687),
(#273688,#273689),(#273690,#273691),(#273692,#273693),(#273694,#273695),
(#273696,#273697),(#273698,#273699),(#273700,#273701),(#273702,#273703),
(#273704,#273705),(#273706,#273707),(#273708,#273709),(#273710,#273711),
(#273712,#273713),(#273714,#273715),(#273716,#273717),(#273718,#273719),
(#273720,#273721),(#273722,#273723),(#273724,#273725),(#273726,#273727),
(#273728,#273729),(#273730,#273731),(#273732,#273733),(#273734,#273735),
(#273736,#273737),(#273738,#273739),(#273740,#273741),(#273742,#273743),
(#273744,#273745),(#273746,#273747),(#273748,#273749),(#273750,#273751),
(#273752,#273753),(#273754,#273755),(#273756,#273757),(#273758,#273759),
(#273760,#273761),(#273762,#273763),(#273764,#273765),(#273766,#273767),
(#273768,#273769),(#273770,#273771),(#273772,#273773),(#273774,#273775),
(#273776,#273777),(#273778,#273779),(#273780,#273781),(#273782,#273783),
(#273784,#273785),(#273786,#273787)),.UNSPECIFIED.,.F.,.F.,.F.,(6,1,1,1,
1,1,1,1,1,1,1,1,1,1,1,1,1,1,1,1,1,1,1,1,1,1,1,1,1,1,1,1,1,1,1,1,1,1,1,1,
1,1,1,1,1,1,1,1,1,1,1,1,1,1,1,1,1,1,1,1,1,1,1,1,1,1,1,1,1,1,1,1,1,1,1,1,
1,1,1,1,1,1,1,1,1,1,1,1,1,1,1,1,1,1,1,1,1,1,1,1,1,1,1,1,1,1,1,1,1,1,1,1,
1,1,1,1,1,1,1,1,1,1,1,1,1,1,1,1,1,1,1,1,1,1,1,1,1,1,1,1,1,1,1,1,1,1,1,1,
1,1,1,1,1,1,1,1,1,1,1,1,1,1,1,1,1,1,1,1,1,1,1,1,1,1,1,1,1,1,1,1,1,1,1,1,
1,1,1,1,1,1,1,1,1,1,1,1,1,1,1,1,1,1,1,1,1,1,1,1,1,1,1,1,1,1,1,1,1,1,1,1,
1,1,1,1,1,1,1,1,1,1,1,1,1,1,1,1,1,1,1,1,1,1,1,1,1,1,1,1,1,1,1,1,1,1,1,1,
1,1,1,1,1,1,1,1,1,1,1,1,1,1,1,1,1,1,1,1,1,1,1,1,1,1,1,1,1,1,1,1,1,1,1,1,
1,1,1,1,1,1,1,1,1,1,1,1,1,1,1,1,1,1,1,1,1,1,1,1,1,1,1,1,1,1,1,1,1,1,1,1,
1,1,1,1,1,1,1,1,1,1,1,1,1,1,1,1,1,1,1,1,1,1,1,1,1,1,1,1,1,1,1,1,1,1,1,1,
1,1,1,1,1,1,1,1,1,1,1,1,1,1,1,1,1,1,1,1,1,1,1,1,1,1,1,1,1,1,1,1,1,1,1,1,
1,1,1,1,1,1,1,1,1,1,1,1,1,1,1,1,1,1,1,1,1,1,1,1,1,1,1,1,1,1,1,1,1,1,1,1,
1,1,1,1,1,1,1,1,1,1,1,1,1,1,1,1,1,1,1,1,1,1,1,1,1,1,1,1,1,1,1,6),(2,2),
(0.143172103,0.144954128,0.146788991,0.148623853,0.150458716,0.152293578,
0.15412844,0.155963303,0.157798165,0.159633028,0.16146789,0.163302752,0.165137615,
0.166972477,0.168807339,0.170642202,0.172477064,0.174311927,0.176146789,
0.177981651,0.179816514,0.181651376,0.183486239,0.185321101,0.187155963,
0.188990826,0.190825688,0.19266055,0.194495413,0.196330275,0.198165138,
0.2,0.201834862,0.203669725,0.205504587,0.20733945,0.209174312,0.211009174,
0.212844037,0.214678899,0.216513761,0.218348624,0.220183486,0.222018349,
0.223853211,0.225688073,0.227522936,0.229357798,0.231192661,0.233027523,
0.234862385,0.236697248,0.23853211,0.240366972,0.242201835,0.244036697,
0.24587156,0.247706422,0.249541284,0.251376147,0.253211009,0.255045872,
0.256880734,0.258715596,0.260550459,0.262385321,0.264220183,0.266055046,
0.267889908,0.269724771,0.271559633,0.273394495,0.275229358,0.27706422,
0.278899083,0.280733945,0.282568807,0.28440367,0.286238532,0.288073394,
0.289908257,0.291743119,0.293577982,0.295412844,0.297247706,0.299082569,
0.300917431,0.302752294,0.304587156,0.306422018,0.308256881,0.310091743,
0.311926606,0.313761468,0.31559633,0.317431193,0.319266055,0.321100917,
0.32293578,0.324770642,0.326605505,0.328440367,0.330275229,0.332110092,
0.333944954,0.335779817,0.337614679,0.339449541,0.341284404,0.343119266,
0.344954128,0.346788991,0.348623853,0.350458716,0.352293578,0.35412844,
0.355963303,0.357798165,0.359633028,0.36146789,0.363302752,0.365137615,
0.366972477,0.368807339,0.370642202,0.372477064,0.374311927,0.376146789,
0.377981651,0.379816514,0.381651376,0.383486239,0.385321101,0.387155963,
0.388990826,0.390825688,0.39266055,0.394495413,0.396330275,0.398165138,
0.4,0.401834862,0.403669725,0.405504587,0.40733945,0.409174312,0.411009174,
0.412844037,0.414678899,0.416513761,0.418348624,0.420183486,0.422018349,
0.423853211,0.425688073,0.427522936,0.429357798,0.431192661,0.433027523,
0.434862385,0.436697248,0.43853211,0.440366972,0.442201835,0.444036697,
0.44587156,0.447706422,0.449541284,0.451376147,0.453211009,0.455045872,
0.456880734,0.458715596,0.460550459,0.462385321,0.464220183,0.466055046,
0.467889908,0.469724771,0.471559633,0.473394495,0.475229358,0.47706422,
0.478899083,0.480733945,0.482568807,0.48440367,0.486238532,0.488073394,
0.489908257,0.491743119,0.493577982,0.495412844,0.497247706,0.499082569,
0.500917431,0.502752294,0.504587156,0.506422018,0.508256881,0.510091743,
0.511926606,0.513761468,0.51559633,0.517431193,0.519266055,0.521100917,
0.52293578,0.524770642,0.526605505,0.528440367,0.530275229,0.532110092,
0.533944954,0.535779817,0.537614679,0.539449541,0.541284404,0.543119266,
0.544954128,0.546788991,0.548623853,0.550458716,0.552293578,0.55412844,
0.555963303,0.557798165,0.559633028,0.56146789,0.563302752,0.565137615,
0.566972477,0.568807339,0.570642202,0.572477064,0.574311927,0.576146789,
0.577981651,0.579816514,0.581651376,0.583486239,0.585321101,0.587155963,
0.588990826,0.590825688,0.59266055,0.594495413,0.596330275,0.598165138,
0.6,0.601834862,0.603669725,0.605504587,0.60733945,0.609174312,0.611009174,
0.612844037,0.614678899,0.616513761,0.618348624,0.620183486,0.622018349,
0.623853211,0.625688073,0.627522936,0.629357798,0.631192661,0.633027523,
0.634862385,0.636697248,0.63853211,0.640366972,0.642201835,0.644036697,
0.64587156,0.647706422,0.649541284,0.651376147,0.653211009,0.655045872,
0.656880734,0.658715596,0.660550459,0.662385321,0.664220183,0.666055046,
0.667889908,0.669724771,0.671559633,0.673394495,0.675229358,0.67706422,
0.678899083,0.680733945,0.682568807,0.68440367,0.686238532,0.688073394,
0.689908257,0.691743119,0.693577982,0.695412844,0.697247706,0.699082569,
0.700917431,0.702752294,0.704587156,0.706422018,0.708256881,0.710091743,
0.711926606,0.713761468,0.71559633,0.717431193,0.719266055,0.721100917,
0.72293578,0.724770642,0.726605505,0.728440367,0.730275229,0.732110092,
0.733944954,0.735779817,0.737614679,0.739449541,0.741284404,0.743119266,
0.744954128,0.746788991,0.748623853,0.750458716,0.752293578,0.75412844,
0.755963303,0.757798165,0.759633028,0.76146789,0.763302752,0.765137615,
0.766972477,0.768807339,0.770642202,0.772477064,0.774311927,0.776146789,
0.777981651,0.779816514,0.781651376,0.783486239,0.785321101,0.787155963,
0.788990826,0.790825688,0.79266055,0.794495413,0.796330275,0.798165138,
0.8,0.801834862,0.803669725,0.805504587,0.80733945,0.809174312,0.811009174,
0.812844037,0.814678899,0.816513761,0.818348624,0.820183486,0.822018349,
0.823853211,0.825688073,0.827522936,0.829357798,0.831192661,0.833027523,
0.834862385,0.836697248,0.83853211,0.840366972,0.842201835,0.844036697,
0.84587156,0.847706422,0.849541284,0.851376147,0.853211009,0.855045872,
0.856880734,0.858715596,0.860550459,0.862385321,0.864220183,0.866055046,
0.867889908,0.869724771,0.871559633,0.873394495,0.875229358,0.87706422,
0.878899083,0.880733945,0.882568807,0.88440367,0.886238532,0.888073394,
0.889908257,0.891743119,0.893577982,0.895412844,0.897247706,0.899082569,
0.900917431,0.902752294,0.904587156,0.906422018,0.908256881,0.910091743,
0.911926606,0.913761468,0.91559633,0.917431193,0.919266055,0.921100917,
0.92293578,0.924770642,0.926605505,0.928440367,0.930275229,0.932110092,
0.933944954,0.935779817,0.937614679,0.939449541,0.941284404,0.943119266,
0.944954128,0.946788991,0.948623853,0.950458716,0.952293578,0.95412844,
0.955963303,0.957798165,0.959633028,0.96146789,0.963302752,0.965137615,
0.966972477,0.968807339,0.970642202,0.972477064,0.974311927,0.976146789,
0.977981651,0.979816514,0.981651376,0.983486239,0.985321101,0.987155963,
0.988990826,0.990825688,0.99266055,0.994495413,0.996330275,0.998165138,
1.),(0.,0.36),.UNSPECIFIED.);
#6288=B_SPLINE_SURFACE_WITH_KNOTS('',5,1,((#274438,#274439),(#274440,#274441),
(#274442,#274443),(#274444,#274445),(#274446,#274447),(#274448,#274449),
(#274450,#274451),(#274452,#274453),(#274454,#274455),(#274456,#274457),
(#274458,#274459),(#274460,#274461),(#274462,#274463),(#274464,#274465),
(#274466,#274467),(#274468,#274469),(#274470,#274471),(#274472,#274473),
(#274474,#274475),(#274476,#274477),(#274478,#274479),(#274480,#274481),
(#274482,#274483),(#274484,#274485),(#274486,#274487),(#274488,#274489),
(#274490,#274491),(#274492,#274493),(#274494,#274495),(#274496,#274497),
(#274498,#274499),(#274500,#274501),(#274502,#274503),(#274504,#274505),
(#274506,#274507),(#274508,#274509),(#274510,#274511),(#274512,#274513),
(#274514,#274515),(#274516,#274517),(#274518,#274519),(#274520,#274521),
(#274522,#274523),(#274524,#274525),(#274526,#274527),(#274528,#274529),
(#274530,#274531),(#274532,#274533),(#274534,#274535),(#274536,#274537),
(#274538,#274539),(#274540,#274541),(#274542,#274543),(#274544,#274545),
(#274546,#274547),(#274548,#274549),(#274550,#274551),(#274552,#274553),
(#274554,#274555),(#274556,#274557),(#274558,#274559),(#274560,#274561),
(#274562,#274563),(#274564,#274565),(#274566,#274567),(#274568,#274569),
(#274570,#274571),(#274572,#274573),(#274574,#274575),(#274576,#274577),
(#274578,#274579),(#274580,#274581),(#274582,#274583),(#274584,#274585),
(#274586,#274587),(#274588,#274589),(#274590,#274591),(#274592,#274593),
(#274594,#274595),(#274596,#274597),(#274598,#274599),(#274600,#274601),
(#274602,#274603),(#274604,#274605),(#274606,#274607),(#274608,#274609),
(#274610,#274611),(#274612,#274613),(#274614,#274615),(#274616,#274617),
(#274618,#274619),(#274620,#274621),(#274622,#274623),(#274624,#274625),
(#274626,#274627),(#274628,#274629),(#274630,#274631),(#274632,#274633),
(#274634,#274635),(#274636,#274637),(#274638,#274639),(#274640,#274641),
(#274642,#274643),(#274644,#274645),(#274646,#274647),(#274648,#274649),
(#274650,#274651),(#274652,#274653),(#274654,#274655),(#274656,#274657),
(#274658,#274659),(#274660,#274661),(#274662,#274663),(#274664,#274665),
(#274666,#274667),(#274668,#274669),(#274670,#274671),(#274672,#274673),
(#274674,#274675),(#274676,#274677),(#274678,#274679),(#274680,#274681),
(#274682,#274683),(#274684,#274685),(#274686,#274687),(#274688,#274689),
(#274690,#274691),(#274692,#274693),(#274694,#274695),(#274696,#274697),
(#274698,#274699),(#274700,#274701),(#274702,#274703),(#274704,#274705),
(#274706,#274707),(#274708,#274709),(#274710,#274711),(#274712,#274713),
(#274714,#274715),(#274716,#274717),(#274718,#274719),(#274720,#274721),
(#274722,#274723),(#274724,#274725),(#274726,#274727),(#274728,#274729),
(#274730,#274731),(#274732,#274733),(#274734,#274735),(#274736,#274737),
(#274738,#274739),(#274740,#274741),(#274742,#274743),(#274744,#274745),
(#274746,#274747),(#274748,#274749),(#274750,#274751),(#274752,#274753),
(#274754,#274755),(#274756,#274757),(#274758,#274759),(#274760,#274761),
(#274762,#274763),(#274764,#274765),(#274766,#274767),(#274768,#274769),
(#274770,#274771),(#274772,#274773),(#274774,#274775),(#274776,#274777),
(#274778,#274779),(#274780,#274781),(#274782,#274783),(#274784,#274785),
(#274786,#274787),(#274788,#274789),(#274790,#274791),(#274792,#274793),
(#274794,#274795),(#274796,#274797),(#274798,#274799),(#274800,#274801),
(#274802,#274803),(#274804,#274805),(#274806,#274807),(#274808,#274809),
(#274810,#274811),(#274812,#274813),(#274814,#274815),(#274816,#274817),
(#274818,#274819),(#274820,#274821),(#274822,#274823),(#274824,#274825),
(#274826,#274827),(#274828,#274829),(#274830,#274831),(#274832,#274833),
(#274834,#274835),(#274836,#274837),(#274838,#274839),(#274840,#274841),
(#274842,#274843),(#274844,#274845),(#274846,#274847),(#274848,#274849),
(#274850,#274851),(#274852,#274853),(#274854,#274855),(#274856,#274857),
(#274858,#274859),(#274860,#274861),(#274862,#274863),(#274864,#274865),
(#274866,#274867),(#274868,#274869),(#274870,#274871),(#274872,#274873),
(#274874,#274875),(#274876,#274877),(#274878,#274879),(#274880,#274881),
(#274882,#274883),(#274884,#274885),(#274886,#274887),(#274888,#274889),
(#274890,#274891),(#274892,#274893),(#274894,#274895),(#274896,#274897),
(#274898,#274899),(#274900,#274901),(#274902,#274903),(#274904,#274905),
(#274906,#274907),(#274908,#274909),(#274910,#274911),(#274912,#274913),
(#274914,#274915),(#274916,#274917),(#274918,#274919),(#274920,#274921),
(#274922,#274923),(#274924,#274925),(#274926,#274927),(#274928,#274929),
(#274930,#274931),(#274932,#274933),(#274934,#274935),(#274936,#274937),
(#274938,#274939),(#274940,#274941),(#274942,#274943),(#274944,#274945),
(#274946,#274947),(#274948,#274949),(#274950,#274951),(#274952,#274953),
(#274954,#274955),(#274956,#274957),(#274958,#274959),(#274960,#274961),
(#274962,#274963),(#274964,#274965),(#274966,#274967),(#274968,#274969),
(#274970,#274971),(#274972,#274973),(#274974,#274975),(#274976,#274977),
(#274978,#274979),(#274980,#274981),(#274982,#274983),(#274984,#274985),
(#274986,#274987),(#274988,#274989),(#274990,#274991),(#274992,#274993),
(#274994,#274995),(#274996,#274997),(#274998,#274999),(#275000,#275001),
(#275002,#275003),(#275004,#275005),(#275006,#275007),(#275008,#275009),
(#275010,#275011),(#275012,#275013),(#275014,#275015),(#275016,#275017),
(#275018,#275019),(#275020,#275021),(#275022,#275023),(#275024,#275025),
(#275026,#275027),(#275028,#275029),(#275030,#275031),(#275032,#275033),
(#275034,#275035),(#275036,#275037),(#275038,#275039),(#275040,#275041),
(#275042,#275043),(#275044,#275045),(#275046,#275047),(#275048,#275049),
(#275050,#275051),(#275052,#275053),(#275054,#275055),(#275056,#275057),
(#275058,#275059),(#275060,#275061),(#275062,#275063),(#275064,#275065),
(#275066,#275067),(#275068,#275069),(#275070,#275071),(#275072,#275073),
(#275074,#275075),(#275076,#275077),(#275078,#275079),(#275080,#275081),
(#275082,#275083),(#275084,#275085),(#275086,#275087),(#275088,#275089),
(#275090,#275091),(#275092,#275093),(#275094,#275095),(#275096,#275097),
(#275098,#275099),(#275100,#275101),(#275102,#275103),(#275104,#275105),
(#275106,#275107),(#275108,#275109),(#275110,#275111),(#275112,#275113),
(#275114,#275115),(#275116,#275117),(#275118,#275119),(#275120,#275121),
(#275122,#275123),(#275124,#275125),(#275126,#275127),(#275128,#275129),
(#275130,#275131),(#275132,#275133),(#275134,#275135),(#275136,#275137),
(#275138,#275139),(#275140,#275141),(#275142,#275143),(#275144,#275145),
(#275146,#275147),(#275148,#275149),(#275150,#275151),(#275152,#275153),
(#275154,#275155),(#275156,#275157),(#275158,#275159),(#275160,#275161),
(#275162,#275163),(#275164,#275165),(#275166,#275167),(#275168,#275169),
(#275170,#275171),(#275172,#275173),(#275174,#275175),(#275176,#275177),
(#275178,#275179),(#275180,#275181),(#275182,#275183),(#275184,#275185),
(#275186,#275187),(#275188,#275189),(#275190,#275191),(#275192,#275193),
(#275194,#275195),(#275196,#275197),(#275198,#275199),(#275200,#275201),
(#275202,#275203),(#275204,#275205),(#275206,#275207),(#275208,#275209),
(#275210,#275211),(#275212,#275213),(#275214,#275215),(#275216,#275217),
(#275218,#275219),(#275220,#275221),(#275222,#275223),(#275224,#275225),
(#275226,#275227),(#275228,#275229),(#275230,#275231),(#275232,#275233),
(#275234,#275235),(#275236,#275237),(#275238,#275239),(#275240,#275241),
(#275242,#275243),(#275244,#275245),(#275246,#275247),(#275248,#275249),
(#275250,#275251),(#275252,#275253),(#275254,#275255),(#275256,#275257),
(#275258,#275259),(#275260,#275261),(#275262,#275263),(#275264,#275265),
(#275266,#275267),(#275268,#275269),(#275270,#275271),(#275272,#275273),
(#275274,#275275),(#275276,#275277),(#275278,#275279),(#275280,#275281),
(#275282,#275283),(#275284,#275285),(#275286,#275287),(#275288,#275289),
(#275290,#275291),(#275292,#275293),(#275294,#275295),(#275296,#275297),
(#275298,#275299),(#275300,#275301),(#275302,#275303),(#275304,#275305),
(#275306,#275307),(#275308,#275309),(#275310,#275311),(#275312,#275313),
(#275314,#275315),(#275316,#275317),(#275318,#275319),(#275320,#275321),
(#275322,#275323),(#275324,#275325),(#275326,#275327),(#275328,#275329),
(#275330,#275331),(#275332,#275333),(#275334,#275335),(#275336,#275337),
(#275338,#275339),(#275340,#275341),(#275342,#275343),(#275344,#275345),
(#275346,#275347),(#275348,#275349),(#275350,#275351),(#275352,#275353),
(#275354,#275355),(#275356,#275357),(#275358,#275359),(#275360,#275361),
(#275362,#275363),(#275364,#275365),(#275366,#275367),(#275368,#275369),
(#275370,#275371),(#275372,#275373),(#275374,#275375),(#275376,#275377),
(#275378,#275379),(#275380,#275381)),.UNSPECIFIED.,.F.,.F.,.F.,(6,1,1,1,
1,1,1,1,1,1,1,1,1,1,1,1,1,1,1,1,1,1,1,1,1,1,1,1,1,1,1,1,1,1,1,1,1,1,1,1,
1,1,1,1,1,1,1,1,1,1,1,1,1,1,1,1,1,1,1,1,1,1,1,1,1,1,1,1,1,1,1,1,1,1,1,1,
1,1,1,1,1,1,1,1,1,1,1,1,1,1,1,1,1,1,1,1,1,1,1,1,1,1,1,1,1,1,1,1,1,1,1,1,
1,1,1,1,1,1,1,1,1,1,1,1,1,1,1,1,1,1,1,1,1,1,1,1,1,1,1,1,1,1,1,1,1,1,1,1,
1,1,1,1,1,1,1,1,1,1,1,1,1,1,1,1,1,1,1,1,1,1,1,1,1,1,1,1,1,1,1,1,1,1,1,1,
1,1,1,1,1,1,1,1,1,1,1,1,1,1,1,1,1,1,1,1,1,1,1,1,1,1,1,1,1,1,1,1,1,1,1,1,
1,1,1,1,1,1,1,1,1,1,1,1,1,1,1,1,1,1,1,1,1,1,1,1,1,1,1,1,1,1,1,1,1,1,1,1,
1,1,1,1,1,1,1,1,1,1,1,1,1,1,1,1,1,1,1,1,1,1,1,1,1,1,1,1,1,1,1,1,1,1,1,1,
1,1,1,1,1,1,1,1,1,1,1,1,1,1,1,1,1,1,1,1,1,1,1,1,1,1,1,1,1,1,1,1,1,1,1,1,
1,1,1,1,1,1,1,1,1,1,1,1,1,1,1,1,1,1,1,1,1,1,1,1,1,1,1,1,1,1,1,1,1,1,1,1,
1,1,1,1,1,1,1,1,1,1,1,1,1,1,1,1,1,1,1,1,1,1,1,1,1,1,1,1,1,1,1,1,1,1,1,1,
1,1,1,1,1,1,1,1,1,1,1,1,1,1,1,1,1,1,1,1,1,1,1,1,1,1,1,1,1,1,1,1,1,1,1,1,
1,1,1,1,1,1,1,1,1,1,1,1,1,1,1,1,1,1,1,1,1,1,1,1,1,1,1,1,1,1,1,6),(2,2),
(-1.,-0.998165138,-0.996330275,-0.994495413,-0.99266055,-0.990825688,-0.988990826,
-0.987155963,-0.985321101,-0.983486239,-0.981651376,-0.979816514,-0.977981651,
-0.976146789,-0.974311927,-0.972477064,-0.970642202,-0.968807339,-0.966972477,
-0.965137615,-0.963302752,-0.96146789,-0.959633028,-0.957798165,-0.955963303,
-0.95412844,-0.952293578,-0.950458716,-0.948623853,-0.946788991,-0.944954128,
-0.943119266,-0.941284404,-0.939449541,-0.937614679,-0.935779817,-0.933944954,
-0.932110092,-0.930275229,-0.928440367,-0.926605505,-0.924770642,-0.92293578,
-0.921100917,-0.919266055,-0.917431193,-0.91559633,-0.913761468,-0.911926606,
-0.910091743,-0.908256881,-0.906422018,-0.904587156,-0.902752294,-0.900917431,
-0.899082569,-0.897247706,-0.895412844,-0.893577982,-0.891743119,-0.889908257,
-0.888073394,-0.886238532,-0.88440367,-0.882568807,-0.880733945,-0.878899083,
-0.87706422,-0.875229358,-0.873394495,-0.871559633,-0.869724771,-0.867889908,
-0.866055046,-0.864220183,-0.862385321,-0.860550459,-0.858715596,-0.856880734,
-0.855045872,-0.853211009,-0.851376147,-0.849541284,-0.847706422,-0.84587156,
-0.844036697,-0.842201835,-0.840366972,-0.83853211,-0.836697248,-0.834862385,
-0.833027523,-0.831192661,-0.829357798,-0.827522936,-0.825688073,-0.823853211,
-0.822018349,-0.820183486,-0.818348624,-0.816513761,-0.814678899,-0.812844037,
-0.811009174,-0.809174312,-0.80733945,-0.805504587,-0.803669725,-0.801834862,
-0.8,-0.798165138,-0.796330275,-0.794495413,-0.79266055,-0.790825688,-0.788990826,
-0.787155963,-0.785321101,-0.783486239,-0.781651376,-0.779816514,-0.777981651,
-0.776146789,-0.774311927,-0.772477064,-0.770642202,-0.768807339,-0.766972477,
-0.765137615,-0.763302752,-0.76146789,-0.759633028,-0.757798165,-0.755963303,
-0.75412844,-0.752293578,-0.750458716,-0.748623853,-0.746788991,-0.744954128,
-0.743119266,-0.741284404,-0.739449541,-0.737614679,-0.735779817,-0.733944954,
-0.732110092,-0.730275229,-0.728440367,-0.726605505,-0.724770642,-0.72293578,
-0.721100917,-0.719266055,-0.717431193,-0.71559633,-0.713761468,-0.711926606,
-0.710091743,-0.708256881,-0.706422018,-0.704587156,-0.702752294,-0.700917431,
-0.699082569,-0.697247706,-0.695412844,-0.693577982,-0.691743119,-0.689908257,
-0.688073394,-0.686238532,-0.68440367,-0.682568807,-0.680733945,-0.678899083,
-0.67706422,-0.675229358,-0.673394495,-0.671559633,-0.669724771,-0.667889908,
-0.666055046,-0.664220183,-0.662385321,-0.660550459,-0.658715596,-0.656880734,
-0.655045872,-0.653211009,-0.651376147,-0.649541284,-0.647706422,-0.64587156,
-0.644036697,-0.642201835,-0.640366972,-0.63853211,-0.636697248,-0.634862385,
-0.633027523,-0.631192661,-0.629357798,-0.627522936,-0.625688073,-0.623853211,
-0.622018349,-0.620183486,-0.618348624,-0.616513761,-0.614678899,-0.612844037,
-0.611009174,-0.609174312,-0.60733945,-0.605504587,-0.603669725,-0.601834862,
-0.6,-0.598165138,-0.596330275,-0.594495413,-0.59266055,-0.590825688,-0.588990826,
-0.587155963,-0.585321101,-0.583486239,-0.581651376,-0.579816514,-0.577981651,
-0.576146789,-0.574311927,-0.572477064,-0.570642202,-0.568807339,-0.566972477,
-0.565137615,-0.563302752,-0.56146789,-0.559633028,-0.557798165,-0.555963303,
-0.55412844,-0.552293578,-0.550458716,-0.548623853,-0.546788991,-0.544954128,
-0.543119266,-0.541284404,-0.539449541,-0.537614679,-0.535779817,-0.533944954,
-0.532110092,-0.530275229,-0.528440367,-0.526605505,-0.524770642,-0.52293578,
-0.521100917,-0.519266055,-0.517431193,-0.51559633,-0.513761468,-0.511926606,
-0.510091743,-0.508256881,-0.506422018,-0.504587156,-0.502752294,-0.500917431,
-0.499082569,-0.497247706,-0.495412844,-0.493577982,-0.491743119,-0.489908257,
-0.488073394,-0.486238532,-0.48440367,-0.482568807,-0.480733945,-0.478899083,
-0.47706422,-0.475229358,-0.473394495,-0.471559633,-0.469724771,-0.467889908,
-0.466055046,-0.464220183,-0.462385321,-0.460550459,-0.458715596,-0.456880734,
-0.455045872,-0.453211009,-0.451376147,-0.449541284,-0.447706422,-0.44587156,
-0.444036697,-0.442201835,-0.440366972,-0.43853211,-0.436697248,-0.434862385,
-0.433027523,-0.431192661,-0.429357798,-0.427522936,-0.425688073,-0.423853211,
-0.422018349,-0.420183486,-0.418348624,-0.416513761,-0.414678899,-0.412844037,
-0.411009174,-0.409174312,-0.40733945,-0.405504587,-0.403669725,-0.401834862,
-0.4,-0.398165138,-0.396330275,-0.394495413,-0.39266055,-0.390825688,-0.388990826,
-0.387155963,-0.385321101,-0.383486239,-0.381651376,-0.379816514,-0.377981651,
-0.376146789,-0.374311927,-0.372477064,-0.370642202,-0.368807339,-0.366972477,
-0.365137615,-0.363302752,-0.36146789,-0.359633028,-0.357798165,-0.355963303,
-0.35412844,-0.352293578,-0.350458716,-0.348623853,-0.346788991,-0.344954128,
-0.343119266,-0.341284404,-0.339449541,-0.337614679,-0.335779817,-0.333944954,
-0.332110092,-0.330275229,-0.328440367,-0.326605505,-0.324770642,-0.32293578,
-0.321100917,-0.319266055,-0.317431193,-0.31559633,-0.313761468,-0.311926606,
-0.310091743,-0.308256881,-0.306422018,-0.304587156,-0.302752294,-0.300917431,
-0.299082569,-0.297247706,-0.295412844,-0.293577982,-0.291743119,-0.289908257,
-0.288073394,-0.286238532,-0.28440367,-0.282568807,-0.280733945,-0.278899083,
-0.27706422,-0.275229358,-0.273394495,-0.271559633,-0.269724771,-0.267889908,
-0.266055046,-0.264220183,-0.262385321,-0.260550459,-0.258715596,-0.256880734,
-0.255045872,-0.253211009,-0.251376147,-0.249541284,-0.247706422,-0.24587156,
-0.244036697,-0.242201835,-0.240366972,-0.23853211,-0.236697248,-0.234862385,
-0.233027523,-0.231192661,-0.229357798,-0.227522936,-0.225688073,-0.223853211,
-0.222018349,-0.220183486,-0.218348624,-0.216513761,-0.214678899,-0.212844037,
-0.211009174,-0.209174312,-0.20733945,-0.205504587,-0.203669725,-0.201834862,
-0.2,-0.198165138,-0.196330275,-0.194495413,-0.19266055,-0.190825688,-0.188990826,
-0.187155963,-0.185321101,-0.183486239,-0.181651376,-0.179816514,-0.177981651,
-0.176146789,-0.174311927,-0.172477064,-0.170642202,-0.168807339,-0.166972477,
-0.165137615,-0.163302752,-0.16146789,-0.159633028,-0.157798165,-0.155963303,
-0.15412844,-0.152293578,-0.150458716,-0.148623853,-0.146788991,-0.144954128,
-0.143172103),(0.,0.36),.UNSPECIFIED.);
#6289=B_SPLINE_SURFACE_WITH_KNOTS('',5,1,((#276047,#276048),(#276049,#276050),
(#276051,#276052),(#276053,#276054),(#276055,#276056),(#276057,#276058),
(#276059,#276060),(#276061,#276062),(#276063,#276064),(#276065,#276066),
(#276067,#276068),(#276069,#276070),(#276071,#276072),(#276073,#276074),
(#276075,#276076),(#276077,#276078),(#276079,#276080),(#276081,#276082),
(#276083,#276084),(#276085,#276086),(#276087,#276088),(#276089,#276090),
(#276091,#276092),(#276093,#276094),(#276095,#276096),(#276097,#276098),
(#276099,#276100),(#276101,#276102),(#276103,#276104),(#276105,#276106),
(#276107,#276108),(#276109,#276110),(#276111,#276112),(#276113,#276114),
(#276115,#276116),(#276117,#276118),(#276119,#276120),(#276121,#276122),
(#276123,#276124),(#276125,#276126),(#276127,#276128),(#276129,#276130),
(#276131,#276132),(#276133,#276134),(#276135,#276136),(#276137,#276138),
(#276139,#276140),(#276141,#276142),(#276143,#276144),(#276145,#276146),
(#276147,#276148),(#276149,#276150),(#276151,#276152),(#276153,#276154),
(#276155,#276156),(#276157,#276158),(#276159,#276160),(#276161,#276162),
(#276163,#276164),(#276165,#276166),(#276167,#276168),(#276169,#276170),
(#276171,#276172),(#276173,#276174),(#276175,#276176),(#276177,#276178),
(#276179,#276180),(#276181,#276182),(#276183,#276184),(#276185,#276186),
(#276187,#276188),(#276189,#276190),(#276191,#276192),(#276193,#276194),
(#276195,#276196),(#276197,#276198),(#276199,#276200),(#276201,#276202),
(#276203,#276204),(#276205,#276206),(#276207,#276208),(#276209,#276210),
(#276211,#276212),(#276213,#276214),(#276215,#276216),(#276217,#276218),
(#276219,#276220),(#276221,#276222),(#276223,#276224),(#276225,#276226),
(#276227,#276228),(#276229,#276230),(#276231,#276232),(#276233,#276234),
(#276235,#276236),(#276237,#276238),(#276239,#276240),(#276241,#276242),
(#276243,#276244),(#276245,#276246),(#276247,#276248),(#276249,#276250),
(#276251,#276252),(#276253,#276254),(#276255,#276256),(#276257,#276258),
(#276259,#276260),(#276261,#276262),(#276263,#276264),(#276265,#276266),
(#276267,#276268),(#276269,#276270),(#276271,#276272),(#276273,#276274),
(#276275,#276276),(#276277,#276278),(#276279,#276280),(#276281,#276282),
(#276283,#276284),(#276285,#276286),(#276287,#276288),(#276289,#276290),
(#276291,#276292),(#276293,#276294),(#276295,#276296),(#276297,#276298),
(#276299,#276300),(#276301,#276302),(#276303,#276304),(#276305,#276306),
(#276307,#276308),(#276309,#276310),(#276311,#276312),(#276313,#276314),
(#276315,#276316),(#276317,#276318),(#276319,#276320),(#276321,#276322),
(#276323,#276324),(#276325,#276326),(#276327,#276328),(#276329,#276330),
(#276331,#276332),(#276333,#276334),(#276335,#276336),(#276337,#276338),
(#276339,#276340),(#276341,#276342),(#276343,#276344),(#276345,#276346),
(#276347,#276348),(#276349,#276350),(#276351,#276352),(#276353,#276354),
(#276355,#276356),(#276357,#276358),(#276359,#276360),(#276361,#276362),
(#276363,#276364),(#276365,#276366),(#276367,#276368),(#276369,#276370),
(#276371,#276372),(#276373,#276374),(#276375,#276376),(#276377,#276378),
(#276379,#276380),(#276381,#276382),(#276383,#276384),(#276385,#276386),
(#276387,#276388),(#276389,#276390),(#276391,#276392),(#276393,#276394),
(#276395,#276396),(#276397,#276398),(#276399,#276400),(#276401,#276402),
(#276403,#276404),(#276405,#276406),(#276407,#276408),(#276409,#276410),
(#276411,#276412),(#276413,#276414),(#276415,#276416),(#276417,#276418),
(#276419,#276420),(#276421,#276422),(#276423,#276424),(#276425,#276426),
(#276427,#276428),(#276429,#276430),(#276431,#276432),(#276433,#276434),
(#276435,#276436),(#276437,#276438),(#276439,#276440),(#276441,#276442),
(#276443,#276444),(#276445,#276446),(#276447,#276448),(#276449,#276450),
(#276451,#276452),(#276453,#276454),(#276455,#276456),(#276457,#276458),
(#276459,#276460),(#276461,#276462),(#276463,#276464),(#276465,#276466),
(#276467,#276468),(#276469,#276470),(#276471,#276472),(#276473,#276474),
(#276475,#276476),(#276477,#276478),(#276479,#276480),(#276481,#276482),
(#276483,#276484),(#276485,#276486),(#276487,#276488),(#276489,#276490),
(#276491,#276492),(#276493,#276494),(#276495,#276496),(#276497,#276498),
(#276499,#276500),(#276501,#276502),(#276503,#276504),(#276505,#276506),
(#276507,#276508),(#276509,#276510),(#276511,#276512),(#276513,#276514),
(#276515,#276516),(#276517,#276518),(#276519,#276520),(#276521,#276522),
(#276523,#276524),(#276525,#276526),(#276527,#276528),(#276529,#276530),
(#276531,#276532),(#276533,#276534),(#276535,#276536),(#276537,#276538),
(#276539,#276540),(#276541,#276542),(#276543,#276544),(#276545,#276546),
(#276547,#276548),(#276549,#276550),(#276551,#276552),(#276553,#276554),
(#276555,#276556),(#276557,#276558),(#276559,#276560),(#276561,#276562),
(#276563,#276564),(#276565,#276566),(#276567,#276568),(#276569,#276570),
(#276571,#276572),(#276573,#276574),(#276575,#276576),(#276577,#276578),
(#276579,#276580),(#276581,#276582),(#276583,#276584),(#276585,#276586),
(#276587,#276588),(#276589,#276590),(#276591,#276592),(#276593,#276594),
(#276595,#276596),(#276597,#276598),(#276599,#276600),(#276601,#276602),
(#276603,#276604),(#276605,#276606),(#276607,#276608),(#276609,#276610),
(#276611,#276612),(#276613,#276614),(#276615,#276616),(#276617,#276618),
(#276619,#276620),(#276621,#276622),(#276623,#276624),(#276625,#276626),
(#276627,#276628),(#276629,#276630),(#276631,#276632),(#276633,#276634),
(#276635,#276636),(#276637,#276638),(#276639,#276640),(#276641,#276642),
(#276643,#276644),(#276645,#276646),(#276647,#276648),(#276649,#276650),
(#276651,#276652),(#276653,#276654),(#276655,#276656),(#276657,#276658),
(#276659,#276660),(#276661,#276662),(#276663,#276664),(#276665,#276666),
(#276667,#276668),(#276669,#276670),(#276671,#276672),(#276673,#276674),
(#276675,#276676),(#276677,#276678),(#276679,#276680),(#276681,#276682),
(#276683,#276684),(#276685,#276686),(#276687,#276688),(#276689,#276690),
(#276691,#276692),(#276693,#276694),(#276695,#276696),(#276697,#276698),
(#276699,#276700),(#276701,#276702),(#276703,#276704),(#276705,#276706),
(#276707,#276708),(#276709,#276710),(#276711,#276712),(#276713,#276714),
(#276715,#276716),(#276717,#276718),(#276719,#276720),(#276721,#276722),
(#276723,#276724),(#276725,#276726),(#276727,#276728),(#276729,#276730),
(#276731,#276732),(#276733,#276734),(#276735,#276736),(#276737,#276738),
(#276739,#276740),(#276741,#276742),(#276743,#276744),(#276745,#276746),
(#276747,#276748),(#276749,#276750),(#276751,#276752),(#276753,#276754),
(#276755,#276756),(#276757,#276758),(#276759,#276760),(#276761,#276762),
(#276763,#276764),(#276765,#276766),(#276767,#276768),(#276769,#276770),
(#276771,#276772),(#276773,#276774),(#276775,#276776),(#276777,#276778),
(#276779,#276780),(#276781,#276782),(#276783,#276784),(#276785,#276786),
(#276787,#276788),(#276789,#276790),(#276791,#276792),(#276793,#276794),
(#276795,#276796),(#276797,#276798),(#276799,#276800),(#276801,#276802),
(#276803,#276804),(#276805,#276806),(#276807,#276808),(#276809,#276810),
(#276811,#276812),(#276813,#276814),(#276815,#276816),(#276817,#276818),
(#276819,#276820),(#276821,#276822),(#276823,#276824),(#276825,#276826),
(#276827,#276828),(#276829,#276830),(#276831,#276832),(#276833,#276834),
(#276835,#276836),(#276837,#276838),(#276839,#276840),(#276841,#276842),
(#276843,#276844),(#276845,#276846),(#276847,#276848),(#276849,#276850),
(#276851,#276852),(#276853,#276854),(#276855,#276856),(#276857,#276858),
(#276859,#276860),(#276861,#276862),(#276863,#276864),(#276865,#276866),
(#276867,#276868),(#276869,#276870),(#276871,#276872),(#276873,#276874),
(#276875,#276876),(#276877,#276878),(#276879,#276880),(#276881,#276882),
(#276883,#276884),(#276885,#276886),(#276887,#276888),(#276889,#276890),
(#276891,#276892),(#276893,#276894),(#276895,#276896),(#276897,#276898),
(#276899,#276900),(#276901,#276902),(#276903,#276904),(#276905,#276906),
(#276907,#276908),(#276909,#276910),(#276911,#276912),(#276913,#276914),
(#276915,#276916),(#276917,#276918),(#276919,#276920),(#276921,#276922),
(#276923,#276924),(#276925,#276926),(#276927,#276928),(#276929,#276930),
(#276931,#276932),(#276933,#276934),(#276935,#276936),(#276937,#276938),
(#276939,#276940),(#276941,#276942),(#276943,#276944),(#276945,#276946),
(#276947,#276948),(#276949,#276950),(#276951,#276952),(#276953,#276954),
(#276955,#276956),(#276957,#276958),(#276959,#276960),(#276961,#276962),
(#276963,#276964),(#276965,#276966),(#276967,#276968),(#276969,#276970),
(#276971,#276972),(#276973,#276974),(#276975,#276976),(#276977,#276978),
(#276979,#276980),(#276981,#276982),(#276983,#276984),(#276985,#276986),
(#276987,#276988),(#276989,#276990)),.UNSPECIFIED.,.F.,.F.,.F.,(6,1,1,1,
1,1,1,1,1,1,1,1,1,1,1,1,1,1,1,1,1,1,1,1,1,1,1,1,1,1,1,1,1,1,1,1,1,1,1,1,
1,1,1,1,1,1,1,1,1,1,1,1,1,1,1,1,1,1,1,1,1,1,1,1,1,1,1,1,1,1,1,1,1,1,1,1,
1,1,1,1,1,1,1,1,1,1,1,1,1,1,1,1,1,1,1,1,1,1,1,1,1,1,1,1,1,1,1,1,1,1,1,1,
1,1,1,1,1,1,1,1,1,1,1,1,1,1,1,1,1,1,1,1,1,1,1,1,1,1,1,1,1,1,1,1,1,1,1,1,
1,1,1,1,1,1,1,1,1,1,1,1,1,1,1,1,1,1,1,1,1,1,1,1,1,1,1,1,1,1,1,1,1,1,1,1,
1,1,1,1,1,1,1,1,1,1,1,1,1,1,1,1,1,1,1,1,1,1,1,1,1,1,1,1,1,1,1,1,1,1,1,1,
1,1,1,1,1,1,1,1,1,1,1,1,1,1,1,1,1,1,1,1,1,1,1,1,1,1,1,1,1,1,1,1,1,1,1,1,
1,1,1,1,1,1,1,1,1,1,1,1,1,1,1,1,1,1,1,1,1,1,1,1,1,1,1,1,1,1,1,1,1,1,1,1,
1,1,1,1,1,1,1,1,1,1,1,1,1,1,1,1,1,1,1,1,1,1,1,1,1,1,1,1,1,1,1,1,1,1,1,1,
1,1,1,1,1,1,1,1,1,1,1,1,1,1,1,1,1,1,1,1,1,1,1,1,1,1,1,1,1,1,1,1,1,1,1,1,
1,1,1,1,1,1,1,1,1,1,1,1,1,1,1,1,1,1,1,1,1,1,1,1,1,1,1,1,1,1,1,1,1,1,1,1,
1,1,1,1,1,1,1,1,1,1,1,1,1,1,1,1,1,1,1,1,1,1,1,1,1,1,1,1,1,1,1,1,1,1,1,1,
1,1,1,1,1,1,1,1,1,1,1,1,1,1,1,1,1,1,1,1,1,1,1,1,1,1,1,1,1,1,1,6),(2,2),
(-1.,-0.998165138,-0.996330275,-0.994495413,-0.99266055,-0.990825688,-0.988990826,
-0.987155963,-0.985321101,-0.983486239,-0.981651376,-0.979816514,-0.977981651,
-0.976146789,-0.974311927,-0.972477064,-0.970642202,-0.968807339,-0.966972477,
-0.965137615,-0.963302752,-0.96146789,-0.959633028,-0.957798165,-0.955963303,
-0.95412844,-0.952293578,-0.950458716,-0.948623853,-0.946788991,-0.944954128,
-0.943119266,-0.941284404,-0.939449541,-0.937614679,-0.935779817,-0.933944954,
-0.932110092,-0.930275229,-0.928440367,-0.926605505,-0.924770642,-0.92293578,
-0.921100917,-0.919266055,-0.917431193,-0.91559633,-0.913761468,-0.911926606,
-0.910091743,-0.908256881,-0.906422018,-0.904587156,-0.902752294,-0.900917431,
-0.899082569,-0.897247706,-0.895412844,-0.893577982,-0.891743119,-0.889908257,
-0.888073394,-0.886238532,-0.88440367,-0.882568807,-0.880733945,-0.878899083,
-0.87706422,-0.875229358,-0.873394495,-0.871559633,-0.869724771,-0.867889908,
-0.866055046,-0.864220183,-0.862385321,-0.860550459,-0.858715596,-0.856880734,
-0.855045872,-0.853211009,-0.851376147,-0.849541284,-0.847706422,-0.84587156,
-0.844036697,-0.842201835,-0.840366972,-0.83853211,-0.836697248,-0.834862385,
-0.833027523,-0.831192661,-0.829357798,-0.827522936,-0.825688073,-0.823853211,
-0.822018349,-0.820183486,-0.818348624,-0.816513761,-0.814678899,-0.812844037,
-0.811009174,-0.809174312,-0.80733945,-0.805504587,-0.803669725,-0.801834862,
-0.8,-0.798165138,-0.796330275,-0.794495413,-0.79266055,-0.790825688,-0.788990826,
-0.787155963,-0.785321101,-0.783486239,-0.781651376,-0.779816514,-0.777981651,
-0.776146789,-0.774311927,-0.772477064,-0.770642202,-0.768807339,-0.766972477,
-0.765137615,-0.763302752,-0.76146789,-0.759633028,-0.757798165,-0.755963303,
-0.75412844,-0.752293578,-0.750458716,-0.748623853,-0.746788991,-0.744954128,
-0.743119266,-0.741284404,-0.739449541,-0.737614679,-0.735779817,-0.733944954,
-0.732110092,-0.730275229,-0.728440367,-0.726605505,-0.724770642,-0.72293578,
-0.721100917,-0.719266055,-0.717431193,-0.71559633,-0.713761468,-0.711926606,
-0.710091743,-0.708256881,-0.706422018,-0.704587156,-0.702752294,-0.700917431,
-0.699082569,-0.697247706,-0.695412844,-0.693577982,-0.691743119,-0.689908257,
-0.688073394,-0.686238532,-0.68440367,-0.682568807,-0.680733945,-0.678899083,
-0.67706422,-0.675229358,-0.673394495,-0.671559633,-0.669724771,-0.667889908,
-0.666055046,-0.664220183,-0.662385321,-0.660550459,-0.658715596,-0.656880734,
-0.655045872,-0.653211009,-0.651376147,-0.649541284,-0.647706422,-0.64587156,
-0.644036697,-0.642201835,-0.640366972,-0.63853211,-0.636697248,-0.634862385,
-0.633027523,-0.631192661,-0.629357798,-0.627522936,-0.625688073,-0.623853211,
-0.622018349,-0.620183486,-0.618348624,-0.616513761,-0.614678899,-0.612844037,
-0.611009174,-0.609174312,-0.60733945,-0.605504587,-0.603669725,-0.601834862,
-0.6,-0.598165138,-0.596330275,-0.594495413,-0.59266055,-0.590825688,-0.588990826,
-0.587155963,-0.585321101,-0.583486239,-0.581651376,-0.579816514,-0.577981651,
-0.576146789,-0.574311927,-0.572477064,-0.570642202,-0.568807339,-0.566972477,
-0.565137615,-0.563302752,-0.56146789,-0.559633028,-0.557798165,-0.555963303,
-0.55412844,-0.552293578,-0.550458716,-0.548623853,-0.546788991,-0.544954128,
-0.543119266,-0.541284404,-0.539449541,-0.537614679,-0.535779817,-0.533944954,
-0.532110092,-0.530275229,-0.528440367,-0.526605505,-0.524770642,-0.52293578,
-0.521100917,-0.519266055,-0.517431193,-0.51559633,-0.513761468,-0.511926606,
-0.510091743,-0.508256881,-0.506422018,-0.504587156,-0.502752294,-0.500917431,
-0.499082569,-0.497247706,-0.495412844,-0.493577982,-0.491743119,-0.489908257,
-0.488073394,-0.486238532,-0.48440367,-0.482568807,-0.480733945,-0.478899083,
-0.47706422,-0.475229358,-0.473394495,-0.471559633,-0.469724771,-0.467889908,
-0.466055046,-0.464220183,-0.462385321,-0.460550459,-0.458715596,-0.456880734,
-0.455045872,-0.453211009,-0.451376147,-0.449541284,-0.447706422,-0.44587156,
-0.444036697,-0.442201835,-0.440366972,-0.43853211,-0.436697248,-0.434862385,
-0.433027523,-0.431192661,-0.429357798,-0.427522936,-0.425688073,-0.423853211,
-0.422018349,-0.420183486,-0.418348624,-0.416513761,-0.414678899,-0.412844037,
-0.411009174,-0.409174312,-0.40733945,-0.405504587,-0.403669725,-0.401834862,
-0.4,-0.398165138,-0.396330275,-0.394495413,-0.39266055,-0.390825688,-0.388990826,
-0.387155963,-0.385321101,-0.383486239,-0.381651376,-0.379816514,-0.377981651,
-0.376146789,-0.374311927,-0.372477064,-0.370642202,-0.368807339,-0.366972477,
-0.365137615,-0.363302752,-0.36146789,-0.359633028,-0.357798165,-0.355963303,
-0.35412844,-0.352293578,-0.350458716,-0.348623853,-0.346788991,-0.344954128,
-0.343119266,-0.341284404,-0.339449541,-0.337614679,-0.335779817,-0.333944954,
-0.332110092,-0.330275229,-0.328440367,-0.326605505,-0.324770642,-0.32293578,
-0.321100917,-0.319266055,-0.317431193,-0.31559633,-0.313761468,-0.311926606,
-0.310091743,-0.308256881,-0.306422018,-0.304587156,-0.302752294,-0.300917431,
-0.299082569,-0.297247706,-0.295412844,-0.293577982,-0.291743119,-0.289908257,
-0.288073394,-0.286238532,-0.28440367,-0.282568807,-0.280733945,-0.278899083,
-0.27706422,-0.275229358,-0.273394495,-0.271559633,-0.269724771,-0.267889908,
-0.266055046,-0.264220183,-0.262385321,-0.260550459,-0.258715596,-0.256880734,
-0.255045872,-0.253211009,-0.251376147,-0.249541284,-0.247706422,-0.24587156,
-0.244036697,-0.242201835,-0.240366972,-0.23853211,-0.236697248,-0.234862385,
-0.233027523,-0.231192661,-0.229357798,-0.227522936,-0.225688073,-0.223853211,
-0.222018349,-0.220183486,-0.218348624,-0.216513761,-0.214678899,-0.212844037,
-0.211009174,-0.209174312,-0.20733945,-0.205504587,-0.203669725,-0.201834862,
-0.2,-0.198165138,-0.196330275,-0.194495413,-0.19266055,-0.190825688,-0.188990826,
-0.187155963,-0.185321101,-0.183486239,-0.181651376,-0.179816514,-0.177981651,
-0.176146789,-0.174311927,-0.172477064,-0.170642202,-0.168807339,-0.166972477,
-0.165137615,-0.163302752,-0.16146789,-0.159633028,-0.157798165,-0.155963303,
-0.15412844,-0.152293578,-0.150458716,-0.148623853,-0.146788991,-0.144954128,
-0.143172103),(0.,0.36),.UNSPECIFIED.);
#6290=B_SPLINE_SURFACE_WITH_KNOTS('',5,1,((#277936,#277937),(#277938,#277939),
(#277940,#277941),(#277942,#277943),(#277944,#277945),(#277946,#277947),
(#277948,#277949),(#277950,#277951),(#277952,#277953),(#277954,#277955),
(#277956,#277957),(#277958,#277959),(#277960,#277961),(#277962,#277963),
(#277964,#277965),(#277966,#277967),(#277968,#277969),(#277970,#277971),
(#277972,#277973),(#277974,#277975),(#277976,#277977),(#277978,#277979),
(#277980,#277981),(#277982,#277983),(#277984,#277985),(#277986,#277987),
(#277988,#277989),(#277990,#277991),(#277992,#277993),(#277994,#277995),
(#277996,#277997),(#277998,#277999),(#278000,#278001),(#278002,#278003),
(#278004,#278005),(#278006,#278007),(#278008,#278009),(#278010,#278011),
(#278012,#278013),(#278014,#278015),(#278016,#278017),(#278018,#278019),
(#278020,#278021),(#278022,#278023),(#278024,#278025),(#278026,#278027),
(#278028,#278029),(#278030,#278031),(#278032,#278033),(#278034,#278035),
(#278036,#278037),(#278038,#278039),(#278040,#278041),(#278042,#278043),
(#278044,#278045),(#278046,#278047),(#278048,#278049),(#278050,#278051),
(#278052,#278053),(#278054,#278055),(#278056,#278057),(#278058,#278059),
(#278060,#278061),(#278062,#278063),(#278064,#278065),(#278066,#278067),
(#278068,#278069),(#278070,#278071),(#278072,#278073),(#278074,#278075),
(#278076,#278077),(#278078,#278079),(#278080,#278081),(#278082,#278083),
(#278084,#278085),(#278086,#278087),(#278088,#278089),(#278090,#278091),
(#278092,#278093),(#278094,#278095),(#278096,#278097),(#278098,#278099),
(#278100,#278101),(#278102,#278103),(#278104,#278105),(#278106,#278107),
(#278108,#278109),(#278110,#278111),(#278112,#278113),(#278114,#278115),
(#278116,#278117),(#278118,#278119),(#278120,#278121),(#278122,#278123),
(#278124,#278125),(#278126,#278127),(#278128,#278129),(#278130,#278131),
(#278132,#278133),(#278134,#278135),(#278136,#278137),(#278138,#278139),
(#278140,#278141),(#278142,#278143),(#278144,#278145),(#278146,#278147),
(#278148,#278149),(#278150,#278151),(#278152,#278153),(#278154,#278155),
(#278156,#278157),(#278158,#278159),(#278160,#278161),(#278162,#278163),
(#278164,#278165),(#278166,#278167),(#278168,#278169),(#278170,#278171),
(#278172,#278173),(#278174,#278175),(#278176,#278177),(#278178,#278179),
(#278180,#278181),(#278182,#278183),(#278184,#278185),(#278186,#278187),
(#278188,#278189),(#278190,#278191),(#278192,#278193),(#278194,#278195),
(#278196,#278197),(#278198,#278199),(#278200,#278201),(#278202,#278203),
(#278204,#278205),(#278206,#278207),(#278208,#278209),(#278210,#278211),
(#278212,#278213),(#278214,#278215),(#278216,#278217),(#278218,#278219),
(#278220,#278221),(#278222,#278223),(#278224,#278225),(#278226,#278227),
(#278228,#278229),(#278230,#278231),(#278232,#278233),(#278234,#278235),
(#278236,#278237),(#278238,#278239),(#278240,#278241),(#278242,#278243),
(#278244,#278245),(#278246,#278247),(#278248,#278249),(#278250,#278251),
(#278252,#278253),(#278254,#278255),(#278256,#278257),(#278258,#278259),
(#278260,#278261),(#278262,#278263),(#278264,#278265),(#278266,#278267),
(#278268,#278269),(#278270,#278271),(#278272,#278273),(#278274,#278275),
(#278276,#278277),(#278278,#278279),(#278280,#278281),(#278282,#278283),
(#278284,#278285),(#278286,#278287),(#278288,#278289),(#278290,#278291),
(#278292,#278293),(#278294,#278295),(#278296,#278297),(#278298,#278299),
(#278300,#278301),(#278302,#278303),(#278304,#278305),(#278306,#278307),
(#278308,#278309),(#278310,#278311),(#278312,#278313),(#278314,#278315),
(#278316,#278317),(#278318,#278319),(#278320,#278321),(#278322,#278323),
(#278324,#278325),(#278326,#278327),(#278328,#278329),(#278330,#278331),
(#278332,#278333),(#278334,#278335),(#278336,#278337),(#278338,#278339),
(#278340,#278341),(#278342,#278343),(#278344,#278345),(#278346,#278347),
(#278348,#278349),(#278350,#278351),(#278352,#278353),(#278354,#278355),
(#278356,#278357),(#278358,#278359),(#278360,#278361),(#278362,#278363),
(#278364,#278365),(#278366,#278367),(#278368,#278369),(#278370,#278371),
(#278372,#278373),(#278374,#278375),(#278376,#278377),(#278378,#278379),
(#278380,#278381),(#278382,#278383),(#278384,#278385),(#278386,#278387),
(#278388,#278389),(#278390,#278391),(#278392,#278393),(#278394,#278395),
(#278396,#278397),(#278398,#278399),(#278400,#278401),(#278402,#278403),
(#278404,#278405),(#278406,#278407),(#278408,#278409),(#278410,#278411),
(#278412,#278413),(#278414,#278415),(#278416,#278417),(#278418,#278419),
(#278420,#278421),(#278422,#278423),(#278424,#278425),(#278426,#278427),
(#278428,#278429),(#278430,#278431),(#278432,#278433),(#278434,#278435),
(#278436,#278437),(#278438,#278439),(#278440,#278441),(#278442,#278443),
(#278444,#278445),(#278446,#278447),(#278448,#278449),(#278450,#278451),
(#278452,#278453),(#278454,#278455),(#278456,#278457),(#278458,#278459),
(#278460,#278461),(#278462,#278463),(#278464,#278465),(#278466,#278467),
(#278468,#278469),(#278470,#278471),(#278472,#278473),(#278474,#278475),
(#278476,#278477),(#278478,#278479),(#278480,#278481),(#278482,#278483),
(#278484,#278485),(#278486,#278487),(#278488,#278489),(#278490,#278491),
(#278492,#278493),(#278494,#278495),(#278496,#278497),(#278498,#278499),
(#278500,#278501),(#278502,#278503),(#278504,#278505),(#278506,#278507),
(#278508,#278509),(#278510,#278511),(#278512,#278513),(#278514,#278515),
(#278516,#278517),(#278518,#278519),(#278520,#278521),(#278522,#278523),
(#278524,#278525),(#278526,#278527),(#278528,#278529),(#278530,#278531),
(#278532,#278533),(#278534,#278535),(#278536,#278537),(#278538,#278539),
(#278540,#278541),(#278542,#278543),(#278544,#278545),(#278546,#278547),
(#278548,#278549),(#278550,#278551),(#278552,#278553),(#278554,#278555),
(#278556,#278557),(#278558,#278559),(#278560,#278561),(#278562,#278563),
(#278564,#278565),(#278566,#278567),(#278568,#278569),(#278570,#278571),
(#278572,#278573),(#278574,#278575),(#278576,#278577),(#278578,#278579),
(#278580,#278581),(#278582,#278583),(#278584,#278585),(#278586,#278587),
(#278588,#278589),(#278590,#278591),(#278592,#278593),(#278594,#278595),
(#278596,#278597),(#278598,#278599),(#278600,#278601),(#278602,#278603),
(#278604,#278605),(#278606,#278607),(#278608,#278609),(#278610,#278611),
(#278612,#278613),(#278614,#278615),(#278616,#278617),(#278618,#278619),
(#278620,#278621),(#278622,#278623),(#278624,#278625),(#278626,#278627),
(#278628,#278629),(#278630,#278631),(#278632,#278633),(#278634,#278635),
(#278636,#278637),(#278638,#278639),(#278640,#278641),(#278642,#278643),
(#278644,#278645),(#278646,#278647),(#278648,#278649),(#278650,#278651),
(#278652,#278653),(#278654,#278655),(#278656,#278657),(#278658,#278659),
(#278660,#278661),(#278662,#278663),(#278664,#278665),(#278666,#278667),
(#278668,#278669),(#278670,#278671),(#278672,#278673),(#278674,#278675),
(#278676,#278677),(#278678,#278679),(#278680,#278681),(#278682,#278683),
(#278684,#278685),(#278686,#278687),(#278688,#278689),(#278690,#278691),
(#278692,#278693),(#278694,#278695),(#278696,#278697),(#278698,#278699),
(#278700,#278701),(#278702,#278703),(#278704,#278705),(#278706,#278707),
(#278708,#278709),(#278710,#278711),(#278712,#278713),(#278714,#278715),
(#278716,#278717),(#278718,#278719),(#278720,#278721),(#278722,#278723),
(#278724,#278725),(#278726,#278727),(#278728,#278729),(#278730,#278731),
(#278732,#278733),(#278734,#278735),(#278736,#278737),(#278738,#278739),
(#278740,#278741),(#278742,#278743),(#278744,#278745),(#278746,#278747),
(#278748,#278749),(#278750,#278751),(#278752,#278753),(#278754,#278755),
(#278756,#278757),(#278758,#278759),(#278760,#278761),(#278762,#278763),
(#278764,#278765),(#278766,#278767),(#278768,#278769),(#278770,#278771),
(#278772,#278773),(#278774,#278775),(#278776,#278777),(#278778,#278779),
(#278780,#278781),(#278782,#278783),(#278784,#278785),(#278786,#278787),
(#278788,#278789),(#278790,#278791),(#278792,#278793),(#278794,#278795),
(#278796,#278797),(#278798,#278799),(#278800,#278801),(#278802,#278803),
(#278804,#278805),(#278806,#278807),(#278808,#278809),(#278810,#278811),
(#278812,#278813),(#278814,#278815),(#278816,#278817),(#278818,#278819),
(#278820,#278821),(#278822,#278823),(#278824,#278825),(#278826,#278827),
(#278828,#278829),(#278830,#278831),(#278832,#278833),(#278834,#278835),
(#278836,#278837),(#278838,#278839),(#278840,#278841),(#278842,#278843),
(#278844,#278845),(#278846,#278847),(#278848,#278849),(#278850,#278851),
(#278852,#278853),(#278854,#278855),(#278856,#278857),(#278858,#278859),
(#278860,#278861),(#278862,#278863),(#278864,#278865),(#278866,#278867),
(#278868,#278869),(#278870,#278871),(#278872,#278873),(#278874,#278875),
(#278876,#278877),(#278878,#278879)),.UNSPECIFIED.,.F.,.F.,.F.,(6,1,1,1,
1,1,1,1,1,1,1,1,1,1,1,1,1,1,1,1,1,1,1,1,1,1,1,1,1,1,1,1,1,1,1,1,1,1,1,1,
1,1,1,1,1,1,1,1,1,1,1,1,1,1,1,1,1,1,1,1,1,1,1,1,1,1,1,1,1,1,1,1,1,1,1,1,
1,1,1,1,1,1,1,1,1,1,1,1,1,1,1,1,1,1,1,1,1,1,1,1,1,1,1,1,1,1,1,1,1,1,1,1,
1,1,1,1,1,1,1,1,1,1,1,1,1,1,1,1,1,1,1,1,1,1,1,1,1,1,1,1,1,1,1,1,1,1,1,1,
1,1,1,1,1,1,1,1,1,1,1,1,1,1,1,1,1,1,1,1,1,1,1,1,1,1,1,1,1,1,1,1,1,1,1,1,
1,1,1,1,1,1,1,1,1,1,1,1,1,1,1,1,1,1,1,1,1,1,1,1,1,1,1,1,1,1,1,1,1,1,1,1,
1,1,1,1,1,1,1,1,1,1,1,1,1,1,1,1,1,1,1,1,1,1,1,1,1,1,1,1,1,1,1,1,1,1,1,1,
1,1,1,1,1,1,1,1,1,1,1,1,1,1,1,1,1,1,1,1,1,1,1,1,1,1,1,1,1,1,1,1,1,1,1,1,
1,1,1,1,1,1,1,1,1,1,1,1,1,1,1,1,1,1,1,1,1,1,1,1,1,1,1,1,1,1,1,1,1,1,1,1,
1,1,1,1,1,1,1,1,1,1,1,1,1,1,1,1,1,1,1,1,1,1,1,1,1,1,1,1,1,1,1,1,1,1,1,1,
1,1,1,1,1,1,1,1,1,1,1,1,1,1,1,1,1,1,1,1,1,1,1,1,1,1,1,1,1,1,1,1,1,1,1,1,
1,1,1,1,1,1,1,1,1,1,1,1,1,1,1,1,1,1,1,1,1,1,1,1,1,1,1,1,1,1,1,1,1,1,1,1,
1,1,1,1,1,1,1,1,1,1,1,1,1,1,1,1,1,1,1,1,1,1,1,1,1,1,1,1,1,1,1,6),(2,2),
(0.143172103,0.144954128,0.146788991,0.148623853,0.150458716,0.152293578,
0.15412844,0.155963303,0.157798165,0.159633028,0.16146789,0.163302752,0.165137615,
0.166972477,0.168807339,0.170642202,0.172477064,0.174311927,0.176146789,
0.177981651,0.179816514,0.181651376,0.183486239,0.185321101,0.187155963,
0.188990826,0.190825688,0.19266055,0.194495413,0.196330275,0.198165138,
0.2,0.201834862,0.203669725,0.205504587,0.20733945,0.209174312,0.211009174,
0.212844037,0.214678899,0.216513761,0.218348624,0.220183486,0.222018349,
0.223853211,0.225688073,0.227522936,0.229357798,0.231192661,0.233027523,
0.234862385,0.236697248,0.23853211,0.240366972,0.242201835,0.244036697,
0.24587156,0.247706422,0.249541284,0.251376147,0.253211009,0.255045872,
0.256880734,0.258715596,0.260550459,0.262385321,0.264220183,0.266055046,
0.267889908,0.269724771,0.271559633,0.273394495,0.275229358,0.27706422,
0.278899083,0.280733945,0.282568807,0.28440367,0.286238532,0.288073394,
0.289908257,0.291743119,0.293577982,0.295412844,0.297247706,0.299082569,
0.300917431,0.302752294,0.304587156,0.306422018,0.308256881,0.310091743,
0.311926606,0.313761468,0.31559633,0.317431193,0.319266055,0.321100917,
0.32293578,0.324770642,0.326605505,0.328440367,0.330275229,0.332110092,
0.333944954,0.335779817,0.337614679,0.339449541,0.341284404,0.343119266,
0.344954128,0.346788991,0.348623853,0.350458716,0.352293578,0.35412844,
0.355963303,0.357798165,0.359633028,0.36146789,0.363302752,0.365137615,
0.366972477,0.368807339,0.370642202,0.372477064,0.374311927,0.376146789,
0.377981651,0.379816514,0.381651376,0.383486239,0.385321101,0.387155963,
0.388990826,0.390825688,0.39266055,0.394495413,0.396330275,0.398165138,
0.4,0.401834862,0.403669725,0.405504587,0.40733945,0.409174312,0.411009174,
0.412844037,0.414678899,0.416513761,0.418348624,0.420183486,0.422018349,
0.423853211,0.425688073,0.427522936,0.429357798,0.431192661,0.433027523,
0.434862385,0.436697248,0.43853211,0.440366972,0.442201835,0.444036697,
0.44587156,0.447706422,0.449541284,0.451376147,0.453211009,0.455045872,
0.456880734,0.458715596,0.460550459,0.462385321,0.464220183,0.466055046,
0.467889908,0.469724771,0.471559633,0.473394495,0.475229358,0.47706422,
0.478899083,0.480733945,0.482568807,0.48440367,0.486238532,0.488073394,
0.489908257,0.491743119,0.493577982,0.495412844,0.497247706,0.499082569,
0.500917431,0.502752294,0.504587156,0.506422018,0.508256881,0.510091743,
0.511926606,0.513761468,0.51559633,0.517431193,0.519266055,0.521100917,
0.52293578,0.524770642,0.526605505,0.528440367,0.530275229,0.532110092,
0.533944954,0.535779817,0.537614679,0.539449541,0.541284404,0.543119266,
0.544954128,0.546788991,0.548623853,0.550458716,0.552293578,0.55412844,
0.555963303,0.557798165,0.559633028,0.56146789,0.563302752,0.565137615,
0.566972477,0.568807339,0.570642202,0.572477064,0.574311927,0.576146789,
0.577981651,0.579816514,0.581651376,0.583486239,0.585321101,0.587155963,
0.588990826,0.590825688,0.59266055,0.594495413,0.596330275,0.598165138,
0.6,0.601834862,0.603669725,0.605504587,0.60733945,0.609174312,0.611009174,
0.612844037,0.614678899,0.616513761,0.618348624,0.620183486,0.622018349,
0.623853211,0.625688073,0.627522936,0.629357798,0.631192661,0.633027523,
0.634862385,0.636697248,0.63853211,0.640366972,0.642201835,0.644036697,
0.64587156,0.647706422,0.649541284,0.651376147,0.653211009,0.655045872,
0.656880734,0.658715596,0.660550459,0.662385321,0.664220183,0.666055046,
0.667889908,0.669724771,0.671559633,0.673394495,0.675229358,0.67706422,
0.678899083,0.680733945,0.682568807,0.68440367,0.686238532,0.688073394,
0.689908257,0.691743119,0.693577982,0.695412844,0.697247706,0.699082569,
0.700917431,0.702752294,0.704587156,0.706422018,0.708256881,0.710091743,
0.711926606,0.713761468,0.71559633,0.717431193,0.719266055,0.721100917,
0.72293578,0.724770642,0.726605505,0.728440367,0.730275229,0.732110092,
0.733944954,0.735779817,0.737614679,0.739449541,0.741284404,0.743119266,
0.744954128,0.746788991,0.748623853,0.750458716,0.752293578,0.75412844,
0.755963303,0.757798165,0.759633028,0.76146789,0.763302752,0.765137615,
0.766972477,0.768807339,0.770642202,0.772477064,0.774311927,0.776146789,
0.777981651,0.779816514,0.781651376,0.783486239,0.785321101,0.787155963,
0.788990826,0.790825688,0.79266055,0.794495413,0.796330275,0.798165138,
0.8,0.801834862,0.803669725,0.805504587,0.80733945,0.809174312,0.811009174,
0.812844037,0.814678899,0.816513761,0.818348624,0.820183486,0.822018349,
0.823853211,0.825688073,0.827522936,0.829357798,0.831192661,0.833027523,
0.834862385,0.836697248,0.83853211,0.840366972,0.842201835,0.844036697,
0.84587156,0.847706422,0.849541284,0.851376147,0.853211009,0.855045872,
0.856880734,0.858715596,0.860550459,0.862385321,0.864220183,0.866055046,
0.867889908,0.869724771,0.871559633,0.873394495,0.875229358,0.87706422,
0.878899083,0.880733945,0.882568807,0.88440367,0.886238532,0.888073394,
0.889908257,0.891743119,0.893577982,0.895412844,0.897247706,0.899082569,
0.900917431,0.902752294,0.904587156,0.906422018,0.908256881,0.910091743,
0.911926606,0.913761468,0.91559633,0.917431193,0.919266055,0.921100917,
0.92293578,0.924770642,0.926605505,0.928440367,0.930275229,0.932110092,
0.933944954,0.935779817,0.937614679,0.939449541,0.941284404,0.943119266,
0.944954128,0.946788991,0.948623853,0.950458716,0.952293578,0.95412844,
0.955963303,0.957798165,0.959633028,0.96146789,0.963302752,0.965137615,
0.966972477,0.968807339,0.970642202,0.972477064,0.974311927,0.976146789,
0.977981651,0.979816514,0.981651376,0.983486239,0.985321101,0.987155963,
0.988990826,0.990825688,0.99266055,0.994495413,0.996330275,0.998165138,
1.),(0.,0.36),.UNSPECIFIED.);
#6291=B_SPLINE_SURFACE_WITH_KNOTS('',5,1,((#279542,#279543),(#279544,#279545),
(#279546,#279547),(#279548,#279549),(#279550,#279551),(#279552,#279553),
(#279554,#279555),(#279556,#279557),(#279558,#279559),(#279560,#279561),
(#279562,#279563),(#279564,#279565),(#279566,#279567),(#279568,#279569),
(#279570,#279571),(#279572,#279573),(#279574,#279575),(#279576,#279577),
(#279578,#279579),(#279580,#279581),(#279582,#279583),(#279584,#279585),
(#279586,#279587),(#279588,#279589),(#279590,#279591),(#279592,#279593),
(#279594,#279595),(#279596,#279597),(#279598,#279599),(#279600,#279601),
(#279602,#279603),(#279604,#279605),(#279606,#279607),(#279608,#279609),
(#279610,#279611),(#279612,#279613),(#279614,#279615),(#279616,#279617),
(#279618,#279619),(#279620,#279621),(#279622,#279623),(#279624,#279625),
(#279626,#279627),(#279628,#279629),(#279630,#279631),(#279632,#279633),
(#279634,#279635),(#279636,#279637),(#279638,#279639),(#279640,#279641),
(#279642,#279643),(#279644,#279645),(#279646,#279647),(#279648,#279649),
(#279650,#279651),(#279652,#279653),(#279654,#279655),(#279656,#279657),
(#279658,#279659),(#279660,#279661),(#279662,#279663),(#279664,#279665),
(#279666,#279667),(#279668,#279669),(#279670,#279671),(#279672,#279673),
(#279674,#279675),(#279676,#279677),(#279678,#279679),(#279680,#279681),
(#279682,#279683),(#279684,#279685),(#279686,#279687),(#279688,#279689),
(#279690,#279691),(#279692,#279693),(#279694,#279695),(#279696,#279697),
(#279698,#279699),(#279700,#279701),(#279702,#279703),(#279704,#279705),
(#279706,#279707),(#279708,#279709),(#279710,#279711),(#279712,#279713),
(#279714,#279715),(#279716,#279717),(#279718,#279719),(#279720,#279721),
(#279722,#279723),(#279724,#279725),(#279726,#279727),(#279728,#279729),
(#279730,#279731),(#279732,#279733),(#279734,#279735),(#279736,#279737),
(#279738,#279739),(#279740,#279741),(#279742,#279743),(#279744,#279745),
(#279746,#279747),(#279748,#279749),(#279750,#279751),(#279752,#279753),
(#279754,#279755),(#279756,#279757),(#279758,#279759),(#279760,#279761),
(#279762,#279763),(#279764,#279765),(#279766,#279767),(#279768,#279769),
(#279770,#279771),(#279772,#279773),(#279774,#279775),(#279776,#279777),
(#279778,#279779),(#279780,#279781),(#279782,#279783),(#279784,#279785),
(#279786,#279787),(#279788,#279789),(#279790,#279791),(#279792,#279793),
(#279794,#279795),(#279796,#279797),(#279798,#279799),(#279800,#279801),
(#279802,#279803),(#279804,#279805),(#279806,#279807),(#279808,#279809),
(#279810,#279811),(#279812,#279813),(#279814,#279815),(#279816,#279817),
(#279818,#279819),(#279820,#279821),(#279822,#279823),(#279824,#279825),
(#279826,#279827),(#279828,#279829),(#279830,#279831),(#279832,#279833),
(#279834,#279835),(#279836,#279837),(#279838,#279839),(#279840,#279841),
(#279842,#279843),(#279844,#279845),(#279846,#279847),(#279848,#279849),
(#279850,#279851),(#279852,#279853),(#279854,#279855),(#279856,#279857),
(#279858,#279859),(#279860,#279861),(#279862,#279863),(#279864,#279865),
(#279866,#279867),(#279868,#279869),(#279870,#279871),(#279872,#279873),
(#279874,#279875),(#279876,#279877),(#279878,#279879),(#279880,#279881),
(#279882,#279883),(#279884,#279885),(#279886,#279887),(#279888,#279889),
(#279890,#279891),(#279892,#279893),(#279894,#279895),(#279896,#279897),
(#279898,#279899),(#279900,#279901),(#279902,#279903),(#279904,#279905),
(#279906,#279907),(#279908,#279909),(#279910,#279911),(#279912,#279913),
(#279914,#279915),(#279916,#279917),(#279918,#279919),(#279920,#279921),
(#279922,#279923),(#279924,#279925),(#279926,#279927),(#279928,#279929),
(#279930,#279931),(#279932,#279933),(#279934,#279935),(#279936,#279937),
(#279938,#279939),(#279940,#279941),(#279942,#279943),(#279944,#279945),
(#279946,#279947),(#279948,#279949),(#279950,#279951),(#279952,#279953),
(#279954,#279955),(#279956,#279957),(#279958,#279959),(#279960,#279961),
(#279962,#279963),(#279964,#279965),(#279966,#279967),(#279968,#279969),
(#279970,#279971),(#279972,#279973),(#279974,#279975),(#279976,#279977),
(#279978,#279979),(#279980,#279981),(#279982,#279983),(#279984,#279985),
(#279986,#279987),(#279988,#279989),(#279990,#279991),(#279992,#279993),
(#279994,#279995),(#279996,#279997),(#279998,#279999),(#280000,#280001),
(#280002,#280003),(#280004,#280005),(#280006,#280007),(#280008,#280009),
(#280010,#280011),(#280012,#280013),(#280014,#280015),(#280016,#280017),
(#280018,#280019),(#280020,#280021),(#280022,#280023),(#280024,#280025),
(#280026,#280027),(#280028,#280029),(#280030,#280031),(#280032,#280033),
(#280034,#280035),(#280036,#280037),(#280038,#280039),(#280040,#280041),
(#280042,#280043),(#280044,#280045),(#280046,#280047),(#280048,#280049),
(#280050,#280051),(#280052,#280053),(#280054,#280055),(#280056,#280057),
(#280058,#280059),(#280060,#280061),(#280062,#280063),(#280064,#280065),
(#280066,#280067),(#280068,#280069),(#280070,#280071),(#280072,#280073),
(#280074,#280075),(#280076,#280077),(#280078,#280079),(#280080,#280081),
(#280082,#280083),(#280084,#280085),(#280086,#280087),(#280088,#280089),
(#280090,#280091),(#280092,#280093),(#280094,#280095),(#280096,#280097),
(#280098,#280099),(#280100,#280101),(#280102,#280103),(#280104,#280105),
(#280106,#280107),(#280108,#280109),(#280110,#280111),(#280112,#280113),
(#280114,#280115),(#280116,#280117),(#280118,#280119),(#280120,#280121),
(#280122,#280123),(#280124,#280125),(#280126,#280127),(#280128,#280129),
(#280130,#280131),(#280132,#280133),(#280134,#280135),(#280136,#280137),
(#280138,#280139),(#280140,#280141),(#280142,#280143),(#280144,#280145),
(#280146,#280147),(#280148,#280149),(#280150,#280151),(#280152,#280153),
(#280154,#280155),(#280156,#280157),(#280158,#280159),(#280160,#280161),
(#280162,#280163),(#280164,#280165),(#280166,#280167),(#280168,#280169),
(#280170,#280171),(#280172,#280173),(#280174,#280175),(#280176,#280177),
(#280178,#280179),(#280180,#280181),(#280182,#280183),(#280184,#280185),
(#280186,#280187),(#280188,#280189),(#280190,#280191),(#280192,#280193),
(#280194,#280195),(#280196,#280197),(#280198,#280199),(#280200,#280201),
(#280202,#280203),(#280204,#280205),(#280206,#280207),(#280208,#280209),
(#280210,#280211),(#280212,#280213),(#280214,#280215),(#280216,#280217),
(#280218,#280219),(#280220,#280221),(#280222,#280223),(#280224,#280225),
(#280226,#280227),(#280228,#280229),(#280230,#280231),(#280232,#280233),
(#280234,#280235),(#280236,#280237),(#280238,#280239),(#280240,#280241),
(#280242,#280243),(#280244,#280245),(#280246,#280247),(#280248,#280249),
(#280250,#280251),(#280252,#280253),(#280254,#280255),(#280256,#280257),
(#280258,#280259),(#280260,#280261),(#280262,#280263),(#280264,#280265),
(#280266,#280267),(#280268,#280269),(#280270,#280271),(#280272,#280273),
(#280274,#280275),(#280276,#280277),(#280278,#280279),(#280280,#280281),
(#280282,#280283),(#280284,#280285),(#280286,#280287),(#280288,#280289),
(#280290,#280291),(#280292,#280293),(#280294,#280295),(#280296,#280297),
(#280298,#280299),(#280300,#280301),(#280302,#280303),(#280304,#280305),
(#280306,#280307),(#280308,#280309),(#280310,#280311),(#280312,#280313),
(#280314,#280315),(#280316,#280317),(#280318,#280319),(#280320,#280321),
(#280322,#280323),(#280324,#280325),(#280326,#280327),(#280328,#280329),
(#280330,#280331),(#280332,#280333),(#280334,#280335),(#280336,#280337),
(#280338,#280339),(#280340,#280341),(#280342,#280343),(#280344,#280345),
(#280346,#280347),(#280348,#280349),(#280350,#280351),(#280352,#280353),
(#280354,#280355),(#280356,#280357),(#280358,#280359),(#280360,#280361),
(#280362,#280363),(#280364,#280365),(#280366,#280367),(#280368,#280369),
(#280370,#280371),(#280372,#280373),(#280374,#280375),(#280376,#280377),
(#280378,#280379),(#280380,#280381),(#280382,#280383),(#280384,#280385),
(#280386,#280387),(#280388,#280389),(#280390,#280391),(#280392,#280393),
(#280394,#280395),(#280396,#280397),(#280398,#280399),(#280400,#280401),
(#280402,#280403),(#280404,#280405),(#280406,#280407),(#280408,#280409),
(#280410,#280411),(#280412,#280413),(#280414,#280415),(#280416,#280417),
(#280418,#280419),(#280420,#280421),(#280422,#280423),(#280424,#280425),
(#280426,#280427),(#280428,#280429),(#280430,#280431),(#280432,#280433),
(#280434,#280435),(#280436,#280437),(#280438,#280439),(#280440,#280441),
(#280442,#280443),(#280444,#280445),(#280446,#280447),(#280448,#280449),
(#280450,#280451),(#280452,#280453),(#280454,#280455),(#280456,#280457),
(#280458,#280459),(#280460,#280461),(#280462,#280463),(#280464,#280465),
(#280466,#280467),(#280468,#280469),(#280470,#280471),(#280472,#280473),
(#280474,#280475),(#280476,#280477),(#280478,#280479),(#280480,#280481),
(#280482,#280483),(#280484,#280485)),.UNSPECIFIED.,.F.,.F.,.F.,(6,1,1,1,
1,1,1,1,1,1,1,1,1,1,1,1,1,1,1,1,1,1,1,1,1,1,1,1,1,1,1,1,1,1,1,1,1,1,1,1,
1,1,1,1,1,1,1,1,1,1,1,1,1,1,1,1,1,1,1,1,1,1,1,1,1,1,1,1,1,1,1,1,1,1,1,1,
1,1,1,1,1,1,1,1,1,1,1,1,1,1,1,1,1,1,1,1,1,1,1,1,1,1,1,1,1,1,1,1,1,1,1,1,
1,1,1,1,1,1,1,1,1,1,1,1,1,1,1,1,1,1,1,1,1,1,1,1,1,1,1,1,1,1,1,1,1,1,1,1,
1,1,1,1,1,1,1,1,1,1,1,1,1,1,1,1,1,1,1,1,1,1,1,1,1,1,1,1,1,1,1,1,1,1,1,1,
1,1,1,1,1,1,1,1,1,1,1,1,1,1,1,1,1,1,1,1,1,1,1,1,1,1,1,1,1,1,1,1,1,1,1,1,
1,1,1,1,1,1,1,1,1,1,1,1,1,1,1,1,1,1,1,1,1,1,1,1,1,1,1,1,1,1,1,1,1,1,1,1,
1,1,1,1,1,1,1,1,1,1,1,1,1,1,1,1,1,1,1,1,1,1,1,1,1,1,1,1,1,1,1,1,1,1,1,1,
1,1,1,1,1,1,1,1,1,1,1,1,1,1,1,1,1,1,1,1,1,1,1,1,1,1,1,1,1,1,1,1,1,1,1,1,
1,1,1,1,1,1,1,1,1,1,1,1,1,1,1,1,1,1,1,1,1,1,1,1,1,1,1,1,1,1,1,1,1,1,1,1,
1,1,1,1,1,1,1,1,1,1,1,1,1,1,1,1,1,1,1,1,1,1,1,1,1,1,1,1,1,1,1,1,1,1,1,1,
1,1,1,1,1,1,1,1,1,1,1,1,1,1,1,1,1,1,1,1,1,1,1,1,1,1,1,1,1,1,1,1,1,1,1,1,
1,1,1,1,1,1,1,1,1,1,1,1,1,1,1,1,1,1,1,1,1,1,1,1,1,1,1,1,1,1,1,6),(2,2),
(0.143172103,0.144954128,0.146788991,0.148623853,0.150458716,0.152293578,
0.15412844,0.155963303,0.157798165,0.159633028,0.16146789,0.163302752,0.165137615,
0.166972477,0.168807339,0.170642202,0.172477064,0.174311927,0.176146789,
0.177981651,0.179816514,0.181651376,0.183486239,0.185321101,0.187155963,
0.188990826,0.190825688,0.19266055,0.194495413,0.196330275,0.198165138,
0.2,0.201834862,0.203669725,0.205504587,0.20733945,0.209174312,0.211009174,
0.212844037,0.214678899,0.216513761,0.218348624,0.220183486,0.222018349,
0.223853211,0.225688073,0.227522936,0.229357798,0.231192661,0.233027523,
0.234862385,0.236697248,0.23853211,0.240366972,0.242201835,0.244036697,
0.24587156,0.247706422,0.249541284,0.251376147,0.253211009,0.255045872,
0.256880734,0.258715596,0.260550459,0.262385321,0.264220183,0.266055046,
0.267889908,0.269724771,0.271559633,0.273394495,0.275229358,0.27706422,
0.278899083,0.280733945,0.282568807,0.28440367,0.286238532,0.288073394,
0.289908257,0.291743119,0.293577982,0.295412844,0.297247706,0.299082569,
0.300917431,0.302752294,0.304587156,0.306422018,0.308256881,0.310091743,
0.311926606,0.313761468,0.31559633,0.317431193,0.319266055,0.321100917,
0.32293578,0.324770642,0.326605505,0.328440367,0.330275229,0.332110092,
0.333944954,0.335779817,0.337614679,0.339449541,0.341284404,0.343119266,
0.344954128,0.346788991,0.348623853,0.350458716,0.352293578,0.35412844,
0.355963303,0.357798165,0.359633028,0.36146789,0.363302752,0.365137615,
0.366972477,0.368807339,0.370642202,0.372477064,0.374311927,0.376146789,
0.377981651,0.379816514,0.381651376,0.383486239,0.385321101,0.387155963,
0.388990826,0.390825688,0.39266055,0.394495413,0.396330275,0.398165138,
0.4,0.401834862,0.403669725,0.405504587,0.40733945,0.409174312,0.411009174,
0.412844037,0.414678899,0.416513761,0.418348624,0.420183486,0.422018349,
0.423853211,0.425688073,0.427522936,0.429357798,0.431192661,0.433027523,
0.434862385,0.436697248,0.43853211,0.440366972,0.442201835,0.444036697,
0.44587156,0.447706422,0.449541284,0.451376147,0.453211009,0.455045872,
0.456880734,0.458715596,0.460550459,0.462385321,0.464220183,0.466055046,
0.467889908,0.469724771,0.471559633,0.473394495,0.475229358,0.47706422,
0.478899083,0.480733945,0.482568807,0.48440367,0.486238532,0.488073394,
0.489908257,0.491743119,0.493577982,0.495412844,0.497247706,0.499082569,
0.500917431,0.502752294,0.504587156,0.506422018,0.508256881,0.510091743,
0.511926606,0.513761468,0.51559633,0.517431193,0.519266055,0.521100917,
0.52293578,0.524770642,0.526605505,0.528440367,0.530275229,0.532110092,
0.533944954,0.535779817,0.537614679,0.539449541,0.541284404,0.543119266,
0.544954128,0.546788991,0.548623853,0.550458716,0.552293578,0.55412844,
0.555963303,0.557798165,0.559633028,0.56146789,0.563302752,0.565137615,
0.566972477,0.568807339,0.570642202,0.572477064,0.574311927,0.576146789,
0.577981651,0.579816514,0.581651376,0.583486239,0.585321101,0.587155963,
0.588990826,0.590825688,0.59266055,0.594495413,0.596330275,0.598165138,
0.6,0.601834862,0.603669725,0.605504587,0.60733945,0.609174312,0.611009174,
0.612844037,0.614678899,0.616513761,0.618348624,0.620183486,0.622018349,
0.623853211,0.625688073,0.627522936,0.629357798,0.631192661,0.633027523,
0.634862385,0.636697248,0.63853211,0.640366972,0.642201835,0.644036697,
0.64587156,0.647706422,0.649541284,0.651376147,0.653211009,0.655045872,
0.656880734,0.658715596,0.660550459,0.662385321,0.664220183,0.666055046,
0.667889908,0.669724771,0.671559633,0.673394495,0.675229358,0.67706422,
0.678899083,0.680733945,0.682568807,0.68440367,0.686238532,0.688073394,
0.689908257,0.691743119,0.693577982,0.695412844,0.697247706,0.699082569,
0.700917431,0.702752294,0.704587156,0.706422018,0.708256881,0.710091743,
0.711926606,0.713761468,0.71559633,0.717431193,0.719266055,0.721100917,
0.72293578,0.724770642,0.726605505,0.728440367,0.730275229,0.732110092,
0.733944954,0.735779817,0.737614679,0.739449541,0.741284404,0.743119266,
0.744954128,0.746788991,0.748623853,0.750458716,0.752293578,0.75412844,
0.755963303,0.757798165,0.759633028,0.76146789,0.763302752,0.765137615,
0.766972477,0.768807339,0.770642202,0.772477064,0.774311927,0.776146789,
0.777981651,0.779816514,0.781651376,0.783486239,0.785321101,0.787155963,
0.788990826,0.790825688,0.79266055,0.794495413,0.796330275,0.798165138,
0.8,0.801834862,0.803669725,0.805504587,0.80733945,0.809174312,0.811009174,
0.812844037,0.814678899,0.816513761,0.818348624,0.820183486,0.822018349,
0.823853211,0.825688073,0.827522936,0.829357798,0.831192661,0.833027523,
0.834862385,0.836697248,0.83853211,0.840366972,0.842201835,0.844036697,
0.84587156,0.847706422,0.849541284,0.851376147,0.853211009,0.855045872,
0.856880734,0.858715596,0.860550459,0.862385321,0.864220183,0.866055046,
0.867889908,0.869724771,0.871559633,0.873394495,0.875229358,0.87706422,
0.878899083,0.880733945,0.882568807,0.88440367,0.886238532,0.888073394,
0.889908257,0.891743119,0.893577982,0.895412844,0.897247706,0.899082569,
0.900917431,0.902752294,0.904587156,0.906422018,0.908256881,0.910091743,
0.911926606,0.913761468,0.91559633,0.917431193,0.919266055,0.921100917,
0.92293578,0.924770642,0.926605505,0.928440367,0.930275229,0.932110092,
0.933944954,0.935779817,0.937614679,0.939449541,0.941284404,0.943119266,
0.944954128,0.946788991,0.948623853,0.950458716,0.952293578,0.95412844,
0.955963303,0.957798165,0.959633028,0.96146789,0.963302752,0.965137615,
0.966972477,0.968807339,0.970642202,0.972477064,0.974311927,0.976146789,
0.977981651,0.979816514,0.981651376,0.983486239,0.985321101,0.987155963,
0.988990826,0.990825688,0.99266055,0.994495413,0.996330275,0.998165138,
1.),(0.,0.36),.UNSPECIFIED.);
#6292=B_SPLINE_SURFACE_WITH_KNOTS('',5,1,((#281133,#281134),(#281135,#281136),
(#281137,#281138),(#281139,#281140),(#281141,#281142),(#281143,#281144),
(#281145,#281146),(#281147,#281148),(#281149,#281150),(#281151,#281152),
(#281153,#281154),(#281155,#281156),(#281157,#281158),(#281159,#281160),
(#281161,#281162),(#281163,#281164),(#281165,#281166),(#281167,#281168),
(#281169,#281170),(#281171,#281172),(#281173,#281174),(#281175,#281176),
(#281177,#281178),(#281179,#281180),(#281181,#281182),(#281183,#281184),
(#281185,#281186),(#281187,#281188),(#281189,#281190),(#281191,#281192),
(#281193,#281194),(#281195,#281196),(#281197,#281198),(#281199,#281200),
(#281201,#281202),(#281203,#281204),(#281205,#281206),(#281207,#281208),
(#281209,#281210),(#281211,#281212),(#281213,#281214),(#281215,#281216),
(#281217,#281218),(#281219,#281220),(#281221,#281222),(#281223,#281224),
(#281225,#281226),(#281227,#281228),(#281229,#281230),(#281231,#281232),
(#281233,#281234),(#281235,#281236),(#281237,#281238),(#281239,#281240),
(#281241,#281242),(#281243,#281244),(#281245,#281246),(#281247,#281248),
(#281249,#281250),(#281251,#281252),(#281253,#281254),(#281255,#281256),
(#281257,#281258),(#281259,#281260),(#281261,#281262),(#281263,#281264),
(#281265,#281266),(#281267,#281268),(#281269,#281270),(#281271,#281272),
(#281273,#281274),(#281275,#281276),(#281277,#281278),(#281279,#281280),
(#281281,#281282),(#281283,#281284),(#281285,#281286),(#281287,#281288),
(#281289,#281290),(#281291,#281292),(#281293,#281294),(#281295,#281296),
(#281297,#281298),(#281299,#281300),(#281301,#281302),(#281303,#281304),
(#281305,#281306),(#281307,#281308),(#281309,#281310),(#281311,#281312),
(#281313,#281314),(#281315,#281316),(#281317,#281318),(#281319,#281320),
(#281321,#281322),(#281323,#281324),(#281325,#281326),(#281327,#281328),
(#281329,#281330),(#281331,#281332),(#281333,#281334),(#281335,#281336),
(#281337,#281338),(#281339,#281340),(#281341,#281342),(#281343,#281344),
(#281345,#281346),(#281347,#281348),(#281349,#281350),(#281351,#281352),
(#281353,#281354),(#281355,#281356),(#281357,#281358),(#281359,#281360),
(#281361,#281362),(#281363,#281364),(#281365,#281366),(#281367,#281368),
(#281369,#281370),(#281371,#281372),(#281373,#281374),(#281375,#281376),
(#281377,#281378),(#281379,#281380),(#281381,#281382),(#281383,#281384),
(#281385,#281386),(#281387,#281388),(#281389,#281390),(#281391,#281392),
(#281393,#281394),(#281395,#281396),(#281397,#281398),(#281399,#281400),
(#281401,#281402),(#281403,#281404),(#281405,#281406),(#281407,#281408),
(#281409,#281410),(#281411,#281412),(#281413,#281414),(#281415,#281416),
(#281417,#281418),(#281419,#281420),(#281421,#281422),(#281423,#281424),
(#281425,#281426),(#281427,#281428),(#281429,#281430),(#281431,#281432),
(#281433,#281434),(#281435,#281436),(#281437,#281438),(#281439,#281440),
(#281441,#281442),(#281443,#281444),(#281445,#281446),(#281447,#281448),
(#281449,#281450),(#281451,#281452),(#281453,#281454),(#281455,#281456),
(#281457,#281458),(#281459,#281460),(#281461,#281462),(#281463,#281464),
(#281465,#281466),(#281467,#281468),(#281469,#281470),(#281471,#281472),
(#281473,#281474),(#281475,#281476),(#281477,#281478),(#281479,#281480),
(#281481,#281482),(#281483,#281484),(#281485,#281486),(#281487,#281488),
(#281489,#281490),(#281491,#281492),(#281493,#281494),(#281495,#281496),
(#281497,#281498),(#281499,#281500),(#281501,#281502),(#281503,#281504),
(#281505,#281506),(#281507,#281508),(#281509,#281510),(#281511,#281512),
(#281513,#281514),(#281515,#281516),(#281517,#281518),(#281519,#281520),
(#281521,#281522),(#281523,#281524),(#281525,#281526),(#281527,#281528),
(#281529,#281530),(#281531,#281532),(#281533,#281534),(#281535,#281536),
(#281537,#281538),(#281539,#281540),(#281541,#281542),(#281543,#281544),
(#281545,#281546),(#281547,#281548),(#281549,#281550),(#281551,#281552),
(#281553,#281554),(#281555,#281556),(#281557,#281558),(#281559,#281560),
(#281561,#281562),(#281563,#281564),(#281565,#281566),(#281567,#281568),
(#281569,#281570),(#281571,#281572),(#281573,#281574),(#281575,#281576),
(#281577,#281578),(#281579,#281580),(#281581,#281582),(#281583,#281584),
(#281585,#281586),(#281587,#281588),(#281589,#281590),(#281591,#281592),
(#281593,#281594),(#281595,#281596),(#281597,#281598),(#281599,#281600),
(#281601,#281602),(#281603,#281604),(#281605,#281606),(#281607,#281608),
(#281609,#281610),(#281611,#281612),(#281613,#281614),(#281615,#281616),
(#281617,#281618),(#281619,#281620),(#281621,#281622),(#281623,#281624),
(#281625,#281626),(#281627,#281628),(#281629,#281630),(#281631,#281632),
(#281633,#281634),(#281635,#281636),(#281637,#281638),(#281639,#281640),
(#281641,#281642),(#281643,#281644),(#281645,#281646),(#281647,#281648),
(#281649,#281650),(#281651,#281652),(#281653,#281654),(#281655,#281656),
(#281657,#281658),(#281659,#281660),(#281661,#281662),(#281663,#281664),
(#281665,#281666),(#281667,#281668),(#281669,#281670),(#281671,#281672),
(#281673,#281674),(#281675,#281676),(#281677,#281678),(#281679,#281680),
(#281681,#281682),(#281683,#281684),(#281685,#281686),(#281687,#281688),
(#281689,#281690),(#281691,#281692),(#281693,#281694),(#281695,#281696),
(#281697,#281698),(#281699,#281700),(#281701,#281702),(#281703,#281704),
(#281705,#281706),(#281707,#281708),(#281709,#281710),(#281711,#281712),
(#281713,#281714),(#281715,#281716),(#281717,#281718),(#281719,#281720),
(#281721,#281722),(#281723,#281724),(#281725,#281726),(#281727,#281728),
(#281729,#281730),(#281731,#281732),(#281733,#281734),(#281735,#281736),
(#281737,#281738),(#281739,#281740),(#281741,#281742),(#281743,#281744),
(#281745,#281746),(#281747,#281748),(#281749,#281750),(#281751,#281752),
(#281753,#281754),(#281755,#281756),(#281757,#281758),(#281759,#281760),
(#281761,#281762),(#281763,#281764),(#281765,#281766),(#281767,#281768),
(#281769,#281770),(#281771,#281772),(#281773,#281774),(#281775,#281776),
(#281777,#281778),(#281779,#281780),(#281781,#281782),(#281783,#281784),
(#281785,#281786),(#281787,#281788),(#281789,#281790),(#281791,#281792),
(#281793,#281794),(#281795,#281796),(#281797,#281798),(#281799,#281800),
(#281801,#281802),(#281803,#281804),(#281805,#281806),(#281807,#281808),
(#281809,#281810),(#281811,#281812),(#281813,#281814),(#281815,#281816),
(#281817,#281818),(#281819,#281820),(#281821,#281822),(#281823,#281824),
(#281825,#281826),(#281827,#281828),(#281829,#281830),(#281831,#281832),
(#281833,#281834),(#281835,#281836),(#281837,#281838),(#281839,#281840),
(#281841,#281842),(#281843,#281844),(#281845,#281846),(#281847,#281848),
(#281849,#281850),(#281851,#281852),(#281853,#281854),(#281855,#281856),
(#281857,#281858),(#281859,#281860),(#281861,#281862),(#281863,#281864),
(#281865,#281866),(#281867,#281868),(#281869,#281870),(#281871,#281872),
(#281873,#281874),(#281875,#281876),(#281877,#281878),(#281879,#281880),
(#281881,#281882),(#281883,#281884),(#281885,#281886),(#281887,#281888),
(#281889,#281890),(#281891,#281892),(#281893,#281894),(#281895,#281896),
(#281897,#281898),(#281899,#281900),(#281901,#281902),(#281903,#281904),
(#281905,#281906),(#281907,#281908),(#281909,#281910),(#281911,#281912),
(#281913,#281914),(#281915,#281916),(#281917,#281918),(#281919,#281920),
(#281921,#281922),(#281923,#281924),(#281925,#281926),(#281927,#281928),
(#281929,#281930),(#281931,#281932),(#281933,#281934),(#281935,#281936),
(#281937,#281938),(#281939,#281940),(#281941,#281942),(#281943,#281944),
(#281945,#281946),(#281947,#281948),(#281949,#281950),(#281951,#281952),
(#281953,#281954),(#281955,#281956),(#281957,#281958),(#281959,#281960),
(#281961,#281962),(#281963,#281964),(#281965,#281966),(#281967,#281968),
(#281969,#281970),(#281971,#281972),(#281973,#281974),(#281975,#281976),
(#281977,#281978),(#281979,#281980),(#281981,#281982),(#281983,#281984),
(#281985,#281986),(#281987,#281988),(#281989,#281990),(#281991,#281992),
(#281993,#281994),(#281995,#281996),(#281997,#281998),(#281999,#282000),
(#282001,#282002),(#282003,#282004),(#282005,#282006),(#282007,#282008),
(#282009,#282010),(#282011,#282012),(#282013,#282014),(#282015,#282016),
(#282017,#282018),(#282019,#282020),(#282021,#282022),(#282023,#282024),
(#282025,#282026),(#282027,#282028),(#282029,#282030),(#282031,#282032),
(#282033,#282034),(#282035,#282036),(#282037,#282038),(#282039,#282040),
(#282041,#282042),(#282043,#282044),(#282045,#282046),(#282047,#282048),
(#282049,#282050),(#282051,#282052),(#282053,#282054),(#282055,#282056),
(#282057,#282058),(#282059,#282060),(#282061,#282062),(#282063,#282064),
(#282065,#282066),(#282067,#282068),(#282069,#282070),(#282071,#282072),
(#282073,#282074),(#282075,#282076)),.UNSPECIFIED.,.F.,.F.,.F.,(6,1,1,1,
1,1,1,1,1,1,1,1,1,1,1,1,1,1,1,1,1,1,1,1,1,1,1,1,1,1,1,1,1,1,1,1,1,1,1,1,
1,1,1,1,1,1,1,1,1,1,1,1,1,1,1,1,1,1,1,1,1,1,1,1,1,1,1,1,1,1,1,1,1,1,1,1,
1,1,1,1,1,1,1,1,1,1,1,1,1,1,1,1,1,1,1,1,1,1,1,1,1,1,1,1,1,1,1,1,1,1,1,1,
1,1,1,1,1,1,1,1,1,1,1,1,1,1,1,1,1,1,1,1,1,1,1,1,1,1,1,1,1,1,1,1,1,1,1,1,
1,1,1,1,1,1,1,1,1,1,1,1,1,1,1,1,1,1,1,1,1,1,1,1,1,1,1,1,1,1,1,1,1,1,1,1,
1,1,1,1,1,1,1,1,1,1,1,1,1,1,1,1,1,1,1,1,1,1,1,1,1,1,1,1,1,1,1,1,1,1,1,1,
1,1,1,1,1,1,1,1,1,1,1,1,1,1,1,1,1,1,1,1,1,1,1,1,1,1,1,1,1,1,1,1,1,1,1,1,
1,1,1,1,1,1,1,1,1,1,1,1,1,1,1,1,1,1,1,1,1,1,1,1,1,1,1,1,1,1,1,1,1,1,1,1,
1,1,1,1,1,1,1,1,1,1,1,1,1,1,1,1,1,1,1,1,1,1,1,1,1,1,1,1,1,1,1,1,1,1,1,1,
1,1,1,1,1,1,1,1,1,1,1,1,1,1,1,1,1,1,1,1,1,1,1,1,1,1,1,1,1,1,1,1,1,1,1,1,
1,1,1,1,1,1,1,1,1,1,1,1,1,1,1,1,1,1,1,1,1,1,1,1,1,1,1,1,1,1,1,1,1,1,1,1,
1,1,1,1,1,1,1,1,1,1,1,1,1,1,1,1,1,1,1,1,1,1,1,1,1,1,1,1,1,1,1,1,1,1,1,1,
1,1,1,1,1,1,1,1,1,1,1,1,1,1,1,1,1,1,1,1,1,1,1,1,1,1,1,1,1,1,1,6),(2,2),
(-1.,-0.998165138,-0.996330275,-0.994495413,-0.99266055,-0.990825688,-0.988990826,
-0.987155963,-0.985321101,-0.983486239,-0.981651376,-0.979816514,-0.977981651,
-0.976146789,-0.974311927,-0.972477064,-0.970642202,-0.968807339,-0.966972477,
-0.965137615,-0.963302752,-0.96146789,-0.959633028,-0.957798165,-0.955963303,
-0.95412844,-0.952293578,-0.950458716,-0.948623853,-0.946788991,-0.944954128,
-0.943119266,-0.941284404,-0.939449541,-0.937614679,-0.935779817,-0.933944954,
-0.932110092,-0.930275229,-0.928440367,-0.926605505,-0.924770642,-0.92293578,
-0.921100917,-0.919266055,-0.917431193,-0.91559633,-0.913761468,-0.911926606,
-0.910091743,-0.908256881,-0.906422018,-0.904587156,-0.902752294,-0.900917431,
-0.899082569,-0.897247706,-0.895412844,-0.893577982,-0.891743119,-0.889908257,
-0.888073394,-0.886238532,-0.88440367,-0.882568807,-0.880733945,-0.878899083,
-0.87706422,-0.875229358,-0.873394495,-0.871559633,-0.869724771,-0.867889908,
-0.866055046,-0.864220183,-0.862385321,-0.860550459,-0.858715596,-0.856880734,
-0.855045872,-0.853211009,-0.851376147,-0.849541284,-0.847706422,-0.84587156,
-0.844036697,-0.842201835,-0.840366972,-0.83853211,-0.836697248,-0.834862385,
-0.833027523,-0.831192661,-0.829357798,-0.827522936,-0.825688073,-0.823853211,
-0.822018349,-0.820183486,-0.818348624,-0.816513761,-0.814678899,-0.812844037,
-0.811009174,-0.809174312,-0.80733945,-0.805504587,-0.803669725,-0.801834862,
-0.8,-0.798165138,-0.796330275,-0.794495413,-0.79266055,-0.790825688,-0.788990826,
-0.787155963,-0.785321101,-0.783486239,-0.781651376,-0.779816514,-0.777981651,
-0.776146789,-0.774311927,-0.772477064,-0.770642202,-0.768807339,-0.766972477,
-0.765137615,-0.763302752,-0.76146789,-0.759633028,-0.757798165,-0.755963303,
-0.75412844,-0.752293578,-0.750458716,-0.748623853,-0.746788991,-0.744954128,
-0.743119266,-0.741284404,-0.739449541,-0.737614679,-0.735779817,-0.733944954,
-0.732110092,-0.730275229,-0.728440367,-0.726605505,-0.724770642,-0.72293578,
-0.721100917,-0.719266055,-0.717431193,-0.71559633,-0.713761468,-0.711926606,
-0.710091743,-0.708256881,-0.706422018,-0.704587156,-0.702752294,-0.700917431,
-0.699082569,-0.697247706,-0.695412844,-0.693577982,-0.691743119,-0.689908257,
-0.688073394,-0.686238532,-0.68440367,-0.682568807,-0.680733945,-0.678899083,
-0.67706422,-0.675229358,-0.673394495,-0.671559633,-0.669724771,-0.667889908,
-0.666055046,-0.664220183,-0.662385321,-0.660550459,-0.658715596,-0.656880734,
-0.655045872,-0.653211009,-0.651376147,-0.649541284,-0.647706422,-0.64587156,
-0.644036697,-0.642201835,-0.640366972,-0.63853211,-0.636697248,-0.634862385,
-0.633027523,-0.631192661,-0.629357798,-0.627522936,-0.625688073,-0.623853211,
-0.622018349,-0.620183486,-0.618348624,-0.616513761,-0.614678899,-0.612844037,
-0.611009174,-0.609174312,-0.60733945,-0.605504587,-0.603669725,-0.601834862,
-0.6,-0.598165138,-0.596330275,-0.594495413,-0.59266055,-0.590825688,-0.588990826,
-0.587155963,-0.585321101,-0.583486239,-0.581651376,-0.579816514,-0.577981651,
-0.576146789,-0.574311927,-0.572477064,-0.570642202,-0.568807339,-0.566972477,
-0.565137615,-0.563302752,-0.56146789,-0.559633028,-0.557798165,-0.555963303,
-0.55412844,-0.552293578,-0.550458716,-0.548623853,-0.546788991,-0.544954128,
-0.543119266,-0.541284404,-0.539449541,-0.537614679,-0.535779817,-0.533944954,
-0.532110092,-0.530275229,-0.528440367,-0.526605505,-0.524770642,-0.52293578,
-0.521100917,-0.519266055,-0.517431193,-0.51559633,-0.513761468,-0.511926606,
-0.510091743,-0.508256881,-0.506422018,-0.504587156,-0.502752294,-0.500917431,
-0.499082569,-0.497247706,-0.495412844,-0.493577982,-0.491743119,-0.489908257,
-0.488073394,-0.486238532,-0.48440367,-0.482568807,-0.480733945,-0.478899083,
-0.47706422,-0.475229358,-0.473394495,-0.471559633,-0.469724771,-0.467889908,
-0.466055046,-0.464220183,-0.462385321,-0.460550459,-0.458715596,-0.456880734,
-0.455045872,-0.453211009,-0.451376147,-0.449541284,-0.447706422,-0.44587156,
-0.444036697,-0.442201835,-0.440366972,-0.43853211,-0.436697248,-0.434862385,
-0.433027523,-0.431192661,-0.429357798,-0.427522936,-0.425688073,-0.423853211,
-0.422018349,-0.420183486,-0.418348624,-0.416513761,-0.414678899,-0.412844037,
-0.411009174,-0.409174312,-0.40733945,-0.405504587,-0.403669725,-0.401834862,
-0.4,-0.398165138,-0.396330275,-0.394495413,-0.39266055,-0.390825688,-0.388990826,
-0.387155963,-0.385321101,-0.383486239,-0.381651376,-0.379816514,-0.377981651,
-0.376146789,-0.374311927,-0.372477064,-0.370642202,-0.368807339,-0.366972477,
-0.365137615,-0.363302752,-0.36146789,-0.359633028,-0.357798165,-0.355963303,
-0.35412844,-0.352293578,-0.350458716,-0.348623853,-0.346788991,-0.344954128,
-0.343119266,-0.341284404,-0.339449541,-0.337614679,-0.335779817,-0.333944954,
-0.332110092,-0.330275229,-0.328440367,-0.326605505,-0.324770642,-0.32293578,
-0.321100917,-0.319266055,-0.317431193,-0.31559633,-0.313761468,-0.311926606,
-0.310091743,-0.308256881,-0.306422018,-0.304587156,-0.302752294,-0.300917431,
-0.299082569,-0.297247706,-0.295412844,-0.293577982,-0.291743119,-0.289908257,
-0.288073394,-0.286238532,-0.28440367,-0.282568807,-0.280733945,-0.278899083,
-0.27706422,-0.275229358,-0.273394495,-0.271559633,-0.269724771,-0.267889908,
-0.266055046,-0.264220183,-0.262385321,-0.260550459,-0.258715596,-0.256880734,
-0.255045872,-0.253211009,-0.251376147,-0.249541284,-0.247706422,-0.24587156,
-0.244036697,-0.242201835,-0.240366972,-0.23853211,-0.236697248,-0.234862385,
-0.233027523,-0.231192661,-0.229357798,-0.227522936,-0.225688073,-0.223853211,
-0.222018349,-0.220183486,-0.218348624,-0.216513761,-0.214678899,-0.212844037,
-0.211009174,-0.209174312,-0.20733945,-0.205504587,-0.203669725,-0.201834862,
-0.2,-0.198165138,-0.196330275,-0.194495413,-0.19266055,-0.190825688,-0.188990826,
-0.187155963,-0.185321101,-0.183486239,-0.181651376,-0.179816514,-0.177981651,
-0.176146789,-0.174311927,-0.172477064,-0.170642202,-0.168807339,-0.166972477,
-0.165137615,-0.163302752,-0.16146789,-0.159633028,-0.157798165,-0.155963303,
-0.15412844,-0.152293578,-0.150458716,-0.148623853,-0.146788991,-0.144954128,
-0.143172103),(0.,0.36),.UNSPECIFIED.);
#6293=B_SPLINE_SURFACE_WITH_KNOTS('',5,1,((#282751,#282752),(#282753,#282754),
(#282755,#282756),(#282757,#282758),(#282759,#282760),(#282761,#282762),
(#282763,#282764),(#282765,#282766),(#282767,#282768),(#282769,#282770),
(#282771,#282772),(#282773,#282774),(#282775,#282776),(#282777,#282778),
(#282779,#282780),(#282781,#282782),(#282783,#282784),(#282785,#282786),
(#282787,#282788),(#282789,#282790),(#282791,#282792),(#282793,#282794),
(#282795,#282796),(#282797,#282798),(#282799,#282800),(#282801,#282802),
(#282803,#282804),(#282805,#282806),(#282807,#282808),(#282809,#282810),
(#282811,#282812),(#282813,#282814),(#282815,#282816),(#282817,#282818),
(#282819,#282820),(#282821,#282822),(#282823,#282824),(#282825,#282826),
(#282827,#282828),(#282829,#282830),(#282831,#282832),(#282833,#282834),
(#282835,#282836),(#282837,#282838),(#282839,#282840),(#282841,#282842),
(#282843,#282844),(#282845,#282846),(#282847,#282848),(#282849,#282850),
(#282851,#282852),(#282853,#282854),(#282855,#282856),(#282857,#282858),
(#282859,#282860),(#282861,#282862),(#282863,#282864),(#282865,#282866),
(#282867,#282868),(#282869,#282870),(#282871,#282872),(#282873,#282874),
(#282875,#282876),(#282877,#282878),(#282879,#282880),(#282881,#282882),
(#282883,#282884),(#282885,#282886),(#282887,#282888),(#282889,#282890),
(#282891,#282892),(#282893,#282894),(#282895,#282896),(#282897,#282898),
(#282899,#282900),(#282901,#282902),(#282903,#282904),(#282905,#282906),
(#282907,#282908),(#282909,#282910),(#282911,#282912),(#282913,#282914),
(#282915,#282916),(#282917,#282918),(#282919,#282920),(#282921,#282922),
(#282923,#282924),(#282925,#282926),(#282927,#282928),(#282929,#282930),
(#282931,#282932),(#282933,#282934),(#282935,#282936),(#282937,#282938),
(#282939,#282940),(#282941,#282942),(#282943,#282944),(#282945,#282946),
(#282947,#282948),(#282949,#282950),(#282951,#282952),(#282953,#282954),
(#282955,#282956),(#282957,#282958),(#282959,#282960),(#282961,#282962),
(#282963,#282964),(#282965,#282966),(#282967,#282968),(#282969,#282970),
(#282971,#282972),(#282973,#282974),(#282975,#282976),(#282977,#282978),
(#282979,#282980),(#282981,#282982),(#282983,#282984),(#282985,#282986),
(#282987,#282988),(#282989,#282990),(#282991,#282992),(#282993,#282994),
(#282995,#282996),(#282997,#282998),(#282999,#283000),(#283001,#283002),
(#283003,#283004),(#283005,#283006),(#283007,#283008),(#283009,#283010),
(#283011,#283012),(#283013,#283014),(#283015,#283016),(#283017,#283018),
(#283019,#283020),(#283021,#283022),(#283023,#283024),(#283025,#283026),
(#283027,#283028),(#283029,#283030),(#283031,#283032),(#283033,#283034),
(#283035,#283036),(#283037,#283038),(#283039,#283040),(#283041,#283042),
(#283043,#283044),(#283045,#283046),(#283047,#283048),(#283049,#283050),
(#283051,#283052),(#283053,#283054),(#283055,#283056),(#283057,#283058),
(#283059,#283060),(#283061,#283062),(#283063,#283064),(#283065,#283066),
(#283067,#283068),(#283069,#283070),(#283071,#283072),(#283073,#283074),
(#283075,#283076),(#283077,#283078),(#283079,#283080),(#283081,#283082),
(#283083,#283084),(#283085,#283086),(#283087,#283088),(#283089,#283090),
(#283091,#283092),(#283093,#283094),(#283095,#283096),(#283097,#283098),
(#283099,#283100),(#283101,#283102),(#283103,#283104),(#283105,#283106),
(#283107,#283108),(#283109,#283110),(#283111,#283112),(#283113,#283114),
(#283115,#283116),(#283117,#283118),(#283119,#283120),(#283121,#283122),
(#283123,#283124),(#283125,#283126),(#283127,#283128),(#283129,#283130),
(#283131,#283132),(#283133,#283134),(#283135,#283136),(#283137,#283138),
(#283139,#283140),(#283141,#283142),(#283143,#283144),(#283145,#283146),
(#283147,#283148),(#283149,#283150),(#283151,#283152),(#283153,#283154),
(#283155,#283156),(#283157,#283158),(#283159,#283160),(#283161,#283162),
(#283163,#283164),(#283165,#283166),(#283167,#283168),(#283169,#283170),
(#283171,#283172),(#283173,#283174),(#283175,#283176),(#283177,#283178),
(#283179,#283180),(#283181,#283182),(#283183,#283184),(#283185,#283186),
(#283187,#283188),(#283189,#283190),(#283191,#283192),(#283193,#283194),
(#283195,#283196),(#283197,#283198),(#283199,#283200),(#283201,#283202),
(#283203,#283204),(#283205,#283206),(#283207,#283208),(#283209,#283210),
(#283211,#283212),(#283213,#283214),(#283215,#283216),(#283217,#283218),
(#283219,#283220),(#283221,#283222),(#283223,#283224),(#283225,#283226),
(#283227,#283228),(#283229,#283230),(#283231,#283232),(#283233,#283234),
(#283235,#283236),(#283237,#283238),(#283239,#283240),(#283241,#283242),
(#283243,#283244),(#283245,#283246),(#283247,#283248),(#283249,#283250),
(#283251,#283252),(#283253,#283254),(#283255,#283256),(#283257,#283258),
(#283259,#283260),(#283261,#283262),(#283263,#283264),(#283265,#283266),
(#283267,#283268),(#283269,#283270),(#283271,#283272),(#283273,#283274),
(#283275,#283276),(#283277,#283278),(#283279,#283280),(#283281,#283282),
(#283283,#283284),(#283285,#283286),(#283287,#283288),(#283289,#283290),
(#283291,#283292),(#283293,#283294),(#283295,#283296),(#283297,#283298),
(#283299,#283300),(#283301,#283302),(#283303,#283304),(#283305,#283306),
(#283307,#283308),(#283309,#283310),(#283311,#283312),(#283313,#283314),
(#283315,#283316),(#283317,#283318),(#283319,#283320),(#283321,#283322),
(#283323,#283324),(#283325,#283326),(#283327,#283328),(#283329,#283330),
(#283331,#283332),(#283333,#283334),(#283335,#283336),(#283337,#283338),
(#283339,#283340),(#283341,#283342),(#283343,#283344),(#283345,#283346),
(#283347,#283348),(#283349,#283350),(#283351,#283352),(#283353,#283354),
(#283355,#283356),(#283357,#283358),(#283359,#283360),(#283361,#283362),
(#283363,#283364),(#283365,#283366),(#283367,#283368),(#283369,#283370),
(#283371,#283372),(#283373,#283374),(#283375,#283376),(#283377,#283378),
(#283379,#283380),(#283381,#283382),(#283383,#283384),(#283385,#283386),
(#283387,#283388),(#283389,#283390),(#283391,#283392),(#283393,#283394),
(#283395,#283396),(#283397,#283398),(#283399,#283400),(#283401,#283402),
(#283403,#283404),(#283405,#283406),(#283407,#283408),(#283409,#283410),
(#283411,#283412),(#283413,#283414),(#283415,#283416),(#283417,#283418),
(#283419,#283420),(#283421,#283422),(#283423,#283424),(#283425,#283426),
(#283427,#283428),(#283429,#283430),(#283431,#283432),(#283433,#283434),
(#283435,#283436),(#283437,#283438),(#283439,#283440),(#283441,#283442),
(#283443,#283444),(#283445,#283446),(#283447,#283448),(#283449,#283450),
(#283451,#283452),(#283453,#283454),(#283455,#283456),(#283457,#283458),
(#283459,#283460),(#283461,#283462),(#283463,#283464),(#283465,#283466),
(#283467,#283468),(#283469,#283470),(#283471,#283472),(#283473,#283474),
(#283475,#283476),(#283477,#283478),(#283479,#283480),(#283481,#283482),
(#283483,#283484),(#283485,#283486),(#283487,#283488),(#283489,#283490),
(#283491,#283492),(#283493,#283494),(#283495,#283496),(#283497,#283498),
(#283499,#283500),(#283501,#283502),(#283503,#283504),(#283505,#283506),
(#283507,#283508),(#283509,#283510),(#283511,#283512),(#283513,#283514),
(#283515,#283516),(#283517,#283518),(#283519,#283520),(#283521,#283522),
(#283523,#283524),(#283525,#283526),(#283527,#283528),(#283529,#283530),
(#283531,#283532),(#283533,#283534),(#283535,#283536),(#283537,#283538),
(#283539,#283540),(#283541,#283542),(#283543,#283544),(#283545,#283546),
(#283547,#283548),(#283549,#283550),(#283551,#283552),(#283553,#283554),
(#283555,#283556),(#283557,#283558),(#283559,#283560),(#283561,#283562),
(#283563,#283564),(#283565,#283566),(#283567,#283568),(#283569,#283570),
(#283571,#283572),(#283573,#283574),(#283575,#283576),(#283577,#283578),
(#283579,#283580),(#283581,#283582),(#283583,#283584),(#283585,#283586),
(#283587,#283588),(#283589,#283590),(#283591,#283592),(#283593,#283594),
(#283595,#283596),(#283597,#283598),(#283599,#283600),(#283601,#283602),
(#283603,#283604),(#283605,#283606),(#283607,#283608),(#283609,#283610),
(#283611,#283612),(#283613,#283614),(#283615,#283616),(#283617,#283618),
(#283619,#283620),(#283621,#283622),(#283623,#283624),(#283625,#283626),
(#283627,#283628),(#283629,#283630),(#283631,#283632),(#283633,#283634),
(#283635,#283636),(#283637,#283638),(#283639,#283640),(#283641,#283642),
(#283643,#283644),(#283645,#283646),(#283647,#283648),(#283649,#283650),
(#283651,#283652),(#283653,#283654),(#283655,#283656),(#283657,#283658),
(#283659,#283660),(#283661,#283662),(#283663,#283664),(#283665,#283666),
(#283667,#283668),(#283669,#283670),(#283671,#283672),(#283673,#283674),
(#283675,#283676),(#283677,#283678),(#283679,#283680),(#283681,#283682),
(#283683,#283684),(#283685,#283686),(#283687,#283688),(#283689,#283690),
(#283691,#283692),(#283693,#283694)),.UNSPECIFIED.,.F.,.F.,.F.,(6,1,1,1,
1,1,1,1,1,1,1,1,1,1,1,1,1,1,1,1,1,1,1,1,1,1,1,1,1,1,1,1,1,1,1,1,1,1,1,1,
1,1,1,1,1,1,1,1,1,1,1,1,1,1,1,1,1,1,1,1,1,1,1,1,1,1,1,1,1,1,1,1,1,1,1,1,
1,1,1,1,1,1,1,1,1,1,1,1,1,1,1,1,1,1,1,1,1,1,1,1,1,1,1,1,1,1,1,1,1,1,1,1,
1,1,1,1,1,1,1,1,1,1,1,1,1,1,1,1,1,1,1,1,1,1,1,1,1,1,1,1,1,1,1,1,1,1,1,1,
1,1,1,1,1,1,1,1,1,1,1,1,1,1,1,1,1,1,1,1,1,1,1,1,1,1,1,1,1,1,1,1,1,1,1,1,
1,1,1,1,1,1,1,1,1,1,1,1,1,1,1,1,1,1,1,1,1,1,1,1,1,1,1,1,1,1,1,1,1,1,1,1,
1,1,1,1,1,1,1,1,1,1,1,1,1,1,1,1,1,1,1,1,1,1,1,1,1,1,1,1,1,1,1,1,1,1,1,1,
1,1,1,1,1,1,1,1,1,1,1,1,1,1,1,1,1,1,1,1,1,1,1,1,1,1,1,1,1,1,1,1,1,1,1,1,
1,1,1,1,1,1,1,1,1,1,1,1,1,1,1,1,1,1,1,1,1,1,1,1,1,1,1,1,1,1,1,1,1,1,1,1,
1,1,1,1,1,1,1,1,1,1,1,1,1,1,1,1,1,1,1,1,1,1,1,1,1,1,1,1,1,1,1,1,1,1,1,1,
1,1,1,1,1,1,1,1,1,1,1,1,1,1,1,1,1,1,1,1,1,1,1,1,1,1,1,1,1,1,1,1,1,1,1,1,
1,1,1,1,1,1,1,1,1,1,1,1,1,1,1,1,1,1,1,1,1,1,1,1,1,1,1,1,1,1,1,1,1,1,1,1,
1,1,1,1,1,1,1,1,1,1,1,1,1,1,1,1,1,1,1,1,1,1,1,1,1,1,1,1,1,1,1,6),(2,2),
(-1.,-0.998165138,-0.996330275,-0.994495413,-0.99266055,-0.990825688,-0.988990826,
-0.987155963,-0.985321101,-0.983486239,-0.981651376,-0.979816514,-0.977981651,
-0.976146789,-0.974311927,-0.972477064,-0.970642202,-0.968807339,-0.966972477,
-0.965137615,-0.963302752,-0.96146789,-0.959633028,-0.957798165,-0.955963303,
-0.95412844,-0.952293578,-0.950458716,-0.948623853,-0.946788991,-0.944954128,
-0.943119266,-0.941284404,-0.939449541,-0.937614679,-0.935779817,-0.933944954,
-0.932110092,-0.930275229,-0.928440367,-0.926605505,-0.924770642,-0.92293578,
-0.921100917,-0.919266055,-0.917431193,-0.91559633,-0.913761468,-0.911926606,
-0.910091743,-0.908256881,-0.906422018,-0.904587156,-0.902752294,-0.900917431,
-0.899082569,-0.897247706,-0.895412844,-0.893577982,-0.891743119,-0.889908257,
-0.888073394,-0.886238532,-0.88440367,-0.882568807,-0.880733945,-0.878899083,
-0.87706422,-0.875229358,-0.873394495,-0.871559633,-0.869724771,-0.867889908,
-0.866055046,-0.864220183,-0.862385321,-0.860550459,-0.858715596,-0.856880734,
-0.855045872,-0.853211009,-0.851376147,-0.849541284,-0.847706422,-0.84587156,
-0.844036697,-0.842201835,-0.840366972,-0.83853211,-0.836697248,-0.834862385,
-0.833027523,-0.831192661,-0.829357798,-0.827522936,-0.825688073,-0.823853211,
-0.822018349,-0.820183486,-0.818348624,-0.816513761,-0.814678899,-0.812844037,
-0.811009174,-0.809174312,-0.80733945,-0.805504587,-0.803669725,-0.801834862,
-0.8,-0.798165138,-0.796330275,-0.794495413,-0.79266055,-0.790825688,-0.788990826,
-0.787155963,-0.785321101,-0.783486239,-0.781651376,-0.779816514,-0.777981651,
-0.776146789,-0.774311927,-0.772477064,-0.770642202,-0.768807339,-0.766972477,
-0.765137615,-0.763302752,-0.76146789,-0.759633028,-0.757798165,-0.755963303,
-0.75412844,-0.752293578,-0.750458716,-0.748623853,-0.746788991,-0.744954128,
-0.743119266,-0.741284404,-0.739449541,-0.737614679,-0.735779817,-0.733944954,
-0.732110092,-0.730275229,-0.728440367,-0.726605505,-0.724770642,-0.72293578,
-0.721100917,-0.719266055,-0.717431193,-0.71559633,-0.713761468,-0.711926606,
-0.710091743,-0.708256881,-0.706422018,-0.704587156,-0.702752294,-0.700917431,
-0.699082569,-0.697247706,-0.695412844,-0.693577982,-0.691743119,-0.689908257,
-0.688073394,-0.686238532,-0.68440367,-0.682568807,-0.680733945,-0.678899083,
-0.67706422,-0.675229358,-0.673394495,-0.671559633,-0.669724771,-0.667889908,
-0.666055046,-0.664220183,-0.662385321,-0.660550459,-0.658715596,-0.656880734,
-0.655045872,-0.653211009,-0.651376147,-0.649541284,-0.647706422,-0.64587156,
-0.644036697,-0.642201835,-0.640366972,-0.63853211,-0.636697248,-0.634862385,
-0.633027523,-0.631192661,-0.629357798,-0.627522936,-0.625688073,-0.623853211,
-0.622018349,-0.620183486,-0.618348624,-0.616513761,-0.614678899,-0.612844037,
-0.611009174,-0.609174312,-0.60733945,-0.605504587,-0.603669725,-0.601834862,
-0.6,-0.598165138,-0.596330275,-0.594495413,-0.59266055,-0.590825688,-0.588990826,
-0.587155963,-0.585321101,-0.583486239,-0.581651376,-0.579816514,-0.577981651,
-0.576146789,-0.574311927,-0.572477064,-0.570642202,-0.568807339,-0.566972477,
-0.565137615,-0.563302752,-0.56146789,-0.559633028,-0.557798165,-0.555963303,
-0.55412844,-0.552293578,-0.550458716,-0.548623853,-0.546788991,-0.544954128,
-0.543119266,-0.541284404,-0.539449541,-0.537614679,-0.535779817,-0.533944954,
-0.532110092,-0.530275229,-0.528440367,-0.526605505,-0.524770642,-0.52293578,
-0.521100917,-0.519266055,-0.517431193,-0.51559633,-0.513761468,-0.511926606,
-0.510091743,-0.508256881,-0.506422018,-0.504587156,-0.502752294,-0.500917431,
-0.499082569,-0.497247706,-0.495412844,-0.493577982,-0.491743119,-0.489908257,
-0.488073394,-0.486238532,-0.48440367,-0.482568807,-0.480733945,-0.478899083,
-0.47706422,-0.475229358,-0.473394495,-0.471559633,-0.469724771,-0.467889908,
-0.466055046,-0.464220183,-0.462385321,-0.460550459,-0.458715596,-0.456880734,
-0.455045872,-0.453211009,-0.451376147,-0.449541284,-0.447706422,-0.44587156,
-0.444036697,-0.442201835,-0.440366972,-0.43853211,-0.436697248,-0.434862385,
-0.433027523,-0.431192661,-0.429357798,-0.427522936,-0.425688073,-0.423853211,
-0.422018349,-0.420183486,-0.418348624,-0.416513761,-0.414678899,-0.412844037,
-0.411009174,-0.409174312,-0.40733945,-0.405504587,-0.403669725,-0.401834862,
-0.4,-0.398165138,-0.396330275,-0.394495413,-0.39266055,-0.390825688,-0.388990826,
-0.387155963,-0.385321101,-0.383486239,-0.381651376,-0.379816514,-0.377981651,
-0.376146789,-0.374311927,-0.372477064,-0.370642202,-0.368807339,-0.366972477,
-0.365137615,-0.363302752,-0.36146789,-0.359633028,-0.357798165,-0.355963303,
-0.35412844,-0.352293578,-0.350458716,-0.348623853,-0.346788991,-0.344954128,
-0.343119266,-0.341284404,-0.339449541,-0.337614679,-0.335779817,-0.333944954,
-0.332110092,-0.330275229,-0.328440367,-0.326605505,-0.324770642,-0.32293578,
-0.321100917,-0.319266055,-0.317431193,-0.31559633,-0.313761468,-0.311926606,
-0.310091743,-0.308256881,-0.306422018,-0.304587156,-0.302752294,-0.300917431,
-0.299082569,-0.297247706,-0.295412844,-0.293577982,-0.291743119,-0.289908257,
-0.288073394,-0.286238532,-0.28440367,-0.282568807,-0.280733945,-0.278899083,
-0.27706422,-0.275229358,-0.273394495,-0.271559633,-0.269724771,-0.267889908,
-0.266055046,-0.264220183,-0.262385321,-0.260550459,-0.258715596,-0.256880734,
-0.255045872,-0.253211009,-0.251376147,-0.249541284,-0.247706422,-0.24587156,
-0.244036697,-0.242201835,-0.240366972,-0.23853211,-0.236697248,-0.234862385,
-0.233027523,-0.231192661,-0.229357798,-0.227522936,-0.225688073,-0.223853211,
-0.222018349,-0.220183486,-0.218348624,-0.216513761,-0.214678899,-0.212844037,
-0.211009174,-0.209174312,-0.20733945,-0.205504587,-0.203669725,-0.201834862,
-0.2,-0.198165138,-0.196330275,-0.194495413,-0.19266055,-0.190825688,-0.188990826,
-0.187155963,-0.185321101,-0.183486239,-0.181651376,-0.179816514,-0.177981651,
-0.176146789,-0.174311927,-0.172477064,-0.170642202,-0.168807339,-0.166972477,
-0.165137615,-0.163302752,-0.16146789,-0.159633028,-0.157798165,-0.155963303,
-0.15412844,-0.152293578,-0.150458716,-0.148623853,-0.146788991,-0.144954128,
-0.143172103),(0.,0.36),.UNSPECIFIED.);
#6294=B_SPLINE_SURFACE_WITH_KNOTS('',5,1,((#284642,#284643),(#284644,#284645),
(#284646,#284647),(#284648,#284649),(#284650,#284651),(#284652,#284653),
(#284654,#284655),(#284656,#284657),(#284658,#284659),(#284660,#284661),
(#284662,#284663),(#284664,#284665),(#284666,#284667),(#284668,#284669),
(#284670,#284671),(#284672,#284673),(#284674,#284675),(#284676,#284677),
(#284678,#284679),(#284680,#284681),(#284682,#284683),(#284684,#284685),
(#284686,#284687),(#284688,#284689),(#284690,#284691),(#284692,#284693),
(#284694,#284695),(#284696,#284697),(#284698,#284699),(#284700,#284701),
(#284702,#284703),(#284704,#284705),(#284706,#284707),(#284708,#284709),
(#284710,#284711),(#284712,#284713),(#284714,#284715),(#284716,#284717),
(#284718,#284719),(#284720,#284721),(#284722,#284723),(#284724,#284725),
(#284726,#284727),(#284728,#284729),(#284730,#284731),(#284732,#284733),
(#284734,#284735),(#284736,#284737),(#284738,#284739),(#284740,#284741),
(#284742,#284743),(#284744,#284745),(#284746,#284747),(#284748,#284749),
(#284750,#284751),(#284752,#284753),(#284754,#284755),(#284756,#284757),
(#284758,#284759),(#284760,#284761),(#284762,#284763),(#284764,#284765),
(#284766,#284767),(#284768,#284769),(#284770,#284771),(#284772,#284773),
(#284774,#284775),(#284776,#284777),(#284778,#284779),(#284780,#284781),
(#284782,#284783),(#284784,#284785),(#284786,#284787),(#284788,#284789),
(#284790,#284791),(#284792,#284793),(#284794,#284795),(#284796,#284797),
(#284798,#284799),(#284800,#284801),(#284802,#284803),(#284804,#284805),
(#284806,#284807),(#284808,#284809),(#284810,#284811),(#284812,#284813),
(#284814,#284815),(#284816,#284817),(#284818,#284819),(#284820,#284821),
(#284822,#284823),(#284824,#284825),(#284826,#284827),(#284828,#284829),
(#284830,#284831),(#284832,#284833),(#284834,#284835),(#284836,#284837),
(#284838,#284839),(#284840,#284841),(#284842,#284843),(#284844,#284845),
(#284846,#284847),(#284848,#284849),(#284850,#284851),(#284852,#284853),
(#284854,#284855),(#284856,#284857),(#284858,#284859),(#284860,#284861),
(#284862,#284863),(#284864,#284865),(#284866,#284867),(#284868,#284869),
(#284870,#284871),(#284872,#284873),(#284874,#284875),(#284876,#284877),
(#284878,#284879),(#284880,#284881),(#284882,#284883),(#284884,#284885),
(#284886,#284887),(#284888,#284889),(#284890,#284891),(#284892,#284893),
(#284894,#284895),(#284896,#284897),(#284898,#284899),(#284900,#284901),
(#284902,#284903),(#284904,#284905),(#284906,#284907),(#284908,#284909),
(#284910,#284911),(#284912,#284913),(#284914,#284915),(#284916,#284917),
(#284918,#284919),(#284920,#284921),(#284922,#284923),(#284924,#284925),
(#284926,#284927),(#284928,#284929),(#284930,#284931),(#284932,#284933),
(#284934,#284935),(#284936,#284937),(#284938,#284939),(#284940,#284941),
(#284942,#284943),(#284944,#284945),(#284946,#284947),(#284948,#284949),
(#284950,#284951),(#284952,#284953),(#284954,#284955),(#284956,#284957),
(#284958,#284959),(#284960,#284961),(#284962,#284963),(#284964,#284965),
(#284966,#284967),(#284968,#284969),(#284970,#284971),(#284972,#284973),
(#284974,#284975),(#284976,#284977),(#284978,#284979),(#284980,#284981),
(#284982,#284983),(#284984,#284985),(#284986,#284987),(#284988,#284989),
(#284990,#284991),(#284992,#284993),(#284994,#284995),(#284996,#284997),
(#284998,#284999),(#285000,#285001),(#285002,#285003),(#285004,#285005),
(#285006,#285007),(#285008,#285009),(#285010,#285011),(#285012,#285013),
(#285014,#285015),(#285016,#285017),(#285018,#285019),(#285020,#285021),
(#285022,#285023),(#285024,#285025),(#285026,#285027),(#285028,#285029),
(#285030,#285031),(#285032,#285033),(#285034,#285035),(#285036,#285037),
(#285038,#285039),(#285040,#285041),(#285042,#285043),(#285044,#285045),
(#285046,#285047),(#285048,#285049),(#285050,#285051),(#285052,#285053),
(#285054,#285055),(#285056,#285057),(#285058,#285059),(#285060,#285061),
(#285062,#285063),(#285064,#285065),(#285066,#285067),(#285068,#285069),
(#285070,#285071),(#285072,#285073),(#285074,#285075),(#285076,#285077),
(#285078,#285079),(#285080,#285081),(#285082,#285083),(#285084,#285085),
(#285086,#285087),(#285088,#285089),(#285090,#285091),(#285092,#285093),
(#285094,#285095),(#285096,#285097),(#285098,#285099),(#285100,#285101),
(#285102,#285103),(#285104,#285105),(#285106,#285107),(#285108,#285109),
(#285110,#285111),(#285112,#285113),(#285114,#285115),(#285116,#285117),
(#285118,#285119),(#285120,#285121),(#285122,#285123),(#285124,#285125),
(#285126,#285127),(#285128,#285129),(#285130,#285131),(#285132,#285133),
(#285134,#285135),(#285136,#285137),(#285138,#285139),(#285140,#285141),
(#285142,#285143),(#285144,#285145),(#285146,#285147),(#285148,#285149),
(#285150,#285151),(#285152,#285153),(#285154,#285155),(#285156,#285157),
(#285158,#285159),(#285160,#285161),(#285162,#285163),(#285164,#285165),
(#285166,#285167),(#285168,#285169),(#285170,#285171),(#285172,#285173),
(#285174,#285175),(#285176,#285177),(#285178,#285179),(#285180,#285181),
(#285182,#285183),(#285184,#285185),(#285186,#285187),(#285188,#285189),
(#285190,#285191),(#285192,#285193),(#285194,#285195),(#285196,#285197),
(#285198,#285199),(#285200,#285201),(#285202,#285203),(#285204,#285205),
(#285206,#285207),(#285208,#285209),(#285210,#285211),(#285212,#285213),
(#285214,#285215),(#285216,#285217),(#285218,#285219),(#285220,#285221),
(#285222,#285223),(#285224,#285225),(#285226,#285227),(#285228,#285229),
(#285230,#285231),(#285232,#285233),(#285234,#285235),(#285236,#285237),
(#285238,#285239),(#285240,#285241),(#285242,#285243),(#285244,#285245),
(#285246,#285247),(#285248,#285249),(#285250,#285251),(#285252,#285253),
(#285254,#285255),(#285256,#285257),(#285258,#285259),(#285260,#285261),
(#285262,#285263),(#285264,#285265),(#285266,#285267),(#285268,#285269),
(#285270,#285271),(#285272,#285273),(#285274,#285275),(#285276,#285277),
(#285278,#285279),(#285280,#285281),(#285282,#285283),(#285284,#285285),
(#285286,#285287),(#285288,#285289),(#285290,#285291),(#285292,#285293),
(#285294,#285295),(#285296,#285297),(#285298,#285299),(#285300,#285301),
(#285302,#285303),(#285304,#285305),(#285306,#285307),(#285308,#285309),
(#285310,#285311),(#285312,#285313),(#285314,#285315),(#285316,#285317),
(#285318,#285319),(#285320,#285321),(#285322,#285323),(#285324,#285325),
(#285326,#285327),(#285328,#285329),(#285330,#285331),(#285332,#285333),
(#285334,#285335),(#285336,#285337),(#285338,#285339),(#285340,#285341),
(#285342,#285343),(#285344,#285345),(#285346,#285347),(#285348,#285349),
(#285350,#285351),(#285352,#285353),(#285354,#285355),(#285356,#285357),
(#285358,#285359),(#285360,#285361),(#285362,#285363),(#285364,#285365),
(#285366,#285367),(#285368,#285369),(#285370,#285371),(#285372,#285373),
(#285374,#285375),(#285376,#285377),(#285378,#285379),(#285380,#285381),
(#285382,#285383),(#285384,#285385),(#285386,#285387),(#285388,#285389),
(#285390,#285391),(#285392,#285393),(#285394,#285395),(#285396,#285397),
(#285398,#285399),(#285400,#285401),(#285402,#285403),(#285404,#285405),
(#285406,#285407),(#285408,#285409),(#285410,#285411),(#285412,#285413),
(#285414,#285415),(#285416,#285417),(#285418,#285419),(#285420,#285421),
(#285422,#285423),(#285424,#285425),(#285426,#285427),(#285428,#285429),
(#285430,#285431),(#285432,#285433),(#285434,#285435),(#285436,#285437),
(#285438,#285439),(#285440,#285441),(#285442,#285443),(#285444,#285445),
(#285446,#285447),(#285448,#285449),(#285450,#285451),(#285452,#285453),
(#285454,#285455),(#285456,#285457),(#285458,#285459),(#285460,#285461),
(#285462,#285463),(#285464,#285465),(#285466,#285467),(#285468,#285469),
(#285470,#285471),(#285472,#285473),(#285474,#285475),(#285476,#285477),
(#285478,#285479),(#285480,#285481),(#285482,#285483),(#285484,#285485),
(#285486,#285487),(#285488,#285489),(#285490,#285491),(#285492,#285493),
(#285494,#285495),(#285496,#285497),(#285498,#285499),(#285500,#285501),
(#285502,#285503),(#285504,#285505),(#285506,#285507),(#285508,#285509),
(#285510,#285511),(#285512,#285513),(#285514,#285515),(#285516,#285517),
(#285518,#285519),(#285520,#285521),(#285522,#285523),(#285524,#285525),
(#285526,#285527),(#285528,#285529),(#285530,#285531),(#285532,#285533),
(#285534,#285535),(#285536,#285537),(#285538,#285539),(#285540,#285541),
(#285542,#285543),(#285544,#285545),(#285546,#285547),(#285548,#285549),
(#285550,#285551),(#285552,#285553),(#285554,#285555),(#285556,#285557),
(#285558,#285559),(#285560,#285561),(#285562,#285563),(#285564,#285565),
(#285566,#285567),(#285568,#285569),(#285570,#285571),(#285572,#285573),
(#285574,#285575),(#285576,#285577),(#285578,#285579),(#285580,#285581),
(#285582,#285583),(#285584,#285585)),.UNSPECIFIED.,.F.,.F.,.F.,(6,1,1,1,
1,1,1,1,1,1,1,1,1,1,1,1,1,1,1,1,1,1,1,1,1,1,1,1,1,1,1,1,1,1,1,1,1,1,1,1,
1,1,1,1,1,1,1,1,1,1,1,1,1,1,1,1,1,1,1,1,1,1,1,1,1,1,1,1,1,1,1,1,1,1,1,1,
1,1,1,1,1,1,1,1,1,1,1,1,1,1,1,1,1,1,1,1,1,1,1,1,1,1,1,1,1,1,1,1,1,1,1,1,
1,1,1,1,1,1,1,1,1,1,1,1,1,1,1,1,1,1,1,1,1,1,1,1,1,1,1,1,1,1,1,1,1,1,1,1,
1,1,1,1,1,1,1,1,1,1,1,1,1,1,1,1,1,1,1,1,1,1,1,1,1,1,1,1,1,1,1,1,1,1,1,1,
1,1,1,1,1,1,1,1,1,1,1,1,1,1,1,1,1,1,1,1,1,1,1,1,1,1,1,1,1,1,1,1,1,1,1,1,
1,1,1,1,1,1,1,1,1,1,1,1,1,1,1,1,1,1,1,1,1,1,1,1,1,1,1,1,1,1,1,1,1,1,1,1,
1,1,1,1,1,1,1,1,1,1,1,1,1,1,1,1,1,1,1,1,1,1,1,1,1,1,1,1,1,1,1,1,1,1,1,1,
1,1,1,1,1,1,1,1,1,1,1,1,1,1,1,1,1,1,1,1,1,1,1,1,1,1,1,1,1,1,1,1,1,1,1,1,
1,1,1,1,1,1,1,1,1,1,1,1,1,1,1,1,1,1,1,1,1,1,1,1,1,1,1,1,1,1,1,1,1,1,1,1,
1,1,1,1,1,1,1,1,1,1,1,1,1,1,1,1,1,1,1,1,1,1,1,1,1,1,1,1,1,1,1,1,1,1,1,1,
1,1,1,1,1,1,1,1,1,1,1,1,1,1,1,1,1,1,1,1,1,1,1,1,1,1,1,1,1,1,1,1,1,1,1,1,
1,1,1,1,1,1,1,1,1,1,1,1,1,1,1,1,1,1,1,1,1,1,1,1,1,1,1,1,1,1,1,6),(2,2),
(0.143172103,0.144954128,0.146788991,0.148623853,0.150458716,0.152293578,
0.15412844,0.155963303,0.157798165,0.159633028,0.16146789,0.163302752,0.165137615,
0.166972477,0.168807339,0.170642202,0.172477064,0.174311927,0.176146789,
0.177981651,0.179816514,0.181651376,0.183486239,0.185321101,0.187155963,
0.188990826,0.190825688,0.19266055,0.194495413,0.196330275,0.198165138,
0.2,0.201834862,0.203669725,0.205504587,0.20733945,0.209174312,0.211009174,
0.212844037,0.214678899,0.216513761,0.218348624,0.220183486,0.222018349,
0.223853211,0.225688073,0.227522936,0.229357798,0.231192661,0.233027523,
0.234862385,0.236697248,0.23853211,0.240366972,0.242201835,0.244036697,
0.24587156,0.247706422,0.249541284,0.251376147,0.253211009,0.255045872,
0.256880734,0.258715596,0.260550459,0.262385321,0.264220183,0.266055046,
0.267889908,0.269724771,0.271559633,0.273394495,0.275229358,0.27706422,
0.278899083,0.280733945,0.282568807,0.28440367,0.286238532,0.288073394,
0.289908257,0.291743119,0.293577982,0.295412844,0.297247706,0.299082569,
0.300917431,0.302752294,0.304587156,0.306422018,0.308256881,0.310091743,
0.311926606,0.313761468,0.31559633,0.317431193,0.319266055,0.321100917,
0.32293578,0.324770642,0.326605505,0.328440367,0.330275229,0.332110092,
0.333944954,0.335779817,0.337614679,0.339449541,0.341284404,0.343119266,
0.344954128,0.346788991,0.348623853,0.350458716,0.352293578,0.35412844,
0.355963303,0.357798165,0.359633028,0.36146789,0.363302752,0.365137615,
0.366972477,0.368807339,0.370642202,0.372477064,0.374311927,0.376146789,
0.377981651,0.379816514,0.381651376,0.383486239,0.385321101,0.387155963,
0.388990826,0.390825688,0.39266055,0.394495413,0.396330275,0.398165138,
0.4,0.401834862,0.403669725,0.405504587,0.40733945,0.409174312,0.411009174,
0.412844037,0.414678899,0.416513761,0.418348624,0.420183486,0.422018349,
0.423853211,0.425688073,0.427522936,0.429357798,0.431192661,0.433027523,
0.434862385,0.436697248,0.43853211,0.440366972,0.442201835,0.444036697,
0.44587156,0.447706422,0.449541284,0.451376147,0.453211009,0.455045872,
0.456880734,0.458715596,0.460550459,0.462385321,0.464220183,0.466055046,
0.467889908,0.469724771,0.471559633,0.473394495,0.475229358,0.47706422,
0.478899083,0.480733945,0.482568807,0.48440367,0.486238532,0.488073394,
0.489908257,0.491743119,0.493577982,0.495412844,0.497247706,0.499082569,
0.500917431,0.502752294,0.504587156,0.506422018,0.508256881,0.510091743,
0.511926606,0.513761468,0.51559633,0.517431193,0.519266055,0.521100917,
0.52293578,0.524770642,0.526605505,0.528440367,0.530275229,0.532110092,
0.533944954,0.535779817,0.537614679,0.539449541,0.541284404,0.543119266,
0.544954128,0.546788991,0.548623853,0.550458716,0.552293578,0.55412844,
0.555963303,0.557798165,0.559633028,0.56146789,0.563302752,0.565137615,
0.566972477,0.568807339,0.570642202,0.572477064,0.574311927,0.576146789,
0.577981651,0.579816514,0.581651376,0.583486239,0.585321101,0.587155963,
0.588990826,0.590825688,0.59266055,0.594495413,0.596330275,0.598165138,
0.6,0.601834862,0.603669725,0.605504587,0.60733945,0.609174312,0.611009174,
0.612844037,0.614678899,0.616513761,0.618348624,0.620183486,0.622018349,
0.623853211,0.625688073,0.627522936,0.629357798,0.631192661,0.633027523,
0.634862385,0.636697248,0.63853211,0.640366972,0.642201835,0.644036697,
0.64587156,0.647706422,0.649541284,0.651376147,0.653211009,0.655045872,
0.656880734,0.658715596,0.660550459,0.662385321,0.664220183,0.666055046,
0.667889908,0.669724771,0.671559633,0.673394495,0.675229358,0.67706422,
0.678899083,0.680733945,0.682568807,0.68440367,0.686238532,0.688073394,
0.689908257,0.691743119,0.693577982,0.695412844,0.697247706,0.699082569,
0.700917431,0.702752294,0.704587156,0.706422018,0.708256881,0.710091743,
0.711926606,0.713761468,0.71559633,0.717431193,0.719266055,0.721100917,
0.72293578,0.724770642,0.726605505,0.728440367,0.730275229,0.732110092,
0.733944954,0.735779817,0.737614679,0.739449541,0.741284404,0.743119266,
0.744954128,0.746788991,0.748623853,0.750458716,0.752293578,0.75412844,
0.755963303,0.757798165,0.759633028,0.76146789,0.763302752,0.765137615,
0.766972477,0.768807339,0.770642202,0.772477064,0.774311927,0.776146789,
0.777981651,0.779816514,0.781651376,0.783486239,0.785321101,0.787155963,
0.788990826,0.790825688,0.79266055,0.794495413,0.796330275,0.798165138,
0.8,0.801834862,0.803669725,0.805504587,0.80733945,0.809174312,0.811009174,
0.812844037,0.814678899,0.816513761,0.818348624,0.820183486,0.822018349,
0.823853211,0.825688073,0.827522936,0.829357798,0.831192661,0.833027523,
0.834862385,0.836697248,0.83853211,0.840366972,0.842201835,0.844036697,
0.84587156,0.847706422,0.849541284,0.851376147,0.853211009,0.855045872,
0.856880734,0.858715596,0.860550459,0.862385321,0.864220183,0.866055046,
0.867889908,0.869724771,0.871559633,0.873394495,0.875229358,0.87706422,
0.878899083,0.880733945,0.882568807,0.88440367,0.886238532,0.888073394,
0.889908257,0.891743119,0.893577982,0.895412844,0.897247706,0.899082569,
0.900917431,0.902752294,0.904587156,0.906422018,0.908256881,0.910091743,
0.911926606,0.913761468,0.91559633,0.917431193,0.919266055,0.921100917,
0.92293578,0.924770642,0.926605505,0.928440367,0.930275229,0.932110092,
0.933944954,0.935779817,0.937614679,0.939449541,0.941284404,0.943119266,
0.944954128,0.946788991,0.948623853,0.950458716,0.952293578,0.95412844,
0.955963303,0.957798165,0.959633028,0.96146789,0.963302752,0.965137615,
0.966972477,0.968807339,0.970642202,0.972477064,0.974311927,0.976146789,
0.977981651,0.979816514,0.981651376,0.983486239,0.985321101,0.987155963,
0.988990826,0.990825688,0.99266055,0.994495413,0.996330275,0.998165138,
1.),(0.,0.36),.UNSPECIFIED.);
#6295=B_SPLINE_SURFACE_WITH_KNOTS('',5,1,((#286545,#286546),(#286547,#286548),
(#286549,#286550),(#286551,#286552),(#286553,#286554),(#286555,#286556),
(#286557,#286558),(#286559,#286560),(#286561,#286562),(#286563,#286564),
(#286565,#286566),(#286567,#286568),(#286569,#286570),(#286571,#286572),
(#286573,#286574),(#286575,#286576),(#286577,#286578),(#286579,#286580),
(#286581,#286582),(#286583,#286584),(#286585,#286586),(#286587,#286588),
(#286589,#286590),(#286591,#286592),(#286593,#286594),(#286595,#286596),
(#286597,#286598),(#286599,#286600),(#286601,#286602),(#286603,#286604),
(#286605,#286606),(#286607,#286608),(#286609,#286610),(#286611,#286612),
(#286613,#286614),(#286615,#286616),(#286617,#286618),(#286619,#286620),
(#286621,#286622),(#286623,#286624),(#286625,#286626),(#286627,#286628),
(#286629,#286630),(#286631,#286632),(#286633,#286634),(#286635,#286636),
(#286637,#286638),(#286639,#286640),(#286641,#286642),(#286643,#286644),
(#286645,#286646),(#286647,#286648),(#286649,#286650),(#286651,#286652),
(#286653,#286654),(#286655,#286656),(#286657,#286658),(#286659,#286660),
(#286661,#286662),(#286663,#286664),(#286665,#286666),(#286667,#286668),
(#286669,#286670),(#286671,#286672),(#286673,#286674),(#286675,#286676),
(#286677,#286678),(#286679,#286680),(#286681,#286682),(#286683,#286684),
(#286685,#286686),(#286687,#286688),(#286689,#286690),(#286691,#286692),
(#286693,#286694),(#286695,#286696),(#286697,#286698),(#286699,#286700),
(#286701,#286702),(#286703,#286704),(#286705,#286706),(#286707,#286708),
(#286709,#286710),(#286711,#286712),(#286713,#286714),(#286715,#286716),
(#286717,#286718),(#286719,#286720),(#286721,#286722),(#286723,#286724),
(#286725,#286726),(#286727,#286728),(#286729,#286730),(#286731,#286732),
(#286733,#286734),(#286735,#286736),(#286737,#286738),(#286739,#286740),
(#286741,#286742),(#286743,#286744),(#286745,#286746),(#286747,#286748),
(#286749,#286750),(#286751,#286752),(#286753,#286754),(#286755,#286756),
(#286757,#286758),(#286759,#286760),(#286761,#286762),(#286763,#286764),
(#286765,#286766),(#286767,#286768),(#286769,#286770),(#286771,#286772),
(#286773,#286774),(#286775,#286776),(#286777,#286778),(#286779,#286780),
(#286781,#286782),(#286783,#286784),(#286785,#286786),(#286787,#286788),
(#286789,#286790),(#286791,#286792),(#286793,#286794),(#286795,#286796),
(#286797,#286798),(#286799,#286800),(#286801,#286802),(#286803,#286804),
(#286805,#286806),(#286807,#286808),(#286809,#286810),(#286811,#286812),
(#286813,#286814),(#286815,#286816),(#286817,#286818),(#286819,#286820),
(#286821,#286822),(#286823,#286824),(#286825,#286826),(#286827,#286828),
(#286829,#286830),(#286831,#286832),(#286833,#286834),(#286835,#286836),
(#286837,#286838),(#286839,#286840),(#286841,#286842),(#286843,#286844),
(#286845,#286846),(#286847,#286848),(#286849,#286850),(#286851,#286852),
(#286853,#286854),(#286855,#286856),(#286857,#286858),(#286859,#286860),
(#286861,#286862),(#286863,#286864),(#286865,#286866),(#286867,#286868),
(#286869,#286870),(#286871,#286872),(#286873,#286874),(#286875,#286876),
(#286877,#286878),(#286879,#286880),(#286881,#286882),(#286883,#286884),
(#286885,#286886),(#286887,#286888),(#286889,#286890),(#286891,#286892),
(#286893,#286894),(#286895,#286896),(#286897,#286898),(#286899,#286900),
(#286901,#286902),(#286903,#286904),(#286905,#286906),(#286907,#286908),
(#286909,#286910),(#286911,#286912),(#286913,#286914),(#286915,#286916),
(#286917,#286918),(#286919,#286920),(#286921,#286922),(#286923,#286924),
(#286925,#286926),(#286927,#286928),(#286929,#286930),(#286931,#286932),
(#286933,#286934),(#286935,#286936),(#286937,#286938),(#286939,#286940),
(#286941,#286942),(#286943,#286944),(#286945,#286946),(#286947,#286948),
(#286949,#286950),(#286951,#286952),(#286953,#286954),(#286955,#286956),
(#286957,#286958),(#286959,#286960),(#286961,#286962),(#286963,#286964),
(#286965,#286966),(#286967,#286968),(#286969,#286970),(#286971,#286972),
(#286973,#286974),(#286975,#286976),(#286977,#286978),(#286979,#286980),
(#286981,#286982),(#286983,#286984),(#286985,#286986),(#286987,#286988),
(#286989,#286990),(#286991,#286992),(#286993,#286994),(#286995,#286996),
(#286997,#286998),(#286999,#287000),(#287001,#287002),(#287003,#287004),
(#287005,#287006),(#287007,#287008),(#287009,#287010),(#287011,#287012),
(#287013,#287014),(#287015,#287016),(#287017,#287018),(#287019,#287020),
(#287021,#287022),(#287023,#287024),(#287025,#287026),(#287027,#287028),
(#287029,#287030),(#287031,#287032),(#287033,#287034),(#287035,#287036),
(#287037,#287038),(#287039,#287040),(#287041,#287042),(#287043,#287044),
(#287045,#287046),(#287047,#287048),(#287049,#287050),(#287051,#287052),
(#287053,#287054),(#287055,#287056),(#287057,#287058),(#287059,#287060),
(#287061,#287062),(#287063,#287064),(#287065,#287066),(#287067,#287068),
(#287069,#287070),(#287071,#287072),(#287073,#287074),(#287075,#287076),
(#287077,#287078),(#287079,#287080),(#287081,#287082),(#287083,#287084),
(#287085,#287086),(#287087,#287088),(#287089,#287090),(#287091,#287092),
(#287093,#287094),(#287095,#287096),(#287097,#287098),(#287099,#287100),
(#287101,#287102),(#287103,#287104),(#287105,#287106),(#287107,#287108),
(#287109,#287110),(#287111,#287112),(#287113,#287114),(#287115,#287116),
(#287117,#287118),(#287119,#287120),(#287121,#287122),(#287123,#287124),
(#287125,#287126),(#287127,#287128),(#287129,#287130),(#287131,#287132),
(#287133,#287134),(#287135,#287136),(#287137,#287138),(#287139,#287140),
(#287141,#287142),(#287143,#287144),(#287145,#287146),(#287147,#287148),
(#287149,#287150),(#287151,#287152),(#287153,#287154),(#287155,#287156),
(#287157,#287158),(#287159,#287160),(#287161,#287162),(#287163,#287164),
(#287165,#287166),(#287167,#287168),(#287169,#287170),(#287171,#287172),
(#287173,#287174),(#287175,#287176),(#287177,#287178),(#287179,#287180),
(#287181,#287182),(#287183,#287184),(#287185,#287186),(#287187,#287188),
(#287189,#287190),(#287191,#287192),(#287193,#287194),(#287195,#287196),
(#287197,#287198),(#287199,#287200),(#287201,#287202),(#287203,#287204),
(#287205,#287206),(#287207,#287208),(#287209,#287210),(#287211,#287212),
(#287213,#287214),(#287215,#287216),(#287217,#287218),(#287219,#287220),
(#287221,#287222),(#287223,#287224),(#287225,#287226),(#287227,#287228),
(#287229,#287230),(#287231,#287232),(#287233,#287234),(#287235,#287236),
(#287237,#287238),(#287239,#287240),(#287241,#287242),(#287243,#287244),
(#287245,#287246),(#287247,#287248),(#287249,#287250),(#287251,#287252),
(#287253,#287254),(#287255,#287256),(#287257,#287258),(#287259,#287260),
(#287261,#287262),(#287263,#287264),(#287265,#287266),(#287267,#287268),
(#287269,#287270),(#287271,#287272),(#287273,#287274),(#287275,#287276),
(#287277,#287278),(#287279,#287280),(#287281,#287282),(#287283,#287284),
(#287285,#287286),(#287287,#287288),(#287289,#287290),(#287291,#287292),
(#287293,#287294),(#287295,#287296),(#287297,#287298),(#287299,#287300),
(#287301,#287302),(#287303,#287304),(#287305,#287306),(#287307,#287308),
(#287309,#287310),(#287311,#287312),(#287313,#287314),(#287315,#287316),
(#287317,#287318),(#287319,#287320),(#287321,#287322),(#287323,#287324),
(#287325,#287326),(#287327,#287328),(#287329,#287330),(#287331,#287332),
(#287333,#287334),(#287335,#287336),(#287337,#287338),(#287339,#287340),
(#287341,#287342),(#287343,#287344),(#287345,#287346),(#287347,#287348),
(#287349,#287350),(#287351,#287352),(#287353,#287354),(#287355,#287356),
(#287357,#287358),(#287359,#287360),(#287361,#287362),(#287363,#287364),
(#287365,#287366),(#287367,#287368),(#287369,#287370),(#287371,#287372),
(#287373,#287374),(#287375,#287376),(#287377,#287378),(#287379,#287380),
(#287381,#287382),(#287383,#287384),(#287385,#287386),(#287387,#287388),
(#287389,#287390),(#287391,#287392),(#287393,#287394),(#287395,#287396),
(#287397,#287398),(#287399,#287400),(#287401,#287402),(#287403,#287404),
(#287405,#287406),(#287407,#287408),(#287409,#287410),(#287411,#287412),
(#287413,#287414),(#287415,#287416),(#287417,#287418),(#287419,#287420),
(#287421,#287422),(#287423,#287424),(#287425,#287426),(#287427,#287428),
(#287429,#287430),(#287431,#287432),(#287433,#287434),(#287435,#287436),
(#287437,#287438),(#287439,#287440),(#287441,#287442),(#287443,#287444),
(#287445,#287446),(#287447,#287448),(#287449,#287450),(#287451,#287452),
(#287453,#287454),(#287455,#287456),(#287457,#287458),(#287459,#287460),
(#287461,#287462),(#287463,#287464),(#287465,#287466),(#287467,#287468),
(#287469,#287470),(#287471,#287472),(#287473,#287474),(#287475,#287476),
(#287477,#287478),(#287479,#287480),(#287481,#287482),(#287483,#287484),
(#287485,#287486),(#287487,#287488)),.UNSPECIFIED.,.F.,.F.,.F.,(6,1,1,1,
1,1,1,1,1,1,1,1,1,1,1,1,1,1,1,1,1,1,1,1,1,1,1,1,1,1,1,1,1,1,1,1,1,1,1,1,
1,1,1,1,1,1,1,1,1,1,1,1,1,1,1,1,1,1,1,1,1,1,1,1,1,1,1,1,1,1,1,1,1,1,1,1,
1,1,1,1,1,1,1,1,1,1,1,1,1,1,1,1,1,1,1,1,1,1,1,1,1,1,1,1,1,1,1,1,1,1,1,1,
1,1,1,1,1,1,1,1,1,1,1,1,1,1,1,1,1,1,1,1,1,1,1,1,1,1,1,1,1,1,1,1,1,1,1,1,
1,1,1,1,1,1,1,1,1,1,1,1,1,1,1,1,1,1,1,1,1,1,1,1,1,1,1,1,1,1,1,1,1,1,1,1,
1,1,1,1,1,1,1,1,1,1,1,1,1,1,1,1,1,1,1,1,1,1,1,1,1,1,1,1,1,1,1,1,1,1,1,1,
1,1,1,1,1,1,1,1,1,1,1,1,1,1,1,1,1,1,1,1,1,1,1,1,1,1,1,1,1,1,1,1,1,1,1,1,
1,1,1,1,1,1,1,1,1,1,1,1,1,1,1,1,1,1,1,1,1,1,1,1,1,1,1,1,1,1,1,1,1,1,1,1,
1,1,1,1,1,1,1,1,1,1,1,1,1,1,1,1,1,1,1,1,1,1,1,1,1,1,1,1,1,1,1,1,1,1,1,1,
1,1,1,1,1,1,1,1,1,1,1,1,1,1,1,1,1,1,1,1,1,1,1,1,1,1,1,1,1,1,1,1,1,1,1,1,
1,1,1,1,1,1,1,1,1,1,1,1,1,1,1,1,1,1,1,1,1,1,1,1,1,1,1,1,1,1,1,1,1,1,1,1,
1,1,1,1,1,1,1,1,1,1,1,1,1,1,1,1,1,1,1,1,1,1,1,1,1,1,1,1,1,1,1,1,1,1,1,1,
1,1,1,1,1,1,1,1,1,1,1,1,1,1,1,1,1,1,1,1,1,1,1,1,1,1,1,1,1,1,1,6),(2,2),
(0.143172104,0.144954128,0.146788991,0.148623853,0.150458716,0.152293578,
0.15412844,0.155963303,0.157798165,0.159633028,0.16146789,0.163302752,0.165137615,
0.166972477,0.168807339,0.170642202,0.172477064,0.174311927,0.176146789,
0.177981651,0.179816514,0.181651376,0.183486239,0.185321101,0.187155963,
0.188990826,0.190825688,0.19266055,0.194495413,0.196330275,0.198165138,
0.2,0.201834862,0.203669725,0.205504587,0.20733945,0.209174312,0.211009174,
0.212844037,0.214678899,0.216513761,0.218348624,0.220183486,0.222018349,
0.223853211,0.225688073,0.227522936,0.229357798,0.231192661,0.233027523,
0.234862385,0.236697248,0.23853211,0.240366972,0.242201835,0.244036697,
0.24587156,0.247706422,0.249541284,0.251376147,0.253211009,0.255045872,
0.256880734,0.258715596,0.260550459,0.262385321,0.264220183,0.266055046,
0.267889908,0.269724771,0.271559633,0.273394495,0.275229358,0.27706422,
0.278899083,0.280733945,0.282568807,0.28440367,0.286238532,0.288073394,
0.289908257,0.291743119,0.293577982,0.295412844,0.297247706,0.299082569,
0.300917431,0.302752294,0.304587156,0.306422018,0.308256881,0.310091743,
0.311926606,0.313761468,0.31559633,0.317431193,0.319266055,0.321100917,
0.32293578,0.324770642,0.326605505,0.328440367,0.330275229,0.332110092,
0.333944954,0.335779817,0.337614679,0.339449541,0.341284404,0.343119266,
0.344954128,0.346788991,0.348623853,0.350458716,0.352293578,0.35412844,
0.355963303,0.357798165,0.359633028,0.36146789,0.363302752,0.365137615,
0.366972477,0.368807339,0.370642202,0.372477064,0.374311927,0.376146789,
0.377981651,0.379816514,0.381651376,0.383486239,0.385321101,0.387155963,
0.388990826,0.390825688,0.39266055,0.394495413,0.396330275,0.398165138,
0.4,0.401834862,0.403669725,0.405504587,0.40733945,0.409174312,0.411009174,
0.412844037,0.414678899,0.416513761,0.418348624,0.420183486,0.422018349,
0.423853211,0.425688073,0.427522936,0.429357798,0.431192661,0.433027523,
0.434862385,0.436697248,0.43853211,0.440366972,0.442201835,0.444036697,
0.44587156,0.447706422,0.449541284,0.451376147,0.453211009,0.455045872,
0.456880734,0.458715596,0.460550459,0.462385321,0.464220183,0.466055046,
0.467889908,0.469724771,0.471559633,0.473394495,0.475229358,0.47706422,
0.478899083,0.480733945,0.482568807,0.48440367,0.486238532,0.488073394,
0.489908257,0.491743119,0.493577982,0.495412844,0.497247706,0.499082569,
0.500917431,0.502752294,0.504587156,0.506422018,0.508256881,0.510091743,
0.511926606,0.513761468,0.51559633,0.517431193,0.519266055,0.521100917,
0.52293578,0.524770642,0.526605505,0.528440367,0.530275229,0.532110092,
0.533944954,0.535779817,0.537614679,0.539449541,0.541284404,0.543119266,
0.544954128,0.546788991,0.548623853,0.550458716,0.552293578,0.55412844,
0.555963303,0.557798165,0.559633028,0.56146789,0.563302752,0.565137615,
0.566972477,0.568807339,0.570642202,0.572477064,0.574311927,0.576146789,
0.577981651,0.579816514,0.581651376,0.583486239,0.585321101,0.587155963,
0.588990826,0.590825688,0.59266055,0.594495413,0.596330275,0.598165138,
0.6,0.601834862,0.603669725,0.605504587,0.60733945,0.609174312,0.611009174,
0.612844037,0.614678899,0.616513761,0.618348624,0.620183486,0.622018349,
0.623853211,0.625688073,0.627522936,0.629357798,0.631192661,0.633027523,
0.634862385,0.636697248,0.63853211,0.640366972,0.642201835,0.644036697,
0.64587156,0.647706422,0.649541284,0.651376147,0.653211009,0.655045872,
0.656880734,0.658715596,0.660550459,0.662385321,0.664220183,0.666055046,
0.667889908,0.669724771,0.671559633,0.673394495,0.675229358,0.67706422,
0.678899083,0.680733945,0.682568807,0.68440367,0.686238532,0.688073394,
0.689908257,0.691743119,0.693577982,0.695412844,0.697247706,0.699082569,
0.700917431,0.702752294,0.704587156,0.706422018,0.708256881,0.710091743,
0.711926606,0.713761468,0.71559633,0.717431193,0.719266055,0.721100917,
0.72293578,0.724770642,0.726605505,0.728440367,0.730275229,0.732110092,
0.733944954,0.735779817,0.737614679,0.739449541,0.741284404,0.743119266,
0.744954128,0.746788991,0.748623853,0.750458716,0.752293578,0.75412844,
0.755963303,0.757798165,0.759633028,0.76146789,0.763302752,0.765137615,
0.766972477,0.768807339,0.770642202,0.772477064,0.774311927,0.776146789,
0.777981651,0.779816514,0.781651376,0.783486239,0.785321101,0.787155963,
0.788990826,0.790825688,0.79266055,0.794495413,0.796330275,0.798165138,
0.8,0.801834862,0.803669725,0.805504587,0.80733945,0.809174312,0.811009174,
0.812844037,0.814678899,0.816513761,0.818348624,0.820183486,0.822018349,
0.823853211,0.825688073,0.827522936,0.829357798,0.831192661,0.833027523,
0.834862385,0.836697248,0.83853211,0.840366972,0.842201835,0.844036697,
0.84587156,0.847706422,0.849541284,0.851376147,0.853211009,0.855045872,
0.856880734,0.858715596,0.860550459,0.862385321,0.864220183,0.866055046,
0.867889908,0.869724771,0.871559633,0.873394495,0.875229358,0.87706422,
0.878899083,0.880733945,0.882568807,0.88440367,0.886238532,0.888073394,
0.889908257,0.891743119,0.893577982,0.895412844,0.897247706,0.899082569,
0.900917431,0.902752294,0.904587156,0.906422018,0.908256881,0.910091743,
0.911926606,0.913761468,0.91559633,0.917431193,0.919266055,0.921100917,
0.92293578,0.924770642,0.926605505,0.928440367,0.930275229,0.932110092,
0.933944954,0.935779817,0.937614679,0.939449541,0.941284404,0.943119266,
0.944954128,0.946788991,0.948623853,0.950458716,0.952293578,0.95412844,
0.955963303,0.957798165,0.959633028,0.96146789,0.963302752,0.965137615,
0.966972477,0.968807339,0.970642202,0.972477064,0.974311927,0.976146789,
0.977981651,0.979816514,0.981651376,0.983486239,0.985321101,0.987155963,
0.988990826,0.990825688,0.99266055,0.994495413,0.996330275,0.998165138,
1.),(0.,0.36),.UNSPECIFIED.);
#6296=B_SPLINE_SURFACE_WITH_KNOTS('',5,1,((#288431,#288432),(#288433,#288434),
(#288435,#288436),(#288437,#288438),(#288439,#288440),(#288441,#288442),
(#288443,#288444),(#288445,#288446),(#288447,#288448),(#288449,#288450),
(#288451,#288452),(#288453,#288454),(#288455,#288456),(#288457,#288458),
(#288459,#288460),(#288461,#288462),(#288463,#288464),(#288465,#288466),
(#288467,#288468),(#288469,#288470),(#288471,#288472),(#288473,#288474),
(#288475,#288476),(#288477,#288478),(#288479,#288480),(#288481,#288482),
(#288483,#288484),(#288485,#288486),(#288487,#288488),(#288489,#288490),
(#288491,#288492),(#288493,#288494),(#288495,#288496),(#288497,#288498),
(#288499,#288500),(#288501,#288502),(#288503,#288504),(#288505,#288506),
(#288507,#288508),(#288509,#288510),(#288511,#288512),(#288513,#288514),
(#288515,#288516),(#288517,#288518),(#288519,#288520),(#288521,#288522),
(#288523,#288524),(#288525,#288526),(#288527,#288528),(#288529,#288530),
(#288531,#288532),(#288533,#288534),(#288535,#288536),(#288537,#288538),
(#288539,#288540),(#288541,#288542),(#288543,#288544),(#288545,#288546),
(#288547,#288548),(#288549,#288550),(#288551,#288552),(#288553,#288554),
(#288555,#288556),(#288557,#288558),(#288559,#288560),(#288561,#288562),
(#288563,#288564),(#288565,#288566),(#288567,#288568),(#288569,#288570),
(#288571,#288572),(#288573,#288574),(#288575,#288576),(#288577,#288578),
(#288579,#288580),(#288581,#288582),(#288583,#288584),(#288585,#288586),
(#288587,#288588),(#288589,#288590),(#288591,#288592),(#288593,#288594),
(#288595,#288596),(#288597,#288598),(#288599,#288600),(#288601,#288602),
(#288603,#288604),(#288605,#288606),(#288607,#288608),(#288609,#288610),
(#288611,#288612),(#288613,#288614),(#288615,#288616),(#288617,#288618),
(#288619,#288620),(#288621,#288622),(#288623,#288624),(#288625,#288626),
(#288627,#288628),(#288629,#288630),(#288631,#288632),(#288633,#288634),
(#288635,#288636),(#288637,#288638),(#288639,#288640),(#288641,#288642),
(#288643,#288644),(#288645,#288646),(#288647,#288648),(#288649,#288650),
(#288651,#288652),(#288653,#288654),(#288655,#288656),(#288657,#288658),
(#288659,#288660),(#288661,#288662),(#288663,#288664),(#288665,#288666),
(#288667,#288668),(#288669,#288670),(#288671,#288672),(#288673,#288674),
(#288675,#288676),(#288677,#288678),(#288679,#288680),(#288681,#288682),
(#288683,#288684),(#288685,#288686),(#288687,#288688),(#288689,#288690),
(#288691,#288692),(#288693,#288694),(#288695,#288696),(#288697,#288698),
(#288699,#288700),(#288701,#288702),(#288703,#288704),(#288705,#288706),
(#288707,#288708),(#288709,#288710),(#288711,#288712),(#288713,#288714),
(#288715,#288716),(#288717,#288718),(#288719,#288720),(#288721,#288722),
(#288723,#288724),(#288725,#288726),(#288727,#288728),(#288729,#288730),
(#288731,#288732),(#288733,#288734),(#288735,#288736),(#288737,#288738),
(#288739,#288740),(#288741,#288742),(#288743,#288744),(#288745,#288746),
(#288747,#288748),(#288749,#288750),(#288751,#288752),(#288753,#288754),
(#288755,#288756),(#288757,#288758),(#288759,#288760),(#288761,#288762),
(#288763,#288764),(#288765,#288766),(#288767,#288768),(#288769,#288770),
(#288771,#288772),(#288773,#288774),(#288775,#288776),(#288777,#288778),
(#288779,#288780),(#288781,#288782),(#288783,#288784),(#288785,#288786),
(#288787,#288788),(#288789,#288790),(#288791,#288792),(#288793,#288794),
(#288795,#288796),(#288797,#288798),(#288799,#288800),(#288801,#288802),
(#288803,#288804),(#288805,#288806),(#288807,#288808),(#288809,#288810),
(#288811,#288812),(#288813,#288814),(#288815,#288816),(#288817,#288818),
(#288819,#288820),(#288821,#288822),(#288823,#288824),(#288825,#288826),
(#288827,#288828),(#288829,#288830),(#288831,#288832),(#288833,#288834),
(#288835,#288836),(#288837,#288838),(#288839,#288840),(#288841,#288842),
(#288843,#288844),(#288845,#288846),(#288847,#288848),(#288849,#288850),
(#288851,#288852),(#288853,#288854),(#288855,#288856),(#288857,#288858),
(#288859,#288860),(#288861,#288862),(#288863,#288864),(#288865,#288866),
(#288867,#288868),(#288869,#288870),(#288871,#288872),(#288873,#288874),
(#288875,#288876),(#288877,#288878),(#288879,#288880),(#288881,#288882),
(#288883,#288884),(#288885,#288886),(#288887,#288888),(#288889,#288890),
(#288891,#288892),(#288893,#288894),(#288895,#288896),(#288897,#288898),
(#288899,#288900),(#288901,#288902),(#288903,#288904),(#288905,#288906),
(#288907,#288908),(#288909,#288910),(#288911,#288912),(#288913,#288914),
(#288915,#288916),(#288917,#288918),(#288919,#288920),(#288921,#288922),
(#288923,#288924),(#288925,#288926),(#288927,#288928),(#288929,#288930),
(#288931,#288932),(#288933,#288934),(#288935,#288936),(#288937,#288938),
(#288939,#288940),(#288941,#288942),(#288943,#288944),(#288945,#288946),
(#288947,#288948),(#288949,#288950),(#288951,#288952),(#288953,#288954),
(#288955,#288956),(#288957,#288958),(#288959,#288960),(#288961,#288962),
(#288963,#288964),(#288965,#288966),(#288967,#288968),(#288969,#288970),
(#288971,#288972),(#288973,#288974),(#288975,#288976),(#288977,#288978),
(#288979,#288980),(#288981,#288982),(#288983,#288984),(#288985,#288986),
(#288987,#288988),(#288989,#288990),(#288991,#288992),(#288993,#288994),
(#288995,#288996),(#288997,#288998),(#288999,#289000),(#289001,#289002),
(#289003,#289004),(#289005,#289006),(#289007,#289008),(#289009,#289010),
(#289011,#289012),(#289013,#289014),(#289015,#289016),(#289017,#289018),
(#289019,#289020),(#289021,#289022),(#289023,#289024),(#289025,#289026),
(#289027,#289028),(#289029,#289030),(#289031,#289032),(#289033,#289034),
(#289035,#289036),(#289037,#289038),(#289039,#289040),(#289041,#289042),
(#289043,#289044),(#289045,#289046),(#289047,#289048),(#289049,#289050),
(#289051,#289052),(#289053,#289054),(#289055,#289056),(#289057,#289058),
(#289059,#289060),(#289061,#289062),(#289063,#289064),(#289065,#289066),
(#289067,#289068),(#289069,#289070),(#289071,#289072),(#289073,#289074),
(#289075,#289076),(#289077,#289078),(#289079,#289080),(#289081,#289082),
(#289083,#289084),(#289085,#289086),(#289087,#289088),(#289089,#289090),
(#289091,#289092),(#289093,#289094),(#289095,#289096),(#289097,#289098),
(#289099,#289100),(#289101,#289102),(#289103,#289104),(#289105,#289106),
(#289107,#289108),(#289109,#289110),(#289111,#289112),(#289113,#289114),
(#289115,#289116),(#289117,#289118),(#289119,#289120),(#289121,#289122),
(#289123,#289124),(#289125,#289126),(#289127,#289128),(#289129,#289130),
(#289131,#289132),(#289133,#289134),(#289135,#289136),(#289137,#289138),
(#289139,#289140),(#289141,#289142),(#289143,#289144),(#289145,#289146),
(#289147,#289148),(#289149,#289150),(#289151,#289152),(#289153,#289154),
(#289155,#289156),(#289157,#289158),(#289159,#289160),(#289161,#289162),
(#289163,#289164),(#289165,#289166),(#289167,#289168),(#289169,#289170),
(#289171,#289172),(#289173,#289174),(#289175,#289176),(#289177,#289178),
(#289179,#289180),(#289181,#289182),(#289183,#289184),(#289185,#289186),
(#289187,#289188),(#289189,#289190),(#289191,#289192),(#289193,#289194),
(#289195,#289196),(#289197,#289198),(#289199,#289200),(#289201,#289202),
(#289203,#289204),(#289205,#289206),(#289207,#289208),(#289209,#289210),
(#289211,#289212),(#289213,#289214),(#289215,#289216),(#289217,#289218),
(#289219,#289220),(#289221,#289222),(#289223,#289224),(#289225,#289226),
(#289227,#289228),(#289229,#289230),(#289231,#289232),(#289233,#289234),
(#289235,#289236),(#289237,#289238),(#289239,#289240),(#289241,#289242),
(#289243,#289244),(#289245,#289246),(#289247,#289248),(#289249,#289250),
(#289251,#289252),(#289253,#289254),(#289255,#289256),(#289257,#289258),
(#289259,#289260),(#289261,#289262),(#289263,#289264),(#289265,#289266),
(#289267,#289268),(#289269,#289270),(#289271,#289272),(#289273,#289274),
(#289275,#289276),(#289277,#289278),(#289279,#289280),(#289281,#289282),
(#289283,#289284),(#289285,#289286),(#289287,#289288),(#289289,#289290),
(#289291,#289292),(#289293,#289294),(#289295,#289296),(#289297,#289298),
(#289299,#289300),(#289301,#289302),(#289303,#289304),(#289305,#289306),
(#289307,#289308),(#289309,#289310),(#289311,#289312),(#289313,#289314),
(#289315,#289316),(#289317,#289318),(#289319,#289320),(#289321,#289322),
(#289323,#289324),(#289325,#289326),(#289327,#289328),(#289329,#289330),
(#289331,#289332),(#289333,#289334),(#289335,#289336),(#289337,#289338),
(#289339,#289340),(#289341,#289342),(#289343,#289344),(#289345,#289346),
(#289347,#289348),(#289349,#289350),(#289351,#289352),(#289353,#289354),
(#289355,#289356),(#289357,#289358),(#289359,#289360),(#289361,#289362),
(#289363,#289364),(#289365,#289366),(#289367,#289368),(#289369,#289370),
(#289371,#289372),(#289373,#289374)),.UNSPECIFIED.,.F.,.F.,.F.,(6,1,1,1,
1,1,1,1,1,1,1,1,1,1,1,1,1,1,1,1,1,1,1,1,1,1,1,1,1,1,1,1,1,1,1,1,1,1,1,1,
1,1,1,1,1,1,1,1,1,1,1,1,1,1,1,1,1,1,1,1,1,1,1,1,1,1,1,1,1,1,1,1,1,1,1,1,
1,1,1,1,1,1,1,1,1,1,1,1,1,1,1,1,1,1,1,1,1,1,1,1,1,1,1,1,1,1,1,1,1,1,1,1,
1,1,1,1,1,1,1,1,1,1,1,1,1,1,1,1,1,1,1,1,1,1,1,1,1,1,1,1,1,1,1,1,1,1,1,1,
1,1,1,1,1,1,1,1,1,1,1,1,1,1,1,1,1,1,1,1,1,1,1,1,1,1,1,1,1,1,1,1,1,1,1,1,
1,1,1,1,1,1,1,1,1,1,1,1,1,1,1,1,1,1,1,1,1,1,1,1,1,1,1,1,1,1,1,1,1,1,1,1,
1,1,1,1,1,1,1,1,1,1,1,1,1,1,1,1,1,1,1,1,1,1,1,1,1,1,1,1,1,1,1,1,1,1,1,1,
1,1,1,1,1,1,1,1,1,1,1,1,1,1,1,1,1,1,1,1,1,1,1,1,1,1,1,1,1,1,1,1,1,1,1,1,
1,1,1,1,1,1,1,1,1,1,1,1,1,1,1,1,1,1,1,1,1,1,1,1,1,1,1,1,1,1,1,1,1,1,1,1,
1,1,1,1,1,1,1,1,1,1,1,1,1,1,1,1,1,1,1,1,1,1,1,1,1,1,1,1,1,1,1,1,1,1,1,1,
1,1,1,1,1,1,1,1,1,1,1,1,1,1,1,1,1,1,1,1,1,1,1,1,1,1,1,1,1,1,1,1,1,1,1,1,
1,1,1,1,1,1,1,1,1,1,1,1,1,1,1,1,1,1,1,1,1,1,1,1,1,1,1,1,1,1,1,1,1,1,1,1,
1,1,1,1,1,1,1,1,1,1,1,1,1,1,1,1,1,1,1,1,1,1,1,1,1,1,1,1,1,1,1,6),(2,2),
(-1.,-0.998165138,-0.996330275,-0.994495413,-0.99266055,-0.990825688,-0.988990826,
-0.987155963,-0.985321101,-0.983486239,-0.981651376,-0.979816514,-0.977981651,
-0.976146789,-0.974311927,-0.972477064,-0.970642202,-0.968807339,-0.966972477,
-0.965137615,-0.963302752,-0.96146789,-0.959633028,-0.957798165,-0.955963303,
-0.95412844,-0.952293578,-0.950458716,-0.948623853,-0.946788991,-0.944954128,
-0.943119266,-0.941284404,-0.939449541,-0.937614679,-0.935779817,-0.933944954,
-0.932110092,-0.930275229,-0.928440367,-0.926605505,-0.924770642,-0.92293578,
-0.921100917,-0.919266055,-0.917431193,-0.91559633,-0.913761468,-0.911926606,
-0.910091743,-0.908256881,-0.906422018,-0.904587156,-0.902752294,-0.900917431,
-0.899082569,-0.897247706,-0.895412844,-0.893577982,-0.891743119,-0.889908257,
-0.888073394,-0.886238532,-0.88440367,-0.882568807,-0.880733945,-0.878899083,
-0.87706422,-0.875229358,-0.873394495,-0.871559633,-0.869724771,-0.867889908,
-0.866055046,-0.864220183,-0.862385321,-0.860550459,-0.858715596,-0.856880734,
-0.855045872,-0.853211009,-0.851376147,-0.849541284,-0.847706422,-0.84587156,
-0.844036697,-0.842201835,-0.840366972,-0.83853211,-0.836697248,-0.834862385,
-0.833027523,-0.831192661,-0.829357798,-0.827522936,-0.825688073,-0.823853211,
-0.822018349,-0.820183486,-0.818348624,-0.816513761,-0.814678899,-0.812844037,
-0.811009174,-0.809174312,-0.80733945,-0.805504587,-0.803669725,-0.801834862,
-0.8,-0.798165138,-0.796330275,-0.794495413,-0.79266055,-0.790825688,-0.788990826,
-0.787155963,-0.785321101,-0.783486239,-0.781651376,-0.779816514,-0.777981651,
-0.776146789,-0.774311927,-0.772477064,-0.770642202,-0.768807339,-0.766972477,
-0.765137615,-0.763302752,-0.76146789,-0.759633028,-0.757798165,-0.755963303,
-0.75412844,-0.752293578,-0.750458716,-0.748623853,-0.746788991,-0.744954128,
-0.743119266,-0.741284404,-0.739449541,-0.737614679,-0.735779817,-0.733944954,
-0.732110092,-0.730275229,-0.728440367,-0.726605505,-0.724770642,-0.72293578,
-0.721100917,-0.719266055,-0.717431193,-0.71559633,-0.713761468,-0.711926606,
-0.710091743,-0.708256881,-0.706422018,-0.704587156,-0.702752294,-0.700917431,
-0.699082569,-0.697247706,-0.695412844,-0.693577982,-0.691743119,-0.689908257,
-0.688073394,-0.686238532,-0.68440367,-0.682568807,-0.680733945,-0.678899083,
-0.67706422,-0.675229358,-0.673394495,-0.671559633,-0.669724771,-0.667889908,
-0.666055046,-0.664220183,-0.662385321,-0.660550459,-0.658715596,-0.656880734,
-0.655045872,-0.653211009,-0.651376147,-0.649541284,-0.647706422,-0.64587156,
-0.644036697,-0.642201835,-0.640366972,-0.63853211,-0.636697248,-0.634862385,
-0.633027523,-0.631192661,-0.629357798,-0.627522936,-0.625688073,-0.623853211,
-0.622018349,-0.620183486,-0.618348624,-0.616513761,-0.614678899,-0.612844037,
-0.611009174,-0.609174312,-0.60733945,-0.605504587,-0.603669725,-0.601834862,
-0.6,-0.598165138,-0.596330275,-0.594495413,-0.59266055,-0.590825688,-0.588990826,
-0.587155963,-0.585321101,-0.583486239,-0.581651376,-0.579816514,-0.577981651,
-0.576146789,-0.574311927,-0.572477064,-0.570642202,-0.568807339,-0.566972477,
-0.565137615,-0.563302752,-0.56146789,-0.559633028,-0.557798165,-0.555963303,
-0.55412844,-0.552293578,-0.550458716,-0.548623853,-0.546788991,-0.544954128,
-0.543119266,-0.541284404,-0.539449541,-0.537614679,-0.535779817,-0.533944954,
-0.532110092,-0.530275229,-0.528440367,-0.526605505,-0.524770642,-0.52293578,
-0.521100917,-0.519266055,-0.517431193,-0.51559633,-0.513761468,-0.511926606,
-0.510091743,-0.508256881,-0.506422018,-0.504587156,-0.502752294,-0.500917431,
-0.499082569,-0.497247706,-0.495412844,-0.493577982,-0.491743119,-0.489908257,
-0.488073394,-0.486238532,-0.48440367,-0.482568807,-0.480733945,-0.478899083,
-0.47706422,-0.475229358,-0.473394495,-0.471559633,-0.469724771,-0.467889908,
-0.466055046,-0.464220183,-0.462385321,-0.460550459,-0.458715596,-0.456880734,
-0.455045872,-0.453211009,-0.451376147,-0.449541284,-0.447706422,-0.44587156,
-0.444036697,-0.442201835,-0.440366972,-0.43853211,-0.436697248,-0.434862385,
-0.433027523,-0.431192661,-0.429357798,-0.427522936,-0.425688073,-0.423853211,
-0.422018349,-0.420183486,-0.418348624,-0.416513761,-0.414678899,-0.412844037,
-0.411009174,-0.409174312,-0.40733945,-0.405504587,-0.403669725,-0.401834862,
-0.4,-0.398165138,-0.396330275,-0.394495413,-0.39266055,-0.390825688,-0.388990826,
-0.387155963,-0.385321101,-0.383486239,-0.381651376,-0.379816514,-0.377981651,
-0.376146789,-0.374311927,-0.372477064,-0.370642202,-0.368807339,-0.366972477,
-0.365137615,-0.363302752,-0.36146789,-0.359633028,-0.357798165,-0.355963303,
-0.35412844,-0.352293578,-0.350458716,-0.348623853,-0.346788991,-0.344954128,
-0.343119266,-0.341284404,-0.339449541,-0.337614679,-0.335779817,-0.333944954,
-0.332110092,-0.330275229,-0.328440367,-0.326605505,-0.324770642,-0.32293578,
-0.321100917,-0.319266055,-0.317431193,-0.31559633,-0.313761468,-0.311926606,
-0.310091743,-0.308256881,-0.306422018,-0.304587156,-0.302752294,-0.300917431,
-0.299082569,-0.297247706,-0.295412844,-0.293577982,-0.291743119,-0.289908257,
-0.288073394,-0.286238532,-0.28440367,-0.282568807,-0.280733945,-0.278899083,
-0.27706422,-0.275229358,-0.273394495,-0.271559633,-0.269724771,-0.267889908,
-0.266055046,-0.264220183,-0.262385321,-0.260550459,-0.258715596,-0.256880734,
-0.255045872,-0.253211009,-0.251376147,-0.249541284,-0.247706422,-0.24587156,
-0.244036697,-0.242201835,-0.240366972,-0.23853211,-0.236697248,-0.234862385,
-0.233027523,-0.231192661,-0.229357798,-0.227522936,-0.225688073,-0.223853211,
-0.222018349,-0.220183486,-0.218348624,-0.216513761,-0.214678899,-0.212844037,
-0.211009174,-0.209174312,-0.20733945,-0.205504587,-0.203669725,-0.201834862,
-0.2,-0.198165138,-0.196330275,-0.194495413,-0.19266055,-0.190825688,-0.188990826,
-0.187155963,-0.185321101,-0.183486239,-0.181651376,-0.179816514,-0.177981651,
-0.176146789,-0.174311927,-0.172477064,-0.170642202,-0.168807339,-0.166972477,
-0.165137615,-0.163302752,-0.16146789,-0.159633028,-0.157798165,-0.155963303,
-0.15412844,-0.152293578,-0.150458716,-0.148623853,-0.146788991,-0.144954128,
-0.143172103),(0.,0.36),.UNSPECIFIED.);
#6297=B_SPLINE_SURFACE_WITH_KNOTS('',5,1,((#290040,#290041),(#290042,#290043),
(#290044,#290045),(#290046,#290047),(#290048,#290049),(#290050,#290051),
(#290052,#290053),(#290054,#290055),(#290056,#290057),(#290058,#290059),
(#290060,#290061),(#290062,#290063),(#290064,#290065),(#290066,#290067),
(#290068,#290069),(#290070,#290071),(#290072,#290073),(#290074,#290075),
(#290076,#290077),(#290078,#290079),(#290080,#290081),(#290082,#290083),
(#290084,#290085),(#290086,#290087),(#290088,#290089),(#290090,#290091),
(#290092,#290093),(#290094,#290095),(#290096,#290097),(#290098,#290099),
(#290100,#290101),(#290102,#290103),(#290104,#290105),(#290106,#290107),
(#290108,#290109),(#290110,#290111),(#290112,#290113),(#290114,#290115),
(#290116,#290117),(#290118,#290119),(#290120,#290121),(#290122,#290123),
(#290124,#290125),(#290126,#290127),(#290128,#290129),(#290130,#290131),
(#290132,#290133),(#290134,#290135),(#290136,#290137),(#290138,#290139),
(#290140,#290141),(#290142,#290143),(#290144,#290145),(#290146,#290147),
(#290148,#290149),(#290150,#290151),(#290152,#290153),(#290154,#290155),
(#290156,#290157),(#290158,#290159),(#290160,#290161),(#290162,#290163),
(#290164,#290165),(#290166,#290167),(#290168,#290169),(#290170,#290171),
(#290172,#290173),(#290174,#290175),(#290176,#290177),(#290178,#290179),
(#290180,#290181),(#290182,#290183),(#290184,#290185),(#290186,#290187),
(#290188,#290189),(#290190,#290191),(#290192,#290193),(#290194,#290195),
(#290196,#290197),(#290198,#290199),(#290200,#290201),(#290202,#290203),
(#290204,#290205),(#290206,#290207),(#290208,#290209),(#290210,#290211),
(#290212,#290213),(#290214,#290215),(#290216,#290217),(#290218,#290219),
(#290220,#290221),(#290222,#290223),(#290224,#290225),(#290226,#290227),
(#290228,#290229),(#290230,#290231),(#290232,#290233),(#290234,#290235),
(#290236,#290237),(#290238,#290239),(#290240,#290241),(#290242,#290243),
(#290244,#290245),(#290246,#290247),(#290248,#290249),(#290250,#290251),
(#290252,#290253),(#290254,#290255),(#290256,#290257),(#290258,#290259),
(#290260,#290261),(#290262,#290263),(#290264,#290265),(#290266,#290267),
(#290268,#290269),(#290270,#290271),(#290272,#290273),(#290274,#290275),
(#290276,#290277),(#290278,#290279),(#290280,#290281),(#290282,#290283),
(#290284,#290285),(#290286,#290287),(#290288,#290289),(#290290,#290291),
(#290292,#290293),(#290294,#290295),(#290296,#290297),(#290298,#290299),
(#290300,#290301),(#290302,#290303),(#290304,#290305),(#290306,#290307),
(#290308,#290309),(#290310,#290311),(#290312,#290313),(#290314,#290315),
(#290316,#290317),(#290318,#290319),(#290320,#290321),(#290322,#290323),
(#290324,#290325),(#290326,#290327),(#290328,#290329),(#290330,#290331),
(#290332,#290333),(#290334,#290335),(#290336,#290337),(#290338,#290339),
(#290340,#290341),(#290342,#290343),(#290344,#290345),(#290346,#290347),
(#290348,#290349),(#290350,#290351),(#290352,#290353),(#290354,#290355),
(#290356,#290357),(#290358,#290359),(#290360,#290361),(#290362,#290363),
(#290364,#290365),(#290366,#290367),(#290368,#290369),(#290370,#290371),
(#290372,#290373),(#290374,#290375),(#290376,#290377),(#290378,#290379),
(#290380,#290381),(#290382,#290383),(#290384,#290385),(#290386,#290387),
(#290388,#290389),(#290390,#290391),(#290392,#290393),(#290394,#290395),
(#290396,#290397),(#290398,#290399),(#290400,#290401),(#290402,#290403),
(#290404,#290405),(#290406,#290407),(#290408,#290409),(#290410,#290411),
(#290412,#290413),(#290414,#290415),(#290416,#290417),(#290418,#290419),
(#290420,#290421),(#290422,#290423),(#290424,#290425),(#290426,#290427),
(#290428,#290429),(#290430,#290431),(#290432,#290433),(#290434,#290435),
(#290436,#290437),(#290438,#290439),(#290440,#290441),(#290442,#290443),
(#290444,#290445),(#290446,#290447),(#290448,#290449),(#290450,#290451),
(#290452,#290453),(#290454,#290455),(#290456,#290457),(#290458,#290459),
(#290460,#290461),(#290462,#290463),(#290464,#290465),(#290466,#290467),
(#290468,#290469),(#290470,#290471),(#290472,#290473),(#290474,#290475),
(#290476,#290477),(#290478,#290479),(#290480,#290481),(#290482,#290483),
(#290484,#290485),(#290486,#290487),(#290488,#290489),(#290490,#290491),
(#290492,#290493),(#290494,#290495),(#290496,#290497),(#290498,#290499),
(#290500,#290501),(#290502,#290503),(#290504,#290505),(#290506,#290507),
(#290508,#290509),(#290510,#290511),(#290512,#290513),(#290514,#290515),
(#290516,#290517),(#290518,#290519),(#290520,#290521),(#290522,#290523),
(#290524,#290525),(#290526,#290527),(#290528,#290529),(#290530,#290531),
(#290532,#290533),(#290534,#290535),(#290536,#290537),(#290538,#290539),
(#290540,#290541),(#290542,#290543),(#290544,#290545),(#290546,#290547),
(#290548,#290549),(#290550,#290551),(#290552,#290553),(#290554,#290555),
(#290556,#290557),(#290558,#290559),(#290560,#290561),(#290562,#290563),
(#290564,#290565),(#290566,#290567),(#290568,#290569),(#290570,#290571),
(#290572,#290573),(#290574,#290575),(#290576,#290577),(#290578,#290579),
(#290580,#290581),(#290582,#290583),(#290584,#290585),(#290586,#290587),
(#290588,#290589),(#290590,#290591),(#290592,#290593),(#290594,#290595),
(#290596,#290597),(#290598,#290599),(#290600,#290601),(#290602,#290603),
(#290604,#290605),(#290606,#290607),(#290608,#290609),(#290610,#290611),
(#290612,#290613),(#290614,#290615),(#290616,#290617),(#290618,#290619),
(#290620,#290621),(#290622,#290623),(#290624,#290625),(#290626,#290627),
(#290628,#290629),(#290630,#290631),(#290632,#290633),(#290634,#290635),
(#290636,#290637),(#290638,#290639),(#290640,#290641),(#290642,#290643),
(#290644,#290645),(#290646,#290647),(#290648,#290649),(#290650,#290651),
(#290652,#290653),(#290654,#290655),(#290656,#290657),(#290658,#290659),
(#290660,#290661),(#290662,#290663),(#290664,#290665),(#290666,#290667),
(#290668,#290669),(#290670,#290671),(#290672,#290673),(#290674,#290675),
(#290676,#290677),(#290678,#290679),(#290680,#290681),(#290682,#290683),
(#290684,#290685),(#290686,#290687),(#290688,#290689),(#290690,#290691),
(#290692,#290693),(#290694,#290695),(#290696,#290697),(#290698,#290699),
(#290700,#290701),(#290702,#290703),(#290704,#290705),(#290706,#290707),
(#290708,#290709),(#290710,#290711),(#290712,#290713),(#290714,#290715),
(#290716,#290717),(#290718,#290719),(#290720,#290721),(#290722,#290723),
(#290724,#290725),(#290726,#290727),(#290728,#290729),(#290730,#290731),
(#290732,#290733),(#290734,#290735),(#290736,#290737),(#290738,#290739),
(#290740,#290741),(#290742,#290743),(#290744,#290745),(#290746,#290747),
(#290748,#290749),(#290750,#290751),(#290752,#290753),(#290754,#290755),
(#290756,#290757),(#290758,#290759),(#290760,#290761),(#290762,#290763),
(#290764,#290765),(#290766,#290767),(#290768,#290769),(#290770,#290771),
(#290772,#290773),(#290774,#290775),(#290776,#290777),(#290778,#290779),
(#290780,#290781),(#290782,#290783),(#290784,#290785),(#290786,#290787),
(#290788,#290789),(#290790,#290791),(#290792,#290793),(#290794,#290795),
(#290796,#290797),(#290798,#290799),(#290800,#290801),(#290802,#290803),
(#290804,#290805),(#290806,#290807),(#290808,#290809),(#290810,#290811),
(#290812,#290813),(#290814,#290815),(#290816,#290817),(#290818,#290819),
(#290820,#290821),(#290822,#290823),(#290824,#290825),(#290826,#290827),
(#290828,#290829),(#290830,#290831),(#290832,#290833),(#290834,#290835),
(#290836,#290837),(#290838,#290839),(#290840,#290841),(#290842,#290843),
(#290844,#290845),(#290846,#290847),(#290848,#290849),(#290850,#290851),
(#290852,#290853),(#290854,#290855),(#290856,#290857),(#290858,#290859),
(#290860,#290861),(#290862,#290863),(#290864,#290865),(#290866,#290867),
(#290868,#290869),(#290870,#290871),(#290872,#290873),(#290874,#290875),
(#290876,#290877),(#290878,#290879),(#290880,#290881),(#290882,#290883),
(#290884,#290885),(#290886,#290887),(#290888,#290889),(#290890,#290891),
(#290892,#290893),(#290894,#290895),(#290896,#290897),(#290898,#290899),
(#290900,#290901),(#290902,#290903),(#290904,#290905),(#290906,#290907),
(#290908,#290909),(#290910,#290911),(#290912,#290913),(#290914,#290915),
(#290916,#290917),(#290918,#290919),(#290920,#290921),(#290922,#290923),
(#290924,#290925),(#290926,#290927),(#290928,#290929),(#290930,#290931),
(#290932,#290933),(#290934,#290935),(#290936,#290937),(#290938,#290939),
(#290940,#290941),(#290942,#290943),(#290944,#290945),(#290946,#290947),
(#290948,#290949),(#290950,#290951),(#290952,#290953),(#290954,#290955),
(#290956,#290957),(#290958,#290959),(#290960,#290961),(#290962,#290963),
(#290964,#290965),(#290966,#290967),(#290968,#290969),(#290970,#290971),
(#290972,#290973),(#290974,#290975),(#290976,#290977),(#290978,#290979),
(#290980,#290981),(#290982,#290983)),.UNSPECIFIED.,.F.,.F.,.F.,(6,1,1,1,
1,1,1,1,1,1,1,1,1,1,1,1,1,1,1,1,1,1,1,1,1,1,1,1,1,1,1,1,1,1,1,1,1,1,1,1,
1,1,1,1,1,1,1,1,1,1,1,1,1,1,1,1,1,1,1,1,1,1,1,1,1,1,1,1,1,1,1,1,1,1,1,1,
1,1,1,1,1,1,1,1,1,1,1,1,1,1,1,1,1,1,1,1,1,1,1,1,1,1,1,1,1,1,1,1,1,1,1,1,
1,1,1,1,1,1,1,1,1,1,1,1,1,1,1,1,1,1,1,1,1,1,1,1,1,1,1,1,1,1,1,1,1,1,1,1,
1,1,1,1,1,1,1,1,1,1,1,1,1,1,1,1,1,1,1,1,1,1,1,1,1,1,1,1,1,1,1,1,1,1,1,1,
1,1,1,1,1,1,1,1,1,1,1,1,1,1,1,1,1,1,1,1,1,1,1,1,1,1,1,1,1,1,1,1,1,1,1,1,
1,1,1,1,1,1,1,1,1,1,1,1,1,1,1,1,1,1,1,1,1,1,1,1,1,1,1,1,1,1,1,1,1,1,1,1,
1,1,1,1,1,1,1,1,1,1,1,1,1,1,1,1,1,1,1,1,1,1,1,1,1,1,1,1,1,1,1,1,1,1,1,1,
1,1,1,1,1,1,1,1,1,1,1,1,1,1,1,1,1,1,1,1,1,1,1,1,1,1,1,1,1,1,1,1,1,1,1,1,
1,1,1,1,1,1,1,1,1,1,1,1,1,1,1,1,1,1,1,1,1,1,1,1,1,1,1,1,1,1,1,1,1,1,1,1,
1,1,1,1,1,1,1,1,1,1,1,1,1,1,1,1,1,1,1,1,1,1,1,1,1,1,1,1,1,1,1,1,1,1,1,1,
1,1,1,1,1,1,1,1,1,1,1,1,1,1,1,1,1,1,1,1,1,1,1,1,1,1,1,1,1,1,1,1,1,1,1,1,
1,1,1,1,1,1,1,1,1,1,1,1,1,1,1,1,1,1,1,1,1,1,1,1,1,1,1,1,1,1,1,6),(2,2),
(-1.,-0.998165138,-0.996330275,-0.994495413,-0.99266055,-0.990825688,-0.988990826,
-0.987155963,-0.985321101,-0.983486239,-0.981651376,-0.979816514,-0.977981651,
-0.976146789,-0.974311927,-0.972477064,-0.970642202,-0.968807339,-0.966972477,
-0.965137615,-0.963302752,-0.96146789,-0.959633028,-0.957798165,-0.955963303,
-0.95412844,-0.952293578,-0.950458716,-0.948623853,-0.946788991,-0.944954128,
-0.943119266,-0.941284404,-0.939449541,-0.937614679,-0.935779817,-0.933944954,
-0.932110092,-0.930275229,-0.928440367,-0.926605505,-0.924770642,-0.92293578,
-0.921100917,-0.919266055,-0.917431193,-0.91559633,-0.913761468,-0.911926606,
-0.910091743,-0.908256881,-0.906422018,-0.904587156,-0.902752294,-0.900917431,
-0.899082569,-0.897247706,-0.895412844,-0.893577982,-0.891743119,-0.889908257,
-0.888073394,-0.886238532,-0.88440367,-0.882568807,-0.880733945,-0.878899083,
-0.87706422,-0.875229358,-0.873394495,-0.871559633,-0.869724771,-0.867889908,
-0.866055046,-0.864220183,-0.862385321,-0.860550459,-0.858715596,-0.856880734,
-0.855045872,-0.853211009,-0.851376147,-0.849541284,-0.847706422,-0.84587156,
-0.844036697,-0.842201835,-0.840366972,-0.83853211,-0.836697248,-0.834862385,
-0.833027523,-0.831192661,-0.829357798,-0.827522936,-0.825688073,-0.823853211,
-0.822018349,-0.820183486,-0.818348624,-0.816513761,-0.814678899,-0.812844037,
-0.811009174,-0.809174312,-0.80733945,-0.805504587,-0.803669725,-0.801834862,
-0.8,-0.798165138,-0.796330275,-0.794495413,-0.79266055,-0.790825688,-0.788990826,
-0.787155963,-0.785321101,-0.783486239,-0.781651376,-0.779816514,-0.777981651,
-0.776146789,-0.774311927,-0.772477064,-0.770642202,-0.768807339,-0.766972477,
-0.765137615,-0.763302752,-0.76146789,-0.759633028,-0.757798165,-0.755963303,
-0.75412844,-0.752293578,-0.750458716,-0.748623853,-0.746788991,-0.744954128,
-0.743119266,-0.741284404,-0.739449541,-0.737614679,-0.735779817,-0.733944954,
-0.732110092,-0.730275229,-0.728440367,-0.726605505,-0.724770642,-0.72293578,
-0.721100917,-0.719266055,-0.717431193,-0.71559633,-0.713761468,-0.711926606,
-0.710091743,-0.708256881,-0.706422018,-0.704587156,-0.702752294,-0.700917431,
-0.699082569,-0.697247706,-0.695412844,-0.693577982,-0.691743119,-0.689908257,
-0.688073394,-0.686238532,-0.68440367,-0.682568807,-0.680733945,-0.678899083,
-0.67706422,-0.675229358,-0.673394495,-0.671559633,-0.669724771,-0.667889908,
-0.666055046,-0.664220183,-0.662385321,-0.660550459,-0.658715596,-0.656880734,
-0.655045872,-0.653211009,-0.651376147,-0.649541284,-0.647706422,-0.64587156,
-0.644036697,-0.642201835,-0.640366972,-0.63853211,-0.636697248,-0.634862385,
-0.633027523,-0.631192661,-0.629357798,-0.627522936,-0.625688073,-0.623853211,
-0.622018349,-0.620183486,-0.618348624,-0.616513761,-0.614678899,-0.612844037,
-0.611009174,-0.609174312,-0.60733945,-0.605504587,-0.603669725,-0.601834862,
-0.6,-0.598165138,-0.596330275,-0.594495413,-0.59266055,-0.590825688,-0.588990826,
-0.587155963,-0.585321101,-0.583486239,-0.581651376,-0.579816514,-0.577981651,
-0.576146789,-0.574311927,-0.572477064,-0.570642202,-0.568807339,-0.566972477,
-0.565137615,-0.563302752,-0.56146789,-0.559633028,-0.557798165,-0.555963303,
-0.55412844,-0.552293578,-0.550458716,-0.548623853,-0.546788991,-0.544954128,
-0.543119266,-0.541284404,-0.539449541,-0.537614679,-0.535779817,-0.533944954,
-0.532110092,-0.530275229,-0.528440367,-0.526605505,-0.524770642,-0.52293578,
-0.521100917,-0.519266055,-0.517431193,-0.51559633,-0.513761468,-0.511926606,
-0.510091743,-0.508256881,-0.506422018,-0.504587156,-0.502752294,-0.500917431,
-0.499082569,-0.497247706,-0.495412844,-0.493577982,-0.491743119,-0.489908257,
-0.488073394,-0.486238532,-0.48440367,-0.482568807,-0.480733945,-0.478899083,
-0.47706422,-0.475229358,-0.473394495,-0.471559633,-0.469724771,-0.467889908,
-0.466055046,-0.464220183,-0.462385321,-0.460550459,-0.458715596,-0.456880734,
-0.455045872,-0.453211009,-0.451376147,-0.449541284,-0.447706422,-0.44587156,
-0.444036697,-0.442201835,-0.440366972,-0.43853211,-0.436697248,-0.434862385,
-0.433027523,-0.431192661,-0.429357798,-0.427522936,-0.425688073,-0.423853211,
-0.422018349,-0.420183486,-0.418348624,-0.416513761,-0.414678899,-0.412844037,
-0.411009174,-0.409174312,-0.40733945,-0.405504587,-0.403669725,-0.401834862,
-0.4,-0.398165138,-0.396330275,-0.394495413,-0.39266055,-0.390825688,-0.388990826,
-0.387155963,-0.385321101,-0.383486239,-0.381651376,-0.379816514,-0.377981651,
-0.376146789,-0.374311927,-0.372477064,-0.370642202,-0.368807339,-0.366972477,
-0.365137615,-0.363302752,-0.36146789,-0.359633028,-0.357798165,-0.355963303,
-0.35412844,-0.352293578,-0.350458716,-0.348623853,-0.346788991,-0.344954128,
-0.343119266,-0.341284404,-0.339449541,-0.337614679,-0.335779817,-0.333944954,
-0.332110092,-0.330275229,-0.328440367,-0.326605505,-0.324770642,-0.32293578,
-0.321100917,-0.319266055,-0.317431193,-0.31559633,-0.313761468,-0.311926606,
-0.310091743,-0.308256881,-0.306422018,-0.304587156,-0.302752294,-0.300917431,
-0.299082569,-0.297247706,-0.295412844,-0.293577982,-0.291743119,-0.289908257,
-0.288073394,-0.286238532,-0.28440367,-0.282568807,-0.280733945,-0.278899083,
-0.27706422,-0.275229358,-0.273394495,-0.271559633,-0.269724771,-0.267889908,
-0.266055046,-0.264220183,-0.262385321,-0.260550459,-0.258715596,-0.256880734,
-0.255045872,-0.253211009,-0.251376147,-0.249541284,-0.247706422,-0.24587156,
-0.244036697,-0.242201835,-0.240366972,-0.23853211,-0.236697248,-0.234862385,
-0.233027523,-0.231192661,-0.229357798,-0.227522936,-0.225688073,-0.223853211,
-0.222018349,-0.220183486,-0.218348624,-0.216513761,-0.214678899,-0.212844037,
-0.211009174,-0.209174312,-0.20733945,-0.205504587,-0.203669725,-0.201834862,
-0.2,-0.198165138,-0.196330275,-0.194495413,-0.19266055,-0.190825688,-0.188990826,
-0.187155963,-0.185321101,-0.183486239,-0.181651376,-0.179816514,-0.177981651,
-0.176146789,-0.174311927,-0.172477064,-0.170642202,-0.168807339,-0.166972477,
-0.165137615,-0.163302752,-0.16146789,-0.159633028,-0.157798165,-0.155963303,
-0.15412844,-0.152293578,-0.150458716,-0.148623853,-0.146788991,-0.144954128,
-0.143172103),(0.,0.36),.UNSPECIFIED.);
#6298=B_SPLINE_SURFACE_WITH_KNOTS('',5,1,((#291634,#291635),(#291636,#291637),
(#291638,#291639),(#291640,#291641),(#291642,#291643),(#291644,#291645),
(#291646,#291647),(#291648,#291649),(#291650,#291651),(#291652,#291653),
(#291654,#291655),(#291656,#291657),(#291658,#291659),(#291660,#291661),
(#291662,#291663),(#291664,#291665),(#291666,#291667),(#291668,#291669),
(#291670,#291671),(#291672,#291673),(#291674,#291675),(#291676,#291677),
(#291678,#291679),(#291680,#291681),(#291682,#291683),(#291684,#291685),
(#291686,#291687),(#291688,#291689),(#291690,#291691),(#291692,#291693),
(#291694,#291695),(#291696,#291697),(#291698,#291699),(#291700,#291701),
(#291702,#291703),(#291704,#291705),(#291706,#291707),(#291708,#291709),
(#291710,#291711),(#291712,#291713),(#291714,#291715),(#291716,#291717),
(#291718,#291719),(#291720,#291721),(#291722,#291723),(#291724,#291725),
(#291726,#291727),(#291728,#291729),(#291730,#291731),(#291732,#291733),
(#291734,#291735),(#291736,#291737),(#291738,#291739),(#291740,#291741),
(#291742,#291743),(#291744,#291745),(#291746,#291747),(#291748,#291749),
(#291750,#291751),(#291752,#291753),(#291754,#291755),(#291756,#291757),
(#291758,#291759),(#291760,#291761),(#291762,#291763),(#291764,#291765),
(#291766,#291767),(#291768,#291769),(#291770,#291771),(#291772,#291773),
(#291774,#291775),(#291776,#291777),(#291778,#291779),(#291780,#291781),
(#291782,#291783),(#291784,#291785),(#291786,#291787),(#291788,#291789),
(#291790,#291791),(#291792,#291793),(#291794,#291795),(#291796,#291797),
(#291798,#291799),(#291800,#291801),(#291802,#291803),(#291804,#291805),
(#291806,#291807),(#291808,#291809),(#291810,#291811),(#291812,#291813),
(#291814,#291815),(#291816,#291817),(#291818,#291819),(#291820,#291821),
(#291822,#291823),(#291824,#291825),(#291826,#291827),(#291828,#291829),
(#291830,#291831),(#291832,#291833),(#291834,#291835),(#291836,#291837),
(#291838,#291839),(#291840,#291841),(#291842,#291843),(#291844,#291845),
(#291846,#291847),(#291848,#291849),(#291850,#291851),(#291852,#291853),
(#291854,#291855),(#291856,#291857),(#291858,#291859),(#291860,#291861),
(#291862,#291863),(#291864,#291865),(#291866,#291867),(#291868,#291869),
(#291870,#291871),(#291872,#291873),(#291874,#291875),(#291876,#291877),
(#291878,#291879),(#291880,#291881),(#291882,#291883),(#291884,#291885),
(#291886,#291887),(#291888,#291889),(#291890,#291891),(#291892,#291893),
(#291894,#291895),(#291896,#291897),(#291898,#291899),(#291900,#291901),
(#291902,#291903),(#291904,#291905),(#291906,#291907),(#291908,#291909),
(#291910,#291911),(#291912,#291913),(#291914,#291915),(#291916,#291917),
(#291918,#291919),(#291920,#291921),(#291922,#291923),(#291924,#291925),
(#291926,#291927),(#291928,#291929),(#291930,#291931),(#291932,#291933),
(#291934,#291935),(#291936,#291937),(#291938,#291939),(#291940,#291941),
(#291942,#291943),(#291944,#291945),(#291946,#291947),(#291948,#291949),
(#291950,#291951),(#291952,#291953),(#291954,#291955),(#291956,#291957),
(#291958,#291959),(#291960,#291961),(#291962,#291963),(#291964,#291965),
(#291966,#291967),(#291968,#291969),(#291970,#291971),(#291972,#291973),
(#291974,#291975),(#291976,#291977),(#291978,#291979),(#291980,#291981),
(#291982,#291983),(#291984,#291985),(#291986,#291987),(#291988,#291989),
(#291990,#291991),(#291992,#291993),(#291994,#291995),(#291996,#291997),
(#291998,#291999),(#292000,#292001),(#292002,#292003),(#292004,#292005),
(#292006,#292007),(#292008,#292009),(#292010,#292011),(#292012,#292013),
(#292014,#292015),(#292016,#292017),(#292018,#292019),(#292020,#292021),
(#292022,#292023),(#292024,#292025),(#292026,#292027),(#292028,#292029),
(#292030,#292031),(#292032,#292033),(#292034,#292035),(#292036,#292037),
(#292038,#292039),(#292040,#292041),(#292042,#292043),(#292044,#292045),
(#292046,#292047),(#292048,#292049),(#292050,#292051),(#292052,#292053),
(#292054,#292055),(#292056,#292057),(#292058,#292059),(#292060,#292061),
(#292062,#292063),(#292064,#292065),(#292066,#292067),(#292068,#292069),
(#292070,#292071),(#292072,#292073),(#292074,#292075),(#292076,#292077),
(#292078,#292079),(#292080,#292081),(#292082,#292083),(#292084,#292085),
(#292086,#292087),(#292088,#292089),(#292090,#292091),(#292092,#292093),
(#292094,#292095),(#292096,#292097),(#292098,#292099),(#292100,#292101),
(#292102,#292103),(#292104,#292105),(#292106,#292107),(#292108,#292109),
(#292110,#292111),(#292112,#292113),(#292114,#292115),(#292116,#292117),
(#292118,#292119),(#292120,#292121),(#292122,#292123),(#292124,#292125),
(#292126,#292127),(#292128,#292129),(#292130,#292131),(#292132,#292133),
(#292134,#292135),(#292136,#292137),(#292138,#292139),(#292140,#292141),
(#292142,#292143),(#292144,#292145),(#292146,#292147),(#292148,#292149),
(#292150,#292151),(#292152,#292153),(#292154,#292155),(#292156,#292157),
(#292158,#292159),(#292160,#292161),(#292162,#292163),(#292164,#292165),
(#292166,#292167),(#292168,#292169),(#292170,#292171),(#292172,#292173),
(#292174,#292175),(#292176,#292177),(#292178,#292179),(#292180,#292181),
(#292182,#292183),(#292184,#292185),(#292186,#292187),(#292188,#292189),
(#292190,#292191),(#292192,#292193),(#292194,#292195),(#292196,#292197),
(#292198,#292199),(#292200,#292201),(#292202,#292203),(#292204,#292205),
(#292206,#292207),(#292208,#292209),(#292210,#292211),(#292212,#292213),
(#292214,#292215),(#292216,#292217),(#292218,#292219),(#292220,#292221),
(#292222,#292223),(#292224,#292225),(#292226,#292227),(#292228,#292229),
(#292230,#292231),(#292232,#292233),(#292234,#292235),(#292236,#292237),
(#292238,#292239),(#292240,#292241),(#292242,#292243),(#292244,#292245),
(#292246,#292247),(#292248,#292249),(#292250,#292251),(#292252,#292253),
(#292254,#292255),(#292256,#292257),(#292258,#292259),(#292260,#292261),
(#292262,#292263),(#292264,#292265),(#292266,#292267),(#292268,#292269),
(#292270,#292271),(#292272,#292273),(#292274,#292275),(#292276,#292277),
(#292278,#292279),(#292280,#292281),(#292282,#292283),(#292284,#292285),
(#292286,#292287),(#292288,#292289),(#292290,#292291),(#292292,#292293),
(#292294,#292295),(#292296,#292297),(#292298,#292299),(#292300,#292301),
(#292302,#292303),(#292304,#292305),(#292306,#292307),(#292308,#292309),
(#292310,#292311),(#292312,#292313),(#292314,#292315),(#292316,#292317),
(#292318,#292319),(#292320,#292321),(#292322,#292323),(#292324,#292325),
(#292326,#292327),(#292328,#292329),(#292330,#292331),(#292332,#292333),
(#292334,#292335),(#292336,#292337),(#292338,#292339),(#292340,#292341),
(#292342,#292343),(#292344,#292345),(#292346,#292347),(#292348,#292349),
(#292350,#292351),(#292352,#292353),(#292354,#292355),(#292356,#292357),
(#292358,#292359),(#292360,#292361),(#292362,#292363),(#292364,#292365),
(#292366,#292367),(#292368,#292369),(#292370,#292371),(#292372,#292373),
(#292374,#292375),(#292376,#292377),(#292378,#292379),(#292380,#292381),
(#292382,#292383),(#292384,#292385),(#292386,#292387),(#292388,#292389),
(#292390,#292391),(#292392,#292393),(#292394,#292395),(#292396,#292397),
(#292398,#292399),(#292400,#292401),(#292402,#292403),(#292404,#292405),
(#292406,#292407),(#292408,#292409),(#292410,#292411),(#292412,#292413),
(#292414,#292415),(#292416,#292417),(#292418,#292419),(#292420,#292421),
(#292422,#292423),(#292424,#292425),(#292426,#292427),(#292428,#292429),
(#292430,#292431),(#292432,#292433),(#292434,#292435),(#292436,#292437),
(#292438,#292439),(#292440,#292441),(#292442,#292443),(#292444,#292445),
(#292446,#292447),(#292448,#292449),(#292450,#292451),(#292452,#292453),
(#292454,#292455),(#292456,#292457),(#292458,#292459),(#292460,#292461),
(#292462,#292463),(#292464,#292465),(#292466,#292467),(#292468,#292469),
(#292470,#292471),(#292472,#292473),(#292474,#292475),(#292476,#292477),
(#292478,#292479),(#292480,#292481),(#292482,#292483),(#292484,#292485),
(#292486,#292487),(#292488,#292489),(#292490,#292491),(#292492,#292493),
(#292494,#292495),(#292496,#292497),(#292498,#292499),(#292500,#292501),
(#292502,#292503),(#292504,#292505),(#292506,#292507),(#292508,#292509),
(#292510,#292511),(#292512,#292513),(#292514,#292515),(#292516,#292517),
(#292518,#292519),(#292520,#292521),(#292522,#292523),(#292524,#292525),
(#292526,#292527),(#292528,#292529),(#292530,#292531),(#292532,#292533),
(#292534,#292535),(#292536,#292537),(#292538,#292539),(#292540,#292541),
(#292542,#292543),(#292544,#292545),(#292546,#292547),(#292548,#292549),
(#292550,#292551),(#292552,#292553),(#292554,#292555),(#292556,#292557),
(#292558,#292559),(#292560,#292561),(#292562,#292563),(#292564,#292565),
(#292566,#292567),(#292568,#292569),(#292570,#292571),(#292572,#292573),
(#292574,#292575),(#292576,#292577)),.UNSPECIFIED.,.F.,.F.,.F.,(6,1,1,1,
1,1,1,1,1,1,1,1,1,1,1,1,1,1,1,1,1,1,1,1,1,1,1,1,1,1,1,1,1,1,1,1,1,1,1,1,
1,1,1,1,1,1,1,1,1,1,1,1,1,1,1,1,1,1,1,1,1,1,1,1,1,1,1,1,1,1,1,1,1,1,1,1,
1,1,1,1,1,1,1,1,1,1,1,1,1,1,1,1,1,1,1,1,1,1,1,1,1,1,1,1,1,1,1,1,1,1,1,1,
1,1,1,1,1,1,1,1,1,1,1,1,1,1,1,1,1,1,1,1,1,1,1,1,1,1,1,1,1,1,1,1,1,1,1,1,
1,1,1,1,1,1,1,1,1,1,1,1,1,1,1,1,1,1,1,1,1,1,1,1,1,1,1,1,1,1,1,1,1,1,1,1,
1,1,1,1,1,1,1,1,1,1,1,1,1,1,1,1,1,1,1,1,1,1,1,1,1,1,1,1,1,1,1,1,1,1,1,1,
1,1,1,1,1,1,1,1,1,1,1,1,1,1,1,1,1,1,1,1,1,1,1,1,1,1,1,1,1,1,1,1,1,1,1,1,
1,1,1,1,1,1,1,1,1,1,1,1,1,1,1,1,1,1,1,1,1,1,1,1,1,1,1,1,1,1,1,1,1,1,1,1,
1,1,1,1,1,1,1,1,1,1,1,1,1,1,1,1,1,1,1,1,1,1,1,1,1,1,1,1,1,1,1,1,1,1,1,1,
1,1,1,1,1,1,1,1,1,1,1,1,1,1,1,1,1,1,1,1,1,1,1,1,1,1,1,1,1,1,1,1,1,1,1,1,
1,1,1,1,1,1,1,1,1,1,1,1,1,1,1,1,1,1,1,1,1,1,1,1,1,1,1,1,1,1,1,1,1,1,1,1,
1,1,1,1,1,1,1,1,1,1,1,1,1,1,1,1,1,1,1,1,1,1,1,1,1,1,1,1,1,1,1,1,1,1,1,1,
1,1,1,1,1,1,1,1,1,1,1,1,1,1,1,1,1,1,1,1,1,1,1,1,1,1,1,1,1,1,1,6),(2,2),
(0.143172103,0.144954128,0.146788991,0.148623853,0.150458716,0.152293578,
0.15412844,0.155963303,0.157798165,0.159633028,0.16146789,0.163302752,0.165137615,
0.166972477,0.168807339,0.170642202,0.172477064,0.174311927,0.176146789,
0.177981651,0.179816514,0.181651376,0.183486239,0.185321101,0.187155963,
0.188990826,0.190825688,0.19266055,0.194495413,0.196330275,0.198165138,
0.2,0.201834862,0.203669725,0.205504587,0.20733945,0.209174312,0.211009174,
0.212844037,0.214678899,0.216513761,0.218348624,0.220183486,0.222018349,
0.223853211,0.225688073,0.227522936,0.229357798,0.231192661,0.233027523,
0.234862385,0.236697248,0.23853211,0.240366972,0.242201835,0.244036697,
0.24587156,0.247706422,0.249541284,0.251376147,0.253211009,0.255045872,
0.256880734,0.258715596,0.260550459,0.262385321,0.264220183,0.266055046,
0.267889908,0.269724771,0.271559633,0.273394495,0.275229358,0.27706422,
0.278899083,0.280733945,0.282568807,0.28440367,0.286238532,0.288073394,
0.289908257,0.291743119,0.293577982,0.295412844,0.297247706,0.299082569,
0.300917431,0.302752294,0.304587156,0.306422018,0.308256881,0.310091743,
0.311926606,0.313761468,0.31559633,0.317431193,0.319266055,0.321100917,
0.32293578,0.324770642,0.326605505,0.328440367,0.330275229,0.332110092,
0.333944954,0.335779817,0.337614679,0.339449541,0.341284404,0.343119266,
0.344954128,0.346788991,0.348623853,0.350458716,0.352293578,0.35412844,
0.355963303,0.357798165,0.359633028,0.36146789,0.363302752,0.365137615,
0.366972477,0.368807339,0.370642202,0.372477064,0.374311927,0.376146789,
0.377981651,0.379816514,0.381651376,0.383486239,0.385321101,0.387155963,
0.388990826,0.390825688,0.39266055,0.394495413,0.396330275,0.398165138,
0.4,0.401834862,0.403669725,0.405504587,0.40733945,0.409174312,0.411009174,
0.412844037,0.414678899,0.416513761,0.418348624,0.420183486,0.422018349,
0.423853211,0.425688073,0.427522936,0.429357798,0.431192661,0.433027523,
0.434862385,0.436697248,0.43853211,0.440366972,0.442201835,0.444036697,
0.44587156,0.447706422,0.449541284,0.451376147,0.453211009,0.455045872,
0.456880734,0.458715596,0.460550459,0.462385321,0.464220183,0.466055046,
0.467889908,0.469724771,0.471559633,0.473394495,0.475229358,0.47706422,
0.478899083,0.480733945,0.482568807,0.48440367,0.486238532,0.488073394,
0.489908257,0.491743119,0.493577982,0.495412844,0.497247706,0.499082569,
0.500917431,0.502752294,0.504587156,0.506422018,0.508256881,0.510091743,
0.511926606,0.513761468,0.51559633,0.517431193,0.519266055,0.521100917,
0.52293578,0.524770642,0.526605505,0.528440367,0.530275229,0.532110092,
0.533944954,0.535779817,0.537614679,0.539449541,0.541284404,0.543119266,
0.544954128,0.546788991,0.548623853,0.550458716,0.552293578,0.55412844,
0.555963303,0.557798165,0.559633028,0.56146789,0.563302752,0.565137615,
0.566972477,0.568807339,0.570642202,0.572477064,0.574311927,0.576146789,
0.577981651,0.579816514,0.581651376,0.583486239,0.585321101,0.587155963,
0.588990826,0.590825688,0.59266055,0.594495413,0.596330275,0.598165138,
0.6,0.601834862,0.603669725,0.605504587,0.60733945,0.609174312,0.611009174,
0.612844037,0.614678899,0.616513761,0.618348624,0.620183486,0.622018349,
0.623853211,0.625688073,0.627522936,0.629357798,0.631192661,0.633027523,
0.634862385,0.636697248,0.63853211,0.640366972,0.642201835,0.644036697,
0.64587156,0.647706422,0.649541284,0.651376147,0.653211009,0.655045872,
0.656880734,0.658715596,0.660550459,0.662385321,0.664220183,0.666055046,
0.667889908,0.669724771,0.671559633,0.673394495,0.675229358,0.67706422,
0.678899083,0.680733945,0.682568807,0.68440367,0.686238532,0.688073394,
0.689908257,0.691743119,0.693577982,0.695412844,0.697247706,0.699082569,
0.700917431,0.702752294,0.704587156,0.706422018,0.708256881,0.710091743,
0.711926606,0.713761468,0.71559633,0.717431193,0.719266055,0.721100917,
0.72293578,0.724770642,0.726605505,0.728440367,0.730275229,0.732110092,
0.733944954,0.735779817,0.737614679,0.739449541,0.741284404,0.743119266,
0.744954128,0.746788991,0.748623853,0.750458716,0.752293578,0.75412844,
0.755963303,0.757798165,0.759633028,0.76146789,0.763302752,0.765137615,
0.766972477,0.768807339,0.770642202,0.772477064,0.774311927,0.776146789,
0.777981651,0.779816514,0.781651376,0.783486239,0.785321101,0.787155963,
0.788990826,0.790825688,0.79266055,0.794495413,0.796330275,0.798165138,
0.8,0.801834862,0.803669725,0.805504587,0.80733945,0.809174312,0.811009174,
0.812844037,0.814678899,0.816513761,0.818348624,0.820183486,0.822018349,
0.823853211,0.825688073,0.827522936,0.829357798,0.831192661,0.833027523,
0.834862385,0.836697248,0.83853211,0.840366972,0.842201835,0.844036697,
0.84587156,0.847706422,0.849541284,0.851376147,0.853211009,0.855045872,
0.856880734,0.858715596,0.860550459,0.862385321,0.864220183,0.866055046,
0.867889908,0.869724771,0.871559633,0.873394495,0.875229358,0.87706422,
0.878899083,0.880733945,0.882568807,0.88440367,0.886238532,0.888073394,
0.889908257,0.891743119,0.893577982,0.895412844,0.897247706,0.899082569,
0.900917431,0.902752294,0.904587156,0.906422018,0.908256881,0.910091743,
0.911926606,0.913761468,0.91559633,0.917431193,0.919266055,0.921100917,
0.92293578,0.924770642,0.926605505,0.928440367,0.930275229,0.932110092,
0.933944954,0.935779817,0.937614679,0.939449541,0.941284404,0.943119266,
0.944954128,0.946788991,0.948623853,0.950458716,0.952293578,0.95412844,
0.955963303,0.957798165,0.959633028,0.96146789,0.963302752,0.965137615,
0.966972477,0.968807339,0.970642202,0.972477064,0.974311927,0.976146789,
0.977981651,0.979816514,0.981651376,0.983486239,0.985321101,0.987155963,
0.988990826,0.990825688,0.99266055,0.994495413,0.996330275,0.998165138,
1.),(0.,0.36),.UNSPECIFIED.);
#6299=B_SPLINE_SURFACE_WITH_KNOTS('',5,1,((#293228,#293229),(#293230,#293231),
(#293232,#293233),(#293234,#293235),(#293236,#293237),(#293238,#293239),
(#293240,#293241),(#293242,#293243),(#293244,#293245),(#293246,#293247),
(#293248,#293249),(#293250,#293251),(#293252,#293253),(#293254,#293255),
(#293256,#293257),(#293258,#293259),(#293260,#293261),(#293262,#293263),
(#293264,#293265),(#293266,#293267),(#293268,#293269),(#293270,#293271),
(#293272,#293273),(#293274,#293275),(#293276,#293277),(#293278,#293279),
(#293280,#293281),(#293282,#293283),(#293284,#293285),(#293286,#293287),
(#293288,#293289),(#293290,#293291),(#293292,#293293),(#293294,#293295),
(#293296,#293297),(#293298,#293299),(#293300,#293301),(#293302,#293303),
(#293304,#293305),(#293306,#293307),(#293308,#293309),(#293310,#293311),
(#293312,#293313),(#293314,#293315),(#293316,#293317),(#293318,#293319),
(#293320,#293321),(#293322,#293323),(#293324,#293325),(#293326,#293327),
(#293328,#293329),(#293330,#293331),(#293332,#293333),(#293334,#293335),
(#293336,#293337),(#293338,#293339),(#293340,#293341),(#293342,#293343),
(#293344,#293345),(#293346,#293347),(#293348,#293349),(#293350,#293351),
(#293352,#293353),(#293354,#293355),(#293356,#293357),(#293358,#293359),
(#293360,#293361),(#293362,#293363),(#293364,#293365),(#293366,#293367),
(#293368,#293369),(#293370,#293371),(#293372,#293373),(#293374,#293375),
(#293376,#293377),(#293378,#293379),(#293380,#293381),(#293382,#293383),
(#293384,#293385),(#293386,#293387),(#293388,#293389),(#293390,#293391),
(#293392,#293393),(#293394,#293395),(#293396,#293397),(#293398,#293399),
(#293400,#293401),(#293402,#293403),(#293404,#293405),(#293406,#293407),
(#293408,#293409),(#293410,#293411),(#293412,#293413),(#293414,#293415),
(#293416,#293417),(#293418,#293419),(#293420,#293421),(#293422,#293423),
(#293424,#293425),(#293426,#293427),(#293428,#293429),(#293430,#293431),
(#293432,#293433),(#293434,#293435),(#293436,#293437),(#293438,#293439),
(#293440,#293441),(#293442,#293443),(#293444,#293445),(#293446,#293447),
(#293448,#293449),(#293450,#293451),(#293452,#293453),(#293454,#293455),
(#293456,#293457),(#293458,#293459),(#293460,#293461),(#293462,#293463),
(#293464,#293465),(#293466,#293467),(#293468,#293469),(#293470,#293471),
(#293472,#293473),(#293474,#293475),(#293476,#293477),(#293478,#293479),
(#293480,#293481),(#293482,#293483),(#293484,#293485),(#293486,#293487),
(#293488,#293489),(#293490,#293491),(#293492,#293493),(#293494,#293495),
(#293496,#293497),(#293498,#293499),(#293500,#293501),(#293502,#293503),
(#293504,#293505),(#293506,#293507),(#293508,#293509),(#293510,#293511),
(#293512,#293513),(#293514,#293515),(#293516,#293517),(#293518,#293519),
(#293520,#293521),(#293522,#293523),(#293524,#293525),(#293526,#293527),
(#293528,#293529),(#293530,#293531),(#293532,#293533),(#293534,#293535),
(#293536,#293537),(#293538,#293539),(#293540,#293541),(#293542,#293543),
(#293544,#293545),(#293546,#293547),(#293548,#293549),(#293550,#293551),
(#293552,#293553),(#293554,#293555),(#293556,#293557),(#293558,#293559),
(#293560,#293561),(#293562,#293563),(#293564,#293565),(#293566,#293567),
(#293568,#293569),(#293570,#293571),(#293572,#293573),(#293574,#293575),
(#293576,#293577),(#293578,#293579),(#293580,#293581),(#293582,#293583),
(#293584,#293585),(#293586,#293587),(#293588,#293589),(#293590,#293591),
(#293592,#293593),(#293594,#293595),(#293596,#293597),(#293598,#293599),
(#293600,#293601),(#293602,#293603),(#293604,#293605),(#293606,#293607),
(#293608,#293609),(#293610,#293611),(#293612,#293613),(#293614,#293615),
(#293616,#293617),(#293618,#293619),(#293620,#293621),(#293622,#293623),
(#293624,#293625),(#293626,#293627),(#293628,#293629),(#293630,#293631),
(#293632,#293633),(#293634,#293635),(#293636,#293637),(#293638,#293639),
(#293640,#293641),(#293642,#293643),(#293644,#293645),(#293646,#293647),
(#293648,#293649),(#293650,#293651),(#293652,#293653),(#293654,#293655),
(#293656,#293657),(#293658,#293659),(#293660,#293661),(#293662,#293663),
(#293664,#293665),(#293666,#293667),(#293668,#293669),(#293670,#293671),
(#293672,#293673),(#293674,#293675),(#293676,#293677),(#293678,#293679),
(#293680,#293681),(#293682,#293683),(#293684,#293685),(#293686,#293687),
(#293688,#293689),(#293690,#293691),(#293692,#293693),(#293694,#293695),
(#293696,#293697),(#293698,#293699),(#293700,#293701),(#293702,#293703),
(#293704,#293705),(#293706,#293707),(#293708,#293709),(#293710,#293711),
(#293712,#293713),(#293714,#293715),(#293716,#293717),(#293718,#293719),
(#293720,#293721),(#293722,#293723),(#293724,#293725),(#293726,#293727),
(#293728,#293729),(#293730,#293731),(#293732,#293733),(#293734,#293735),
(#293736,#293737),(#293738,#293739),(#293740,#293741),(#293742,#293743),
(#293744,#293745),(#293746,#293747),(#293748,#293749),(#293750,#293751),
(#293752,#293753),(#293754,#293755),(#293756,#293757),(#293758,#293759),
(#293760,#293761),(#293762,#293763),(#293764,#293765),(#293766,#293767),
(#293768,#293769),(#293770,#293771),(#293772,#293773),(#293774,#293775),
(#293776,#293777),(#293778,#293779),(#293780,#293781),(#293782,#293783),
(#293784,#293785),(#293786,#293787),(#293788,#293789),(#293790,#293791),
(#293792,#293793),(#293794,#293795),(#293796,#293797),(#293798,#293799),
(#293800,#293801),(#293802,#293803),(#293804,#293805),(#293806,#293807),
(#293808,#293809),(#293810,#293811),(#293812,#293813),(#293814,#293815),
(#293816,#293817),(#293818,#293819),(#293820,#293821),(#293822,#293823),
(#293824,#293825),(#293826,#293827),(#293828,#293829),(#293830,#293831),
(#293832,#293833),(#293834,#293835),(#293836,#293837),(#293838,#293839),
(#293840,#293841),(#293842,#293843),(#293844,#293845),(#293846,#293847),
(#293848,#293849),(#293850,#293851),(#293852,#293853),(#293854,#293855),
(#293856,#293857),(#293858,#293859),(#293860,#293861),(#293862,#293863),
(#293864,#293865),(#293866,#293867),(#293868,#293869),(#293870,#293871),
(#293872,#293873),(#293874,#293875),(#293876,#293877),(#293878,#293879),
(#293880,#293881),(#293882,#293883),(#293884,#293885),(#293886,#293887),
(#293888,#293889),(#293890,#293891),(#293892,#293893),(#293894,#293895),
(#293896,#293897),(#293898,#293899),(#293900,#293901),(#293902,#293903),
(#293904,#293905),(#293906,#293907),(#293908,#293909),(#293910,#293911),
(#293912,#293913),(#293914,#293915),(#293916,#293917),(#293918,#293919),
(#293920,#293921),(#293922,#293923),(#293924,#293925),(#293926,#293927),
(#293928,#293929),(#293930,#293931),(#293932,#293933),(#293934,#293935),
(#293936,#293937),(#293938,#293939),(#293940,#293941),(#293942,#293943),
(#293944,#293945),(#293946,#293947),(#293948,#293949),(#293950,#293951),
(#293952,#293953),(#293954,#293955),(#293956,#293957),(#293958,#293959),
(#293960,#293961),(#293962,#293963),(#293964,#293965),(#293966,#293967),
(#293968,#293969),(#293970,#293971),(#293972,#293973),(#293974,#293975),
(#293976,#293977),(#293978,#293979),(#293980,#293981),(#293982,#293983),
(#293984,#293985),(#293986,#293987),(#293988,#293989),(#293990,#293991),
(#293992,#293993),(#293994,#293995),(#293996,#293997),(#293998,#293999),
(#294000,#294001),(#294002,#294003),(#294004,#294005),(#294006,#294007),
(#294008,#294009),(#294010,#294011),(#294012,#294013),(#294014,#294015),
(#294016,#294017),(#294018,#294019),(#294020,#294021),(#294022,#294023),
(#294024,#294025),(#294026,#294027),(#294028,#294029),(#294030,#294031),
(#294032,#294033),(#294034,#294035),(#294036,#294037),(#294038,#294039),
(#294040,#294041),(#294042,#294043),(#294044,#294045),(#294046,#294047),
(#294048,#294049),(#294050,#294051),(#294052,#294053),(#294054,#294055),
(#294056,#294057),(#294058,#294059),(#294060,#294061),(#294062,#294063),
(#294064,#294065),(#294066,#294067),(#294068,#294069),(#294070,#294071),
(#294072,#294073),(#294074,#294075),(#294076,#294077),(#294078,#294079),
(#294080,#294081),(#294082,#294083),(#294084,#294085),(#294086,#294087),
(#294088,#294089),(#294090,#294091),(#294092,#294093),(#294094,#294095),
(#294096,#294097),(#294098,#294099),(#294100,#294101),(#294102,#294103),
(#294104,#294105),(#294106,#294107),(#294108,#294109),(#294110,#294111),
(#294112,#294113),(#294114,#294115),(#294116,#294117),(#294118,#294119),
(#294120,#294121),(#294122,#294123),(#294124,#294125),(#294126,#294127),
(#294128,#294129),(#294130,#294131),(#294132,#294133),(#294134,#294135),
(#294136,#294137),(#294138,#294139),(#294140,#294141),(#294142,#294143),
(#294144,#294145),(#294146,#294147),(#294148,#294149),(#294150,#294151),
(#294152,#294153),(#294154,#294155),(#294156,#294157),(#294158,#294159),
(#294160,#294161),(#294162,#294163),(#294164,#294165),(#294166,#294167),
(#294168,#294169),(#294170,#294171)),.UNSPECIFIED.,.F.,.F.,.F.,(6,1,1,1,
1,1,1,1,1,1,1,1,1,1,1,1,1,1,1,1,1,1,1,1,1,1,1,1,1,1,1,1,1,1,1,1,1,1,1,1,
1,1,1,1,1,1,1,1,1,1,1,1,1,1,1,1,1,1,1,1,1,1,1,1,1,1,1,1,1,1,1,1,1,1,1,1,
1,1,1,1,1,1,1,1,1,1,1,1,1,1,1,1,1,1,1,1,1,1,1,1,1,1,1,1,1,1,1,1,1,1,1,1,
1,1,1,1,1,1,1,1,1,1,1,1,1,1,1,1,1,1,1,1,1,1,1,1,1,1,1,1,1,1,1,1,1,1,1,1,
1,1,1,1,1,1,1,1,1,1,1,1,1,1,1,1,1,1,1,1,1,1,1,1,1,1,1,1,1,1,1,1,1,1,1,1,
1,1,1,1,1,1,1,1,1,1,1,1,1,1,1,1,1,1,1,1,1,1,1,1,1,1,1,1,1,1,1,1,1,1,1,1,
1,1,1,1,1,1,1,1,1,1,1,1,1,1,1,1,1,1,1,1,1,1,1,1,1,1,1,1,1,1,1,1,1,1,1,1,
1,1,1,1,1,1,1,1,1,1,1,1,1,1,1,1,1,1,1,1,1,1,1,1,1,1,1,1,1,1,1,1,1,1,1,1,
1,1,1,1,1,1,1,1,1,1,1,1,1,1,1,1,1,1,1,1,1,1,1,1,1,1,1,1,1,1,1,1,1,1,1,1,
1,1,1,1,1,1,1,1,1,1,1,1,1,1,1,1,1,1,1,1,1,1,1,1,1,1,1,1,1,1,1,1,1,1,1,1,
1,1,1,1,1,1,1,1,1,1,1,1,1,1,1,1,1,1,1,1,1,1,1,1,1,1,1,1,1,1,1,1,1,1,1,1,
1,1,1,1,1,1,1,1,1,1,1,1,1,1,1,1,1,1,1,1,1,1,1,1,1,1,1,1,1,1,1,1,1,1,1,1,
1,1,1,1,1,1,1,1,1,1,1,1,1,1,1,1,1,1,1,1,1,1,1,1,1,1,1,1,1,1,1,6),(2,2),
(0.143172103,0.144954128,0.146788991,0.148623853,0.150458716,0.152293578,
0.15412844,0.155963303,0.157798165,0.159633028,0.16146789,0.163302752,0.165137615,
0.166972477,0.168807339,0.170642202,0.172477064,0.174311927,0.176146789,
0.177981651,0.179816514,0.181651376,0.183486239,0.185321101,0.187155963,
0.188990826,0.190825688,0.19266055,0.194495413,0.196330275,0.198165138,
0.2,0.201834862,0.203669725,0.205504587,0.20733945,0.209174312,0.211009174,
0.212844037,0.214678899,0.216513761,0.218348624,0.220183486,0.222018349,
0.223853211,0.225688073,0.227522936,0.229357798,0.231192661,0.233027523,
0.234862385,0.236697248,0.23853211,0.240366972,0.242201835,0.244036697,
0.24587156,0.247706422,0.249541284,0.251376147,0.253211009,0.255045872,
0.256880734,0.258715596,0.260550459,0.262385321,0.264220183,0.266055046,
0.267889908,0.269724771,0.271559633,0.273394495,0.275229358,0.27706422,
0.278899083,0.280733945,0.282568807,0.28440367,0.286238532,0.288073394,
0.289908257,0.291743119,0.293577982,0.295412844,0.297247706,0.299082569,
0.300917431,0.302752294,0.304587156,0.306422018,0.308256881,0.310091743,
0.311926606,0.313761468,0.31559633,0.317431193,0.319266055,0.321100917,
0.32293578,0.324770642,0.326605505,0.328440367,0.330275229,0.332110092,
0.333944954,0.335779817,0.337614679,0.339449541,0.341284404,0.343119266,
0.344954128,0.346788991,0.348623853,0.350458716,0.352293578,0.35412844,
0.355963303,0.357798165,0.359633028,0.36146789,0.363302752,0.365137615,
0.366972477,0.368807339,0.370642202,0.372477064,0.374311927,0.376146789,
0.377981651,0.379816514,0.381651376,0.383486239,0.385321101,0.387155963,
0.388990826,0.390825688,0.39266055,0.394495413,0.396330275,0.398165138,
0.4,0.401834862,0.403669725,0.405504587,0.40733945,0.409174312,0.411009174,
0.412844037,0.414678899,0.416513761,0.418348624,0.420183486,0.422018349,
0.423853211,0.425688073,0.427522936,0.429357798,0.431192661,0.433027523,
0.434862385,0.436697248,0.43853211,0.440366972,0.442201835,0.444036697,
0.44587156,0.447706422,0.449541284,0.451376147,0.453211009,0.455045872,
0.456880734,0.458715596,0.460550459,0.462385321,0.464220183,0.466055046,
0.467889908,0.469724771,0.471559633,0.473394495,0.475229358,0.47706422,
0.478899083,0.480733945,0.482568807,0.48440367,0.486238532,0.488073394,
0.489908257,0.491743119,0.493577982,0.495412844,0.497247706,0.499082569,
0.500917431,0.502752294,0.504587156,0.506422018,0.508256881,0.510091743,
0.511926606,0.513761468,0.51559633,0.517431193,0.519266055,0.521100917,
0.52293578,0.524770642,0.526605505,0.528440367,0.530275229,0.532110092,
0.533944954,0.535779817,0.537614679,0.539449541,0.541284404,0.543119266,
0.544954128,0.546788991,0.548623853,0.550458716,0.552293578,0.55412844,
0.555963303,0.557798165,0.559633028,0.56146789,0.563302752,0.565137615,
0.566972477,0.568807339,0.570642202,0.572477064,0.574311927,0.576146789,
0.577981651,0.579816514,0.581651376,0.583486239,0.585321101,0.587155963,
0.588990826,0.590825688,0.59266055,0.594495413,0.596330275,0.598165138,
0.6,0.601834862,0.603669725,0.605504587,0.60733945,0.609174312,0.611009174,
0.612844037,0.614678899,0.616513761,0.618348624,0.620183486,0.622018349,
0.623853211,0.625688073,0.627522936,0.629357798,0.631192661,0.633027523,
0.634862385,0.636697248,0.63853211,0.640366972,0.642201835,0.644036697,
0.64587156,0.647706422,0.649541284,0.651376147,0.653211009,0.655045872,
0.656880734,0.658715596,0.660550459,0.662385321,0.664220183,0.666055046,
0.667889908,0.669724771,0.671559633,0.673394495,0.675229358,0.67706422,
0.678899083,0.680733945,0.682568807,0.68440367,0.686238532,0.688073394,
0.689908257,0.691743119,0.693577982,0.695412844,0.697247706,0.699082569,
0.700917431,0.702752294,0.704587156,0.706422018,0.708256881,0.710091743,
0.711926606,0.713761468,0.71559633,0.717431193,0.719266055,0.721100917,
0.72293578,0.724770642,0.726605505,0.728440367,0.730275229,0.732110092,
0.733944954,0.735779817,0.737614679,0.739449541,0.741284404,0.743119266,
0.744954128,0.746788991,0.748623853,0.750458716,0.752293578,0.75412844,
0.755963303,0.757798165,0.759633028,0.76146789,0.763302752,0.765137615,
0.766972477,0.768807339,0.770642202,0.772477064,0.774311927,0.776146789,
0.777981651,0.779816514,0.781651376,0.783486239,0.785321101,0.787155963,
0.788990826,0.790825688,0.79266055,0.794495413,0.796330275,0.798165138,
0.8,0.801834862,0.803669725,0.805504587,0.80733945,0.809174312,0.811009174,
0.812844037,0.814678899,0.816513761,0.818348624,0.820183486,0.822018349,
0.823853211,0.825688073,0.827522936,0.829357798,0.831192661,0.833027523,
0.834862385,0.836697248,0.83853211,0.840366972,0.842201835,0.844036697,
0.84587156,0.847706422,0.849541284,0.851376147,0.853211009,0.855045872,
0.856880734,0.858715596,0.860550459,0.862385321,0.864220183,0.866055046,
0.867889908,0.869724771,0.871559633,0.873394495,0.875229358,0.87706422,
0.878899083,0.880733945,0.882568807,0.88440367,0.886238532,0.888073394,
0.889908257,0.891743119,0.893577982,0.895412844,0.897247706,0.899082569,
0.900917431,0.902752294,0.904587156,0.906422018,0.908256881,0.910091743,
0.911926606,0.913761468,0.91559633,0.917431193,0.919266055,0.921100917,
0.92293578,0.924770642,0.926605505,0.928440367,0.930275229,0.932110092,
0.933944954,0.935779817,0.937614679,0.939449541,0.941284404,0.943119266,
0.944954128,0.946788991,0.948623853,0.950458716,0.952293578,0.95412844,
0.955963303,0.957798165,0.959633028,0.96146789,0.963302752,0.965137615,
0.966972477,0.968807339,0.970642202,0.972477064,0.974311927,0.976146789,
0.977981651,0.979816514,0.981651376,0.983486239,0.985321101,0.987155963,
0.988990826,0.990825688,0.99266055,0.994495413,0.996330275,0.998165138,
1.),(0.,0.36),.UNSPECIFIED.);
#6300=B_SPLINE_SURFACE_WITH_KNOTS('',5,1,((#294807,#294808),(#294809,#294810),
(#294811,#294812),(#294813,#294814),(#294815,#294816),(#294817,#294818),
(#294819,#294820),(#294821,#294822),(#294823,#294824),(#294825,#294826),
(#294827,#294828),(#294829,#294830),(#294831,#294832),(#294833,#294834),
(#294835,#294836),(#294837,#294838),(#294839,#294840),(#294841,#294842),
(#294843,#294844),(#294845,#294846),(#294847,#294848),(#294849,#294850),
(#294851,#294852),(#294853,#294854),(#294855,#294856),(#294857,#294858),
(#294859,#294860),(#294861,#294862),(#294863,#294864),(#294865,#294866),
(#294867,#294868),(#294869,#294870),(#294871,#294872),(#294873,#294874),
(#294875,#294876),(#294877,#294878),(#294879,#294880),(#294881,#294882),
(#294883,#294884),(#294885,#294886),(#294887,#294888),(#294889,#294890),
(#294891,#294892),(#294893,#294894),(#294895,#294896),(#294897,#294898),
(#294899,#294900),(#294901,#294902),(#294903,#294904),(#294905,#294906),
(#294907,#294908),(#294909,#294910),(#294911,#294912),(#294913,#294914),
(#294915,#294916),(#294917,#294918),(#294919,#294920),(#294921,#294922),
(#294923,#294924),(#294925,#294926),(#294927,#294928),(#294929,#294930),
(#294931,#294932),(#294933,#294934),(#294935,#294936),(#294937,#294938),
(#294939,#294940),(#294941,#294942),(#294943,#294944),(#294945,#294946),
(#294947,#294948),(#294949,#294950),(#294951,#294952),(#294953,#294954),
(#294955,#294956),(#294957,#294958),(#294959,#294960),(#294961,#294962),
(#294963,#294964),(#294965,#294966),(#294967,#294968),(#294969,#294970),
(#294971,#294972),(#294973,#294974),(#294975,#294976),(#294977,#294978),
(#294979,#294980),(#294981,#294982),(#294983,#294984),(#294985,#294986),
(#294987,#294988),(#294989,#294990),(#294991,#294992),(#294993,#294994),
(#294995,#294996),(#294997,#294998),(#294999,#295000),(#295001,#295002),
(#295003,#295004),(#295005,#295006),(#295007,#295008),(#295009,#295010),
(#295011,#295012),(#295013,#295014),(#295015,#295016),(#295017,#295018),
(#295019,#295020),(#295021,#295022),(#295023,#295024),(#295025,#295026),
(#295027,#295028),(#295029,#295030),(#295031,#295032),(#295033,#295034),
(#295035,#295036),(#295037,#295038),(#295039,#295040),(#295041,#295042),
(#295043,#295044),(#295045,#295046),(#295047,#295048),(#295049,#295050),
(#295051,#295052),(#295053,#295054),(#295055,#295056),(#295057,#295058),
(#295059,#295060),(#295061,#295062),(#295063,#295064),(#295065,#295066),
(#295067,#295068),(#295069,#295070),(#295071,#295072),(#295073,#295074),
(#295075,#295076),(#295077,#295078),(#295079,#295080),(#295081,#295082),
(#295083,#295084),(#295085,#295086),(#295087,#295088),(#295089,#295090),
(#295091,#295092),(#295093,#295094),(#295095,#295096),(#295097,#295098),
(#295099,#295100),(#295101,#295102),(#295103,#295104),(#295105,#295106),
(#295107,#295108),(#295109,#295110),(#295111,#295112),(#295113,#295114),
(#295115,#295116),(#295117,#295118),(#295119,#295120),(#295121,#295122),
(#295123,#295124),(#295125,#295126),(#295127,#295128),(#295129,#295130),
(#295131,#295132),(#295133,#295134),(#295135,#295136),(#295137,#295138),
(#295139,#295140),(#295141,#295142),(#295143,#295144),(#295145,#295146),
(#295147,#295148),(#295149,#295150),(#295151,#295152),(#295153,#295154),
(#295155,#295156),(#295157,#295158),(#295159,#295160),(#295161,#295162),
(#295163,#295164),(#295165,#295166),(#295167,#295168),(#295169,#295170),
(#295171,#295172),(#295173,#295174),(#295175,#295176),(#295177,#295178),
(#295179,#295180),(#295181,#295182),(#295183,#295184),(#295185,#295186),
(#295187,#295188),(#295189,#295190),(#295191,#295192),(#295193,#295194),
(#295195,#295196),(#295197,#295198),(#295199,#295200),(#295201,#295202),
(#295203,#295204),(#295205,#295206),(#295207,#295208),(#295209,#295210),
(#295211,#295212),(#295213,#295214),(#295215,#295216),(#295217,#295218),
(#295219,#295220),(#295221,#295222),(#295223,#295224),(#295225,#295226),
(#295227,#295228),(#295229,#295230),(#295231,#295232),(#295233,#295234),
(#295235,#295236),(#295237,#295238),(#295239,#295240),(#295241,#295242),
(#295243,#295244),(#295245,#295246),(#295247,#295248),(#295249,#295250),
(#295251,#295252),(#295253,#295254),(#295255,#295256),(#295257,#295258),
(#295259,#295260),(#295261,#295262),(#295263,#295264),(#295265,#295266),
(#295267,#295268),(#295269,#295270),(#295271,#295272),(#295273,#295274),
(#295275,#295276),(#295277,#295278),(#295279,#295280),(#295281,#295282),
(#295283,#295284),(#295285,#295286),(#295287,#295288),(#295289,#295290),
(#295291,#295292),(#295293,#295294),(#295295,#295296),(#295297,#295298),
(#295299,#295300),(#295301,#295302),(#295303,#295304),(#295305,#295306),
(#295307,#295308),(#295309,#295310),(#295311,#295312),(#295313,#295314),
(#295315,#295316),(#295317,#295318),(#295319,#295320),(#295321,#295322),
(#295323,#295324),(#295325,#295326),(#295327,#295328),(#295329,#295330),
(#295331,#295332),(#295333,#295334),(#295335,#295336),(#295337,#295338),
(#295339,#295340),(#295341,#295342),(#295343,#295344),(#295345,#295346),
(#295347,#295348),(#295349,#295350),(#295351,#295352),(#295353,#295354),
(#295355,#295356),(#295357,#295358),(#295359,#295360),(#295361,#295362),
(#295363,#295364),(#295365,#295366),(#295367,#295368),(#295369,#295370),
(#295371,#295372),(#295373,#295374),(#295375,#295376),(#295377,#295378),
(#295379,#295380),(#295381,#295382),(#295383,#295384),(#295385,#295386),
(#295387,#295388),(#295389,#295390),(#295391,#295392),(#295393,#295394),
(#295395,#295396),(#295397,#295398),(#295399,#295400),(#295401,#295402),
(#295403,#295404),(#295405,#295406),(#295407,#295408),(#295409,#295410),
(#295411,#295412),(#295413,#295414),(#295415,#295416),(#295417,#295418),
(#295419,#295420),(#295421,#295422),(#295423,#295424),(#295425,#295426),
(#295427,#295428),(#295429,#295430),(#295431,#295432),(#295433,#295434),
(#295435,#295436),(#295437,#295438),(#295439,#295440),(#295441,#295442),
(#295443,#295444),(#295445,#295446),(#295447,#295448),(#295449,#295450),
(#295451,#295452),(#295453,#295454),(#295455,#295456),(#295457,#295458),
(#295459,#295460),(#295461,#295462),(#295463,#295464),(#295465,#295466),
(#295467,#295468),(#295469,#295470),(#295471,#295472),(#295473,#295474),
(#295475,#295476),(#295477,#295478),(#295479,#295480),(#295481,#295482),
(#295483,#295484),(#295485,#295486),(#295487,#295488),(#295489,#295490),
(#295491,#295492),(#295493,#295494),(#295495,#295496),(#295497,#295498),
(#295499,#295500),(#295501,#295502),(#295503,#295504),(#295505,#295506),
(#295507,#295508),(#295509,#295510),(#295511,#295512),(#295513,#295514),
(#295515,#295516),(#295517,#295518),(#295519,#295520),(#295521,#295522),
(#295523,#295524),(#295525,#295526),(#295527,#295528),(#295529,#295530),
(#295531,#295532),(#295533,#295534),(#295535,#295536),(#295537,#295538),
(#295539,#295540),(#295541,#295542),(#295543,#295544),(#295545,#295546),
(#295547,#295548),(#295549,#295550),(#295551,#295552),(#295553,#295554),
(#295555,#295556),(#295557,#295558),(#295559,#295560),(#295561,#295562),
(#295563,#295564),(#295565,#295566),(#295567,#295568),(#295569,#295570),
(#295571,#295572),(#295573,#295574),(#295575,#295576),(#295577,#295578),
(#295579,#295580),(#295581,#295582),(#295583,#295584),(#295585,#295586),
(#295587,#295588),(#295589,#295590),(#295591,#295592),(#295593,#295594),
(#295595,#295596),(#295597,#295598),(#295599,#295600),(#295601,#295602),
(#295603,#295604),(#295605,#295606),(#295607,#295608),(#295609,#295610),
(#295611,#295612),(#295613,#295614),(#295615,#295616),(#295617,#295618),
(#295619,#295620),(#295621,#295622),(#295623,#295624),(#295625,#295626),
(#295627,#295628),(#295629,#295630),(#295631,#295632),(#295633,#295634),
(#295635,#295636),(#295637,#295638),(#295639,#295640),(#295641,#295642),
(#295643,#295644),(#295645,#295646),(#295647,#295648),(#295649,#295650),
(#295651,#295652),(#295653,#295654),(#295655,#295656),(#295657,#295658),
(#295659,#295660),(#295661,#295662),(#295663,#295664),(#295665,#295666),
(#295667,#295668),(#295669,#295670),(#295671,#295672),(#295673,#295674),
(#295675,#295676),(#295677,#295678),(#295679,#295680),(#295681,#295682),
(#295683,#295684),(#295685,#295686),(#295687,#295688),(#295689,#295690),
(#295691,#295692),(#295693,#295694),(#295695,#295696),(#295697,#295698),
(#295699,#295700),(#295701,#295702),(#295703,#295704),(#295705,#295706),
(#295707,#295708),(#295709,#295710),(#295711,#295712),(#295713,#295714),
(#295715,#295716),(#295717,#295718),(#295719,#295720),(#295721,#295722),
(#295723,#295724),(#295725,#295726),(#295727,#295728),(#295729,#295730),
(#295731,#295732),(#295733,#295734),(#295735,#295736),(#295737,#295738),
(#295739,#295740),(#295741,#295742),(#295743,#295744),(#295745,#295746),
(#295747,#295748),(#295749,#295750)),.UNSPECIFIED.,.F.,.F.,.F.,(6,1,1,1,
1,1,1,1,1,1,1,1,1,1,1,1,1,1,1,1,1,1,1,1,1,1,1,1,1,1,1,1,1,1,1,1,1,1,1,1,
1,1,1,1,1,1,1,1,1,1,1,1,1,1,1,1,1,1,1,1,1,1,1,1,1,1,1,1,1,1,1,1,1,1,1,1,
1,1,1,1,1,1,1,1,1,1,1,1,1,1,1,1,1,1,1,1,1,1,1,1,1,1,1,1,1,1,1,1,1,1,1,1,
1,1,1,1,1,1,1,1,1,1,1,1,1,1,1,1,1,1,1,1,1,1,1,1,1,1,1,1,1,1,1,1,1,1,1,1,
1,1,1,1,1,1,1,1,1,1,1,1,1,1,1,1,1,1,1,1,1,1,1,1,1,1,1,1,1,1,1,1,1,1,1,1,
1,1,1,1,1,1,1,1,1,1,1,1,1,1,1,1,1,1,1,1,1,1,1,1,1,1,1,1,1,1,1,1,1,1,1,1,
1,1,1,1,1,1,1,1,1,1,1,1,1,1,1,1,1,1,1,1,1,1,1,1,1,1,1,1,1,1,1,1,1,1,1,1,
1,1,1,1,1,1,1,1,1,1,1,1,1,1,1,1,1,1,1,1,1,1,1,1,1,1,1,1,1,1,1,1,1,1,1,1,
1,1,1,1,1,1,1,1,1,1,1,1,1,1,1,1,1,1,1,1,1,1,1,1,1,1,1,1,1,1,1,1,1,1,1,1,
1,1,1,1,1,1,1,1,1,1,1,1,1,1,1,1,1,1,1,1,1,1,1,1,1,1,1,1,1,1,1,1,1,1,1,1,
1,1,1,1,1,1,1,1,1,1,1,1,1,1,1,1,1,1,1,1,1,1,1,1,1,1,1,1,1,1,1,1,1,1,1,1,
1,1,1,1,1,1,1,1,1,1,1,1,1,1,1,1,1,1,1,1,1,1,1,1,1,1,1,1,1,1,1,1,1,1,1,1,
1,1,1,1,1,1,1,1,1,1,1,1,1,1,1,1,1,1,1,1,1,1,1,1,1,1,1,1,1,1,1,6),(2,2),
(-1.,-0.998165138,-0.996330275,-0.994495413,-0.99266055,-0.990825688,-0.988990826,
-0.987155963,-0.985321101,-0.983486239,-0.981651376,-0.979816514,-0.977981651,
-0.976146789,-0.974311927,-0.972477064,-0.970642202,-0.968807339,-0.966972477,
-0.965137615,-0.963302752,-0.96146789,-0.959633028,-0.957798165,-0.955963303,
-0.95412844,-0.952293578,-0.950458716,-0.948623853,-0.946788991,-0.944954128,
-0.943119266,-0.941284404,-0.939449541,-0.937614679,-0.935779817,-0.933944954,
-0.932110092,-0.930275229,-0.928440367,-0.926605505,-0.924770642,-0.92293578,
-0.921100917,-0.919266055,-0.917431193,-0.91559633,-0.913761468,-0.911926606,
-0.910091743,-0.908256881,-0.906422018,-0.904587156,-0.902752294,-0.900917431,
-0.899082569,-0.897247706,-0.895412844,-0.893577982,-0.891743119,-0.889908257,
-0.888073394,-0.886238532,-0.88440367,-0.882568807,-0.880733945,-0.878899083,
-0.87706422,-0.875229358,-0.873394495,-0.871559633,-0.869724771,-0.867889908,
-0.866055046,-0.864220183,-0.862385321,-0.860550459,-0.858715596,-0.856880734,
-0.855045872,-0.853211009,-0.851376147,-0.849541284,-0.847706422,-0.84587156,
-0.844036697,-0.842201835,-0.840366972,-0.83853211,-0.836697248,-0.834862385,
-0.833027523,-0.831192661,-0.829357798,-0.827522936,-0.825688073,-0.823853211,
-0.822018349,-0.820183486,-0.818348624,-0.816513761,-0.814678899,-0.812844037,
-0.811009174,-0.809174312,-0.80733945,-0.805504587,-0.803669725,-0.801834862,
-0.8,-0.798165138,-0.796330275,-0.794495413,-0.79266055,-0.790825688,-0.788990826,
-0.787155963,-0.785321101,-0.783486239,-0.781651376,-0.779816514,-0.777981651,
-0.776146789,-0.774311927,-0.772477064,-0.770642202,-0.768807339,-0.766972477,
-0.765137615,-0.763302752,-0.76146789,-0.759633028,-0.757798165,-0.755963303,
-0.75412844,-0.752293578,-0.750458716,-0.748623853,-0.746788991,-0.744954128,
-0.743119266,-0.741284404,-0.739449541,-0.737614679,-0.735779817,-0.733944954,
-0.732110092,-0.730275229,-0.728440367,-0.726605505,-0.724770642,-0.72293578,
-0.721100917,-0.719266055,-0.717431193,-0.71559633,-0.713761468,-0.711926606,
-0.710091743,-0.708256881,-0.706422018,-0.704587156,-0.702752294,-0.700917431,
-0.699082569,-0.697247706,-0.695412844,-0.693577982,-0.691743119,-0.689908257,
-0.688073394,-0.686238532,-0.68440367,-0.682568807,-0.680733945,-0.678899083,
-0.67706422,-0.675229358,-0.673394495,-0.671559633,-0.669724771,-0.667889908,
-0.666055046,-0.664220183,-0.662385321,-0.660550459,-0.658715596,-0.656880734,
-0.655045872,-0.653211009,-0.651376147,-0.649541284,-0.647706422,-0.64587156,
-0.644036697,-0.642201835,-0.640366972,-0.63853211,-0.636697248,-0.634862385,
-0.633027523,-0.631192661,-0.629357798,-0.627522936,-0.625688073,-0.623853211,
-0.622018349,-0.620183486,-0.618348624,-0.616513761,-0.614678899,-0.612844037,
-0.611009174,-0.609174312,-0.60733945,-0.605504587,-0.603669725,-0.601834862,
-0.6,-0.598165138,-0.596330275,-0.594495413,-0.59266055,-0.590825688,-0.588990826,
-0.587155963,-0.585321101,-0.583486239,-0.581651376,-0.579816514,-0.577981651,
-0.576146789,-0.574311927,-0.572477064,-0.570642202,-0.568807339,-0.566972477,
-0.565137615,-0.563302752,-0.56146789,-0.559633028,-0.557798165,-0.555963303,
-0.55412844,-0.552293578,-0.550458716,-0.548623853,-0.546788991,-0.544954128,
-0.543119266,-0.541284404,-0.539449541,-0.537614679,-0.535779817,-0.533944954,
-0.532110092,-0.530275229,-0.528440367,-0.526605505,-0.524770642,-0.52293578,
-0.521100917,-0.519266055,-0.517431193,-0.51559633,-0.513761468,-0.511926606,
-0.510091743,-0.508256881,-0.506422018,-0.504587156,-0.502752294,-0.500917431,
-0.499082569,-0.497247706,-0.495412844,-0.493577982,-0.491743119,-0.489908257,
-0.488073394,-0.486238532,-0.48440367,-0.482568807,-0.480733945,-0.478899083,
-0.47706422,-0.475229358,-0.473394495,-0.471559633,-0.469724771,-0.467889908,
-0.466055046,-0.464220183,-0.462385321,-0.460550459,-0.458715596,-0.456880734,
-0.455045872,-0.453211009,-0.451376147,-0.449541284,-0.447706422,-0.44587156,
-0.444036697,-0.442201835,-0.440366972,-0.43853211,-0.436697248,-0.434862385,
-0.433027523,-0.431192661,-0.429357798,-0.427522936,-0.425688073,-0.423853211,
-0.422018349,-0.420183486,-0.418348624,-0.416513761,-0.414678899,-0.412844037,
-0.411009174,-0.409174312,-0.40733945,-0.405504587,-0.403669725,-0.401834862,
-0.4,-0.398165138,-0.396330275,-0.394495413,-0.39266055,-0.390825688,-0.388990826,
-0.387155963,-0.385321101,-0.383486239,-0.381651376,-0.379816514,-0.377981651,
-0.376146789,-0.374311927,-0.372477064,-0.370642202,-0.368807339,-0.366972477,
-0.365137615,-0.363302752,-0.36146789,-0.359633028,-0.357798165,-0.355963303,
-0.35412844,-0.352293578,-0.350458716,-0.348623853,-0.346788991,-0.344954128,
-0.343119266,-0.341284404,-0.339449541,-0.337614679,-0.335779817,-0.333944954,
-0.332110092,-0.330275229,-0.328440367,-0.326605505,-0.324770642,-0.32293578,
-0.321100917,-0.319266055,-0.317431193,-0.31559633,-0.313761468,-0.311926606,
-0.310091743,-0.308256881,-0.306422018,-0.304587156,-0.302752294,-0.300917431,
-0.299082569,-0.297247706,-0.295412844,-0.293577982,-0.291743119,-0.289908257,
-0.288073394,-0.286238532,-0.28440367,-0.282568807,-0.280733945,-0.278899083,
-0.27706422,-0.275229358,-0.273394495,-0.271559633,-0.269724771,-0.267889908,
-0.266055046,-0.264220183,-0.262385321,-0.260550459,-0.258715596,-0.256880734,
-0.255045872,-0.253211009,-0.251376147,-0.249541284,-0.247706422,-0.24587156,
-0.244036697,-0.242201835,-0.240366972,-0.23853211,-0.236697248,-0.234862385,
-0.233027523,-0.231192661,-0.229357798,-0.227522936,-0.225688073,-0.223853211,
-0.222018349,-0.220183486,-0.218348624,-0.216513761,-0.214678899,-0.212844037,
-0.211009174,-0.209174312,-0.20733945,-0.205504587,-0.203669725,-0.201834862,
-0.2,-0.198165138,-0.196330275,-0.194495413,-0.19266055,-0.190825688,-0.188990826,
-0.187155963,-0.185321101,-0.183486239,-0.181651376,-0.179816514,-0.177981651,
-0.176146789,-0.174311927,-0.172477064,-0.170642202,-0.168807339,-0.166972477,
-0.165137615,-0.163302752,-0.16146789,-0.159633028,-0.157798165,-0.155963303,
-0.15412844,-0.152293578,-0.150458716,-0.148623853,-0.146788991,-0.144954128,
-0.143172103),(0.,0.36),.UNSPECIFIED.);
#6301=B_SPLINE_SURFACE_WITH_KNOTS('',5,1,((#297515,#297516),(#297517,#297518),
(#297519,#297520),(#297521,#297522),(#297523,#297524),(#297525,#297526),
(#297527,#297528),(#297529,#297530),(#297531,#297532),(#297533,#297534),
(#297535,#297536),(#297537,#297538),(#297539,#297540),(#297541,#297542),
(#297543,#297544),(#297545,#297546),(#297547,#297548),(#297549,#297550),
(#297551,#297552),(#297553,#297554),(#297555,#297556),(#297557,#297558),
(#297559,#297560),(#297561,#297562),(#297563,#297564),(#297565,#297566),
(#297567,#297568),(#297569,#297570),(#297571,#297572),(#297573,#297574),
(#297575,#297576),(#297577,#297578),(#297579,#297580),(#297581,#297582),
(#297583,#297584),(#297585,#297586),(#297587,#297588),(#297589,#297590),
(#297591,#297592),(#297593,#297594),(#297595,#297596),(#297597,#297598),
(#297599,#297600),(#297601,#297602),(#297603,#297604),(#297605,#297606),
(#297607,#297608),(#297609,#297610),(#297611,#297612),(#297613,#297614),
(#297615,#297616),(#297617,#297618),(#297619,#297620),(#297621,#297622),
(#297623,#297624),(#297625,#297626),(#297627,#297628),(#297629,#297630),
(#297631,#297632),(#297633,#297634),(#297635,#297636),(#297637,#297638),
(#297639,#297640),(#297641,#297642),(#297643,#297644),(#297645,#297646),
(#297647,#297648),(#297649,#297650),(#297651,#297652),(#297653,#297654),
(#297655,#297656),(#297657,#297658),(#297659,#297660),(#297661,#297662),
(#297663,#297664),(#297665,#297666),(#297667,#297668),(#297669,#297670),
(#297671,#297672),(#297673,#297674),(#297675,#297676),(#297677,#297678),
(#297679,#297680),(#297681,#297682),(#297683,#297684),(#297685,#297686),
(#297687,#297688),(#297689,#297690),(#297691,#297692),(#297693,#297694),
(#297695,#297696),(#297697,#297698),(#297699,#297700),(#297701,#297702),
(#297703,#297704),(#297705,#297706),(#297707,#297708),(#297709,#297710),
(#297711,#297712),(#297713,#297714),(#297715,#297716),(#297717,#297718),
(#297719,#297720),(#297721,#297722),(#297723,#297724),(#297725,#297726),
(#297727,#297728),(#297729,#297730),(#297731,#297732),(#297733,#297734),
(#297735,#297736),(#297737,#297738),(#297739,#297740),(#297741,#297742),
(#297743,#297744),(#297745,#297746),(#297747,#297748),(#297749,#297750),
(#297751,#297752),(#297753,#297754),(#297755,#297756),(#297757,#297758),
(#297759,#297760),(#297761,#297762),(#297763,#297764),(#297765,#297766),
(#297767,#297768),(#297769,#297770),(#297771,#297772),(#297773,#297774),
(#297775,#297776),(#297777,#297778),(#297779,#297780),(#297781,#297782),
(#297783,#297784),(#297785,#297786),(#297787,#297788),(#297789,#297790),
(#297791,#297792),(#297793,#297794),(#297795,#297796),(#297797,#297798),
(#297799,#297800),(#297801,#297802),(#297803,#297804),(#297805,#297806),
(#297807,#297808),(#297809,#297810),(#297811,#297812),(#297813,#297814),
(#297815,#297816),(#297817,#297818),(#297819,#297820),(#297821,#297822),
(#297823,#297824),(#297825,#297826),(#297827,#297828),(#297829,#297830),
(#297831,#297832),(#297833,#297834),(#297835,#297836),(#297837,#297838),
(#297839,#297840),(#297841,#297842),(#297843,#297844),(#297845,#297846),
(#297847,#297848),(#297849,#297850),(#297851,#297852),(#297853,#297854),
(#297855,#297856),(#297857,#297858),(#297859,#297860),(#297861,#297862),
(#297863,#297864),(#297865,#297866),(#297867,#297868),(#297869,#297870),
(#297871,#297872),(#297873,#297874),(#297875,#297876),(#297877,#297878),
(#297879,#297880),(#297881,#297882),(#297883,#297884),(#297885,#297886),
(#297887,#297888),(#297889,#297890),(#297891,#297892),(#297893,#297894),
(#297895,#297896),(#297897,#297898),(#297899,#297900),(#297901,#297902),
(#297903,#297904),(#297905,#297906),(#297907,#297908),(#297909,#297910),
(#297911,#297912),(#297913,#297914),(#297915,#297916),(#297917,#297918),
(#297919,#297920),(#297921,#297922),(#297923,#297924),(#297925,#297926),
(#297927,#297928),(#297929,#297930),(#297931,#297932),(#297933,#297934),
(#297935,#297936),(#297937,#297938),(#297939,#297940),(#297941,#297942),
(#297943,#297944),(#297945,#297946),(#297947,#297948),(#297949,#297950),
(#297951,#297952),(#297953,#297954),(#297955,#297956),(#297957,#297958),
(#297959,#297960),(#297961,#297962),(#297963,#297964),(#297965,#297966),
(#297967,#297968),(#297969,#297970),(#297971,#297972),(#297973,#297974),
(#297975,#297976),(#297977,#297978),(#297979,#297980),(#297981,#297982),
(#297983,#297984),(#297985,#297986),(#297987,#297988),(#297989,#297990),
(#297991,#297992),(#297993,#297994),(#297995,#297996),(#297997,#297998),
(#297999,#298000),(#298001,#298002),(#298003,#298004),(#298005,#298006),
(#298007,#298008),(#298009,#298010),(#298011,#298012),(#298013,#298014),
(#298015,#298016),(#298017,#298018),(#298019,#298020),(#298021,#298022),
(#298023,#298024),(#298025,#298026),(#298027,#298028),(#298029,#298030),
(#298031,#298032),(#298033,#298034),(#298035,#298036),(#298037,#298038),
(#298039,#298040),(#298041,#298042),(#298043,#298044),(#298045,#298046),
(#298047,#298048),(#298049,#298050),(#298051,#298052),(#298053,#298054),
(#298055,#298056),(#298057,#298058),(#298059,#298060),(#298061,#298062),
(#298063,#298064),(#298065,#298066),(#298067,#298068),(#298069,#298070),
(#298071,#298072),(#298073,#298074),(#298075,#298076),(#298077,#298078),
(#298079,#298080),(#298081,#298082),(#298083,#298084),(#298085,#298086),
(#298087,#298088),(#298089,#298090),(#298091,#298092),(#298093,#298094),
(#298095,#298096),(#298097,#298098),(#298099,#298100),(#298101,#298102),
(#298103,#298104),(#298105,#298106),(#298107,#298108),(#298109,#298110),
(#298111,#298112),(#298113,#298114),(#298115,#298116),(#298117,#298118),
(#298119,#298120),(#298121,#298122),(#298123,#298124),(#298125,#298126),
(#298127,#298128),(#298129,#298130),(#298131,#298132),(#298133,#298134),
(#298135,#298136),(#298137,#298138),(#298139,#298140),(#298141,#298142),
(#298143,#298144),(#298145,#298146),(#298147,#298148),(#298149,#298150),
(#298151,#298152),(#298153,#298154),(#298155,#298156),(#298157,#298158),
(#298159,#298160),(#298161,#298162),(#298163,#298164),(#298165,#298166),
(#298167,#298168),(#298169,#298170),(#298171,#298172),(#298173,#298174),
(#298175,#298176),(#298177,#298178),(#298179,#298180),(#298181,#298182),
(#298183,#298184),(#298185,#298186),(#298187,#298188),(#298189,#298190),
(#298191,#298192),(#298193,#298194),(#298195,#298196),(#298197,#298198),
(#298199,#298200),(#298201,#298202),(#298203,#298204),(#298205,#298206),
(#298207,#298208),(#298209,#298210),(#298211,#298212),(#298213,#298214),
(#298215,#298216),(#298217,#298218),(#298219,#298220),(#298221,#298222),
(#298223,#298224),(#298225,#298226),(#298227,#298228),(#298229,#298230),
(#298231,#298232),(#298233,#298234),(#298235,#298236),(#298237,#298238),
(#298239,#298240),(#298241,#298242),(#298243,#298244),(#298245,#298246),
(#298247,#298248),(#298249,#298250),(#298251,#298252),(#298253,#298254),
(#298255,#298256),(#298257,#298258),(#298259,#298260),(#298261,#298262),
(#298263,#298264),(#298265,#298266),(#298267,#298268),(#298269,#298270),
(#298271,#298272),(#298273,#298274),(#298275,#298276),(#298277,#298278),
(#298279,#298280),(#298281,#298282),(#298283,#298284),(#298285,#298286),
(#298287,#298288),(#298289,#298290),(#298291,#298292),(#298293,#298294),
(#298295,#298296),(#298297,#298298),(#298299,#298300),(#298301,#298302),
(#298303,#298304),(#298305,#298306),(#298307,#298308),(#298309,#298310),
(#298311,#298312),(#298313,#298314),(#298315,#298316),(#298317,#298318),
(#298319,#298320),(#298321,#298322),(#298323,#298324),(#298325,#298326),
(#298327,#298328),(#298329,#298330),(#298331,#298332),(#298333,#298334),
(#298335,#298336),(#298337,#298338),(#298339,#298340),(#298341,#298342),
(#298343,#298344),(#298345,#298346),(#298347,#298348),(#298349,#298350),
(#298351,#298352),(#298353,#298354),(#298355,#298356),(#298357,#298358),
(#298359,#298360),(#298361,#298362),(#298363,#298364),(#298365,#298366),
(#298367,#298368),(#298369,#298370),(#298371,#298372),(#298373,#298374),
(#298375,#298376),(#298377,#298378),(#298379,#298380),(#298381,#298382),
(#298383,#298384),(#298385,#298386),(#298387,#298388),(#298389,#298390),
(#298391,#298392),(#298393,#298394),(#298395,#298396),(#298397,#298398),
(#298399,#298400),(#298401,#298402),(#298403,#298404),(#298405,#298406),
(#298407,#298408),(#298409,#298410),(#298411,#298412),(#298413,#298414),
(#298415,#298416),(#298417,#298418),(#298419,#298420),(#298421,#298422),
(#298423,#298424),(#298425,#298426),(#298427,#298428),(#298429,#298430),
(#298431,#298432),(#298433,#298434),(#298435,#298436),(#298437,#298438),
(#298439,#298440),(#298441,#298442),(#298443,#298444),(#298445,#298446),
(#298447,#298448),(#298449,#298450),(#298451,#298452),(#298453,#298454),
(#298455,#298456),(#298457,#298458)),.UNSPECIFIED.,.F.,.F.,.F.,(6,1,1,1,
1,1,1,1,1,1,1,1,1,1,1,1,1,1,1,1,1,1,1,1,1,1,1,1,1,1,1,1,1,1,1,1,1,1,1,1,
1,1,1,1,1,1,1,1,1,1,1,1,1,1,1,1,1,1,1,1,1,1,1,1,1,1,1,1,1,1,1,1,1,1,1,1,
1,1,1,1,1,1,1,1,1,1,1,1,1,1,1,1,1,1,1,1,1,1,1,1,1,1,1,1,1,1,1,1,1,1,1,1,
1,1,1,1,1,1,1,1,1,1,1,1,1,1,1,1,1,1,1,1,1,1,1,1,1,1,1,1,1,1,1,1,1,1,1,1,
1,1,1,1,1,1,1,1,1,1,1,1,1,1,1,1,1,1,1,1,1,1,1,1,1,1,1,1,1,1,1,1,1,1,1,1,
1,1,1,1,1,1,1,1,1,1,1,1,1,1,1,1,1,1,1,1,1,1,1,1,1,1,1,1,1,1,1,1,1,1,1,1,
1,1,1,1,1,1,1,1,1,1,1,1,1,1,1,1,1,1,1,1,1,1,1,1,1,1,1,1,1,1,1,1,1,1,1,1,
1,1,1,1,1,1,1,1,1,1,1,1,1,1,1,1,1,1,1,1,1,1,1,1,1,1,1,1,1,1,1,1,1,1,1,1,
1,1,1,1,1,1,1,1,1,1,1,1,1,1,1,1,1,1,1,1,1,1,1,1,1,1,1,1,1,1,1,1,1,1,1,1,
1,1,1,1,1,1,1,1,1,1,1,1,1,1,1,1,1,1,1,1,1,1,1,1,1,1,1,1,1,1,1,1,1,1,1,1,
1,1,1,1,1,1,1,1,1,1,1,1,1,1,1,1,1,1,1,1,1,1,1,1,1,1,1,1,1,1,1,1,1,1,1,1,
1,1,1,1,1,1,1,1,1,1,1,1,1,1,1,1,1,1,1,1,1,1,1,1,1,1,1,1,1,1,1,1,1,1,1,1,
1,1,1,1,1,1,1,1,1,1,1,1,1,1,1,1,1,1,1,1,1,1,1,1,1,1,1,1,1,1,1,6),(2,2),
(-1.,-0.998165138,-0.996330275,-0.994495413,-0.99266055,-0.990825688,-0.988990826,
-0.987155963,-0.985321101,-0.983486239,-0.981651376,-0.979816514,-0.977981651,
-0.976146789,-0.974311927,-0.972477064,-0.970642202,-0.968807339,-0.966972477,
-0.965137615,-0.963302752,-0.96146789,-0.959633028,-0.957798165,-0.955963303,
-0.95412844,-0.952293578,-0.950458716,-0.948623853,-0.946788991,-0.944954128,
-0.943119266,-0.941284404,-0.939449541,-0.937614679,-0.935779817,-0.933944954,
-0.932110092,-0.930275229,-0.928440367,-0.926605505,-0.924770642,-0.92293578,
-0.921100917,-0.919266055,-0.917431193,-0.91559633,-0.913761468,-0.911926606,
-0.910091743,-0.908256881,-0.906422018,-0.904587156,-0.902752294,-0.900917431,
-0.899082569,-0.897247706,-0.895412844,-0.893577982,-0.891743119,-0.889908257,
-0.888073394,-0.886238532,-0.88440367,-0.882568807,-0.880733945,-0.878899083,
-0.87706422,-0.875229358,-0.873394495,-0.871559633,-0.869724771,-0.867889908,
-0.866055046,-0.864220183,-0.862385321,-0.860550459,-0.858715596,-0.856880734,
-0.855045872,-0.853211009,-0.851376147,-0.849541284,-0.847706422,-0.84587156,
-0.844036697,-0.842201835,-0.840366972,-0.83853211,-0.836697248,-0.834862385,
-0.833027523,-0.831192661,-0.829357798,-0.827522936,-0.825688073,-0.823853211,
-0.822018349,-0.820183486,-0.818348624,-0.816513761,-0.814678899,-0.812844037,
-0.811009174,-0.809174312,-0.80733945,-0.805504587,-0.803669725,-0.801834862,
-0.8,-0.798165138,-0.796330275,-0.794495413,-0.79266055,-0.790825688,-0.788990826,
-0.787155963,-0.785321101,-0.783486239,-0.781651376,-0.779816514,-0.777981651,
-0.776146789,-0.774311927,-0.772477064,-0.770642202,-0.768807339,-0.766972477,
-0.765137615,-0.763302752,-0.76146789,-0.759633028,-0.757798165,-0.755963303,
-0.75412844,-0.752293578,-0.750458716,-0.748623853,-0.746788991,-0.744954128,
-0.743119266,-0.741284404,-0.739449541,-0.737614679,-0.735779817,-0.733944954,
-0.732110092,-0.730275229,-0.728440367,-0.726605505,-0.724770642,-0.72293578,
-0.721100917,-0.719266055,-0.717431193,-0.71559633,-0.713761468,-0.711926606,
-0.710091743,-0.708256881,-0.706422018,-0.704587156,-0.702752294,-0.700917431,
-0.699082569,-0.697247706,-0.695412844,-0.693577982,-0.691743119,-0.689908257,
-0.688073394,-0.686238532,-0.68440367,-0.682568807,-0.680733945,-0.678899083,
-0.67706422,-0.675229358,-0.673394495,-0.671559633,-0.669724771,-0.667889908,
-0.666055046,-0.664220183,-0.662385321,-0.660550459,-0.658715596,-0.656880734,
-0.655045872,-0.653211009,-0.651376147,-0.649541284,-0.647706422,-0.64587156,
-0.644036697,-0.642201835,-0.640366972,-0.63853211,-0.636697248,-0.634862385,
-0.633027523,-0.631192661,-0.629357798,-0.627522936,-0.625688073,-0.623853211,
-0.622018349,-0.620183486,-0.618348624,-0.616513761,-0.614678899,-0.612844037,
-0.611009174,-0.609174312,-0.60733945,-0.605504587,-0.603669725,-0.601834862,
-0.6,-0.598165138,-0.596330275,-0.594495413,-0.59266055,-0.590825688,-0.588990826,
-0.587155963,-0.585321101,-0.583486239,-0.581651376,-0.579816514,-0.577981651,
-0.576146789,-0.574311927,-0.572477064,-0.570642202,-0.568807339,-0.566972477,
-0.565137615,-0.563302752,-0.56146789,-0.559633028,-0.557798165,-0.555963303,
-0.55412844,-0.552293578,-0.550458716,-0.548623853,-0.546788991,-0.544954128,
-0.543119266,-0.541284404,-0.539449541,-0.537614679,-0.535779817,-0.533944954,
-0.532110092,-0.530275229,-0.528440367,-0.526605505,-0.524770642,-0.52293578,
-0.521100917,-0.519266055,-0.517431193,-0.51559633,-0.513761468,-0.511926606,
-0.510091743,-0.508256881,-0.506422018,-0.504587156,-0.502752294,-0.500917431,
-0.499082569,-0.497247706,-0.495412844,-0.493577982,-0.491743119,-0.489908257,
-0.488073394,-0.486238532,-0.48440367,-0.482568807,-0.480733945,-0.478899083,
-0.47706422,-0.475229358,-0.473394495,-0.471559633,-0.469724771,-0.467889908,
-0.466055046,-0.464220183,-0.462385321,-0.460550459,-0.458715596,-0.456880734,
-0.455045872,-0.453211009,-0.451376147,-0.449541284,-0.447706422,-0.44587156,
-0.444036697,-0.442201835,-0.440366972,-0.43853211,-0.436697248,-0.434862385,
-0.433027523,-0.431192661,-0.429357798,-0.427522936,-0.425688073,-0.423853211,
-0.422018349,-0.420183486,-0.418348624,-0.416513761,-0.414678899,-0.412844037,
-0.411009174,-0.409174312,-0.40733945,-0.405504587,-0.403669725,-0.401834862,
-0.4,-0.398165138,-0.396330275,-0.394495413,-0.39266055,-0.390825688,-0.388990826,
-0.387155963,-0.385321101,-0.383486239,-0.381651376,-0.379816514,-0.377981651,
-0.376146789,-0.374311927,-0.372477064,-0.370642202,-0.368807339,-0.366972477,
-0.365137615,-0.363302752,-0.36146789,-0.359633028,-0.357798165,-0.355963303,
-0.35412844,-0.352293578,-0.350458716,-0.348623853,-0.346788991,-0.344954128,
-0.343119266,-0.341284404,-0.339449541,-0.337614679,-0.335779817,-0.333944954,
-0.332110092,-0.330275229,-0.328440367,-0.326605505,-0.324770642,-0.32293578,
-0.321100917,-0.319266055,-0.317431193,-0.31559633,-0.313761468,-0.311926606,
-0.310091743,-0.308256881,-0.306422018,-0.304587156,-0.302752294,-0.300917431,
-0.299082569,-0.297247706,-0.295412844,-0.293577982,-0.291743119,-0.289908257,
-0.288073394,-0.286238532,-0.28440367,-0.282568807,-0.280733945,-0.278899083,
-0.27706422,-0.275229358,-0.273394495,-0.271559633,-0.269724771,-0.267889908,
-0.266055046,-0.264220183,-0.262385321,-0.260550459,-0.258715596,-0.256880734,
-0.255045872,-0.253211009,-0.251376147,-0.249541284,-0.247706422,-0.24587156,
-0.244036697,-0.242201835,-0.240366972,-0.23853211,-0.236697248,-0.234862385,
-0.233027523,-0.231192661,-0.229357798,-0.227522936,-0.225688073,-0.223853211,
-0.222018349,-0.220183486,-0.218348624,-0.216513761,-0.214678899,-0.212844037,
-0.211009174,-0.209174312,-0.20733945,-0.205504587,-0.203669725,-0.201834862,
-0.2,-0.198165138,-0.196330275,-0.194495413,-0.19266055,-0.190825688,-0.188990826,
-0.187155963,-0.185321101,-0.183486239,-0.181651376,-0.179816514,-0.177981651,
-0.176146789,-0.174311927,-0.172477064,-0.170642202,-0.168807339,-0.166972477,
-0.165137615,-0.163302752,-0.16146789,-0.159633028,-0.157798165,-0.155963303,
-0.15412844,-0.152293578,-0.150458716,-0.148623853,-0.146788991,-0.144954128,
-0.143172103),(0.,0.36),.UNSPECIFIED.);
#6302=B_SPLINE_SURFACE_WITH_KNOTS('',5,1,((#298930,#298931),(#298932,#298933),
(#298934,#298935),(#298936,#298937),(#298938,#298939),(#298940,#298941),
(#298942,#298943),(#298944,#298945),(#298946,#298947),(#298948,#298949),
(#298950,#298951),(#298952,#298953),(#298954,#298955),(#298956,#298957),
(#298958,#298959),(#298960,#298961),(#298962,#298963),(#298964,#298965),
(#298966,#298967),(#298968,#298969),(#298970,#298971),(#298972,#298973),
(#298974,#298975),(#298976,#298977),(#298978,#298979),(#298980,#298981),
(#298982,#298983),(#298984,#298985),(#298986,#298987),(#298988,#298989),
(#298990,#298991),(#298992,#298993),(#298994,#298995),(#298996,#298997),
(#298998,#298999),(#299000,#299001),(#299002,#299003),(#299004,#299005),
(#299006,#299007),(#299008,#299009),(#299010,#299011),(#299012,#299013),
(#299014,#299015),(#299016,#299017),(#299018,#299019),(#299020,#299021),
(#299022,#299023),(#299024,#299025),(#299026,#299027),(#299028,#299029),
(#299030,#299031),(#299032,#299033),(#299034,#299035),(#299036,#299037),
(#299038,#299039),(#299040,#299041),(#299042,#299043),(#299044,#299045),
(#299046,#299047),(#299048,#299049),(#299050,#299051),(#299052,#299053),
(#299054,#299055),(#299056,#299057),(#299058,#299059),(#299060,#299061),
(#299062,#299063),(#299064,#299065),(#299066,#299067),(#299068,#299069),
(#299070,#299071),(#299072,#299073),(#299074,#299075),(#299076,#299077),
(#299078,#299079),(#299080,#299081),(#299082,#299083),(#299084,#299085),
(#299086,#299087),(#299088,#299089),(#299090,#299091),(#299092,#299093),
(#299094,#299095),(#299096,#299097),(#299098,#299099),(#299100,#299101),
(#299102,#299103),(#299104,#299105),(#299106,#299107),(#299108,#299109),
(#299110,#299111),(#299112,#299113),(#299114,#299115),(#299116,#299117),
(#299118,#299119),(#299120,#299121),(#299122,#299123),(#299124,#299125),
(#299126,#299127),(#299128,#299129),(#299130,#299131),(#299132,#299133),
(#299134,#299135),(#299136,#299137),(#299138,#299139),(#299140,#299141),
(#299142,#299143),(#299144,#299145),(#299146,#299147),(#299148,#299149),
(#299150,#299151),(#299152,#299153),(#299154,#299155),(#299156,#299157),
(#299158,#299159),(#299160,#299161),(#299162,#299163),(#299164,#299165),
(#299166,#299167),(#299168,#299169),(#299170,#299171),(#299172,#299173),
(#299174,#299175),(#299176,#299177),(#299178,#299179),(#299180,#299181),
(#299182,#299183),(#299184,#299185),(#299186,#299187),(#299188,#299189),
(#299190,#299191),(#299192,#299193),(#299194,#299195),(#299196,#299197),
(#299198,#299199),(#299200,#299201),(#299202,#299203),(#299204,#299205),
(#299206,#299207),(#299208,#299209),(#299210,#299211),(#299212,#299213),
(#299214,#299215),(#299216,#299217),(#299218,#299219),(#299220,#299221),
(#299222,#299223),(#299224,#299225),(#299226,#299227),(#299228,#299229),
(#299230,#299231),(#299232,#299233),(#299234,#299235),(#299236,#299237),
(#299238,#299239),(#299240,#299241),(#299242,#299243),(#299244,#299245),
(#299246,#299247),(#299248,#299249),(#299250,#299251),(#299252,#299253),
(#299254,#299255),(#299256,#299257),(#299258,#299259),(#299260,#299261),
(#299262,#299263),(#299264,#299265),(#299266,#299267),(#299268,#299269),
(#299270,#299271),(#299272,#299273),(#299274,#299275),(#299276,#299277),
(#299278,#299279),(#299280,#299281),(#299282,#299283),(#299284,#299285),
(#299286,#299287),(#299288,#299289),(#299290,#299291),(#299292,#299293),
(#299294,#299295),(#299296,#299297),(#299298,#299299),(#299300,#299301),
(#299302,#299303),(#299304,#299305),(#299306,#299307),(#299308,#299309),
(#299310,#299311),(#299312,#299313),(#299314,#299315),(#299316,#299317),
(#299318,#299319),(#299320,#299321),(#299322,#299323),(#299324,#299325),
(#299326,#299327),(#299328,#299329),(#299330,#299331),(#299332,#299333),
(#299334,#299335),(#299336,#299337),(#299338,#299339),(#299340,#299341),
(#299342,#299343),(#299344,#299345),(#299346,#299347),(#299348,#299349),
(#299350,#299351),(#299352,#299353),(#299354,#299355),(#299356,#299357),
(#299358,#299359),(#299360,#299361),(#299362,#299363),(#299364,#299365),
(#299366,#299367),(#299368,#299369),(#299370,#299371),(#299372,#299373),
(#299374,#299375),(#299376,#299377),(#299378,#299379),(#299380,#299381),
(#299382,#299383),(#299384,#299385),(#299386,#299387),(#299388,#299389),
(#299390,#299391),(#299392,#299393),(#299394,#299395),(#299396,#299397),
(#299398,#299399),(#299400,#299401),(#299402,#299403),(#299404,#299405),
(#299406,#299407),(#299408,#299409),(#299410,#299411),(#299412,#299413),
(#299414,#299415),(#299416,#299417),(#299418,#299419),(#299420,#299421),
(#299422,#299423),(#299424,#299425),(#299426,#299427),(#299428,#299429),
(#299430,#299431),(#299432,#299433),(#299434,#299435),(#299436,#299437),
(#299438,#299439),(#299440,#299441),(#299442,#299443),(#299444,#299445),
(#299446,#299447),(#299448,#299449),(#299450,#299451),(#299452,#299453),
(#299454,#299455),(#299456,#299457),(#299458,#299459),(#299460,#299461),
(#299462,#299463),(#299464,#299465),(#299466,#299467),(#299468,#299469),
(#299470,#299471),(#299472,#299473),(#299474,#299475),(#299476,#299477),
(#299478,#299479),(#299480,#299481),(#299482,#299483),(#299484,#299485),
(#299486,#299487),(#299488,#299489),(#299490,#299491),(#299492,#299493),
(#299494,#299495),(#299496,#299497),(#299498,#299499),(#299500,#299501),
(#299502,#299503),(#299504,#299505),(#299506,#299507),(#299508,#299509),
(#299510,#299511),(#299512,#299513),(#299514,#299515),(#299516,#299517),
(#299518,#299519),(#299520,#299521),(#299522,#299523),(#299524,#299525),
(#299526,#299527),(#299528,#299529),(#299530,#299531),(#299532,#299533),
(#299534,#299535),(#299536,#299537),(#299538,#299539),(#299540,#299541),
(#299542,#299543),(#299544,#299545),(#299546,#299547),(#299548,#299549),
(#299550,#299551),(#299552,#299553),(#299554,#299555),(#299556,#299557),
(#299558,#299559),(#299560,#299561),(#299562,#299563),(#299564,#299565),
(#299566,#299567),(#299568,#299569),(#299570,#299571),(#299572,#299573),
(#299574,#299575),(#299576,#299577),(#299578,#299579),(#299580,#299581),
(#299582,#299583),(#299584,#299585),(#299586,#299587),(#299588,#299589),
(#299590,#299591),(#299592,#299593),(#299594,#299595),(#299596,#299597),
(#299598,#299599),(#299600,#299601),(#299602,#299603),(#299604,#299605),
(#299606,#299607),(#299608,#299609),(#299610,#299611),(#299612,#299613),
(#299614,#299615),(#299616,#299617),(#299618,#299619),(#299620,#299621),
(#299622,#299623),(#299624,#299625),(#299626,#299627),(#299628,#299629),
(#299630,#299631),(#299632,#299633),(#299634,#299635),(#299636,#299637),
(#299638,#299639),(#299640,#299641),(#299642,#299643),(#299644,#299645),
(#299646,#299647),(#299648,#299649),(#299650,#299651),(#299652,#299653),
(#299654,#299655),(#299656,#299657),(#299658,#299659),(#299660,#299661),
(#299662,#299663),(#299664,#299665),(#299666,#299667),(#299668,#299669),
(#299670,#299671),(#299672,#299673),(#299674,#299675),(#299676,#299677),
(#299678,#299679),(#299680,#299681),(#299682,#299683),(#299684,#299685),
(#299686,#299687),(#299688,#299689),(#299690,#299691),(#299692,#299693),
(#299694,#299695),(#299696,#299697),(#299698,#299699),(#299700,#299701),
(#299702,#299703),(#299704,#299705),(#299706,#299707),(#299708,#299709),
(#299710,#299711),(#299712,#299713),(#299714,#299715),(#299716,#299717),
(#299718,#299719),(#299720,#299721),(#299722,#299723),(#299724,#299725),
(#299726,#299727),(#299728,#299729),(#299730,#299731),(#299732,#299733),
(#299734,#299735),(#299736,#299737),(#299738,#299739),(#299740,#299741),
(#299742,#299743),(#299744,#299745),(#299746,#299747),(#299748,#299749),
(#299750,#299751),(#299752,#299753),(#299754,#299755),(#299756,#299757),
(#299758,#299759),(#299760,#299761),(#299762,#299763),(#299764,#299765),
(#299766,#299767),(#299768,#299769),(#299770,#299771),(#299772,#299773),
(#299774,#299775),(#299776,#299777),(#299778,#299779),(#299780,#299781),
(#299782,#299783),(#299784,#299785),(#299786,#299787),(#299788,#299789),
(#299790,#299791),(#299792,#299793),(#299794,#299795),(#299796,#299797),
(#299798,#299799),(#299800,#299801),(#299802,#299803),(#299804,#299805),
(#299806,#299807),(#299808,#299809),(#299810,#299811),(#299812,#299813),
(#299814,#299815),(#299816,#299817),(#299818,#299819),(#299820,#299821),
(#299822,#299823),(#299824,#299825),(#299826,#299827),(#299828,#299829),
(#299830,#299831),(#299832,#299833),(#299834,#299835),(#299836,#299837),
(#299838,#299839),(#299840,#299841),(#299842,#299843),(#299844,#299845),
(#299846,#299847),(#299848,#299849),(#299850,#299851),(#299852,#299853),
(#299854,#299855),(#299856,#299857),(#299858,#299859),(#299860,#299861),
(#299862,#299863),(#299864,#299865),(#299866,#299867),(#299868,#299869),
(#299870,#299871),(#299872,#299873)),.UNSPECIFIED.,.F.,.F.,.F.,(6,1,1,1,
1,1,1,1,1,1,1,1,1,1,1,1,1,1,1,1,1,1,1,1,1,1,1,1,1,1,1,1,1,1,1,1,1,1,1,1,
1,1,1,1,1,1,1,1,1,1,1,1,1,1,1,1,1,1,1,1,1,1,1,1,1,1,1,1,1,1,1,1,1,1,1,1,
1,1,1,1,1,1,1,1,1,1,1,1,1,1,1,1,1,1,1,1,1,1,1,1,1,1,1,1,1,1,1,1,1,1,1,1,
1,1,1,1,1,1,1,1,1,1,1,1,1,1,1,1,1,1,1,1,1,1,1,1,1,1,1,1,1,1,1,1,1,1,1,1,
1,1,1,1,1,1,1,1,1,1,1,1,1,1,1,1,1,1,1,1,1,1,1,1,1,1,1,1,1,1,1,1,1,1,1,1,
1,1,1,1,1,1,1,1,1,1,1,1,1,1,1,1,1,1,1,1,1,1,1,1,1,1,1,1,1,1,1,1,1,1,1,1,
1,1,1,1,1,1,1,1,1,1,1,1,1,1,1,1,1,1,1,1,1,1,1,1,1,1,1,1,1,1,1,1,1,1,1,1,
1,1,1,1,1,1,1,1,1,1,1,1,1,1,1,1,1,1,1,1,1,1,1,1,1,1,1,1,1,1,1,1,1,1,1,1,
1,1,1,1,1,1,1,1,1,1,1,1,1,1,1,1,1,1,1,1,1,1,1,1,1,1,1,1,1,1,1,1,1,1,1,1,
1,1,1,1,1,1,1,1,1,1,1,1,1,1,1,1,1,1,1,1,1,1,1,1,1,1,1,1,1,1,1,1,1,1,1,1,
1,1,1,1,1,1,1,1,1,1,1,1,1,1,1,1,1,1,1,1,1,1,1,1,1,1,1,1,1,1,1,1,1,1,1,1,
1,1,1,1,1,1,1,1,1,1,1,1,1,1,1,1,1,1,1,1,1,1,1,1,1,1,1,1,1,1,1,1,1,1,1,1,
1,1,1,1,1,1,1,1,1,1,1,1,1,1,1,1,1,1,1,1,1,1,1,1,1,1,1,1,1,1,1,6),(2,2),
(0.143172104,0.144954128,0.146788991,0.148623853,0.150458716,0.152293578,
0.15412844,0.155963303,0.157798165,0.159633028,0.16146789,0.163302752,0.165137615,
0.166972477,0.168807339,0.170642202,0.172477064,0.174311927,0.176146789,
0.177981651,0.179816514,0.181651376,0.183486239,0.185321101,0.187155963,
0.188990826,0.190825688,0.19266055,0.194495413,0.196330275,0.198165138,
0.2,0.201834862,0.203669725,0.205504587,0.20733945,0.209174312,0.211009174,
0.212844037,0.214678899,0.216513761,0.218348624,0.220183486,0.222018349,
0.223853211,0.225688073,0.227522936,0.229357798,0.231192661,0.233027523,
0.234862385,0.236697248,0.23853211,0.240366972,0.242201835,0.244036697,
0.24587156,0.247706422,0.249541284,0.251376147,0.253211009,0.255045872,
0.256880734,0.258715596,0.260550459,0.262385321,0.264220183,0.266055046,
0.267889908,0.269724771,0.271559633,0.273394495,0.275229358,0.27706422,
0.278899083,0.280733945,0.282568807,0.28440367,0.286238532,0.288073394,
0.289908257,0.291743119,0.293577982,0.295412844,0.297247706,0.299082569,
0.300917431,0.302752294,0.304587156,0.306422018,0.308256881,0.310091743,
0.311926606,0.313761468,0.31559633,0.317431193,0.319266055,0.321100917,
0.32293578,0.324770642,0.326605505,0.328440367,0.330275229,0.332110092,
0.333944954,0.335779817,0.337614679,0.339449541,0.341284404,0.343119266,
0.344954128,0.346788991,0.348623853,0.350458716,0.352293578,0.35412844,
0.355963303,0.357798165,0.359633028,0.36146789,0.363302752,0.365137615,
0.366972477,0.368807339,0.370642202,0.372477064,0.374311927,0.376146789,
0.377981651,0.379816514,0.381651376,0.383486239,0.385321101,0.387155963,
0.388990826,0.390825688,0.39266055,0.394495413,0.396330275,0.398165138,
0.4,0.401834862,0.403669725,0.405504587,0.40733945,0.409174312,0.411009174,
0.412844037,0.414678899,0.416513761,0.418348624,0.420183486,0.422018349,
0.423853211,0.425688073,0.427522936,0.429357798,0.431192661,0.433027523,
0.434862385,0.436697248,0.43853211,0.440366972,0.442201835,0.444036697,
0.44587156,0.447706422,0.449541284,0.451376147,0.453211009,0.455045872,
0.456880734,0.458715596,0.460550459,0.462385321,0.464220183,0.466055046,
0.467889908,0.469724771,0.471559633,0.473394495,0.475229358,0.47706422,
0.478899083,0.480733945,0.482568807,0.48440367,0.486238532,0.488073394,
0.489908257,0.491743119,0.493577982,0.495412844,0.497247706,0.499082569,
0.500917431,0.502752294,0.504587156,0.506422018,0.508256881,0.510091743,
0.511926606,0.513761468,0.51559633,0.517431193,0.519266055,0.521100917,
0.52293578,0.524770642,0.526605505,0.528440367,0.530275229,0.532110092,
0.533944954,0.535779817,0.537614679,0.539449541,0.541284404,0.543119266,
0.544954128,0.546788991,0.548623853,0.550458716,0.552293578,0.55412844,
0.555963303,0.557798165,0.559633028,0.56146789,0.563302752,0.565137615,
0.566972477,0.568807339,0.570642202,0.572477064,0.574311927,0.576146789,
0.577981651,0.579816514,0.581651376,0.583486239,0.585321101,0.587155963,
0.588990826,0.590825688,0.59266055,0.594495413,0.596330275,0.598165138,
0.6,0.601834862,0.603669725,0.605504587,0.60733945,0.609174312,0.611009174,
0.612844037,0.614678899,0.616513761,0.618348624,0.620183486,0.622018349,
0.623853211,0.625688073,0.627522936,0.629357798,0.631192661,0.633027523,
0.634862385,0.636697248,0.63853211,0.640366972,0.642201835,0.644036697,
0.64587156,0.647706422,0.649541284,0.651376147,0.653211009,0.655045872,
0.656880734,0.658715596,0.660550459,0.662385321,0.664220183,0.666055046,
0.667889908,0.669724771,0.671559633,0.673394495,0.675229358,0.67706422,
0.678899083,0.680733945,0.682568807,0.68440367,0.686238532,0.688073394,
0.689908257,0.691743119,0.693577982,0.695412844,0.697247706,0.699082569,
0.700917431,0.702752294,0.704587156,0.706422018,0.708256881,0.710091743,
0.711926606,0.713761468,0.71559633,0.717431193,0.719266055,0.721100917,
0.72293578,0.724770642,0.726605505,0.728440367,0.730275229,0.732110092,
0.733944954,0.735779817,0.737614679,0.739449541,0.741284404,0.743119266,
0.744954128,0.746788991,0.748623853,0.750458716,0.752293578,0.75412844,
0.755963303,0.757798165,0.759633028,0.76146789,0.763302752,0.765137615,
0.766972477,0.768807339,0.770642202,0.772477064,0.774311927,0.776146789,
0.777981651,0.779816514,0.781651376,0.783486239,0.785321101,0.787155963,
0.788990826,0.790825688,0.79266055,0.794495413,0.796330275,0.798165138,
0.8,0.801834862,0.803669725,0.805504587,0.80733945,0.809174312,0.811009174,
0.812844037,0.814678899,0.816513761,0.818348624,0.820183486,0.822018349,
0.823853211,0.825688073,0.827522936,0.829357798,0.831192661,0.833027523,
0.834862385,0.836697248,0.83853211,0.840366972,0.842201835,0.844036697,
0.84587156,0.847706422,0.849541284,0.851376147,0.853211009,0.855045872,
0.856880734,0.858715596,0.860550459,0.862385321,0.864220183,0.866055046,
0.867889908,0.869724771,0.871559633,0.873394495,0.875229358,0.87706422,
0.878899083,0.880733945,0.882568807,0.88440367,0.886238532,0.888073394,
0.889908257,0.891743119,0.893577982,0.895412844,0.897247706,0.899082569,
0.900917431,0.902752294,0.904587156,0.906422018,0.908256881,0.910091743,
0.911926606,0.913761468,0.91559633,0.917431193,0.919266055,0.921100917,
0.92293578,0.924770642,0.926605505,0.928440367,0.930275229,0.932110092,
0.933944954,0.935779817,0.937614679,0.939449541,0.941284404,0.943119266,
0.944954128,0.946788991,0.948623853,0.950458716,0.952293578,0.95412844,
0.955963303,0.957798165,0.959633028,0.96146789,0.963302752,0.965137615,
0.966972477,0.968807339,0.970642202,0.972477064,0.974311927,0.976146789,
0.977981651,0.979816514,0.981651376,0.983486239,0.985321101,0.987155963,
0.988990826,0.990825688,0.99266055,0.994495413,0.996330275,0.998165138,
1.),(0.,0.36),.UNSPECIFIED.);
#6303=B_SPLINE_SURFACE_WITH_KNOTS('',5,1,((#301296,#301297,#301298),(#301299,
#301300,#301301),(#301302,#301303,#301304),(#301305,#301306,#301307),(#301308,
#301309,#301310),(#301311,#301312,#301313),(#301314,#301315,#301316),(#301317,
#301318,#301319),(#301320,#301321,#301322),(#301323,#301324,#301325),(#301326,
#301327,#301328),(#301329,#301330,#301331),(#301332,#301333,#301334),(#301335,
#301336,#301337),(#301338,#301339,#301340),(#301341,#301342,#301343),(#301344,
#301345,#301346),(#301347,#301348,#301349),(#301350,#301351,#301352),(#301353,
#301354,#301355),(#301356,#301357,#301358),(#301359,#301360,#301361),(#301362,
#301363,#301364),(#301365,#301366,#301367),(#301368,#301369,#301370),(#301371,
#301372,#301373),(#301374,#301375,#301376),(#301377,#301378,#301379),(#301380,
#301381,#301382),(#301383,#301384,#301385),(#301386,#301387,#301388),(#301389,
#301390,#301391),(#301392,#301393,#301394),(#301395,#301396,#301397),(#301398,
#301399,#301400),(#301401,#301402,#301403),(#301404,#301405,#301406),(#301407,
#301408,#301409),(#301410,#301411,#301412),(#301413,#301414,#301415),(#301416,
#301417,#301418),(#301419,#301420,#301421),(#301422,#301423,#301424),(#301425,
#301426,#301427),(#301428,#301429,#301430),(#301431,#301432,#301433),(#301434,
#301435,#301436),(#301437,#301438,#301439),(#301440,#301441,#301442),(#301443,
#301444,#301445),(#301446,#301447,#301448),(#301449,#301450,#301451),(#301452,
#301453,#301454),(#301455,#301456,#301457),(#301458,#301459,#301460),(#301461,
#301462,#301463),(#301464,#301465,#301466),(#301467,#301468,#301469),(#301470,
#301471,#301472),(#301473,#301474,#301475),(#301476,#301477,#301478),(#301479,
#301480,#301481),(#301482,#301483,#301484),(#301485,#301486,#301487),(#301488,
#301489,#301490),(#301491,#301492,#301493),(#301494,#301495,#301496),(#301497,
#301498,#301499),(#301500,#301501,#301502),(#301503,#301504,#301505),(#301506,
#301507,#301508),(#301509,#301510,#301511),(#301512,#301513,#301514),(#301515,
#301516,#301517),(#301518,#301519,#301520),(#301521,#301522,#301523),(#301524,
#301525,#301526),(#301527,#301528,#301529),(#301530,#301531,#301532),(#301533,
#301534,#301535),(#301536,#301537,#301538),(#301539,#301540,#301541),(#301542,
#301543,#301544),(#301545,#301546,#301547),(#301548,#301549,#301550),(#301551,
#301552,#301553),(#301554,#301555,#301556),(#301557,#301558,#301559),(#301560,
#301561,#301562),(#301563,#301564,#301565),(#301566,#301567,#301568),(#301569,
#301570,#301571),(#301572,#301573,#301574),(#301575,#301576,#301577),(#301578,
#301579,#301580),(#301581,#301582,#301583),(#301584,#301585,#301586),(#301587,
#301588,#301589),(#301590,#301591,#301592),(#301593,#301594,#301595),(#301596,
#301597,#301598),(#301599,#301600,#301601),(#301602,#301603,#301604),(#301605,
#301606,#301607),(#301608,#301609,#301610),(#301611,#301612,#301613),(#301614,
#301615,#301616),(#301617,#301618,#301619),(#301620,#301621,#301622),(#301623,
#301624,#301625),(#301626,#301627,#301628),(#301629,#301630,#301631),(#301632,
#301633,#301634),(#301635,#301636,#301637),(#301638,#301639,#301640),(#301641,
#301642,#301643),(#301644,#301645,#301646),(#301647,#301648,#301649),(#301650,
#301651,#301652),(#301653,#301654,#301655),(#301656,#301657,#301658),(#301659,
#301660,#301661),(#301662,#301663,#301664),(#301665,#301666,#301667),(#301668,
#301669,#301670),(#301671,#301672,#301673),(#301674,#301675,#301676),(#301677,
#301678,#301679),(#301680,#301681,#301682),(#301683,#301684,#301685),(#301686,
#301687,#301688),(#301689,#301690,#301691),(#301692,#301693,#301694),(#301695,
#301696,#301697),(#301698,#301699,#301700),(#301701,#301702,#301703),(#301704,
#301705,#301706),(#301707,#301708,#301709),(#301710,#301711,#301712),(#301713,
#301714,#301715),(#301716,#301717,#301718),(#301719,#301720,#301721),(#301722,
#301723,#301724),(#301725,#301726,#301727),(#301728,#301729,#301730),(#301731,
#301732,#301733),(#301734,#301735,#301736),(#301737,#301738,#301739),(#301740,
#301741,#301742),(#301743,#301744,#301745),(#301746,#301747,#301748),(#301749,
#301750,#301751),(#301752,#301753,#301754),(#301755,#301756,#301757),(#301758,
#301759,#301760),(#301761,#301762,#301763),(#301764,#301765,#301766),(#301767,
#301768,#301769),(#301770,#301771,#301772),(#301773,#301774,#301775),(#301776,
#301777,#301778),(#301779,#301780,#301781),(#301782,#301783,#301784),(#301785,
#301786,#301787),(#301788,#301789,#301790),(#301791,#301792,#301793),(#301794,
#301795,#301796),(#301797,#301798,#301799),(#301800,#301801,#301802),(#301803,
#301804,#301805),(#301806,#301807,#301808),(#301809,#301810,#301811),(#301812,
#301813,#301814),(#301815,#301816,#301817),(#301818,#301819,#301820),(#301821,
#301822,#301823),(#301824,#301825,#301826),(#301827,#301828,#301829),(#301830,
#301831,#301832),(#301833,#301834,#301835),(#301836,#301837,#301838),(#301839,
#301840,#301841),(#301842,#301843,#301844),(#301845,#301846,#301847),(#301848,
#301849,#301850),(#301851,#301852,#301853),(#301854,#301855,#301856),(#301857,
#301858,#301859),(#301860,#301861,#301862),(#301863,#301864,#301865),(#301866,
#301867,#301868),(#301869,#301870,#301871),(#301872,#301873,#301874),(#301875,
#301876,#301877),(#301878,#301879,#301880),(#301881,#301882,#301883),(#301884,
#301885,#301886),(#301887,#301888,#301889),(#301890,#301891,#301892),(#301893,
#301894,#301895),(#301896,#301897,#301898),(#301899,#301900,#301901),(#301902,
#301903,#301904),(#301905,#301906,#301907),(#301908,#301909,#301910),(#301911,
#301912,#301913),(#301914,#301915,#301916),(#301917,#301918,#301919),(#301920,
#301921,#301922),(#301923,#301924,#301925),(#301926,#301927,#301928),(#301929,
#301930,#301931),(#301932,#301933,#301934),(#301935,#301936,#301937),(#301938,
#301939,#301940),(#301941,#301942,#301943),(#301944,#301945,#301946),(#301947,
#301948,#301949),(#301950,#301951,#301952),(#301953,#301954,#301955),(#301956,
#301957,#301958),(#301959,#301960,#301961),(#301962,#301963,#301964),(#301965,
#301966,#301967),(#301968,#301969,#301970),(#301971,#301972,#301973),(#301974,
#301975,#301976),(#301977,#301978,#301979),(#301980,#301981,#301982),(#301983,
#301984,#301985),(#301986,#301987,#301988),(#301989,#301990,#301991),(#301992,
#301993,#301994),(#301995,#301996,#301997),(#301998,#301999,#302000),(#302001,
#302002,#302003),(#302004,#302005,#302006),(#302007,#302008,#302009),(#302010,
#302011,#302012),(#302013,#302014,#302015),(#302016,#302017,#302018),(#302019,
#302020,#302021),(#302022,#302023,#302024),(#302025,#302026,#302027),(#302028,
#302029,#302030),(#302031,#302032,#302033),(#302034,#302035,#302036),(#302037,
#302038,#302039),(#302040,#302041,#302042),(#302043,#302044,#302045),(#302046,
#302047,#302048),(#302049,#302050,#302051),(#302052,#302053,#302054),(#302055,
#302056,#302057),(#302058,#302059,#302060),(#302061,#302062,#302063),(#302064,
#302065,#302066),(#302067,#302068,#302069),(#302070,#302071,#302072),(#302073,
#302074,#302075),(#302076,#302077,#302078),(#302079,#302080,#302081),(#302082,
#302083,#302084),(#302085,#302086,#302087),(#302088,#302089,#302090),(#302091,
#302092,#302093),(#302094,#302095,#302096),(#302097,#302098,#302099),(#302100,
#302101,#302102),(#302103,#302104,#302105),(#302106,#302107,#302108),(#302109,
#302110,#302111),(#302112,#302113,#302114),(#302115,#302116,#302117),(#302118,
#302119,#302120),(#302121,#302122,#302123),(#302124,#302125,#302126),(#302127,
#302128,#302129),(#302130,#302131,#302132),(#302133,#302134,#302135),(#302136,
#302137,#302138),(#302139,#302140,#302141),(#302142,#302143,#302144),(#302145,
#302146,#302147),(#302148,#302149,#302150),(#302151,#302152,#302153),(#302154,
#302155,#302156),(#302157,#302158,#302159),(#302160,#302161,#302162),(#302163,
#302164,#302165),(#302166,#302167,#302168),(#302169,#302170,#302171),(#302172,
#302173,#302174),(#302175,#302176,#302177),(#302178,#302179,#302180),(#302181,
#302182,#302183),(#302184,#302185,#302186),(#302187,#302188,#302189),(#302190,
#302191,#302192),(#302193,#302194,#302195),(#302196,#302197,#302198),(#302199,
#302200,#302201),(#302202,#302203,#302204),(#302205,#302206,#302207),(#302208,
#302209,#302210),(#302211,#302212,#302213),(#302214,#302215,#302216),(#302217,
#302218,#302219),(#302220,#302221,#302222),(#302223,#302224,#302225),(#302226,
#302227,#302228),(#302229,#302230,#302231),(#302232,#302233,#302234),(#302235,
#302236,#302237),(#302238,#302239,#302240),(#302241,#302242,#302243),(#302244,
#302245,#302246),(#302247,#302248,#302249),(#302250,#302251,#302252),(#302253,
#302254,#302255),(#302256,#302257,#302258),(#302259,#302260,#302261),(#302262,
#302263,#302264),(#302265,#302266,#302267),(#302268,#302269,#302270),(#302271,
#302272,#302273),(#302274,#302275,#302276),(#302277,#302278,#302279),(#302280,
#302281,#302282),(#302283,#302284,#302285),(#302286,#302287,#302288),(#302289,
#302290,#302291),(#302292,#302293,#302294),(#302295,#302296,#302297),(#302298,
#302299,#302300),(#302301,#302302,#302303),(#302304,#302305,#302306),(#302307,
#302308,#302309),(#302310,#302311,#302312),(#302313,#302314,#302315),(#302316,
#302317,#302318),(#302319,#302320,#302321),(#302322,#302323,#302324),(#302325,
#302326,#302327),(#302328,#302329,#302330),(#302331,#302332,#302333),(#302334,
#302335,#302336),(#302337,#302338,#302339),(#302340,#302341,#302342),(#302343,
#302344,#302345),(#302346,#302347,#302348),(#302349,#302350,#302351),(#302352,
#302353,#302354),(#302355,#302356,#302357),(#302358,#302359,#302360),(#302361,
#302362,#302363),(#302364,#302365,#302366),(#302367,#302368,#302369),(#302370,
#302371,#302372),(#302373,#302374,#302375),(#302376,#302377,#302378),(#302379,
#302380,#302381),(#302382,#302383,#302384),(#302385,#302386,#302387),(#302388,
#302389,#302390),(#302391,#302392,#302393),(#302394,#302395,#302396),(#302397,
#302398,#302399),(#302400,#302401,#302402),(#302403,#302404,#302405),(#302406,
#302407,#302408),(#302409,#302410,#302411),(#302412,#302413,#302414),(#302415,
#302416,#302417),(#302418,#302419,#302420),(#302421,#302422,#302423),(#302424,
#302425,#302426),(#302427,#302428,#302429),(#302430,#302431,#302432),(#302433,
#302434,#302435),(#302436,#302437,#302438),(#302439,#302440,#302441),(#302442,
#302443,#302444),(#302445,#302446,#302447),(#302448,#302449,#302450),(#302451,
#302452,#302453),(#302454,#302455,#302456),(#302457,#302458,#302459),(#302460,
#302461,#302462),(#302463,#302464,#302465),(#302466,#302467,#302468),(#302469,
#302470,#302471),(#302472,#302473,#302474),(#302475,#302476,#302477),(#302478,
#302479,#302480),(#302481,#302482,#302483),(#302484,#302485,#302486),(#302487,
#302488,#302489),(#302490,#302491,#302492),(#302493,#302494,#302495),(#302496,
#302497,#302498),(#302499,#302500,#302501),(#302502,#302503,#302504),(#302505,
#302506,#302507),(#302508,#302509,#302510),(#302511,#302512,#302513),(#302514,
#302515,#302516),(#302517,#302518,#302519),(#302520,#302521,#302522),(#302523,
#302524,#302525),(#302526,#302527,#302528),(#302529,#302530,#302531),(#302532,
#302533,#302534),(#302535,#302536,#302537),(#302538,#302539,#302540),(#302541,
#302542,#302543),(#302544,#302545,#302546),(#302547,#302548,#302549),(#302550,
#302551,#302552),(#302553,#302554,#302555),(#302556,#302557,#302558),(#302559,
#302560,#302561),(#302562,#302563,#302564),(#302565,#302566,#302567),(#302568,
#302569,#302570),(#302571,#302572,#302573),(#302574,#302575,#302576),(#302577,
#302578,#302579),(#302580,#302581,#302582),(#302583,#302584,#302585),(#302586,
#302587,#302588),(#302589,#302590,#302591),(#302592,#302593,#302594),(#302595,
#302596,#302597),(#302598,#302599,#302600),(#302601,#302602,#302603),(#302604,
#302605,#302606),(#302607,#302608,#302609),(#302610,#302611,#302612),(#302613,
#302614,#302615),(#302616,#302617,#302618),(#302619,#302620,#302621),(#302622,
#302623,#302624),(#302625,#302626,#302627),(#302628,#302629,#302630),(#302631,
#302632,#302633),(#302634,#302635,#302636),(#302637,#302638,#302639),(#302640,
#302641,#302642),(#302643,#302644,#302645),(#302646,#302647,#302648),(#302649,
#302650,#302651),(#302652,#302653,#302654),(#302655,#302656,#302657),(#302658,
#302659,#302660),(#302661,#302662,#302663),(#302664,#302665,#302666),(#302667,
#302668,#302669),(#302670,#302671,#302672),(#302673,#302674,#302675),(#302676,
#302677,#302678),(#302679,#302680,#302681),(#302682,#302683,#302684),(#302685,
#302686,#302687),(#302688,#302689,#302690),(#302691,#302692,#302693),(#302694,
#302695,#302696),(#302697,#302698,#302699),(#302700,#302701,#302702),(#302703,
#302704,#302705),(#302706,#302707,#302708),(#302709,#302710,#302711),(#302712,
#302713,#302714),(#302715,#302716,#302717),(#302718,#302719,#302720),(#302721,
#302722,#302723),(#302724,#302725,#302726),(#302727,#302728,#302729),(#302730,
#302731,#302732),(#302733,#302734,#302735),(#302736,#302737,#302738),(#302739,
#302740,#302741),(#302742,#302743,#302744),(#302745,#302746,#302747),(#302748,
#302749,#302750),(#302751,#302752,#302753),(#302754,#302755,#302756),(#302757,
#302758,#302759),(#302760,#302761,#302762),(#302763,#302764,#302765),(#302766,
#302767,#302768),(#302769,#302770,#302771),(#302772,#302773,#302774),(#302775,
#302776,#302777),(#302778,#302779,#302780),(#302781,#302782,#302783),(#302784,
#302785,#302786),(#302787,#302788,#302789),(#302790,#302791,#302792),(#302793,
#302794,#302795),(#302796,#302797,#302798),(#302799,#302800,#302801),(#302802,
#302803,#302804),(#302805,#302806,#302807),(#302808,#302809,#302810),(#302811,
#302812,#302813),(#302814,#302815,#302816),(#302817,#302818,#302819),(#302820,
#302821,#302822),(#302823,#302824,#302825),(#302826,#302827,#302828),(#302829,
#302830,#302831),(#302832,#302833,#302834),(#302835,#302836,#302837),(#302838,
#302839,#302840),(#302841,#302842,#302843),(#302844,#302845,#302846),(#302847,
#302848,#302849),(#302850,#302851,#302852),(#302853,#302854,#302855),(#302856,
#302857,#302858),(#302859,#302860,#302861),(#302862,#302863,#302864),(#302865,
#302866,#302867),(#302868,#302869,#302870),(#302871,#302872,#302873),(#302874,
#302875,#302876),(#302877,#302878,#302879),(#302880,#302881,#302882),(#302883,
#302884,#302885),(#302886,#302887,#302888),(#302889,#302890,#302891),(#302892,
#302893,#302894),(#302895,#302896,#302897),(#302898,#302899,#302900),(#302901,
#302902,#302903),(#302904,#302905,#302906),(#302907,#302908,#302909),(#302910,
#302911,#302912),(#302913,#302914,#302915),(#302916,#302917,#302918),(#302919,
#302920,#302921),(#302922,#302923,#302924),(#302925,#302926,#302927),(#302928,
#302929,#302930),(#302931,#302932,#302933),(#302934,#302935,#302936),(#302937,
#302938,#302939),(#302940,#302941,#302942),(#302943,#302944,#302945)),
 .UNSPECIFIED.,.F.,.F.,.F.,(6,1,1,1,1,1,1,1,1,1,1,1,1,1,1,1,1,1,1,1,1,1,
1,1,1,1,1,1,1,1,1,1,1,1,1,1,1,1,1,1,1,1,1,1,1,1,1,1,1,1,1,1,1,1,1,1,1,1,
1,1,1,1,1,1,1,1,1,1,1,1,1,1,1,1,1,1,1,1,1,1,1,1,1,1,1,1,1,1,1,1,1,1,1,1,
1,1,1,1,1,1,1,1,1,1,1,1,1,1,1,1,1,1,1,1,1,1,1,1,1,1,1,1,1,1,1,1,1,1,1,1,
1,1,1,1,1,1,1,1,1,1,1,1,1,1,1,1,1,1,1,1,1,1,1,1,1,1,1,1,1,1,1,1,1,1,1,1,
1,1,1,1,1,1,1,1,1,1,1,1,1,1,1,1,1,1,1,1,1,1,1,1,1,1,1,1,1,1,1,1,1,1,1,1,
1,1,1,1,1,1,1,1,1,1,1,1,1,1,1,1,1,1,1,1,1,1,1,1,1,1,1,1,1,1,1,1,1,1,1,1,
1,1,1,1,1,1,1,1,1,1,1,1,1,1,1,1,1,1,1,1,1,1,1,1,1,1,1,1,1,1,1,1,1,1,1,1,
1,1,1,1,1,1,1,1,1,1,1,1,1,1,1,1,1,1,1,1,1,1,1,1,1,1,1,1,1,1,1,1,1,1,1,1,
1,1,1,1,1,1,1,1,1,1,1,1,1,1,1,1,1,1,1,1,1,1,1,1,1,1,1,1,1,1,1,1,1,1,1,1,
1,1,1,1,1,1,1,1,1,1,1,1,1,1,1,1,1,1,1,1,1,1,1,1,1,1,1,1,1,1,1,1,1,1,1,1,
1,1,1,1,1,1,1,1,1,1,1,1,1,1,1,1,1,1,1,1,1,1,1,1,1,1,1,1,1,1,1,1,1,1,1,1,
1,1,1,1,1,1,1,1,1,1,1,1,1,1,1,1,1,1,1,1,1,1,1,1,1,1,1,1,1,1,1,1,1,1,1,1,
1,1,1,1,1,1,1,1,1,1,1,1,1,1,1,1,1,1,1,1,1,1,1,1,1,1,1,1,1,1,1,1,1,1,1,1,
1,1,1,1,1,1,1,1,1,1,1,1,1,1,1,1,1,1,1,1,1,1,1,1,1,1,1,1,1,1,1,1,1,1,1,1,
1,1,1,1,1,1,1,1,1,1,1,1,1,1,1,1,1,1,1,6),(2,1,2),(-1.,-0.998165138,-0.996330275,
-0.994495413,-0.99266055,-0.990825688,-0.988990826,-0.987155963,-0.985321101,
-0.983486239,-0.981651376,-0.979816514,-0.977981651,-0.976146789,-0.974311927,
-0.972477064,-0.970642202,-0.968807339,-0.966972477,-0.965137615,-0.963302752,
-0.96146789,-0.959633028,-0.957798165,-0.955963303,-0.95412844,-0.952293578,
-0.950458716,-0.948623853,-0.946788991,-0.944954128,-0.943119266,-0.941284404,
-0.939449541,-0.937614679,-0.935779817,-0.933944954,-0.932110092,-0.930275229,
-0.928440367,-0.926605505,-0.924770642,-0.92293578,-0.921100917,-0.919266055,
-0.917431193,-0.91559633,-0.913761468,-0.911926606,-0.910091743,-0.908256881,
-0.906422018,-0.904587156,-0.902752294,-0.900917431,-0.899082569,-0.897247706,
-0.895412844,-0.893577982,-0.891743119,-0.889908257,-0.888073394,-0.886238532,
-0.88440367,-0.882568807,-0.880733945,-0.878899083,-0.87706422,-0.875229358,
-0.873394495,-0.871559633,-0.869724771,-0.867889908,-0.866055046,-0.864220183,
-0.862385321,-0.860550459,-0.858715596,-0.856880734,-0.855045872,-0.853211009,
-0.851376147,-0.849541284,-0.847706422,-0.84587156,-0.844036697,-0.842201835,
-0.840366972,-0.83853211,-0.836697248,-0.834862385,-0.833027523,-0.831192661,
-0.829357798,-0.827522936,-0.825688073,-0.823853211,-0.822018349,-0.820183486,
-0.818348624,-0.816513761,-0.814678899,-0.812844037,-0.811009174,-0.809174312,
-0.80733945,-0.805504587,-0.803669725,-0.801834862,-0.8,-0.798165138,-0.796330275,
-0.794495413,-0.79266055,-0.790825688,-0.788990826,-0.787155963,-0.785321101,
-0.783486239,-0.781651376,-0.779816514,-0.777981651,-0.776146789,-0.774311927,
-0.772477064,-0.770642202,-0.768807339,-0.766972477,-0.765137615,-0.763302752,
-0.76146789,-0.759633028,-0.757798165,-0.755963303,-0.75412844,-0.752293578,
-0.750458716,-0.748623853,-0.746788991,-0.744954128,-0.743119266,-0.741284404,
-0.739449541,-0.737614679,-0.735779817,-0.733944954,-0.732110092,-0.730275229,
-0.728440367,-0.726605505,-0.724770642,-0.72293578,-0.721100917,-0.719266055,
-0.717431193,-0.71559633,-0.713761468,-0.711926606,-0.710091743,-0.708256881,
-0.706422018,-0.704587156,-0.702752294,-0.700917431,-0.699082569,-0.697247706,
-0.695412844,-0.693577982,-0.691743119,-0.689908257,-0.688073394,-0.686238532,
-0.68440367,-0.682568807,-0.680733945,-0.678899083,-0.67706422,-0.675229358,
-0.673394495,-0.671559633,-0.669724771,-0.667889908,-0.666055046,-0.664220183,
-0.662385321,-0.660550459,-0.658715596,-0.656880734,-0.655045872,-0.653211009,
-0.651376147,-0.649541284,-0.647706422,-0.64587156,-0.644036697,-0.642201835,
-0.640366972,-0.63853211,-0.636697248,-0.634862385,-0.633027523,-0.631192661,
-0.629357798,-0.627522936,-0.625688073,-0.623853211,-0.622018349,-0.620183486,
-0.618348624,-0.616513761,-0.614678899,-0.612844037,-0.611009174,-0.609174312,
-0.60733945,-0.605504587,-0.603669725,-0.601834862,-0.6,-0.598165138,-0.596330275,
-0.594495413,-0.59266055,-0.590825688,-0.588990826,-0.587155963,-0.585321101,
-0.583486239,-0.581651376,-0.579816514,-0.577981651,-0.576146789,-0.574311927,
-0.572477064,-0.570642202,-0.568807339,-0.566972477,-0.565137615,-0.563302752,
-0.56146789,-0.559633028,-0.557798165,-0.555963303,-0.55412844,-0.552293578,
-0.550458716,-0.548623853,-0.546788991,-0.544954128,-0.543119266,-0.541284404,
-0.539449541,-0.537614679,-0.535779817,-0.533944954,-0.532110092,-0.530275229,
-0.528440367,-0.526605505,-0.524770642,-0.52293578,-0.521100917,-0.519266055,
-0.517431193,-0.51559633,-0.513761468,-0.511926606,-0.510091743,-0.508256881,
-0.506422018,-0.504587156,-0.502752294,-0.500917431,-0.499082569,-0.497247706,
-0.495412844,-0.493577982,-0.491743119,-0.489908257,-0.488073394,-0.486238532,
-0.48440367,-0.482568807,-0.480733945,-0.478899083,-0.47706422,-0.475229358,
-0.473394495,-0.471559633,-0.469724771,-0.467889908,-0.466055046,-0.464220183,
-0.462385321,-0.460550459,-0.458715596,-0.456880734,-0.455045872,-0.453211009,
-0.451376147,-0.449541284,-0.447706422,-0.44587156,-0.444036697,-0.442201835,
-0.440366972,-0.43853211,-0.436697248,-0.434862385,-0.433027523,-0.431192661,
-0.429357798,-0.427522936,-0.425688073,-0.423853211,-0.422018349,-0.420183486,
-0.418348624,-0.416513761,-0.414678899,-0.412844037,-0.411009174,-0.409174312,
-0.40733945,-0.405504587,-0.403669725,-0.401834862,-0.4,-0.398165138,-0.396330275,
-0.394495413,-0.39266055,-0.390825688,-0.388990826,-0.387155963,-0.385321101,
-0.383486239,-0.381651376,-0.379816514,-0.377981651,-0.376146789,-0.374311927,
-0.372477064,-0.370642202,-0.368807339,-0.366972477,-0.365137615,-0.363302752,
-0.36146789,-0.359633028,-0.357798165,-0.355963303,-0.35412844,-0.352293578,
-0.350458716,-0.348623853,-0.346788991,-0.344954128,-0.343119266,-0.341284404,
-0.339449541,-0.337614679,-0.335779817,-0.333944954,-0.332110092,-0.330275229,
-0.328440367,-0.326605505,-0.324770642,-0.32293578,-0.321100917,-0.319266055,
-0.317431193,-0.31559633,-0.313761468,-0.311926606,-0.310091743,-0.308256881,
-0.306422018,-0.304587156,-0.302752294,-0.300917431,-0.299082569,-0.297247706,
-0.295412844,-0.293577982,-0.291743119,-0.289908257,-0.288073394,-0.286238532,
-0.28440367,-0.282568807,-0.280733945,-0.278899083,-0.27706422,-0.275229358,
-0.273394495,-0.271559633,-0.269724771,-0.267889908,-0.266055046,-0.264220183,
-0.262385321,-0.260550459,-0.258715596,-0.256880734,-0.255045872,-0.253211009,
-0.251376147,-0.249541284,-0.247706422,-0.24587156,-0.244036697,-0.242201835,
-0.240366972,-0.23853211,-0.236697248,-0.234862385,-0.233027523,-0.231192661,
-0.229357798,-0.227522936,-0.225688073,-0.223853211,-0.222018349,-0.220183486,
-0.218348624,-0.216513761,-0.214678899,-0.212844037,-0.211009174,-0.209174312,
-0.20733945,-0.205504587,-0.203669725,-0.201834862,-0.2,-0.198165138,-0.196330275,
-0.194495413,-0.19266055,-0.190825688,-0.188990826,-0.187155963,-0.185321101,
-0.183486239,-0.181651376,-0.179816514,-0.177981651,-0.176146789,-0.174311927,
-0.172477064,-0.170642202,-0.168807339,-0.166972477,-0.165137615,-0.163302752,
-0.16146789,-0.159633028,-0.157798165,-0.155963303,-0.15412844,-0.152293578,
-0.150458716,-0.148623853,-0.146788991,-0.144954128,-0.143119266,-0.141284404,
-0.139449541,-0.137614679,-0.135779817,-0.133944954,-0.132110092,-0.130275229,
-0.128440367,-0.126605505,-0.124770642,-0.12293578,-0.121100917,-0.119266055,
-0.117431193,-0.11559633,-0.113761468,-0.111926606,-0.110091743,-0.108256881,
-0.106422018,-0.104587156,-0.102752294,-0.100917431,-0.099082569,-0.097247706,
-0.095412844,-0.093577982,-0.091743119,-0.089908257,-0.088073394,-0.086238532,
-0.08440367,-0.082568807,-0.080733945,-0.078899083,-0.07706422,-0.075229358,
-0.073394495,-0.071559633,-0.069724771,-0.067889908,-0.066055046,-0.064220183,
-0.062385321,-0.060550459,-0.058715596,-0.056880734,-0.055045872,-0.053211009,
-0.051376147,-0.049541284,-0.047706422,-0.04587156,-0.044036697,-0.042201835,
-0.040366972,-0.03853211,-0.036697248,-0.034862385,-0.033027523,-0.031192661,
-0.029357798,-0.027522936,-0.025688073,-0.023853211,-0.022018349,-0.020183486,
-0.018348624,-0.016513761,-0.014678899,-0.012844037,-0.011009174,-0.009174312,
-0.00733945,-0.005504587,-0.003669725,-0.001834862,0.000982105),(0.3,1.,
1.3),.UNSPECIFIED.);
#6304=B_SPLINE_SURFACE_WITH_KNOTS('',5,1,((#302968,#302969,#302970),(#302971,
#302972,#302973),(#302974,#302975,#302976),(#302977,#302978,#302979),(#302980,
#302981,#302982),(#302983,#302984,#302985),(#302986,#302987,#302988),(#302989,
#302990,#302991),(#302992,#302993,#302994),(#302995,#302996,#302997),(#302998,
#302999,#303000),(#303001,#303002,#303003),(#303004,#303005,#303006),(#303007,
#303008,#303009),(#303010,#303011,#303012),(#303013,#303014,#303015),(#303016,
#303017,#303018),(#303019,#303020,#303021),(#303022,#303023,#303024),(#303025,
#303026,#303027),(#303028,#303029,#303030),(#303031,#303032,#303033),(#303034,
#303035,#303036),(#303037,#303038,#303039),(#303040,#303041,#303042),(#303043,
#303044,#303045),(#303046,#303047,#303048),(#303049,#303050,#303051),(#303052,
#303053,#303054),(#303055,#303056,#303057),(#303058,#303059,#303060),(#303061,
#303062,#303063),(#303064,#303065,#303066),(#303067,#303068,#303069),(#303070,
#303071,#303072),(#303073,#303074,#303075),(#303076,#303077,#303078),(#303079,
#303080,#303081),(#303082,#303083,#303084),(#303085,#303086,#303087),(#303088,
#303089,#303090),(#303091,#303092,#303093),(#303094,#303095,#303096),(#303097,
#303098,#303099),(#303100,#303101,#303102),(#303103,#303104,#303105),(#303106,
#303107,#303108),(#303109,#303110,#303111),(#303112,#303113,#303114),(#303115,
#303116,#303117),(#303118,#303119,#303120),(#303121,#303122,#303123),(#303124,
#303125,#303126),(#303127,#303128,#303129),(#303130,#303131,#303132),(#303133,
#303134,#303135),(#303136,#303137,#303138),(#303139,#303140,#303141),(#303142,
#303143,#303144),(#303145,#303146,#303147),(#303148,#303149,#303150),(#303151,
#303152,#303153),(#303154,#303155,#303156),(#303157,#303158,#303159),(#303160,
#303161,#303162),(#303163,#303164,#303165),(#303166,#303167,#303168),(#303169,
#303170,#303171),(#303172,#303173,#303174),(#303175,#303176,#303177),(#303178,
#303179,#303180),(#303181,#303182,#303183),(#303184,#303185,#303186),(#303187,
#303188,#303189),(#303190,#303191,#303192),(#303193,#303194,#303195),(#303196,
#303197,#303198),(#303199,#303200,#303201),(#303202,#303203,#303204),(#303205,
#303206,#303207),(#303208,#303209,#303210),(#303211,#303212,#303213),(#303214,
#303215,#303216),(#303217,#303218,#303219),(#303220,#303221,#303222),(#303223,
#303224,#303225),(#303226,#303227,#303228),(#303229,#303230,#303231),(#303232,
#303233,#303234),(#303235,#303236,#303237),(#303238,#303239,#303240),(#303241,
#303242,#303243),(#303244,#303245,#303246),(#303247,#303248,#303249),(#303250,
#303251,#303252),(#303253,#303254,#303255),(#303256,#303257,#303258),(#303259,
#303260,#303261),(#303262,#303263,#303264),(#303265,#303266,#303267),(#303268,
#303269,#303270),(#303271,#303272,#303273),(#303274,#303275,#303276),(#303277,
#303278,#303279),(#303280,#303281,#303282),(#303283,#303284,#303285),(#303286,
#303287,#303288),(#303289,#303290,#303291),(#303292,#303293,#303294),(#303295,
#303296,#303297),(#303298,#303299,#303300),(#303301,#303302,#303303),(#303304,
#303305,#303306),(#303307,#303308,#303309),(#303310,#303311,#303312),(#303313,
#303314,#303315),(#303316,#303317,#303318),(#303319,#303320,#303321),(#303322,
#303323,#303324),(#303325,#303326,#303327),(#303328,#303329,#303330),(#303331,
#303332,#303333),(#303334,#303335,#303336),(#303337,#303338,#303339),(#303340,
#303341,#303342),(#303343,#303344,#303345),(#303346,#303347,#303348),(#303349,
#303350,#303351),(#303352,#303353,#303354),(#303355,#303356,#303357),(#303358,
#303359,#303360),(#303361,#303362,#303363),(#303364,#303365,#303366),(#303367,
#303368,#303369),(#303370,#303371,#303372),(#303373,#303374,#303375),(#303376,
#303377,#303378),(#303379,#303380,#303381),(#303382,#303383,#303384),(#303385,
#303386,#303387),(#303388,#303389,#303390),(#303391,#303392,#303393),(#303394,
#303395,#303396),(#303397,#303398,#303399),(#303400,#303401,#303402),(#303403,
#303404,#303405),(#303406,#303407,#303408),(#303409,#303410,#303411),(#303412,
#303413,#303414),(#303415,#303416,#303417),(#303418,#303419,#303420),(#303421,
#303422,#303423),(#303424,#303425,#303426),(#303427,#303428,#303429),(#303430,
#303431,#303432),(#303433,#303434,#303435),(#303436,#303437,#303438),(#303439,
#303440,#303441),(#303442,#303443,#303444),(#303445,#303446,#303447),(#303448,
#303449,#303450),(#303451,#303452,#303453),(#303454,#303455,#303456),(#303457,
#303458,#303459),(#303460,#303461,#303462),(#303463,#303464,#303465),(#303466,
#303467,#303468),(#303469,#303470,#303471),(#303472,#303473,#303474),(#303475,
#303476,#303477),(#303478,#303479,#303480),(#303481,#303482,#303483),(#303484,
#303485,#303486),(#303487,#303488,#303489),(#303490,#303491,#303492),(#303493,
#303494,#303495),(#303496,#303497,#303498),(#303499,#303500,#303501),(#303502,
#303503,#303504),(#303505,#303506,#303507),(#303508,#303509,#303510),(#303511,
#303512,#303513),(#303514,#303515,#303516),(#303517,#303518,#303519),(#303520,
#303521,#303522),(#303523,#303524,#303525),(#303526,#303527,#303528),(#303529,
#303530,#303531),(#303532,#303533,#303534),(#303535,#303536,#303537),(#303538,
#303539,#303540),(#303541,#303542,#303543),(#303544,#303545,#303546),(#303547,
#303548,#303549),(#303550,#303551,#303552),(#303553,#303554,#303555),(#303556,
#303557,#303558),(#303559,#303560,#303561),(#303562,#303563,#303564),(#303565,
#303566,#303567),(#303568,#303569,#303570),(#303571,#303572,#303573),(#303574,
#303575,#303576),(#303577,#303578,#303579),(#303580,#303581,#303582),(#303583,
#303584,#303585),(#303586,#303587,#303588),(#303589,#303590,#303591),(#303592,
#303593,#303594),(#303595,#303596,#303597),(#303598,#303599,#303600),(#303601,
#303602,#303603),(#303604,#303605,#303606),(#303607,#303608,#303609),(#303610,
#303611,#303612),(#303613,#303614,#303615),(#303616,#303617,#303618),(#303619,
#303620,#303621),(#303622,#303623,#303624),(#303625,#303626,#303627),(#303628,
#303629,#303630),(#303631,#303632,#303633),(#303634,#303635,#303636),(#303637,
#303638,#303639),(#303640,#303641,#303642),(#303643,#303644,#303645),(#303646,
#303647,#303648),(#303649,#303650,#303651),(#303652,#303653,#303654),(#303655,
#303656,#303657),(#303658,#303659,#303660),(#303661,#303662,#303663),(#303664,
#303665,#303666),(#303667,#303668,#303669),(#303670,#303671,#303672),(#303673,
#303674,#303675),(#303676,#303677,#303678),(#303679,#303680,#303681),(#303682,
#303683,#303684),(#303685,#303686,#303687),(#303688,#303689,#303690),(#303691,
#303692,#303693),(#303694,#303695,#303696),(#303697,#303698,#303699),(#303700,
#303701,#303702),(#303703,#303704,#303705),(#303706,#303707,#303708),(#303709,
#303710,#303711),(#303712,#303713,#303714),(#303715,#303716,#303717),(#303718,
#303719,#303720),(#303721,#303722,#303723),(#303724,#303725,#303726),(#303727,
#303728,#303729),(#303730,#303731,#303732),(#303733,#303734,#303735),(#303736,
#303737,#303738),(#303739,#303740,#303741),(#303742,#303743,#303744),(#303745,
#303746,#303747),(#303748,#303749,#303750),(#303751,#303752,#303753),(#303754,
#303755,#303756),(#303757,#303758,#303759),(#303760,#303761,#303762),(#303763,
#303764,#303765),(#303766,#303767,#303768),(#303769,#303770,#303771),(#303772,
#303773,#303774),(#303775,#303776,#303777),(#303778,#303779,#303780),(#303781,
#303782,#303783),(#303784,#303785,#303786),(#303787,#303788,#303789),(#303790,
#303791,#303792),(#303793,#303794,#303795),(#303796,#303797,#303798),(#303799,
#303800,#303801),(#303802,#303803,#303804),(#303805,#303806,#303807),(#303808,
#303809,#303810),(#303811,#303812,#303813),(#303814,#303815,#303816),(#303817,
#303818,#303819),(#303820,#303821,#303822),(#303823,#303824,#303825),(#303826,
#303827,#303828),(#303829,#303830,#303831),(#303832,#303833,#303834),(#303835,
#303836,#303837),(#303838,#303839,#303840),(#303841,#303842,#303843),(#303844,
#303845,#303846),(#303847,#303848,#303849),(#303850,#303851,#303852),(#303853,
#303854,#303855),(#303856,#303857,#303858),(#303859,#303860,#303861),(#303862,
#303863,#303864),(#303865,#303866,#303867),(#303868,#303869,#303870),(#303871,
#303872,#303873),(#303874,#303875,#303876),(#303877,#303878,#303879),(#303880,
#303881,#303882),(#303883,#303884,#303885),(#303886,#303887,#303888),(#303889,
#303890,#303891),(#303892,#303893,#303894),(#303895,#303896,#303897),(#303898,
#303899,#303900),(#303901,#303902,#303903),(#303904,#303905,#303906),(#303907,
#303908,#303909),(#303910,#303911,#303912),(#303913,#303914,#303915),(#303916,
#303917,#303918),(#303919,#303920,#303921),(#303922,#303923,#303924),(#303925,
#303926,#303927),(#303928,#303929,#303930),(#303931,#303932,#303933),(#303934,
#303935,#303936),(#303937,#303938,#303939),(#303940,#303941,#303942),(#303943,
#303944,#303945),(#303946,#303947,#303948),(#303949,#303950,#303951),(#303952,
#303953,#303954),(#303955,#303956,#303957),(#303958,#303959,#303960),(#303961,
#303962,#303963),(#303964,#303965,#303966),(#303967,#303968,#303969),(#303970,
#303971,#303972),(#303973,#303974,#303975),(#303976,#303977,#303978),(#303979,
#303980,#303981),(#303982,#303983,#303984),(#303985,#303986,#303987),(#303988,
#303989,#303990),(#303991,#303992,#303993),(#303994,#303995,#303996),(#303997,
#303998,#303999),(#304000,#304001,#304002),(#304003,#304004,#304005),(#304006,
#304007,#304008),(#304009,#304010,#304011),(#304012,#304013,#304014),(#304015,
#304016,#304017),(#304018,#304019,#304020),(#304021,#304022,#304023),(#304024,
#304025,#304026),(#304027,#304028,#304029),(#304030,#304031,#304032),(#304033,
#304034,#304035),(#304036,#304037,#304038),(#304039,#304040,#304041),(#304042,
#304043,#304044),(#304045,#304046,#304047),(#304048,#304049,#304050),(#304051,
#304052,#304053),(#304054,#304055,#304056),(#304057,#304058,#304059),(#304060,
#304061,#304062),(#304063,#304064,#304065),(#304066,#304067,#304068),(#304069,
#304070,#304071),(#304072,#304073,#304074),(#304075,#304076,#304077),(#304078,
#304079,#304080),(#304081,#304082,#304083),(#304084,#304085,#304086),(#304087,
#304088,#304089),(#304090,#304091,#304092),(#304093,#304094,#304095),(#304096,
#304097,#304098),(#304099,#304100,#304101),(#304102,#304103,#304104),(#304105,
#304106,#304107),(#304108,#304109,#304110),(#304111,#304112,#304113),(#304114,
#304115,#304116),(#304117,#304118,#304119),(#304120,#304121,#304122),(#304123,
#304124,#304125),(#304126,#304127,#304128),(#304129,#304130,#304131),(#304132,
#304133,#304134),(#304135,#304136,#304137),(#304138,#304139,#304140),(#304141,
#304142,#304143),(#304144,#304145,#304146),(#304147,#304148,#304149),(#304150,
#304151,#304152),(#304153,#304154,#304155),(#304156,#304157,#304158),(#304159,
#304160,#304161),(#304162,#304163,#304164),(#304165,#304166,#304167),(#304168,
#304169,#304170),(#304171,#304172,#304173),(#304174,#304175,#304176),(#304177,
#304178,#304179),(#304180,#304181,#304182),(#304183,#304184,#304185),(#304186,
#304187,#304188),(#304189,#304190,#304191),(#304192,#304193,#304194),(#304195,
#304196,#304197),(#304198,#304199,#304200),(#304201,#304202,#304203),(#304204,
#304205,#304206),(#304207,#304208,#304209),(#304210,#304211,#304212),(#304213,
#304214,#304215),(#304216,#304217,#304218),(#304219,#304220,#304221),(#304222,
#304223,#304224),(#304225,#304226,#304227),(#304228,#304229,#304230),(#304231,
#304232,#304233),(#304234,#304235,#304236),(#304237,#304238,#304239),(#304240,
#304241,#304242),(#304243,#304244,#304245),(#304246,#304247,#304248),(#304249,
#304250,#304251),(#304252,#304253,#304254),(#304255,#304256,#304257),(#304258,
#304259,#304260),(#304261,#304262,#304263),(#304264,#304265,#304266),(#304267,
#304268,#304269),(#304270,#304271,#304272),(#304273,#304274,#304275),(#304276,
#304277,#304278),(#304279,#304280,#304281),(#304282,#304283,#304284),(#304285,
#304286,#304287),(#304288,#304289,#304290),(#304291,#304292,#304293),(#304294,
#304295,#304296),(#304297,#304298,#304299),(#304300,#304301,#304302),(#304303,
#304304,#304305),(#304306,#304307,#304308),(#304309,#304310,#304311),(#304312,
#304313,#304314),(#304315,#304316,#304317),(#304318,#304319,#304320),(#304321,
#304322,#304323),(#304324,#304325,#304326),(#304327,#304328,#304329),(#304330,
#304331,#304332),(#304333,#304334,#304335),(#304336,#304337,#304338),(#304339,
#304340,#304341),(#304342,#304343,#304344),(#304345,#304346,#304347),(#304348,
#304349,#304350),(#304351,#304352,#304353),(#304354,#304355,#304356),(#304357,
#304358,#304359),(#304360,#304361,#304362),(#304363,#304364,#304365),(#304366,
#304367,#304368),(#304369,#304370,#304371),(#304372,#304373,#304374),(#304375,
#304376,#304377),(#304378,#304379,#304380),(#304381,#304382,#304383),(#304384,
#304385,#304386),(#304387,#304388,#304389),(#304390,#304391,#304392),(#304393,
#304394,#304395),(#304396,#304397,#304398),(#304399,#304400,#304401),(#304402,
#304403,#304404),(#304405,#304406,#304407),(#304408,#304409,#304410),(#304411,
#304412,#304413),(#304414,#304415,#304416),(#304417,#304418,#304419),(#304420,
#304421,#304422),(#304423,#304424,#304425),(#304426,#304427,#304428),(#304429,
#304430,#304431),(#304432,#304433,#304434),(#304435,#304436,#304437),(#304438,
#304439,#304440),(#304441,#304442,#304443),(#304444,#304445,#304446),(#304447,
#304448,#304449),(#304450,#304451,#304452),(#304453,#304454,#304455),(#304456,
#304457,#304458),(#304459,#304460,#304461),(#304462,#304463,#304464),(#304465,
#304466,#304467),(#304468,#304469,#304470),(#304471,#304472,#304473),(#304474,
#304475,#304476),(#304477,#304478,#304479),(#304480,#304481,#304482),(#304483,
#304484,#304485),(#304486,#304487,#304488),(#304489,#304490,#304491),(#304492,
#304493,#304494),(#304495,#304496,#304497),(#304498,#304499,#304500),(#304501,
#304502,#304503),(#304504,#304505,#304506),(#304507,#304508,#304509),(#304510,
#304511,#304512),(#304513,#304514,#304515),(#304516,#304517,#304518),(#304519,
#304520,#304521),(#304522,#304523,#304524),(#304525,#304526,#304527),(#304528,
#304529,#304530),(#304531,#304532,#304533),(#304534,#304535,#304536),(#304537,
#304538,#304539),(#304540,#304541,#304542),(#304543,#304544,#304545),(#304546,
#304547,#304548),(#304549,#304550,#304551),(#304552,#304553,#304554),(#304555,
#304556,#304557),(#304558,#304559,#304560),(#304561,#304562,#304563),(#304564,
#304565,#304566),(#304567,#304568,#304569),(#304570,#304571,#304572),(#304573,
#304574,#304575),(#304576,#304577,#304578),(#304579,#304580,#304581),(#304582,
#304583,#304584),(#304585,#304586,#304587),(#304588,#304589,#304590),(#304591,
#304592,#304593),(#304594,#304595,#304596),(#304597,#304598,#304599),(#304600,
#304601,#304602),(#304603,#304604,#304605),(#304606,#304607,#304608),(#304609,
#304610,#304611),(#304612,#304613,#304614),(#304615,#304616,#304617),(#304618,
#304619,#304620)),.UNSPECIFIED.,.F.,.F.,.F.,(6,1,1,1,1,1,1,1,1,1,1,1,1,
1,1,1,1,1,1,1,1,1,1,1,1,1,1,1,1,1,1,1,1,1,1,1,1,1,1,1,1,1,1,1,1,1,1,1,1,
1,1,1,1,1,1,1,1,1,1,1,1,1,1,1,1,1,1,1,1,1,1,1,1,1,1,1,1,1,1,1,1,1,1,1,1,
1,1,1,1,1,1,1,1,1,1,1,1,1,1,1,1,1,1,1,1,1,1,1,1,1,1,1,1,1,1,1,1,1,1,1,1,
1,1,1,1,1,1,1,1,1,1,1,1,1,1,1,1,1,1,1,1,1,1,1,1,1,1,1,1,1,1,1,1,1,1,1,1,
1,1,1,1,1,1,1,1,1,1,1,1,1,1,1,1,1,1,1,1,1,1,1,1,1,1,1,1,1,1,1,1,1,1,1,1,
1,1,1,1,1,1,1,1,1,1,1,1,1,1,1,1,1,1,1,1,1,1,1,1,1,1,1,1,1,1,1,1,1,1,1,1,
1,1,1,1,1,1,1,1,1,1,1,1,1,1,1,1,1,1,1,1,1,1,1,1,1,1,1,1,1,1,1,1,1,1,1,1,
1,1,1,1,1,1,1,1,1,1,1,1,1,1,1,1,1,1,1,1,1,1,1,1,1,1,1,1,1,1,1,1,1,1,1,1,
1,1,1,1,1,1,1,1,1,1,1,1,1,1,1,1,1,1,1,1,1,1,1,1,1,1,1,1,1,1,1,1,1,1,1,1,
1,1,1,1,1,1,1,1,1,1,1,1,1,1,1,1,1,1,1,1,1,1,1,1,1,1,1,1,1,1,1,1,1,1,1,1,
1,1,1,1,1,1,1,1,1,1,1,1,1,1,1,1,1,1,1,1,1,1,1,1,1,1,1,1,1,1,1,1,1,1,1,1,
1,1,1,1,1,1,1,1,1,1,1,1,1,1,1,1,1,1,1,1,1,1,1,1,1,1,1,1,1,1,1,1,1,1,1,1,
1,1,1,1,1,1,1,1,1,1,1,1,1,1,1,1,1,1,1,1,1,1,1,1,1,1,1,1,1,1,1,1,1,1,1,1,
1,1,1,1,1,1,1,1,1,1,1,1,1,1,1,1,1,1,1,1,1,1,1,1,1,1,1,1,1,1,1,1,1,1,1,1,
1,1,1,1,1,1,1,1,1,1,1,1,1,1,1,1,1,1,1,1,1,1,1,1,1,1,1,1,1,6),(2,1,2),(-0.001964151,
0.,0.001834862,0.003669725,0.005504587,0.00733945,0.009174312,0.011009174,
0.012844037,0.014678899,0.016513761,0.018348624,0.020183486,0.022018349,
0.023853211,0.025688073,0.027522936,0.029357798,0.031192661,0.033027523,
0.034862385,0.036697248,0.03853211,0.040366972,0.042201835,0.044036697,
0.04587156,0.047706422,0.049541284,0.051376147,0.053211009,0.055045872,
0.056880734,0.058715596,0.060550459,0.062385321,0.064220183,0.066055046,
0.067889908,0.069724771,0.071559633,0.073394495,0.075229358,0.07706422,
0.078899083,0.080733945,0.082568807,0.08440367,0.086238532,0.088073394,
0.089908257,0.091743119,0.093577982,0.095412844,0.097247706,0.099082569,
0.100917431,0.102752294,0.104587156,0.106422018,0.108256881,0.110091743,
0.111926606,0.113761468,0.11559633,0.117431193,0.119266055,0.121100917,
0.12293578,0.124770642,0.126605505,0.128440367,0.130275229,0.132110092,
0.133944954,0.135779817,0.137614679,0.139449541,0.141284404,0.143119266,
0.144954128,0.146788991,0.148623853,0.150458716,0.152293578,0.15412844,
0.155963303,0.157798165,0.159633028,0.16146789,0.163302752,0.165137615,
0.166972477,0.168807339,0.170642202,0.172477064,0.174311927,0.176146789,
0.177981651,0.179816514,0.181651376,0.183486239,0.185321101,0.187155963,
0.188990826,0.190825688,0.19266055,0.194495413,0.196330275,0.198165138,
0.2,0.201834862,0.203669725,0.205504587,0.20733945,0.209174312,0.211009174,
0.212844037,0.214678899,0.216513761,0.218348624,0.220183486,0.222018349,
0.223853211,0.225688073,0.227522936,0.229357798,0.231192661,0.233027523,
0.234862385,0.236697248,0.23853211,0.240366972,0.242201835,0.244036697,
0.24587156,0.247706422,0.249541284,0.251376147,0.253211009,0.255045872,
0.256880734,0.258715596,0.260550459,0.262385321,0.264220183,0.266055046,
0.267889908,0.269724771,0.271559633,0.273394495,0.275229358,0.27706422,
0.278899083,0.280733945,0.282568807,0.28440367,0.286238532,0.288073394,
0.289908257,0.291743119,0.293577982,0.295412844,0.297247706,0.299082569,
0.300917431,0.302752294,0.304587156,0.306422018,0.308256881,0.310091743,
0.311926606,0.313761468,0.31559633,0.317431193,0.319266055,0.321100917,
0.32293578,0.324770642,0.326605505,0.328440367,0.330275229,0.332110092,
0.333944954,0.335779817,0.337614679,0.339449541,0.341284404,0.343119266,
0.344954128,0.346788991,0.348623853,0.350458716,0.352293578,0.35412844,
0.355963303,0.357798165,0.359633028,0.36146789,0.363302752,0.365137615,
0.366972477,0.368807339,0.370642202,0.372477064,0.374311927,0.376146789,
0.377981651,0.379816514,0.381651376,0.383486239,0.385321101,0.387155963,
0.388990826,0.390825688,0.39266055,0.394495413,0.396330275,0.398165138,
0.4,0.401834862,0.403669725,0.405504587,0.40733945,0.409174312,0.411009174,
0.412844037,0.414678899,0.416513761,0.418348624,0.420183486,0.422018349,
0.423853211,0.425688073,0.427522936,0.429357798,0.431192661,0.433027523,
0.434862385,0.436697248,0.43853211,0.440366972,0.442201835,0.444036697,
0.44587156,0.447706422,0.449541284,0.451376147,0.453211009,0.455045872,
0.456880734,0.458715596,0.460550459,0.462385321,0.464220183,0.466055046,
0.467889908,0.469724771,0.471559633,0.473394495,0.475229358,0.47706422,
0.478899083,0.480733945,0.482568807,0.48440367,0.486238532,0.488073394,
0.489908257,0.491743119,0.493577982,0.495412844,0.497247706,0.499082569,
0.500917431,0.502752294,0.504587156,0.506422018,0.508256881,0.510091743,
0.511926606,0.513761468,0.51559633,0.517431193,0.519266055,0.521100917,
0.52293578,0.524770642,0.526605505,0.528440367,0.530275229,0.532110092,
0.533944954,0.535779817,0.537614679,0.539449541,0.541284404,0.543119266,
0.544954128,0.546788991,0.548623853,0.550458716,0.552293578,0.55412844,
0.555963303,0.557798165,0.559633028,0.56146789,0.563302752,0.565137615,
0.566972477,0.568807339,0.570642202,0.572477064,0.574311927,0.576146789,
0.577981651,0.579816514,0.581651376,0.583486239,0.585321101,0.587155963,
0.588990826,0.590825688,0.59266055,0.594495413,0.596330275,0.598165138,
0.6,0.601834862,0.603669725,0.605504587,0.60733945,0.609174312,0.611009174,
0.612844037,0.614678899,0.616513761,0.618348624,0.620183486,0.622018349,
0.623853211,0.625688073,0.627522936,0.629357798,0.631192661,0.633027523,
0.634862385,0.636697248,0.63853211,0.640366972,0.642201835,0.644036697,
0.64587156,0.647706422,0.649541284,0.651376147,0.653211009,0.655045872,
0.656880734,0.658715596,0.660550459,0.662385321,0.664220183,0.666055046,
0.667889908,0.669724771,0.671559633,0.673394495,0.675229358,0.67706422,
0.678899083,0.680733945,0.682568807,0.68440367,0.686238532,0.688073394,
0.689908257,0.691743119,0.693577982,0.695412844,0.697247706,0.699082569,
0.700917431,0.702752294,0.704587156,0.706422018,0.708256881,0.710091743,
0.711926606,0.713761468,0.71559633,0.717431193,0.719266055,0.721100917,
0.72293578,0.724770642,0.726605505,0.728440367,0.730275229,0.732110092,
0.733944954,0.735779817,0.737614679,0.739449541,0.741284404,0.743119266,
0.744954128,0.746788991,0.748623853,0.750458716,0.752293578,0.75412844,
0.755963303,0.757798165,0.759633028,0.76146789,0.763302752,0.765137615,
0.766972477,0.768807339,0.770642202,0.772477064,0.774311927,0.776146789,
0.777981651,0.779816514,0.781651376,0.783486239,0.785321101,0.787155963,
0.788990826,0.790825688,0.79266055,0.794495413,0.796330275,0.798165138,
0.8,0.801834862,0.803669725,0.805504587,0.80733945,0.809174312,0.811009174,
0.812844037,0.814678899,0.816513761,0.818348624,0.820183486,0.822018349,
0.823853211,0.825688073,0.827522936,0.829357798,0.831192661,0.833027523,
0.834862385,0.836697248,0.83853211,0.840366972,0.842201835,0.844036697,
0.84587156,0.847706422,0.849541284,0.851376147,0.853211009,0.855045872,
0.856880734,0.858715596,0.860550459,0.862385321,0.864220183,0.866055046,
0.867889908,0.869724771,0.871559633,0.873394495,0.875229358,0.87706422,
0.878899083,0.880733945,0.882568807,0.88440367,0.886238532,0.888073394,
0.889908257,0.891743119,0.893577982,0.895412844,0.897247706,0.899082569,
0.900917431,0.902752294,0.904587156,0.906422018,0.908256881,0.910091743,
0.911926606,0.913761468,0.91559633,0.917431193,0.919266055,0.921100917,
0.92293578,0.924770642,0.926605505,0.928440367,0.930275229,0.932110092,
0.933944954,0.935779817,0.937614679,0.939449541,0.941284404,0.943119266,
0.944954128,0.946788991,0.948623853,0.950458716,0.952293578,0.95412844,
0.955963303,0.957798165,0.959633028,0.96146789,0.963302752,0.965137615,
0.966972477,0.968807339,0.970642202,0.972477064,0.974311927,0.976146789,
0.977981651,0.979816514,0.981651376,0.983486239,0.985321101,0.987155963,
0.988990826,0.990825688,0.99266055,0.994495413,0.996330275,0.998165138,
1.000000000411),(0.3,1.,1.3),.UNSPECIFIED.);
#6305=B_SPLINE_SURFACE_WITH_KNOTS('',5,1,((#304635,#304636,#304637),(#304638,
#304639,#304640),(#304641,#304642,#304643),(#304644,#304645,#304646),(#304647,
#304648,#304649),(#304650,#304651,#304652),(#304653,#304654,#304655),(#304656,
#304657,#304658),(#304659,#304660,#304661),(#304662,#304663,#304664),(#304665,
#304666,#304667),(#304668,#304669,#304670),(#304671,#304672,#304673),(#304674,
#304675,#304676),(#304677,#304678,#304679),(#304680,#304681,#304682),(#304683,
#304684,#304685),(#304686,#304687,#304688),(#304689,#304690,#304691),(#304692,
#304693,#304694),(#304695,#304696,#304697),(#304698,#304699,#304700),(#304701,
#304702,#304703),(#304704,#304705,#304706),(#304707,#304708,#304709),(#304710,
#304711,#304712),(#304713,#304714,#304715),(#304716,#304717,#304718),(#304719,
#304720,#304721),(#304722,#304723,#304724),(#304725,#304726,#304727),(#304728,
#304729,#304730),(#304731,#304732,#304733),(#304734,#304735,#304736),(#304737,
#304738,#304739),(#304740,#304741,#304742),(#304743,#304744,#304745),(#304746,
#304747,#304748),(#304749,#304750,#304751),(#304752,#304753,#304754),(#304755,
#304756,#304757),(#304758,#304759,#304760),(#304761,#304762,#304763),(#304764,
#304765,#304766),(#304767,#304768,#304769),(#304770,#304771,#304772),(#304773,
#304774,#304775),(#304776,#304777,#304778),(#304779,#304780,#304781),(#304782,
#304783,#304784),(#304785,#304786,#304787),(#304788,#304789,#304790),(#304791,
#304792,#304793),(#304794,#304795,#304796),(#304797,#304798,#304799),(#304800,
#304801,#304802),(#304803,#304804,#304805),(#304806,#304807,#304808),(#304809,
#304810,#304811),(#304812,#304813,#304814),(#304815,#304816,#304817),(#304818,
#304819,#304820),(#304821,#304822,#304823),(#304824,#304825,#304826),(#304827,
#304828,#304829),(#304830,#304831,#304832),(#304833,#304834,#304835),(#304836,
#304837,#304838),(#304839,#304840,#304841),(#304842,#304843,#304844),(#304845,
#304846,#304847),(#304848,#304849,#304850),(#304851,#304852,#304853),(#304854,
#304855,#304856),(#304857,#304858,#304859),(#304860,#304861,#304862),(#304863,
#304864,#304865),(#304866,#304867,#304868),(#304869,#304870,#304871),(#304872,
#304873,#304874),(#304875,#304876,#304877),(#304878,#304879,#304880),(#304881,
#304882,#304883),(#304884,#304885,#304886),(#304887,#304888,#304889),(#304890,
#304891,#304892),(#304893,#304894,#304895),(#304896,#304897,#304898),(#304899,
#304900,#304901),(#304902,#304903,#304904),(#304905,#304906,#304907),(#304908,
#304909,#304910),(#304911,#304912,#304913),(#304914,#304915,#304916),(#304917,
#304918,#304919),(#304920,#304921,#304922),(#304923,#304924,#304925),(#304926,
#304927,#304928),(#304929,#304930,#304931),(#304932,#304933,#304934),(#304935,
#304936,#304937),(#304938,#304939,#304940),(#304941,#304942,#304943),(#304944,
#304945,#304946),(#304947,#304948,#304949),(#304950,#304951,#304952),(#304953,
#304954,#304955),(#304956,#304957,#304958),(#304959,#304960,#304961),(#304962,
#304963,#304964),(#304965,#304966,#304967),(#304968,#304969,#304970),(#304971,
#304972,#304973),(#304974,#304975,#304976),(#304977,#304978,#304979),(#304980,
#304981,#304982),(#304983,#304984,#304985),(#304986,#304987,#304988),(#304989,
#304990,#304991),(#304992,#304993,#304994),(#304995,#304996,#304997),(#304998,
#304999,#305000),(#305001,#305002,#305003),(#305004,#305005,#305006),(#305007,
#305008,#305009),(#305010,#305011,#305012),(#305013,#305014,#305015),(#305016,
#305017,#305018),(#305019,#305020,#305021),(#305022,#305023,#305024),(#305025,
#305026,#305027),(#305028,#305029,#305030),(#305031,#305032,#305033),(#305034,
#305035,#305036),(#305037,#305038,#305039),(#305040,#305041,#305042),(#305043,
#305044,#305045),(#305046,#305047,#305048),(#305049,#305050,#305051),(#305052,
#305053,#305054),(#305055,#305056,#305057),(#305058,#305059,#305060),(#305061,
#305062,#305063),(#305064,#305065,#305066),(#305067,#305068,#305069),(#305070,
#305071,#305072),(#305073,#305074,#305075),(#305076,#305077,#305078),(#305079,
#305080,#305081),(#305082,#305083,#305084),(#305085,#305086,#305087),(#305088,
#305089,#305090),(#305091,#305092,#305093),(#305094,#305095,#305096),(#305097,
#305098,#305099),(#305100,#305101,#305102),(#305103,#305104,#305105),(#305106,
#305107,#305108),(#305109,#305110,#305111),(#305112,#305113,#305114),(#305115,
#305116,#305117),(#305118,#305119,#305120),(#305121,#305122,#305123),(#305124,
#305125,#305126),(#305127,#305128,#305129),(#305130,#305131,#305132),(#305133,
#305134,#305135),(#305136,#305137,#305138),(#305139,#305140,#305141),(#305142,
#305143,#305144),(#305145,#305146,#305147),(#305148,#305149,#305150),(#305151,
#305152,#305153),(#305154,#305155,#305156),(#305157,#305158,#305159),(#305160,
#305161,#305162),(#305163,#305164,#305165),(#305166,#305167,#305168),(#305169,
#305170,#305171),(#305172,#305173,#305174),(#305175,#305176,#305177),(#305178,
#305179,#305180),(#305181,#305182,#305183),(#305184,#305185,#305186),(#305187,
#305188,#305189),(#305190,#305191,#305192),(#305193,#305194,#305195),(#305196,
#305197,#305198),(#305199,#305200,#305201),(#305202,#305203,#305204),(#305205,
#305206,#305207),(#305208,#305209,#305210),(#305211,#305212,#305213),(#305214,
#305215,#305216),(#305217,#305218,#305219),(#305220,#305221,#305222),(#305223,
#305224,#305225),(#305226,#305227,#305228),(#305229,#305230,#305231),(#305232,
#305233,#305234),(#305235,#305236,#305237),(#305238,#305239,#305240),(#305241,
#305242,#305243),(#305244,#305245,#305246),(#305247,#305248,#305249),(#305250,
#305251,#305252),(#305253,#305254,#305255),(#305256,#305257,#305258),(#305259,
#305260,#305261),(#305262,#305263,#305264),(#305265,#305266,#305267),(#305268,
#305269,#305270),(#305271,#305272,#305273),(#305274,#305275,#305276),(#305277,
#305278,#305279),(#305280,#305281,#305282),(#305283,#305284,#305285),(#305286,
#305287,#305288),(#305289,#305290,#305291),(#305292,#305293,#305294),(#305295,
#305296,#305297),(#305298,#305299,#305300),(#305301,#305302,#305303),(#305304,
#305305,#305306),(#305307,#305308,#305309),(#305310,#305311,#305312),(#305313,
#305314,#305315),(#305316,#305317,#305318),(#305319,#305320,#305321),(#305322,
#305323,#305324),(#305325,#305326,#305327),(#305328,#305329,#305330),(#305331,
#305332,#305333),(#305334,#305335,#305336),(#305337,#305338,#305339),(#305340,
#305341,#305342),(#305343,#305344,#305345),(#305346,#305347,#305348),(#305349,
#305350,#305351),(#305352,#305353,#305354),(#305355,#305356,#305357),(#305358,
#305359,#305360),(#305361,#305362,#305363),(#305364,#305365,#305366),(#305367,
#305368,#305369),(#305370,#305371,#305372),(#305373,#305374,#305375),(#305376,
#305377,#305378),(#305379,#305380,#305381),(#305382,#305383,#305384),(#305385,
#305386,#305387),(#305388,#305389,#305390),(#305391,#305392,#305393),(#305394,
#305395,#305396),(#305397,#305398,#305399),(#305400,#305401,#305402),(#305403,
#305404,#305405),(#305406,#305407,#305408),(#305409,#305410,#305411),(#305412,
#305413,#305414),(#305415,#305416,#305417),(#305418,#305419,#305420),(#305421,
#305422,#305423),(#305424,#305425,#305426),(#305427,#305428,#305429),(#305430,
#305431,#305432),(#305433,#305434,#305435),(#305436,#305437,#305438),(#305439,
#305440,#305441),(#305442,#305443,#305444),(#305445,#305446,#305447),(#305448,
#305449,#305450),(#305451,#305452,#305453),(#305454,#305455,#305456),(#305457,
#305458,#305459),(#305460,#305461,#305462),(#305463,#305464,#305465),(#305466,
#305467,#305468),(#305469,#305470,#305471),(#305472,#305473,#305474),(#305475,
#305476,#305477),(#305478,#305479,#305480),(#305481,#305482,#305483),(#305484,
#305485,#305486),(#305487,#305488,#305489),(#305490,#305491,#305492),(#305493,
#305494,#305495),(#305496,#305497,#305498),(#305499,#305500,#305501),(#305502,
#305503,#305504),(#305505,#305506,#305507),(#305508,#305509,#305510),(#305511,
#305512,#305513),(#305514,#305515,#305516),(#305517,#305518,#305519),(#305520,
#305521,#305522),(#305523,#305524,#305525),(#305526,#305527,#305528),(#305529,
#305530,#305531),(#305532,#305533,#305534),(#305535,#305536,#305537),(#305538,
#305539,#305540),(#305541,#305542,#305543),(#305544,#305545,#305546),(#305547,
#305548,#305549),(#305550,#305551,#305552),(#305553,#305554,#305555),(#305556,
#305557,#305558),(#305559,#305560,#305561),(#305562,#305563,#305564),(#305565,
#305566,#305567),(#305568,#305569,#305570),(#305571,#305572,#305573),(#305574,
#305575,#305576),(#305577,#305578,#305579),(#305580,#305581,#305582),(#305583,
#305584,#305585),(#305586,#305587,#305588),(#305589,#305590,#305591),(#305592,
#305593,#305594),(#305595,#305596,#305597),(#305598,#305599,#305600),(#305601,
#305602,#305603),(#305604,#305605,#305606),(#305607,#305608,#305609),(#305610,
#305611,#305612),(#305613,#305614,#305615),(#305616,#305617,#305618),(#305619,
#305620,#305621),(#305622,#305623,#305624),(#305625,#305626,#305627),(#305628,
#305629,#305630),(#305631,#305632,#305633),(#305634,#305635,#305636),(#305637,
#305638,#305639),(#305640,#305641,#305642),(#305643,#305644,#305645),(#305646,
#305647,#305648),(#305649,#305650,#305651),(#305652,#305653,#305654),(#305655,
#305656,#305657),(#305658,#305659,#305660),(#305661,#305662,#305663),(#305664,
#305665,#305666),(#305667,#305668,#305669),(#305670,#305671,#305672),(#305673,
#305674,#305675),(#305676,#305677,#305678),(#305679,#305680,#305681),(#305682,
#305683,#305684),(#305685,#305686,#305687),(#305688,#305689,#305690),(#305691,
#305692,#305693),(#305694,#305695,#305696),(#305697,#305698,#305699),(#305700,
#305701,#305702),(#305703,#305704,#305705),(#305706,#305707,#305708),(#305709,
#305710,#305711),(#305712,#305713,#305714),(#305715,#305716,#305717),(#305718,
#305719,#305720),(#305721,#305722,#305723),(#305724,#305725,#305726),(#305727,
#305728,#305729),(#305730,#305731,#305732),(#305733,#305734,#305735),(#305736,
#305737,#305738),(#305739,#305740,#305741),(#305742,#305743,#305744),(#305745,
#305746,#305747),(#305748,#305749,#305750),(#305751,#305752,#305753),(#305754,
#305755,#305756),(#305757,#305758,#305759),(#305760,#305761,#305762),(#305763,
#305764,#305765),(#305766,#305767,#305768),(#305769,#305770,#305771),(#305772,
#305773,#305774),(#305775,#305776,#305777),(#305778,#305779,#305780),(#305781,
#305782,#305783),(#305784,#305785,#305786),(#305787,#305788,#305789),(#305790,
#305791,#305792),(#305793,#305794,#305795),(#305796,#305797,#305798),(#305799,
#305800,#305801),(#305802,#305803,#305804),(#305805,#305806,#305807),(#305808,
#305809,#305810),(#305811,#305812,#305813),(#305814,#305815,#305816),(#305817,
#305818,#305819),(#305820,#305821,#305822),(#305823,#305824,#305825),(#305826,
#305827,#305828),(#305829,#305830,#305831),(#305832,#305833,#305834),(#305835,
#305836,#305837),(#305838,#305839,#305840),(#305841,#305842,#305843),(#305844,
#305845,#305846),(#305847,#305848,#305849),(#305850,#305851,#305852),(#305853,
#305854,#305855),(#305856,#305857,#305858),(#305859,#305860,#305861),(#305862,
#305863,#305864),(#305865,#305866,#305867),(#305868,#305869,#305870),(#305871,
#305872,#305873),(#305874,#305875,#305876),(#305877,#305878,#305879),(#305880,
#305881,#305882),(#305883,#305884,#305885),(#305886,#305887,#305888),(#305889,
#305890,#305891),(#305892,#305893,#305894),(#305895,#305896,#305897),(#305898,
#305899,#305900),(#305901,#305902,#305903),(#305904,#305905,#305906),(#305907,
#305908,#305909),(#305910,#305911,#305912),(#305913,#305914,#305915),(#305916,
#305917,#305918),(#305919,#305920,#305921),(#305922,#305923,#305924),(#305925,
#305926,#305927),(#305928,#305929,#305930),(#305931,#305932,#305933),(#305934,
#305935,#305936),(#305937,#305938,#305939),(#305940,#305941,#305942),(#305943,
#305944,#305945),(#305946,#305947,#305948),(#305949,#305950,#305951),(#305952,
#305953,#305954),(#305955,#305956,#305957),(#305958,#305959,#305960),(#305961,
#305962,#305963),(#305964,#305965,#305966),(#305967,#305968,#305969),(#305970,
#305971,#305972),(#305973,#305974,#305975),(#305976,#305977,#305978),(#305979,
#305980,#305981),(#305982,#305983,#305984),(#305985,#305986,#305987),(#305988,
#305989,#305990),(#305991,#305992,#305993),(#305994,#305995,#305996),(#305997,
#305998,#305999),(#306000,#306001,#306002),(#306003,#306004,#306005),(#306006,
#306007,#306008),(#306009,#306010,#306011),(#306012,#306013,#306014),(#306015,
#306016,#306017),(#306018,#306019,#306020),(#306021,#306022,#306023),(#306024,
#306025,#306026),(#306027,#306028,#306029),(#306030,#306031,#306032),(#306033,
#306034,#306035),(#306036,#306037,#306038),(#306039,#306040,#306041),(#306042,
#306043,#306044),(#306045,#306046,#306047),(#306048,#306049,#306050),(#306051,
#306052,#306053),(#306054,#306055,#306056),(#306057,#306058,#306059),(#306060,
#306061,#306062),(#306063,#306064,#306065),(#306066,#306067,#306068),(#306069,
#306070,#306071),(#306072,#306073,#306074),(#306075,#306076,#306077),(#306078,
#306079,#306080),(#306081,#306082,#306083),(#306084,#306085,#306086),(#306087,
#306088,#306089),(#306090,#306091,#306092),(#306093,#306094,#306095),(#306096,
#306097,#306098),(#306099,#306100,#306101),(#306102,#306103,#306104),(#306105,
#306106,#306107),(#306108,#306109,#306110),(#306111,#306112,#306113),(#306114,
#306115,#306116),(#306117,#306118,#306119),(#306120,#306121,#306122),(#306123,
#306124,#306125),(#306126,#306127,#306128),(#306129,#306130,#306131),(#306132,
#306133,#306134),(#306135,#306136,#306137),(#306138,#306139,#306140),(#306141,
#306142,#306143),(#306144,#306145,#306146),(#306147,#306148,#306149),(#306150,
#306151,#306152),(#306153,#306154,#306155),(#306156,#306157,#306158),(#306159,
#306160,#306161),(#306162,#306163,#306164),(#306165,#306166,#306167),(#306168,
#306169,#306170),(#306171,#306172,#306173),(#306174,#306175,#306176),(#306177,
#306178,#306179),(#306180,#306181,#306182),(#306183,#306184,#306185),(#306186,
#306187,#306188),(#306189,#306190,#306191),(#306192,#306193,#306194),(#306195,
#306196,#306197),(#306198,#306199,#306200),(#306201,#306202,#306203),(#306204,
#306205,#306206),(#306207,#306208,#306209),(#306210,#306211,#306212),(#306213,
#306214,#306215),(#306216,#306217,#306218),(#306219,#306220,#306221),(#306222,
#306223,#306224),(#306225,#306226,#306227),(#306228,#306229,#306230),(#306231,
#306232,#306233),(#306234,#306235,#306236),(#306237,#306238,#306239),(#306240,
#306241,#306242),(#306243,#306244,#306245),(#306246,#306247,#306248),(#306249,
#306250,#306251),(#306252,#306253,#306254),(#306255,#306256,#306257),(#306258,
#306259,#306260),(#306261,#306262,#306263),(#306264,#306265,#306266),(#306267,
#306268,#306269),(#306270,#306271,#306272),(#306273,#306274,#306275),(#306276,
#306277,#306278),(#306279,#306280,#306281),(#306282,#306283,#306284)),
 .UNSPECIFIED.,.F.,.F.,.F.,(6,1,1,1,1,1,1,1,1,1,1,1,1,1,1,1,1,1,1,1,1,1,
1,1,1,1,1,1,1,1,1,1,1,1,1,1,1,1,1,1,1,1,1,1,1,1,1,1,1,1,1,1,1,1,1,1,1,1,
1,1,1,1,1,1,1,1,1,1,1,1,1,1,1,1,1,1,1,1,1,1,1,1,1,1,1,1,1,1,1,1,1,1,1,1,
1,1,1,1,1,1,1,1,1,1,1,1,1,1,1,1,1,1,1,1,1,1,1,1,1,1,1,1,1,1,1,1,1,1,1,1,
1,1,1,1,1,1,1,1,1,1,1,1,1,1,1,1,1,1,1,1,1,1,1,1,1,1,1,1,1,1,1,1,1,1,1,1,
1,1,1,1,1,1,1,1,1,1,1,1,1,1,1,1,1,1,1,1,1,1,1,1,1,1,1,1,1,1,1,1,1,1,1,1,
1,1,1,1,1,1,1,1,1,1,1,1,1,1,1,1,1,1,1,1,1,1,1,1,1,1,1,1,1,1,1,1,1,1,1,1,
1,1,1,1,1,1,1,1,1,1,1,1,1,1,1,1,1,1,1,1,1,1,1,1,1,1,1,1,1,1,1,1,1,1,1,1,
1,1,1,1,1,1,1,1,1,1,1,1,1,1,1,1,1,1,1,1,1,1,1,1,1,1,1,1,1,1,1,1,1,1,1,1,
1,1,1,1,1,1,1,1,1,1,1,1,1,1,1,1,1,1,1,1,1,1,1,1,1,1,1,1,1,1,1,1,1,1,1,1,
1,1,1,1,1,1,1,1,1,1,1,1,1,1,1,1,1,1,1,1,1,1,1,1,1,1,1,1,1,1,1,1,1,1,1,1,
1,1,1,1,1,1,1,1,1,1,1,1,1,1,1,1,1,1,1,1,1,1,1,1,1,1,1,1,1,1,1,1,1,1,1,1,
1,1,1,1,1,1,1,1,1,1,1,1,1,1,1,1,1,1,1,1,1,1,1,1,1,1,1,1,1,1,1,1,1,1,1,1,
1,1,1,1,1,1,1,1,1,1,1,1,1,1,1,1,1,1,1,1,1,1,1,1,1,1,1,1,1,1,1,1,1,1,1,1,
1,1,1,1,1,1,1,1,1,1,1,1,1,1,1,1,1,1,1,1,1,1,1,1,1,1,1,1,1,1,1,1,1,1,1,1,
1,1,1,1,1,1,1,1,1,1,1,1,1,1,1,1,1,1,1,6),(2,1,2),(-1.,-0.998165138,-0.996330275,
-0.994495413,-0.99266055,-0.990825688,-0.988990826,-0.987155963,-0.985321101,
-0.983486239,-0.981651376,-0.979816514,-0.977981651,-0.976146789,-0.974311927,
-0.972477064,-0.970642202,-0.968807339,-0.966972477,-0.965137615,-0.963302752,
-0.96146789,-0.959633028,-0.957798165,-0.955963303,-0.95412844,-0.952293578,
-0.950458716,-0.948623853,-0.946788991,-0.944954128,-0.943119266,-0.941284404,
-0.939449541,-0.937614679,-0.935779817,-0.933944954,-0.932110092,-0.930275229,
-0.928440367,-0.926605505,-0.924770642,-0.92293578,-0.921100917,-0.919266055,
-0.917431193,-0.91559633,-0.913761468,-0.911926606,-0.910091743,-0.908256881,
-0.906422018,-0.904587156,-0.902752294,-0.900917431,-0.899082569,-0.897247706,
-0.895412844,-0.893577982,-0.891743119,-0.889908257,-0.888073394,-0.886238532,
-0.88440367,-0.882568807,-0.880733945,-0.878899083,-0.87706422,-0.875229358,
-0.873394495,-0.871559633,-0.869724771,-0.867889908,-0.866055046,-0.864220183,
-0.862385321,-0.860550459,-0.858715596,-0.856880734,-0.855045872,-0.853211009,
-0.851376147,-0.849541284,-0.847706422,-0.84587156,-0.844036697,-0.842201835,
-0.840366972,-0.83853211,-0.836697248,-0.834862385,-0.833027523,-0.831192661,
-0.829357798,-0.827522936,-0.825688073,-0.823853211,-0.822018349,-0.820183486,
-0.818348624,-0.816513761,-0.814678899,-0.812844037,-0.811009174,-0.809174312,
-0.80733945,-0.805504587,-0.803669725,-0.801834862,-0.8,-0.798165138,-0.796330275,
-0.794495413,-0.79266055,-0.790825688,-0.788990826,-0.787155963,-0.785321101,
-0.783486239,-0.781651376,-0.779816514,-0.777981651,-0.776146789,-0.774311927,
-0.772477064,-0.770642202,-0.768807339,-0.766972477,-0.765137615,-0.763302752,
-0.76146789,-0.759633028,-0.757798165,-0.755963303,-0.75412844,-0.752293578,
-0.750458716,-0.748623853,-0.746788991,-0.744954128,-0.743119266,-0.741284404,
-0.739449541,-0.737614679,-0.735779817,-0.733944954,-0.732110092,-0.730275229,
-0.728440367,-0.726605505,-0.724770642,-0.72293578,-0.721100917,-0.719266055,
-0.717431193,-0.71559633,-0.713761468,-0.711926606,-0.710091743,-0.708256881,
-0.706422018,-0.704587156,-0.702752294,-0.700917431,-0.699082569,-0.697247706,
-0.695412844,-0.693577982,-0.691743119,-0.689908257,-0.688073394,-0.686238532,
-0.68440367,-0.682568807,-0.680733945,-0.678899083,-0.67706422,-0.675229358,
-0.673394495,-0.671559633,-0.669724771,-0.667889908,-0.666055046,-0.664220183,
-0.662385321,-0.660550459,-0.658715596,-0.656880734,-0.655045872,-0.653211009,
-0.651376147,-0.649541284,-0.647706422,-0.64587156,-0.644036697,-0.642201835,
-0.640366972,-0.63853211,-0.636697248,-0.634862385,-0.633027523,-0.631192661,
-0.629357798,-0.627522936,-0.625688073,-0.623853211,-0.622018349,-0.620183486,
-0.618348624,-0.616513761,-0.614678899,-0.612844037,-0.611009174,-0.609174312,
-0.60733945,-0.605504587,-0.603669725,-0.601834862,-0.6,-0.598165138,-0.596330275,
-0.594495413,-0.59266055,-0.590825688,-0.588990826,-0.587155963,-0.585321101,
-0.583486239,-0.581651376,-0.579816514,-0.577981651,-0.576146789,-0.574311927,
-0.572477064,-0.570642202,-0.568807339,-0.566972477,-0.565137615,-0.563302752,
-0.56146789,-0.559633028,-0.557798165,-0.555963303,-0.55412844,-0.552293578,
-0.550458716,-0.548623853,-0.546788991,-0.544954128,-0.543119266,-0.541284404,
-0.539449541,-0.537614679,-0.535779817,-0.533944954,-0.532110092,-0.530275229,
-0.528440367,-0.526605505,-0.524770642,-0.52293578,-0.521100917,-0.519266055,
-0.517431193,-0.51559633,-0.513761468,-0.511926606,-0.510091743,-0.508256881,
-0.506422018,-0.504587156,-0.502752294,-0.500917431,-0.499082569,-0.497247706,
-0.495412844,-0.493577982,-0.491743119,-0.489908257,-0.488073394,-0.486238532,
-0.48440367,-0.482568807,-0.480733945,-0.478899083,-0.47706422,-0.475229358,
-0.473394495,-0.471559633,-0.469724771,-0.467889908,-0.466055046,-0.464220183,
-0.462385321,-0.460550459,-0.458715596,-0.456880734,-0.455045872,-0.453211009,
-0.451376147,-0.449541284,-0.447706422,-0.44587156,-0.444036697,-0.442201835,
-0.440366972,-0.43853211,-0.436697248,-0.434862385,-0.433027523,-0.431192661,
-0.429357798,-0.427522936,-0.425688073,-0.423853211,-0.422018349,-0.420183486,
-0.418348624,-0.416513761,-0.414678899,-0.412844037,-0.411009174,-0.409174312,
-0.40733945,-0.405504587,-0.403669725,-0.401834862,-0.4,-0.398165138,-0.396330275,
-0.394495413,-0.39266055,-0.390825688,-0.388990826,-0.387155963,-0.385321101,
-0.383486239,-0.381651376,-0.379816514,-0.377981651,-0.376146789,-0.374311927,
-0.372477064,-0.370642202,-0.368807339,-0.366972477,-0.365137615,-0.363302752,
-0.36146789,-0.359633028,-0.357798165,-0.355963303,-0.35412844,-0.352293578,
-0.350458716,-0.348623853,-0.346788991,-0.344954128,-0.343119266,-0.341284404,
-0.339449541,-0.337614679,-0.335779817,-0.333944954,-0.332110092,-0.330275229,
-0.328440367,-0.326605505,-0.324770642,-0.32293578,-0.321100917,-0.319266055,
-0.317431193,-0.31559633,-0.313761468,-0.311926606,-0.310091743,-0.308256881,
-0.306422018,-0.304587156,-0.302752294,-0.300917431,-0.299082569,-0.297247706,
-0.295412844,-0.293577982,-0.291743119,-0.289908257,-0.288073394,-0.286238532,
-0.28440367,-0.282568807,-0.280733945,-0.278899083,-0.27706422,-0.275229358,
-0.273394495,-0.271559633,-0.269724771,-0.267889908,-0.266055046,-0.264220183,
-0.262385321,-0.260550459,-0.258715596,-0.256880734,-0.255045872,-0.253211009,
-0.251376147,-0.249541284,-0.247706422,-0.24587156,-0.244036697,-0.242201835,
-0.240366972,-0.23853211,-0.236697248,-0.234862385,-0.233027523,-0.231192661,
-0.229357798,-0.227522936,-0.225688073,-0.223853211,-0.222018349,-0.220183486,
-0.218348624,-0.216513761,-0.214678899,-0.212844037,-0.211009174,-0.209174312,
-0.20733945,-0.205504587,-0.203669725,-0.201834862,-0.2,-0.198165138,-0.196330275,
-0.194495413,-0.19266055,-0.190825688,-0.188990826,-0.187155963,-0.185321101,
-0.183486239,-0.181651376,-0.179816514,-0.177981651,-0.176146789,-0.174311927,
-0.172477064,-0.170642202,-0.168807339,-0.166972477,-0.165137615,-0.163302752,
-0.16146789,-0.159633028,-0.157798165,-0.155963303,-0.15412844,-0.152293578,
-0.150458716,-0.148623853,-0.146788991,-0.144954128,-0.143119266,-0.141284404,
-0.139449541,-0.137614679,-0.135779817,-0.133944954,-0.132110092,-0.130275229,
-0.128440367,-0.126605505,-0.124770642,-0.12293578,-0.121100917,-0.119266055,
-0.117431193,-0.11559633,-0.113761468,-0.111926606,-0.110091743,-0.108256881,
-0.106422018,-0.104587156,-0.102752294,-0.100917431,-0.099082569,-0.097247706,
-0.095412844,-0.093577982,-0.091743119,-0.089908257,-0.088073394,-0.086238532,
-0.08440367,-0.082568807,-0.080733945,-0.078899083,-0.07706422,-0.075229358,
-0.073394495,-0.071559633,-0.069724771,-0.067889908,-0.066055046,-0.064220183,
-0.062385321,-0.060550459,-0.058715596,-0.056880734,-0.055045872,-0.053211009,
-0.051376147,-0.049541284,-0.047706422,-0.04587156,-0.044036697,-0.042201835,
-0.040366972,-0.03853211,-0.036697248,-0.034862385,-0.033027523,-0.031192661,
-0.029357798,-0.027522936,-0.025688073,-0.023853211,-0.022018349,-0.020183486,
-0.018348624,-0.016513761,-0.014678899,-0.012844037,-0.011009174,-0.009174312,
-0.00733945,-0.005504587,-0.003669725,-0.001834862,0.000982135),(0.3,1.,
1.3),.UNSPECIFIED.);
#6306=B_SPLINE_SURFACE_WITH_KNOTS('',5,1,((#306307,#306308,#306309),(#306310,
#306311,#306312),(#306313,#306314,#306315),(#306316,#306317,#306318),(#306319,
#306320,#306321),(#306322,#306323,#306324),(#306325,#306326,#306327),(#306328,
#306329,#306330),(#306331,#306332,#306333),(#306334,#306335,#306336),(#306337,
#306338,#306339),(#306340,#306341,#306342),(#306343,#306344,#306345),(#306346,
#306347,#306348),(#306349,#306350,#306351),(#306352,#306353,#306354),(#306355,
#306356,#306357),(#306358,#306359,#306360),(#306361,#306362,#306363),(#306364,
#306365,#306366),(#306367,#306368,#306369),(#306370,#306371,#306372),(#306373,
#306374,#306375),(#306376,#306377,#306378),(#306379,#306380,#306381),(#306382,
#306383,#306384),(#306385,#306386,#306387),(#306388,#306389,#306390),(#306391,
#306392,#306393),(#306394,#306395,#306396),(#306397,#306398,#306399),(#306400,
#306401,#306402),(#306403,#306404,#306405),(#306406,#306407,#306408),(#306409,
#306410,#306411),(#306412,#306413,#306414),(#306415,#306416,#306417),(#306418,
#306419,#306420),(#306421,#306422,#306423),(#306424,#306425,#306426),(#306427,
#306428,#306429),(#306430,#306431,#306432),(#306433,#306434,#306435),(#306436,
#306437,#306438),(#306439,#306440,#306441),(#306442,#306443,#306444),(#306445,
#306446,#306447),(#306448,#306449,#306450),(#306451,#306452,#306453),(#306454,
#306455,#306456),(#306457,#306458,#306459),(#306460,#306461,#306462),(#306463,
#306464,#306465),(#306466,#306467,#306468),(#306469,#306470,#306471),(#306472,
#306473,#306474),(#306475,#306476,#306477),(#306478,#306479,#306480),(#306481,
#306482,#306483),(#306484,#306485,#306486),(#306487,#306488,#306489),(#306490,
#306491,#306492),(#306493,#306494,#306495),(#306496,#306497,#306498),(#306499,
#306500,#306501),(#306502,#306503,#306504),(#306505,#306506,#306507),(#306508,
#306509,#306510),(#306511,#306512,#306513),(#306514,#306515,#306516),(#306517,
#306518,#306519),(#306520,#306521,#306522),(#306523,#306524,#306525),(#306526,
#306527,#306528),(#306529,#306530,#306531),(#306532,#306533,#306534),(#306535,
#306536,#306537),(#306538,#306539,#306540),(#306541,#306542,#306543),(#306544,
#306545,#306546),(#306547,#306548,#306549),(#306550,#306551,#306552),(#306553,
#306554,#306555),(#306556,#306557,#306558),(#306559,#306560,#306561),(#306562,
#306563,#306564),(#306565,#306566,#306567),(#306568,#306569,#306570),(#306571,
#306572,#306573),(#306574,#306575,#306576),(#306577,#306578,#306579),(#306580,
#306581,#306582),(#306583,#306584,#306585),(#306586,#306587,#306588),(#306589,
#306590,#306591),(#306592,#306593,#306594),(#306595,#306596,#306597),(#306598,
#306599,#306600),(#306601,#306602,#306603),(#306604,#306605,#306606),(#306607,
#306608,#306609),(#306610,#306611,#306612),(#306613,#306614,#306615),(#306616,
#306617,#306618),(#306619,#306620,#306621),(#306622,#306623,#306624),(#306625,
#306626,#306627),(#306628,#306629,#306630),(#306631,#306632,#306633),(#306634,
#306635,#306636),(#306637,#306638,#306639),(#306640,#306641,#306642),(#306643,
#306644,#306645),(#306646,#306647,#306648),(#306649,#306650,#306651),(#306652,
#306653,#306654),(#306655,#306656,#306657),(#306658,#306659,#306660),(#306661,
#306662,#306663),(#306664,#306665,#306666),(#306667,#306668,#306669),(#306670,
#306671,#306672),(#306673,#306674,#306675),(#306676,#306677,#306678),(#306679,
#306680,#306681),(#306682,#306683,#306684),(#306685,#306686,#306687),(#306688,
#306689,#306690),(#306691,#306692,#306693),(#306694,#306695,#306696),(#306697,
#306698,#306699),(#306700,#306701,#306702),(#306703,#306704,#306705),(#306706,
#306707,#306708),(#306709,#306710,#306711),(#306712,#306713,#306714),(#306715,
#306716,#306717),(#306718,#306719,#306720),(#306721,#306722,#306723),(#306724,
#306725,#306726),(#306727,#306728,#306729),(#306730,#306731,#306732),(#306733,
#306734,#306735),(#306736,#306737,#306738),(#306739,#306740,#306741),(#306742,
#306743,#306744),(#306745,#306746,#306747),(#306748,#306749,#306750),(#306751,
#306752,#306753),(#306754,#306755,#306756),(#306757,#306758,#306759),(#306760,
#306761,#306762),(#306763,#306764,#306765),(#306766,#306767,#306768),(#306769,
#306770,#306771),(#306772,#306773,#306774),(#306775,#306776,#306777),(#306778,
#306779,#306780),(#306781,#306782,#306783),(#306784,#306785,#306786),(#306787,
#306788,#306789),(#306790,#306791,#306792),(#306793,#306794,#306795),(#306796,
#306797,#306798),(#306799,#306800,#306801),(#306802,#306803,#306804),(#306805,
#306806,#306807),(#306808,#306809,#306810),(#306811,#306812,#306813),(#306814,
#306815,#306816),(#306817,#306818,#306819),(#306820,#306821,#306822),(#306823,
#306824,#306825),(#306826,#306827,#306828),(#306829,#306830,#306831),(#306832,
#306833,#306834),(#306835,#306836,#306837),(#306838,#306839,#306840),(#306841,
#306842,#306843),(#306844,#306845,#306846),(#306847,#306848,#306849),(#306850,
#306851,#306852),(#306853,#306854,#306855),(#306856,#306857,#306858),(#306859,
#306860,#306861),(#306862,#306863,#306864),(#306865,#306866,#306867),(#306868,
#306869,#306870),(#306871,#306872,#306873),(#306874,#306875,#306876),(#306877,
#306878,#306879),(#306880,#306881,#306882),(#306883,#306884,#306885),(#306886,
#306887,#306888),(#306889,#306890,#306891),(#306892,#306893,#306894),(#306895,
#306896,#306897),(#306898,#306899,#306900),(#306901,#306902,#306903),(#306904,
#306905,#306906),(#306907,#306908,#306909),(#306910,#306911,#306912),(#306913,
#306914,#306915),(#306916,#306917,#306918),(#306919,#306920,#306921),(#306922,
#306923,#306924),(#306925,#306926,#306927),(#306928,#306929,#306930),(#306931,
#306932,#306933),(#306934,#306935,#306936),(#306937,#306938,#306939),(#306940,
#306941,#306942),(#306943,#306944,#306945),(#306946,#306947,#306948),(#306949,
#306950,#306951),(#306952,#306953,#306954),(#306955,#306956,#306957),(#306958,
#306959,#306960),(#306961,#306962,#306963),(#306964,#306965,#306966),(#306967,
#306968,#306969),(#306970,#306971,#306972),(#306973,#306974,#306975),(#306976,
#306977,#306978),(#306979,#306980,#306981),(#306982,#306983,#306984),(#306985,
#306986,#306987),(#306988,#306989,#306990),(#306991,#306992,#306993),(#306994,
#306995,#306996),(#306997,#306998,#306999),(#307000,#307001,#307002),(#307003,
#307004,#307005),(#307006,#307007,#307008),(#307009,#307010,#307011),(#307012,
#307013,#307014),(#307015,#307016,#307017),(#307018,#307019,#307020),(#307021,
#307022,#307023),(#307024,#307025,#307026),(#307027,#307028,#307029),(#307030,
#307031,#307032),(#307033,#307034,#307035),(#307036,#307037,#307038),(#307039,
#307040,#307041),(#307042,#307043,#307044),(#307045,#307046,#307047),(#307048,
#307049,#307050),(#307051,#307052,#307053),(#307054,#307055,#307056),(#307057,
#307058,#307059),(#307060,#307061,#307062),(#307063,#307064,#307065),(#307066,
#307067,#307068),(#307069,#307070,#307071),(#307072,#307073,#307074),(#307075,
#307076,#307077),(#307078,#307079,#307080),(#307081,#307082,#307083),(#307084,
#307085,#307086),(#307087,#307088,#307089),(#307090,#307091,#307092),(#307093,
#307094,#307095),(#307096,#307097,#307098),(#307099,#307100,#307101),(#307102,
#307103,#307104),(#307105,#307106,#307107),(#307108,#307109,#307110),(#307111,
#307112,#307113),(#307114,#307115,#307116),(#307117,#307118,#307119),(#307120,
#307121,#307122),(#307123,#307124,#307125),(#307126,#307127,#307128),(#307129,
#307130,#307131),(#307132,#307133,#307134),(#307135,#307136,#307137),(#307138,
#307139,#307140),(#307141,#307142,#307143),(#307144,#307145,#307146),(#307147,
#307148,#307149),(#307150,#307151,#307152),(#307153,#307154,#307155),(#307156,
#307157,#307158),(#307159,#307160,#307161),(#307162,#307163,#307164),(#307165,
#307166,#307167),(#307168,#307169,#307170),(#307171,#307172,#307173),(#307174,
#307175,#307176),(#307177,#307178,#307179),(#307180,#307181,#307182),(#307183,
#307184,#307185),(#307186,#307187,#307188),(#307189,#307190,#307191),(#307192,
#307193,#307194),(#307195,#307196,#307197),(#307198,#307199,#307200),(#307201,
#307202,#307203),(#307204,#307205,#307206),(#307207,#307208,#307209),(#307210,
#307211,#307212),(#307213,#307214,#307215),(#307216,#307217,#307218),(#307219,
#307220,#307221),(#307222,#307223,#307224),(#307225,#307226,#307227),(#307228,
#307229,#307230),(#307231,#307232,#307233),(#307234,#307235,#307236),(#307237,
#307238,#307239),(#307240,#307241,#307242),(#307243,#307244,#307245),(#307246,
#307247,#307248),(#307249,#307250,#307251),(#307252,#307253,#307254),(#307255,
#307256,#307257),(#307258,#307259,#307260),(#307261,#307262,#307263),(#307264,
#307265,#307266),(#307267,#307268,#307269),(#307270,#307271,#307272),(#307273,
#307274,#307275),(#307276,#307277,#307278),(#307279,#307280,#307281),(#307282,
#307283,#307284),(#307285,#307286,#307287),(#307288,#307289,#307290),(#307291,
#307292,#307293),(#307294,#307295,#307296),(#307297,#307298,#307299),(#307300,
#307301,#307302),(#307303,#307304,#307305),(#307306,#307307,#307308),(#307309,
#307310,#307311),(#307312,#307313,#307314),(#307315,#307316,#307317),(#307318,
#307319,#307320),(#307321,#307322,#307323),(#307324,#307325,#307326),(#307327,
#307328,#307329),(#307330,#307331,#307332),(#307333,#307334,#307335),(#307336,
#307337,#307338),(#307339,#307340,#307341),(#307342,#307343,#307344),(#307345,
#307346,#307347),(#307348,#307349,#307350),(#307351,#307352,#307353),(#307354,
#307355,#307356),(#307357,#307358,#307359),(#307360,#307361,#307362),(#307363,
#307364,#307365),(#307366,#307367,#307368),(#307369,#307370,#307371),(#307372,
#307373,#307374),(#307375,#307376,#307377),(#307378,#307379,#307380),(#307381,
#307382,#307383),(#307384,#307385,#307386),(#307387,#307388,#307389),(#307390,
#307391,#307392),(#307393,#307394,#307395),(#307396,#307397,#307398),(#307399,
#307400,#307401),(#307402,#307403,#307404),(#307405,#307406,#307407),(#307408,
#307409,#307410),(#307411,#307412,#307413),(#307414,#307415,#307416),(#307417,
#307418,#307419),(#307420,#307421,#307422),(#307423,#307424,#307425),(#307426,
#307427,#307428),(#307429,#307430,#307431),(#307432,#307433,#307434),(#307435,
#307436,#307437),(#307438,#307439,#307440),(#307441,#307442,#307443),(#307444,
#307445,#307446),(#307447,#307448,#307449),(#307450,#307451,#307452),(#307453,
#307454,#307455),(#307456,#307457,#307458),(#307459,#307460,#307461),(#307462,
#307463,#307464),(#307465,#307466,#307467),(#307468,#307469,#307470),(#307471,
#307472,#307473),(#307474,#307475,#307476),(#307477,#307478,#307479),(#307480,
#307481,#307482),(#307483,#307484,#307485),(#307486,#307487,#307488),(#307489,
#307490,#307491),(#307492,#307493,#307494),(#307495,#307496,#307497),(#307498,
#307499,#307500),(#307501,#307502,#307503),(#307504,#307505,#307506),(#307507,
#307508,#307509),(#307510,#307511,#307512),(#307513,#307514,#307515),(#307516,
#307517,#307518),(#307519,#307520,#307521),(#307522,#307523,#307524),(#307525,
#307526,#307527),(#307528,#307529,#307530),(#307531,#307532,#307533),(#307534,
#307535,#307536),(#307537,#307538,#307539),(#307540,#307541,#307542),(#307543,
#307544,#307545),(#307546,#307547,#307548),(#307549,#307550,#307551),(#307552,
#307553,#307554),(#307555,#307556,#307557),(#307558,#307559,#307560),(#307561,
#307562,#307563),(#307564,#307565,#307566),(#307567,#307568,#307569),(#307570,
#307571,#307572),(#307573,#307574,#307575),(#307576,#307577,#307578),(#307579,
#307580,#307581),(#307582,#307583,#307584),(#307585,#307586,#307587),(#307588,
#307589,#307590),(#307591,#307592,#307593),(#307594,#307595,#307596),(#307597,
#307598,#307599),(#307600,#307601,#307602),(#307603,#307604,#307605),(#307606,
#307607,#307608),(#307609,#307610,#307611),(#307612,#307613,#307614),(#307615,
#307616,#307617),(#307618,#307619,#307620),(#307621,#307622,#307623),(#307624,
#307625,#307626),(#307627,#307628,#307629),(#307630,#307631,#307632),(#307633,
#307634,#307635),(#307636,#307637,#307638),(#307639,#307640,#307641),(#307642,
#307643,#307644),(#307645,#307646,#307647),(#307648,#307649,#307650),(#307651,
#307652,#307653),(#307654,#307655,#307656),(#307657,#307658,#307659),(#307660,
#307661,#307662),(#307663,#307664,#307665),(#307666,#307667,#307668),(#307669,
#307670,#307671),(#307672,#307673,#307674),(#307675,#307676,#307677),(#307678,
#307679,#307680),(#307681,#307682,#307683),(#307684,#307685,#307686),(#307687,
#307688,#307689),(#307690,#307691,#307692),(#307693,#307694,#307695),(#307696,
#307697,#307698),(#307699,#307700,#307701),(#307702,#307703,#307704),(#307705,
#307706,#307707),(#307708,#307709,#307710),(#307711,#307712,#307713),(#307714,
#307715,#307716),(#307717,#307718,#307719),(#307720,#307721,#307722),(#307723,
#307724,#307725),(#307726,#307727,#307728),(#307729,#307730,#307731),(#307732,
#307733,#307734),(#307735,#307736,#307737),(#307738,#307739,#307740),(#307741,
#307742,#307743),(#307744,#307745,#307746),(#307747,#307748,#307749),(#307750,
#307751,#307752),(#307753,#307754,#307755),(#307756,#307757,#307758),(#307759,
#307760,#307761),(#307762,#307763,#307764),(#307765,#307766,#307767),(#307768,
#307769,#307770),(#307771,#307772,#307773),(#307774,#307775,#307776),(#307777,
#307778,#307779),(#307780,#307781,#307782),(#307783,#307784,#307785),(#307786,
#307787,#307788),(#307789,#307790,#307791),(#307792,#307793,#307794),(#307795,
#307796,#307797),(#307798,#307799,#307800),(#307801,#307802,#307803),(#307804,
#307805,#307806),(#307807,#307808,#307809),(#307810,#307811,#307812),(#307813,
#307814,#307815),(#307816,#307817,#307818),(#307819,#307820,#307821),(#307822,
#307823,#307824),(#307825,#307826,#307827),(#307828,#307829,#307830),(#307831,
#307832,#307833),(#307834,#307835,#307836),(#307837,#307838,#307839),(#307840,
#307841,#307842),(#307843,#307844,#307845),(#307846,#307847,#307848),(#307849,
#307850,#307851),(#307852,#307853,#307854),(#307855,#307856,#307857),(#307858,
#307859,#307860),(#307861,#307862,#307863),(#307864,#307865,#307866),(#307867,
#307868,#307869),(#307870,#307871,#307872),(#307873,#307874,#307875),(#307876,
#307877,#307878),(#307879,#307880,#307881),(#307882,#307883,#307884),(#307885,
#307886,#307887),(#307888,#307889,#307890),(#307891,#307892,#307893),(#307894,
#307895,#307896),(#307897,#307898,#307899),(#307900,#307901,#307902),(#307903,
#307904,#307905),(#307906,#307907,#307908),(#307909,#307910,#307911),(#307912,
#307913,#307914),(#307915,#307916,#307917),(#307918,#307919,#307920),(#307921,
#307922,#307923),(#307924,#307925,#307926),(#307927,#307928,#307929),(#307930,
#307931,#307932),(#307933,#307934,#307935),(#307936,#307937,#307938),(#307939,
#307940,#307941),(#307942,#307943,#307944),(#307945,#307946,#307947),(#307948,
#307949,#307950),(#307951,#307952,#307953),(#307954,#307955,#307956),(#307957,
#307958,#307959)),.UNSPECIFIED.,.F.,.F.,.F.,(6,1,1,1,1,1,1,1,1,1,1,1,1,
1,1,1,1,1,1,1,1,1,1,1,1,1,1,1,1,1,1,1,1,1,1,1,1,1,1,1,1,1,1,1,1,1,1,1,1,
1,1,1,1,1,1,1,1,1,1,1,1,1,1,1,1,1,1,1,1,1,1,1,1,1,1,1,1,1,1,1,1,1,1,1,1,
1,1,1,1,1,1,1,1,1,1,1,1,1,1,1,1,1,1,1,1,1,1,1,1,1,1,1,1,1,1,1,1,1,1,1,1,
1,1,1,1,1,1,1,1,1,1,1,1,1,1,1,1,1,1,1,1,1,1,1,1,1,1,1,1,1,1,1,1,1,1,1,1,
1,1,1,1,1,1,1,1,1,1,1,1,1,1,1,1,1,1,1,1,1,1,1,1,1,1,1,1,1,1,1,1,1,1,1,1,
1,1,1,1,1,1,1,1,1,1,1,1,1,1,1,1,1,1,1,1,1,1,1,1,1,1,1,1,1,1,1,1,1,1,1,1,
1,1,1,1,1,1,1,1,1,1,1,1,1,1,1,1,1,1,1,1,1,1,1,1,1,1,1,1,1,1,1,1,1,1,1,1,
1,1,1,1,1,1,1,1,1,1,1,1,1,1,1,1,1,1,1,1,1,1,1,1,1,1,1,1,1,1,1,1,1,1,1,1,
1,1,1,1,1,1,1,1,1,1,1,1,1,1,1,1,1,1,1,1,1,1,1,1,1,1,1,1,1,1,1,1,1,1,1,1,
1,1,1,1,1,1,1,1,1,1,1,1,1,1,1,1,1,1,1,1,1,1,1,1,1,1,1,1,1,1,1,1,1,1,1,1,
1,1,1,1,1,1,1,1,1,1,1,1,1,1,1,1,1,1,1,1,1,1,1,1,1,1,1,1,1,1,1,1,1,1,1,1,
1,1,1,1,1,1,1,1,1,1,1,1,1,1,1,1,1,1,1,1,1,1,1,1,1,1,1,1,1,1,1,1,1,1,1,1,
1,1,1,1,1,1,1,1,1,1,1,1,1,1,1,1,1,1,1,1,1,1,1,1,1,1,1,1,1,1,1,1,1,1,1,1,
1,1,1,1,1,1,1,1,1,1,1,1,1,1,1,1,1,1,1,1,1,1,1,1,1,1,1,1,1,1,1,1,1,1,1,1,
1,1,1,1,1,1,1,1,1,1,1,1,1,1,1,1,1,1,1,1,1,1,1,1,1,1,1,1,1,6),(2,1,2),(-0.001964191,
0.,0.001834862,0.003669725,0.005504587,0.00733945,0.009174312,0.011009174,
0.012844037,0.014678899,0.016513761,0.018348624,0.020183486,0.022018349,
0.023853211,0.025688073,0.027522936,0.029357798,0.031192661,0.033027523,
0.034862385,0.036697248,0.03853211,0.040366972,0.042201835,0.044036697,
0.04587156,0.047706422,0.049541284,0.051376147,0.053211009,0.055045872,
0.056880734,0.058715596,0.060550459,0.062385321,0.064220183,0.066055046,
0.067889908,0.069724771,0.071559633,0.073394495,0.075229358,0.07706422,
0.078899083,0.080733945,0.082568807,0.08440367,0.086238532,0.088073394,
0.089908257,0.091743119,0.093577982,0.095412844,0.097247706,0.099082569,
0.100917431,0.102752294,0.104587156,0.106422018,0.108256881,0.110091743,
0.111926606,0.113761468,0.11559633,0.117431193,0.119266055,0.121100917,
0.12293578,0.124770642,0.126605505,0.128440367,0.130275229,0.132110092,
0.133944954,0.135779817,0.137614679,0.139449541,0.141284404,0.143119266,
0.144954128,0.146788991,0.148623853,0.150458716,0.152293578,0.15412844,
0.155963303,0.157798165,0.159633028,0.16146789,0.163302752,0.165137615,
0.166972477,0.168807339,0.170642202,0.172477064,0.174311927,0.176146789,
0.177981651,0.179816514,0.181651376,0.183486239,0.185321101,0.187155963,
0.188990826,0.190825688,0.19266055,0.194495413,0.196330275,0.198165138,
0.2,0.201834862,0.203669725,0.205504587,0.20733945,0.209174312,0.211009174,
0.212844037,0.214678899,0.216513761,0.218348624,0.220183486,0.222018349,
0.223853211,0.225688073,0.227522936,0.229357798,0.231192661,0.233027523,
0.234862385,0.236697248,0.23853211,0.240366972,0.242201835,0.244036697,
0.24587156,0.247706422,0.249541284,0.251376147,0.253211009,0.255045872,
0.256880734,0.258715596,0.260550459,0.262385321,0.264220183,0.266055046,
0.267889908,0.269724771,0.271559633,0.273394495,0.275229358,0.27706422,
0.278899083,0.280733945,0.282568807,0.28440367,0.286238532,0.288073394,
0.289908257,0.291743119,0.293577982,0.295412844,0.297247706,0.299082569,
0.300917431,0.302752294,0.304587156,0.306422018,0.308256881,0.310091743,
0.311926606,0.313761468,0.31559633,0.317431193,0.319266055,0.321100917,
0.32293578,0.324770642,0.326605505,0.328440367,0.330275229,0.332110092,
0.333944954,0.335779817,0.337614679,0.339449541,0.341284404,0.343119266,
0.344954128,0.346788991,0.348623853,0.350458716,0.352293578,0.35412844,
0.355963303,0.357798165,0.359633028,0.36146789,0.363302752,0.365137615,
0.366972477,0.368807339,0.370642202,0.372477064,0.374311927,0.376146789,
0.377981651,0.379816514,0.381651376,0.383486239,0.385321101,0.387155963,
0.388990826,0.390825688,0.39266055,0.394495413,0.396330275,0.398165138,
0.4,0.401834862,0.403669725,0.405504587,0.40733945,0.409174312,0.411009174,
0.412844037,0.414678899,0.416513761,0.418348624,0.420183486,0.422018349,
0.423853211,0.425688073,0.427522936,0.429357798,0.431192661,0.433027523,
0.434862385,0.436697248,0.43853211,0.440366972,0.442201835,0.444036697,
0.44587156,0.447706422,0.449541284,0.451376147,0.453211009,0.455045872,
0.456880734,0.458715596,0.460550459,0.462385321,0.464220183,0.466055046,
0.467889908,0.469724771,0.471559633,0.473394495,0.475229358,0.47706422,
0.478899083,0.480733945,0.482568807,0.48440367,0.486238532,0.488073394,
0.489908257,0.491743119,0.493577982,0.495412844,0.497247706,0.499082569,
0.500917431,0.502752294,0.504587156,0.506422018,0.508256881,0.510091743,
0.511926606,0.513761468,0.51559633,0.517431193,0.519266055,0.521100917,
0.52293578,0.524770642,0.526605505,0.528440367,0.530275229,0.532110092,
0.533944954,0.535779817,0.537614679,0.539449541,0.541284404,0.543119266,
0.544954128,0.546788991,0.548623853,0.550458716,0.552293578,0.55412844,
0.555963303,0.557798165,0.559633028,0.56146789,0.563302752,0.565137615,
0.566972477,0.568807339,0.570642202,0.572477064,0.574311927,0.576146789,
0.577981651,0.579816514,0.581651376,0.583486239,0.585321101,0.587155963,
0.588990826,0.590825688,0.59266055,0.594495413,0.596330275,0.598165138,
0.6,0.601834862,0.603669725,0.605504587,0.60733945,0.609174312,0.611009174,
0.612844037,0.614678899,0.616513761,0.618348624,0.620183486,0.622018349,
0.623853211,0.625688073,0.627522936,0.629357798,0.631192661,0.633027523,
0.634862385,0.636697248,0.63853211,0.640366972,0.642201835,0.644036697,
0.64587156,0.647706422,0.649541284,0.651376147,0.653211009,0.655045872,
0.656880734,0.658715596,0.660550459,0.662385321,0.664220183,0.666055046,
0.667889908,0.669724771,0.671559633,0.673394495,0.675229358,0.67706422,
0.678899083,0.680733945,0.682568807,0.68440367,0.686238532,0.688073394,
0.689908257,0.691743119,0.693577982,0.695412844,0.697247706,0.699082569,
0.700917431,0.702752294,0.704587156,0.706422018,0.708256881,0.710091743,
0.711926606,0.713761468,0.71559633,0.717431193,0.719266055,0.721100917,
0.72293578,0.724770642,0.726605505,0.728440367,0.730275229,0.732110092,
0.733944954,0.735779817,0.737614679,0.739449541,0.741284404,0.743119266,
0.744954128,0.746788991,0.748623853,0.750458716,0.752293578,0.75412844,
0.755963303,0.757798165,0.759633028,0.76146789,0.763302752,0.765137615,
0.766972477,0.768807339,0.770642202,0.772477064,0.774311927,0.776146789,
0.777981651,0.779816514,0.781651376,0.783486239,0.785321101,0.787155963,
0.788990826,0.790825688,0.79266055,0.794495413,0.796330275,0.798165138,
0.8,0.801834862,0.803669725,0.805504587,0.80733945,0.809174312,0.811009174,
0.812844037,0.814678899,0.816513761,0.818348624,0.820183486,0.822018349,
0.823853211,0.825688073,0.827522936,0.829357798,0.831192661,0.833027523,
0.834862385,0.836697248,0.83853211,0.840366972,0.842201835,0.844036697,
0.84587156,0.847706422,0.849541284,0.851376147,0.853211009,0.855045872,
0.856880734,0.858715596,0.860550459,0.862385321,0.864220183,0.866055046,
0.867889908,0.869724771,0.871559633,0.873394495,0.875229358,0.87706422,
0.878899083,0.880733945,0.882568807,0.88440367,0.886238532,0.888073394,
0.889908257,0.891743119,0.893577982,0.895412844,0.897247706,0.899082569,
0.900917431,0.902752294,0.904587156,0.906422018,0.908256881,0.910091743,
0.911926606,0.913761468,0.91559633,0.917431193,0.919266055,0.921100917,
0.92293578,0.924770642,0.926605505,0.928440367,0.930275229,0.932110092,
0.933944954,0.935779817,0.937614679,0.939449541,0.941284404,0.943119266,
0.944954128,0.946788991,0.948623853,0.950458716,0.952293578,0.95412844,
0.955963303,0.957798165,0.959633028,0.96146789,0.963302752,0.965137615,
0.966972477,0.968807339,0.970642202,0.972477064,0.974311927,0.976146789,
0.977981651,0.979816514,0.981651376,0.983486239,0.985321101,0.987155963,
0.988990826,0.990825688,0.99266055,0.994495413,0.996330275,0.998165138,
1.),(0.3,1.,1.3),.UNSPECIFIED.);
#6307=B_SPLINE_SURFACE_WITH_KNOTS('',5,1,((#307978,#307979,#307980),(#307981,
#307982,#307983),(#307984,#307985,#307986),(#307987,#307988,#307989),(#307990,
#307991,#307992),(#307993,#307994,#307995),(#307996,#307997,#307998),(#307999,
#308000,#308001),(#308002,#308003,#308004),(#308005,#308006,#308007),(#308008,
#308009,#308010),(#308011,#308012,#308013),(#308014,#308015,#308016),(#308017,
#308018,#308019),(#308020,#308021,#308022),(#308023,#308024,#308025),(#308026,
#308027,#308028),(#308029,#308030,#308031),(#308032,#308033,#308034),(#308035,
#308036,#308037),(#308038,#308039,#308040),(#308041,#308042,#308043),(#308044,
#308045,#308046),(#308047,#308048,#308049),(#308050,#308051,#308052),(#308053,
#308054,#308055),(#308056,#308057,#308058),(#308059,#308060,#308061),(#308062,
#308063,#308064),(#308065,#308066,#308067),(#308068,#308069,#308070),(#308071,
#308072,#308073),(#308074,#308075,#308076),(#308077,#308078,#308079),(#308080,
#308081,#308082),(#308083,#308084,#308085),(#308086,#308087,#308088),(#308089,
#308090,#308091),(#308092,#308093,#308094),(#308095,#308096,#308097),(#308098,
#308099,#308100),(#308101,#308102,#308103),(#308104,#308105,#308106),(#308107,
#308108,#308109),(#308110,#308111,#308112),(#308113,#308114,#308115),(#308116,
#308117,#308118),(#308119,#308120,#308121),(#308122,#308123,#308124),(#308125,
#308126,#308127),(#308128,#308129,#308130),(#308131,#308132,#308133),(#308134,
#308135,#308136),(#308137,#308138,#308139),(#308140,#308141,#308142),(#308143,
#308144,#308145),(#308146,#308147,#308148),(#308149,#308150,#308151),(#308152,
#308153,#308154),(#308155,#308156,#308157),(#308158,#308159,#308160),(#308161,
#308162,#308163),(#308164,#308165,#308166),(#308167,#308168,#308169),(#308170,
#308171,#308172),(#308173,#308174,#308175),(#308176,#308177,#308178),(#308179,
#308180,#308181),(#308182,#308183,#308184),(#308185,#308186,#308187),(#308188,
#308189,#308190),(#308191,#308192,#308193),(#308194,#308195,#308196),(#308197,
#308198,#308199),(#308200,#308201,#308202),(#308203,#308204,#308205),(#308206,
#308207,#308208),(#308209,#308210,#308211),(#308212,#308213,#308214),(#308215,
#308216,#308217),(#308218,#308219,#308220),(#308221,#308222,#308223),(#308224,
#308225,#308226),(#308227,#308228,#308229),(#308230,#308231,#308232),(#308233,
#308234,#308235),(#308236,#308237,#308238),(#308239,#308240,#308241),(#308242,
#308243,#308244),(#308245,#308246,#308247),(#308248,#308249,#308250),(#308251,
#308252,#308253),(#308254,#308255,#308256),(#308257,#308258,#308259),(#308260,
#308261,#308262),(#308263,#308264,#308265),(#308266,#308267,#308268),(#308269,
#308270,#308271),(#308272,#308273,#308274),(#308275,#308276,#308277),(#308278,
#308279,#308280),(#308281,#308282,#308283),(#308284,#308285,#308286),(#308287,
#308288,#308289),(#308290,#308291,#308292),(#308293,#308294,#308295),(#308296,
#308297,#308298),(#308299,#308300,#308301),(#308302,#308303,#308304),(#308305,
#308306,#308307),(#308308,#308309,#308310),(#308311,#308312,#308313),(#308314,
#308315,#308316),(#308317,#308318,#308319),(#308320,#308321,#308322),(#308323,
#308324,#308325),(#308326,#308327,#308328),(#308329,#308330,#308331),(#308332,
#308333,#308334),(#308335,#308336,#308337),(#308338,#308339,#308340),(#308341,
#308342,#308343),(#308344,#308345,#308346),(#308347,#308348,#308349),(#308350,
#308351,#308352),(#308353,#308354,#308355),(#308356,#308357,#308358),(#308359,
#308360,#308361),(#308362,#308363,#308364),(#308365,#308366,#308367),(#308368,
#308369,#308370),(#308371,#308372,#308373),(#308374,#308375,#308376),(#308377,
#308378,#308379),(#308380,#308381,#308382),(#308383,#308384,#308385),(#308386,
#308387,#308388),(#308389,#308390,#308391),(#308392,#308393,#308394),(#308395,
#308396,#308397),(#308398,#308399,#308400),(#308401,#308402,#308403),(#308404,
#308405,#308406),(#308407,#308408,#308409),(#308410,#308411,#308412),(#308413,
#308414,#308415),(#308416,#308417,#308418),(#308419,#308420,#308421),(#308422,
#308423,#308424),(#308425,#308426,#308427),(#308428,#308429,#308430),(#308431,
#308432,#308433),(#308434,#308435,#308436),(#308437,#308438,#308439),(#308440,
#308441,#308442),(#308443,#308444,#308445),(#308446,#308447,#308448),(#308449,
#308450,#308451),(#308452,#308453,#308454),(#308455,#308456,#308457),(#308458,
#308459,#308460),(#308461,#308462,#308463),(#308464,#308465,#308466),(#308467,
#308468,#308469),(#308470,#308471,#308472),(#308473,#308474,#308475),(#308476,
#308477,#308478),(#308479,#308480,#308481),(#308482,#308483,#308484),(#308485,
#308486,#308487),(#308488,#308489,#308490),(#308491,#308492,#308493),(#308494,
#308495,#308496),(#308497,#308498,#308499),(#308500,#308501,#308502),(#308503,
#308504,#308505),(#308506,#308507,#308508),(#308509,#308510,#308511),(#308512,
#308513,#308514),(#308515,#308516,#308517),(#308518,#308519,#308520),(#308521,
#308522,#308523),(#308524,#308525,#308526),(#308527,#308528,#308529),(#308530,
#308531,#308532),(#308533,#308534,#308535),(#308536,#308537,#308538),(#308539,
#308540,#308541),(#308542,#308543,#308544),(#308545,#308546,#308547),(#308548,
#308549,#308550),(#308551,#308552,#308553),(#308554,#308555,#308556),(#308557,
#308558,#308559),(#308560,#308561,#308562),(#308563,#308564,#308565),(#308566,
#308567,#308568),(#308569,#308570,#308571),(#308572,#308573,#308574),(#308575,
#308576,#308577),(#308578,#308579,#308580),(#308581,#308582,#308583),(#308584,
#308585,#308586),(#308587,#308588,#308589),(#308590,#308591,#308592),(#308593,
#308594,#308595),(#308596,#308597,#308598),(#308599,#308600,#308601),(#308602,
#308603,#308604),(#308605,#308606,#308607),(#308608,#308609,#308610),(#308611,
#308612,#308613),(#308614,#308615,#308616),(#308617,#308618,#308619),(#308620,
#308621,#308622),(#308623,#308624,#308625),(#308626,#308627,#308628),(#308629,
#308630,#308631),(#308632,#308633,#308634),(#308635,#308636,#308637),(#308638,
#308639,#308640),(#308641,#308642,#308643),(#308644,#308645,#308646),(#308647,
#308648,#308649),(#308650,#308651,#308652),(#308653,#308654,#308655),(#308656,
#308657,#308658),(#308659,#308660,#308661),(#308662,#308663,#308664),(#308665,
#308666,#308667),(#308668,#308669,#308670),(#308671,#308672,#308673),(#308674,
#308675,#308676),(#308677,#308678,#308679),(#308680,#308681,#308682),(#308683,
#308684,#308685),(#308686,#308687,#308688),(#308689,#308690,#308691),(#308692,
#308693,#308694),(#308695,#308696,#308697),(#308698,#308699,#308700),(#308701,
#308702,#308703),(#308704,#308705,#308706),(#308707,#308708,#308709),(#308710,
#308711,#308712),(#308713,#308714,#308715),(#308716,#308717,#308718),(#308719,
#308720,#308721),(#308722,#308723,#308724),(#308725,#308726,#308727),(#308728,
#308729,#308730),(#308731,#308732,#308733),(#308734,#308735,#308736),(#308737,
#308738,#308739),(#308740,#308741,#308742),(#308743,#308744,#308745),(#308746,
#308747,#308748),(#308749,#308750,#308751),(#308752,#308753,#308754),(#308755,
#308756,#308757),(#308758,#308759,#308760),(#308761,#308762,#308763),(#308764,
#308765,#308766),(#308767,#308768,#308769),(#308770,#308771,#308772),(#308773,
#308774,#308775),(#308776,#308777,#308778),(#308779,#308780,#308781),(#308782,
#308783,#308784),(#308785,#308786,#308787),(#308788,#308789,#308790),(#308791,
#308792,#308793),(#308794,#308795,#308796),(#308797,#308798,#308799),(#308800,
#308801,#308802),(#308803,#308804,#308805),(#308806,#308807,#308808),(#308809,
#308810,#308811),(#308812,#308813,#308814),(#308815,#308816,#308817),(#308818,
#308819,#308820),(#308821,#308822,#308823),(#308824,#308825,#308826),(#308827,
#308828,#308829),(#308830,#308831,#308832),(#308833,#308834,#308835),(#308836,
#308837,#308838),(#308839,#308840,#308841),(#308842,#308843,#308844),(#308845,
#308846,#308847),(#308848,#308849,#308850),(#308851,#308852,#308853),(#308854,
#308855,#308856),(#308857,#308858,#308859),(#308860,#308861,#308862),(#308863,
#308864,#308865),(#308866,#308867,#308868),(#308869,#308870,#308871),(#308872,
#308873,#308874),(#308875,#308876,#308877),(#308878,#308879,#308880),(#308881,
#308882,#308883),(#308884,#308885,#308886),(#308887,#308888,#308889),(#308890,
#308891,#308892),(#308893,#308894,#308895),(#308896,#308897,#308898),(#308899,
#308900,#308901),(#308902,#308903,#308904),(#308905,#308906,#308907),(#308908,
#308909,#308910),(#308911,#308912,#308913),(#308914,#308915,#308916),(#308917,
#308918,#308919),(#308920,#308921,#308922),(#308923,#308924,#308925),(#308926,
#308927,#308928),(#308929,#308930,#308931),(#308932,#308933,#308934),(#308935,
#308936,#308937),(#308938,#308939,#308940),(#308941,#308942,#308943),(#308944,
#308945,#308946),(#308947,#308948,#308949),(#308950,#308951,#308952),(#308953,
#308954,#308955),(#308956,#308957,#308958),(#308959,#308960,#308961),(#308962,
#308963,#308964),(#308965,#308966,#308967),(#308968,#308969,#308970),(#308971,
#308972,#308973),(#308974,#308975,#308976),(#308977,#308978,#308979),(#308980,
#308981,#308982),(#308983,#308984,#308985),(#308986,#308987,#308988),(#308989,
#308990,#308991),(#308992,#308993,#308994),(#308995,#308996,#308997),(#308998,
#308999,#309000),(#309001,#309002,#309003),(#309004,#309005,#309006),(#309007,
#309008,#309009),(#309010,#309011,#309012),(#309013,#309014,#309015),(#309016,
#309017,#309018),(#309019,#309020,#309021),(#309022,#309023,#309024),(#309025,
#309026,#309027),(#309028,#309029,#309030),(#309031,#309032,#309033),(#309034,
#309035,#309036),(#309037,#309038,#309039),(#309040,#309041,#309042),(#309043,
#309044,#309045),(#309046,#309047,#309048),(#309049,#309050,#309051),(#309052,
#309053,#309054),(#309055,#309056,#309057),(#309058,#309059,#309060),(#309061,
#309062,#309063),(#309064,#309065,#309066),(#309067,#309068,#309069),(#309070,
#309071,#309072),(#309073,#309074,#309075),(#309076,#309077,#309078),(#309079,
#309080,#309081),(#309082,#309083,#309084),(#309085,#309086,#309087),(#309088,
#309089,#309090),(#309091,#309092,#309093),(#309094,#309095,#309096),(#309097,
#309098,#309099),(#309100,#309101,#309102),(#309103,#309104,#309105),(#309106,
#309107,#309108),(#309109,#309110,#309111),(#309112,#309113,#309114),(#309115,
#309116,#309117),(#309118,#309119,#309120),(#309121,#309122,#309123),(#309124,
#309125,#309126),(#309127,#309128,#309129),(#309130,#309131,#309132),(#309133,
#309134,#309135),(#309136,#309137,#309138),(#309139,#309140,#309141),(#309142,
#309143,#309144),(#309145,#309146,#309147),(#309148,#309149,#309150),(#309151,
#309152,#309153),(#309154,#309155,#309156),(#309157,#309158,#309159),(#309160,
#309161,#309162),(#309163,#309164,#309165),(#309166,#309167,#309168),(#309169,
#309170,#309171),(#309172,#309173,#309174),(#309175,#309176,#309177),(#309178,
#309179,#309180),(#309181,#309182,#309183),(#309184,#309185,#309186),(#309187,
#309188,#309189),(#309190,#309191,#309192),(#309193,#309194,#309195),(#309196,
#309197,#309198),(#309199,#309200,#309201),(#309202,#309203,#309204),(#309205,
#309206,#309207),(#309208,#309209,#309210),(#309211,#309212,#309213),(#309214,
#309215,#309216),(#309217,#309218,#309219),(#309220,#309221,#309222),(#309223,
#309224,#309225),(#309226,#309227,#309228),(#309229,#309230,#309231),(#309232,
#309233,#309234),(#309235,#309236,#309237),(#309238,#309239,#309240),(#309241,
#309242,#309243),(#309244,#309245,#309246),(#309247,#309248,#309249),(#309250,
#309251,#309252),(#309253,#309254,#309255),(#309256,#309257,#309258),(#309259,
#309260,#309261),(#309262,#309263,#309264),(#309265,#309266,#309267),(#309268,
#309269,#309270),(#309271,#309272,#309273),(#309274,#309275,#309276),(#309277,
#309278,#309279),(#309280,#309281,#309282),(#309283,#309284,#309285),(#309286,
#309287,#309288),(#309289,#309290,#309291),(#309292,#309293,#309294),(#309295,
#309296,#309297),(#309298,#309299,#309300),(#309301,#309302,#309303),(#309304,
#309305,#309306),(#309307,#309308,#309309),(#309310,#309311,#309312),(#309313,
#309314,#309315),(#309316,#309317,#309318),(#309319,#309320,#309321),(#309322,
#309323,#309324),(#309325,#309326,#309327),(#309328,#309329,#309330),(#309331,
#309332,#309333),(#309334,#309335,#309336),(#309337,#309338,#309339),(#309340,
#309341,#309342),(#309343,#309344,#309345),(#309346,#309347,#309348),(#309349,
#309350,#309351),(#309352,#309353,#309354),(#309355,#309356,#309357),(#309358,
#309359,#309360),(#309361,#309362,#309363),(#309364,#309365,#309366),(#309367,
#309368,#309369),(#309370,#309371,#309372),(#309373,#309374,#309375),(#309376,
#309377,#309378),(#309379,#309380,#309381),(#309382,#309383,#309384),(#309385,
#309386,#309387),(#309388,#309389,#309390),(#309391,#309392,#309393),(#309394,
#309395,#309396),(#309397,#309398,#309399),(#309400,#309401,#309402),(#309403,
#309404,#309405),(#309406,#309407,#309408),(#309409,#309410,#309411),(#309412,
#309413,#309414),(#309415,#309416,#309417),(#309418,#309419,#309420),(#309421,
#309422,#309423),(#309424,#309425,#309426),(#309427,#309428,#309429),(#309430,
#309431,#309432),(#309433,#309434,#309435),(#309436,#309437,#309438),(#309439,
#309440,#309441),(#309442,#309443,#309444),(#309445,#309446,#309447),(#309448,
#309449,#309450),(#309451,#309452,#309453),(#309454,#309455,#309456),(#309457,
#309458,#309459),(#309460,#309461,#309462),(#309463,#309464,#309465),(#309466,
#309467,#309468),(#309469,#309470,#309471),(#309472,#309473,#309474),(#309475,
#309476,#309477),(#309478,#309479,#309480),(#309481,#309482,#309483),(#309484,
#309485,#309486),(#309487,#309488,#309489),(#309490,#309491,#309492),(#309493,
#309494,#309495),(#309496,#309497,#309498),(#309499,#309500,#309501),(#309502,
#309503,#309504),(#309505,#309506,#309507),(#309508,#309509,#309510),(#309511,
#309512,#309513),(#309514,#309515,#309516),(#309517,#309518,#309519),(#309520,
#309521,#309522),(#309523,#309524,#309525),(#309526,#309527,#309528),(#309529,
#309530,#309531),(#309532,#309533,#309534),(#309535,#309536,#309537),(#309538,
#309539,#309540),(#309541,#309542,#309543),(#309544,#309545,#309546),(#309547,
#309548,#309549),(#309550,#309551,#309552),(#309553,#309554,#309555),(#309556,
#309557,#309558),(#309559,#309560,#309561),(#309562,#309563,#309564),(#309565,
#309566,#309567),(#309568,#309569,#309570),(#309571,#309572,#309573),(#309574,
#309575,#309576),(#309577,#309578,#309579),(#309580,#309581,#309582),(#309583,
#309584,#309585),(#309586,#309587,#309588),(#309589,#309590,#309591),(#309592,
#309593,#309594),(#309595,#309596,#309597),(#309598,#309599,#309600),(#309601,
#309602,#309603),(#309604,#309605,#309606),(#309607,#309608,#309609),(#309610,
#309611,#309612),(#309613,#309614,#309615),(#309616,#309617,#309618),(#309619,
#309620,#309621),(#309622,#309623,#309624),(#309625,#309626,#309627)),
 .UNSPECIFIED.,.F.,.F.,.F.,(6,1,1,1,1,1,1,1,1,1,1,1,1,1,1,1,1,1,1,1,1,1,
1,1,1,1,1,1,1,1,1,1,1,1,1,1,1,1,1,1,1,1,1,1,1,1,1,1,1,1,1,1,1,1,1,1,1,1,
1,1,1,1,1,1,1,1,1,1,1,1,1,1,1,1,1,1,1,1,1,1,1,1,1,1,1,1,1,1,1,1,1,1,1,1,
1,1,1,1,1,1,1,1,1,1,1,1,1,1,1,1,1,1,1,1,1,1,1,1,1,1,1,1,1,1,1,1,1,1,1,1,
1,1,1,1,1,1,1,1,1,1,1,1,1,1,1,1,1,1,1,1,1,1,1,1,1,1,1,1,1,1,1,1,1,1,1,1,
1,1,1,1,1,1,1,1,1,1,1,1,1,1,1,1,1,1,1,1,1,1,1,1,1,1,1,1,1,1,1,1,1,1,1,1,
1,1,1,1,1,1,1,1,1,1,1,1,1,1,1,1,1,1,1,1,1,1,1,1,1,1,1,1,1,1,1,1,1,1,1,1,
1,1,1,1,1,1,1,1,1,1,1,1,1,1,1,1,1,1,1,1,1,1,1,1,1,1,1,1,1,1,1,1,1,1,1,1,
1,1,1,1,1,1,1,1,1,1,1,1,1,1,1,1,1,1,1,1,1,1,1,1,1,1,1,1,1,1,1,1,1,1,1,1,
1,1,1,1,1,1,1,1,1,1,1,1,1,1,1,1,1,1,1,1,1,1,1,1,1,1,1,1,1,1,1,1,1,1,1,1,
1,1,1,1,1,1,1,1,1,1,1,1,1,1,1,1,1,1,1,1,1,1,1,1,1,1,1,1,1,1,1,1,1,1,1,1,
1,1,1,1,1,1,1,1,1,1,1,1,1,1,1,1,1,1,1,1,1,1,1,1,1,1,1,1,1,1,1,1,1,1,1,1,
1,1,1,1,1,1,1,1,1,1,1,1,1,1,1,1,1,1,1,1,1,1,1,1,1,1,1,1,1,1,1,1,1,1,1,1,
1,1,1,1,1,1,1,1,1,1,1,1,1,1,1,1,1,1,1,1,1,1,1,1,1,1,1,1,1,1,1,1,1,1,1,1,
1,1,1,1,1,1,1,1,1,1,1,1,1,1,1,1,1,1,1,1,1,1,1,1,1,1,1,1,1,1,1,1,1,1,1,1,
1,1,1,1,1,1,1,1,1,1,1,1,1,1,1,1,1,1,1,6),(2,1,2),(-1.,-0.998165138,-0.996330275,
-0.994495413,-0.99266055,-0.990825688,-0.988990826,-0.987155963,-0.985321101,
-0.983486239,-0.981651376,-0.979816514,-0.977981651,-0.976146789,-0.974311927,
-0.972477064,-0.970642202,-0.968807339,-0.966972477,-0.965137615,-0.963302752,
-0.96146789,-0.959633028,-0.957798165,-0.955963303,-0.95412844,-0.952293578,
-0.950458716,-0.948623853,-0.946788991,-0.944954128,-0.943119266,-0.941284404,
-0.939449541,-0.937614679,-0.935779817,-0.933944954,-0.932110092,-0.930275229,
-0.928440367,-0.926605505,-0.924770642,-0.92293578,-0.921100917,-0.919266055,
-0.917431193,-0.91559633,-0.913761468,-0.911926606,-0.910091743,-0.908256881,
-0.906422018,-0.904587156,-0.902752294,-0.900917431,-0.899082569,-0.897247706,
-0.895412844,-0.893577982,-0.891743119,-0.889908257,-0.888073394,-0.886238532,
-0.88440367,-0.882568807,-0.880733945,-0.878899083,-0.87706422,-0.875229358,
-0.873394495,-0.871559633,-0.869724771,-0.867889908,-0.866055046,-0.864220183,
-0.862385321,-0.860550459,-0.858715596,-0.856880734,-0.855045872,-0.853211009,
-0.851376147,-0.849541284,-0.847706422,-0.84587156,-0.844036697,-0.842201835,
-0.840366972,-0.83853211,-0.836697248,-0.834862385,-0.833027523,-0.831192661,
-0.829357798,-0.827522936,-0.825688073,-0.823853211,-0.822018349,-0.820183486,
-0.818348624,-0.816513761,-0.814678899,-0.812844037,-0.811009174,-0.809174312,
-0.80733945,-0.805504587,-0.803669725,-0.801834862,-0.8,-0.798165138,-0.796330275,
-0.794495413,-0.79266055,-0.790825688,-0.788990826,-0.787155963,-0.785321101,
-0.783486239,-0.781651376,-0.779816514,-0.777981651,-0.776146789,-0.774311927,
-0.772477064,-0.770642202,-0.768807339,-0.766972477,-0.765137615,-0.763302752,
-0.76146789,-0.759633028,-0.757798165,-0.755963303,-0.75412844,-0.752293578,
-0.750458716,-0.748623853,-0.746788991,-0.744954128,-0.743119266,-0.741284404,
-0.739449541,-0.737614679,-0.735779817,-0.733944954,-0.732110092,-0.730275229,
-0.728440367,-0.726605505,-0.724770642,-0.72293578,-0.721100917,-0.719266055,
-0.717431193,-0.71559633,-0.713761468,-0.711926606,-0.710091743,-0.708256881,
-0.706422018,-0.704587156,-0.702752294,-0.700917431,-0.699082569,-0.697247706,
-0.695412844,-0.693577982,-0.691743119,-0.689908257,-0.688073394,-0.686238532,
-0.68440367,-0.682568807,-0.680733945,-0.678899083,-0.67706422,-0.675229358,
-0.673394495,-0.671559633,-0.669724771,-0.667889908,-0.666055046,-0.664220183,
-0.662385321,-0.660550459,-0.658715596,-0.656880734,-0.655045872,-0.653211009,
-0.651376147,-0.649541284,-0.647706422,-0.64587156,-0.644036697,-0.642201835,
-0.640366972,-0.63853211,-0.636697248,-0.634862385,-0.633027523,-0.631192661,
-0.629357798,-0.627522936,-0.625688073,-0.623853211,-0.622018349,-0.620183486,
-0.618348624,-0.616513761,-0.614678899,-0.612844037,-0.611009174,-0.609174312,
-0.60733945,-0.605504587,-0.603669725,-0.601834862,-0.6,-0.598165138,-0.596330275,
-0.594495413,-0.59266055,-0.590825688,-0.588990826,-0.587155963,-0.585321101,
-0.583486239,-0.581651376,-0.579816514,-0.577981651,-0.576146789,-0.574311927,
-0.572477064,-0.570642202,-0.568807339,-0.566972477,-0.565137615,-0.563302752,
-0.56146789,-0.559633028,-0.557798165,-0.555963303,-0.55412844,-0.552293578,
-0.550458716,-0.548623853,-0.546788991,-0.544954128,-0.543119266,-0.541284404,
-0.539449541,-0.537614679,-0.535779817,-0.533944954,-0.532110092,-0.530275229,
-0.528440367,-0.526605505,-0.524770642,-0.52293578,-0.521100917,-0.519266055,
-0.517431193,-0.51559633,-0.513761468,-0.511926606,-0.510091743,-0.508256881,
-0.506422018,-0.504587156,-0.502752294,-0.500917431,-0.499082569,-0.497247706,
-0.495412844,-0.493577982,-0.491743119,-0.489908257,-0.488073394,-0.486238532,
-0.48440367,-0.482568807,-0.480733945,-0.478899083,-0.47706422,-0.475229358,
-0.473394495,-0.471559633,-0.469724771,-0.467889908,-0.466055046,-0.464220183,
-0.462385321,-0.460550459,-0.458715596,-0.456880734,-0.455045872,-0.453211009,
-0.451376147,-0.449541284,-0.447706422,-0.44587156,-0.444036697,-0.442201835,
-0.440366972,-0.43853211,-0.436697248,-0.434862385,-0.433027523,-0.431192661,
-0.429357798,-0.427522936,-0.425688073,-0.423853211,-0.422018349,-0.420183486,
-0.418348624,-0.416513761,-0.414678899,-0.412844037,-0.411009174,-0.409174312,
-0.40733945,-0.405504587,-0.403669725,-0.401834862,-0.4,-0.398165138,-0.396330275,
-0.394495413,-0.39266055,-0.390825688,-0.388990826,-0.387155963,-0.385321101,
-0.383486239,-0.381651376,-0.379816514,-0.377981651,-0.376146789,-0.374311927,
-0.372477064,-0.370642202,-0.368807339,-0.366972477,-0.365137615,-0.363302752,
-0.36146789,-0.359633028,-0.357798165,-0.355963303,-0.35412844,-0.352293578,
-0.350458716,-0.348623853,-0.346788991,-0.344954128,-0.343119266,-0.341284404,
-0.339449541,-0.337614679,-0.335779817,-0.333944954,-0.332110092,-0.330275229,
-0.328440367,-0.326605505,-0.324770642,-0.32293578,-0.321100917,-0.319266055,
-0.317431193,-0.31559633,-0.313761468,-0.311926606,-0.310091743,-0.308256881,
-0.306422018,-0.304587156,-0.302752294,-0.300917431,-0.299082569,-0.297247706,
-0.295412844,-0.293577982,-0.291743119,-0.289908257,-0.288073394,-0.286238532,
-0.28440367,-0.282568807,-0.280733945,-0.278899083,-0.27706422,-0.275229358,
-0.273394495,-0.271559633,-0.269724771,-0.267889908,-0.266055046,-0.264220183,
-0.262385321,-0.260550459,-0.258715596,-0.256880734,-0.255045872,-0.253211009,
-0.251376147,-0.249541284,-0.247706422,-0.24587156,-0.244036697,-0.242201835,
-0.240366972,-0.23853211,-0.236697248,-0.234862385,-0.233027523,-0.231192661,
-0.229357798,-0.227522936,-0.225688073,-0.223853211,-0.222018349,-0.220183486,
-0.218348624,-0.216513761,-0.214678899,-0.212844037,-0.211009174,-0.209174312,
-0.20733945,-0.205504587,-0.203669725,-0.201834862,-0.2,-0.198165138,-0.196330275,
-0.194495413,-0.19266055,-0.190825688,-0.188990826,-0.187155963,-0.185321101,
-0.183486239,-0.181651376,-0.179816514,-0.177981651,-0.176146789,-0.174311927,
-0.172477064,-0.170642202,-0.168807339,-0.166972477,-0.165137615,-0.163302752,
-0.16146789,-0.159633028,-0.157798165,-0.155963303,-0.15412844,-0.152293578,
-0.150458716,-0.148623853,-0.146788991,-0.144954128,-0.143119266,-0.141284404,
-0.139449541,-0.137614679,-0.135779817,-0.133944954,-0.132110092,-0.130275229,
-0.128440367,-0.126605505,-0.124770642,-0.12293578,-0.121100917,-0.119266055,
-0.117431193,-0.11559633,-0.113761468,-0.111926606,-0.110091743,-0.108256881,
-0.106422018,-0.104587156,-0.102752294,-0.100917431,-0.099082569,-0.097247706,
-0.095412844,-0.093577982,-0.091743119,-0.089908257,-0.088073394,-0.086238532,
-0.08440367,-0.082568807,-0.080733945,-0.078899083,-0.07706422,-0.075229358,
-0.073394495,-0.071559633,-0.069724771,-0.067889908,-0.066055046,-0.064220183,
-0.062385321,-0.060550459,-0.058715596,-0.056880734,-0.055045872,-0.053211009,
-0.051376147,-0.049541284,-0.047706422,-0.04587156,-0.044036697,-0.042201835,
-0.040366972,-0.03853211,-0.036697248,-0.034862385,-0.033027523,-0.031192661,
-0.029357798,-0.027522936,-0.025688073,-0.023853211,-0.022018349,-0.020183486,
-0.018348624,-0.016513761,-0.014678899,-0.012844037,-0.011009174,-0.009174312,
-0.00733945,-0.005504587,-0.003669725,-0.001834862,0.000982108),(0.3,1.,
1.3),.UNSPECIFIED.);
#6308=B_SPLINE_SURFACE_WITH_KNOTS('',5,1,((#309650,#309651,#309652),(#309653,
#309654,#309655),(#309656,#309657,#309658),(#309659,#309660,#309661),(#309662,
#309663,#309664),(#309665,#309666,#309667),(#309668,#309669,#309670),(#309671,
#309672,#309673),(#309674,#309675,#309676),(#309677,#309678,#309679),(#309680,
#309681,#309682),(#309683,#309684,#309685),(#309686,#309687,#309688),(#309689,
#309690,#309691),(#309692,#309693,#309694),(#309695,#309696,#309697),(#309698,
#309699,#309700),(#309701,#309702,#309703),(#309704,#309705,#309706),(#309707,
#309708,#309709),(#309710,#309711,#309712),(#309713,#309714,#309715),(#309716,
#309717,#309718),(#309719,#309720,#309721),(#309722,#309723,#309724),(#309725,
#309726,#309727),(#309728,#309729,#309730),(#309731,#309732,#309733),(#309734,
#309735,#309736),(#309737,#309738,#309739),(#309740,#309741,#309742),(#309743,
#309744,#309745),(#309746,#309747,#309748),(#309749,#309750,#309751),(#309752,
#309753,#309754),(#309755,#309756,#309757),(#309758,#309759,#309760),(#309761,
#309762,#309763),(#309764,#309765,#309766),(#309767,#309768,#309769),(#309770,
#309771,#309772),(#309773,#309774,#309775),(#309776,#309777,#309778),(#309779,
#309780,#309781),(#309782,#309783,#309784),(#309785,#309786,#309787),(#309788,
#309789,#309790),(#309791,#309792,#309793),(#309794,#309795,#309796),(#309797,
#309798,#309799),(#309800,#309801,#309802),(#309803,#309804,#309805),(#309806,
#309807,#309808),(#309809,#309810,#309811),(#309812,#309813,#309814),(#309815,
#309816,#309817),(#309818,#309819,#309820),(#309821,#309822,#309823),(#309824,
#309825,#309826),(#309827,#309828,#309829),(#309830,#309831,#309832),(#309833,
#309834,#309835),(#309836,#309837,#309838),(#309839,#309840,#309841),(#309842,
#309843,#309844),(#309845,#309846,#309847),(#309848,#309849,#309850),(#309851,
#309852,#309853),(#309854,#309855,#309856),(#309857,#309858,#309859),(#309860,
#309861,#309862),(#309863,#309864,#309865),(#309866,#309867,#309868),(#309869,
#309870,#309871),(#309872,#309873,#309874),(#309875,#309876,#309877),(#309878,
#309879,#309880),(#309881,#309882,#309883),(#309884,#309885,#309886),(#309887,
#309888,#309889),(#309890,#309891,#309892),(#309893,#309894,#309895),(#309896,
#309897,#309898),(#309899,#309900,#309901),(#309902,#309903,#309904),(#309905,
#309906,#309907),(#309908,#309909,#309910),(#309911,#309912,#309913),(#309914,
#309915,#309916),(#309917,#309918,#309919),(#309920,#309921,#309922),(#309923,
#309924,#309925),(#309926,#309927,#309928),(#309929,#309930,#309931),(#309932,
#309933,#309934),(#309935,#309936,#309937),(#309938,#309939,#309940),(#309941,
#309942,#309943),(#309944,#309945,#309946),(#309947,#309948,#309949),(#309950,
#309951,#309952),(#309953,#309954,#309955),(#309956,#309957,#309958),(#309959,
#309960,#309961),(#309962,#309963,#309964),(#309965,#309966,#309967),(#309968,
#309969,#309970),(#309971,#309972,#309973),(#309974,#309975,#309976),(#309977,
#309978,#309979),(#309980,#309981,#309982),(#309983,#309984,#309985),(#309986,
#309987,#309988),(#309989,#309990,#309991),(#309992,#309993,#309994),(#309995,
#309996,#309997),(#309998,#309999,#310000),(#310001,#310002,#310003),(#310004,
#310005,#310006),(#310007,#310008,#310009),(#310010,#310011,#310012),(#310013,
#310014,#310015),(#310016,#310017,#310018),(#310019,#310020,#310021),(#310022,
#310023,#310024),(#310025,#310026,#310027),(#310028,#310029,#310030),(#310031,
#310032,#310033),(#310034,#310035,#310036),(#310037,#310038,#310039),(#310040,
#310041,#310042),(#310043,#310044,#310045),(#310046,#310047,#310048),(#310049,
#310050,#310051),(#310052,#310053,#310054),(#310055,#310056,#310057),(#310058,
#310059,#310060),(#310061,#310062,#310063),(#310064,#310065,#310066),(#310067,
#310068,#310069),(#310070,#310071,#310072),(#310073,#310074,#310075),(#310076,
#310077,#310078),(#310079,#310080,#310081),(#310082,#310083,#310084),(#310085,
#310086,#310087),(#310088,#310089,#310090),(#310091,#310092,#310093),(#310094,
#310095,#310096),(#310097,#310098,#310099),(#310100,#310101,#310102),(#310103,
#310104,#310105),(#310106,#310107,#310108),(#310109,#310110,#310111),(#310112,
#310113,#310114),(#310115,#310116,#310117),(#310118,#310119,#310120),(#310121,
#310122,#310123),(#310124,#310125,#310126),(#310127,#310128,#310129),(#310130,
#310131,#310132),(#310133,#310134,#310135),(#310136,#310137,#310138),(#310139,
#310140,#310141),(#310142,#310143,#310144),(#310145,#310146,#310147),(#310148,
#310149,#310150),(#310151,#310152,#310153),(#310154,#310155,#310156),(#310157,
#310158,#310159),(#310160,#310161,#310162),(#310163,#310164,#310165),(#310166,
#310167,#310168),(#310169,#310170,#310171),(#310172,#310173,#310174),(#310175,
#310176,#310177),(#310178,#310179,#310180),(#310181,#310182,#310183),(#310184,
#310185,#310186),(#310187,#310188,#310189),(#310190,#310191,#310192),(#310193,
#310194,#310195),(#310196,#310197,#310198),(#310199,#310200,#310201),(#310202,
#310203,#310204),(#310205,#310206,#310207),(#310208,#310209,#310210),(#310211,
#310212,#310213),(#310214,#310215,#310216),(#310217,#310218,#310219),(#310220,
#310221,#310222),(#310223,#310224,#310225),(#310226,#310227,#310228),(#310229,
#310230,#310231),(#310232,#310233,#310234),(#310235,#310236,#310237),(#310238,
#310239,#310240),(#310241,#310242,#310243),(#310244,#310245,#310246),(#310247,
#310248,#310249),(#310250,#310251,#310252),(#310253,#310254,#310255),(#310256,
#310257,#310258),(#310259,#310260,#310261),(#310262,#310263,#310264),(#310265,
#310266,#310267),(#310268,#310269,#310270),(#310271,#310272,#310273),(#310274,
#310275,#310276),(#310277,#310278,#310279),(#310280,#310281,#310282),(#310283,
#310284,#310285),(#310286,#310287,#310288),(#310289,#310290,#310291),(#310292,
#310293,#310294),(#310295,#310296,#310297),(#310298,#310299,#310300),(#310301,
#310302,#310303),(#310304,#310305,#310306),(#310307,#310308,#310309),(#310310,
#310311,#310312),(#310313,#310314,#310315),(#310316,#310317,#310318),(#310319,
#310320,#310321),(#310322,#310323,#310324),(#310325,#310326,#310327),(#310328,
#310329,#310330),(#310331,#310332,#310333),(#310334,#310335,#310336),(#310337,
#310338,#310339),(#310340,#310341,#310342),(#310343,#310344,#310345),(#310346,
#310347,#310348),(#310349,#310350,#310351),(#310352,#310353,#310354),(#310355,
#310356,#310357),(#310358,#310359,#310360),(#310361,#310362,#310363),(#310364,
#310365,#310366),(#310367,#310368,#310369),(#310370,#310371,#310372),(#310373,
#310374,#310375),(#310376,#310377,#310378),(#310379,#310380,#310381),(#310382,
#310383,#310384),(#310385,#310386,#310387),(#310388,#310389,#310390),(#310391,
#310392,#310393),(#310394,#310395,#310396),(#310397,#310398,#310399),(#310400,
#310401,#310402),(#310403,#310404,#310405),(#310406,#310407,#310408),(#310409,
#310410,#310411),(#310412,#310413,#310414),(#310415,#310416,#310417),(#310418,
#310419,#310420),(#310421,#310422,#310423),(#310424,#310425,#310426),(#310427,
#310428,#310429),(#310430,#310431,#310432),(#310433,#310434,#310435),(#310436,
#310437,#310438),(#310439,#310440,#310441),(#310442,#310443,#310444),(#310445,
#310446,#310447),(#310448,#310449,#310450),(#310451,#310452,#310453),(#310454,
#310455,#310456),(#310457,#310458,#310459),(#310460,#310461,#310462),(#310463,
#310464,#310465),(#310466,#310467,#310468),(#310469,#310470,#310471),(#310472,
#310473,#310474),(#310475,#310476,#310477),(#310478,#310479,#310480),(#310481,
#310482,#310483),(#310484,#310485,#310486),(#310487,#310488,#310489),(#310490,
#310491,#310492),(#310493,#310494,#310495),(#310496,#310497,#310498),(#310499,
#310500,#310501),(#310502,#310503,#310504),(#310505,#310506,#310507),(#310508,
#310509,#310510),(#310511,#310512,#310513),(#310514,#310515,#310516),(#310517,
#310518,#310519),(#310520,#310521,#310522),(#310523,#310524,#310525),(#310526,
#310527,#310528),(#310529,#310530,#310531),(#310532,#310533,#310534),(#310535,
#310536,#310537),(#310538,#310539,#310540),(#310541,#310542,#310543),(#310544,
#310545,#310546),(#310547,#310548,#310549),(#310550,#310551,#310552),(#310553,
#310554,#310555),(#310556,#310557,#310558),(#310559,#310560,#310561),(#310562,
#310563,#310564),(#310565,#310566,#310567),(#310568,#310569,#310570),(#310571,
#310572,#310573),(#310574,#310575,#310576),(#310577,#310578,#310579),(#310580,
#310581,#310582),(#310583,#310584,#310585),(#310586,#310587,#310588),(#310589,
#310590,#310591),(#310592,#310593,#310594),(#310595,#310596,#310597),(#310598,
#310599,#310600),(#310601,#310602,#310603),(#310604,#310605,#310606),(#310607,
#310608,#310609),(#310610,#310611,#310612),(#310613,#310614,#310615),(#310616,
#310617,#310618),(#310619,#310620,#310621),(#310622,#310623,#310624),(#310625,
#310626,#310627),(#310628,#310629,#310630),(#310631,#310632,#310633),(#310634,
#310635,#310636),(#310637,#310638,#310639),(#310640,#310641,#310642),(#310643,
#310644,#310645),(#310646,#310647,#310648),(#310649,#310650,#310651),(#310652,
#310653,#310654),(#310655,#310656,#310657),(#310658,#310659,#310660),(#310661,
#310662,#310663),(#310664,#310665,#310666),(#310667,#310668,#310669),(#310670,
#310671,#310672),(#310673,#310674,#310675),(#310676,#310677,#310678),(#310679,
#310680,#310681),(#310682,#310683,#310684),(#310685,#310686,#310687),(#310688,
#310689,#310690),(#310691,#310692,#310693),(#310694,#310695,#310696),(#310697,
#310698,#310699),(#310700,#310701,#310702),(#310703,#310704,#310705),(#310706,
#310707,#310708),(#310709,#310710,#310711),(#310712,#310713,#310714),(#310715,
#310716,#310717),(#310718,#310719,#310720),(#310721,#310722,#310723),(#310724,
#310725,#310726),(#310727,#310728,#310729),(#310730,#310731,#310732),(#310733,
#310734,#310735),(#310736,#310737,#310738),(#310739,#310740,#310741),(#310742,
#310743,#310744),(#310745,#310746,#310747),(#310748,#310749,#310750),(#310751,
#310752,#310753),(#310754,#310755,#310756),(#310757,#310758,#310759),(#310760,
#310761,#310762),(#310763,#310764,#310765),(#310766,#310767,#310768),(#310769,
#310770,#310771),(#310772,#310773,#310774),(#310775,#310776,#310777),(#310778,
#310779,#310780),(#310781,#310782,#310783),(#310784,#310785,#310786),(#310787,
#310788,#310789),(#310790,#310791,#310792),(#310793,#310794,#310795),(#310796,
#310797,#310798),(#310799,#310800,#310801),(#310802,#310803,#310804),(#310805,
#310806,#310807),(#310808,#310809,#310810),(#310811,#310812,#310813),(#310814,
#310815,#310816),(#310817,#310818,#310819),(#310820,#310821,#310822),(#310823,
#310824,#310825),(#310826,#310827,#310828),(#310829,#310830,#310831),(#310832,
#310833,#310834),(#310835,#310836,#310837),(#310838,#310839,#310840),(#310841,
#310842,#310843),(#310844,#310845,#310846),(#310847,#310848,#310849),(#310850,
#310851,#310852),(#310853,#310854,#310855),(#310856,#310857,#310858),(#310859,
#310860,#310861),(#310862,#310863,#310864),(#310865,#310866,#310867),(#310868,
#310869,#310870),(#310871,#310872,#310873),(#310874,#310875,#310876),(#310877,
#310878,#310879),(#310880,#310881,#310882),(#310883,#310884,#310885),(#310886,
#310887,#310888),(#310889,#310890,#310891),(#310892,#310893,#310894),(#310895,
#310896,#310897),(#310898,#310899,#310900),(#310901,#310902,#310903),(#310904,
#310905,#310906),(#310907,#310908,#310909),(#310910,#310911,#310912),(#310913,
#310914,#310915),(#310916,#310917,#310918),(#310919,#310920,#310921),(#310922,
#310923,#310924),(#310925,#310926,#310927),(#310928,#310929,#310930),(#310931,
#310932,#310933),(#310934,#310935,#310936),(#310937,#310938,#310939),(#310940,
#310941,#310942),(#310943,#310944,#310945),(#310946,#310947,#310948),(#310949,
#310950,#310951),(#310952,#310953,#310954),(#310955,#310956,#310957),(#310958,
#310959,#310960),(#310961,#310962,#310963),(#310964,#310965,#310966),(#310967,
#310968,#310969),(#310970,#310971,#310972),(#310973,#310974,#310975),(#310976,
#310977,#310978),(#310979,#310980,#310981),(#310982,#310983,#310984),(#310985,
#310986,#310987),(#310988,#310989,#310990),(#310991,#310992,#310993),(#310994,
#310995,#310996),(#310997,#310998,#310999),(#311000,#311001,#311002),(#311003,
#311004,#311005),(#311006,#311007,#311008),(#311009,#311010,#311011),(#311012,
#311013,#311014),(#311015,#311016,#311017),(#311018,#311019,#311020),(#311021,
#311022,#311023),(#311024,#311025,#311026),(#311027,#311028,#311029),(#311030,
#311031,#311032),(#311033,#311034,#311035),(#311036,#311037,#311038),(#311039,
#311040,#311041),(#311042,#311043,#311044),(#311045,#311046,#311047),(#311048,
#311049,#311050),(#311051,#311052,#311053),(#311054,#311055,#311056),(#311057,
#311058,#311059),(#311060,#311061,#311062),(#311063,#311064,#311065),(#311066,
#311067,#311068),(#311069,#311070,#311071),(#311072,#311073,#311074),(#311075,
#311076,#311077),(#311078,#311079,#311080),(#311081,#311082,#311083),(#311084,
#311085,#311086),(#311087,#311088,#311089),(#311090,#311091,#311092),(#311093,
#311094,#311095),(#311096,#311097,#311098),(#311099,#311100,#311101),(#311102,
#311103,#311104),(#311105,#311106,#311107),(#311108,#311109,#311110),(#311111,
#311112,#311113),(#311114,#311115,#311116),(#311117,#311118,#311119),(#311120,
#311121,#311122),(#311123,#311124,#311125),(#311126,#311127,#311128),(#311129,
#311130,#311131),(#311132,#311133,#311134),(#311135,#311136,#311137),(#311138,
#311139,#311140),(#311141,#311142,#311143),(#311144,#311145,#311146),(#311147,
#311148,#311149),(#311150,#311151,#311152),(#311153,#311154,#311155),(#311156,
#311157,#311158),(#311159,#311160,#311161),(#311162,#311163,#311164),(#311165,
#311166,#311167),(#311168,#311169,#311170),(#311171,#311172,#311173),(#311174,
#311175,#311176),(#311177,#311178,#311179),(#311180,#311181,#311182),(#311183,
#311184,#311185),(#311186,#311187,#311188),(#311189,#311190,#311191),(#311192,
#311193,#311194),(#311195,#311196,#311197),(#311198,#311199,#311200),(#311201,
#311202,#311203),(#311204,#311205,#311206),(#311207,#311208,#311209),(#311210,
#311211,#311212),(#311213,#311214,#311215),(#311216,#311217,#311218),(#311219,
#311220,#311221),(#311222,#311223,#311224),(#311225,#311226,#311227),(#311228,
#311229,#311230),(#311231,#311232,#311233),(#311234,#311235,#311236),(#311237,
#311238,#311239),(#311240,#311241,#311242),(#311243,#311244,#311245),(#311246,
#311247,#311248),(#311249,#311250,#311251),(#311252,#311253,#311254),(#311255,
#311256,#311257),(#311258,#311259,#311260),(#311261,#311262,#311263),(#311264,
#311265,#311266),(#311267,#311268,#311269),(#311270,#311271,#311272),(#311273,
#311274,#311275),(#311276,#311277,#311278),(#311279,#311280,#311281),(#311282,
#311283,#311284),(#311285,#311286,#311287),(#311288,#311289,#311290),(#311291,
#311292,#311293),(#311294,#311295,#311296),(#311297,#311298,#311299)),
 .UNSPECIFIED.,.F.,.F.,.F.,(6,1,1,1,1,1,1,1,1,1,1,1,1,1,1,1,1,1,1,1,1,1,
1,1,1,1,1,1,1,1,1,1,1,1,1,1,1,1,1,1,1,1,1,1,1,1,1,1,1,1,1,1,1,1,1,1,1,1,
1,1,1,1,1,1,1,1,1,1,1,1,1,1,1,1,1,1,1,1,1,1,1,1,1,1,1,1,1,1,1,1,1,1,1,1,
1,1,1,1,1,1,1,1,1,1,1,1,1,1,1,1,1,1,1,1,1,1,1,1,1,1,1,1,1,1,1,1,1,1,1,1,
1,1,1,1,1,1,1,1,1,1,1,1,1,1,1,1,1,1,1,1,1,1,1,1,1,1,1,1,1,1,1,1,1,1,1,1,
1,1,1,1,1,1,1,1,1,1,1,1,1,1,1,1,1,1,1,1,1,1,1,1,1,1,1,1,1,1,1,1,1,1,1,1,
1,1,1,1,1,1,1,1,1,1,1,1,1,1,1,1,1,1,1,1,1,1,1,1,1,1,1,1,1,1,1,1,1,1,1,1,
1,1,1,1,1,1,1,1,1,1,1,1,1,1,1,1,1,1,1,1,1,1,1,1,1,1,1,1,1,1,1,1,1,1,1,1,
1,1,1,1,1,1,1,1,1,1,1,1,1,1,1,1,1,1,1,1,1,1,1,1,1,1,1,1,1,1,1,1,1,1,1,1,
1,1,1,1,1,1,1,1,1,1,1,1,1,1,1,1,1,1,1,1,1,1,1,1,1,1,1,1,1,1,1,1,1,1,1,1,
1,1,1,1,1,1,1,1,1,1,1,1,1,1,1,1,1,1,1,1,1,1,1,1,1,1,1,1,1,1,1,1,1,1,1,1,
1,1,1,1,1,1,1,1,1,1,1,1,1,1,1,1,1,1,1,1,1,1,1,1,1,1,1,1,1,1,1,1,1,1,1,1,
1,1,1,1,1,1,1,1,1,1,1,1,1,1,1,1,1,1,1,1,1,1,1,1,1,1,1,1,1,1,1,1,1,1,1,1,
1,1,1,1,1,1,1,1,1,1,1,1,1,1,1,1,1,1,1,1,1,1,1,1,1,1,1,1,1,1,1,1,1,1,1,1,
1,1,1,1,1,1,1,1,1,1,1,1,1,1,1,1,1,1,1,1,1,1,1,1,1,1,1,1,1,1,1,1,1,1,1,1,
1,1,1,1,1,1,1,1,1,1,1,1,1,1,1,1,1,1,1,6),(2,1,2),(0.,0.001834862,0.003669725,
0.005504587,0.00733945,0.009174312,0.011009174,0.012844037,0.014678899,
0.016513761,0.018348624,0.020183486,0.022018349,0.023853211,0.025688073,
0.027522936,0.029357798,0.031192661,0.033027523,0.034862385,0.036697248,
0.03853211,0.040366972,0.042201835,0.044036697,0.04587156,0.047706422,0.049541284,
0.051376147,0.053211009,0.055045872,0.056880734,0.058715596,0.060550459,
0.062385321,0.064220183,0.066055046,0.067889908,0.069724771,0.071559633,
0.073394495,0.075229358,0.07706422,0.078899083,0.080733945,0.082568807,
0.08440367,0.086238532,0.088073394,0.089908257,0.091743119,0.093577982,
0.095412844,0.097247706,0.099082569,0.100917431,0.102752294,0.104587156,
0.106422018,0.108256881,0.110091743,0.111926606,0.113761468,0.11559633,
0.117431193,0.119266055,0.121100917,0.12293578,0.124770642,0.126605505,
0.128440367,0.130275229,0.132110092,0.133944954,0.135779817,0.137614679,
0.139449541,0.141284404,0.143119266,0.144954128,0.146788991,0.148623853,
0.150458716,0.152293578,0.15412844,0.155963303,0.157798165,0.159633028,
0.16146789,0.163302752,0.165137615,0.166972477,0.168807339,0.170642202,
0.172477064,0.174311927,0.176146789,0.177981651,0.179816514,0.181651376,
0.183486239,0.185321101,0.187155963,0.188990826,0.190825688,0.19266055,
0.194495413,0.196330275,0.198165138,0.2,0.201834862,0.203669725,0.205504587,
0.20733945,0.209174312,0.211009174,0.212844037,0.214678899,0.216513761,
0.218348624,0.220183486,0.222018349,0.223853211,0.225688073,0.227522936,
0.229357798,0.231192661,0.233027523,0.234862385,0.236697248,0.23853211,
0.240366972,0.242201835,0.244036697,0.24587156,0.247706422,0.249541284,
0.251376147,0.253211009,0.255045872,0.256880734,0.258715596,0.260550459,
0.262385321,0.264220183,0.266055046,0.267889908,0.269724771,0.271559633,
0.273394495,0.275229358,0.27706422,0.278899083,0.280733945,0.282568807,
0.28440367,0.286238532,0.288073394,0.289908257,0.291743119,0.293577982,
0.295412844,0.297247706,0.299082569,0.300917431,0.302752294,0.304587156,
0.306422018,0.308256881,0.310091743,0.311926606,0.313761468,0.31559633,
0.317431193,0.319266055,0.321100917,0.32293578,0.324770642,0.326605505,
0.328440367,0.330275229,0.332110092,0.333944954,0.335779817,0.337614679,
0.339449541,0.341284404,0.343119266,0.344954128,0.346788991,0.348623853,
0.350458716,0.352293578,0.35412844,0.355963303,0.357798165,0.359633028,
0.36146789,0.363302752,0.365137615,0.366972477,0.368807339,0.370642202,
0.372477064,0.374311927,0.376146789,0.377981651,0.379816514,0.381651376,
0.383486239,0.385321101,0.387155963,0.388990826,0.390825688,0.39266055,
0.394495413,0.396330275,0.398165138,0.4,0.401834862,0.403669725,0.405504587,
0.40733945,0.409174312,0.411009174,0.412844037,0.414678899,0.416513761,
0.418348624,0.420183486,0.422018349,0.423853211,0.425688073,0.427522936,
0.429357798,0.431192661,0.433027523,0.434862385,0.436697248,0.43853211,
0.440366972,0.442201835,0.444036697,0.44587156,0.447706422,0.449541284,
0.451376147,0.453211009,0.455045872,0.456880734,0.458715596,0.460550459,
0.462385321,0.464220183,0.466055046,0.467889908,0.469724771,0.471559633,
0.473394495,0.475229358,0.47706422,0.478899083,0.480733945,0.482568807,
0.48440367,0.486238532,0.488073394,0.489908257,0.491743119,0.493577982,
0.495412844,0.497247706,0.499082569,0.500917431,0.502752294,0.504587156,
0.506422018,0.508256881,0.510091743,0.511926606,0.513761468,0.51559633,
0.517431193,0.519266055,0.521100917,0.52293578,0.524770642,0.526605505,
0.528440367,0.530275229,0.532110092,0.533944954,0.535779817,0.537614679,
0.539449541,0.541284404,0.543119266,0.544954128,0.546788991,0.548623853,
0.550458716,0.552293578,0.55412844,0.555963303,0.557798165,0.559633028,
0.56146789,0.563302752,0.565137615,0.566972477,0.568807339,0.570642202,
0.572477064,0.574311927,0.576146789,0.577981651,0.579816514,0.581651376,
0.583486239,0.585321101,0.587155963,0.588990826,0.590825688,0.59266055,
0.594495413,0.596330275,0.598165138,0.6,0.601834862,0.603669725,0.605504587,
0.60733945,0.609174312,0.611009174,0.612844037,0.614678899,0.616513761,
0.618348624,0.620183486,0.622018349,0.623853211,0.625688073,0.627522936,
0.629357798,0.631192661,0.633027523,0.634862385,0.636697248,0.63853211,
0.640366972,0.642201835,0.644036697,0.64587156,0.647706422,0.649541284,
0.651376147,0.653211009,0.655045872,0.656880734,0.658715596,0.660550459,
0.662385321,0.664220183,0.666055046,0.667889908,0.669724771,0.671559633,
0.673394495,0.675229358,0.67706422,0.678899083,0.680733945,0.682568807,
0.68440367,0.686238532,0.688073394,0.689908257,0.691743119,0.693577982,
0.695412844,0.697247706,0.699082569,0.700917431,0.702752294,0.704587156,
0.706422018,0.708256881,0.710091743,0.711926606,0.713761468,0.71559633,
0.717431193,0.719266055,0.721100917,0.72293578,0.724770642,0.726605505,
0.728440367,0.730275229,0.732110092,0.733944954,0.735779817,0.737614679,
0.739449541,0.741284404,0.743119266,0.744954128,0.746788991,0.748623853,
0.750458716,0.752293578,0.75412844,0.755963303,0.757798165,0.759633028,
0.76146789,0.763302752,0.765137615,0.766972477,0.768807339,0.770642202,
0.772477064,0.774311927,0.776146789,0.777981651,0.779816514,0.781651376,
0.783486239,0.785321101,0.787155963,0.788990826,0.790825688,0.79266055,
0.794495413,0.796330275,0.798165138,0.8,0.801834862,0.803669725,0.805504587,
0.80733945,0.809174312,0.811009174,0.812844037,0.814678899,0.816513761,
0.818348624,0.820183486,0.822018349,0.823853211,0.825688073,0.827522936,
0.829357798,0.831192661,0.833027523,0.834862385,0.836697248,0.83853211,
0.840366972,0.842201835,0.844036697,0.84587156,0.847706422,0.849541284,
0.851376147,0.853211009,0.855045872,0.856880734,0.858715596,0.860550459,
0.862385321,0.864220183,0.866055046,0.867889908,0.869724771,0.871559633,
0.873394495,0.875229358,0.87706422,0.878899083,0.880733945,0.882568807,
0.88440367,0.886238532,0.888073394,0.889908257,0.891743119,0.893577982,
0.895412844,0.897247706,0.899082569,0.900917431,0.902752294,0.904587156,
0.906422018,0.908256881,0.910091743,0.911926606,0.913761468,0.91559633,
0.917431193,0.919266055,0.921100917,0.92293578,0.924770642,0.926605505,
0.928440367,0.930275229,0.932110092,0.933944954,0.935779817,0.937614679,
0.939449541,0.941284404,0.943119266,0.944954128,0.946788991,0.948623853,
0.950458716,0.952293578,0.95412844,0.955963303,0.957798165,0.959633028,
0.96146789,0.963302752,0.965137615,0.966972477,0.968807339,0.970642202,
0.972477064,0.974311927,0.976146789,0.977981651,0.979816514,0.981651376,
0.983486239,0.985321101,0.987155963,0.988990826,0.990825688,0.99266055,
0.994495413,0.996330275,0.998165138,1.),(0.3,1.,1.3),.UNSPECIFIED.);
#6309=B_SPLINE_SURFACE_WITH_KNOTS('',5,1,((#311318,#311319,#311320),(#311321,
#311322,#311323),(#311324,#311325,#311326),(#311327,#311328,#311329),(#311330,
#311331,#311332),(#311333,#311334,#311335),(#311336,#311337,#311338),(#311339,
#311340,#311341),(#311342,#311343,#311344),(#311345,#311346,#311347),(#311348,
#311349,#311350),(#311351,#311352,#311353),(#311354,#311355,#311356),(#311357,
#311358,#311359),(#311360,#311361,#311362),(#311363,#311364,#311365),(#311366,
#311367,#311368),(#311369,#311370,#311371),(#311372,#311373,#311374),(#311375,
#311376,#311377),(#311378,#311379,#311380),(#311381,#311382,#311383),(#311384,
#311385,#311386),(#311387,#311388,#311389),(#311390,#311391,#311392),(#311393,
#311394,#311395),(#311396,#311397,#311398),(#311399,#311400,#311401),(#311402,
#311403,#311404),(#311405,#311406,#311407),(#311408,#311409,#311410),(#311411,
#311412,#311413),(#311414,#311415,#311416),(#311417,#311418,#311419),(#311420,
#311421,#311422),(#311423,#311424,#311425),(#311426,#311427,#311428),(#311429,
#311430,#311431),(#311432,#311433,#311434),(#311435,#311436,#311437),(#311438,
#311439,#311440),(#311441,#311442,#311443),(#311444,#311445,#311446),(#311447,
#311448,#311449),(#311450,#311451,#311452),(#311453,#311454,#311455),(#311456,
#311457,#311458),(#311459,#311460,#311461),(#311462,#311463,#311464),(#311465,
#311466,#311467),(#311468,#311469,#311470),(#311471,#311472,#311473),(#311474,
#311475,#311476),(#311477,#311478,#311479),(#311480,#311481,#311482),(#311483,
#311484,#311485),(#311486,#311487,#311488),(#311489,#311490,#311491),(#311492,
#311493,#311494),(#311495,#311496,#311497),(#311498,#311499,#311500),(#311501,
#311502,#311503),(#311504,#311505,#311506),(#311507,#311508,#311509),(#311510,
#311511,#311512),(#311513,#311514,#311515),(#311516,#311517,#311518),(#311519,
#311520,#311521),(#311522,#311523,#311524),(#311525,#311526,#311527),(#311528,
#311529,#311530),(#311531,#311532,#311533),(#311534,#311535,#311536),(#311537,
#311538,#311539),(#311540,#311541,#311542),(#311543,#311544,#311545),(#311546,
#311547,#311548),(#311549,#311550,#311551),(#311552,#311553,#311554),(#311555,
#311556,#311557),(#311558,#311559,#311560),(#311561,#311562,#311563),(#311564,
#311565,#311566),(#311567,#311568,#311569),(#311570,#311571,#311572),(#311573,
#311574,#311575),(#311576,#311577,#311578),(#311579,#311580,#311581),(#311582,
#311583,#311584),(#311585,#311586,#311587),(#311588,#311589,#311590),(#311591,
#311592,#311593),(#311594,#311595,#311596),(#311597,#311598,#311599),(#311600,
#311601,#311602),(#311603,#311604,#311605),(#311606,#311607,#311608),(#311609,
#311610,#311611),(#311612,#311613,#311614),(#311615,#311616,#311617),(#311618,
#311619,#311620),(#311621,#311622,#311623),(#311624,#311625,#311626),(#311627,
#311628,#311629),(#311630,#311631,#311632),(#311633,#311634,#311635),(#311636,
#311637,#311638),(#311639,#311640,#311641),(#311642,#311643,#311644),(#311645,
#311646,#311647),(#311648,#311649,#311650),(#311651,#311652,#311653),(#311654,
#311655,#311656),(#311657,#311658,#311659),(#311660,#311661,#311662),(#311663,
#311664,#311665),(#311666,#311667,#311668),(#311669,#311670,#311671),(#311672,
#311673,#311674),(#311675,#311676,#311677),(#311678,#311679,#311680),(#311681,
#311682,#311683),(#311684,#311685,#311686),(#311687,#311688,#311689),(#311690,
#311691,#311692),(#311693,#311694,#311695),(#311696,#311697,#311698),(#311699,
#311700,#311701),(#311702,#311703,#311704),(#311705,#311706,#311707),(#311708,
#311709,#311710),(#311711,#311712,#311713),(#311714,#311715,#311716),(#311717,
#311718,#311719),(#311720,#311721,#311722),(#311723,#311724,#311725),(#311726,
#311727,#311728),(#311729,#311730,#311731),(#311732,#311733,#311734),(#311735,
#311736,#311737),(#311738,#311739,#311740),(#311741,#311742,#311743),(#311744,
#311745,#311746),(#311747,#311748,#311749),(#311750,#311751,#311752),(#311753,
#311754,#311755),(#311756,#311757,#311758),(#311759,#311760,#311761),(#311762,
#311763,#311764),(#311765,#311766,#311767),(#311768,#311769,#311770),(#311771,
#311772,#311773),(#311774,#311775,#311776),(#311777,#311778,#311779),(#311780,
#311781,#311782),(#311783,#311784,#311785),(#311786,#311787,#311788),(#311789,
#311790,#311791),(#311792,#311793,#311794),(#311795,#311796,#311797),(#311798,
#311799,#311800),(#311801,#311802,#311803),(#311804,#311805,#311806),(#311807,
#311808,#311809),(#311810,#311811,#311812),(#311813,#311814,#311815),(#311816,
#311817,#311818),(#311819,#311820,#311821),(#311822,#311823,#311824),(#311825,
#311826,#311827),(#311828,#311829,#311830),(#311831,#311832,#311833),(#311834,
#311835,#311836),(#311837,#311838,#311839),(#311840,#311841,#311842),(#311843,
#311844,#311845),(#311846,#311847,#311848),(#311849,#311850,#311851),(#311852,
#311853,#311854),(#311855,#311856,#311857),(#311858,#311859,#311860),(#311861,
#311862,#311863),(#311864,#311865,#311866),(#311867,#311868,#311869),(#311870,
#311871,#311872),(#311873,#311874,#311875),(#311876,#311877,#311878),(#311879,
#311880,#311881),(#311882,#311883,#311884),(#311885,#311886,#311887),(#311888,
#311889,#311890),(#311891,#311892,#311893),(#311894,#311895,#311896),(#311897,
#311898,#311899),(#311900,#311901,#311902),(#311903,#311904,#311905),(#311906,
#311907,#311908),(#311909,#311910,#311911),(#311912,#311913,#311914),(#311915,
#311916,#311917),(#311918,#311919,#311920),(#311921,#311922,#311923),(#311924,
#311925,#311926),(#311927,#311928,#311929),(#311930,#311931,#311932),(#311933,
#311934,#311935),(#311936,#311937,#311938),(#311939,#311940,#311941),(#311942,
#311943,#311944),(#311945,#311946,#311947),(#311948,#311949,#311950),(#311951,
#311952,#311953),(#311954,#311955,#311956),(#311957,#311958,#311959),(#311960,
#311961,#311962),(#311963,#311964,#311965),(#311966,#311967,#311968),(#311969,
#311970,#311971),(#311972,#311973,#311974),(#311975,#311976,#311977),(#311978,
#311979,#311980),(#311981,#311982,#311983),(#311984,#311985,#311986),(#311987,
#311988,#311989),(#311990,#311991,#311992),(#311993,#311994,#311995),(#311996,
#311997,#311998),(#311999,#312000,#312001),(#312002,#312003,#312004),(#312005,
#312006,#312007),(#312008,#312009,#312010),(#312011,#312012,#312013),(#312014,
#312015,#312016),(#312017,#312018,#312019),(#312020,#312021,#312022),(#312023,
#312024,#312025),(#312026,#312027,#312028),(#312029,#312030,#312031),(#312032,
#312033,#312034),(#312035,#312036,#312037),(#312038,#312039,#312040),(#312041,
#312042,#312043),(#312044,#312045,#312046),(#312047,#312048,#312049),(#312050,
#312051,#312052),(#312053,#312054,#312055),(#312056,#312057,#312058),(#312059,
#312060,#312061),(#312062,#312063,#312064),(#312065,#312066,#312067),(#312068,
#312069,#312070),(#312071,#312072,#312073),(#312074,#312075,#312076),(#312077,
#312078,#312079),(#312080,#312081,#312082),(#312083,#312084,#312085),(#312086,
#312087,#312088),(#312089,#312090,#312091),(#312092,#312093,#312094),(#312095,
#312096,#312097),(#312098,#312099,#312100),(#312101,#312102,#312103),(#312104,
#312105,#312106),(#312107,#312108,#312109),(#312110,#312111,#312112),(#312113,
#312114,#312115),(#312116,#312117,#312118),(#312119,#312120,#312121),(#312122,
#312123,#312124),(#312125,#312126,#312127),(#312128,#312129,#312130),(#312131,
#312132,#312133),(#312134,#312135,#312136),(#312137,#312138,#312139),(#312140,
#312141,#312142),(#312143,#312144,#312145),(#312146,#312147,#312148),(#312149,
#312150,#312151),(#312152,#312153,#312154),(#312155,#312156,#312157),(#312158,
#312159,#312160),(#312161,#312162,#312163),(#312164,#312165,#312166),(#312167,
#312168,#312169),(#312170,#312171,#312172),(#312173,#312174,#312175),(#312176,
#312177,#312178),(#312179,#312180,#312181),(#312182,#312183,#312184),(#312185,
#312186,#312187),(#312188,#312189,#312190),(#312191,#312192,#312193),(#312194,
#312195,#312196),(#312197,#312198,#312199),(#312200,#312201,#312202),(#312203,
#312204,#312205),(#312206,#312207,#312208),(#312209,#312210,#312211),(#312212,
#312213,#312214),(#312215,#312216,#312217),(#312218,#312219,#312220),(#312221,
#312222,#312223),(#312224,#312225,#312226),(#312227,#312228,#312229),(#312230,
#312231,#312232),(#312233,#312234,#312235),(#312236,#312237,#312238),(#312239,
#312240,#312241),(#312242,#312243,#312244),(#312245,#312246,#312247),(#312248,
#312249,#312250),(#312251,#312252,#312253),(#312254,#312255,#312256),(#312257,
#312258,#312259),(#312260,#312261,#312262),(#312263,#312264,#312265),(#312266,
#312267,#312268),(#312269,#312270,#312271),(#312272,#312273,#312274),(#312275,
#312276,#312277),(#312278,#312279,#312280),(#312281,#312282,#312283),(#312284,
#312285,#312286),(#312287,#312288,#312289),(#312290,#312291,#312292),(#312293,
#312294,#312295),(#312296,#312297,#312298),(#312299,#312300,#312301),(#312302,
#312303,#312304),(#312305,#312306,#312307),(#312308,#312309,#312310),(#312311,
#312312,#312313),(#312314,#312315,#312316),(#312317,#312318,#312319),(#312320,
#312321,#312322),(#312323,#312324,#312325),(#312326,#312327,#312328),(#312329,
#312330,#312331),(#312332,#312333,#312334),(#312335,#312336,#312337),(#312338,
#312339,#312340),(#312341,#312342,#312343),(#312344,#312345,#312346),(#312347,
#312348,#312349),(#312350,#312351,#312352),(#312353,#312354,#312355),(#312356,
#312357,#312358),(#312359,#312360,#312361),(#312362,#312363,#312364),(#312365,
#312366,#312367),(#312368,#312369,#312370),(#312371,#312372,#312373),(#312374,
#312375,#312376),(#312377,#312378,#312379),(#312380,#312381,#312382),(#312383,
#312384,#312385),(#312386,#312387,#312388),(#312389,#312390,#312391),(#312392,
#312393,#312394),(#312395,#312396,#312397),(#312398,#312399,#312400),(#312401,
#312402,#312403),(#312404,#312405,#312406),(#312407,#312408,#312409),(#312410,
#312411,#312412),(#312413,#312414,#312415),(#312416,#312417,#312418),(#312419,
#312420,#312421),(#312422,#312423,#312424),(#312425,#312426,#312427),(#312428,
#312429,#312430),(#312431,#312432,#312433),(#312434,#312435,#312436),(#312437,
#312438,#312439),(#312440,#312441,#312442),(#312443,#312444,#312445),(#312446,
#312447,#312448),(#312449,#312450,#312451),(#312452,#312453,#312454),(#312455,
#312456,#312457),(#312458,#312459,#312460),(#312461,#312462,#312463),(#312464,
#312465,#312466),(#312467,#312468,#312469),(#312470,#312471,#312472),(#312473,
#312474,#312475),(#312476,#312477,#312478),(#312479,#312480,#312481),(#312482,
#312483,#312484),(#312485,#312486,#312487),(#312488,#312489,#312490),(#312491,
#312492,#312493),(#312494,#312495,#312496),(#312497,#312498,#312499),(#312500,
#312501,#312502),(#312503,#312504,#312505),(#312506,#312507,#312508),(#312509,
#312510,#312511),(#312512,#312513,#312514),(#312515,#312516,#312517),(#312518,
#312519,#312520),(#312521,#312522,#312523),(#312524,#312525,#312526),(#312527,
#312528,#312529),(#312530,#312531,#312532),(#312533,#312534,#312535),(#312536,
#312537,#312538),(#312539,#312540,#312541),(#312542,#312543,#312544),(#312545,
#312546,#312547),(#312548,#312549,#312550),(#312551,#312552,#312553),(#312554,
#312555,#312556),(#312557,#312558,#312559),(#312560,#312561,#312562),(#312563,
#312564,#312565),(#312566,#312567,#312568),(#312569,#312570,#312571),(#312572,
#312573,#312574),(#312575,#312576,#312577),(#312578,#312579,#312580),(#312581,
#312582,#312583),(#312584,#312585,#312586),(#312587,#312588,#312589),(#312590,
#312591,#312592),(#312593,#312594,#312595),(#312596,#312597,#312598),(#312599,
#312600,#312601),(#312602,#312603,#312604),(#312605,#312606,#312607),(#312608,
#312609,#312610),(#312611,#312612,#312613),(#312614,#312615,#312616),(#312617,
#312618,#312619),(#312620,#312621,#312622),(#312623,#312624,#312625),(#312626,
#312627,#312628),(#312629,#312630,#312631),(#312632,#312633,#312634),(#312635,
#312636,#312637),(#312638,#312639,#312640),(#312641,#312642,#312643),(#312644,
#312645,#312646),(#312647,#312648,#312649),(#312650,#312651,#312652),(#312653,
#312654,#312655),(#312656,#312657,#312658),(#312659,#312660,#312661),(#312662,
#312663,#312664),(#312665,#312666,#312667),(#312668,#312669,#312670),(#312671,
#312672,#312673),(#312674,#312675,#312676),(#312677,#312678,#312679),(#312680,
#312681,#312682),(#312683,#312684,#312685),(#312686,#312687,#312688),(#312689,
#312690,#312691),(#312692,#312693,#312694),(#312695,#312696,#312697),(#312698,
#312699,#312700),(#312701,#312702,#312703),(#312704,#312705,#312706),(#312707,
#312708,#312709),(#312710,#312711,#312712),(#312713,#312714,#312715),(#312716,
#312717,#312718),(#312719,#312720,#312721),(#312722,#312723,#312724),(#312725,
#312726,#312727),(#312728,#312729,#312730),(#312731,#312732,#312733),(#312734,
#312735,#312736),(#312737,#312738,#312739),(#312740,#312741,#312742),(#312743,
#312744,#312745),(#312746,#312747,#312748),(#312749,#312750,#312751),(#312752,
#312753,#312754),(#312755,#312756,#312757),(#312758,#312759,#312760),(#312761,
#312762,#312763),(#312764,#312765,#312766),(#312767,#312768,#312769),(#312770,
#312771,#312772),(#312773,#312774,#312775),(#312776,#312777,#312778),(#312779,
#312780,#312781),(#312782,#312783,#312784),(#312785,#312786,#312787),(#312788,
#312789,#312790),(#312791,#312792,#312793),(#312794,#312795,#312796),(#312797,
#312798,#312799),(#312800,#312801,#312802),(#312803,#312804,#312805),(#312806,
#312807,#312808),(#312809,#312810,#312811),(#312812,#312813,#312814),(#312815,
#312816,#312817),(#312818,#312819,#312820),(#312821,#312822,#312823),(#312824,
#312825,#312826),(#312827,#312828,#312829),(#312830,#312831,#312832),(#312833,
#312834,#312835),(#312836,#312837,#312838),(#312839,#312840,#312841),(#312842,
#312843,#312844),(#312845,#312846,#312847),(#312848,#312849,#312850),(#312851,
#312852,#312853),(#312854,#312855,#312856),(#312857,#312858,#312859),(#312860,
#312861,#312862),(#312863,#312864,#312865),(#312866,#312867,#312868),(#312869,
#312870,#312871),(#312872,#312873,#312874),(#312875,#312876,#312877),(#312878,
#312879,#312880),(#312881,#312882,#312883),(#312884,#312885,#312886),(#312887,
#312888,#312889),(#312890,#312891,#312892),(#312893,#312894,#312895),(#312896,
#312897,#312898),(#312899,#312900,#312901),(#312902,#312903,#312904),(#312905,
#312906,#312907),(#312908,#312909,#312910),(#312911,#312912,#312913),(#312914,
#312915,#312916),(#312917,#312918,#312919),(#312920,#312921,#312922),(#312923,
#312924,#312925),(#312926,#312927,#312928),(#312929,#312930,#312931),(#312932,
#312933,#312934),(#312935,#312936,#312937),(#312938,#312939,#312940),(#312941,
#312942,#312943),(#312944,#312945,#312946),(#312947,#312948,#312949),(#312950,
#312951,#312952),(#312953,#312954,#312955),(#312956,#312957,#312958),(#312959,
#312960,#312961),(#312962,#312963,#312964),(#312965,#312966,#312967)),
 .UNSPECIFIED.,.F.,.F.,.F.,(6,1,1,1,1,1,1,1,1,1,1,1,1,1,1,1,1,1,1,1,1,1,
1,1,1,1,1,1,1,1,1,1,1,1,1,1,1,1,1,1,1,1,1,1,1,1,1,1,1,1,1,1,1,1,1,1,1,1,
1,1,1,1,1,1,1,1,1,1,1,1,1,1,1,1,1,1,1,1,1,1,1,1,1,1,1,1,1,1,1,1,1,1,1,1,
1,1,1,1,1,1,1,1,1,1,1,1,1,1,1,1,1,1,1,1,1,1,1,1,1,1,1,1,1,1,1,1,1,1,1,1,
1,1,1,1,1,1,1,1,1,1,1,1,1,1,1,1,1,1,1,1,1,1,1,1,1,1,1,1,1,1,1,1,1,1,1,1,
1,1,1,1,1,1,1,1,1,1,1,1,1,1,1,1,1,1,1,1,1,1,1,1,1,1,1,1,1,1,1,1,1,1,1,1,
1,1,1,1,1,1,1,1,1,1,1,1,1,1,1,1,1,1,1,1,1,1,1,1,1,1,1,1,1,1,1,1,1,1,1,1,
1,1,1,1,1,1,1,1,1,1,1,1,1,1,1,1,1,1,1,1,1,1,1,1,1,1,1,1,1,1,1,1,1,1,1,1,
1,1,1,1,1,1,1,1,1,1,1,1,1,1,1,1,1,1,1,1,1,1,1,1,1,1,1,1,1,1,1,1,1,1,1,1,
1,1,1,1,1,1,1,1,1,1,1,1,1,1,1,1,1,1,1,1,1,1,1,1,1,1,1,1,1,1,1,1,1,1,1,1,
1,1,1,1,1,1,1,1,1,1,1,1,1,1,1,1,1,1,1,1,1,1,1,1,1,1,1,1,1,1,1,1,1,1,1,1,
1,1,1,1,1,1,1,1,1,1,1,1,1,1,1,1,1,1,1,1,1,1,1,1,1,1,1,1,1,1,1,1,1,1,1,1,
1,1,1,1,1,1,1,1,1,1,1,1,1,1,1,1,1,1,1,1,1,1,1,1,1,1,1,1,1,1,1,1,1,1,1,1,
1,1,1,1,1,1,1,1,1,1,1,1,1,1,1,1,1,1,1,1,1,1,1,1,1,1,1,1,1,1,1,1,1,1,1,1,
1,1,1,1,1,1,1,1,1,1,1,1,1,1,1,1,1,1,1,1,1,1,1,1,1,1,1,1,1,1,1,1,1,1,1,1,
1,1,1,1,1,1,1,1,1,1,1,1,1,1,1,1,1,1,1,6),(2,1,2),(-1.,-0.998165138,-0.996330275,
-0.994495413,-0.99266055,-0.990825688,-0.988990826,-0.987155963,-0.985321101,
-0.983486239,-0.981651376,-0.979816514,-0.977981651,-0.976146789,-0.974311927,
-0.972477064,-0.970642202,-0.968807339,-0.966972477,-0.965137615,-0.963302752,
-0.96146789,-0.959633028,-0.957798165,-0.955963303,-0.95412844,-0.952293578,
-0.950458716,-0.948623853,-0.946788991,-0.944954128,-0.943119266,-0.941284404,
-0.939449541,-0.937614679,-0.935779817,-0.933944954,-0.932110092,-0.930275229,
-0.928440367,-0.926605505,-0.924770642,-0.92293578,-0.921100917,-0.919266055,
-0.917431193,-0.91559633,-0.913761468,-0.911926606,-0.910091743,-0.908256881,
-0.906422018,-0.904587156,-0.902752294,-0.900917431,-0.899082569,-0.897247706,
-0.895412844,-0.893577982,-0.891743119,-0.889908257,-0.888073394,-0.886238532,
-0.88440367,-0.882568807,-0.880733945,-0.878899083,-0.87706422,-0.875229358,
-0.873394495,-0.871559633,-0.869724771,-0.867889908,-0.866055046,-0.864220183,
-0.862385321,-0.860550459,-0.858715596,-0.856880734,-0.855045872,-0.853211009,
-0.851376147,-0.849541284,-0.847706422,-0.84587156,-0.844036697,-0.842201835,
-0.840366972,-0.83853211,-0.836697248,-0.834862385,-0.833027523,-0.831192661,
-0.829357798,-0.827522936,-0.825688073,-0.823853211,-0.822018349,-0.820183486,
-0.818348624,-0.816513761,-0.814678899,-0.812844037,-0.811009174,-0.809174312,
-0.80733945,-0.805504587,-0.803669725,-0.801834862,-0.8,-0.798165138,-0.796330275,
-0.794495413,-0.79266055,-0.790825688,-0.788990826,-0.787155963,-0.785321101,
-0.783486239,-0.781651376,-0.779816514,-0.777981651,-0.776146789,-0.774311927,
-0.772477064,-0.770642202,-0.768807339,-0.766972477,-0.765137615,-0.763302752,
-0.76146789,-0.759633028,-0.757798165,-0.755963303,-0.75412844,-0.752293578,
-0.750458716,-0.748623853,-0.746788991,-0.744954128,-0.743119266,-0.741284404,
-0.739449541,-0.737614679,-0.735779817,-0.733944954,-0.732110092,-0.730275229,
-0.728440367,-0.726605505,-0.724770642,-0.72293578,-0.721100917,-0.719266055,
-0.717431193,-0.71559633,-0.713761468,-0.711926606,-0.710091743,-0.708256881,
-0.706422018,-0.704587156,-0.702752294,-0.700917431,-0.699082569,-0.697247706,
-0.695412844,-0.693577982,-0.691743119,-0.689908257,-0.688073394,-0.686238532,
-0.68440367,-0.682568807,-0.680733945,-0.678899083,-0.67706422,-0.675229358,
-0.673394495,-0.671559633,-0.669724771,-0.667889908,-0.666055046,-0.664220183,
-0.662385321,-0.660550459,-0.658715596,-0.656880734,-0.655045872,-0.653211009,
-0.651376147,-0.649541284,-0.647706422,-0.64587156,-0.644036697,-0.642201835,
-0.640366972,-0.63853211,-0.636697248,-0.634862385,-0.633027523,-0.631192661,
-0.629357798,-0.627522936,-0.625688073,-0.623853211,-0.622018349,-0.620183486,
-0.618348624,-0.616513761,-0.614678899,-0.612844037,-0.611009174,-0.609174312,
-0.60733945,-0.605504587,-0.603669725,-0.601834862,-0.6,-0.598165138,-0.596330275,
-0.594495413,-0.59266055,-0.590825688,-0.588990826,-0.587155963,-0.585321101,
-0.583486239,-0.581651376,-0.579816514,-0.577981651,-0.576146789,-0.574311927,
-0.572477064,-0.570642202,-0.568807339,-0.566972477,-0.565137615,-0.563302752,
-0.56146789,-0.559633028,-0.557798165,-0.555963303,-0.55412844,-0.552293578,
-0.550458716,-0.548623853,-0.546788991,-0.544954128,-0.543119266,-0.541284404,
-0.539449541,-0.537614679,-0.535779817,-0.533944954,-0.532110092,-0.530275229,
-0.528440367,-0.526605505,-0.524770642,-0.52293578,-0.521100917,-0.519266055,
-0.517431193,-0.51559633,-0.513761468,-0.511926606,-0.510091743,-0.508256881,
-0.506422018,-0.504587156,-0.502752294,-0.500917431,-0.499082569,-0.497247706,
-0.495412844,-0.493577982,-0.491743119,-0.489908257,-0.488073394,-0.486238532,
-0.48440367,-0.482568807,-0.480733945,-0.478899083,-0.47706422,-0.475229358,
-0.473394495,-0.471559633,-0.469724771,-0.467889908,-0.466055046,-0.464220183,
-0.462385321,-0.460550459,-0.458715596,-0.456880734,-0.455045872,-0.453211009,
-0.451376147,-0.449541284,-0.447706422,-0.44587156,-0.444036697,-0.442201835,
-0.440366972,-0.43853211,-0.436697248,-0.434862385,-0.433027523,-0.431192661,
-0.429357798,-0.427522936,-0.425688073,-0.423853211,-0.422018349,-0.420183486,
-0.418348624,-0.416513761,-0.414678899,-0.412844037,-0.411009174,-0.409174312,
-0.40733945,-0.405504587,-0.403669725,-0.401834862,-0.4,-0.398165138,-0.396330275,
-0.394495413,-0.39266055,-0.390825688,-0.388990826,-0.387155963,-0.385321101,
-0.383486239,-0.381651376,-0.379816514,-0.377981651,-0.376146789,-0.374311927,
-0.372477064,-0.370642202,-0.368807339,-0.366972477,-0.365137615,-0.363302752,
-0.36146789,-0.359633028,-0.357798165,-0.355963303,-0.35412844,-0.352293578,
-0.350458716,-0.348623853,-0.346788991,-0.344954128,-0.343119266,-0.341284404,
-0.339449541,-0.337614679,-0.335779817,-0.333944954,-0.332110092,-0.330275229,
-0.328440367,-0.326605505,-0.324770642,-0.32293578,-0.321100917,-0.319266055,
-0.317431193,-0.31559633,-0.313761468,-0.311926606,-0.310091743,-0.308256881,
-0.306422018,-0.304587156,-0.302752294,-0.300917431,-0.299082569,-0.297247706,
-0.295412844,-0.293577982,-0.291743119,-0.289908257,-0.288073394,-0.286238532,
-0.28440367,-0.282568807,-0.280733945,-0.278899083,-0.27706422,-0.275229358,
-0.273394495,-0.271559633,-0.269724771,-0.267889908,-0.266055046,-0.264220183,
-0.262385321,-0.260550459,-0.258715596,-0.256880734,-0.255045872,-0.253211009,
-0.251376147,-0.249541284,-0.247706422,-0.24587156,-0.244036697,-0.242201835,
-0.240366972,-0.23853211,-0.236697248,-0.234862385,-0.233027523,-0.231192661,
-0.229357798,-0.227522936,-0.225688073,-0.223853211,-0.222018349,-0.220183486,
-0.218348624,-0.216513761,-0.214678899,-0.212844037,-0.211009174,-0.209174312,
-0.20733945,-0.205504587,-0.203669725,-0.201834862,-0.2,-0.198165138,-0.196330275,
-0.194495413,-0.19266055,-0.190825688,-0.188990826,-0.187155963,-0.185321101,
-0.183486239,-0.181651376,-0.179816514,-0.177981651,-0.176146789,-0.174311927,
-0.172477064,-0.170642202,-0.168807339,-0.166972477,-0.165137615,-0.163302752,
-0.16146789,-0.159633028,-0.157798165,-0.155963303,-0.15412844,-0.152293578,
-0.150458716,-0.148623853,-0.146788991,-0.144954128,-0.143119266,-0.141284404,
-0.139449541,-0.137614679,-0.135779817,-0.133944954,-0.132110092,-0.130275229,
-0.128440367,-0.126605505,-0.124770642,-0.12293578,-0.121100917,-0.119266055,
-0.117431193,-0.11559633,-0.113761468,-0.111926606,-0.110091743,-0.108256881,
-0.106422018,-0.104587156,-0.102752294,-0.100917431,-0.099082569,-0.097247706,
-0.095412844,-0.093577982,-0.091743119,-0.089908257,-0.088073394,-0.086238532,
-0.08440367,-0.082568807,-0.080733945,-0.078899083,-0.07706422,-0.075229358,
-0.073394495,-0.071559633,-0.069724771,-0.067889908,-0.066055046,-0.064220183,
-0.062385321,-0.060550459,-0.058715596,-0.056880734,-0.055045872,-0.053211009,
-0.051376147,-0.049541284,-0.047706422,-0.04587156,-0.044036697,-0.042201835,
-0.040366972,-0.03853211,-0.036697248,-0.034862385,-0.033027523,-0.031192661,
-0.029357798,-0.027522936,-0.025688073,-0.023853211,-0.022018349,-0.020183486,
-0.018348624,-0.016513761,-0.014678899,-0.012844037,-0.011009174,-0.009174312,
-0.00733945,-0.005504587,-0.003669725,-0.001834862,0.00098212),(0.3,1.,
1.3),.UNSPECIFIED.);
#6310=B_SPLINE_SURFACE_WITH_KNOTS('',5,1,((#312990,#312991,#312992),(#312993,
#312994,#312995),(#312996,#312997,#312998),(#312999,#313000,#313001),(#313002,
#313003,#313004),(#313005,#313006,#313007),(#313008,#313009,#313010),(#313011,
#313012,#313013),(#313014,#313015,#313016),(#313017,#313018,#313019),(#313020,
#313021,#313022),(#313023,#313024,#313025),(#313026,#313027,#313028),(#313029,
#313030,#313031),(#313032,#313033,#313034),(#313035,#313036,#313037),(#313038,
#313039,#313040),(#313041,#313042,#313043),(#313044,#313045,#313046),(#313047,
#313048,#313049),(#313050,#313051,#313052),(#313053,#313054,#313055),(#313056,
#313057,#313058),(#313059,#313060,#313061),(#313062,#313063,#313064),(#313065,
#313066,#313067),(#313068,#313069,#313070),(#313071,#313072,#313073),(#313074,
#313075,#313076),(#313077,#313078,#313079),(#313080,#313081,#313082),(#313083,
#313084,#313085),(#313086,#313087,#313088),(#313089,#313090,#313091),(#313092,
#313093,#313094),(#313095,#313096,#313097),(#313098,#313099,#313100),(#313101,
#313102,#313103),(#313104,#313105,#313106),(#313107,#313108,#313109),(#313110,
#313111,#313112),(#313113,#313114,#313115),(#313116,#313117,#313118),(#313119,
#313120,#313121),(#313122,#313123,#313124),(#313125,#313126,#313127),(#313128,
#313129,#313130),(#313131,#313132,#313133),(#313134,#313135,#313136),(#313137,
#313138,#313139),(#313140,#313141,#313142),(#313143,#313144,#313145),(#313146,
#313147,#313148),(#313149,#313150,#313151),(#313152,#313153,#313154),(#313155,
#313156,#313157),(#313158,#313159,#313160),(#313161,#313162,#313163),(#313164,
#313165,#313166),(#313167,#313168,#313169),(#313170,#313171,#313172),(#313173,
#313174,#313175),(#313176,#313177,#313178),(#313179,#313180,#313181),(#313182,
#313183,#313184),(#313185,#313186,#313187),(#313188,#313189,#313190),(#313191,
#313192,#313193),(#313194,#313195,#313196),(#313197,#313198,#313199),(#313200,
#313201,#313202),(#313203,#313204,#313205),(#313206,#313207,#313208),(#313209,
#313210,#313211),(#313212,#313213,#313214),(#313215,#313216,#313217),(#313218,
#313219,#313220),(#313221,#313222,#313223),(#313224,#313225,#313226),(#313227,
#313228,#313229),(#313230,#313231,#313232),(#313233,#313234,#313235),(#313236,
#313237,#313238),(#313239,#313240,#313241),(#313242,#313243,#313244),(#313245,
#313246,#313247),(#313248,#313249,#313250),(#313251,#313252,#313253),(#313254,
#313255,#313256),(#313257,#313258,#313259),(#313260,#313261,#313262),(#313263,
#313264,#313265),(#313266,#313267,#313268),(#313269,#313270,#313271),(#313272,
#313273,#313274),(#313275,#313276,#313277),(#313278,#313279,#313280),(#313281,
#313282,#313283),(#313284,#313285,#313286),(#313287,#313288,#313289),(#313290,
#313291,#313292),(#313293,#313294,#313295),(#313296,#313297,#313298),(#313299,
#313300,#313301),(#313302,#313303,#313304),(#313305,#313306,#313307),(#313308,
#313309,#313310),(#313311,#313312,#313313),(#313314,#313315,#313316),(#313317,
#313318,#313319),(#313320,#313321,#313322),(#313323,#313324,#313325),(#313326,
#313327,#313328),(#313329,#313330,#313331),(#313332,#313333,#313334),(#313335,
#313336,#313337),(#313338,#313339,#313340),(#313341,#313342,#313343),(#313344,
#313345,#313346),(#313347,#313348,#313349),(#313350,#313351,#313352),(#313353,
#313354,#313355),(#313356,#313357,#313358),(#313359,#313360,#313361),(#313362,
#313363,#313364),(#313365,#313366,#313367),(#313368,#313369,#313370),(#313371,
#313372,#313373),(#313374,#313375,#313376),(#313377,#313378,#313379),(#313380,
#313381,#313382),(#313383,#313384,#313385),(#313386,#313387,#313388),(#313389,
#313390,#313391),(#313392,#313393,#313394),(#313395,#313396,#313397),(#313398,
#313399,#313400),(#313401,#313402,#313403),(#313404,#313405,#313406),(#313407,
#313408,#313409),(#313410,#313411,#313412),(#313413,#313414,#313415),(#313416,
#313417,#313418),(#313419,#313420,#313421),(#313422,#313423,#313424),(#313425,
#313426,#313427),(#313428,#313429,#313430),(#313431,#313432,#313433),(#313434,
#313435,#313436),(#313437,#313438,#313439),(#313440,#313441,#313442),(#313443,
#313444,#313445),(#313446,#313447,#313448),(#313449,#313450,#313451),(#313452,
#313453,#313454),(#313455,#313456,#313457),(#313458,#313459,#313460),(#313461,
#313462,#313463),(#313464,#313465,#313466),(#313467,#313468,#313469),(#313470,
#313471,#313472),(#313473,#313474,#313475),(#313476,#313477,#313478),(#313479,
#313480,#313481),(#313482,#313483,#313484),(#313485,#313486,#313487),(#313488,
#313489,#313490),(#313491,#313492,#313493),(#313494,#313495,#313496),(#313497,
#313498,#313499),(#313500,#313501,#313502),(#313503,#313504,#313505),(#313506,
#313507,#313508),(#313509,#313510,#313511),(#313512,#313513,#313514),(#313515,
#313516,#313517),(#313518,#313519,#313520),(#313521,#313522,#313523),(#313524,
#313525,#313526),(#313527,#313528,#313529),(#313530,#313531,#313532),(#313533,
#313534,#313535),(#313536,#313537,#313538),(#313539,#313540,#313541),(#313542,
#313543,#313544),(#313545,#313546,#313547),(#313548,#313549,#313550),(#313551,
#313552,#313553),(#313554,#313555,#313556),(#313557,#313558,#313559),(#313560,
#313561,#313562),(#313563,#313564,#313565),(#313566,#313567,#313568),(#313569,
#313570,#313571),(#313572,#313573,#313574),(#313575,#313576,#313577),(#313578,
#313579,#313580),(#313581,#313582,#313583),(#313584,#313585,#313586),(#313587,
#313588,#313589),(#313590,#313591,#313592),(#313593,#313594,#313595),(#313596,
#313597,#313598),(#313599,#313600,#313601),(#313602,#313603,#313604),(#313605,
#313606,#313607),(#313608,#313609,#313610),(#313611,#313612,#313613),(#313614,
#313615,#313616),(#313617,#313618,#313619),(#313620,#313621,#313622),(#313623,
#313624,#313625),(#313626,#313627,#313628),(#313629,#313630,#313631),(#313632,
#313633,#313634),(#313635,#313636,#313637),(#313638,#313639,#313640),(#313641,
#313642,#313643),(#313644,#313645,#313646),(#313647,#313648,#313649),(#313650,
#313651,#313652),(#313653,#313654,#313655),(#313656,#313657,#313658),(#313659,
#313660,#313661),(#313662,#313663,#313664),(#313665,#313666,#313667),(#313668,
#313669,#313670),(#313671,#313672,#313673),(#313674,#313675,#313676),(#313677,
#313678,#313679),(#313680,#313681,#313682),(#313683,#313684,#313685),(#313686,
#313687,#313688),(#313689,#313690,#313691),(#313692,#313693,#313694),(#313695,
#313696,#313697),(#313698,#313699,#313700),(#313701,#313702,#313703),(#313704,
#313705,#313706),(#313707,#313708,#313709),(#313710,#313711,#313712),(#313713,
#313714,#313715),(#313716,#313717,#313718),(#313719,#313720,#313721),(#313722,
#313723,#313724),(#313725,#313726,#313727),(#313728,#313729,#313730),(#313731,
#313732,#313733),(#313734,#313735,#313736),(#313737,#313738,#313739),(#313740,
#313741,#313742),(#313743,#313744,#313745),(#313746,#313747,#313748),(#313749,
#313750,#313751),(#313752,#313753,#313754),(#313755,#313756,#313757),(#313758,
#313759,#313760),(#313761,#313762,#313763),(#313764,#313765,#313766),(#313767,
#313768,#313769),(#313770,#313771,#313772),(#313773,#313774,#313775),(#313776,
#313777,#313778),(#313779,#313780,#313781),(#313782,#313783,#313784),(#313785,
#313786,#313787),(#313788,#313789,#313790),(#313791,#313792,#313793),(#313794,
#313795,#313796),(#313797,#313798,#313799),(#313800,#313801,#313802),(#313803,
#313804,#313805),(#313806,#313807,#313808),(#313809,#313810,#313811),(#313812,
#313813,#313814),(#313815,#313816,#313817),(#313818,#313819,#313820),(#313821,
#313822,#313823),(#313824,#313825,#313826),(#313827,#313828,#313829),(#313830,
#313831,#313832),(#313833,#313834,#313835),(#313836,#313837,#313838),(#313839,
#313840,#313841),(#313842,#313843,#313844),(#313845,#313846,#313847),(#313848,
#313849,#313850),(#313851,#313852,#313853),(#313854,#313855,#313856),(#313857,
#313858,#313859),(#313860,#313861,#313862),(#313863,#313864,#313865),(#313866,
#313867,#313868),(#313869,#313870,#313871),(#313872,#313873,#313874),(#313875,
#313876,#313877),(#313878,#313879,#313880),(#313881,#313882,#313883),(#313884,
#313885,#313886),(#313887,#313888,#313889),(#313890,#313891,#313892),(#313893,
#313894,#313895),(#313896,#313897,#313898),(#313899,#313900,#313901),(#313902,
#313903,#313904),(#313905,#313906,#313907),(#313908,#313909,#313910),(#313911,
#313912,#313913),(#313914,#313915,#313916),(#313917,#313918,#313919),(#313920,
#313921,#313922),(#313923,#313924,#313925),(#313926,#313927,#313928),(#313929,
#313930,#313931),(#313932,#313933,#313934),(#313935,#313936,#313937),(#313938,
#313939,#313940),(#313941,#313942,#313943),(#313944,#313945,#313946),(#313947,
#313948,#313949),(#313950,#313951,#313952),(#313953,#313954,#313955),(#313956,
#313957,#313958),(#313959,#313960,#313961),(#313962,#313963,#313964),(#313965,
#313966,#313967),(#313968,#313969,#313970),(#313971,#313972,#313973),(#313974,
#313975,#313976),(#313977,#313978,#313979),(#313980,#313981,#313982),(#313983,
#313984,#313985),(#313986,#313987,#313988),(#313989,#313990,#313991),(#313992,
#313993,#313994),(#313995,#313996,#313997),(#313998,#313999,#314000),(#314001,
#314002,#314003),(#314004,#314005,#314006),(#314007,#314008,#314009),(#314010,
#314011,#314012),(#314013,#314014,#314015),(#314016,#314017,#314018),(#314019,
#314020,#314021),(#314022,#314023,#314024),(#314025,#314026,#314027),(#314028,
#314029,#314030),(#314031,#314032,#314033),(#314034,#314035,#314036),(#314037,
#314038,#314039),(#314040,#314041,#314042),(#314043,#314044,#314045),(#314046,
#314047,#314048),(#314049,#314050,#314051),(#314052,#314053,#314054),(#314055,
#314056,#314057),(#314058,#314059,#314060),(#314061,#314062,#314063),(#314064,
#314065,#314066),(#314067,#314068,#314069),(#314070,#314071,#314072),(#314073,
#314074,#314075),(#314076,#314077,#314078),(#314079,#314080,#314081),(#314082,
#314083,#314084),(#314085,#314086,#314087),(#314088,#314089,#314090),(#314091,
#314092,#314093),(#314094,#314095,#314096),(#314097,#314098,#314099),(#314100,
#314101,#314102),(#314103,#314104,#314105),(#314106,#314107,#314108),(#314109,
#314110,#314111),(#314112,#314113,#314114),(#314115,#314116,#314117),(#314118,
#314119,#314120),(#314121,#314122,#314123),(#314124,#314125,#314126),(#314127,
#314128,#314129),(#314130,#314131,#314132),(#314133,#314134,#314135),(#314136,
#314137,#314138),(#314139,#314140,#314141),(#314142,#314143,#314144),(#314145,
#314146,#314147),(#314148,#314149,#314150),(#314151,#314152,#314153),(#314154,
#314155,#314156),(#314157,#314158,#314159),(#314160,#314161,#314162),(#314163,
#314164,#314165),(#314166,#314167,#314168),(#314169,#314170,#314171),(#314172,
#314173,#314174),(#314175,#314176,#314177),(#314178,#314179,#314180),(#314181,
#314182,#314183),(#314184,#314185,#314186),(#314187,#314188,#314189),(#314190,
#314191,#314192),(#314193,#314194,#314195),(#314196,#314197,#314198),(#314199,
#314200,#314201),(#314202,#314203,#314204),(#314205,#314206,#314207),(#314208,
#314209,#314210),(#314211,#314212,#314213),(#314214,#314215,#314216),(#314217,
#314218,#314219),(#314220,#314221,#314222),(#314223,#314224,#314225),(#314226,
#314227,#314228),(#314229,#314230,#314231),(#314232,#314233,#314234),(#314235,
#314236,#314237),(#314238,#314239,#314240),(#314241,#314242,#314243),(#314244,
#314245,#314246),(#314247,#314248,#314249),(#314250,#314251,#314252),(#314253,
#314254,#314255),(#314256,#314257,#314258),(#314259,#314260,#314261),(#314262,
#314263,#314264),(#314265,#314266,#314267),(#314268,#314269,#314270),(#314271,
#314272,#314273),(#314274,#314275,#314276),(#314277,#314278,#314279),(#314280,
#314281,#314282),(#314283,#314284,#314285),(#314286,#314287,#314288),(#314289,
#314290,#314291),(#314292,#314293,#314294),(#314295,#314296,#314297),(#314298,
#314299,#314300),(#314301,#314302,#314303),(#314304,#314305,#314306),(#314307,
#314308,#314309),(#314310,#314311,#314312),(#314313,#314314,#314315),(#314316,
#314317,#314318),(#314319,#314320,#314321),(#314322,#314323,#314324),(#314325,
#314326,#314327),(#314328,#314329,#314330),(#314331,#314332,#314333),(#314334,
#314335,#314336),(#314337,#314338,#314339),(#314340,#314341,#314342),(#314343,
#314344,#314345),(#314346,#314347,#314348),(#314349,#314350,#314351),(#314352,
#314353,#314354),(#314355,#314356,#314357),(#314358,#314359,#314360),(#314361,
#314362,#314363),(#314364,#314365,#314366),(#314367,#314368,#314369),(#314370,
#314371,#314372),(#314373,#314374,#314375),(#314376,#314377,#314378),(#314379,
#314380,#314381),(#314382,#314383,#314384),(#314385,#314386,#314387),(#314388,
#314389,#314390),(#314391,#314392,#314393),(#314394,#314395,#314396),(#314397,
#314398,#314399),(#314400,#314401,#314402),(#314403,#314404,#314405),(#314406,
#314407,#314408),(#314409,#314410,#314411),(#314412,#314413,#314414),(#314415,
#314416,#314417),(#314418,#314419,#314420),(#314421,#314422,#314423),(#314424,
#314425,#314426),(#314427,#314428,#314429),(#314430,#314431,#314432),(#314433,
#314434,#314435),(#314436,#314437,#314438),(#314439,#314440,#314441),(#314442,
#314443,#314444),(#314445,#314446,#314447),(#314448,#314449,#314450),(#314451,
#314452,#314453),(#314454,#314455,#314456),(#314457,#314458,#314459),(#314460,
#314461,#314462),(#314463,#314464,#314465),(#314466,#314467,#314468),(#314469,
#314470,#314471),(#314472,#314473,#314474),(#314475,#314476,#314477),(#314478,
#314479,#314480),(#314481,#314482,#314483),(#314484,#314485,#314486),(#314487,
#314488,#314489),(#314490,#314491,#314492),(#314493,#314494,#314495),(#314496,
#314497,#314498),(#314499,#314500,#314501),(#314502,#314503,#314504),(#314505,
#314506,#314507),(#314508,#314509,#314510),(#314511,#314512,#314513),(#314514,
#314515,#314516),(#314517,#314518,#314519),(#314520,#314521,#314522),(#314523,
#314524,#314525),(#314526,#314527,#314528),(#314529,#314530,#314531),(#314532,
#314533,#314534),(#314535,#314536,#314537),(#314538,#314539,#314540),(#314541,
#314542,#314543),(#314544,#314545,#314546),(#314547,#314548,#314549),(#314550,
#314551,#314552),(#314553,#314554,#314555),(#314556,#314557,#314558),(#314559,
#314560,#314561),(#314562,#314563,#314564),(#314565,#314566,#314567),(#314568,
#314569,#314570),(#314571,#314572,#314573),(#314574,#314575,#314576),(#314577,
#314578,#314579),(#314580,#314581,#314582),(#314583,#314584,#314585),(#314586,
#314587,#314588),(#314589,#314590,#314591),(#314592,#314593,#314594),(#314595,
#314596,#314597),(#314598,#314599,#314600),(#314601,#314602,#314603),(#314604,
#314605,#314606),(#314607,#314608,#314609),(#314610,#314611,#314612),(#314613,
#314614,#314615),(#314616,#314617,#314618),(#314619,#314620,#314621),(#314622,
#314623,#314624),(#314625,#314626,#314627),(#314628,#314629,#314630),(#314631,
#314632,#314633),(#314634,#314635,#314636),(#314637,#314638,#314639),(#314640,
#314641,#314642)),.UNSPECIFIED.,.F.,.F.,.F.,(6,1,1,1,1,1,1,1,1,1,1,1,1,
1,1,1,1,1,1,1,1,1,1,1,1,1,1,1,1,1,1,1,1,1,1,1,1,1,1,1,1,1,1,1,1,1,1,1,1,
1,1,1,1,1,1,1,1,1,1,1,1,1,1,1,1,1,1,1,1,1,1,1,1,1,1,1,1,1,1,1,1,1,1,1,1,
1,1,1,1,1,1,1,1,1,1,1,1,1,1,1,1,1,1,1,1,1,1,1,1,1,1,1,1,1,1,1,1,1,1,1,1,
1,1,1,1,1,1,1,1,1,1,1,1,1,1,1,1,1,1,1,1,1,1,1,1,1,1,1,1,1,1,1,1,1,1,1,1,
1,1,1,1,1,1,1,1,1,1,1,1,1,1,1,1,1,1,1,1,1,1,1,1,1,1,1,1,1,1,1,1,1,1,1,1,
1,1,1,1,1,1,1,1,1,1,1,1,1,1,1,1,1,1,1,1,1,1,1,1,1,1,1,1,1,1,1,1,1,1,1,1,
1,1,1,1,1,1,1,1,1,1,1,1,1,1,1,1,1,1,1,1,1,1,1,1,1,1,1,1,1,1,1,1,1,1,1,1,
1,1,1,1,1,1,1,1,1,1,1,1,1,1,1,1,1,1,1,1,1,1,1,1,1,1,1,1,1,1,1,1,1,1,1,1,
1,1,1,1,1,1,1,1,1,1,1,1,1,1,1,1,1,1,1,1,1,1,1,1,1,1,1,1,1,1,1,1,1,1,1,1,
1,1,1,1,1,1,1,1,1,1,1,1,1,1,1,1,1,1,1,1,1,1,1,1,1,1,1,1,1,1,1,1,1,1,1,1,
1,1,1,1,1,1,1,1,1,1,1,1,1,1,1,1,1,1,1,1,1,1,1,1,1,1,1,1,1,1,1,1,1,1,1,1,
1,1,1,1,1,1,1,1,1,1,1,1,1,1,1,1,1,1,1,1,1,1,1,1,1,1,1,1,1,1,1,1,1,1,1,1,
1,1,1,1,1,1,1,1,1,1,1,1,1,1,1,1,1,1,1,1,1,1,1,1,1,1,1,1,1,1,1,1,1,1,1,1,
1,1,1,1,1,1,1,1,1,1,1,1,1,1,1,1,1,1,1,1,1,1,1,1,1,1,1,1,1,1,1,1,1,1,1,1,
1,1,1,1,1,1,1,1,1,1,1,1,1,1,1,1,1,1,1,1,1,1,1,1,1,1,1,1,1,6),(2,1,2),(-0.001964204,
0.,0.001834862,0.003669725,0.005504587,0.00733945,0.009174312,0.011009174,
0.012844037,0.014678899,0.016513761,0.018348624,0.020183486,0.022018349,
0.023853211,0.025688073,0.027522936,0.029357798,0.031192661,0.033027523,
0.034862385,0.036697248,0.03853211,0.040366972,0.042201835,0.044036697,
0.04587156,0.047706422,0.049541284,0.051376147,0.053211009,0.055045872,
0.056880734,0.058715596,0.060550459,0.062385321,0.064220183,0.066055046,
0.067889908,0.069724771,0.071559633,0.073394495,0.075229358,0.07706422,
0.078899083,0.080733945,0.082568807,0.08440367,0.086238532,0.088073394,
0.089908257,0.091743119,0.093577982,0.095412844,0.097247706,0.099082569,
0.100917431,0.102752294,0.104587156,0.106422018,0.108256881,0.110091743,
0.111926606,0.113761468,0.11559633,0.117431193,0.119266055,0.121100917,
0.12293578,0.124770642,0.126605505,0.128440367,0.130275229,0.132110092,
0.133944954,0.135779817,0.137614679,0.139449541,0.141284404,0.143119266,
0.144954128,0.146788991,0.148623853,0.150458716,0.152293578,0.15412844,
0.155963303,0.157798165,0.159633028,0.16146789,0.163302752,0.165137615,
0.166972477,0.168807339,0.170642202,0.172477064,0.174311927,0.176146789,
0.177981651,0.179816514,0.181651376,0.183486239,0.185321101,0.187155963,
0.188990826,0.190825688,0.19266055,0.194495413,0.196330275,0.198165138,
0.2,0.201834862,0.203669725,0.205504587,0.20733945,0.209174312,0.211009174,
0.212844037,0.214678899,0.216513761,0.218348624,0.220183486,0.222018349,
0.223853211,0.225688073,0.227522936,0.229357798,0.231192661,0.233027523,
0.234862385,0.236697248,0.23853211,0.240366972,0.242201835,0.244036697,
0.24587156,0.247706422,0.249541284,0.251376147,0.253211009,0.255045872,
0.256880734,0.258715596,0.260550459,0.262385321,0.264220183,0.266055046,
0.267889908,0.269724771,0.271559633,0.273394495,0.275229358,0.27706422,
0.278899083,0.280733945,0.282568807,0.28440367,0.286238532,0.288073394,
0.289908257,0.291743119,0.293577982,0.295412844,0.297247706,0.299082569,
0.300917431,0.302752294,0.304587156,0.306422018,0.308256881,0.310091743,
0.311926606,0.313761468,0.31559633,0.317431193,0.319266055,0.321100917,
0.32293578,0.324770642,0.326605505,0.328440367,0.330275229,0.332110092,
0.333944954,0.335779817,0.337614679,0.339449541,0.341284404,0.343119266,
0.344954128,0.346788991,0.348623853,0.350458716,0.352293578,0.35412844,
0.355963303,0.357798165,0.359633028,0.36146789,0.363302752,0.365137615,
0.366972477,0.368807339,0.370642202,0.372477064,0.374311927,0.376146789,
0.377981651,0.379816514,0.381651376,0.383486239,0.385321101,0.387155963,
0.388990826,0.390825688,0.39266055,0.394495413,0.396330275,0.398165138,
0.4,0.401834862,0.403669725,0.405504587,0.40733945,0.409174312,0.411009174,
0.412844037,0.414678899,0.416513761,0.418348624,0.420183486,0.422018349,
0.423853211,0.425688073,0.427522936,0.429357798,0.431192661,0.433027523,
0.434862385,0.436697248,0.43853211,0.440366972,0.442201835,0.444036697,
0.44587156,0.447706422,0.449541284,0.451376147,0.453211009,0.455045872,
0.456880734,0.458715596,0.460550459,0.462385321,0.464220183,0.466055046,
0.467889908,0.469724771,0.471559633,0.473394495,0.475229358,0.47706422,
0.478899083,0.480733945,0.482568807,0.48440367,0.486238532,0.488073394,
0.489908257,0.491743119,0.493577982,0.495412844,0.497247706,0.499082569,
0.500917431,0.502752294,0.504587156,0.506422018,0.508256881,0.510091743,
0.511926606,0.513761468,0.51559633,0.517431193,0.519266055,0.521100917,
0.52293578,0.524770642,0.526605505,0.528440367,0.530275229,0.532110092,
0.533944954,0.535779817,0.537614679,0.539449541,0.541284404,0.543119266,
0.544954128,0.546788991,0.548623853,0.550458716,0.552293578,0.55412844,
0.555963303,0.557798165,0.559633028,0.56146789,0.563302752,0.565137615,
0.566972477,0.568807339,0.570642202,0.572477064,0.574311927,0.576146789,
0.577981651,0.579816514,0.581651376,0.583486239,0.585321101,0.587155963,
0.588990826,0.590825688,0.59266055,0.594495413,0.596330275,0.598165138,
0.6,0.601834862,0.603669725,0.605504587,0.60733945,0.609174312,0.611009174,
0.612844037,0.614678899,0.616513761,0.618348624,0.620183486,0.622018349,
0.623853211,0.625688073,0.627522936,0.629357798,0.631192661,0.633027523,
0.634862385,0.636697248,0.63853211,0.640366972,0.642201835,0.644036697,
0.64587156,0.647706422,0.649541284,0.651376147,0.653211009,0.655045872,
0.656880734,0.658715596,0.660550459,0.662385321,0.664220183,0.666055046,
0.667889908,0.669724771,0.671559633,0.673394495,0.675229358,0.67706422,
0.678899083,0.680733945,0.682568807,0.68440367,0.686238532,0.688073394,
0.689908257,0.691743119,0.693577982,0.695412844,0.697247706,0.699082569,
0.700917431,0.702752294,0.704587156,0.706422018,0.708256881,0.710091743,
0.711926606,0.713761468,0.71559633,0.717431193,0.719266055,0.721100917,
0.72293578,0.724770642,0.726605505,0.728440367,0.730275229,0.732110092,
0.733944954,0.735779817,0.737614679,0.739449541,0.741284404,0.743119266,
0.744954128,0.746788991,0.748623853,0.750458716,0.752293578,0.75412844,
0.755963303,0.757798165,0.759633028,0.76146789,0.763302752,0.765137615,
0.766972477,0.768807339,0.770642202,0.772477064,0.774311927,0.776146789,
0.777981651,0.779816514,0.781651376,0.783486239,0.785321101,0.787155963,
0.788990826,0.790825688,0.79266055,0.794495413,0.796330275,0.798165138,
0.8,0.801834862,0.803669725,0.805504587,0.80733945,0.809174312,0.811009174,
0.812844037,0.814678899,0.816513761,0.818348624,0.820183486,0.822018349,
0.823853211,0.825688073,0.827522936,0.829357798,0.831192661,0.833027523,
0.834862385,0.836697248,0.83853211,0.840366972,0.842201835,0.844036697,
0.84587156,0.847706422,0.849541284,0.851376147,0.853211009,0.855045872,
0.856880734,0.858715596,0.860550459,0.862385321,0.864220183,0.866055046,
0.867889908,0.869724771,0.871559633,0.873394495,0.875229358,0.87706422,
0.878899083,0.880733945,0.882568807,0.88440367,0.886238532,0.888073394,
0.889908257,0.891743119,0.893577982,0.895412844,0.897247706,0.899082569,
0.900917431,0.902752294,0.904587156,0.906422018,0.908256881,0.910091743,
0.911926606,0.913761468,0.91559633,0.917431193,0.919266055,0.921100917,
0.92293578,0.924770642,0.926605505,0.928440367,0.930275229,0.932110092,
0.933944954,0.935779817,0.937614679,0.939449541,0.941284404,0.943119266,
0.944954128,0.946788991,0.948623853,0.950458716,0.952293578,0.95412844,
0.955963303,0.957798165,0.959633028,0.96146789,0.963302752,0.965137615,
0.966972477,0.968807339,0.970642202,0.972477064,0.974311927,0.976146789,
0.977981651,0.979816514,0.981651376,0.983486239,0.985321101,0.987155963,
0.988990826,0.990825688,0.99266055,0.994495413,0.996330275,0.998165138,
1.),(0.3,1.,1.3),.UNSPECIFIED.);
#6311=B_SPLINE_SURFACE_WITH_KNOTS('',5,1,((#314665,#314666,#314667),(#314668,
#314669,#314670),(#314671,#314672,#314673),(#314674,#314675,#314676),(#314677,
#314678,#314679),(#314680,#314681,#314682),(#314683,#314684,#314685),(#314686,
#314687,#314688),(#314689,#314690,#314691),(#314692,#314693,#314694),(#314695,
#314696,#314697),(#314698,#314699,#314700),(#314701,#314702,#314703),(#314704,
#314705,#314706),(#314707,#314708,#314709),(#314710,#314711,#314712),(#314713,
#314714,#314715),(#314716,#314717,#314718),(#314719,#314720,#314721),(#314722,
#314723,#314724),(#314725,#314726,#314727),(#314728,#314729,#314730),(#314731,
#314732,#314733),(#314734,#314735,#314736),(#314737,#314738,#314739),(#314740,
#314741,#314742),(#314743,#314744,#314745),(#314746,#314747,#314748),(#314749,
#314750,#314751),(#314752,#314753,#314754),(#314755,#314756,#314757),(#314758,
#314759,#314760),(#314761,#314762,#314763),(#314764,#314765,#314766),(#314767,
#314768,#314769),(#314770,#314771,#314772),(#314773,#314774,#314775),(#314776,
#314777,#314778),(#314779,#314780,#314781),(#314782,#314783,#314784),(#314785,
#314786,#314787),(#314788,#314789,#314790),(#314791,#314792,#314793),(#314794,
#314795,#314796),(#314797,#314798,#314799),(#314800,#314801,#314802),(#314803,
#314804,#314805),(#314806,#314807,#314808),(#314809,#314810,#314811),(#314812,
#314813,#314814),(#314815,#314816,#314817),(#314818,#314819,#314820),(#314821,
#314822,#314823),(#314824,#314825,#314826),(#314827,#314828,#314829),(#314830,
#314831,#314832),(#314833,#314834,#314835),(#314836,#314837,#314838),(#314839,
#314840,#314841),(#314842,#314843,#314844),(#314845,#314846,#314847),(#314848,
#314849,#314850),(#314851,#314852,#314853),(#314854,#314855,#314856),(#314857,
#314858,#314859),(#314860,#314861,#314862),(#314863,#314864,#314865),(#314866,
#314867,#314868),(#314869,#314870,#314871),(#314872,#314873,#314874),(#314875,
#314876,#314877),(#314878,#314879,#314880),(#314881,#314882,#314883),(#314884,
#314885,#314886),(#314887,#314888,#314889),(#314890,#314891,#314892),(#314893,
#314894,#314895),(#314896,#314897,#314898),(#314899,#314900,#314901),(#314902,
#314903,#314904),(#314905,#314906,#314907),(#314908,#314909,#314910),(#314911,
#314912,#314913),(#314914,#314915,#314916),(#314917,#314918,#314919),(#314920,
#314921,#314922),(#314923,#314924,#314925),(#314926,#314927,#314928),(#314929,
#314930,#314931),(#314932,#314933,#314934),(#314935,#314936,#314937),(#314938,
#314939,#314940),(#314941,#314942,#314943),(#314944,#314945,#314946),(#314947,
#314948,#314949),(#314950,#314951,#314952),(#314953,#314954,#314955),(#314956,
#314957,#314958),(#314959,#314960,#314961),(#314962,#314963,#314964),(#314965,
#314966,#314967),(#314968,#314969,#314970),(#314971,#314972,#314973),(#314974,
#314975,#314976),(#314977,#314978,#314979),(#314980,#314981,#314982),(#314983,
#314984,#314985),(#314986,#314987,#314988),(#314989,#314990,#314991),(#314992,
#314993,#314994),(#314995,#314996,#314997),(#314998,#314999,#315000),(#315001,
#315002,#315003),(#315004,#315005,#315006),(#315007,#315008,#315009),(#315010,
#315011,#315012),(#315013,#315014,#315015),(#315016,#315017,#315018),(#315019,
#315020,#315021),(#315022,#315023,#315024),(#315025,#315026,#315027),(#315028,
#315029,#315030),(#315031,#315032,#315033),(#315034,#315035,#315036),(#315037,
#315038,#315039),(#315040,#315041,#315042),(#315043,#315044,#315045),(#315046,
#315047,#315048),(#315049,#315050,#315051),(#315052,#315053,#315054),(#315055,
#315056,#315057),(#315058,#315059,#315060),(#315061,#315062,#315063),(#315064,
#315065,#315066),(#315067,#315068,#315069),(#315070,#315071,#315072),(#315073,
#315074,#315075),(#315076,#315077,#315078),(#315079,#315080,#315081),(#315082,
#315083,#315084),(#315085,#315086,#315087),(#315088,#315089,#315090),(#315091,
#315092,#315093),(#315094,#315095,#315096),(#315097,#315098,#315099),(#315100,
#315101,#315102),(#315103,#315104,#315105),(#315106,#315107,#315108),(#315109,
#315110,#315111),(#315112,#315113,#315114),(#315115,#315116,#315117),(#315118,
#315119,#315120),(#315121,#315122,#315123),(#315124,#315125,#315126),(#315127,
#315128,#315129),(#315130,#315131,#315132),(#315133,#315134,#315135),(#315136,
#315137,#315138),(#315139,#315140,#315141),(#315142,#315143,#315144),(#315145,
#315146,#315147),(#315148,#315149,#315150),(#315151,#315152,#315153),(#315154,
#315155,#315156),(#315157,#315158,#315159),(#315160,#315161,#315162),(#315163,
#315164,#315165),(#315166,#315167,#315168),(#315169,#315170,#315171),(#315172,
#315173,#315174),(#315175,#315176,#315177),(#315178,#315179,#315180),(#315181,
#315182,#315183),(#315184,#315185,#315186),(#315187,#315188,#315189),(#315190,
#315191,#315192),(#315193,#315194,#315195),(#315196,#315197,#315198),(#315199,
#315200,#315201),(#315202,#315203,#315204),(#315205,#315206,#315207),(#315208,
#315209,#315210),(#315211,#315212,#315213),(#315214,#315215,#315216),(#315217,
#315218,#315219),(#315220,#315221,#315222),(#315223,#315224,#315225),(#315226,
#315227,#315228),(#315229,#315230,#315231),(#315232,#315233,#315234),(#315235,
#315236,#315237),(#315238,#315239,#315240),(#315241,#315242,#315243),(#315244,
#315245,#315246),(#315247,#315248,#315249),(#315250,#315251,#315252),(#315253,
#315254,#315255),(#315256,#315257,#315258),(#315259,#315260,#315261),(#315262,
#315263,#315264),(#315265,#315266,#315267),(#315268,#315269,#315270),(#315271,
#315272,#315273),(#315274,#315275,#315276),(#315277,#315278,#315279),(#315280,
#315281,#315282),(#315283,#315284,#315285),(#315286,#315287,#315288),(#315289,
#315290,#315291),(#315292,#315293,#315294),(#315295,#315296,#315297),(#315298,
#315299,#315300),(#315301,#315302,#315303),(#315304,#315305,#315306),(#315307,
#315308,#315309),(#315310,#315311,#315312),(#315313,#315314,#315315),(#315316,
#315317,#315318),(#315319,#315320,#315321),(#315322,#315323,#315324),(#315325,
#315326,#315327),(#315328,#315329,#315330),(#315331,#315332,#315333),(#315334,
#315335,#315336),(#315337,#315338,#315339),(#315340,#315341,#315342),(#315343,
#315344,#315345),(#315346,#315347,#315348),(#315349,#315350,#315351),(#315352,
#315353,#315354),(#315355,#315356,#315357),(#315358,#315359,#315360),(#315361,
#315362,#315363),(#315364,#315365,#315366),(#315367,#315368,#315369),(#315370,
#315371,#315372),(#315373,#315374,#315375),(#315376,#315377,#315378),(#315379,
#315380,#315381),(#315382,#315383,#315384),(#315385,#315386,#315387),(#315388,
#315389,#315390),(#315391,#315392,#315393),(#315394,#315395,#315396),(#315397,
#315398,#315399),(#315400,#315401,#315402),(#315403,#315404,#315405),(#315406,
#315407,#315408),(#315409,#315410,#315411),(#315412,#315413,#315414),(#315415,
#315416,#315417),(#315418,#315419,#315420),(#315421,#315422,#315423),(#315424,
#315425,#315426),(#315427,#315428,#315429),(#315430,#315431,#315432),(#315433,
#315434,#315435),(#315436,#315437,#315438),(#315439,#315440,#315441),(#315442,
#315443,#315444),(#315445,#315446,#315447),(#315448,#315449,#315450),(#315451,
#315452,#315453),(#315454,#315455,#315456),(#315457,#315458,#315459),(#315460,
#315461,#315462),(#315463,#315464,#315465),(#315466,#315467,#315468),(#315469,
#315470,#315471),(#315472,#315473,#315474),(#315475,#315476,#315477),(#315478,
#315479,#315480),(#315481,#315482,#315483),(#315484,#315485,#315486),(#315487,
#315488,#315489),(#315490,#315491,#315492),(#315493,#315494,#315495),(#315496,
#315497,#315498),(#315499,#315500,#315501),(#315502,#315503,#315504),(#315505,
#315506,#315507),(#315508,#315509,#315510),(#315511,#315512,#315513),(#315514,
#315515,#315516),(#315517,#315518,#315519),(#315520,#315521,#315522),(#315523,
#315524,#315525),(#315526,#315527,#315528),(#315529,#315530,#315531),(#315532,
#315533,#315534),(#315535,#315536,#315537),(#315538,#315539,#315540),(#315541,
#315542,#315543),(#315544,#315545,#315546),(#315547,#315548,#315549),(#315550,
#315551,#315552),(#315553,#315554,#315555),(#315556,#315557,#315558),(#315559,
#315560,#315561),(#315562,#315563,#315564),(#315565,#315566,#315567),(#315568,
#315569,#315570),(#315571,#315572,#315573),(#315574,#315575,#315576),(#315577,
#315578,#315579),(#315580,#315581,#315582),(#315583,#315584,#315585),(#315586,
#315587,#315588),(#315589,#315590,#315591),(#315592,#315593,#315594),(#315595,
#315596,#315597),(#315598,#315599,#315600),(#315601,#315602,#315603),(#315604,
#315605,#315606),(#315607,#315608,#315609),(#315610,#315611,#315612),(#315613,
#315614,#315615),(#315616,#315617,#315618),(#315619,#315620,#315621),(#315622,
#315623,#315624),(#315625,#315626,#315627),(#315628,#315629,#315630),(#315631,
#315632,#315633),(#315634,#315635,#315636),(#315637,#315638,#315639),(#315640,
#315641,#315642),(#315643,#315644,#315645),(#315646,#315647,#315648),(#315649,
#315650,#315651),(#315652,#315653,#315654),(#315655,#315656,#315657),(#315658,
#315659,#315660),(#315661,#315662,#315663),(#315664,#315665,#315666),(#315667,
#315668,#315669),(#315670,#315671,#315672),(#315673,#315674,#315675),(#315676,
#315677,#315678),(#315679,#315680,#315681),(#315682,#315683,#315684),(#315685,
#315686,#315687),(#315688,#315689,#315690),(#315691,#315692,#315693),(#315694,
#315695,#315696),(#315697,#315698,#315699),(#315700,#315701,#315702),(#315703,
#315704,#315705),(#315706,#315707,#315708),(#315709,#315710,#315711),(#315712,
#315713,#315714),(#315715,#315716,#315717),(#315718,#315719,#315720),(#315721,
#315722,#315723),(#315724,#315725,#315726),(#315727,#315728,#315729),(#315730,
#315731,#315732),(#315733,#315734,#315735),(#315736,#315737,#315738),(#315739,
#315740,#315741),(#315742,#315743,#315744),(#315745,#315746,#315747),(#315748,
#315749,#315750),(#315751,#315752,#315753),(#315754,#315755,#315756),(#315757,
#315758,#315759),(#315760,#315761,#315762),(#315763,#315764,#315765),(#315766,
#315767,#315768),(#315769,#315770,#315771),(#315772,#315773,#315774),(#315775,
#315776,#315777),(#315778,#315779,#315780),(#315781,#315782,#315783),(#315784,
#315785,#315786),(#315787,#315788,#315789),(#315790,#315791,#315792),(#315793,
#315794,#315795),(#315796,#315797,#315798),(#315799,#315800,#315801),(#315802,
#315803,#315804),(#315805,#315806,#315807),(#315808,#315809,#315810),(#315811,
#315812,#315813),(#315814,#315815,#315816),(#315817,#315818,#315819),(#315820,
#315821,#315822),(#315823,#315824,#315825),(#315826,#315827,#315828),(#315829,
#315830,#315831),(#315832,#315833,#315834),(#315835,#315836,#315837),(#315838,
#315839,#315840),(#315841,#315842,#315843),(#315844,#315845,#315846),(#315847,
#315848,#315849),(#315850,#315851,#315852),(#315853,#315854,#315855),(#315856,
#315857,#315858),(#315859,#315860,#315861),(#315862,#315863,#315864),(#315865,
#315866,#315867),(#315868,#315869,#315870),(#315871,#315872,#315873),(#315874,
#315875,#315876),(#315877,#315878,#315879),(#315880,#315881,#315882),(#315883,
#315884,#315885),(#315886,#315887,#315888),(#315889,#315890,#315891),(#315892,
#315893,#315894),(#315895,#315896,#315897),(#315898,#315899,#315900),(#315901,
#315902,#315903),(#315904,#315905,#315906),(#315907,#315908,#315909),(#315910,
#315911,#315912),(#315913,#315914,#315915),(#315916,#315917,#315918),(#315919,
#315920,#315921),(#315922,#315923,#315924),(#315925,#315926,#315927),(#315928,
#315929,#315930),(#315931,#315932,#315933),(#315934,#315935,#315936),(#315937,
#315938,#315939),(#315940,#315941,#315942),(#315943,#315944,#315945),(#315946,
#315947,#315948),(#315949,#315950,#315951),(#315952,#315953,#315954),(#315955,
#315956,#315957),(#315958,#315959,#315960),(#315961,#315962,#315963),(#315964,
#315965,#315966),(#315967,#315968,#315969),(#315970,#315971,#315972),(#315973,
#315974,#315975),(#315976,#315977,#315978),(#315979,#315980,#315981),(#315982,
#315983,#315984),(#315985,#315986,#315987),(#315988,#315989,#315990),(#315991,
#315992,#315993),(#315994,#315995,#315996),(#315997,#315998,#315999),(#316000,
#316001,#316002),(#316003,#316004,#316005),(#316006,#316007,#316008),(#316009,
#316010,#316011),(#316012,#316013,#316014),(#316015,#316016,#316017),(#316018,
#316019,#316020),(#316021,#316022,#316023),(#316024,#316025,#316026),(#316027,
#316028,#316029),(#316030,#316031,#316032),(#316033,#316034,#316035),(#316036,
#316037,#316038),(#316039,#316040,#316041),(#316042,#316043,#316044),(#316045,
#316046,#316047),(#316048,#316049,#316050),(#316051,#316052,#316053),(#316054,
#316055,#316056),(#316057,#316058,#316059),(#316060,#316061,#316062),(#316063,
#316064,#316065),(#316066,#316067,#316068),(#316069,#316070,#316071),(#316072,
#316073,#316074),(#316075,#316076,#316077),(#316078,#316079,#316080),(#316081,
#316082,#316083),(#316084,#316085,#316086),(#316087,#316088,#316089),(#316090,
#316091,#316092),(#316093,#316094,#316095),(#316096,#316097,#316098),(#316099,
#316100,#316101),(#316102,#316103,#316104),(#316105,#316106,#316107),(#316108,
#316109,#316110),(#316111,#316112,#316113),(#316114,#316115,#316116),(#316117,
#316118,#316119),(#316120,#316121,#316122),(#316123,#316124,#316125),(#316126,
#316127,#316128),(#316129,#316130,#316131),(#316132,#316133,#316134),(#316135,
#316136,#316137),(#316138,#316139,#316140),(#316141,#316142,#316143),(#316144,
#316145,#316146),(#316147,#316148,#316149),(#316150,#316151,#316152),(#316153,
#316154,#316155),(#316156,#316157,#316158),(#316159,#316160,#316161),(#316162,
#316163,#316164),(#316165,#316166,#316167),(#316168,#316169,#316170),(#316171,
#316172,#316173),(#316174,#316175,#316176),(#316177,#316178,#316179),(#316180,
#316181,#316182),(#316183,#316184,#316185),(#316186,#316187,#316188),(#316189,
#316190,#316191),(#316192,#316193,#316194),(#316195,#316196,#316197),(#316198,
#316199,#316200),(#316201,#316202,#316203),(#316204,#316205,#316206),(#316207,
#316208,#316209),(#316210,#316211,#316212),(#316213,#316214,#316215),(#316216,
#316217,#316218),(#316219,#316220,#316221),(#316222,#316223,#316224),(#316225,
#316226,#316227),(#316228,#316229,#316230),(#316231,#316232,#316233),(#316234,
#316235,#316236),(#316237,#316238,#316239),(#316240,#316241,#316242),(#316243,
#316244,#316245),(#316246,#316247,#316248),(#316249,#316250,#316251),(#316252,
#316253,#316254),(#316255,#316256,#316257),(#316258,#316259,#316260),(#316261,
#316262,#316263),(#316264,#316265,#316266),(#316267,#316268,#316269),(#316270,
#316271,#316272),(#316273,#316274,#316275),(#316276,#316277,#316278),(#316279,
#316280,#316281),(#316282,#316283,#316284),(#316285,#316286,#316287),(#316288,
#316289,#316290),(#316291,#316292,#316293),(#316294,#316295,#316296),(#316297,
#316298,#316299),(#316300,#316301,#316302),(#316303,#316304,#316305),(#316306,
#316307,#316308),(#316309,#316310,#316311),(#316312,#316313,#316314)),
 .UNSPECIFIED.,.F.,.F.,.F.,(6,1,1,1,1,1,1,1,1,1,1,1,1,1,1,1,1,1,1,1,1,1,
1,1,1,1,1,1,1,1,1,1,1,1,1,1,1,1,1,1,1,1,1,1,1,1,1,1,1,1,1,1,1,1,1,1,1,1,
1,1,1,1,1,1,1,1,1,1,1,1,1,1,1,1,1,1,1,1,1,1,1,1,1,1,1,1,1,1,1,1,1,1,1,1,
1,1,1,1,1,1,1,1,1,1,1,1,1,1,1,1,1,1,1,1,1,1,1,1,1,1,1,1,1,1,1,1,1,1,1,1,
1,1,1,1,1,1,1,1,1,1,1,1,1,1,1,1,1,1,1,1,1,1,1,1,1,1,1,1,1,1,1,1,1,1,1,1,
1,1,1,1,1,1,1,1,1,1,1,1,1,1,1,1,1,1,1,1,1,1,1,1,1,1,1,1,1,1,1,1,1,1,1,1,
1,1,1,1,1,1,1,1,1,1,1,1,1,1,1,1,1,1,1,1,1,1,1,1,1,1,1,1,1,1,1,1,1,1,1,1,
1,1,1,1,1,1,1,1,1,1,1,1,1,1,1,1,1,1,1,1,1,1,1,1,1,1,1,1,1,1,1,1,1,1,1,1,
1,1,1,1,1,1,1,1,1,1,1,1,1,1,1,1,1,1,1,1,1,1,1,1,1,1,1,1,1,1,1,1,1,1,1,1,
1,1,1,1,1,1,1,1,1,1,1,1,1,1,1,1,1,1,1,1,1,1,1,1,1,1,1,1,1,1,1,1,1,1,1,1,
1,1,1,1,1,1,1,1,1,1,1,1,1,1,1,1,1,1,1,1,1,1,1,1,1,1,1,1,1,1,1,1,1,1,1,1,
1,1,1,1,1,1,1,1,1,1,1,1,1,1,1,1,1,1,1,1,1,1,1,1,1,1,1,1,1,1,1,1,1,1,1,1,
1,1,1,1,1,1,1,1,1,1,1,1,1,1,1,1,1,1,1,1,1,1,1,1,1,1,1,1,1,1,1,1,1,1,1,1,
1,1,1,1,1,1,1,1,1,1,1,1,1,1,1,1,1,1,1,1,1,1,1,1,1,1,1,1,1,1,1,1,1,1,1,1,
1,1,1,1,1,1,1,1,1,1,1,1,1,1,1,1,1,1,1,1,1,1,1,1,1,1,1,1,1,1,1,1,1,1,1,1,
1,1,1,1,1,1,1,1,1,1,1,1,1,1,1,1,1,1,1,6),(2,1,2),(-1.,-0.998165138,-0.996330275,
-0.994495413,-0.99266055,-0.990825688,-0.988990826,-0.987155963,-0.985321101,
-0.983486239,-0.981651376,-0.979816514,-0.977981651,-0.976146789,-0.974311927,
-0.972477064,-0.970642202,-0.968807339,-0.966972477,-0.965137615,-0.963302752,
-0.96146789,-0.959633028,-0.957798165,-0.955963303,-0.95412844,-0.952293578,
-0.950458716,-0.948623853,-0.946788991,-0.944954128,-0.943119266,-0.941284404,
-0.939449541,-0.937614679,-0.935779817,-0.933944954,-0.932110092,-0.930275229,
-0.928440367,-0.926605505,-0.924770642,-0.92293578,-0.921100917,-0.919266055,
-0.917431193,-0.91559633,-0.913761468,-0.911926606,-0.910091743,-0.908256881,
-0.906422018,-0.904587156,-0.902752294,-0.900917431,-0.899082569,-0.897247706,
-0.895412844,-0.893577982,-0.891743119,-0.889908257,-0.888073394,-0.886238532,
-0.88440367,-0.882568807,-0.880733945,-0.878899083,-0.87706422,-0.875229358,
-0.873394495,-0.871559633,-0.869724771,-0.867889908,-0.866055046,-0.864220183,
-0.862385321,-0.860550459,-0.858715596,-0.856880734,-0.855045872,-0.853211009,
-0.851376147,-0.849541284,-0.847706422,-0.84587156,-0.844036697,-0.842201835,
-0.840366972,-0.83853211,-0.836697248,-0.834862385,-0.833027523,-0.831192661,
-0.829357798,-0.827522936,-0.825688073,-0.823853211,-0.822018349,-0.820183486,
-0.818348624,-0.816513761,-0.814678899,-0.812844037,-0.811009174,-0.809174312,
-0.80733945,-0.805504587,-0.803669725,-0.801834862,-0.8,-0.798165138,-0.796330275,
-0.794495413,-0.79266055,-0.790825688,-0.788990826,-0.787155963,-0.785321101,
-0.783486239,-0.781651376,-0.779816514,-0.777981651,-0.776146789,-0.774311927,
-0.772477064,-0.770642202,-0.768807339,-0.766972477,-0.765137615,-0.763302752,
-0.76146789,-0.759633028,-0.757798165,-0.755963303,-0.75412844,-0.752293578,
-0.750458716,-0.748623853,-0.746788991,-0.744954128,-0.743119266,-0.741284404,
-0.739449541,-0.737614679,-0.735779817,-0.733944954,-0.732110092,-0.730275229,
-0.728440367,-0.726605505,-0.724770642,-0.72293578,-0.721100917,-0.719266055,
-0.717431193,-0.71559633,-0.713761468,-0.711926606,-0.710091743,-0.708256881,
-0.706422018,-0.704587156,-0.702752294,-0.700917431,-0.699082569,-0.697247706,
-0.695412844,-0.693577982,-0.691743119,-0.689908257,-0.688073394,-0.686238532,
-0.68440367,-0.682568807,-0.680733945,-0.678899083,-0.67706422,-0.675229358,
-0.673394495,-0.671559633,-0.669724771,-0.667889908,-0.666055046,-0.664220183,
-0.662385321,-0.660550459,-0.658715596,-0.656880734,-0.655045872,-0.653211009,
-0.651376147,-0.649541284,-0.647706422,-0.64587156,-0.644036697,-0.642201835,
-0.640366972,-0.63853211,-0.636697248,-0.634862385,-0.633027523,-0.631192661,
-0.629357798,-0.627522936,-0.625688073,-0.623853211,-0.622018349,-0.620183486,
-0.618348624,-0.616513761,-0.614678899,-0.612844037,-0.611009174,-0.609174312,
-0.60733945,-0.605504587,-0.603669725,-0.601834862,-0.6,-0.598165138,-0.596330275,
-0.594495413,-0.59266055,-0.590825688,-0.588990826,-0.587155963,-0.585321101,
-0.583486239,-0.581651376,-0.579816514,-0.577981651,-0.576146789,-0.574311927,
-0.572477064,-0.570642202,-0.568807339,-0.566972477,-0.565137615,-0.563302752,
-0.56146789,-0.559633028,-0.557798165,-0.555963303,-0.55412844,-0.552293578,
-0.550458716,-0.548623853,-0.546788991,-0.544954128,-0.543119266,-0.541284404,
-0.539449541,-0.537614679,-0.535779817,-0.533944954,-0.532110092,-0.530275229,
-0.528440367,-0.526605505,-0.524770642,-0.52293578,-0.521100917,-0.519266055,
-0.517431193,-0.51559633,-0.513761468,-0.511926606,-0.510091743,-0.508256881,
-0.506422018,-0.504587156,-0.502752294,-0.500917431,-0.499082569,-0.497247706,
-0.495412844,-0.493577982,-0.491743119,-0.489908257,-0.488073394,-0.486238532,
-0.48440367,-0.482568807,-0.480733945,-0.478899083,-0.47706422,-0.475229358,
-0.473394495,-0.471559633,-0.469724771,-0.467889908,-0.466055046,-0.464220183,
-0.462385321,-0.460550459,-0.458715596,-0.456880734,-0.455045872,-0.453211009,
-0.451376147,-0.449541284,-0.447706422,-0.44587156,-0.444036697,-0.442201835,
-0.440366972,-0.43853211,-0.436697248,-0.434862385,-0.433027523,-0.431192661,
-0.429357798,-0.427522936,-0.425688073,-0.423853211,-0.422018349,-0.420183486,
-0.418348624,-0.416513761,-0.414678899,-0.412844037,-0.411009174,-0.409174312,
-0.40733945,-0.405504587,-0.403669725,-0.401834862,-0.4,-0.398165138,-0.396330275,
-0.394495413,-0.39266055,-0.390825688,-0.388990826,-0.387155963,-0.385321101,
-0.383486239,-0.381651376,-0.379816514,-0.377981651,-0.376146789,-0.374311927,
-0.372477064,-0.370642202,-0.368807339,-0.366972477,-0.365137615,-0.363302752,
-0.36146789,-0.359633028,-0.357798165,-0.355963303,-0.35412844,-0.352293578,
-0.350458716,-0.348623853,-0.346788991,-0.344954128,-0.343119266,-0.341284404,
-0.339449541,-0.337614679,-0.335779817,-0.333944954,-0.332110092,-0.330275229,
-0.328440367,-0.326605505,-0.324770642,-0.32293578,-0.321100917,-0.319266055,
-0.317431193,-0.31559633,-0.313761468,-0.311926606,-0.310091743,-0.308256881,
-0.306422018,-0.304587156,-0.302752294,-0.300917431,-0.299082569,-0.297247706,
-0.295412844,-0.293577982,-0.291743119,-0.289908257,-0.288073394,-0.286238532,
-0.28440367,-0.282568807,-0.280733945,-0.278899083,-0.27706422,-0.275229358,
-0.273394495,-0.271559633,-0.269724771,-0.267889908,-0.266055046,-0.264220183,
-0.262385321,-0.260550459,-0.258715596,-0.256880734,-0.255045872,-0.253211009,
-0.251376147,-0.249541284,-0.247706422,-0.24587156,-0.244036697,-0.242201835,
-0.240366972,-0.23853211,-0.236697248,-0.234862385,-0.233027523,-0.231192661,
-0.229357798,-0.227522936,-0.225688073,-0.223853211,-0.222018349,-0.220183486,
-0.218348624,-0.216513761,-0.214678899,-0.212844037,-0.211009174,-0.209174312,
-0.20733945,-0.205504587,-0.203669725,-0.201834862,-0.2,-0.198165138,-0.196330275,
-0.194495413,-0.19266055,-0.190825688,-0.188990826,-0.187155963,-0.185321101,
-0.183486239,-0.181651376,-0.179816514,-0.177981651,-0.176146789,-0.174311927,
-0.172477064,-0.170642202,-0.168807339,-0.166972477,-0.165137615,-0.163302752,
-0.16146789,-0.159633028,-0.157798165,-0.155963303,-0.15412844,-0.152293578,
-0.150458716,-0.148623853,-0.146788991,-0.144954128,-0.143119266,-0.141284404,
-0.139449541,-0.137614679,-0.135779817,-0.133944954,-0.132110092,-0.130275229,
-0.128440367,-0.126605505,-0.124770642,-0.12293578,-0.121100917,-0.119266055,
-0.117431193,-0.11559633,-0.113761468,-0.111926606,-0.110091743,-0.108256881,
-0.106422018,-0.104587156,-0.102752294,-0.100917431,-0.099082569,-0.097247706,
-0.095412844,-0.093577982,-0.091743119,-0.089908257,-0.088073394,-0.086238532,
-0.08440367,-0.082568807,-0.080733945,-0.078899083,-0.07706422,-0.075229358,
-0.073394495,-0.071559633,-0.069724771,-0.067889908,-0.066055046,-0.064220183,
-0.062385321,-0.060550459,-0.058715596,-0.056880734,-0.055045872,-0.053211009,
-0.051376147,-0.049541284,-0.047706422,-0.04587156,-0.044036697,-0.042201835,
-0.040366972,-0.03853211,-0.036697248,-0.034862385,-0.033027523,-0.031192661,
-0.029357798,-0.027522936,-0.025688073,-0.023853211,-0.022018349,-0.020183486,
-0.018348624,-0.016513761,-0.014678899,-0.012844037,-0.011009174,-0.009174312,
-0.00733945,-0.005504587,-0.003669725,-0.001834862,0.000982124),(0.3,1.,
1.3),.UNSPECIFIED.);
#6312=B_SPLINE_SURFACE_WITH_KNOTS('',5,1,((#316337,#316338,#316339),(#316340,
#316341,#316342),(#316343,#316344,#316345),(#316346,#316347,#316348),(#316349,
#316350,#316351),(#316352,#316353,#316354),(#316355,#316356,#316357),(#316358,
#316359,#316360),(#316361,#316362,#316363),(#316364,#316365,#316366),(#316367,
#316368,#316369),(#316370,#316371,#316372),(#316373,#316374,#316375),(#316376,
#316377,#316378),(#316379,#316380,#316381),(#316382,#316383,#316384),(#316385,
#316386,#316387),(#316388,#316389,#316390),(#316391,#316392,#316393),(#316394,
#316395,#316396),(#316397,#316398,#316399),(#316400,#316401,#316402),(#316403,
#316404,#316405),(#316406,#316407,#316408),(#316409,#316410,#316411),(#316412,
#316413,#316414),(#316415,#316416,#316417),(#316418,#316419,#316420),(#316421,
#316422,#316423),(#316424,#316425,#316426),(#316427,#316428,#316429),(#316430,
#316431,#316432),(#316433,#316434,#316435),(#316436,#316437,#316438),(#316439,
#316440,#316441),(#316442,#316443,#316444),(#316445,#316446,#316447),(#316448,
#316449,#316450),(#316451,#316452,#316453),(#316454,#316455,#316456),(#316457,
#316458,#316459),(#316460,#316461,#316462),(#316463,#316464,#316465),(#316466,
#316467,#316468),(#316469,#316470,#316471),(#316472,#316473,#316474),(#316475,
#316476,#316477),(#316478,#316479,#316480),(#316481,#316482,#316483),(#316484,
#316485,#316486),(#316487,#316488,#316489),(#316490,#316491,#316492),(#316493,
#316494,#316495),(#316496,#316497,#316498),(#316499,#316500,#316501),(#316502,
#316503,#316504),(#316505,#316506,#316507),(#316508,#316509,#316510),(#316511,
#316512,#316513),(#316514,#316515,#316516),(#316517,#316518,#316519),(#316520,
#316521,#316522),(#316523,#316524,#316525),(#316526,#316527,#316528),(#316529,
#316530,#316531),(#316532,#316533,#316534),(#316535,#316536,#316537),(#316538,
#316539,#316540),(#316541,#316542,#316543),(#316544,#316545,#316546),(#316547,
#316548,#316549),(#316550,#316551,#316552),(#316553,#316554,#316555),(#316556,
#316557,#316558),(#316559,#316560,#316561),(#316562,#316563,#316564),(#316565,
#316566,#316567),(#316568,#316569,#316570),(#316571,#316572,#316573),(#316574,
#316575,#316576),(#316577,#316578,#316579),(#316580,#316581,#316582),(#316583,
#316584,#316585),(#316586,#316587,#316588),(#316589,#316590,#316591),(#316592,
#316593,#316594),(#316595,#316596,#316597),(#316598,#316599,#316600),(#316601,
#316602,#316603),(#316604,#316605,#316606),(#316607,#316608,#316609),(#316610,
#316611,#316612),(#316613,#316614,#316615),(#316616,#316617,#316618),(#316619,
#316620,#316621),(#316622,#316623,#316624),(#316625,#316626,#316627),(#316628,
#316629,#316630),(#316631,#316632,#316633),(#316634,#316635,#316636),(#316637,
#316638,#316639),(#316640,#316641,#316642),(#316643,#316644,#316645),(#316646,
#316647,#316648),(#316649,#316650,#316651),(#316652,#316653,#316654),(#316655,
#316656,#316657),(#316658,#316659,#316660),(#316661,#316662,#316663),(#316664,
#316665,#316666),(#316667,#316668,#316669),(#316670,#316671,#316672),(#316673,
#316674,#316675),(#316676,#316677,#316678),(#316679,#316680,#316681),(#316682,
#316683,#316684),(#316685,#316686,#316687),(#316688,#316689,#316690),(#316691,
#316692,#316693),(#316694,#316695,#316696),(#316697,#316698,#316699),(#316700,
#316701,#316702),(#316703,#316704,#316705),(#316706,#316707,#316708),(#316709,
#316710,#316711),(#316712,#316713,#316714),(#316715,#316716,#316717),(#316718,
#316719,#316720),(#316721,#316722,#316723),(#316724,#316725,#316726),(#316727,
#316728,#316729),(#316730,#316731,#316732),(#316733,#316734,#316735),(#316736,
#316737,#316738),(#316739,#316740,#316741),(#316742,#316743,#316744),(#316745,
#316746,#316747),(#316748,#316749,#316750),(#316751,#316752,#316753),(#316754,
#316755,#316756),(#316757,#316758,#316759),(#316760,#316761,#316762),(#316763,
#316764,#316765),(#316766,#316767,#316768),(#316769,#316770,#316771),(#316772,
#316773,#316774),(#316775,#316776,#316777),(#316778,#316779,#316780),(#316781,
#316782,#316783),(#316784,#316785,#316786),(#316787,#316788,#316789),(#316790,
#316791,#316792),(#316793,#316794,#316795),(#316796,#316797,#316798),(#316799,
#316800,#316801),(#316802,#316803,#316804),(#316805,#316806,#316807),(#316808,
#316809,#316810),(#316811,#316812,#316813),(#316814,#316815,#316816),(#316817,
#316818,#316819),(#316820,#316821,#316822),(#316823,#316824,#316825),(#316826,
#316827,#316828),(#316829,#316830,#316831),(#316832,#316833,#316834),(#316835,
#316836,#316837),(#316838,#316839,#316840),(#316841,#316842,#316843),(#316844,
#316845,#316846),(#316847,#316848,#316849),(#316850,#316851,#316852),(#316853,
#316854,#316855),(#316856,#316857,#316858),(#316859,#316860,#316861),(#316862,
#316863,#316864),(#316865,#316866,#316867),(#316868,#316869,#316870),(#316871,
#316872,#316873),(#316874,#316875,#316876),(#316877,#316878,#316879),(#316880,
#316881,#316882),(#316883,#316884,#316885),(#316886,#316887,#316888),(#316889,
#316890,#316891),(#316892,#316893,#316894),(#316895,#316896,#316897),(#316898,
#316899,#316900),(#316901,#316902,#316903),(#316904,#316905,#316906),(#316907,
#316908,#316909),(#316910,#316911,#316912),(#316913,#316914,#316915),(#316916,
#316917,#316918),(#316919,#316920,#316921),(#316922,#316923,#316924),(#316925,
#316926,#316927),(#316928,#316929,#316930),(#316931,#316932,#316933),(#316934,
#316935,#316936),(#316937,#316938,#316939),(#316940,#316941,#316942),(#316943,
#316944,#316945),(#316946,#316947,#316948),(#316949,#316950,#316951),(#316952,
#316953,#316954),(#316955,#316956,#316957),(#316958,#316959,#316960),(#316961,
#316962,#316963),(#316964,#316965,#316966),(#316967,#316968,#316969),(#316970,
#316971,#316972),(#316973,#316974,#316975),(#316976,#316977,#316978),(#316979,
#316980,#316981),(#316982,#316983,#316984),(#316985,#316986,#316987),(#316988,
#316989,#316990),(#316991,#316992,#316993),(#316994,#316995,#316996),(#316997,
#316998,#316999),(#317000,#317001,#317002),(#317003,#317004,#317005),(#317006,
#317007,#317008),(#317009,#317010,#317011),(#317012,#317013,#317014),(#317015,
#317016,#317017),(#317018,#317019,#317020),(#317021,#317022,#317023),(#317024,
#317025,#317026),(#317027,#317028,#317029),(#317030,#317031,#317032),(#317033,
#317034,#317035),(#317036,#317037,#317038),(#317039,#317040,#317041),(#317042,
#317043,#317044),(#317045,#317046,#317047),(#317048,#317049,#317050),(#317051,
#317052,#317053),(#317054,#317055,#317056),(#317057,#317058,#317059),(#317060,
#317061,#317062),(#317063,#317064,#317065),(#317066,#317067,#317068),(#317069,
#317070,#317071),(#317072,#317073,#317074),(#317075,#317076,#317077),(#317078,
#317079,#317080),(#317081,#317082,#317083),(#317084,#317085,#317086),(#317087,
#317088,#317089),(#317090,#317091,#317092),(#317093,#317094,#317095),(#317096,
#317097,#317098),(#317099,#317100,#317101),(#317102,#317103,#317104),(#317105,
#317106,#317107),(#317108,#317109,#317110),(#317111,#317112,#317113),(#317114,
#317115,#317116),(#317117,#317118,#317119),(#317120,#317121,#317122),(#317123,
#317124,#317125),(#317126,#317127,#317128),(#317129,#317130,#317131),(#317132,
#317133,#317134),(#317135,#317136,#317137),(#317138,#317139,#317140),(#317141,
#317142,#317143),(#317144,#317145,#317146),(#317147,#317148,#317149),(#317150,
#317151,#317152),(#317153,#317154,#317155),(#317156,#317157,#317158),(#317159,
#317160,#317161),(#317162,#317163,#317164),(#317165,#317166,#317167),(#317168,
#317169,#317170),(#317171,#317172,#317173),(#317174,#317175,#317176),(#317177,
#317178,#317179),(#317180,#317181,#317182),(#317183,#317184,#317185),(#317186,
#317187,#317188),(#317189,#317190,#317191),(#317192,#317193,#317194),(#317195,
#317196,#317197),(#317198,#317199,#317200),(#317201,#317202,#317203),(#317204,
#317205,#317206),(#317207,#317208,#317209),(#317210,#317211,#317212),(#317213,
#317214,#317215),(#317216,#317217,#317218),(#317219,#317220,#317221),(#317222,
#317223,#317224),(#317225,#317226,#317227),(#317228,#317229,#317230),(#317231,
#317232,#317233),(#317234,#317235,#317236),(#317237,#317238,#317239),(#317240,
#317241,#317242),(#317243,#317244,#317245),(#317246,#317247,#317248),(#317249,
#317250,#317251),(#317252,#317253,#317254),(#317255,#317256,#317257),(#317258,
#317259,#317260),(#317261,#317262,#317263),(#317264,#317265,#317266),(#317267,
#317268,#317269),(#317270,#317271,#317272),(#317273,#317274,#317275),(#317276,
#317277,#317278),(#317279,#317280,#317281),(#317282,#317283,#317284),(#317285,
#317286,#317287),(#317288,#317289,#317290),(#317291,#317292,#317293),(#317294,
#317295,#317296),(#317297,#317298,#317299),(#317300,#317301,#317302),(#317303,
#317304,#317305),(#317306,#317307,#317308),(#317309,#317310,#317311),(#317312,
#317313,#317314),(#317315,#317316,#317317),(#317318,#317319,#317320),(#317321,
#317322,#317323),(#317324,#317325,#317326),(#317327,#317328,#317329),(#317330,
#317331,#317332),(#317333,#317334,#317335),(#317336,#317337,#317338),(#317339,
#317340,#317341),(#317342,#317343,#317344),(#317345,#317346,#317347),(#317348,
#317349,#317350),(#317351,#317352,#317353),(#317354,#317355,#317356),(#317357,
#317358,#317359),(#317360,#317361,#317362),(#317363,#317364,#317365),(#317366,
#317367,#317368),(#317369,#317370,#317371),(#317372,#317373,#317374),(#317375,
#317376,#317377),(#317378,#317379,#317380),(#317381,#317382,#317383),(#317384,
#317385,#317386),(#317387,#317388,#317389),(#317390,#317391,#317392),(#317393,
#317394,#317395),(#317396,#317397,#317398),(#317399,#317400,#317401),(#317402,
#317403,#317404),(#317405,#317406,#317407),(#317408,#317409,#317410),(#317411,
#317412,#317413),(#317414,#317415,#317416),(#317417,#317418,#317419),(#317420,
#317421,#317422),(#317423,#317424,#317425),(#317426,#317427,#317428),(#317429,
#317430,#317431),(#317432,#317433,#317434),(#317435,#317436,#317437),(#317438,
#317439,#317440),(#317441,#317442,#317443),(#317444,#317445,#317446),(#317447,
#317448,#317449),(#317450,#317451,#317452),(#317453,#317454,#317455),(#317456,
#317457,#317458),(#317459,#317460,#317461),(#317462,#317463,#317464),(#317465,
#317466,#317467),(#317468,#317469,#317470),(#317471,#317472,#317473),(#317474,
#317475,#317476),(#317477,#317478,#317479),(#317480,#317481,#317482),(#317483,
#317484,#317485),(#317486,#317487,#317488),(#317489,#317490,#317491),(#317492,
#317493,#317494),(#317495,#317496,#317497),(#317498,#317499,#317500),(#317501,
#317502,#317503),(#317504,#317505,#317506),(#317507,#317508,#317509),(#317510,
#317511,#317512),(#317513,#317514,#317515),(#317516,#317517,#317518),(#317519,
#317520,#317521),(#317522,#317523,#317524),(#317525,#317526,#317527),(#317528,
#317529,#317530),(#317531,#317532,#317533),(#317534,#317535,#317536),(#317537,
#317538,#317539),(#317540,#317541,#317542),(#317543,#317544,#317545),(#317546,
#317547,#317548),(#317549,#317550,#317551),(#317552,#317553,#317554),(#317555,
#317556,#317557),(#317558,#317559,#317560),(#317561,#317562,#317563),(#317564,
#317565,#317566),(#317567,#317568,#317569),(#317570,#317571,#317572),(#317573,
#317574,#317575),(#317576,#317577,#317578),(#317579,#317580,#317581),(#317582,
#317583,#317584),(#317585,#317586,#317587),(#317588,#317589,#317590),(#317591,
#317592,#317593),(#317594,#317595,#317596),(#317597,#317598,#317599),(#317600,
#317601,#317602),(#317603,#317604,#317605),(#317606,#317607,#317608),(#317609,
#317610,#317611),(#317612,#317613,#317614),(#317615,#317616,#317617),(#317618,
#317619,#317620),(#317621,#317622,#317623),(#317624,#317625,#317626),(#317627,
#317628,#317629),(#317630,#317631,#317632),(#317633,#317634,#317635),(#317636,
#317637,#317638),(#317639,#317640,#317641),(#317642,#317643,#317644),(#317645,
#317646,#317647),(#317648,#317649,#317650),(#317651,#317652,#317653),(#317654,
#317655,#317656),(#317657,#317658,#317659),(#317660,#317661,#317662),(#317663,
#317664,#317665),(#317666,#317667,#317668),(#317669,#317670,#317671),(#317672,
#317673,#317674),(#317675,#317676,#317677),(#317678,#317679,#317680),(#317681,
#317682,#317683),(#317684,#317685,#317686),(#317687,#317688,#317689),(#317690,
#317691,#317692),(#317693,#317694,#317695),(#317696,#317697,#317698),(#317699,
#317700,#317701),(#317702,#317703,#317704),(#317705,#317706,#317707),(#317708,
#317709,#317710),(#317711,#317712,#317713),(#317714,#317715,#317716),(#317717,
#317718,#317719),(#317720,#317721,#317722),(#317723,#317724,#317725),(#317726,
#317727,#317728),(#317729,#317730,#317731),(#317732,#317733,#317734),(#317735,
#317736,#317737),(#317738,#317739,#317740),(#317741,#317742,#317743),(#317744,
#317745,#317746),(#317747,#317748,#317749),(#317750,#317751,#317752),(#317753,
#317754,#317755),(#317756,#317757,#317758),(#317759,#317760,#317761),(#317762,
#317763,#317764),(#317765,#317766,#317767),(#317768,#317769,#317770),(#317771,
#317772,#317773),(#317774,#317775,#317776),(#317777,#317778,#317779),(#317780,
#317781,#317782),(#317783,#317784,#317785),(#317786,#317787,#317788),(#317789,
#317790,#317791),(#317792,#317793,#317794),(#317795,#317796,#317797),(#317798,
#317799,#317800),(#317801,#317802,#317803),(#317804,#317805,#317806),(#317807,
#317808,#317809),(#317810,#317811,#317812),(#317813,#317814,#317815),(#317816,
#317817,#317818),(#317819,#317820,#317821),(#317822,#317823,#317824),(#317825,
#317826,#317827),(#317828,#317829,#317830),(#317831,#317832,#317833),(#317834,
#317835,#317836),(#317837,#317838,#317839),(#317840,#317841,#317842),(#317843,
#317844,#317845),(#317846,#317847,#317848),(#317849,#317850,#317851),(#317852,
#317853,#317854),(#317855,#317856,#317857),(#317858,#317859,#317860),(#317861,
#317862,#317863),(#317864,#317865,#317866),(#317867,#317868,#317869),(#317870,
#317871,#317872),(#317873,#317874,#317875),(#317876,#317877,#317878),(#317879,
#317880,#317881),(#317882,#317883,#317884),(#317885,#317886,#317887),(#317888,
#317889,#317890),(#317891,#317892,#317893),(#317894,#317895,#317896),(#317897,
#317898,#317899),(#317900,#317901,#317902),(#317903,#317904,#317905),(#317906,
#317907,#317908),(#317909,#317910,#317911),(#317912,#317913,#317914),(#317915,
#317916,#317917),(#317918,#317919,#317920),(#317921,#317922,#317923),(#317924,
#317925,#317926),(#317927,#317928,#317929),(#317930,#317931,#317932),(#317933,
#317934,#317935),(#317936,#317937,#317938),(#317939,#317940,#317941),(#317942,
#317943,#317944),(#317945,#317946,#317947),(#317948,#317949,#317950),(#317951,
#317952,#317953),(#317954,#317955,#317956),(#317957,#317958,#317959),(#317960,
#317961,#317962),(#317963,#317964,#317965),(#317966,#317967,#317968),(#317969,
#317970,#317971),(#317972,#317973,#317974),(#317975,#317976,#317977),(#317978,
#317979,#317980),(#317981,#317982,#317983),(#317984,#317985,#317986),(#317987,
#317988,#317989)),.UNSPECIFIED.,.F.,.F.,.F.,(6,1,1,1,1,1,1,1,1,1,1,1,1,
1,1,1,1,1,1,1,1,1,1,1,1,1,1,1,1,1,1,1,1,1,1,1,1,1,1,1,1,1,1,1,1,1,1,1,1,
1,1,1,1,1,1,1,1,1,1,1,1,1,1,1,1,1,1,1,1,1,1,1,1,1,1,1,1,1,1,1,1,1,1,1,1,
1,1,1,1,1,1,1,1,1,1,1,1,1,1,1,1,1,1,1,1,1,1,1,1,1,1,1,1,1,1,1,1,1,1,1,1,
1,1,1,1,1,1,1,1,1,1,1,1,1,1,1,1,1,1,1,1,1,1,1,1,1,1,1,1,1,1,1,1,1,1,1,1,
1,1,1,1,1,1,1,1,1,1,1,1,1,1,1,1,1,1,1,1,1,1,1,1,1,1,1,1,1,1,1,1,1,1,1,1,
1,1,1,1,1,1,1,1,1,1,1,1,1,1,1,1,1,1,1,1,1,1,1,1,1,1,1,1,1,1,1,1,1,1,1,1,
1,1,1,1,1,1,1,1,1,1,1,1,1,1,1,1,1,1,1,1,1,1,1,1,1,1,1,1,1,1,1,1,1,1,1,1,
1,1,1,1,1,1,1,1,1,1,1,1,1,1,1,1,1,1,1,1,1,1,1,1,1,1,1,1,1,1,1,1,1,1,1,1,
1,1,1,1,1,1,1,1,1,1,1,1,1,1,1,1,1,1,1,1,1,1,1,1,1,1,1,1,1,1,1,1,1,1,1,1,
1,1,1,1,1,1,1,1,1,1,1,1,1,1,1,1,1,1,1,1,1,1,1,1,1,1,1,1,1,1,1,1,1,1,1,1,
1,1,1,1,1,1,1,1,1,1,1,1,1,1,1,1,1,1,1,1,1,1,1,1,1,1,1,1,1,1,1,1,1,1,1,1,
1,1,1,1,1,1,1,1,1,1,1,1,1,1,1,1,1,1,1,1,1,1,1,1,1,1,1,1,1,1,1,1,1,1,1,1,
1,1,1,1,1,1,1,1,1,1,1,1,1,1,1,1,1,1,1,1,1,1,1,1,1,1,1,1,1,1,1,1,1,1,1,1,
1,1,1,1,1,1,1,1,1,1,1,1,1,1,1,1,1,1,1,1,1,1,1,1,1,1,1,1,1,1,1,1,1,1,1,1,
1,1,1,1,1,1,1,1,1,1,1,1,1,1,1,1,1,1,1,1,1,1,1,1,1,1,1,1,1,6),(2,1,2),(-0.001964191,
0.,0.001834862,0.003669725,0.005504587,0.00733945,0.009174312,0.011009174,
0.012844037,0.014678899,0.016513761,0.018348624,0.020183486,0.022018349,
0.023853211,0.025688073,0.027522936,0.029357798,0.031192661,0.033027523,
0.034862385,0.036697248,0.03853211,0.040366972,0.042201835,0.044036697,
0.04587156,0.047706422,0.049541284,0.051376147,0.053211009,0.055045872,
0.056880734,0.058715596,0.060550459,0.062385321,0.064220183,0.066055046,
0.067889908,0.069724771,0.071559633,0.073394495,0.075229358,0.07706422,
0.078899083,0.080733945,0.082568807,0.08440367,0.086238532,0.088073394,
0.089908257,0.091743119,0.093577982,0.095412844,0.097247706,0.099082569,
0.100917431,0.102752294,0.104587156,0.106422018,0.108256881,0.110091743,
0.111926606,0.113761468,0.11559633,0.117431193,0.119266055,0.121100917,
0.12293578,0.124770642,0.126605505,0.128440367,0.130275229,0.132110092,
0.133944954,0.135779817,0.137614679,0.139449541,0.141284404,0.143119266,
0.144954128,0.146788991,0.148623853,0.150458716,0.152293578,0.15412844,
0.155963303,0.157798165,0.159633028,0.16146789,0.163302752,0.165137615,
0.166972477,0.168807339,0.170642202,0.172477064,0.174311927,0.176146789,
0.177981651,0.179816514,0.181651376,0.183486239,0.185321101,0.187155963,
0.188990826,0.190825688,0.19266055,0.194495413,0.196330275,0.198165138,
0.2,0.201834862,0.203669725,0.205504587,0.20733945,0.209174312,0.211009174,
0.212844037,0.214678899,0.216513761,0.218348624,0.220183486,0.222018349,
0.223853211,0.225688073,0.227522936,0.229357798,0.231192661,0.233027523,
0.234862385,0.236697248,0.23853211,0.240366972,0.242201835,0.244036697,
0.24587156,0.247706422,0.249541284,0.251376147,0.253211009,0.255045872,
0.256880734,0.258715596,0.260550459,0.262385321,0.264220183,0.266055046,
0.267889908,0.269724771,0.271559633,0.273394495,0.275229358,0.27706422,
0.278899083,0.280733945,0.282568807,0.28440367,0.286238532,0.288073394,
0.289908257,0.291743119,0.293577982,0.295412844,0.297247706,0.299082569,
0.300917431,0.302752294,0.304587156,0.306422018,0.308256881,0.310091743,
0.311926606,0.313761468,0.31559633,0.317431193,0.319266055,0.321100917,
0.32293578,0.324770642,0.326605505,0.328440367,0.330275229,0.332110092,
0.333944954,0.335779817,0.337614679,0.339449541,0.341284404,0.343119266,
0.344954128,0.346788991,0.348623853,0.350458716,0.352293578,0.35412844,
0.355963303,0.357798165,0.359633028,0.36146789,0.363302752,0.365137615,
0.366972477,0.368807339,0.370642202,0.372477064,0.374311927,0.376146789,
0.377981651,0.379816514,0.381651376,0.383486239,0.385321101,0.387155963,
0.388990826,0.390825688,0.39266055,0.394495413,0.396330275,0.398165138,
0.4,0.401834862,0.403669725,0.405504587,0.40733945,0.409174312,0.411009174,
0.412844037,0.414678899,0.416513761,0.418348624,0.420183486,0.422018349,
0.423853211,0.425688073,0.427522936,0.429357798,0.431192661,0.433027523,
0.434862385,0.436697248,0.43853211,0.440366972,0.442201835,0.444036697,
0.44587156,0.447706422,0.449541284,0.451376147,0.453211009,0.455045872,
0.456880734,0.458715596,0.460550459,0.462385321,0.464220183,0.466055046,
0.467889908,0.469724771,0.471559633,0.473394495,0.475229358,0.47706422,
0.478899083,0.480733945,0.482568807,0.48440367,0.486238532,0.488073394,
0.489908257,0.491743119,0.493577982,0.495412844,0.497247706,0.499082569,
0.500917431,0.502752294,0.504587156,0.506422018,0.508256881,0.510091743,
0.511926606,0.513761468,0.51559633,0.517431193,0.519266055,0.521100917,
0.52293578,0.524770642,0.526605505,0.528440367,0.530275229,0.532110092,
0.533944954,0.535779817,0.537614679,0.539449541,0.541284404,0.543119266,
0.544954128,0.546788991,0.548623853,0.550458716,0.552293578,0.55412844,
0.555963303,0.557798165,0.559633028,0.56146789,0.563302752,0.565137615,
0.566972477,0.568807339,0.570642202,0.572477064,0.574311927,0.576146789,
0.577981651,0.579816514,0.581651376,0.583486239,0.585321101,0.587155963,
0.588990826,0.590825688,0.59266055,0.594495413,0.596330275,0.598165138,
0.6,0.601834862,0.603669725,0.605504587,0.60733945,0.609174312,0.611009174,
0.612844037,0.614678899,0.616513761,0.618348624,0.620183486,0.622018349,
0.623853211,0.625688073,0.627522936,0.629357798,0.631192661,0.633027523,
0.634862385,0.636697248,0.63853211,0.640366972,0.642201835,0.644036697,
0.64587156,0.647706422,0.649541284,0.651376147,0.653211009,0.655045872,
0.656880734,0.658715596,0.660550459,0.662385321,0.664220183,0.666055046,
0.667889908,0.669724771,0.671559633,0.673394495,0.675229358,0.67706422,
0.678899083,0.680733945,0.682568807,0.68440367,0.686238532,0.688073394,
0.689908257,0.691743119,0.693577982,0.695412844,0.697247706,0.699082569,
0.700917431,0.702752294,0.704587156,0.706422018,0.708256881,0.710091743,
0.711926606,0.713761468,0.71559633,0.717431193,0.719266055,0.721100917,
0.72293578,0.724770642,0.726605505,0.728440367,0.730275229,0.732110092,
0.733944954,0.735779817,0.737614679,0.739449541,0.741284404,0.743119266,
0.744954128,0.746788991,0.748623853,0.750458716,0.752293578,0.75412844,
0.755963303,0.757798165,0.759633028,0.76146789,0.763302752,0.765137615,
0.766972477,0.768807339,0.770642202,0.772477064,0.774311927,0.776146789,
0.777981651,0.779816514,0.781651376,0.783486239,0.785321101,0.787155963,
0.788990826,0.790825688,0.79266055,0.794495413,0.796330275,0.798165138,
0.8,0.801834862,0.803669725,0.805504587,0.80733945,0.809174312,0.811009174,
0.812844037,0.814678899,0.816513761,0.818348624,0.820183486,0.822018349,
0.823853211,0.825688073,0.827522936,0.829357798,0.831192661,0.833027523,
0.834862385,0.836697248,0.83853211,0.840366972,0.842201835,0.844036697,
0.84587156,0.847706422,0.849541284,0.851376147,0.853211009,0.855045872,
0.856880734,0.858715596,0.860550459,0.862385321,0.864220183,0.866055046,
0.867889908,0.869724771,0.871559633,0.873394495,0.875229358,0.87706422,
0.878899083,0.880733945,0.882568807,0.88440367,0.886238532,0.888073394,
0.889908257,0.891743119,0.893577982,0.895412844,0.897247706,0.899082569,
0.900917431,0.902752294,0.904587156,0.906422018,0.908256881,0.910091743,
0.911926606,0.913761468,0.91559633,0.917431193,0.919266055,0.921100917,
0.92293578,0.924770642,0.926605505,0.928440367,0.930275229,0.932110092,
0.933944954,0.935779817,0.937614679,0.939449541,0.941284404,0.943119266,
0.944954128,0.946788991,0.948623853,0.950458716,0.952293578,0.95412844,
0.955963303,0.957798165,0.959633028,0.96146789,0.963302752,0.965137615,
0.966972477,0.968807339,0.970642202,0.972477064,0.974311927,0.976146789,
0.977981651,0.979816514,0.981651376,0.983486239,0.985321101,0.987155963,
0.988990826,0.990825688,0.99266055,0.994495413,0.996330275,0.998165138,
1.),(0.3,1.,1.3),.UNSPECIFIED.);
#6313=B_SPLINE_SURFACE_WITH_KNOTS('',5,1,((#318012,#318013,#318014),(#318015,
#318016,#318017),(#318018,#318019,#318020),(#318021,#318022,#318023),(#318024,
#318025,#318026),(#318027,#318028,#318029),(#318030,#318031,#318032),(#318033,
#318034,#318035),(#318036,#318037,#318038),(#318039,#318040,#318041),(#318042,
#318043,#318044),(#318045,#318046,#318047),(#318048,#318049,#318050),(#318051,
#318052,#318053),(#318054,#318055,#318056),(#318057,#318058,#318059),(#318060,
#318061,#318062),(#318063,#318064,#318065),(#318066,#318067,#318068),(#318069,
#318070,#318071),(#318072,#318073,#318074),(#318075,#318076,#318077),(#318078,
#318079,#318080),(#318081,#318082,#318083),(#318084,#318085,#318086),(#318087,
#318088,#318089),(#318090,#318091,#318092),(#318093,#318094,#318095),(#318096,
#318097,#318098),(#318099,#318100,#318101),(#318102,#318103,#318104),(#318105,
#318106,#318107),(#318108,#318109,#318110),(#318111,#318112,#318113),(#318114,
#318115,#318116),(#318117,#318118,#318119),(#318120,#318121,#318122),(#318123,
#318124,#318125),(#318126,#318127,#318128),(#318129,#318130,#318131),(#318132,
#318133,#318134),(#318135,#318136,#318137),(#318138,#318139,#318140),(#318141,
#318142,#318143),(#318144,#318145,#318146),(#318147,#318148,#318149),(#318150,
#318151,#318152),(#318153,#318154,#318155),(#318156,#318157,#318158),(#318159,
#318160,#318161),(#318162,#318163,#318164),(#318165,#318166,#318167),(#318168,
#318169,#318170),(#318171,#318172,#318173),(#318174,#318175,#318176),(#318177,
#318178,#318179),(#318180,#318181,#318182),(#318183,#318184,#318185),(#318186,
#318187,#318188),(#318189,#318190,#318191),(#318192,#318193,#318194),(#318195,
#318196,#318197),(#318198,#318199,#318200),(#318201,#318202,#318203),(#318204,
#318205,#318206),(#318207,#318208,#318209),(#318210,#318211,#318212),(#318213,
#318214,#318215),(#318216,#318217,#318218),(#318219,#318220,#318221),(#318222,
#318223,#318224),(#318225,#318226,#318227),(#318228,#318229,#318230),(#318231,
#318232,#318233),(#318234,#318235,#318236),(#318237,#318238,#318239),(#318240,
#318241,#318242),(#318243,#318244,#318245),(#318246,#318247,#318248),(#318249,
#318250,#318251),(#318252,#318253,#318254),(#318255,#318256,#318257),(#318258,
#318259,#318260),(#318261,#318262,#318263),(#318264,#318265,#318266),(#318267,
#318268,#318269),(#318270,#318271,#318272),(#318273,#318274,#318275),(#318276,
#318277,#318278),(#318279,#318280,#318281),(#318282,#318283,#318284),(#318285,
#318286,#318287),(#318288,#318289,#318290),(#318291,#318292,#318293),(#318294,
#318295,#318296),(#318297,#318298,#318299),(#318300,#318301,#318302),(#318303,
#318304,#318305),(#318306,#318307,#318308),(#318309,#318310,#318311),(#318312,
#318313,#318314),(#318315,#318316,#318317),(#318318,#318319,#318320),(#318321,
#318322,#318323),(#318324,#318325,#318326),(#318327,#318328,#318329),(#318330,
#318331,#318332),(#318333,#318334,#318335),(#318336,#318337,#318338),(#318339,
#318340,#318341),(#318342,#318343,#318344),(#318345,#318346,#318347),(#318348,
#318349,#318350),(#318351,#318352,#318353),(#318354,#318355,#318356),(#318357,
#318358,#318359),(#318360,#318361,#318362),(#318363,#318364,#318365),(#318366,
#318367,#318368),(#318369,#318370,#318371),(#318372,#318373,#318374),(#318375,
#318376,#318377),(#318378,#318379,#318380),(#318381,#318382,#318383),(#318384,
#318385,#318386),(#318387,#318388,#318389),(#318390,#318391,#318392),(#318393,
#318394,#318395),(#318396,#318397,#318398),(#318399,#318400,#318401),(#318402,
#318403,#318404),(#318405,#318406,#318407),(#318408,#318409,#318410),(#318411,
#318412,#318413),(#318414,#318415,#318416),(#318417,#318418,#318419),(#318420,
#318421,#318422),(#318423,#318424,#318425),(#318426,#318427,#318428),(#318429,
#318430,#318431),(#318432,#318433,#318434),(#318435,#318436,#318437),(#318438,
#318439,#318440),(#318441,#318442,#318443),(#318444,#318445,#318446),(#318447,
#318448,#318449),(#318450,#318451,#318452),(#318453,#318454,#318455),(#318456,
#318457,#318458),(#318459,#318460,#318461),(#318462,#318463,#318464),(#318465,
#318466,#318467),(#318468,#318469,#318470),(#318471,#318472,#318473),(#318474,
#318475,#318476),(#318477,#318478,#318479),(#318480,#318481,#318482),(#318483,
#318484,#318485),(#318486,#318487,#318488),(#318489,#318490,#318491),(#318492,
#318493,#318494),(#318495,#318496,#318497),(#318498,#318499,#318500),(#318501,
#318502,#318503),(#318504,#318505,#318506),(#318507,#318508,#318509),(#318510,
#318511,#318512),(#318513,#318514,#318515),(#318516,#318517,#318518),(#318519,
#318520,#318521),(#318522,#318523,#318524),(#318525,#318526,#318527),(#318528,
#318529,#318530),(#318531,#318532,#318533),(#318534,#318535,#318536),(#318537,
#318538,#318539),(#318540,#318541,#318542),(#318543,#318544,#318545),(#318546,
#318547,#318548),(#318549,#318550,#318551),(#318552,#318553,#318554),(#318555,
#318556,#318557),(#318558,#318559,#318560),(#318561,#318562,#318563),(#318564,
#318565,#318566),(#318567,#318568,#318569),(#318570,#318571,#318572),(#318573,
#318574,#318575),(#318576,#318577,#318578),(#318579,#318580,#318581),(#318582,
#318583,#318584),(#318585,#318586,#318587),(#318588,#318589,#318590),(#318591,
#318592,#318593),(#318594,#318595,#318596),(#318597,#318598,#318599),(#318600,
#318601,#318602),(#318603,#318604,#318605),(#318606,#318607,#318608),(#318609,
#318610,#318611),(#318612,#318613,#318614),(#318615,#318616,#318617),(#318618,
#318619,#318620),(#318621,#318622,#318623),(#318624,#318625,#318626),(#318627,
#318628,#318629),(#318630,#318631,#318632),(#318633,#318634,#318635),(#318636,
#318637,#318638),(#318639,#318640,#318641),(#318642,#318643,#318644),(#318645,
#318646,#318647),(#318648,#318649,#318650),(#318651,#318652,#318653),(#318654,
#318655,#318656),(#318657,#318658,#318659),(#318660,#318661,#318662),(#318663,
#318664,#318665),(#318666,#318667,#318668),(#318669,#318670,#318671),(#318672,
#318673,#318674),(#318675,#318676,#318677),(#318678,#318679,#318680),(#318681,
#318682,#318683),(#318684,#318685,#318686),(#318687,#318688,#318689),(#318690,
#318691,#318692),(#318693,#318694,#318695),(#318696,#318697,#318698),(#318699,
#318700,#318701),(#318702,#318703,#318704),(#318705,#318706,#318707),(#318708,
#318709,#318710),(#318711,#318712,#318713),(#318714,#318715,#318716),(#318717,
#318718,#318719),(#318720,#318721,#318722),(#318723,#318724,#318725),(#318726,
#318727,#318728),(#318729,#318730,#318731),(#318732,#318733,#318734),(#318735,
#318736,#318737),(#318738,#318739,#318740),(#318741,#318742,#318743),(#318744,
#318745,#318746),(#318747,#318748,#318749),(#318750,#318751,#318752),(#318753,
#318754,#318755),(#318756,#318757,#318758),(#318759,#318760,#318761),(#318762,
#318763,#318764),(#318765,#318766,#318767),(#318768,#318769,#318770),(#318771,
#318772,#318773),(#318774,#318775,#318776),(#318777,#318778,#318779),(#318780,
#318781,#318782),(#318783,#318784,#318785),(#318786,#318787,#318788),(#318789,
#318790,#318791),(#318792,#318793,#318794),(#318795,#318796,#318797),(#318798,
#318799,#318800),(#318801,#318802,#318803),(#318804,#318805,#318806),(#318807,
#318808,#318809),(#318810,#318811,#318812),(#318813,#318814,#318815),(#318816,
#318817,#318818),(#318819,#318820,#318821),(#318822,#318823,#318824),(#318825,
#318826,#318827),(#318828,#318829,#318830),(#318831,#318832,#318833),(#318834,
#318835,#318836),(#318837,#318838,#318839),(#318840,#318841,#318842),(#318843,
#318844,#318845),(#318846,#318847,#318848),(#318849,#318850,#318851),(#318852,
#318853,#318854),(#318855,#318856,#318857),(#318858,#318859,#318860),(#318861,
#318862,#318863),(#318864,#318865,#318866),(#318867,#318868,#318869),(#318870,
#318871,#318872),(#318873,#318874,#318875),(#318876,#318877,#318878),(#318879,
#318880,#318881),(#318882,#318883,#318884),(#318885,#318886,#318887),(#318888,
#318889,#318890),(#318891,#318892,#318893),(#318894,#318895,#318896),(#318897,
#318898,#318899),(#318900,#318901,#318902),(#318903,#318904,#318905),(#318906,
#318907,#318908),(#318909,#318910,#318911),(#318912,#318913,#318914),(#318915,
#318916,#318917),(#318918,#318919,#318920),(#318921,#318922,#318923),(#318924,
#318925,#318926),(#318927,#318928,#318929),(#318930,#318931,#318932),(#318933,
#318934,#318935),(#318936,#318937,#318938),(#318939,#318940,#318941),(#318942,
#318943,#318944),(#318945,#318946,#318947),(#318948,#318949,#318950),(#318951,
#318952,#318953),(#318954,#318955,#318956),(#318957,#318958,#318959),(#318960,
#318961,#318962),(#318963,#318964,#318965),(#318966,#318967,#318968),(#318969,
#318970,#318971),(#318972,#318973,#318974),(#318975,#318976,#318977),(#318978,
#318979,#318980),(#318981,#318982,#318983),(#318984,#318985,#318986),(#318987,
#318988,#318989),(#318990,#318991,#318992),(#318993,#318994,#318995),(#318996,
#318997,#318998),(#318999,#319000,#319001),(#319002,#319003,#319004),(#319005,
#319006,#319007),(#319008,#319009,#319010),(#319011,#319012,#319013),(#319014,
#319015,#319016),(#319017,#319018,#319019),(#319020,#319021,#319022),(#319023,
#319024,#319025),(#319026,#319027,#319028),(#319029,#319030,#319031),(#319032,
#319033,#319034),(#319035,#319036,#319037),(#319038,#319039,#319040),(#319041,
#319042,#319043),(#319044,#319045,#319046),(#319047,#319048,#319049),(#319050,
#319051,#319052),(#319053,#319054,#319055),(#319056,#319057,#319058),(#319059,
#319060,#319061),(#319062,#319063,#319064),(#319065,#319066,#319067),(#319068,
#319069,#319070),(#319071,#319072,#319073),(#319074,#319075,#319076),(#319077,
#319078,#319079),(#319080,#319081,#319082),(#319083,#319084,#319085),(#319086,
#319087,#319088),(#319089,#319090,#319091),(#319092,#319093,#319094),(#319095,
#319096,#319097),(#319098,#319099,#319100),(#319101,#319102,#319103),(#319104,
#319105,#319106),(#319107,#319108,#319109),(#319110,#319111,#319112),(#319113,
#319114,#319115),(#319116,#319117,#319118),(#319119,#319120,#319121),(#319122,
#319123,#319124),(#319125,#319126,#319127),(#319128,#319129,#319130),(#319131,
#319132,#319133),(#319134,#319135,#319136),(#319137,#319138,#319139),(#319140,
#319141,#319142),(#319143,#319144,#319145),(#319146,#319147,#319148),(#319149,
#319150,#319151),(#319152,#319153,#319154),(#319155,#319156,#319157),(#319158,
#319159,#319160),(#319161,#319162,#319163),(#319164,#319165,#319166),(#319167,
#319168,#319169),(#319170,#319171,#319172),(#319173,#319174,#319175),(#319176,
#319177,#319178),(#319179,#319180,#319181),(#319182,#319183,#319184),(#319185,
#319186,#319187),(#319188,#319189,#319190),(#319191,#319192,#319193),(#319194,
#319195,#319196),(#319197,#319198,#319199),(#319200,#319201,#319202),(#319203,
#319204,#319205),(#319206,#319207,#319208),(#319209,#319210,#319211),(#319212,
#319213,#319214),(#319215,#319216,#319217),(#319218,#319219,#319220),(#319221,
#319222,#319223),(#319224,#319225,#319226),(#319227,#319228,#319229),(#319230,
#319231,#319232),(#319233,#319234,#319235),(#319236,#319237,#319238),(#319239,
#319240,#319241),(#319242,#319243,#319244),(#319245,#319246,#319247),(#319248,
#319249,#319250),(#319251,#319252,#319253),(#319254,#319255,#319256),(#319257,
#319258,#319259),(#319260,#319261,#319262),(#319263,#319264,#319265),(#319266,
#319267,#319268),(#319269,#319270,#319271),(#319272,#319273,#319274),(#319275,
#319276,#319277),(#319278,#319279,#319280),(#319281,#319282,#319283),(#319284,
#319285,#319286),(#319287,#319288,#319289),(#319290,#319291,#319292),(#319293,
#319294,#319295),(#319296,#319297,#319298),(#319299,#319300,#319301),(#319302,
#319303,#319304),(#319305,#319306,#319307),(#319308,#319309,#319310),(#319311,
#319312,#319313),(#319314,#319315,#319316),(#319317,#319318,#319319),(#319320,
#319321,#319322),(#319323,#319324,#319325),(#319326,#319327,#319328),(#319329,
#319330,#319331),(#319332,#319333,#319334),(#319335,#319336,#319337),(#319338,
#319339,#319340),(#319341,#319342,#319343),(#319344,#319345,#319346),(#319347,
#319348,#319349),(#319350,#319351,#319352),(#319353,#319354,#319355),(#319356,
#319357,#319358),(#319359,#319360,#319361),(#319362,#319363,#319364),(#319365,
#319366,#319367),(#319368,#319369,#319370),(#319371,#319372,#319373),(#319374,
#319375,#319376),(#319377,#319378,#319379),(#319380,#319381,#319382),(#319383,
#319384,#319385),(#319386,#319387,#319388),(#319389,#319390,#319391),(#319392,
#319393,#319394),(#319395,#319396,#319397),(#319398,#319399,#319400),(#319401,
#319402,#319403),(#319404,#319405,#319406),(#319407,#319408,#319409),(#319410,
#319411,#319412),(#319413,#319414,#319415),(#319416,#319417,#319418),(#319419,
#319420,#319421),(#319422,#319423,#319424),(#319425,#319426,#319427),(#319428,
#319429,#319430),(#319431,#319432,#319433),(#319434,#319435,#319436),(#319437,
#319438,#319439),(#319440,#319441,#319442),(#319443,#319444,#319445),(#319446,
#319447,#319448),(#319449,#319450,#319451),(#319452,#319453,#319454),(#319455,
#319456,#319457),(#319458,#319459,#319460),(#319461,#319462,#319463),(#319464,
#319465,#319466),(#319467,#319468,#319469),(#319470,#319471,#319472),(#319473,
#319474,#319475),(#319476,#319477,#319478),(#319479,#319480,#319481),(#319482,
#319483,#319484),(#319485,#319486,#319487),(#319488,#319489,#319490),(#319491,
#319492,#319493),(#319494,#319495,#319496),(#319497,#319498,#319499),(#319500,
#319501,#319502),(#319503,#319504,#319505),(#319506,#319507,#319508),(#319509,
#319510,#319511),(#319512,#319513,#319514),(#319515,#319516,#319517),(#319518,
#319519,#319520),(#319521,#319522,#319523),(#319524,#319525,#319526),(#319527,
#319528,#319529),(#319530,#319531,#319532),(#319533,#319534,#319535),(#319536,
#319537,#319538),(#319539,#319540,#319541),(#319542,#319543,#319544),(#319545,
#319546,#319547),(#319548,#319549,#319550),(#319551,#319552,#319553),(#319554,
#319555,#319556),(#319557,#319558,#319559),(#319560,#319561,#319562),(#319563,
#319564,#319565),(#319566,#319567,#319568),(#319569,#319570,#319571),(#319572,
#319573,#319574),(#319575,#319576,#319577),(#319578,#319579,#319580),(#319581,
#319582,#319583),(#319584,#319585,#319586),(#319587,#319588,#319589),(#319590,
#319591,#319592),(#319593,#319594,#319595),(#319596,#319597,#319598),(#319599,
#319600,#319601),(#319602,#319603,#319604),(#319605,#319606,#319607),(#319608,
#319609,#319610),(#319611,#319612,#319613),(#319614,#319615,#319616),(#319617,
#319618,#319619),(#319620,#319621,#319622),(#319623,#319624,#319625),(#319626,
#319627,#319628),(#319629,#319630,#319631),(#319632,#319633,#319634),(#319635,
#319636,#319637),(#319638,#319639,#319640),(#319641,#319642,#319643),(#319644,
#319645,#319646),(#319647,#319648,#319649),(#319650,#319651,#319652),(#319653,
#319654,#319655),(#319656,#319657,#319658),(#319659,#319660,#319661)),
 .UNSPECIFIED.,.F.,.F.,.F.,(6,1,1,1,1,1,1,1,1,1,1,1,1,1,1,1,1,1,1,1,1,1,
1,1,1,1,1,1,1,1,1,1,1,1,1,1,1,1,1,1,1,1,1,1,1,1,1,1,1,1,1,1,1,1,1,1,1,1,
1,1,1,1,1,1,1,1,1,1,1,1,1,1,1,1,1,1,1,1,1,1,1,1,1,1,1,1,1,1,1,1,1,1,1,1,
1,1,1,1,1,1,1,1,1,1,1,1,1,1,1,1,1,1,1,1,1,1,1,1,1,1,1,1,1,1,1,1,1,1,1,1,
1,1,1,1,1,1,1,1,1,1,1,1,1,1,1,1,1,1,1,1,1,1,1,1,1,1,1,1,1,1,1,1,1,1,1,1,
1,1,1,1,1,1,1,1,1,1,1,1,1,1,1,1,1,1,1,1,1,1,1,1,1,1,1,1,1,1,1,1,1,1,1,1,
1,1,1,1,1,1,1,1,1,1,1,1,1,1,1,1,1,1,1,1,1,1,1,1,1,1,1,1,1,1,1,1,1,1,1,1,
1,1,1,1,1,1,1,1,1,1,1,1,1,1,1,1,1,1,1,1,1,1,1,1,1,1,1,1,1,1,1,1,1,1,1,1,
1,1,1,1,1,1,1,1,1,1,1,1,1,1,1,1,1,1,1,1,1,1,1,1,1,1,1,1,1,1,1,1,1,1,1,1,
1,1,1,1,1,1,1,1,1,1,1,1,1,1,1,1,1,1,1,1,1,1,1,1,1,1,1,1,1,1,1,1,1,1,1,1,
1,1,1,1,1,1,1,1,1,1,1,1,1,1,1,1,1,1,1,1,1,1,1,1,1,1,1,1,1,1,1,1,1,1,1,1,
1,1,1,1,1,1,1,1,1,1,1,1,1,1,1,1,1,1,1,1,1,1,1,1,1,1,1,1,1,1,1,1,1,1,1,1,
1,1,1,1,1,1,1,1,1,1,1,1,1,1,1,1,1,1,1,1,1,1,1,1,1,1,1,1,1,1,1,1,1,1,1,1,
1,1,1,1,1,1,1,1,1,1,1,1,1,1,1,1,1,1,1,1,1,1,1,1,1,1,1,1,1,1,1,1,1,1,1,1,
1,1,1,1,1,1,1,1,1,1,1,1,1,1,1,1,1,1,1,1,1,1,1,1,1,1,1,1,1,1,1,1,1,1,1,1,
1,1,1,1,1,1,1,1,1,1,1,1,1,1,1,1,1,1,1,6),(2,1,2),(-1.,-0.998165138,-0.996330275,
-0.994495413,-0.99266055,-0.990825688,-0.988990826,-0.987155963,-0.985321101,
-0.983486239,-0.981651376,-0.979816514,-0.977981651,-0.976146789,-0.974311927,
-0.972477064,-0.970642202,-0.968807339,-0.966972477,-0.965137615,-0.963302752,
-0.96146789,-0.959633028,-0.957798165,-0.955963303,-0.95412844,-0.952293578,
-0.950458716,-0.948623853,-0.946788991,-0.944954128,-0.943119266,-0.941284404,
-0.939449541,-0.937614679,-0.935779817,-0.933944954,-0.932110092,-0.930275229,
-0.928440367,-0.926605505,-0.924770642,-0.92293578,-0.921100917,-0.919266055,
-0.917431193,-0.91559633,-0.913761468,-0.911926606,-0.910091743,-0.908256881,
-0.906422018,-0.904587156,-0.902752294,-0.900917431,-0.899082569,-0.897247706,
-0.895412844,-0.893577982,-0.891743119,-0.889908257,-0.888073394,-0.886238532,
-0.88440367,-0.882568807,-0.880733945,-0.878899083,-0.87706422,-0.875229358,
-0.873394495,-0.871559633,-0.869724771,-0.867889908,-0.866055046,-0.864220183,
-0.862385321,-0.860550459,-0.858715596,-0.856880734,-0.855045872,-0.853211009,
-0.851376147,-0.849541284,-0.847706422,-0.84587156,-0.844036697,-0.842201835,
-0.840366972,-0.83853211,-0.836697248,-0.834862385,-0.833027523,-0.831192661,
-0.829357798,-0.827522936,-0.825688073,-0.823853211,-0.822018349,-0.820183486,
-0.818348624,-0.816513761,-0.814678899,-0.812844037,-0.811009174,-0.809174312,
-0.80733945,-0.805504587,-0.803669725,-0.801834862,-0.8,-0.798165138,-0.796330275,
-0.794495413,-0.79266055,-0.790825688,-0.788990826,-0.787155963,-0.785321101,
-0.783486239,-0.781651376,-0.779816514,-0.777981651,-0.776146789,-0.774311927,
-0.772477064,-0.770642202,-0.768807339,-0.766972477,-0.765137615,-0.763302752,
-0.76146789,-0.759633028,-0.757798165,-0.755963303,-0.75412844,-0.752293578,
-0.750458716,-0.748623853,-0.746788991,-0.744954128,-0.743119266,-0.741284404,
-0.739449541,-0.737614679,-0.735779817,-0.733944954,-0.732110092,-0.730275229,
-0.728440367,-0.726605505,-0.724770642,-0.72293578,-0.721100917,-0.719266055,
-0.717431193,-0.71559633,-0.713761468,-0.711926606,-0.710091743,-0.708256881,
-0.706422018,-0.704587156,-0.702752294,-0.700917431,-0.699082569,-0.697247706,
-0.695412844,-0.693577982,-0.691743119,-0.689908257,-0.688073394,-0.686238532,
-0.68440367,-0.682568807,-0.680733945,-0.678899083,-0.67706422,-0.675229358,
-0.673394495,-0.671559633,-0.669724771,-0.667889908,-0.666055046,-0.664220183,
-0.662385321,-0.660550459,-0.658715596,-0.656880734,-0.655045872,-0.653211009,
-0.651376147,-0.649541284,-0.647706422,-0.64587156,-0.644036697,-0.642201835,
-0.640366972,-0.63853211,-0.636697248,-0.634862385,-0.633027523,-0.631192661,
-0.629357798,-0.627522936,-0.625688073,-0.623853211,-0.622018349,-0.620183486,
-0.618348624,-0.616513761,-0.614678899,-0.612844037,-0.611009174,-0.609174312,
-0.60733945,-0.605504587,-0.603669725,-0.601834862,-0.6,-0.598165138,-0.596330275,
-0.594495413,-0.59266055,-0.590825688,-0.588990826,-0.587155963,-0.585321101,
-0.583486239,-0.581651376,-0.579816514,-0.577981651,-0.576146789,-0.574311927,
-0.572477064,-0.570642202,-0.568807339,-0.566972477,-0.565137615,-0.563302752,
-0.56146789,-0.559633028,-0.557798165,-0.555963303,-0.55412844,-0.552293578,
-0.550458716,-0.548623853,-0.546788991,-0.544954128,-0.543119266,-0.541284404,
-0.539449541,-0.537614679,-0.535779817,-0.533944954,-0.532110092,-0.530275229,
-0.528440367,-0.526605505,-0.524770642,-0.52293578,-0.521100917,-0.519266055,
-0.517431193,-0.51559633,-0.513761468,-0.511926606,-0.510091743,-0.508256881,
-0.506422018,-0.504587156,-0.502752294,-0.500917431,-0.499082569,-0.497247706,
-0.495412844,-0.493577982,-0.491743119,-0.489908257,-0.488073394,-0.486238532,
-0.48440367,-0.482568807,-0.480733945,-0.478899083,-0.47706422,-0.475229358,
-0.473394495,-0.471559633,-0.469724771,-0.467889908,-0.466055046,-0.464220183,
-0.462385321,-0.460550459,-0.458715596,-0.456880734,-0.455045872,-0.453211009,
-0.451376147,-0.449541284,-0.447706422,-0.44587156,-0.444036697,-0.442201835,
-0.440366972,-0.43853211,-0.436697248,-0.434862385,-0.433027523,-0.431192661,
-0.429357798,-0.427522936,-0.425688073,-0.423853211,-0.422018349,-0.420183486,
-0.418348624,-0.416513761,-0.414678899,-0.412844037,-0.411009174,-0.409174312,
-0.40733945,-0.405504587,-0.403669725,-0.401834862,-0.4,-0.398165138,-0.396330275,
-0.394495413,-0.39266055,-0.390825688,-0.388990826,-0.387155963,-0.385321101,
-0.383486239,-0.381651376,-0.379816514,-0.377981651,-0.376146789,-0.374311927,
-0.372477064,-0.370642202,-0.368807339,-0.366972477,-0.365137615,-0.363302752,
-0.36146789,-0.359633028,-0.357798165,-0.355963303,-0.35412844,-0.352293578,
-0.350458716,-0.348623853,-0.346788991,-0.344954128,-0.343119266,-0.341284404,
-0.339449541,-0.337614679,-0.335779817,-0.333944954,-0.332110092,-0.330275229,
-0.328440367,-0.326605505,-0.324770642,-0.32293578,-0.321100917,-0.319266055,
-0.317431193,-0.31559633,-0.313761468,-0.311926606,-0.310091743,-0.308256881,
-0.306422018,-0.304587156,-0.302752294,-0.300917431,-0.299082569,-0.297247706,
-0.295412844,-0.293577982,-0.291743119,-0.289908257,-0.288073394,-0.286238532,
-0.28440367,-0.282568807,-0.280733945,-0.278899083,-0.27706422,-0.275229358,
-0.273394495,-0.271559633,-0.269724771,-0.267889908,-0.266055046,-0.264220183,
-0.262385321,-0.260550459,-0.258715596,-0.256880734,-0.255045872,-0.253211009,
-0.251376147,-0.249541284,-0.247706422,-0.24587156,-0.244036697,-0.242201835,
-0.240366972,-0.23853211,-0.236697248,-0.234862385,-0.233027523,-0.231192661,
-0.229357798,-0.227522936,-0.225688073,-0.223853211,-0.222018349,-0.220183486,
-0.218348624,-0.216513761,-0.214678899,-0.212844037,-0.211009174,-0.209174312,
-0.20733945,-0.205504587,-0.203669725,-0.201834862,-0.2,-0.198165138,-0.196330275,
-0.194495413,-0.19266055,-0.190825688,-0.188990826,-0.187155963,-0.185321101,
-0.183486239,-0.181651376,-0.179816514,-0.177981651,-0.176146789,-0.174311927,
-0.172477064,-0.170642202,-0.168807339,-0.166972477,-0.165137615,-0.163302752,
-0.16146789,-0.159633028,-0.157798165,-0.155963303,-0.15412844,-0.152293578,
-0.150458716,-0.148623853,-0.146788991,-0.144954128,-0.143119266,-0.141284404,
-0.139449541,-0.137614679,-0.135779817,-0.133944954,-0.132110092,-0.130275229,
-0.128440367,-0.126605505,-0.124770642,-0.12293578,-0.121100917,-0.119266055,
-0.117431193,-0.11559633,-0.113761468,-0.111926606,-0.110091743,-0.108256881,
-0.106422018,-0.104587156,-0.102752294,-0.100917431,-0.099082569,-0.097247706,
-0.095412844,-0.093577982,-0.091743119,-0.089908257,-0.088073394,-0.086238532,
-0.08440367,-0.082568807,-0.080733945,-0.078899083,-0.07706422,-0.075229358,
-0.073394495,-0.071559633,-0.069724771,-0.067889908,-0.066055046,-0.064220183,
-0.062385321,-0.060550459,-0.058715596,-0.056880734,-0.055045872,-0.053211009,
-0.051376147,-0.049541284,-0.047706422,-0.04587156,-0.044036697,-0.042201835,
-0.040366972,-0.03853211,-0.036697248,-0.034862385,-0.033027523,-0.031192661,
-0.029357798,-0.027522936,-0.025688073,-0.023853211,-0.022018349,-0.020183486,
-0.018348624,-0.016513761,-0.014678899,-0.012844037,-0.011009174,-0.009174312,
-0.00733945,-0.005504587,-0.003669725,-0.001834862,0.000982134),(0.3,1.,
1.3),.UNSPECIFIED.);
#6314=B_SPLINE_SURFACE_WITH_KNOTS('',5,1,((#319684,#319685,#319686),(#319687,
#319688,#319689),(#319690,#319691,#319692),(#319693,#319694,#319695),(#319696,
#319697,#319698),(#319699,#319700,#319701),(#319702,#319703,#319704),(#319705,
#319706,#319707),(#319708,#319709,#319710),(#319711,#319712,#319713),(#319714,
#319715,#319716),(#319717,#319718,#319719),(#319720,#319721,#319722),(#319723,
#319724,#319725),(#319726,#319727,#319728),(#319729,#319730,#319731),(#319732,
#319733,#319734),(#319735,#319736,#319737),(#319738,#319739,#319740),(#319741,
#319742,#319743),(#319744,#319745,#319746),(#319747,#319748,#319749),(#319750,
#319751,#319752),(#319753,#319754,#319755),(#319756,#319757,#319758),(#319759,
#319760,#319761),(#319762,#319763,#319764),(#319765,#319766,#319767),(#319768,
#319769,#319770),(#319771,#319772,#319773),(#319774,#319775,#319776),(#319777,
#319778,#319779),(#319780,#319781,#319782),(#319783,#319784,#319785),(#319786,
#319787,#319788),(#319789,#319790,#319791),(#319792,#319793,#319794),(#319795,
#319796,#319797),(#319798,#319799,#319800),(#319801,#319802,#319803),(#319804,
#319805,#319806),(#319807,#319808,#319809),(#319810,#319811,#319812),(#319813,
#319814,#319815),(#319816,#319817,#319818),(#319819,#319820,#319821),(#319822,
#319823,#319824),(#319825,#319826,#319827),(#319828,#319829,#319830),(#319831,
#319832,#319833),(#319834,#319835,#319836),(#319837,#319838,#319839),(#319840,
#319841,#319842),(#319843,#319844,#319845),(#319846,#319847,#319848),(#319849,
#319850,#319851),(#319852,#319853,#319854),(#319855,#319856,#319857),(#319858,
#319859,#319860),(#319861,#319862,#319863),(#319864,#319865,#319866),(#319867,
#319868,#319869),(#319870,#319871,#319872),(#319873,#319874,#319875),(#319876,
#319877,#319878),(#319879,#319880,#319881),(#319882,#319883,#319884),(#319885,
#319886,#319887),(#319888,#319889,#319890),(#319891,#319892,#319893),(#319894,
#319895,#319896),(#319897,#319898,#319899),(#319900,#319901,#319902),(#319903,
#319904,#319905),(#319906,#319907,#319908),(#319909,#319910,#319911),(#319912,
#319913,#319914),(#319915,#319916,#319917),(#319918,#319919,#319920),(#319921,
#319922,#319923),(#319924,#319925,#319926),(#319927,#319928,#319929),(#319930,
#319931,#319932),(#319933,#319934,#319935),(#319936,#319937,#319938),(#319939,
#319940,#319941),(#319942,#319943,#319944),(#319945,#319946,#319947),(#319948,
#319949,#319950),(#319951,#319952,#319953),(#319954,#319955,#319956),(#319957,
#319958,#319959),(#319960,#319961,#319962),(#319963,#319964,#319965),(#319966,
#319967,#319968),(#319969,#319970,#319971),(#319972,#319973,#319974),(#319975,
#319976,#319977),(#319978,#319979,#319980),(#319981,#319982,#319983),(#319984,
#319985,#319986),(#319987,#319988,#319989),(#319990,#319991,#319992),(#319993,
#319994,#319995),(#319996,#319997,#319998),(#319999,#320000,#320001),(#320002,
#320003,#320004),(#320005,#320006,#320007),(#320008,#320009,#320010),(#320011,
#320012,#320013),(#320014,#320015,#320016),(#320017,#320018,#320019),(#320020,
#320021,#320022),(#320023,#320024,#320025),(#320026,#320027,#320028),(#320029,
#320030,#320031),(#320032,#320033,#320034),(#320035,#320036,#320037),(#320038,
#320039,#320040),(#320041,#320042,#320043),(#320044,#320045,#320046),(#320047,
#320048,#320049),(#320050,#320051,#320052),(#320053,#320054,#320055),(#320056,
#320057,#320058),(#320059,#320060,#320061),(#320062,#320063,#320064),(#320065,
#320066,#320067),(#320068,#320069,#320070),(#320071,#320072,#320073),(#320074,
#320075,#320076),(#320077,#320078,#320079),(#320080,#320081,#320082),(#320083,
#320084,#320085),(#320086,#320087,#320088),(#320089,#320090,#320091),(#320092,
#320093,#320094),(#320095,#320096,#320097),(#320098,#320099,#320100),(#320101,
#320102,#320103),(#320104,#320105,#320106),(#320107,#320108,#320109),(#320110,
#320111,#320112),(#320113,#320114,#320115),(#320116,#320117,#320118),(#320119,
#320120,#320121),(#320122,#320123,#320124),(#320125,#320126,#320127),(#320128,
#320129,#320130),(#320131,#320132,#320133),(#320134,#320135,#320136),(#320137,
#320138,#320139),(#320140,#320141,#320142),(#320143,#320144,#320145),(#320146,
#320147,#320148),(#320149,#320150,#320151),(#320152,#320153,#320154),(#320155,
#320156,#320157),(#320158,#320159,#320160),(#320161,#320162,#320163),(#320164,
#320165,#320166),(#320167,#320168,#320169),(#320170,#320171,#320172),(#320173,
#320174,#320175),(#320176,#320177,#320178),(#320179,#320180,#320181),(#320182,
#320183,#320184),(#320185,#320186,#320187),(#320188,#320189,#320190),(#320191,
#320192,#320193),(#320194,#320195,#320196),(#320197,#320198,#320199),(#320200,
#320201,#320202),(#320203,#320204,#320205),(#320206,#320207,#320208),(#320209,
#320210,#320211),(#320212,#320213,#320214),(#320215,#320216,#320217),(#320218,
#320219,#320220),(#320221,#320222,#320223),(#320224,#320225,#320226),(#320227,
#320228,#320229),(#320230,#320231,#320232),(#320233,#320234,#320235),(#320236,
#320237,#320238),(#320239,#320240,#320241),(#320242,#320243,#320244),(#320245,
#320246,#320247),(#320248,#320249,#320250),(#320251,#320252,#320253),(#320254,
#320255,#320256),(#320257,#320258,#320259),(#320260,#320261,#320262),(#320263,
#320264,#320265),(#320266,#320267,#320268),(#320269,#320270,#320271),(#320272,
#320273,#320274),(#320275,#320276,#320277),(#320278,#320279,#320280),(#320281,
#320282,#320283),(#320284,#320285,#320286),(#320287,#320288,#320289),(#320290,
#320291,#320292),(#320293,#320294,#320295),(#320296,#320297,#320298),(#320299,
#320300,#320301),(#320302,#320303,#320304),(#320305,#320306,#320307),(#320308,
#320309,#320310),(#320311,#320312,#320313),(#320314,#320315,#320316),(#320317,
#320318,#320319),(#320320,#320321,#320322),(#320323,#320324,#320325),(#320326,
#320327,#320328),(#320329,#320330,#320331),(#320332,#320333,#320334),(#320335,
#320336,#320337),(#320338,#320339,#320340),(#320341,#320342,#320343),(#320344,
#320345,#320346),(#320347,#320348,#320349),(#320350,#320351,#320352),(#320353,
#320354,#320355),(#320356,#320357,#320358),(#320359,#320360,#320361),(#320362,
#320363,#320364),(#320365,#320366,#320367),(#320368,#320369,#320370),(#320371,
#320372,#320373),(#320374,#320375,#320376),(#320377,#320378,#320379),(#320380,
#320381,#320382),(#320383,#320384,#320385),(#320386,#320387,#320388),(#320389,
#320390,#320391),(#320392,#320393,#320394),(#320395,#320396,#320397),(#320398,
#320399,#320400),(#320401,#320402,#320403),(#320404,#320405,#320406),(#320407,
#320408,#320409),(#320410,#320411,#320412),(#320413,#320414,#320415),(#320416,
#320417,#320418),(#320419,#320420,#320421),(#320422,#320423,#320424),(#320425,
#320426,#320427),(#320428,#320429,#320430),(#320431,#320432,#320433),(#320434,
#320435,#320436),(#320437,#320438,#320439),(#320440,#320441,#320442),(#320443,
#320444,#320445),(#320446,#320447,#320448),(#320449,#320450,#320451),(#320452,
#320453,#320454),(#320455,#320456,#320457),(#320458,#320459,#320460),(#320461,
#320462,#320463),(#320464,#320465,#320466),(#320467,#320468,#320469),(#320470,
#320471,#320472),(#320473,#320474,#320475),(#320476,#320477,#320478),(#320479,
#320480,#320481),(#320482,#320483,#320484),(#320485,#320486,#320487),(#320488,
#320489,#320490),(#320491,#320492,#320493),(#320494,#320495,#320496),(#320497,
#320498,#320499),(#320500,#320501,#320502),(#320503,#320504,#320505),(#320506,
#320507,#320508),(#320509,#320510,#320511),(#320512,#320513,#320514),(#320515,
#320516,#320517),(#320518,#320519,#320520),(#320521,#320522,#320523),(#320524,
#320525,#320526),(#320527,#320528,#320529),(#320530,#320531,#320532),(#320533,
#320534,#320535),(#320536,#320537,#320538),(#320539,#320540,#320541),(#320542,
#320543,#320544),(#320545,#320546,#320547),(#320548,#320549,#320550),(#320551,
#320552,#320553),(#320554,#320555,#320556),(#320557,#320558,#320559),(#320560,
#320561,#320562),(#320563,#320564,#320565),(#320566,#320567,#320568),(#320569,
#320570,#320571),(#320572,#320573,#320574),(#320575,#320576,#320577),(#320578,
#320579,#320580),(#320581,#320582,#320583),(#320584,#320585,#320586),(#320587,
#320588,#320589),(#320590,#320591,#320592),(#320593,#320594,#320595),(#320596,
#320597,#320598),(#320599,#320600,#320601),(#320602,#320603,#320604),(#320605,
#320606,#320607),(#320608,#320609,#320610),(#320611,#320612,#320613),(#320614,
#320615,#320616),(#320617,#320618,#320619),(#320620,#320621,#320622),(#320623,
#320624,#320625),(#320626,#320627,#320628),(#320629,#320630,#320631),(#320632,
#320633,#320634),(#320635,#320636,#320637),(#320638,#320639,#320640),(#320641,
#320642,#320643),(#320644,#320645,#320646),(#320647,#320648,#320649),(#320650,
#320651,#320652),(#320653,#320654,#320655),(#320656,#320657,#320658),(#320659,
#320660,#320661),(#320662,#320663,#320664),(#320665,#320666,#320667),(#320668,
#320669,#320670),(#320671,#320672,#320673),(#320674,#320675,#320676),(#320677,
#320678,#320679),(#320680,#320681,#320682),(#320683,#320684,#320685),(#320686,
#320687,#320688),(#320689,#320690,#320691),(#320692,#320693,#320694),(#320695,
#320696,#320697),(#320698,#320699,#320700),(#320701,#320702,#320703),(#320704,
#320705,#320706),(#320707,#320708,#320709),(#320710,#320711,#320712),(#320713,
#320714,#320715),(#320716,#320717,#320718),(#320719,#320720,#320721),(#320722,
#320723,#320724),(#320725,#320726,#320727),(#320728,#320729,#320730),(#320731,
#320732,#320733),(#320734,#320735,#320736),(#320737,#320738,#320739),(#320740,
#320741,#320742),(#320743,#320744,#320745),(#320746,#320747,#320748),(#320749,
#320750,#320751),(#320752,#320753,#320754),(#320755,#320756,#320757),(#320758,
#320759,#320760),(#320761,#320762,#320763),(#320764,#320765,#320766),(#320767,
#320768,#320769),(#320770,#320771,#320772),(#320773,#320774,#320775),(#320776,
#320777,#320778),(#320779,#320780,#320781),(#320782,#320783,#320784),(#320785,
#320786,#320787),(#320788,#320789,#320790),(#320791,#320792,#320793),(#320794,
#320795,#320796),(#320797,#320798,#320799),(#320800,#320801,#320802),(#320803,
#320804,#320805),(#320806,#320807,#320808),(#320809,#320810,#320811),(#320812,
#320813,#320814),(#320815,#320816,#320817),(#320818,#320819,#320820),(#320821,
#320822,#320823),(#320824,#320825,#320826),(#320827,#320828,#320829),(#320830,
#320831,#320832),(#320833,#320834,#320835),(#320836,#320837,#320838),(#320839,
#320840,#320841),(#320842,#320843,#320844),(#320845,#320846,#320847),(#320848,
#320849,#320850),(#320851,#320852,#320853),(#320854,#320855,#320856),(#320857,
#320858,#320859),(#320860,#320861,#320862),(#320863,#320864,#320865),(#320866,
#320867,#320868),(#320869,#320870,#320871),(#320872,#320873,#320874),(#320875,
#320876,#320877),(#320878,#320879,#320880),(#320881,#320882,#320883),(#320884,
#320885,#320886),(#320887,#320888,#320889),(#320890,#320891,#320892),(#320893,
#320894,#320895),(#320896,#320897,#320898),(#320899,#320900,#320901),(#320902,
#320903,#320904),(#320905,#320906,#320907),(#320908,#320909,#320910),(#320911,
#320912,#320913),(#320914,#320915,#320916),(#320917,#320918,#320919),(#320920,
#320921,#320922),(#320923,#320924,#320925),(#320926,#320927,#320928),(#320929,
#320930,#320931),(#320932,#320933,#320934),(#320935,#320936,#320937),(#320938,
#320939,#320940),(#320941,#320942,#320943),(#320944,#320945,#320946),(#320947,
#320948,#320949),(#320950,#320951,#320952),(#320953,#320954,#320955),(#320956,
#320957,#320958),(#320959,#320960,#320961),(#320962,#320963,#320964),(#320965,
#320966,#320967),(#320968,#320969,#320970),(#320971,#320972,#320973),(#320974,
#320975,#320976),(#320977,#320978,#320979),(#320980,#320981,#320982),(#320983,
#320984,#320985),(#320986,#320987,#320988),(#320989,#320990,#320991),(#320992,
#320993,#320994),(#320995,#320996,#320997),(#320998,#320999,#321000),(#321001,
#321002,#321003),(#321004,#321005,#321006),(#321007,#321008,#321009),(#321010,
#321011,#321012),(#321013,#321014,#321015),(#321016,#321017,#321018),(#321019,
#321020,#321021),(#321022,#321023,#321024),(#321025,#321026,#321027),(#321028,
#321029,#321030),(#321031,#321032,#321033),(#321034,#321035,#321036),(#321037,
#321038,#321039),(#321040,#321041,#321042),(#321043,#321044,#321045),(#321046,
#321047,#321048),(#321049,#321050,#321051),(#321052,#321053,#321054),(#321055,
#321056,#321057),(#321058,#321059,#321060),(#321061,#321062,#321063),(#321064,
#321065,#321066),(#321067,#321068,#321069),(#321070,#321071,#321072),(#321073,
#321074,#321075),(#321076,#321077,#321078),(#321079,#321080,#321081),(#321082,
#321083,#321084),(#321085,#321086,#321087),(#321088,#321089,#321090),(#321091,
#321092,#321093),(#321094,#321095,#321096),(#321097,#321098,#321099),(#321100,
#321101,#321102),(#321103,#321104,#321105),(#321106,#321107,#321108),(#321109,
#321110,#321111),(#321112,#321113,#321114),(#321115,#321116,#321117),(#321118,
#321119,#321120),(#321121,#321122,#321123),(#321124,#321125,#321126),(#321127,
#321128,#321129),(#321130,#321131,#321132),(#321133,#321134,#321135),(#321136,
#321137,#321138),(#321139,#321140,#321141),(#321142,#321143,#321144),(#321145,
#321146,#321147),(#321148,#321149,#321150),(#321151,#321152,#321153),(#321154,
#321155,#321156),(#321157,#321158,#321159),(#321160,#321161,#321162),(#321163,
#321164,#321165),(#321166,#321167,#321168),(#321169,#321170,#321171),(#321172,
#321173,#321174),(#321175,#321176,#321177),(#321178,#321179,#321180),(#321181,
#321182,#321183),(#321184,#321185,#321186),(#321187,#321188,#321189),(#321190,
#321191,#321192),(#321193,#321194,#321195),(#321196,#321197,#321198),(#321199,
#321200,#321201),(#321202,#321203,#321204),(#321205,#321206,#321207),(#321208,
#321209,#321210),(#321211,#321212,#321213),(#321214,#321215,#321216),(#321217,
#321218,#321219),(#321220,#321221,#321222),(#321223,#321224,#321225),(#321226,
#321227,#321228),(#321229,#321230,#321231),(#321232,#321233,#321234),(#321235,
#321236,#321237),(#321238,#321239,#321240),(#321241,#321242,#321243),(#321244,
#321245,#321246),(#321247,#321248,#321249),(#321250,#321251,#321252),(#321253,
#321254,#321255),(#321256,#321257,#321258),(#321259,#321260,#321261),(#321262,
#321263,#321264),(#321265,#321266,#321267),(#321268,#321269,#321270),(#321271,
#321272,#321273),(#321274,#321275,#321276),(#321277,#321278,#321279),(#321280,
#321281,#321282),(#321283,#321284,#321285),(#321286,#321287,#321288),(#321289,
#321290,#321291),(#321292,#321293,#321294),(#321295,#321296,#321297),(#321298,
#321299,#321300),(#321301,#321302,#321303),(#321304,#321305,#321306),(#321307,
#321308,#321309),(#321310,#321311,#321312),(#321313,#321314,#321315),(#321316,
#321317,#321318),(#321319,#321320,#321321),(#321322,#321323,#321324),(#321325,
#321326,#321327),(#321328,#321329,#321330),(#321331,#321332,#321333),(#321334,
#321335,#321336)),.UNSPECIFIED.,.F.,.F.,.F.,(6,1,1,1,1,1,1,1,1,1,1,1,1,
1,1,1,1,1,1,1,1,1,1,1,1,1,1,1,1,1,1,1,1,1,1,1,1,1,1,1,1,1,1,1,1,1,1,1,1,
1,1,1,1,1,1,1,1,1,1,1,1,1,1,1,1,1,1,1,1,1,1,1,1,1,1,1,1,1,1,1,1,1,1,1,1,
1,1,1,1,1,1,1,1,1,1,1,1,1,1,1,1,1,1,1,1,1,1,1,1,1,1,1,1,1,1,1,1,1,1,1,1,
1,1,1,1,1,1,1,1,1,1,1,1,1,1,1,1,1,1,1,1,1,1,1,1,1,1,1,1,1,1,1,1,1,1,1,1,
1,1,1,1,1,1,1,1,1,1,1,1,1,1,1,1,1,1,1,1,1,1,1,1,1,1,1,1,1,1,1,1,1,1,1,1,
1,1,1,1,1,1,1,1,1,1,1,1,1,1,1,1,1,1,1,1,1,1,1,1,1,1,1,1,1,1,1,1,1,1,1,1,
1,1,1,1,1,1,1,1,1,1,1,1,1,1,1,1,1,1,1,1,1,1,1,1,1,1,1,1,1,1,1,1,1,1,1,1,
1,1,1,1,1,1,1,1,1,1,1,1,1,1,1,1,1,1,1,1,1,1,1,1,1,1,1,1,1,1,1,1,1,1,1,1,
1,1,1,1,1,1,1,1,1,1,1,1,1,1,1,1,1,1,1,1,1,1,1,1,1,1,1,1,1,1,1,1,1,1,1,1,
1,1,1,1,1,1,1,1,1,1,1,1,1,1,1,1,1,1,1,1,1,1,1,1,1,1,1,1,1,1,1,1,1,1,1,1,
1,1,1,1,1,1,1,1,1,1,1,1,1,1,1,1,1,1,1,1,1,1,1,1,1,1,1,1,1,1,1,1,1,1,1,1,
1,1,1,1,1,1,1,1,1,1,1,1,1,1,1,1,1,1,1,1,1,1,1,1,1,1,1,1,1,1,1,1,1,1,1,1,
1,1,1,1,1,1,1,1,1,1,1,1,1,1,1,1,1,1,1,1,1,1,1,1,1,1,1,1,1,1,1,1,1,1,1,1,
1,1,1,1,1,1,1,1,1,1,1,1,1,1,1,1,1,1,1,1,1,1,1,1,1,1,1,1,1,1,1,1,1,1,1,1,
1,1,1,1,1,1,1,1,1,1,1,1,1,1,1,1,1,1,1,1,1,1,1,1,1,1,1,1,1,6),(2,1,2),(-0.00196418,
0.,0.001834862,0.003669725,0.005504587,0.00733945,0.009174312,0.011009174,
0.012844037,0.014678899,0.016513761,0.018348624,0.020183486,0.022018349,
0.023853211,0.025688073,0.027522936,0.029357798,0.031192661,0.033027523,
0.034862385,0.036697248,0.03853211,0.040366972,0.042201835,0.044036697,
0.04587156,0.047706422,0.049541284,0.051376147,0.053211009,0.055045872,
0.056880734,0.058715596,0.060550459,0.062385321,0.064220183,0.066055046,
0.067889908,0.069724771,0.071559633,0.073394495,0.075229358,0.07706422,
0.078899083,0.080733945,0.082568807,0.08440367,0.086238532,0.088073394,
0.089908257,0.091743119,0.093577982,0.095412844,0.097247706,0.099082569,
0.100917431,0.102752294,0.104587156,0.106422018,0.108256881,0.110091743,
0.111926606,0.113761468,0.11559633,0.117431193,0.119266055,0.121100917,
0.12293578,0.124770642,0.126605505,0.128440367,0.130275229,0.132110092,
0.133944954,0.135779817,0.137614679,0.139449541,0.141284404,0.143119266,
0.144954128,0.146788991,0.148623853,0.150458716,0.152293578,0.15412844,
0.155963303,0.157798165,0.159633028,0.16146789,0.163302752,0.165137615,
0.166972477,0.168807339,0.170642202,0.172477064,0.174311927,0.176146789,
0.177981651,0.179816514,0.181651376,0.183486239,0.185321101,0.187155963,
0.188990826,0.190825688,0.19266055,0.194495413,0.196330275,0.198165138,
0.2,0.201834862,0.203669725,0.205504587,0.20733945,0.209174312,0.211009174,
0.212844037,0.214678899,0.216513761,0.218348624,0.220183486,0.222018349,
0.223853211,0.225688073,0.227522936,0.229357798,0.231192661,0.233027523,
0.234862385,0.236697248,0.23853211,0.240366972,0.242201835,0.244036697,
0.24587156,0.247706422,0.249541284,0.251376147,0.253211009,0.255045872,
0.256880734,0.258715596,0.260550459,0.262385321,0.264220183,0.266055046,
0.267889908,0.269724771,0.271559633,0.273394495,0.275229358,0.27706422,
0.278899083,0.280733945,0.282568807,0.28440367,0.286238532,0.288073394,
0.289908257,0.291743119,0.293577982,0.295412844,0.297247706,0.299082569,
0.300917431,0.302752294,0.304587156,0.306422018,0.308256881,0.310091743,
0.311926606,0.313761468,0.31559633,0.317431193,0.319266055,0.321100917,
0.32293578,0.324770642,0.326605505,0.328440367,0.330275229,0.332110092,
0.333944954,0.335779817,0.337614679,0.339449541,0.341284404,0.343119266,
0.344954128,0.346788991,0.348623853,0.350458716,0.352293578,0.35412844,
0.355963303,0.357798165,0.359633028,0.36146789,0.363302752,0.365137615,
0.366972477,0.368807339,0.370642202,0.372477064,0.374311927,0.376146789,
0.377981651,0.379816514,0.381651376,0.383486239,0.385321101,0.387155963,
0.388990826,0.390825688,0.39266055,0.394495413,0.396330275,0.398165138,
0.4,0.401834862,0.403669725,0.405504587,0.40733945,0.409174312,0.411009174,
0.412844037,0.414678899,0.416513761,0.418348624,0.420183486,0.422018349,
0.423853211,0.425688073,0.427522936,0.429357798,0.431192661,0.433027523,
0.434862385,0.436697248,0.43853211,0.440366972,0.442201835,0.444036697,
0.44587156,0.447706422,0.449541284,0.451376147,0.453211009,0.455045872,
0.456880734,0.458715596,0.460550459,0.462385321,0.464220183,0.466055046,
0.467889908,0.469724771,0.471559633,0.473394495,0.475229358,0.47706422,
0.478899083,0.480733945,0.482568807,0.48440367,0.486238532,0.488073394,
0.489908257,0.491743119,0.493577982,0.495412844,0.497247706,0.499082569,
0.500917431,0.502752294,0.504587156,0.506422018,0.508256881,0.510091743,
0.511926606,0.513761468,0.51559633,0.517431193,0.519266055,0.521100917,
0.52293578,0.524770642,0.526605505,0.528440367,0.530275229,0.532110092,
0.533944954,0.535779817,0.537614679,0.539449541,0.541284404,0.543119266,
0.544954128,0.546788991,0.548623853,0.550458716,0.552293578,0.55412844,
0.555963303,0.557798165,0.559633028,0.56146789,0.563302752,0.565137615,
0.566972477,0.568807339,0.570642202,0.572477064,0.574311927,0.576146789,
0.577981651,0.579816514,0.581651376,0.583486239,0.585321101,0.587155963,
0.588990826,0.590825688,0.59266055,0.594495413,0.596330275,0.598165138,
0.6,0.601834862,0.603669725,0.605504587,0.60733945,0.609174312,0.611009174,
0.612844037,0.614678899,0.616513761,0.618348624,0.620183486,0.622018349,
0.623853211,0.625688073,0.627522936,0.629357798,0.631192661,0.633027523,
0.634862385,0.636697248,0.63853211,0.640366972,0.642201835,0.644036697,
0.64587156,0.647706422,0.649541284,0.651376147,0.653211009,0.655045872,
0.656880734,0.658715596,0.660550459,0.662385321,0.664220183,0.666055046,
0.667889908,0.669724771,0.671559633,0.673394495,0.675229358,0.67706422,
0.678899083,0.680733945,0.682568807,0.68440367,0.686238532,0.688073394,
0.689908257,0.691743119,0.693577982,0.695412844,0.697247706,0.699082569,
0.700917431,0.702752294,0.704587156,0.706422018,0.708256881,0.710091743,
0.711926606,0.713761468,0.71559633,0.717431193,0.719266055,0.721100917,
0.72293578,0.724770642,0.726605505,0.728440367,0.730275229,0.732110092,
0.733944954,0.735779817,0.737614679,0.739449541,0.741284404,0.743119266,
0.744954128,0.746788991,0.748623853,0.750458716,0.752293578,0.75412844,
0.755963303,0.757798165,0.759633028,0.76146789,0.763302752,0.765137615,
0.766972477,0.768807339,0.770642202,0.772477064,0.774311927,0.776146789,
0.777981651,0.779816514,0.781651376,0.783486239,0.785321101,0.787155963,
0.788990826,0.790825688,0.79266055,0.794495413,0.796330275,0.798165138,
0.8,0.801834862,0.803669725,0.805504587,0.80733945,0.809174312,0.811009174,
0.812844037,0.814678899,0.816513761,0.818348624,0.820183486,0.822018349,
0.823853211,0.825688073,0.827522936,0.829357798,0.831192661,0.833027523,
0.834862385,0.836697248,0.83853211,0.840366972,0.842201835,0.844036697,
0.84587156,0.847706422,0.849541284,0.851376147,0.853211009,0.855045872,
0.856880734,0.858715596,0.860550459,0.862385321,0.864220183,0.866055046,
0.867889908,0.869724771,0.871559633,0.873394495,0.875229358,0.87706422,
0.878899083,0.880733945,0.882568807,0.88440367,0.886238532,0.888073394,
0.889908257,0.891743119,0.893577982,0.895412844,0.897247706,0.899082569,
0.900917431,0.902752294,0.904587156,0.906422018,0.908256881,0.910091743,
0.911926606,0.913761468,0.91559633,0.917431193,0.919266055,0.921100917,
0.92293578,0.924770642,0.926605505,0.928440367,0.930275229,0.932110092,
0.933944954,0.935779817,0.937614679,0.939449541,0.941284404,0.943119266,
0.944954128,0.946788991,0.948623853,0.950458716,0.952293578,0.95412844,
0.955963303,0.957798165,0.959633028,0.96146789,0.963302752,0.965137615,
0.966972477,0.968807339,0.970642202,0.972477064,0.974311927,0.976146789,
0.977981651,0.979816514,0.981651376,0.983486239,0.985321101,0.987155963,
0.988990826,0.990825688,0.99266055,0.994495413,0.996330275,0.998165138,
1.),(0.3,1.,1.3),.UNSPECIFIED.);
#6315=B_SPLINE_SURFACE_WITH_KNOTS('',5,1,((#321359,#321360,#321361),(#321362,
#321363,#321364),(#321365,#321366,#321367),(#321368,#321369,#321370),(#321371,
#321372,#321373),(#321374,#321375,#321376),(#321377,#321378,#321379),(#321380,
#321381,#321382),(#321383,#321384,#321385),(#321386,#321387,#321388),(#321389,
#321390,#321391),(#321392,#321393,#321394),(#321395,#321396,#321397),(#321398,
#321399,#321400),(#321401,#321402,#321403),(#321404,#321405,#321406),(#321407,
#321408,#321409),(#321410,#321411,#321412),(#321413,#321414,#321415),(#321416,
#321417,#321418),(#321419,#321420,#321421),(#321422,#321423,#321424),(#321425,
#321426,#321427),(#321428,#321429,#321430),(#321431,#321432,#321433),(#321434,
#321435,#321436),(#321437,#321438,#321439),(#321440,#321441,#321442),(#321443,
#321444,#321445),(#321446,#321447,#321448),(#321449,#321450,#321451),(#321452,
#321453,#321454),(#321455,#321456,#321457),(#321458,#321459,#321460),(#321461,
#321462,#321463),(#321464,#321465,#321466),(#321467,#321468,#321469),(#321470,
#321471,#321472),(#321473,#321474,#321475),(#321476,#321477,#321478),(#321479,
#321480,#321481),(#321482,#321483,#321484),(#321485,#321486,#321487),(#321488,
#321489,#321490),(#321491,#321492,#321493),(#321494,#321495,#321496),(#321497,
#321498,#321499),(#321500,#321501,#321502),(#321503,#321504,#321505),(#321506,
#321507,#321508),(#321509,#321510,#321511),(#321512,#321513,#321514),(#321515,
#321516,#321517),(#321518,#321519,#321520),(#321521,#321522,#321523),(#321524,
#321525,#321526),(#321527,#321528,#321529),(#321530,#321531,#321532),(#321533,
#321534,#321535),(#321536,#321537,#321538),(#321539,#321540,#321541),(#321542,
#321543,#321544),(#321545,#321546,#321547),(#321548,#321549,#321550),(#321551,
#321552,#321553),(#321554,#321555,#321556),(#321557,#321558,#321559),(#321560,
#321561,#321562),(#321563,#321564,#321565),(#321566,#321567,#321568),(#321569,
#321570,#321571),(#321572,#321573,#321574),(#321575,#321576,#321577),(#321578,
#321579,#321580),(#321581,#321582,#321583),(#321584,#321585,#321586),(#321587,
#321588,#321589),(#321590,#321591,#321592),(#321593,#321594,#321595),(#321596,
#321597,#321598),(#321599,#321600,#321601),(#321602,#321603,#321604),(#321605,
#321606,#321607),(#321608,#321609,#321610),(#321611,#321612,#321613),(#321614,
#321615,#321616),(#321617,#321618,#321619),(#321620,#321621,#321622),(#321623,
#321624,#321625),(#321626,#321627,#321628),(#321629,#321630,#321631),(#321632,
#321633,#321634),(#321635,#321636,#321637),(#321638,#321639,#321640),(#321641,
#321642,#321643),(#321644,#321645,#321646),(#321647,#321648,#321649),(#321650,
#321651,#321652),(#321653,#321654,#321655),(#321656,#321657,#321658),(#321659,
#321660,#321661),(#321662,#321663,#321664),(#321665,#321666,#321667),(#321668,
#321669,#321670),(#321671,#321672,#321673),(#321674,#321675,#321676),(#321677,
#321678,#321679),(#321680,#321681,#321682),(#321683,#321684,#321685),(#321686,
#321687,#321688),(#321689,#321690,#321691),(#321692,#321693,#321694),(#321695,
#321696,#321697),(#321698,#321699,#321700),(#321701,#321702,#321703),(#321704,
#321705,#321706),(#321707,#321708,#321709),(#321710,#321711,#321712),(#321713,
#321714,#321715),(#321716,#321717,#321718),(#321719,#321720,#321721),(#321722,
#321723,#321724),(#321725,#321726,#321727),(#321728,#321729,#321730),(#321731,
#321732,#321733),(#321734,#321735,#321736),(#321737,#321738,#321739),(#321740,
#321741,#321742),(#321743,#321744,#321745),(#321746,#321747,#321748),(#321749,
#321750,#321751),(#321752,#321753,#321754),(#321755,#321756,#321757),(#321758,
#321759,#321760),(#321761,#321762,#321763),(#321764,#321765,#321766),(#321767,
#321768,#321769),(#321770,#321771,#321772),(#321773,#321774,#321775),(#321776,
#321777,#321778),(#321779,#321780,#321781),(#321782,#321783,#321784),(#321785,
#321786,#321787),(#321788,#321789,#321790),(#321791,#321792,#321793),(#321794,
#321795,#321796),(#321797,#321798,#321799),(#321800,#321801,#321802),(#321803,
#321804,#321805),(#321806,#321807,#321808),(#321809,#321810,#321811),(#321812,
#321813,#321814),(#321815,#321816,#321817),(#321818,#321819,#321820),(#321821,
#321822,#321823),(#321824,#321825,#321826),(#321827,#321828,#321829),(#321830,
#321831,#321832),(#321833,#321834,#321835),(#321836,#321837,#321838),(#321839,
#321840,#321841),(#321842,#321843,#321844),(#321845,#321846,#321847),(#321848,
#321849,#321850),(#321851,#321852,#321853),(#321854,#321855,#321856),(#321857,
#321858,#321859),(#321860,#321861,#321862),(#321863,#321864,#321865),(#321866,
#321867,#321868),(#321869,#321870,#321871),(#321872,#321873,#321874),(#321875,
#321876,#321877),(#321878,#321879,#321880),(#321881,#321882,#321883),(#321884,
#321885,#321886),(#321887,#321888,#321889),(#321890,#321891,#321892),(#321893,
#321894,#321895),(#321896,#321897,#321898),(#321899,#321900,#321901),(#321902,
#321903,#321904),(#321905,#321906,#321907),(#321908,#321909,#321910),(#321911,
#321912,#321913),(#321914,#321915,#321916),(#321917,#321918,#321919),(#321920,
#321921,#321922),(#321923,#321924,#321925),(#321926,#321927,#321928),(#321929,
#321930,#321931),(#321932,#321933,#321934),(#321935,#321936,#321937),(#321938,
#321939,#321940),(#321941,#321942,#321943),(#321944,#321945,#321946),(#321947,
#321948,#321949),(#321950,#321951,#321952),(#321953,#321954,#321955),(#321956,
#321957,#321958),(#321959,#321960,#321961),(#321962,#321963,#321964),(#321965,
#321966,#321967),(#321968,#321969,#321970),(#321971,#321972,#321973),(#321974,
#321975,#321976),(#321977,#321978,#321979),(#321980,#321981,#321982),(#321983,
#321984,#321985),(#321986,#321987,#321988),(#321989,#321990,#321991),(#321992,
#321993,#321994),(#321995,#321996,#321997),(#321998,#321999,#322000),(#322001,
#322002,#322003),(#322004,#322005,#322006),(#322007,#322008,#322009),(#322010,
#322011,#322012),(#322013,#322014,#322015),(#322016,#322017,#322018),(#322019,
#322020,#322021),(#322022,#322023,#322024),(#322025,#322026,#322027),(#322028,
#322029,#322030),(#322031,#322032,#322033),(#322034,#322035,#322036),(#322037,
#322038,#322039),(#322040,#322041,#322042),(#322043,#322044,#322045),(#322046,
#322047,#322048),(#322049,#322050,#322051),(#322052,#322053,#322054),(#322055,
#322056,#322057),(#322058,#322059,#322060),(#322061,#322062,#322063),(#322064,
#322065,#322066),(#322067,#322068,#322069),(#322070,#322071,#322072),(#322073,
#322074,#322075),(#322076,#322077,#322078),(#322079,#322080,#322081),(#322082,
#322083,#322084),(#322085,#322086,#322087),(#322088,#322089,#322090),(#322091,
#322092,#322093),(#322094,#322095,#322096),(#322097,#322098,#322099),(#322100,
#322101,#322102),(#322103,#322104,#322105),(#322106,#322107,#322108),(#322109,
#322110,#322111),(#322112,#322113,#322114),(#322115,#322116,#322117),(#322118,
#322119,#322120),(#322121,#322122,#322123),(#322124,#322125,#322126),(#322127,
#322128,#322129),(#322130,#322131,#322132),(#322133,#322134,#322135),(#322136,
#322137,#322138),(#322139,#322140,#322141),(#322142,#322143,#322144),(#322145,
#322146,#322147),(#322148,#322149,#322150),(#322151,#322152,#322153),(#322154,
#322155,#322156),(#322157,#322158,#322159),(#322160,#322161,#322162),(#322163,
#322164,#322165),(#322166,#322167,#322168),(#322169,#322170,#322171),(#322172,
#322173,#322174),(#322175,#322176,#322177),(#322178,#322179,#322180),(#322181,
#322182,#322183),(#322184,#322185,#322186),(#322187,#322188,#322189),(#322190,
#322191,#322192),(#322193,#322194,#322195),(#322196,#322197,#322198),(#322199,
#322200,#322201),(#322202,#322203,#322204),(#322205,#322206,#322207),(#322208,
#322209,#322210),(#322211,#322212,#322213),(#322214,#322215,#322216),(#322217,
#322218,#322219),(#322220,#322221,#322222),(#322223,#322224,#322225),(#322226,
#322227,#322228),(#322229,#322230,#322231),(#322232,#322233,#322234),(#322235,
#322236,#322237),(#322238,#322239,#322240),(#322241,#322242,#322243),(#322244,
#322245,#322246),(#322247,#322248,#322249),(#322250,#322251,#322252),(#322253,
#322254,#322255),(#322256,#322257,#322258),(#322259,#322260,#322261),(#322262,
#322263,#322264),(#322265,#322266,#322267),(#322268,#322269,#322270),(#322271,
#322272,#322273),(#322274,#322275,#322276),(#322277,#322278,#322279),(#322280,
#322281,#322282),(#322283,#322284,#322285),(#322286,#322287,#322288),(#322289,
#322290,#322291),(#322292,#322293,#322294),(#322295,#322296,#322297),(#322298,
#322299,#322300),(#322301,#322302,#322303),(#322304,#322305,#322306),(#322307,
#322308,#322309),(#322310,#322311,#322312),(#322313,#322314,#322315),(#322316,
#322317,#322318),(#322319,#322320,#322321),(#322322,#322323,#322324),(#322325,
#322326,#322327),(#322328,#322329,#322330),(#322331,#322332,#322333),(#322334,
#322335,#322336),(#322337,#322338,#322339),(#322340,#322341,#322342),(#322343,
#322344,#322345),(#322346,#322347,#322348),(#322349,#322350,#322351),(#322352,
#322353,#322354),(#322355,#322356,#322357),(#322358,#322359,#322360),(#322361,
#322362,#322363),(#322364,#322365,#322366),(#322367,#322368,#322369),(#322370,
#322371,#322372),(#322373,#322374,#322375),(#322376,#322377,#322378),(#322379,
#322380,#322381),(#322382,#322383,#322384),(#322385,#322386,#322387),(#322388,
#322389,#322390),(#322391,#322392,#322393),(#322394,#322395,#322396),(#322397,
#322398,#322399),(#322400,#322401,#322402),(#322403,#322404,#322405),(#322406,
#322407,#322408),(#322409,#322410,#322411),(#322412,#322413,#322414),(#322415,
#322416,#322417),(#322418,#322419,#322420),(#322421,#322422,#322423),(#322424,
#322425,#322426),(#322427,#322428,#322429),(#322430,#322431,#322432),(#322433,
#322434,#322435),(#322436,#322437,#322438),(#322439,#322440,#322441),(#322442,
#322443,#322444),(#322445,#322446,#322447),(#322448,#322449,#322450),(#322451,
#322452,#322453),(#322454,#322455,#322456),(#322457,#322458,#322459),(#322460,
#322461,#322462),(#322463,#322464,#322465),(#322466,#322467,#322468),(#322469,
#322470,#322471),(#322472,#322473,#322474),(#322475,#322476,#322477),(#322478,
#322479,#322480),(#322481,#322482,#322483),(#322484,#322485,#322486),(#322487,
#322488,#322489),(#322490,#322491,#322492),(#322493,#322494,#322495),(#322496,
#322497,#322498),(#322499,#322500,#322501),(#322502,#322503,#322504),(#322505,
#322506,#322507),(#322508,#322509,#322510),(#322511,#322512,#322513),(#322514,
#322515,#322516),(#322517,#322518,#322519),(#322520,#322521,#322522),(#322523,
#322524,#322525),(#322526,#322527,#322528),(#322529,#322530,#322531),(#322532,
#322533,#322534),(#322535,#322536,#322537),(#322538,#322539,#322540),(#322541,
#322542,#322543),(#322544,#322545,#322546),(#322547,#322548,#322549),(#322550,
#322551,#322552),(#322553,#322554,#322555),(#322556,#322557,#322558),(#322559,
#322560,#322561),(#322562,#322563,#322564),(#322565,#322566,#322567),(#322568,
#322569,#322570),(#322571,#322572,#322573),(#322574,#322575,#322576),(#322577,
#322578,#322579),(#322580,#322581,#322582),(#322583,#322584,#322585),(#322586,
#322587,#322588),(#322589,#322590,#322591),(#322592,#322593,#322594),(#322595,
#322596,#322597),(#322598,#322599,#322600),(#322601,#322602,#322603),(#322604,
#322605,#322606),(#322607,#322608,#322609),(#322610,#322611,#322612),(#322613,
#322614,#322615),(#322616,#322617,#322618),(#322619,#322620,#322621),(#322622,
#322623,#322624),(#322625,#322626,#322627),(#322628,#322629,#322630),(#322631,
#322632,#322633),(#322634,#322635,#322636),(#322637,#322638,#322639),(#322640,
#322641,#322642),(#322643,#322644,#322645),(#322646,#322647,#322648),(#322649,
#322650,#322651),(#322652,#322653,#322654),(#322655,#322656,#322657),(#322658,
#322659,#322660),(#322661,#322662,#322663),(#322664,#322665,#322666),(#322667,
#322668,#322669),(#322670,#322671,#322672),(#322673,#322674,#322675),(#322676,
#322677,#322678),(#322679,#322680,#322681),(#322682,#322683,#322684),(#322685,
#322686,#322687),(#322688,#322689,#322690),(#322691,#322692,#322693),(#322694,
#322695,#322696),(#322697,#322698,#322699),(#322700,#322701,#322702),(#322703,
#322704,#322705),(#322706,#322707,#322708),(#322709,#322710,#322711),(#322712,
#322713,#322714),(#322715,#322716,#322717),(#322718,#322719,#322720),(#322721,
#322722,#322723),(#322724,#322725,#322726),(#322727,#322728,#322729),(#322730,
#322731,#322732),(#322733,#322734,#322735),(#322736,#322737,#322738),(#322739,
#322740,#322741),(#322742,#322743,#322744),(#322745,#322746,#322747),(#322748,
#322749,#322750),(#322751,#322752,#322753),(#322754,#322755,#322756),(#322757,
#322758,#322759),(#322760,#322761,#322762),(#322763,#322764,#322765),(#322766,
#322767,#322768),(#322769,#322770,#322771),(#322772,#322773,#322774),(#322775,
#322776,#322777),(#322778,#322779,#322780),(#322781,#322782,#322783),(#322784,
#322785,#322786),(#322787,#322788,#322789),(#322790,#322791,#322792),(#322793,
#322794,#322795),(#322796,#322797,#322798),(#322799,#322800,#322801),(#322802,
#322803,#322804),(#322805,#322806,#322807),(#322808,#322809,#322810),(#322811,
#322812,#322813),(#322814,#322815,#322816),(#322817,#322818,#322819),(#322820,
#322821,#322822),(#322823,#322824,#322825),(#322826,#322827,#322828),(#322829,
#322830,#322831),(#322832,#322833,#322834),(#322835,#322836,#322837),(#322838,
#322839,#322840),(#322841,#322842,#322843),(#322844,#322845,#322846),(#322847,
#322848,#322849),(#322850,#322851,#322852),(#322853,#322854,#322855),(#322856,
#322857,#322858),(#322859,#322860,#322861),(#322862,#322863,#322864),(#322865,
#322866,#322867),(#322868,#322869,#322870),(#322871,#322872,#322873),(#322874,
#322875,#322876),(#322877,#322878,#322879),(#322880,#322881,#322882),(#322883,
#322884,#322885),(#322886,#322887,#322888),(#322889,#322890,#322891),(#322892,
#322893,#322894),(#322895,#322896,#322897),(#322898,#322899,#322900),(#322901,
#322902,#322903),(#322904,#322905,#322906),(#322907,#322908,#322909),(#322910,
#322911,#322912),(#322913,#322914,#322915),(#322916,#322917,#322918),(#322919,
#322920,#322921),(#322922,#322923,#322924),(#322925,#322926,#322927),(#322928,
#322929,#322930),(#322931,#322932,#322933),(#322934,#322935,#322936),(#322937,
#322938,#322939),(#322940,#322941,#322942),(#322943,#322944,#322945),(#322946,
#322947,#322948),(#322949,#322950,#322951),(#322952,#322953,#322954),(#322955,
#322956,#322957),(#322958,#322959,#322960),(#322961,#322962,#322963),(#322964,
#322965,#322966),(#322967,#322968,#322969),(#322970,#322971,#322972),(#322973,
#322974,#322975),(#322976,#322977,#322978),(#322979,#322980,#322981),(#322982,
#322983,#322984),(#322985,#322986,#322987),(#322988,#322989,#322990),(#322991,
#322992,#322993),(#322994,#322995,#322996),(#322997,#322998,#322999),(#323000,
#323001,#323002),(#323003,#323004,#323005),(#323006,#323007,#323008)),
 .UNSPECIFIED.,.F.,.F.,.F.,(6,1,1,1,1,1,1,1,1,1,1,1,1,1,1,1,1,1,1,1,1,1,
1,1,1,1,1,1,1,1,1,1,1,1,1,1,1,1,1,1,1,1,1,1,1,1,1,1,1,1,1,1,1,1,1,1,1,1,
1,1,1,1,1,1,1,1,1,1,1,1,1,1,1,1,1,1,1,1,1,1,1,1,1,1,1,1,1,1,1,1,1,1,1,1,
1,1,1,1,1,1,1,1,1,1,1,1,1,1,1,1,1,1,1,1,1,1,1,1,1,1,1,1,1,1,1,1,1,1,1,1,
1,1,1,1,1,1,1,1,1,1,1,1,1,1,1,1,1,1,1,1,1,1,1,1,1,1,1,1,1,1,1,1,1,1,1,1,
1,1,1,1,1,1,1,1,1,1,1,1,1,1,1,1,1,1,1,1,1,1,1,1,1,1,1,1,1,1,1,1,1,1,1,1,
1,1,1,1,1,1,1,1,1,1,1,1,1,1,1,1,1,1,1,1,1,1,1,1,1,1,1,1,1,1,1,1,1,1,1,1,
1,1,1,1,1,1,1,1,1,1,1,1,1,1,1,1,1,1,1,1,1,1,1,1,1,1,1,1,1,1,1,1,1,1,1,1,
1,1,1,1,1,1,1,1,1,1,1,1,1,1,1,1,1,1,1,1,1,1,1,1,1,1,1,1,1,1,1,1,1,1,1,1,
1,1,1,1,1,1,1,1,1,1,1,1,1,1,1,1,1,1,1,1,1,1,1,1,1,1,1,1,1,1,1,1,1,1,1,1,
1,1,1,1,1,1,1,1,1,1,1,1,1,1,1,1,1,1,1,1,1,1,1,1,1,1,1,1,1,1,1,1,1,1,1,1,
1,1,1,1,1,1,1,1,1,1,1,1,1,1,1,1,1,1,1,1,1,1,1,1,1,1,1,1,1,1,1,1,1,1,1,1,
1,1,1,1,1,1,1,1,1,1,1,1,1,1,1,1,1,1,1,1,1,1,1,1,1,1,1,1,1,1,1,1,1,1,1,1,
1,1,1,1,1,1,1,1,1,1,1,1,1,1,1,1,1,1,1,1,1,1,1,1,1,1,1,1,1,1,1,1,1,1,1,1,
1,1,1,1,1,1,1,1,1,1,1,1,1,1,1,1,1,1,1,1,1,1,1,1,1,1,1,1,1,1,1,1,1,1,1,1,
1,1,1,1,1,1,1,1,1,1,1,1,1,1,1,1,1,1,1,6),(2,1,2),(-1.,-0.998165138,-0.996330275,
-0.994495413,-0.99266055,-0.990825688,-0.988990826,-0.987155963,-0.985321101,
-0.983486239,-0.981651376,-0.979816514,-0.977981651,-0.976146789,-0.974311927,
-0.972477064,-0.970642202,-0.968807339,-0.966972477,-0.965137615,-0.963302752,
-0.96146789,-0.959633028,-0.957798165,-0.955963303,-0.95412844,-0.952293578,
-0.950458716,-0.948623853,-0.946788991,-0.944954128,-0.943119266,-0.941284404,
-0.939449541,-0.937614679,-0.935779817,-0.933944954,-0.932110092,-0.930275229,
-0.928440367,-0.926605505,-0.924770642,-0.92293578,-0.921100917,-0.919266055,
-0.917431193,-0.91559633,-0.913761468,-0.911926606,-0.910091743,-0.908256881,
-0.906422018,-0.904587156,-0.902752294,-0.900917431,-0.899082569,-0.897247706,
-0.895412844,-0.893577982,-0.891743119,-0.889908257,-0.888073394,-0.886238532,
-0.88440367,-0.882568807,-0.880733945,-0.878899083,-0.87706422,-0.875229358,
-0.873394495,-0.871559633,-0.869724771,-0.867889908,-0.866055046,-0.864220183,
-0.862385321,-0.860550459,-0.858715596,-0.856880734,-0.855045872,-0.853211009,
-0.851376147,-0.849541284,-0.847706422,-0.84587156,-0.844036697,-0.842201835,
-0.840366972,-0.83853211,-0.836697248,-0.834862385,-0.833027523,-0.831192661,
-0.829357798,-0.827522936,-0.825688073,-0.823853211,-0.822018349,-0.820183486,
-0.818348624,-0.816513761,-0.814678899,-0.812844037,-0.811009174,-0.809174312,
-0.80733945,-0.805504587,-0.803669725,-0.801834862,-0.8,-0.798165138,-0.796330275,
-0.794495413,-0.79266055,-0.790825688,-0.788990826,-0.787155963,-0.785321101,
-0.783486239,-0.781651376,-0.779816514,-0.777981651,-0.776146789,-0.774311927,
-0.772477064,-0.770642202,-0.768807339,-0.766972477,-0.765137615,-0.763302752,
-0.76146789,-0.759633028,-0.757798165,-0.755963303,-0.75412844,-0.752293578,
-0.750458716,-0.748623853,-0.746788991,-0.744954128,-0.743119266,-0.741284404,
-0.739449541,-0.737614679,-0.735779817,-0.733944954,-0.732110092,-0.730275229,
-0.728440367,-0.726605505,-0.724770642,-0.72293578,-0.721100917,-0.719266055,
-0.717431193,-0.71559633,-0.713761468,-0.711926606,-0.710091743,-0.708256881,
-0.706422018,-0.704587156,-0.702752294,-0.700917431,-0.699082569,-0.697247706,
-0.695412844,-0.693577982,-0.691743119,-0.689908257,-0.688073394,-0.686238532,
-0.68440367,-0.682568807,-0.680733945,-0.678899083,-0.67706422,-0.675229358,
-0.673394495,-0.671559633,-0.669724771,-0.667889908,-0.666055046,-0.664220183,
-0.662385321,-0.660550459,-0.658715596,-0.656880734,-0.655045872,-0.653211009,
-0.651376147,-0.649541284,-0.647706422,-0.64587156,-0.644036697,-0.642201835,
-0.640366972,-0.63853211,-0.636697248,-0.634862385,-0.633027523,-0.631192661,
-0.629357798,-0.627522936,-0.625688073,-0.623853211,-0.622018349,-0.620183486,
-0.618348624,-0.616513761,-0.614678899,-0.612844037,-0.611009174,-0.609174312,
-0.60733945,-0.605504587,-0.603669725,-0.601834862,-0.6,-0.598165138,-0.596330275,
-0.594495413,-0.59266055,-0.590825688,-0.588990826,-0.587155963,-0.585321101,
-0.583486239,-0.581651376,-0.579816514,-0.577981651,-0.576146789,-0.574311927,
-0.572477064,-0.570642202,-0.568807339,-0.566972477,-0.565137615,-0.563302752,
-0.56146789,-0.559633028,-0.557798165,-0.555963303,-0.55412844,-0.552293578,
-0.550458716,-0.548623853,-0.546788991,-0.544954128,-0.543119266,-0.541284404,
-0.539449541,-0.537614679,-0.535779817,-0.533944954,-0.532110092,-0.530275229,
-0.528440367,-0.526605505,-0.524770642,-0.52293578,-0.521100917,-0.519266055,
-0.517431193,-0.51559633,-0.513761468,-0.511926606,-0.510091743,-0.508256881,
-0.506422018,-0.504587156,-0.502752294,-0.500917431,-0.499082569,-0.497247706,
-0.495412844,-0.493577982,-0.491743119,-0.489908257,-0.488073394,-0.486238532,
-0.48440367,-0.482568807,-0.480733945,-0.478899083,-0.47706422,-0.475229358,
-0.473394495,-0.471559633,-0.469724771,-0.467889908,-0.466055046,-0.464220183,
-0.462385321,-0.460550459,-0.458715596,-0.456880734,-0.455045872,-0.453211009,
-0.451376147,-0.449541284,-0.447706422,-0.44587156,-0.444036697,-0.442201835,
-0.440366972,-0.43853211,-0.436697248,-0.434862385,-0.433027523,-0.431192661,
-0.429357798,-0.427522936,-0.425688073,-0.423853211,-0.422018349,-0.420183486,
-0.418348624,-0.416513761,-0.414678899,-0.412844037,-0.411009174,-0.409174312,
-0.40733945,-0.405504587,-0.403669725,-0.401834862,-0.4,-0.398165138,-0.396330275,
-0.394495413,-0.39266055,-0.390825688,-0.388990826,-0.387155963,-0.385321101,
-0.383486239,-0.381651376,-0.379816514,-0.377981651,-0.376146789,-0.374311927,
-0.372477064,-0.370642202,-0.368807339,-0.366972477,-0.365137615,-0.363302752,
-0.36146789,-0.359633028,-0.357798165,-0.355963303,-0.35412844,-0.352293578,
-0.350458716,-0.348623853,-0.346788991,-0.344954128,-0.343119266,-0.341284404,
-0.339449541,-0.337614679,-0.335779817,-0.333944954,-0.332110092,-0.330275229,
-0.328440367,-0.326605505,-0.324770642,-0.32293578,-0.321100917,-0.319266055,
-0.317431193,-0.31559633,-0.313761468,-0.311926606,-0.310091743,-0.308256881,
-0.306422018,-0.304587156,-0.302752294,-0.300917431,-0.299082569,-0.297247706,
-0.295412844,-0.293577982,-0.291743119,-0.289908257,-0.288073394,-0.286238532,
-0.28440367,-0.282568807,-0.280733945,-0.278899083,-0.27706422,-0.275229358,
-0.273394495,-0.271559633,-0.269724771,-0.267889908,-0.266055046,-0.264220183,
-0.262385321,-0.260550459,-0.258715596,-0.256880734,-0.255045872,-0.253211009,
-0.251376147,-0.249541284,-0.247706422,-0.24587156,-0.244036697,-0.242201835,
-0.240366972,-0.23853211,-0.236697248,-0.234862385,-0.233027523,-0.231192661,
-0.229357798,-0.227522936,-0.225688073,-0.223853211,-0.222018349,-0.220183486,
-0.218348624,-0.216513761,-0.214678899,-0.212844037,-0.211009174,-0.209174312,
-0.20733945,-0.205504587,-0.203669725,-0.201834862,-0.2,-0.198165138,-0.196330275,
-0.194495413,-0.19266055,-0.190825688,-0.188990826,-0.187155963,-0.185321101,
-0.183486239,-0.181651376,-0.179816514,-0.177981651,-0.176146789,-0.174311927,
-0.172477064,-0.170642202,-0.168807339,-0.166972477,-0.165137615,-0.163302752,
-0.16146789,-0.159633028,-0.157798165,-0.155963303,-0.15412844,-0.152293578,
-0.150458716,-0.148623853,-0.146788991,-0.144954128,-0.143119266,-0.141284404,
-0.139449541,-0.137614679,-0.135779817,-0.133944954,-0.132110092,-0.130275229,
-0.128440367,-0.126605505,-0.124770642,-0.12293578,-0.121100917,-0.119266055,
-0.117431193,-0.11559633,-0.113761468,-0.111926606,-0.110091743,-0.108256881,
-0.106422018,-0.104587156,-0.102752294,-0.100917431,-0.099082569,-0.097247706,
-0.095412844,-0.093577982,-0.091743119,-0.089908257,-0.088073394,-0.086238532,
-0.08440367,-0.082568807,-0.080733945,-0.078899083,-0.07706422,-0.075229358,
-0.073394495,-0.071559633,-0.069724771,-0.067889908,-0.066055046,-0.064220183,
-0.062385321,-0.060550459,-0.058715596,-0.056880734,-0.055045872,-0.053211009,
-0.051376147,-0.049541284,-0.047706422,-0.04587156,-0.044036697,-0.042201835,
-0.040366972,-0.03853211,-0.036697248,-0.034862385,-0.033027523,-0.031192661,
-0.029357798,-0.027522936,-0.025688073,-0.023853211,-0.022018349,-0.020183486,
-0.018348624,-0.016513761,-0.014678899,-0.012844037,-0.011009174,-0.009174312,
-0.00733945,-0.005504587,-0.003669725,-0.001834862,0.000982105),(0.3,1.,
1.3),.UNSPECIFIED.);
#6316=B_SPLINE_SURFACE_WITH_KNOTS('',5,1,((#323031,#323032,#323033),(#323034,
#323035,#323036),(#323037,#323038,#323039),(#323040,#323041,#323042),(#323043,
#323044,#323045),(#323046,#323047,#323048),(#323049,#323050,#323051),(#323052,
#323053,#323054),(#323055,#323056,#323057),(#323058,#323059,#323060),(#323061,
#323062,#323063),(#323064,#323065,#323066),(#323067,#323068,#323069),(#323070,
#323071,#323072),(#323073,#323074,#323075),(#323076,#323077,#323078),(#323079,
#323080,#323081),(#323082,#323083,#323084),(#323085,#323086,#323087),(#323088,
#323089,#323090),(#323091,#323092,#323093),(#323094,#323095,#323096),(#323097,
#323098,#323099),(#323100,#323101,#323102),(#323103,#323104,#323105),(#323106,
#323107,#323108),(#323109,#323110,#323111),(#323112,#323113,#323114),(#323115,
#323116,#323117),(#323118,#323119,#323120),(#323121,#323122,#323123),(#323124,
#323125,#323126),(#323127,#323128,#323129),(#323130,#323131,#323132),(#323133,
#323134,#323135),(#323136,#323137,#323138),(#323139,#323140,#323141),(#323142,
#323143,#323144),(#323145,#323146,#323147),(#323148,#323149,#323150),(#323151,
#323152,#323153),(#323154,#323155,#323156),(#323157,#323158,#323159),(#323160,
#323161,#323162),(#323163,#323164,#323165),(#323166,#323167,#323168),(#323169,
#323170,#323171),(#323172,#323173,#323174),(#323175,#323176,#323177),(#323178,
#323179,#323180),(#323181,#323182,#323183),(#323184,#323185,#323186),(#323187,
#323188,#323189),(#323190,#323191,#323192),(#323193,#323194,#323195),(#323196,
#323197,#323198),(#323199,#323200,#323201),(#323202,#323203,#323204),(#323205,
#323206,#323207),(#323208,#323209,#323210),(#323211,#323212,#323213),(#323214,
#323215,#323216),(#323217,#323218,#323219),(#323220,#323221,#323222),(#323223,
#323224,#323225),(#323226,#323227,#323228),(#323229,#323230,#323231),(#323232,
#323233,#323234),(#323235,#323236,#323237),(#323238,#323239,#323240),(#323241,
#323242,#323243),(#323244,#323245,#323246),(#323247,#323248,#323249),(#323250,
#323251,#323252),(#323253,#323254,#323255),(#323256,#323257,#323258),(#323259,
#323260,#323261),(#323262,#323263,#323264),(#323265,#323266,#323267),(#323268,
#323269,#323270),(#323271,#323272,#323273),(#323274,#323275,#323276),(#323277,
#323278,#323279),(#323280,#323281,#323282),(#323283,#323284,#323285),(#323286,
#323287,#323288),(#323289,#323290,#323291),(#323292,#323293,#323294),(#323295,
#323296,#323297),(#323298,#323299,#323300),(#323301,#323302,#323303),(#323304,
#323305,#323306),(#323307,#323308,#323309),(#323310,#323311,#323312),(#323313,
#323314,#323315),(#323316,#323317,#323318),(#323319,#323320,#323321),(#323322,
#323323,#323324),(#323325,#323326,#323327),(#323328,#323329,#323330),(#323331,
#323332,#323333),(#323334,#323335,#323336),(#323337,#323338,#323339),(#323340,
#323341,#323342),(#323343,#323344,#323345),(#323346,#323347,#323348),(#323349,
#323350,#323351),(#323352,#323353,#323354),(#323355,#323356,#323357),(#323358,
#323359,#323360),(#323361,#323362,#323363),(#323364,#323365,#323366),(#323367,
#323368,#323369),(#323370,#323371,#323372),(#323373,#323374,#323375),(#323376,
#323377,#323378),(#323379,#323380,#323381),(#323382,#323383,#323384),(#323385,
#323386,#323387),(#323388,#323389,#323390),(#323391,#323392,#323393),(#323394,
#323395,#323396),(#323397,#323398,#323399),(#323400,#323401,#323402),(#323403,
#323404,#323405),(#323406,#323407,#323408),(#323409,#323410,#323411),(#323412,
#323413,#323414),(#323415,#323416,#323417),(#323418,#323419,#323420),(#323421,
#323422,#323423),(#323424,#323425,#323426),(#323427,#323428,#323429),(#323430,
#323431,#323432),(#323433,#323434,#323435),(#323436,#323437,#323438),(#323439,
#323440,#323441),(#323442,#323443,#323444),(#323445,#323446,#323447),(#323448,
#323449,#323450),(#323451,#323452,#323453),(#323454,#323455,#323456),(#323457,
#323458,#323459),(#323460,#323461,#323462),(#323463,#323464,#323465),(#323466,
#323467,#323468),(#323469,#323470,#323471),(#323472,#323473,#323474),(#323475,
#323476,#323477),(#323478,#323479,#323480),(#323481,#323482,#323483),(#323484,
#323485,#323486),(#323487,#323488,#323489),(#323490,#323491,#323492),(#323493,
#323494,#323495),(#323496,#323497,#323498),(#323499,#323500,#323501),(#323502,
#323503,#323504),(#323505,#323506,#323507),(#323508,#323509,#323510),(#323511,
#323512,#323513),(#323514,#323515,#323516),(#323517,#323518,#323519),(#323520,
#323521,#323522),(#323523,#323524,#323525),(#323526,#323527,#323528),(#323529,
#323530,#323531),(#323532,#323533,#323534),(#323535,#323536,#323537),(#323538,
#323539,#323540),(#323541,#323542,#323543),(#323544,#323545,#323546),(#323547,
#323548,#323549),(#323550,#323551,#323552),(#323553,#323554,#323555),(#323556,
#323557,#323558),(#323559,#323560,#323561),(#323562,#323563,#323564),(#323565,
#323566,#323567),(#323568,#323569,#323570),(#323571,#323572,#323573),(#323574,
#323575,#323576),(#323577,#323578,#323579),(#323580,#323581,#323582),(#323583,
#323584,#323585),(#323586,#323587,#323588),(#323589,#323590,#323591),(#323592,
#323593,#323594),(#323595,#323596,#323597),(#323598,#323599,#323600),(#323601,
#323602,#323603),(#323604,#323605,#323606),(#323607,#323608,#323609),(#323610,
#323611,#323612),(#323613,#323614,#323615),(#323616,#323617,#323618),(#323619,
#323620,#323621),(#323622,#323623,#323624),(#323625,#323626,#323627),(#323628,
#323629,#323630),(#323631,#323632,#323633),(#323634,#323635,#323636),(#323637,
#323638,#323639),(#323640,#323641,#323642),(#323643,#323644,#323645),(#323646,
#323647,#323648),(#323649,#323650,#323651),(#323652,#323653,#323654),(#323655,
#323656,#323657),(#323658,#323659,#323660),(#323661,#323662,#323663),(#323664,
#323665,#323666),(#323667,#323668,#323669),(#323670,#323671,#323672),(#323673,
#323674,#323675),(#323676,#323677,#323678),(#323679,#323680,#323681),(#323682,
#323683,#323684),(#323685,#323686,#323687),(#323688,#323689,#323690),(#323691,
#323692,#323693),(#323694,#323695,#323696),(#323697,#323698,#323699),(#323700,
#323701,#323702),(#323703,#323704,#323705),(#323706,#323707,#323708),(#323709,
#323710,#323711),(#323712,#323713,#323714),(#323715,#323716,#323717),(#323718,
#323719,#323720),(#323721,#323722,#323723),(#323724,#323725,#323726),(#323727,
#323728,#323729),(#323730,#323731,#323732),(#323733,#323734,#323735),(#323736,
#323737,#323738),(#323739,#323740,#323741),(#323742,#323743,#323744),(#323745,
#323746,#323747),(#323748,#323749,#323750),(#323751,#323752,#323753),(#323754,
#323755,#323756),(#323757,#323758,#323759),(#323760,#323761,#323762),(#323763,
#323764,#323765),(#323766,#323767,#323768),(#323769,#323770,#323771),(#323772,
#323773,#323774),(#323775,#323776,#323777),(#323778,#323779,#323780),(#323781,
#323782,#323783),(#323784,#323785,#323786),(#323787,#323788,#323789),(#323790,
#323791,#323792),(#323793,#323794,#323795),(#323796,#323797,#323798),(#323799,
#323800,#323801),(#323802,#323803,#323804),(#323805,#323806,#323807),(#323808,
#323809,#323810),(#323811,#323812,#323813),(#323814,#323815,#323816),(#323817,
#323818,#323819),(#323820,#323821,#323822),(#323823,#323824,#323825),(#323826,
#323827,#323828),(#323829,#323830,#323831),(#323832,#323833,#323834),(#323835,
#323836,#323837),(#323838,#323839,#323840),(#323841,#323842,#323843),(#323844,
#323845,#323846),(#323847,#323848,#323849),(#323850,#323851,#323852),(#323853,
#323854,#323855),(#323856,#323857,#323858),(#323859,#323860,#323861),(#323862,
#323863,#323864),(#323865,#323866,#323867),(#323868,#323869,#323870),(#323871,
#323872,#323873),(#323874,#323875,#323876),(#323877,#323878,#323879),(#323880,
#323881,#323882),(#323883,#323884,#323885),(#323886,#323887,#323888),(#323889,
#323890,#323891),(#323892,#323893,#323894),(#323895,#323896,#323897),(#323898,
#323899,#323900),(#323901,#323902,#323903),(#323904,#323905,#323906),(#323907,
#323908,#323909),(#323910,#323911,#323912),(#323913,#323914,#323915),(#323916,
#323917,#323918),(#323919,#323920,#323921),(#323922,#323923,#323924),(#323925,
#323926,#323927),(#323928,#323929,#323930),(#323931,#323932,#323933),(#323934,
#323935,#323936),(#323937,#323938,#323939),(#323940,#323941,#323942),(#323943,
#323944,#323945),(#323946,#323947,#323948),(#323949,#323950,#323951),(#323952,
#323953,#323954),(#323955,#323956,#323957),(#323958,#323959,#323960),(#323961,
#323962,#323963),(#323964,#323965,#323966),(#323967,#323968,#323969),(#323970,
#323971,#323972),(#323973,#323974,#323975),(#323976,#323977,#323978),(#323979,
#323980,#323981),(#323982,#323983,#323984),(#323985,#323986,#323987),(#323988,
#323989,#323990),(#323991,#323992,#323993),(#323994,#323995,#323996),(#323997,
#323998,#323999),(#324000,#324001,#324002),(#324003,#324004,#324005),(#324006,
#324007,#324008),(#324009,#324010,#324011),(#324012,#324013,#324014),(#324015,
#324016,#324017),(#324018,#324019,#324020),(#324021,#324022,#324023),(#324024,
#324025,#324026),(#324027,#324028,#324029),(#324030,#324031,#324032),(#324033,
#324034,#324035),(#324036,#324037,#324038),(#324039,#324040,#324041),(#324042,
#324043,#324044),(#324045,#324046,#324047),(#324048,#324049,#324050),(#324051,
#324052,#324053),(#324054,#324055,#324056),(#324057,#324058,#324059),(#324060,
#324061,#324062),(#324063,#324064,#324065),(#324066,#324067,#324068),(#324069,
#324070,#324071),(#324072,#324073,#324074),(#324075,#324076,#324077),(#324078,
#324079,#324080),(#324081,#324082,#324083),(#324084,#324085,#324086),(#324087,
#324088,#324089),(#324090,#324091,#324092),(#324093,#324094,#324095),(#324096,
#324097,#324098),(#324099,#324100,#324101),(#324102,#324103,#324104),(#324105,
#324106,#324107),(#324108,#324109,#324110),(#324111,#324112,#324113),(#324114,
#324115,#324116),(#324117,#324118,#324119),(#324120,#324121,#324122),(#324123,
#324124,#324125),(#324126,#324127,#324128),(#324129,#324130,#324131),(#324132,
#324133,#324134),(#324135,#324136,#324137),(#324138,#324139,#324140),(#324141,
#324142,#324143),(#324144,#324145,#324146),(#324147,#324148,#324149),(#324150,
#324151,#324152),(#324153,#324154,#324155),(#324156,#324157,#324158),(#324159,
#324160,#324161),(#324162,#324163,#324164),(#324165,#324166,#324167),(#324168,
#324169,#324170),(#324171,#324172,#324173),(#324174,#324175,#324176),(#324177,
#324178,#324179),(#324180,#324181,#324182),(#324183,#324184,#324185),(#324186,
#324187,#324188),(#324189,#324190,#324191),(#324192,#324193,#324194),(#324195,
#324196,#324197),(#324198,#324199,#324200),(#324201,#324202,#324203),(#324204,
#324205,#324206),(#324207,#324208,#324209),(#324210,#324211,#324212),(#324213,
#324214,#324215),(#324216,#324217,#324218),(#324219,#324220,#324221),(#324222,
#324223,#324224),(#324225,#324226,#324227),(#324228,#324229,#324230),(#324231,
#324232,#324233),(#324234,#324235,#324236),(#324237,#324238,#324239),(#324240,
#324241,#324242),(#324243,#324244,#324245),(#324246,#324247,#324248),(#324249,
#324250,#324251),(#324252,#324253,#324254),(#324255,#324256,#324257),(#324258,
#324259,#324260),(#324261,#324262,#324263),(#324264,#324265,#324266),(#324267,
#324268,#324269),(#324270,#324271,#324272),(#324273,#324274,#324275),(#324276,
#324277,#324278),(#324279,#324280,#324281),(#324282,#324283,#324284),(#324285,
#324286,#324287),(#324288,#324289,#324290),(#324291,#324292,#324293),(#324294,
#324295,#324296),(#324297,#324298,#324299),(#324300,#324301,#324302),(#324303,
#324304,#324305),(#324306,#324307,#324308),(#324309,#324310,#324311),(#324312,
#324313,#324314),(#324315,#324316,#324317),(#324318,#324319,#324320),(#324321,
#324322,#324323),(#324324,#324325,#324326),(#324327,#324328,#324329),(#324330,
#324331,#324332),(#324333,#324334,#324335),(#324336,#324337,#324338),(#324339,
#324340,#324341),(#324342,#324343,#324344),(#324345,#324346,#324347),(#324348,
#324349,#324350),(#324351,#324352,#324353),(#324354,#324355,#324356),(#324357,
#324358,#324359),(#324360,#324361,#324362),(#324363,#324364,#324365),(#324366,
#324367,#324368),(#324369,#324370,#324371),(#324372,#324373,#324374),(#324375,
#324376,#324377),(#324378,#324379,#324380),(#324381,#324382,#324383),(#324384,
#324385,#324386),(#324387,#324388,#324389),(#324390,#324391,#324392),(#324393,
#324394,#324395),(#324396,#324397,#324398),(#324399,#324400,#324401),(#324402,
#324403,#324404),(#324405,#324406,#324407),(#324408,#324409,#324410),(#324411,
#324412,#324413),(#324414,#324415,#324416),(#324417,#324418,#324419),(#324420,
#324421,#324422),(#324423,#324424,#324425),(#324426,#324427,#324428),(#324429,
#324430,#324431),(#324432,#324433,#324434),(#324435,#324436,#324437),(#324438,
#324439,#324440),(#324441,#324442,#324443),(#324444,#324445,#324446),(#324447,
#324448,#324449),(#324450,#324451,#324452),(#324453,#324454,#324455),(#324456,
#324457,#324458),(#324459,#324460,#324461),(#324462,#324463,#324464),(#324465,
#324466,#324467),(#324468,#324469,#324470),(#324471,#324472,#324473),(#324474,
#324475,#324476),(#324477,#324478,#324479),(#324480,#324481,#324482),(#324483,
#324484,#324485),(#324486,#324487,#324488),(#324489,#324490,#324491),(#324492,
#324493,#324494),(#324495,#324496,#324497),(#324498,#324499,#324500),(#324501,
#324502,#324503),(#324504,#324505,#324506),(#324507,#324508,#324509),(#324510,
#324511,#324512),(#324513,#324514,#324515),(#324516,#324517,#324518),(#324519,
#324520,#324521),(#324522,#324523,#324524),(#324525,#324526,#324527),(#324528,
#324529,#324530),(#324531,#324532,#324533),(#324534,#324535,#324536),(#324537,
#324538,#324539),(#324540,#324541,#324542),(#324543,#324544,#324545),(#324546,
#324547,#324548),(#324549,#324550,#324551),(#324552,#324553,#324554),(#324555,
#324556,#324557),(#324558,#324559,#324560),(#324561,#324562,#324563),(#324564,
#324565,#324566),(#324567,#324568,#324569),(#324570,#324571,#324572),(#324573,
#324574,#324575),(#324576,#324577,#324578),(#324579,#324580,#324581),(#324582,
#324583,#324584),(#324585,#324586,#324587),(#324588,#324589,#324590),(#324591,
#324592,#324593),(#324594,#324595,#324596),(#324597,#324598,#324599),(#324600,
#324601,#324602),(#324603,#324604,#324605),(#324606,#324607,#324608),(#324609,
#324610,#324611),(#324612,#324613,#324614),(#324615,#324616,#324617),(#324618,
#324619,#324620),(#324621,#324622,#324623),(#324624,#324625,#324626),(#324627,
#324628,#324629),(#324630,#324631,#324632),(#324633,#324634,#324635),(#324636,
#324637,#324638),(#324639,#324640,#324641),(#324642,#324643,#324644),(#324645,
#324646,#324647),(#324648,#324649,#324650),(#324651,#324652,#324653),(#324654,
#324655,#324656),(#324657,#324658,#324659),(#324660,#324661,#324662),(#324663,
#324664,#324665),(#324666,#324667,#324668),(#324669,#324670,#324671),(#324672,
#324673,#324674),(#324675,#324676,#324677),(#324678,#324679,#324680),(#324681,
#324682,#324683)),.UNSPECIFIED.,.F.,.F.,.F.,(6,1,1,1,1,1,1,1,1,1,1,1,1,
1,1,1,1,1,1,1,1,1,1,1,1,1,1,1,1,1,1,1,1,1,1,1,1,1,1,1,1,1,1,1,1,1,1,1,1,
1,1,1,1,1,1,1,1,1,1,1,1,1,1,1,1,1,1,1,1,1,1,1,1,1,1,1,1,1,1,1,1,1,1,1,1,
1,1,1,1,1,1,1,1,1,1,1,1,1,1,1,1,1,1,1,1,1,1,1,1,1,1,1,1,1,1,1,1,1,1,1,1,
1,1,1,1,1,1,1,1,1,1,1,1,1,1,1,1,1,1,1,1,1,1,1,1,1,1,1,1,1,1,1,1,1,1,1,1,
1,1,1,1,1,1,1,1,1,1,1,1,1,1,1,1,1,1,1,1,1,1,1,1,1,1,1,1,1,1,1,1,1,1,1,1,
1,1,1,1,1,1,1,1,1,1,1,1,1,1,1,1,1,1,1,1,1,1,1,1,1,1,1,1,1,1,1,1,1,1,1,1,
1,1,1,1,1,1,1,1,1,1,1,1,1,1,1,1,1,1,1,1,1,1,1,1,1,1,1,1,1,1,1,1,1,1,1,1,
1,1,1,1,1,1,1,1,1,1,1,1,1,1,1,1,1,1,1,1,1,1,1,1,1,1,1,1,1,1,1,1,1,1,1,1,
1,1,1,1,1,1,1,1,1,1,1,1,1,1,1,1,1,1,1,1,1,1,1,1,1,1,1,1,1,1,1,1,1,1,1,1,
1,1,1,1,1,1,1,1,1,1,1,1,1,1,1,1,1,1,1,1,1,1,1,1,1,1,1,1,1,1,1,1,1,1,1,1,
1,1,1,1,1,1,1,1,1,1,1,1,1,1,1,1,1,1,1,1,1,1,1,1,1,1,1,1,1,1,1,1,1,1,1,1,
1,1,1,1,1,1,1,1,1,1,1,1,1,1,1,1,1,1,1,1,1,1,1,1,1,1,1,1,1,1,1,1,1,1,1,1,
1,1,1,1,1,1,1,1,1,1,1,1,1,1,1,1,1,1,1,1,1,1,1,1,1,1,1,1,1,1,1,1,1,1,1,1,
1,1,1,1,1,1,1,1,1,1,1,1,1,1,1,1,1,1,1,1,1,1,1,1,1,1,1,1,1,1,1,1,1,1,1,1,
1,1,1,1,1,1,1,1,1,1,1,1,1,1,1,1,1,1,1,1,1,1,1,1,1,1,1,1,1,6),(2,1,2),(-0.001964187,
0.,0.001834862,0.003669725,0.005504587,0.00733945,0.009174312,0.011009174,
0.012844037,0.014678899,0.016513761,0.018348624,0.020183486,0.022018349,
0.023853211,0.025688073,0.027522936,0.029357798,0.031192661,0.033027523,
0.034862385,0.036697248,0.03853211,0.040366972,0.042201835,0.044036697,
0.04587156,0.047706422,0.049541284,0.051376147,0.053211009,0.055045872,
0.056880734,0.058715596,0.060550459,0.062385321,0.064220183,0.066055046,
0.067889908,0.069724771,0.071559633,0.073394495,0.075229358,0.07706422,
0.078899083,0.080733945,0.082568807,0.08440367,0.086238532,0.088073394,
0.089908257,0.091743119,0.093577982,0.095412844,0.097247706,0.099082569,
0.100917431,0.102752294,0.104587156,0.106422018,0.108256881,0.110091743,
0.111926606,0.113761468,0.11559633,0.117431193,0.119266055,0.121100917,
0.12293578,0.124770642,0.126605505,0.128440367,0.130275229,0.132110092,
0.133944954,0.135779817,0.137614679,0.139449541,0.141284404,0.143119266,
0.144954128,0.146788991,0.148623853,0.150458716,0.152293578,0.15412844,
0.155963303,0.157798165,0.159633028,0.16146789,0.163302752,0.165137615,
0.166972477,0.168807339,0.170642202,0.172477064,0.174311927,0.176146789,
0.177981651,0.179816514,0.181651376,0.183486239,0.185321101,0.187155963,
0.188990826,0.190825688,0.19266055,0.194495413,0.196330275,0.198165138,
0.2,0.201834862,0.203669725,0.205504587,0.20733945,0.209174312,0.211009174,
0.212844037,0.214678899,0.216513761,0.218348624,0.220183486,0.222018349,
0.223853211,0.225688073,0.227522936,0.229357798,0.231192661,0.233027523,
0.234862385,0.236697248,0.23853211,0.240366972,0.242201835,0.244036697,
0.24587156,0.247706422,0.249541284,0.251376147,0.253211009,0.255045872,
0.256880734,0.258715596,0.260550459,0.262385321,0.264220183,0.266055046,
0.267889908,0.269724771,0.271559633,0.273394495,0.275229358,0.27706422,
0.278899083,0.280733945,0.282568807,0.28440367,0.286238532,0.288073394,
0.289908257,0.291743119,0.293577982,0.295412844,0.297247706,0.299082569,
0.300917431,0.302752294,0.304587156,0.306422018,0.308256881,0.310091743,
0.311926606,0.313761468,0.31559633,0.317431193,0.319266055,0.321100917,
0.32293578,0.324770642,0.326605505,0.328440367,0.330275229,0.332110092,
0.333944954,0.335779817,0.337614679,0.339449541,0.341284404,0.343119266,
0.344954128,0.346788991,0.348623853,0.350458716,0.352293578,0.35412844,
0.355963303,0.357798165,0.359633028,0.36146789,0.363302752,0.365137615,
0.366972477,0.368807339,0.370642202,0.372477064,0.374311927,0.376146789,
0.377981651,0.379816514,0.381651376,0.383486239,0.385321101,0.387155963,
0.388990826,0.390825688,0.39266055,0.394495413,0.396330275,0.398165138,
0.4,0.401834862,0.403669725,0.405504587,0.40733945,0.409174312,0.411009174,
0.412844037,0.414678899,0.416513761,0.418348624,0.420183486,0.422018349,
0.423853211,0.425688073,0.427522936,0.429357798,0.431192661,0.433027523,
0.434862385,0.436697248,0.43853211,0.440366972,0.442201835,0.444036697,
0.44587156,0.447706422,0.449541284,0.451376147,0.453211009,0.455045872,
0.456880734,0.458715596,0.460550459,0.462385321,0.464220183,0.466055046,
0.467889908,0.469724771,0.471559633,0.473394495,0.475229358,0.47706422,
0.478899083,0.480733945,0.482568807,0.48440367,0.486238532,0.488073394,
0.489908257,0.491743119,0.493577982,0.495412844,0.497247706,0.499082569,
0.500917431,0.502752294,0.504587156,0.506422018,0.508256881,0.510091743,
0.511926606,0.513761468,0.51559633,0.517431193,0.519266055,0.521100917,
0.52293578,0.524770642,0.526605505,0.528440367,0.530275229,0.532110092,
0.533944954,0.535779817,0.537614679,0.539449541,0.541284404,0.543119266,
0.544954128,0.546788991,0.548623853,0.550458716,0.552293578,0.55412844,
0.555963303,0.557798165,0.559633028,0.56146789,0.563302752,0.565137615,
0.566972477,0.568807339,0.570642202,0.572477064,0.574311927,0.576146789,
0.577981651,0.579816514,0.581651376,0.583486239,0.585321101,0.587155963,
0.588990826,0.590825688,0.59266055,0.594495413,0.596330275,0.598165138,
0.6,0.601834862,0.603669725,0.605504587,0.60733945,0.609174312,0.611009174,
0.612844037,0.614678899,0.616513761,0.618348624,0.620183486,0.622018349,
0.623853211,0.625688073,0.627522936,0.629357798,0.631192661,0.633027523,
0.634862385,0.636697248,0.63853211,0.640366972,0.642201835,0.644036697,
0.64587156,0.647706422,0.649541284,0.651376147,0.653211009,0.655045872,
0.656880734,0.658715596,0.660550459,0.662385321,0.664220183,0.666055046,
0.667889908,0.669724771,0.671559633,0.673394495,0.675229358,0.67706422,
0.678899083,0.680733945,0.682568807,0.68440367,0.686238532,0.688073394,
0.689908257,0.691743119,0.693577982,0.695412844,0.697247706,0.699082569,
0.700917431,0.702752294,0.704587156,0.706422018,0.708256881,0.710091743,
0.711926606,0.713761468,0.71559633,0.717431193,0.719266055,0.721100917,
0.72293578,0.724770642,0.726605505,0.728440367,0.730275229,0.732110092,
0.733944954,0.735779817,0.737614679,0.739449541,0.741284404,0.743119266,
0.744954128,0.746788991,0.748623853,0.750458716,0.752293578,0.75412844,
0.755963303,0.757798165,0.759633028,0.76146789,0.763302752,0.765137615,
0.766972477,0.768807339,0.770642202,0.772477064,0.774311927,0.776146789,
0.777981651,0.779816514,0.781651376,0.783486239,0.785321101,0.787155963,
0.788990826,0.790825688,0.79266055,0.794495413,0.796330275,0.798165138,
0.8,0.801834862,0.803669725,0.805504587,0.80733945,0.809174312,0.811009174,
0.812844037,0.814678899,0.816513761,0.818348624,0.820183486,0.822018349,
0.823853211,0.825688073,0.827522936,0.829357798,0.831192661,0.833027523,
0.834862385,0.836697248,0.83853211,0.840366972,0.842201835,0.844036697,
0.84587156,0.847706422,0.849541284,0.851376147,0.853211009,0.855045872,
0.856880734,0.858715596,0.860550459,0.862385321,0.864220183,0.866055046,
0.867889908,0.869724771,0.871559633,0.873394495,0.875229358,0.87706422,
0.878899083,0.880733945,0.882568807,0.88440367,0.886238532,0.888073394,
0.889908257,0.891743119,0.893577982,0.895412844,0.897247706,0.899082569,
0.900917431,0.902752294,0.904587156,0.906422018,0.908256881,0.910091743,
0.911926606,0.913761468,0.91559633,0.917431193,0.919266055,0.921100917,
0.92293578,0.924770642,0.926605505,0.928440367,0.930275229,0.932110092,
0.933944954,0.935779817,0.937614679,0.939449541,0.941284404,0.943119266,
0.944954128,0.946788991,0.948623853,0.950458716,0.952293578,0.95412844,
0.955963303,0.957798165,0.959633028,0.96146789,0.963302752,0.965137615,
0.966972477,0.968807339,0.970642202,0.972477064,0.974311927,0.976146789,
0.977981651,0.979816514,0.981651376,0.983486239,0.985321101,0.987155963,
0.988990826,0.990825688,0.99266055,0.994495413,0.996330275,0.998165138,
1.),(0.3,1.,1.3),.UNSPECIFIED.);
#6317=B_SPLINE_SURFACE_WITH_KNOTS('',5,1,((#324706,#324707,#324708),(#324709,
#324710,#324711),(#324712,#324713,#324714),(#324715,#324716,#324717),(#324718,
#324719,#324720),(#324721,#324722,#324723),(#324724,#324725,#324726),(#324727,
#324728,#324729),(#324730,#324731,#324732),(#324733,#324734,#324735),(#324736,
#324737,#324738),(#324739,#324740,#324741),(#324742,#324743,#324744),(#324745,
#324746,#324747),(#324748,#324749,#324750),(#324751,#324752,#324753),(#324754,
#324755,#324756),(#324757,#324758,#324759),(#324760,#324761,#324762),(#324763,
#324764,#324765),(#324766,#324767,#324768),(#324769,#324770,#324771),(#324772,
#324773,#324774),(#324775,#324776,#324777),(#324778,#324779,#324780),(#324781,
#324782,#324783),(#324784,#324785,#324786),(#324787,#324788,#324789),(#324790,
#324791,#324792),(#324793,#324794,#324795),(#324796,#324797,#324798),(#324799,
#324800,#324801),(#324802,#324803,#324804),(#324805,#324806,#324807),(#324808,
#324809,#324810),(#324811,#324812,#324813),(#324814,#324815,#324816),(#324817,
#324818,#324819),(#324820,#324821,#324822),(#324823,#324824,#324825),(#324826,
#324827,#324828),(#324829,#324830,#324831),(#324832,#324833,#324834),(#324835,
#324836,#324837),(#324838,#324839,#324840),(#324841,#324842,#324843),(#324844,
#324845,#324846),(#324847,#324848,#324849),(#324850,#324851,#324852),(#324853,
#324854,#324855),(#324856,#324857,#324858),(#324859,#324860,#324861),(#324862,
#324863,#324864),(#324865,#324866,#324867),(#324868,#324869,#324870),(#324871,
#324872,#324873),(#324874,#324875,#324876),(#324877,#324878,#324879),(#324880,
#324881,#324882),(#324883,#324884,#324885),(#324886,#324887,#324888),(#324889,
#324890,#324891),(#324892,#324893,#324894),(#324895,#324896,#324897),(#324898,
#324899,#324900),(#324901,#324902,#324903),(#324904,#324905,#324906),(#324907,
#324908,#324909),(#324910,#324911,#324912),(#324913,#324914,#324915),(#324916,
#324917,#324918),(#324919,#324920,#324921),(#324922,#324923,#324924),(#324925,
#324926,#324927),(#324928,#324929,#324930),(#324931,#324932,#324933),(#324934,
#324935,#324936),(#324937,#324938,#324939),(#324940,#324941,#324942),(#324943,
#324944,#324945),(#324946,#324947,#324948),(#324949,#324950,#324951),(#324952,
#324953,#324954),(#324955,#324956,#324957),(#324958,#324959,#324960),(#324961,
#324962,#324963),(#324964,#324965,#324966),(#324967,#324968,#324969),(#324970,
#324971,#324972),(#324973,#324974,#324975),(#324976,#324977,#324978),(#324979,
#324980,#324981),(#324982,#324983,#324984),(#324985,#324986,#324987),(#324988,
#324989,#324990),(#324991,#324992,#324993),(#324994,#324995,#324996),(#324997,
#324998,#324999),(#325000,#325001,#325002),(#325003,#325004,#325005),(#325006,
#325007,#325008),(#325009,#325010,#325011),(#325012,#325013,#325014),(#325015,
#325016,#325017),(#325018,#325019,#325020),(#325021,#325022,#325023),(#325024,
#325025,#325026),(#325027,#325028,#325029),(#325030,#325031,#325032),(#325033,
#325034,#325035),(#325036,#325037,#325038),(#325039,#325040,#325041),(#325042,
#325043,#325044),(#325045,#325046,#325047),(#325048,#325049,#325050),(#325051,
#325052,#325053),(#325054,#325055,#325056),(#325057,#325058,#325059),(#325060,
#325061,#325062),(#325063,#325064,#325065),(#325066,#325067,#325068),(#325069,
#325070,#325071),(#325072,#325073,#325074),(#325075,#325076,#325077),(#325078,
#325079,#325080),(#325081,#325082,#325083),(#325084,#325085,#325086),(#325087,
#325088,#325089),(#325090,#325091,#325092),(#325093,#325094,#325095),(#325096,
#325097,#325098),(#325099,#325100,#325101),(#325102,#325103,#325104),(#325105,
#325106,#325107),(#325108,#325109,#325110),(#325111,#325112,#325113),(#325114,
#325115,#325116),(#325117,#325118,#325119),(#325120,#325121,#325122),(#325123,
#325124,#325125),(#325126,#325127,#325128),(#325129,#325130,#325131),(#325132,
#325133,#325134),(#325135,#325136,#325137),(#325138,#325139,#325140),(#325141,
#325142,#325143),(#325144,#325145,#325146),(#325147,#325148,#325149),(#325150,
#325151,#325152),(#325153,#325154,#325155),(#325156,#325157,#325158),(#325159,
#325160,#325161),(#325162,#325163,#325164),(#325165,#325166,#325167),(#325168,
#325169,#325170),(#325171,#325172,#325173),(#325174,#325175,#325176),(#325177,
#325178,#325179),(#325180,#325181,#325182),(#325183,#325184,#325185),(#325186,
#325187,#325188),(#325189,#325190,#325191),(#325192,#325193,#325194),(#325195,
#325196,#325197),(#325198,#325199,#325200),(#325201,#325202,#325203),(#325204,
#325205,#325206),(#325207,#325208,#325209),(#325210,#325211,#325212),(#325213,
#325214,#325215),(#325216,#325217,#325218),(#325219,#325220,#325221),(#325222,
#325223,#325224),(#325225,#325226,#325227),(#325228,#325229,#325230),(#325231,
#325232,#325233),(#325234,#325235,#325236),(#325237,#325238,#325239),(#325240,
#325241,#325242),(#325243,#325244,#325245),(#325246,#325247,#325248),(#325249,
#325250,#325251),(#325252,#325253,#325254),(#325255,#325256,#325257),(#325258,
#325259,#325260),(#325261,#325262,#325263),(#325264,#325265,#325266),(#325267,
#325268,#325269),(#325270,#325271,#325272),(#325273,#325274,#325275),(#325276,
#325277,#325278),(#325279,#325280,#325281),(#325282,#325283,#325284),(#325285,
#325286,#325287),(#325288,#325289,#325290),(#325291,#325292,#325293),(#325294,
#325295,#325296),(#325297,#325298,#325299),(#325300,#325301,#325302),(#325303,
#325304,#325305),(#325306,#325307,#325308),(#325309,#325310,#325311),(#325312,
#325313,#325314),(#325315,#325316,#325317),(#325318,#325319,#325320),(#325321,
#325322,#325323),(#325324,#325325,#325326),(#325327,#325328,#325329),(#325330,
#325331,#325332),(#325333,#325334,#325335),(#325336,#325337,#325338),(#325339,
#325340,#325341),(#325342,#325343,#325344),(#325345,#325346,#325347),(#325348,
#325349,#325350),(#325351,#325352,#325353),(#325354,#325355,#325356),(#325357,
#325358,#325359),(#325360,#325361,#325362),(#325363,#325364,#325365),(#325366,
#325367,#325368),(#325369,#325370,#325371),(#325372,#325373,#325374),(#325375,
#325376,#325377),(#325378,#325379,#325380),(#325381,#325382,#325383),(#325384,
#325385,#325386),(#325387,#325388,#325389),(#325390,#325391,#325392),(#325393,
#325394,#325395),(#325396,#325397,#325398),(#325399,#325400,#325401),(#325402,
#325403,#325404),(#325405,#325406,#325407),(#325408,#325409,#325410),(#325411,
#325412,#325413),(#325414,#325415,#325416),(#325417,#325418,#325419),(#325420,
#325421,#325422),(#325423,#325424,#325425),(#325426,#325427,#325428),(#325429,
#325430,#325431),(#325432,#325433,#325434),(#325435,#325436,#325437),(#325438,
#325439,#325440),(#325441,#325442,#325443),(#325444,#325445,#325446),(#325447,
#325448,#325449),(#325450,#325451,#325452),(#325453,#325454,#325455),(#325456,
#325457,#325458),(#325459,#325460,#325461),(#325462,#325463,#325464),(#325465,
#325466,#325467),(#325468,#325469,#325470),(#325471,#325472,#325473),(#325474,
#325475,#325476),(#325477,#325478,#325479),(#325480,#325481,#325482),(#325483,
#325484,#325485),(#325486,#325487,#325488),(#325489,#325490,#325491),(#325492,
#325493,#325494),(#325495,#325496,#325497),(#325498,#325499,#325500),(#325501,
#325502,#325503),(#325504,#325505,#325506),(#325507,#325508,#325509),(#325510,
#325511,#325512),(#325513,#325514,#325515),(#325516,#325517,#325518),(#325519,
#325520,#325521),(#325522,#325523,#325524),(#325525,#325526,#325527),(#325528,
#325529,#325530),(#325531,#325532,#325533),(#325534,#325535,#325536),(#325537,
#325538,#325539),(#325540,#325541,#325542),(#325543,#325544,#325545),(#325546,
#325547,#325548),(#325549,#325550,#325551),(#325552,#325553,#325554),(#325555,
#325556,#325557),(#325558,#325559,#325560),(#325561,#325562,#325563),(#325564,
#325565,#325566),(#325567,#325568,#325569),(#325570,#325571,#325572),(#325573,
#325574,#325575),(#325576,#325577,#325578),(#325579,#325580,#325581),(#325582,
#325583,#325584),(#325585,#325586,#325587),(#325588,#325589,#325590),(#325591,
#325592,#325593),(#325594,#325595,#325596),(#325597,#325598,#325599),(#325600,
#325601,#325602),(#325603,#325604,#325605),(#325606,#325607,#325608),(#325609,
#325610,#325611),(#325612,#325613,#325614),(#325615,#325616,#325617),(#325618,
#325619,#325620),(#325621,#325622,#325623),(#325624,#325625,#325626),(#325627,
#325628,#325629),(#325630,#325631,#325632),(#325633,#325634,#325635),(#325636,
#325637,#325638),(#325639,#325640,#325641),(#325642,#325643,#325644),(#325645,
#325646,#325647),(#325648,#325649,#325650),(#325651,#325652,#325653),(#325654,
#325655,#325656),(#325657,#325658,#325659),(#325660,#325661,#325662),(#325663,
#325664,#325665),(#325666,#325667,#325668),(#325669,#325670,#325671),(#325672,
#325673,#325674),(#325675,#325676,#325677),(#325678,#325679,#325680),(#325681,
#325682,#325683),(#325684,#325685,#325686),(#325687,#325688,#325689),(#325690,
#325691,#325692),(#325693,#325694,#325695),(#325696,#325697,#325698),(#325699,
#325700,#325701),(#325702,#325703,#325704),(#325705,#325706,#325707),(#325708,
#325709,#325710),(#325711,#325712,#325713),(#325714,#325715,#325716),(#325717,
#325718,#325719),(#325720,#325721,#325722),(#325723,#325724,#325725),(#325726,
#325727,#325728),(#325729,#325730,#325731),(#325732,#325733,#325734),(#325735,
#325736,#325737),(#325738,#325739,#325740),(#325741,#325742,#325743),(#325744,
#325745,#325746),(#325747,#325748,#325749),(#325750,#325751,#325752),(#325753,
#325754,#325755),(#325756,#325757,#325758),(#325759,#325760,#325761),(#325762,
#325763,#325764),(#325765,#325766,#325767),(#325768,#325769,#325770),(#325771,
#325772,#325773),(#325774,#325775,#325776),(#325777,#325778,#325779),(#325780,
#325781,#325782),(#325783,#325784,#325785),(#325786,#325787,#325788),(#325789,
#325790,#325791),(#325792,#325793,#325794),(#325795,#325796,#325797),(#325798,
#325799,#325800),(#325801,#325802,#325803),(#325804,#325805,#325806),(#325807,
#325808,#325809),(#325810,#325811,#325812),(#325813,#325814,#325815),(#325816,
#325817,#325818),(#325819,#325820,#325821),(#325822,#325823,#325824),(#325825,
#325826,#325827),(#325828,#325829,#325830),(#325831,#325832,#325833),(#325834,
#325835,#325836),(#325837,#325838,#325839),(#325840,#325841,#325842),(#325843,
#325844,#325845),(#325846,#325847,#325848),(#325849,#325850,#325851),(#325852,
#325853,#325854),(#325855,#325856,#325857),(#325858,#325859,#325860),(#325861,
#325862,#325863),(#325864,#325865,#325866),(#325867,#325868,#325869),(#325870,
#325871,#325872),(#325873,#325874,#325875),(#325876,#325877,#325878),(#325879,
#325880,#325881),(#325882,#325883,#325884),(#325885,#325886,#325887),(#325888,
#325889,#325890),(#325891,#325892,#325893),(#325894,#325895,#325896),(#325897,
#325898,#325899),(#325900,#325901,#325902),(#325903,#325904,#325905),(#325906,
#325907,#325908),(#325909,#325910,#325911),(#325912,#325913,#325914),(#325915,
#325916,#325917),(#325918,#325919,#325920),(#325921,#325922,#325923),(#325924,
#325925,#325926),(#325927,#325928,#325929),(#325930,#325931,#325932),(#325933,
#325934,#325935),(#325936,#325937,#325938),(#325939,#325940,#325941),(#325942,
#325943,#325944),(#325945,#325946,#325947),(#325948,#325949,#325950),(#325951,
#325952,#325953),(#325954,#325955,#325956),(#325957,#325958,#325959),(#325960,
#325961,#325962),(#325963,#325964,#325965),(#325966,#325967,#325968),(#325969,
#325970,#325971),(#325972,#325973,#325974),(#325975,#325976,#325977),(#325978,
#325979,#325980),(#325981,#325982,#325983),(#325984,#325985,#325986),(#325987,
#325988,#325989),(#325990,#325991,#325992),(#325993,#325994,#325995),(#325996,
#325997,#325998),(#325999,#326000,#326001),(#326002,#326003,#326004),(#326005,
#326006,#326007),(#326008,#326009,#326010),(#326011,#326012,#326013),(#326014,
#326015,#326016),(#326017,#326018,#326019),(#326020,#326021,#326022),(#326023,
#326024,#326025),(#326026,#326027,#326028),(#326029,#326030,#326031),(#326032,
#326033,#326034),(#326035,#326036,#326037),(#326038,#326039,#326040),(#326041,
#326042,#326043),(#326044,#326045,#326046),(#326047,#326048,#326049),(#326050,
#326051,#326052),(#326053,#326054,#326055),(#326056,#326057,#326058),(#326059,
#326060,#326061),(#326062,#326063,#326064),(#326065,#326066,#326067),(#326068,
#326069,#326070),(#326071,#326072,#326073),(#326074,#326075,#326076),(#326077,
#326078,#326079),(#326080,#326081,#326082),(#326083,#326084,#326085),(#326086,
#326087,#326088),(#326089,#326090,#326091),(#326092,#326093,#326094),(#326095,
#326096,#326097),(#326098,#326099,#326100),(#326101,#326102,#326103),(#326104,
#326105,#326106),(#326107,#326108,#326109),(#326110,#326111,#326112),(#326113,
#326114,#326115),(#326116,#326117,#326118),(#326119,#326120,#326121),(#326122,
#326123,#326124),(#326125,#326126,#326127),(#326128,#326129,#326130),(#326131,
#326132,#326133),(#326134,#326135,#326136),(#326137,#326138,#326139),(#326140,
#326141,#326142),(#326143,#326144,#326145),(#326146,#326147,#326148),(#326149,
#326150,#326151),(#326152,#326153,#326154),(#326155,#326156,#326157),(#326158,
#326159,#326160),(#326161,#326162,#326163),(#326164,#326165,#326166),(#326167,
#326168,#326169),(#326170,#326171,#326172),(#326173,#326174,#326175),(#326176,
#326177,#326178),(#326179,#326180,#326181),(#326182,#326183,#326184),(#326185,
#326186,#326187),(#326188,#326189,#326190),(#326191,#326192,#326193),(#326194,
#326195,#326196),(#326197,#326198,#326199),(#326200,#326201,#326202),(#326203,
#326204,#326205),(#326206,#326207,#326208),(#326209,#326210,#326211),(#326212,
#326213,#326214),(#326215,#326216,#326217),(#326218,#326219,#326220),(#326221,
#326222,#326223),(#326224,#326225,#326226),(#326227,#326228,#326229),(#326230,
#326231,#326232),(#326233,#326234,#326235),(#326236,#326237,#326238),(#326239,
#326240,#326241),(#326242,#326243,#326244),(#326245,#326246,#326247),(#326248,
#326249,#326250),(#326251,#326252,#326253),(#326254,#326255,#326256),(#326257,
#326258,#326259),(#326260,#326261,#326262),(#326263,#326264,#326265),(#326266,
#326267,#326268),(#326269,#326270,#326271),(#326272,#326273,#326274),(#326275,
#326276,#326277),(#326278,#326279,#326280),(#326281,#326282,#326283),(#326284,
#326285,#326286),(#326287,#326288,#326289),(#326290,#326291,#326292),(#326293,
#326294,#326295),(#326296,#326297,#326298),(#326299,#326300,#326301),(#326302,
#326303,#326304),(#326305,#326306,#326307),(#326308,#326309,#326310),(#326311,
#326312,#326313),(#326314,#326315,#326316),(#326317,#326318,#326319),(#326320,
#326321,#326322),(#326323,#326324,#326325),(#326326,#326327,#326328),(#326329,
#326330,#326331),(#326332,#326333,#326334),(#326335,#326336,#326337),(#326338,
#326339,#326340),(#326341,#326342,#326343),(#326344,#326345,#326346),(#326347,
#326348,#326349),(#326350,#326351,#326352),(#326353,#326354,#326355)),
 .UNSPECIFIED.,.F.,.F.,.F.,(6,1,1,1,1,1,1,1,1,1,1,1,1,1,1,1,1,1,1,1,1,1,
1,1,1,1,1,1,1,1,1,1,1,1,1,1,1,1,1,1,1,1,1,1,1,1,1,1,1,1,1,1,1,1,1,1,1,1,
1,1,1,1,1,1,1,1,1,1,1,1,1,1,1,1,1,1,1,1,1,1,1,1,1,1,1,1,1,1,1,1,1,1,1,1,
1,1,1,1,1,1,1,1,1,1,1,1,1,1,1,1,1,1,1,1,1,1,1,1,1,1,1,1,1,1,1,1,1,1,1,1,
1,1,1,1,1,1,1,1,1,1,1,1,1,1,1,1,1,1,1,1,1,1,1,1,1,1,1,1,1,1,1,1,1,1,1,1,
1,1,1,1,1,1,1,1,1,1,1,1,1,1,1,1,1,1,1,1,1,1,1,1,1,1,1,1,1,1,1,1,1,1,1,1,
1,1,1,1,1,1,1,1,1,1,1,1,1,1,1,1,1,1,1,1,1,1,1,1,1,1,1,1,1,1,1,1,1,1,1,1,
1,1,1,1,1,1,1,1,1,1,1,1,1,1,1,1,1,1,1,1,1,1,1,1,1,1,1,1,1,1,1,1,1,1,1,1,
1,1,1,1,1,1,1,1,1,1,1,1,1,1,1,1,1,1,1,1,1,1,1,1,1,1,1,1,1,1,1,1,1,1,1,1,
1,1,1,1,1,1,1,1,1,1,1,1,1,1,1,1,1,1,1,1,1,1,1,1,1,1,1,1,1,1,1,1,1,1,1,1,
1,1,1,1,1,1,1,1,1,1,1,1,1,1,1,1,1,1,1,1,1,1,1,1,1,1,1,1,1,1,1,1,1,1,1,1,
1,1,1,1,1,1,1,1,1,1,1,1,1,1,1,1,1,1,1,1,1,1,1,1,1,1,1,1,1,1,1,1,1,1,1,1,
1,1,1,1,1,1,1,1,1,1,1,1,1,1,1,1,1,1,1,1,1,1,1,1,1,1,1,1,1,1,1,1,1,1,1,1,
1,1,1,1,1,1,1,1,1,1,1,1,1,1,1,1,1,1,1,1,1,1,1,1,1,1,1,1,1,1,1,1,1,1,1,1,
1,1,1,1,1,1,1,1,1,1,1,1,1,1,1,1,1,1,1,1,1,1,1,1,1,1,1,1,1,1,1,1,1,1,1,1,
1,1,1,1,1,1,1,1,1,1,1,1,1,1,1,1,1,1,1,6),(2,1,2),(-1.,-0.998165138,-0.996330275,
-0.994495413,-0.99266055,-0.990825688,-0.988990826,-0.987155963,-0.985321101,
-0.983486239,-0.981651376,-0.979816514,-0.977981651,-0.976146789,-0.974311927,
-0.972477064,-0.970642202,-0.968807339,-0.966972477,-0.965137615,-0.963302752,
-0.96146789,-0.959633028,-0.957798165,-0.955963303,-0.95412844,-0.952293578,
-0.950458716,-0.948623853,-0.946788991,-0.944954128,-0.943119266,-0.941284404,
-0.939449541,-0.937614679,-0.935779817,-0.933944954,-0.932110092,-0.930275229,
-0.928440367,-0.926605505,-0.924770642,-0.92293578,-0.921100917,-0.919266055,
-0.917431193,-0.91559633,-0.913761468,-0.911926606,-0.910091743,-0.908256881,
-0.906422018,-0.904587156,-0.902752294,-0.900917431,-0.899082569,-0.897247706,
-0.895412844,-0.893577982,-0.891743119,-0.889908257,-0.888073394,-0.886238532,
-0.88440367,-0.882568807,-0.880733945,-0.878899083,-0.87706422,-0.875229358,
-0.873394495,-0.871559633,-0.869724771,-0.867889908,-0.866055046,-0.864220183,
-0.862385321,-0.860550459,-0.858715596,-0.856880734,-0.855045872,-0.853211009,
-0.851376147,-0.849541284,-0.847706422,-0.84587156,-0.844036697,-0.842201835,
-0.840366972,-0.83853211,-0.836697248,-0.834862385,-0.833027523,-0.831192661,
-0.829357798,-0.827522936,-0.825688073,-0.823853211,-0.822018349,-0.820183486,
-0.818348624,-0.816513761,-0.814678899,-0.812844037,-0.811009174,-0.809174312,
-0.80733945,-0.805504587,-0.803669725,-0.801834862,-0.8,-0.798165138,-0.796330275,
-0.794495413,-0.79266055,-0.790825688,-0.788990826,-0.787155963,-0.785321101,
-0.783486239,-0.781651376,-0.779816514,-0.777981651,-0.776146789,-0.774311927,
-0.772477064,-0.770642202,-0.768807339,-0.766972477,-0.765137615,-0.763302752,
-0.76146789,-0.759633028,-0.757798165,-0.755963303,-0.75412844,-0.752293578,
-0.750458716,-0.748623853,-0.746788991,-0.744954128,-0.743119266,-0.741284404,
-0.739449541,-0.737614679,-0.735779817,-0.733944954,-0.732110092,-0.730275229,
-0.728440367,-0.726605505,-0.724770642,-0.72293578,-0.721100917,-0.719266055,
-0.717431193,-0.71559633,-0.713761468,-0.711926606,-0.710091743,-0.708256881,
-0.706422018,-0.704587156,-0.702752294,-0.700917431,-0.699082569,-0.697247706,
-0.695412844,-0.693577982,-0.691743119,-0.689908257,-0.688073394,-0.686238532,
-0.68440367,-0.682568807,-0.680733945,-0.678899083,-0.67706422,-0.675229358,
-0.673394495,-0.671559633,-0.669724771,-0.667889908,-0.666055046,-0.664220183,
-0.662385321,-0.660550459,-0.658715596,-0.656880734,-0.655045872,-0.653211009,
-0.651376147,-0.649541284,-0.647706422,-0.64587156,-0.644036697,-0.642201835,
-0.640366972,-0.63853211,-0.636697248,-0.634862385,-0.633027523,-0.631192661,
-0.629357798,-0.627522936,-0.625688073,-0.623853211,-0.622018349,-0.620183486,
-0.618348624,-0.616513761,-0.614678899,-0.612844037,-0.611009174,-0.609174312,
-0.60733945,-0.605504587,-0.603669725,-0.601834862,-0.6,-0.598165138,-0.596330275,
-0.594495413,-0.59266055,-0.590825688,-0.588990826,-0.587155963,-0.585321101,
-0.583486239,-0.581651376,-0.579816514,-0.577981651,-0.576146789,-0.574311927,
-0.572477064,-0.570642202,-0.568807339,-0.566972477,-0.565137615,-0.563302752,
-0.56146789,-0.559633028,-0.557798165,-0.555963303,-0.55412844,-0.552293578,
-0.550458716,-0.548623853,-0.546788991,-0.544954128,-0.543119266,-0.541284404,
-0.539449541,-0.537614679,-0.535779817,-0.533944954,-0.532110092,-0.530275229,
-0.528440367,-0.526605505,-0.524770642,-0.52293578,-0.521100917,-0.519266055,
-0.517431193,-0.51559633,-0.513761468,-0.511926606,-0.510091743,-0.508256881,
-0.506422018,-0.504587156,-0.502752294,-0.500917431,-0.499082569,-0.497247706,
-0.495412844,-0.493577982,-0.491743119,-0.489908257,-0.488073394,-0.486238532,
-0.48440367,-0.482568807,-0.480733945,-0.478899083,-0.47706422,-0.475229358,
-0.473394495,-0.471559633,-0.469724771,-0.467889908,-0.466055046,-0.464220183,
-0.462385321,-0.460550459,-0.458715596,-0.456880734,-0.455045872,-0.453211009,
-0.451376147,-0.449541284,-0.447706422,-0.44587156,-0.444036697,-0.442201835,
-0.440366972,-0.43853211,-0.436697248,-0.434862385,-0.433027523,-0.431192661,
-0.429357798,-0.427522936,-0.425688073,-0.423853211,-0.422018349,-0.420183486,
-0.418348624,-0.416513761,-0.414678899,-0.412844037,-0.411009174,-0.409174312,
-0.40733945,-0.405504587,-0.403669725,-0.401834862,-0.4,-0.398165138,-0.396330275,
-0.394495413,-0.39266055,-0.390825688,-0.388990826,-0.387155963,-0.385321101,
-0.383486239,-0.381651376,-0.379816514,-0.377981651,-0.376146789,-0.374311927,
-0.372477064,-0.370642202,-0.368807339,-0.366972477,-0.365137615,-0.363302752,
-0.36146789,-0.359633028,-0.357798165,-0.355963303,-0.35412844,-0.352293578,
-0.350458716,-0.348623853,-0.346788991,-0.344954128,-0.343119266,-0.341284404,
-0.339449541,-0.337614679,-0.335779817,-0.333944954,-0.332110092,-0.330275229,
-0.328440367,-0.326605505,-0.324770642,-0.32293578,-0.321100917,-0.319266055,
-0.317431193,-0.31559633,-0.313761468,-0.311926606,-0.310091743,-0.308256881,
-0.306422018,-0.304587156,-0.302752294,-0.300917431,-0.299082569,-0.297247706,
-0.295412844,-0.293577982,-0.291743119,-0.289908257,-0.288073394,-0.286238532,
-0.28440367,-0.282568807,-0.280733945,-0.278899083,-0.27706422,-0.275229358,
-0.273394495,-0.271559633,-0.269724771,-0.267889908,-0.266055046,-0.264220183,
-0.262385321,-0.260550459,-0.258715596,-0.256880734,-0.255045872,-0.253211009,
-0.251376147,-0.249541284,-0.247706422,-0.24587156,-0.244036697,-0.242201835,
-0.240366972,-0.23853211,-0.236697248,-0.234862385,-0.233027523,-0.231192661,
-0.229357798,-0.227522936,-0.225688073,-0.223853211,-0.222018349,-0.220183486,
-0.218348624,-0.216513761,-0.214678899,-0.212844037,-0.211009174,-0.209174312,
-0.20733945,-0.205504587,-0.203669725,-0.201834862,-0.2,-0.198165138,-0.196330275,
-0.194495413,-0.19266055,-0.190825688,-0.188990826,-0.187155963,-0.185321101,
-0.183486239,-0.181651376,-0.179816514,-0.177981651,-0.176146789,-0.174311927,
-0.172477064,-0.170642202,-0.168807339,-0.166972477,-0.165137615,-0.163302752,
-0.16146789,-0.159633028,-0.157798165,-0.155963303,-0.15412844,-0.152293578,
-0.150458716,-0.148623853,-0.146788991,-0.144954128,-0.143119266,-0.141284404,
-0.139449541,-0.137614679,-0.135779817,-0.133944954,-0.132110092,-0.130275229,
-0.128440367,-0.126605505,-0.124770642,-0.12293578,-0.121100917,-0.119266055,
-0.117431193,-0.11559633,-0.113761468,-0.111926606,-0.110091743,-0.108256881,
-0.106422018,-0.104587156,-0.102752294,-0.100917431,-0.099082569,-0.097247706,
-0.095412844,-0.093577982,-0.091743119,-0.089908257,-0.088073394,-0.086238532,
-0.08440367,-0.082568807,-0.080733945,-0.078899083,-0.07706422,-0.075229358,
-0.073394495,-0.071559633,-0.069724771,-0.067889908,-0.066055046,-0.064220183,
-0.062385321,-0.060550459,-0.058715596,-0.056880734,-0.055045872,-0.053211009,
-0.051376147,-0.049541284,-0.047706422,-0.04587156,-0.044036697,-0.042201835,
-0.040366972,-0.03853211,-0.036697248,-0.034862385,-0.033027523,-0.031192661,
-0.029357798,-0.027522936,-0.025688073,-0.023853211,-0.022018349,-0.020183486,
-0.018348624,-0.016513761,-0.014678899,-0.012844037,-0.011009174,-0.009174312,
-0.00733945,-0.005504587,-0.003669725,-0.001834862,0.000982147),(0.3,1.,
1.3),.UNSPECIFIED.);
#6318=B_SPLINE_SURFACE_WITH_KNOTS('',5,1,((#326378,#326379,#326380),(#326381,
#326382,#326383),(#326384,#326385,#326386),(#326387,#326388,#326389),(#326390,
#326391,#326392),(#326393,#326394,#326395),(#326396,#326397,#326398),(#326399,
#326400,#326401),(#326402,#326403,#326404),(#326405,#326406,#326407),(#326408,
#326409,#326410),(#326411,#326412,#326413),(#326414,#326415,#326416),(#326417,
#326418,#326419),(#326420,#326421,#326422),(#326423,#326424,#326425),(#326426,
#326427,#326428),(#326429,#326430,#326431),(#326432,#326433,#326434),(#326435,
#326436,#326437),(#326438,#326439,#326440),(#326441,#326442,#326443),(#326444,
#326445,#326446),(#326447,#326448,#326449),(#326450,#326451,#326452),(#326453,
#326454,#326455),(#326456,#326457,#326458),(#326459,#326460,#326461),(#326462,
#326463,#326464),(#326465,#326466,#326467),(#326468,#326469,#326470),(#326471,
#326472,#326473),(#326474,#326475,#326476),(#326477,#326478,#326479),(#326480,
#326481,#326482),(#326483,#326484,#326485),(#326486,#326487,#326488),(#326489,
#326490,#326491),(#326492,#326493,#326494),(#326495,#326496,#326497),(#326498,
#326499,#326500),(#326501,#326502,#326503),(#326504,#326505,#326506),(#326507,
#326508,#326509),(#326510,#326511,#326512),(#326513,#326514,#326515),(#326516,
#326517,#326518),(#326519,#326520,#326521),(#326522,#326523,#326524),(#326525,
#326526,#326527),(#326528,#326529,#326530),(#326531,#326532,#326533),(#326534,
#326535,#326536),(#326537,#326538,#326539),(#326540,#326541,#326542),(#326543,
#326544,#326545),(#326546,#326547,#326548),(#326549,#326550,#326551),(#326552,
#326553,#326554),(#326555,#326556,#326557),(#326558,#326559,#326560),(#326561,
#326562,#326563),(#326564,#326565,#326566),(#326567,#326568,#326569),(#326570,
#326571,#326572),(#326573,#326574,#326575),(#326576,#326577,#326578),(#326579,
#326580,#326581),(#326582,#326583,#326584),(#326585,#326586,#326587),(#326588,
#326589,#326590),(#326591,#326592,#326593),(#326594,#326595,#326596),(#326597,
#326598,#326599),(#326600,#326601,#326602),(#326603,#326604,#326605),(#326606,
#326607,#326608),(#326609,#326610,#326611),(#326612,#326613,#326614),(#326615,
#326616,#326617),(#326618,#326619,#326620),(#326621,#326622,#326623),(#326624,
#326625,#326626),(#326627,#326628,#326629),(#326630,#326631,#326632),(#326633,
#326634,#326635),(#326636,#326637,#326638),(#326639,#326640,#326641),(#326642,
#326643,#326644),(#326645,#326646,#326647),(#326648,#326649,#326650),(#326651,
#326652,#326653),(#326654,#326655,#326656),(#326657,#326658,#326659),(#326660,
#326661,#326662),(#326663,#326664,#326665),(#326666,#326667,#326668),(#326669,
#326670,#326671),(#326672,#326673,#326674),(#326675,#326676,#326677),(#326678,
#326679,#326680),(#326681,#326682,#326683),(#326684,#326685,#326686),(#326687,
#326688,#326689),(#326690,#326691,#326692),(#326693,#326694,#326695),(#326696,
#326697,#326698),(#326699,#326700,#326701),(#326702,#326703,#326704),(#326705,
#326706,#326707),(#326708,#326709,#326710),(#326711,#326712,#326713),(#326714,
#326715,#326716),(#326717,#326718,#326719),(#326720,#326721,#326722),(#326723,
#326724,#326725),(#326726,#326727,#326728),(#326729,#326730,#326731),(#326732,
#326733,#326734),(#326735,#326736,#326737),(#326738,#326739,#326740),(#326741,
#326742,#326743),(#326744,#326745,#326746),(#326747,#326748,#326749),(#326750,
#326751,#326752),(#326753,#326754,#326755),(#326756,#326757,#326758),(#326759,
#326760,#326761),(#326762,#326763,#326764),(#326765,#326766,#326767),(#326768,
#326769,#326770),(#326771,#326772,#326773),(#326774,#326775,#326776),(#326777,
#326778,#326779),(#326780,#326781,#326782),(#326783,#326784,#326785),(#326786,
#326787,#326788),(#326789,#326790,#326791),(#326792,#326793,#326794),(#326795,
#326796,#326797),(#326798,#326799,#326800),(#326801,#326802,#326803),(#326804,
#326805,#326806),(#326807,#326808,#326809),(#326810,#326811,#326812),(#326813,
#326814,#326815),(#326816,#326817,#326818),(#326819,#326820,#326821),(#326822,
#326823,#326824),(#326825,#326826,#326827),(#326828,#326829,#326830),(#326831,
#326832,#326833),(#326834,#326835,#326836),(#326837,#326838,#326839),(#326840,
#326841,#326842),(#326843,#326844,#326845),(#326846,#326847,#326848),(#326849,
#326850,#326851),(#326852,#326853,#326854),(#326855,#326856,#326857),(#326858,
#326859,#326860),(#326861,#326862,#326863),(#326864,#326865,#326866),(#326867,
#326868,#326869),(#326870,#326871,#326872),(#326873,#326874,#326875),(#326876,
#326877,#326878),(#326879,#326880,#326881),(#326882,#326883,#326884),(#326885,
#326886,#326887),(#326888,#326889,#326890),(#326891,#326892,#326893),(#326894,
#326895,#326896),(#326897,#326898,#326899),(#326900,#326901,#326902),(#326903,
#326904,#326905),(#326906,#326907,#326908),(#326909,#326910,#326911),(#326912,
#326913,#326914),(#326915,#326916,#326917),(#326918,#326919,#326920),(#326921,
#326922,#326923),(#326924,#326925,#326926),(#326927,#326928,#326929),(#326930,
#326931,#326932),(#326933,#326934,#326935),(#326936,#326937,#326938),(#326939,
#326940,#326941),(#326942,#326943,#326944),(#326945,#326946,#326947),(#326948,
#326949,#326950),(#326951,#326952,#326953),(#326954,#326955,#326956),(#326957,
#326958,#326959),(#326960,#326961,#326962),(#326963,#326964,#326965),(#326966,
#326967,#326968),(#326969,#326970,#326971),(#326972,#326973,#326974),(#326975,
#326976,#326977),(#326978,#326979,#326980),(#326981,#326982,#326983),(#326984,
#326985,#326986),(#326987,#326988,#326989),(#326990,#326991,#326992),(#326993,
#326994,#326995),(#326996,#326997,#326998),(#326999,#327000,#327001),(#327002,
#327003,#327004),(#327005,#327006,#327007),(#327008,#327009,#327010),(#327011,
#327012,#327013),(#327014,#327015,#327016),(#327017,#327018,#327019),(#327020,
#327021,#327022),(#327023,#327024,#327025),(#327026,#327027,#327028),(#327029,
#327030,#327031),(#327032,#327033,#327034),(#327035,#327036,#327037),(#327038,
#327039,#327040),(#327041,#327042,#327043),(#327044,#327045,#327046),(#327047,
#327048,#327049),(#327050,#327051,#327052),(#327053,#327054,#327055),(#327056,
#327057,#327058),(#327059,#327060,#327061),(#327062,#327063,#327064),(#327065,
#327066,#327067),(#327068,#327069,#327070),(#327071,#327072,#327073),(#327074,
#327075,#327076),(#327077,#327078,#327079),(#327080,#327081,#327082),(#327083,
#327084,#327085),(#327086,#327087,#327088),(#327089,#327090,#327091),(#327092,
#327093,#327094),(#327095,#327096,#327097),(#327098,#327099,#327100),(#327101,
#327102,#327103),(#327104,#327105,#327106),(#327107,#327108,#327109),(#327110,
#327111,#327112),(#327113,#327114,#327115),(#327116,#327117,#327118),(#327119,
#327120,#327121),(#327122,#327123,#327124),(#327125,#327126,#327127),(#327128,
#327129,#327130),(#327131,#327132,#327133),(#327134,#327135,#327136),(#327137,
#327138,#327139),(#327140,#327141,#327142),(#327143,#327144,#327145),(#327146,
#327147,#327148),(#327149,#327150,#327151),(#327152,#327153,#327154),(#327155,
#327156,#327157),(#327158,#327159,#327160),(#327161,#327162,#327163),(#327164,
#327165,#327166),(#327167,#327168,#327169),(#327170,#327171,#327172),(#327173,
#327174,#327175),(#327176,#327177,#327178),(#327179,#327180,#327181),(#327182,
#327183,#327184),(#327185,#327186,#327187),(#327188,#327189,#327190),(#327191,
#327192,#327193),(#327194,#327195,#327196),(#327197,#327198,#327199),(#327200,
#327201,#327202),(#327203,#327204,#327205),(#327206,#327207,#327208),(#327209,
#327210,#327211),(#327212,#327213,#327214),(#327215,#327216,#327217),(#327218,
#327219,#327220),(#327221,#327222,#327223),(#327224,#327225,#327226),(#327227,
#327228,#327229),(#327230,#327231,#327232),(#327233,#327234,#327235),(#327236,
#327237,#327238),(#327239,#327240,#327241),(#327242,#327243,#327244),(#327245,
#327246,#327247),(#327248,#327249,#327250),(#327251,#327252,#327253),(#327254,
#327255,#327256),(#327257,#327258,#327259),(#327260,#327261,#327262),(#327263,
#327264,#327265),(#327266,#327267,#327268),(#327269,#327270,#327271),(#327272,
#327273,#327274),(#327275,#327276,#327277),(#327278,#327279,#327280),(#327281,
#327282,#327283),(#327284,#327285,#327286),(#327287,#327288,#327289),(#327290,
#327291,#327292),(#327293,#327294,#327295),(#327296,#327297,#327298),(#327299,
#327300,#327301),(#327302,#327303,#327304),(#327305,#327306,#327307),(#327308,
#327309,#327310),(#327311,#327312,#327313),(#327314,#327315,#327316),(#327317,
#327318,#327319),(#327320,#327321,#327322),(#327323,#327324,#327325),(#327326,
#327327,#327328),(#327329,#327330,#327331),(#327332,#327333,#327334),(#327335,
#327336,#327337),(#327338,#327339,#327340),(#327341,#327342,#327343),(#327344,
#327345,#327346),(#327347,#327348,#327349),(#327350,#327351,#327352),(#327353,
#327354,#327355),(#327356,#327357,#327358),(#327359,#327360,#327361),(#327362,
#327363,#327364),(#327365,#327366,#327367),(#327368,#327369,#327370),(#327371,
#327372,#327373),(#327374,#327375,#327376),(#327377,#327378,#327379),(#327380,
#327381,#327382),(#327383,#327384,#327385),(#327386,#327387,#327388),(#327389,
#327390,#327391),(#327392,#327393,#327394),(#327395,#327396,#327397),(#327398,
#327399,#327400),(#327401,#327402,#327403),(#327404,#327405,#327406),(#327407,
#327408,#327409),(#327410,#327411,#327412),(#327413,#327414,#327415),(#327416,
#327417,#327418),(#327419,#327420,#327421),(#327422,#327423,#327424),(#327425,
#327426,#327427),(#327428,#327429,#327430),(#327431,#327432,#327433),(#327434,
#327435,#327436),(#327437,#327438,#327439),(#327440,#327441,#327442),(#327443,
#327444,#327445),(#327446,#327447,#327448),(#327449,#327450,#327451),(#327452,
#327453,#327454),(#327455,#327456,#327457),(#327458,#327459,#327460),(#327461,
#327462,#327463),(#327464,#327465,#327466),(#327467,#327468,#327469),(#327470,
#327471,#327472),(#327473,#327474,#327475),(#327476,#327477,#327478),(#327479,
#327480,#327481),(#327482,#327483,#327484),(#327485,#327486,#327487),(#327488,
#327489,#327490),(#327491,#327492,#327493),(#327494,#327495,#327496),(#327497,
#327498,#327499),(#327500,#327501,#327502),(#327503,#327504,#327505),(#327506,
#327507,#327508),(#327509,#327510,#327511),(#327512,#327513,#327514),(#327515,
#327516,#327517),(#327518,#327519,#327520),(#327521,#327522,#327523),(#327524,
#327525,#327526),(#327527,#327528,#327529),(#327530,#327531,#327532),(#327533,
#327534,#327535),(#327536,#327537,#327538),(#327539,#327540,#327541),(#327542,
#327543,#327544),(#327545,#327546,#327547),(#327548,#327549,#327550),(#327551,
#327552,#327553),(#327554,#327555,#327556),(#327557,#327558,#327559),(#327560,
#327561,#327562),(#327563,#327564,#327565),(#327566,#327567,#327568),(#327569,
#327570,#327571),(#327572,#327573,#327574),(#327575,#327576,#327577),(#327578,
#327579,#327580),(#327581,#327582,#327583),(#327584,#327585,#327586),(#327587,
#327588,#327589),(#327590,#327591,#327592),(#327593,#327594,#327595),(#327596,
#327597,#327598),(#327599,#327600,#327601),(#327602,#327603,#327604),(#327605,
#327606,#327607),(#327608,#327609,#327610),(#327611,#327612,#327613),(#327614,
#327615,#327616),(#327617,#327618,#327619),(#327620,#327621,#327622),(#327623,
#327624,#327625),(#327626,#327627,#327628),(#327629,#327630,#327631),(#327632,
#327633,#327634),(#327635,#327636,#327637),(#327638,#327639,#327640),(#327641,
#327642,#327643),(#327644,#327645,#327646),(#327647,#327648,#327649),(#327650,
#327651,#327652),(#327653,#327654,#327655),(#327656,#327657,#327658),(#327659,
#327660,#327661),(#327662,#327663,#327664),(#327665,#327666,#327667),(#327668,
#327669,#327670),(#327671,#327672,#327673),(#327674,#327675,#327676),(#327677,
#327678,#327679),(#327680,#327681,#327682),(#327683,#327684,#327685),(#327686,
#327687,#327688),(#327689,#327690,#327691),(#327692,#327693,#327694),(#327695,
#327696,#327697),(#327698,#327699,#327700),(#327701,#327702,#327703),(#327704,
#327705,#327706),(#327707,#327708,#327709),(#327710,#327711,#327712),(#327713,
#327714,#327715),(#327716,#327717,#327718),(#327719,#327720,#327721),(#327722,
#327723,#327724),(#327725,#327726,#327727),(#327728,#327729,#327730),(#327731,
#327732,#327733),(#327734,#327735,#327736),(#327737,#327738,#327739),(#327740,
#327741,#327742),(#327743,#327744,#327745),(#327746,#327747,#327748),(#327749,
#327750,#327751),(#327752,#327753,#327754),(#327755,#327756,#327757),(#327758,
#327759,#327760),(#327761,#327762,#327763),(#327764,#327765,#327766),(#327767,
#327768,#327769),(#327770,#327771,#327772),(#327773,#327774,#327775),(#327776,
#327777,#327778),(#327779,#327780,#327781),(#327782,#327783,#327784),(#327785,
#327786,#327787),(#327788,#327789,#327790),(#327791,#327792,#327793),(#327794,
#327795,#327796),(#327797,#327798,#327799),(#327800,#327801,#327802),(#327803,
#327804,#327805),(#327806,#327807,#327808),(#327809,#327810,#327811),(#327812,
#327813,#327814),(#327815,#327816,#327817),(#327818,#327819,#327820),(#327821,
#327822,#327823),(#327824,#327825,#327826),(#327827,#327828,#327829),(#327830,
#327831,#327832),(#327833,#327834,#327835),(#327836,#327837,#327838),(#327839,
#327840,#327841),(#327842,#327843,#327844),(#327845,#327846,#327847),(#327848,
#327849,#327850),(#327851,#327852,#327853),(#327854,#327855,#327856),(#327857,
#327858,#327859),(#327860,#327861,#327862),(#327863,#327864,#327865),(#327866,
#327867,#327868),(#327869,#327870,#327871),(#327872,#327873,#327874),(#327875,
#327876,#327877),(#327878,#327879,#327880),(#327881,#327882,#327883),(#327884,
#327885,#327886),(#327887,#327888,#327889),(#327890,#327891,#327892),(#327893,
#327894,#327895),(#327896,#327897,#327898),(#327899,#327900,#327901),(#327902,
#327903,#327904),(#327905,#327906,#327907),(#327908,#327909,#327910),(#327911,
#327912,#327913),(#327914,#327915,#327916),(#327917,#327918,#327919),(#327920,
#327921,#327922),(#327923,#327924,#327925),(#327926,#327927,#327928),(#327929,
#327930,#327931),(#327932,#327933,#327934),(#327935,#327936,#327937),(#327938,
#327939,#327940),(#327941,#327942,#327943),(#327944,#327945,#327946),(#327947,
#327948,#327949),(#327950,#327951,#327952),(#327953,#327954,#327955),(#327956,
#327957,#327958),(#327959,#327960,#327961),(#327962,#327963,#327964),(#327965,
#327966,#327967),(#327968,#327969,#327970),(#327971,#327972,#327973),(#327974,
#327975,#327976),(#327977,#327978,#327979),(#327980,#327981,#327982),(#327983,
#327984,#327985),(#327986,#327987,#327988),(#327989,#327990,#327991),(#327992,
#327993,#327994),(#327995,#327996,#327997),(#327998,#327999,#328000),(#328001,
#328002,#328003),(#328004,#328005,#328006),(#328007,#328008,#328009),(#328010,
#328011,#328012),(#328013,#328014,#328015),(#328016,#328017,#328018),(#328019,
#328020,#328021),(#328022,#328023,#328024),(#328025,#328026,#328027),(#328028,
#328029,#328030)),.UNSPECIFIED.,.F.,.F.,.F.,(6,1,1,1,1,1,1,1,1,1,1,1,1,
1,1,1,1,1,1,1,1,1,1,1,1,1,1,1,1,1,1,1,1,1,1,1,1,1,1,1,1,1,1,1,1,1,1,1,1,
1,1,1,1,1,1,1,1,1,1,1,1,1,1,1,1,1,1,1,1,1,1,1,1,1,1,1,1,1,1,1,1,1,1,1,1,
1,1,1,1,1,1,1,1,1,1,1,1,1,1,1,1,1,1,1,1,1,1,1,1,1,1,1,1,1,1,1,1,1,1,1,1,
1,1,1,1,1,1,1,1,1,1,1,1,1,1,1,1,1,1,1,1,1,1,1,1,1,1,1,1,1,1,1,1,1,1,1,1,
1,1,1,1,1,1,1,1,1,1,1,1,1,1,1,1,1,1,1,1,1,1,1,1,1,1,1,1,1,1,1,1,1,1,1,1,
1,1,1,1,1,1,1,1,1,1,1,1,1,1,1,1,1,1,1,1,1,1,1,1,1,1,1,1,1,1,1,1,1,1,1,1,
1,1,1,1,1,1,1,1,1,1,1,1,1,1,1,1,1,1,1,1,1,1,1,1,1,1,1,1,1,1,1,1,1,1,1,1,
1,1,1,1,1,1,1,1,1,1,1,1,1,1,1,1,1,1,1,1,1,1,1,1,1,1,1,1,1,1,1,1,1,1,1,1,
1,1,1,1,1,1,1,1,1,1,1,1,1,1,1,1,1,1,1,1,1,1,1,1,1,1,1,1,1,1,1,1,1,1,1,1,
1,1,1,1,1,1,1,1,1,1,1,1,1,1,1,1,1,1,1,1,1,1,1,1,1,1,1,1,1,1,1,1,1,1,1,1,
1,1,1,1,1,1,1,1,1,1,1,1,1,1,1,1,1,1,1,1,1,1,1,1,1,1,1,1,1,1,1,1,1,1,1,1,
1,1,1,1,1,1,1,1,1,1,1,1,1,1,1,1,1,1,1,1,1,1,1,1,1,1,1,1,1,1,1,1,1,1,1,1,
1,1,1,1,1,1,1,1,1,1,1,1,1,1,1,1,1,1,1,1,1,1,1,1,1,1,1,1,1,1,1,1,1,1,1,1,
1,1,1,1,1,1,1,1,1,1,1,1,1,1,1,1,1,1,1,1,1,1,1,1,1,1,1,1,1,1,1,1,1,1,1,1,
1,1,1,1,1,1,1,1,1,1,1,1,1,1,1,1,1,1,1,1,1,1,1,1,1,1,1,1,1,6),(2,1,2),(-0.001964192,
0.,0.001834862,0.003669725,0.005504587,0.00733945,0.009174312,0.011009174,
0.012844037,0.014678899,0.016513761,0.018348624,0.020183486,0.022018349,
0.023853211,0.025688073,0.027522936,0.029357798,0.031192661,0.033027523,
0.034862385,0.036697248,0.03853211,0.040366972,0.042201835,0.044036697,
0.04587156,0.047706422,0.049541284,0.051376147,0.053211009,0.055045872,
0.056880734,0.058715596,0.060550459,0.062385321,0.064220183,0.066055046,
0.067889908,0.069724771,0.071559633,0.073394495,0.075229358,0.07706422,
0.078899083,0.080733945,0.082568807,0.08440367,0.086238532,0.088073394,
0.089908257,0.091743119,0.093577982,0.095412844,0.097247706,0.099082569,
0.100917431,0.102752294,0.104587156,0.106422018,0.108256881,0.110091743,
0.111926606,0.113761468,0.11559633,0.117431193,0.119266055,0.121100917,
0.12293578,0.124770642,0.126605505,0.128440367,0.130275229,0.132110092,
0.133944954,0.135779817,0.137614679,0.139449541,0.141284404,0.143119266,
0.144954128,0.146788991,0.148623853,0.150458716,0.152293578,0.15412844,
0.155963303,0.157798165,0.159633028,0.16146789,0.163302752,0.165137615,
0.166972477,0.168807339,0.170642202,0.172477064,0.174311927,0.176146789,
0.177981651,0.179816514,0.181651376,0.183486239,0.185321101,0.187155963,
0.188990826,0.190825688,0.19266055,0.194495413,0.196330275,0.198165138,
0.2,0.201834862,0.203669725,0.205504587,0.20733945,0.209174312,0.211009174,
0.212844037,0.214678899,0.216513761,0.218348624,0.220183486,0.222018349,
0.223853211,0.225688073,0.227522936,0.229357798,0.231192661,0.233027523,
0.234862385,0.236697248,0.23853211,0.240366972,0.242201835,0.244036697,
0.24587156,0.247706422,0.249541284,0.251376147,0.253211009,0.255045872,
0.256880734,0.258715596,0.260550459,0.262385321,0.264220183,0.266055046,
0.267889908,0.269724771,0.271559633,0.273394495,0.275229358,0.27706422,
0.278899083,0.280733945,0.282568807,0.28440367,0.286238532,0.288073394,
0.289908257,0.291743119,0.293577982,0.295412844,0.297247706,0.299082569,
0.300917431,0.302752294,0.304587156,0.306422018,0.308256881,0.310091743,
0.311926606,0.313761468,0.31559633,0.317431193,0.319266055,0.321100917,
0.32293578,0.324770642,0.326605505,0.328440367,0.330275229,0.332110092,
0.333944954,0.335779817,0.337614679,0.339449541,0.341284404,0.343119266,
0.344954128,0.346788991,0.348623853,0.350458716,0.352293578,0.35412844,
0.355963303,0.357798165,0.359633028,0.36146789,0.363302752,0.365137615,
0.366972477,0.368807339,0.370642202,0.372477064,0.374311927,0.376146789,
0.377981651,0.379816514,0.381651376,0.383486239,0.385321101,0.387155963,
0.388990826,0.390825688,0.39266055,0.394495413,0.396330275,0.398165138,
0.4,0.401834862,0.403669725,0.405504587,0.40733945,0.409174312,0.411009174,
0.412844037,0.414678899,0.416513761,0.418348624,0.420183486,0.422018349,
0.423853211,0.425688073,0.427522936,0.429357798,0.431192661,0.433027523,
0.434862385,0.436697248,0.43853211,0.440366972,0.442201835,0.444036697,
0.44587156,0.447706422,0.449541284,0.451376147,0.453211009,0.455045872,
0.456880734,0.458715596,0.460550459,0.462385321,0.464220183,0.466055046,
0.467889908,0.469724771,0.471559633,0.473394495,0.475229358,0.47706422,
0.478899083,0.480733945,0.482568807,0.48440367,0.486238532,0.488073394,
0.489908257,0.491743119,0.493577982,0.495412844,0.497247706,0.499082569,
0.500917431,0.502752294,0.504587156,0.506422018,0.508256881,0.510091743,
0.511926606,0.513761468,0.51559633,0.517431193,0.519266055,0.521100917,
0.52293578,0.524770642,0.526605505,0.528440367,0.530275229,0.532110092,
0.533944954,0.535779817,0.537614679,0.539449541,0.541284404,0.543119266,
0.544954128,0.546788991,0.548623853,0.550458716,0.552293578,0.55412844,
0.555963303,0.557798165,0.559633028,0.56146789,0.563302752,0.565137615,
0.566972477,0.568807339,0.570642202,0.572477064,0.574311927,0.576146789,
0.577981651,0.579816514,0.581651376,0.583486239,0.585321101,0.587155963,
0.588990826,0.590825688,0.59266055,0.594495413,0.596330275,0.598165138,
0.6,0.601834862,0.603669725,0.605504587,0.60733945,0.609174312,0.611009174,
0.612844037,0.614678899,0.616513761,0.618348624,0.620183486,0.622018349,
0.623853211,0.625688073,0.627522936,0.629357798,0.631192661,0.633027523,
0.634862385,0.636697248,0.63853211,0.640366972,0.642201835,0.644036697,
0.64587156,0.647706422,0.649541284,0.651376147,0.653211009,0.655045872,
0.656880734,0.658715596,0.660550459,0.662385321,0.664220183,0.666055046,
0.667889908,0.669724771,0.671559633,0.673394495,0.675229358,0.67706422,
0.678899083,0.680733945,0.682568807,0.68440367,0.686238532,0.688073394,
0.689908257,0.691743119,0.693577982,0.695412844,0.697247706,0.699082569,
0.700917431,0.702752294,0.704587156,0.706422018,0.708256881,0.710091743,
0.711926606,0.713761468,0.71559633,0.717431193,0.719266055,0.721100917,
0.72293578,0.724770642,0.726605505,0.728440367,0.730275229,0.732110092,
0.733944954,0.735779817,0.737614679,0.739449541,0.741284404,0.743119266,
0.744954128,0.746788991,0.748623853,0.750458716,0.752293578,0.75412844,
0.755963303,0.757798165,0.759633028,0.76146789,0.763302752,0.765137615,
0.766972477,0.768807339,0.770642202,0.772477064,0.774311927,0.776146789,
0.777981651,0.779816514,0.781651376,0.783486239,0.785321101,0.787155963,
0.788990826,0.790825688,0.79266055,0.794495413,0.796330275,0.798165138,
0.8,0.801834862,0.803669725,0.805504587,0.80733945,0.809174312,0.811009174,
0.812844037,0.814678899,0.816513761,0.818348624,0.820183486,0.822018349,
0.823853211,0.825688073,0.827522936,0.829357798,0.831192661,0.833027523,
0.834862385,0.836697248,0.83853211,0.840366972,0.842201835,0.844036697,
0.84587156,0.847706422,0.849541284,0.851376147,0.853211009,0.855045872,
0.856880734,0.858715596,0.860550459,0.862385321,0.864220183,0.866055046,
0.867889908,0.869724771,0.871559633,0.873394495,0.875229358,0.87706422,
0.878899083,0.880733945,0.882568807,0.88440367,0.886238532,0.888073394,
0.889908257,0.891743119,0.893577982,0.895412844,0.897247706,0.899082569,
0.900917431,0.902752294,0.904587156,0.906422018,0.908256881,0.910091743,
0.911926606,0.913761468,0.91559633,0.917431193,0.919266055,0.921100917,
0.92293578,0.924770642,0.926605505,0.928440367,0.930275229,0.932110092,
0.933944954,0.935779817,0.937614679,0.939449541,0.941284404,0.943119266,
0.944954128,0.946788991,0.948623853,0.950458716,0.952293578,0.95412844,
0.955963303,0.957798165,0.959633028,0.96146789,0.963302752,0.965137615,
0.966972477,0.968807339,0.970642202,0.972477064,0.974311927,0.976146789,
0.977981651,0.979816514,0.981651376,0.983486239,0.985321101,0.987155963,
0.988990826,0.990825688,0.99266055,0.994495413,0.996330275,0.998165138,
1.),(0.3,1.,1.3),.UNSPECIFIED.);
#6319=B_SPLINE_SURFACE_WITH_KNOTS('',5,1,((#328049,#328050,#328051),(#328052,
#328053,#328054),(#328055,#328056,#328057),(#328058,#328059,#328060),(#328061,
#328062,#328063),(#328064,#328065,#328066),(#328067,#328068,#328069),(#328070,
#328071,#328072),(#328073,#328074,#328075),(#328076,#328077,#328078),(#328079,
#328080,#328081),(#328082,#328083,#328084),(#328085,#328086,#328087),(#328088,
#328089,#328090),(#328091,#328092,#328093),(#328094,#328095,#328096),(#328097,
#328098,#328099),(#328100,#328101,#328102),(#328103,#328104,#328105),(#328106,
#328107,#328108),(#328109,#328110,#328111),(#328112,#328113,#328114),(#328115,
#328116,#328117),(#328118,#328119,#328120),(#328121,#328122,#328123),(#328124,
#328125,#328126),(#328127,#328128,#328129),(#328130,#328131,#328132),(#328133,
#328134,#328135),(#328136,#328137,#328138),(#328139,#328140,#328141),(#328142,
#328143,#328144),(#328145,#328146,#328147),(#328148,#328149,#328150),(#328151,
#328152,#328153),(#328154,#328155,#328156),(#328157,#328158,#328159),(#328160,
#328161,#328162),(#328163,#328164,#328165),(#328166,#328167,#328168),(#328169,
#328170,#328171),(#328172,#328173,#328174),(#328175,#328176,#328177),(#328178,
#328179,#328180),(#328181,#328182,#328183),(#328184,#328185,#328186),(#328187,
#328188,#328189),(#328190,#328191,#328192),(#328193,#328194,#328195),(#328196,
#328197,#328198),(#328199,#328200,#328201),(#328202,#328203,#328204),(#328205,
#328206,#328207),(#328208,#328209,#328210),(#328211,#328212,#328213),(#328214,
#328215,#328216),(#328217,#328218,#328219),(#328220,#328221,#328222),(#328223,
#328224,#328225),(#328226,#328227,#328228),(#328229,#328230,#328231),(#328232,
#328233,#328234),(#328235,#328236,#328237),(#328238,#328239,#328240),(#328241,
#328242,#328243),(#328244,#328245,#328246),(#328247,#328248,#328249),(#328250,
#328251,#328252),(#328253,#328254,#328255),(#328256,#328257,#328258),(#328259,
#328260,#328261),(#328262,#328263,#328264),(#328265,#328266,#328267),(#328268,
#328269,#328270),(#328271,#328272,#328273),(#328274,#328275,#328276),(#328277,
#328278,#328279),(#328280,#328281,#328282),(#328283,#328284,#328285),(#328286,
#328287,#328288),(#328289,#328290,#328291),(#328292,#328293,#328294),(#328295,
#328296,#328297),(#328298,#328299,#328300),(#328301,#328302,#328303),(#328304,
#328305,#328306),(#328307,#328308,#328309),(#328310,#328311,#328312),(#328313,
#328314,#328315),(#328316,#328317,#328318),(#328319,#328320,#328321),(#328322,
#328323,#328324),(#328325,#328326,#328327),(#328328,#328329,#328330),(#328331,
#328332,#328333),(#328334,#328335,#328336),(#328337,#328338,#328339),(#328340,
#328341,#328342),(#328343,#328344,#328345),(#328346,#328347,#328348),(#328349,
#328350,#328351),(#328352,#328353,#328354),(#328355,#328356,#328357),(#328358,
#328359,#328360),(#328361,#328362,#328363),(#328364,#328365,#328366),(#328367,
#328368,#328369),(#328370,#328371,#328372),(#328373,#328374,#328375),(#328376,
#328377,#328378),(#328379,#328380,#328381),(#328382,#328383,#328384),(#328385,
#328386,#328387),(#328388,#328389,#328390),(#328391,#328392,#328393),(#328394,
#328395,#328396),(#328397,#328398,#328399),(#328400,#328401,#328402),(#328403,
#328404,#328405),(#328406,#328407,#328408),(#328409,#328410,#328411),(#328412,
#328413,#328414),(#328415,#328416,#328417),(#328418,#328419,#328420),(#328421,
#328422,#328423),(#328424,#328425,#328426),(#328427,#328428,#328429),(#328430,
#328431,#328432),(#328433,#328434,#328435),(#328436,#328437,#328438),(#328439,
#328440,#328441),(#328442,#328443,#328444),(#328445,#328446,#328447),(#328448,
#328449,#328450),(#328451,#328452,#328453),(#328454,#328455,#328456),(#328457,
#328458,#328459),(#328460,#328461,#328462),(#328463,#328464,#328465),(#328466,
#328467,#328468),(#328469,#328470,#328471),(#328472,#328473,#328474),(#328475,
#328476,#328477),(#328478,#328479,#328480),(#328481,#328482,#328483),(#328484,
#328485,#328486),(#328487,#328488,#328489),(#328490,#328491,#328492),(#328493,
#328494,#328495),(#328496,#328497,#328498),(#328499,#328500,#328501),(#328502,
#328503,#328504),(#328505,#328506,#328507),(#328508,#328509,#328510),(#328511,
#328512,#328513),(#328514,#328515,#328516),(#328517,#328518,#328519),(#328520,
#328521,#328522),(#328523,#328524,#328525),(#328526,#328527,#328528),(#328529,
#328530,#328531),(#328532,#328533,#328534),(#328535,#328536,#328537),(#328538,
#328539,#328540),(#328541,#328542,#328543),(#328544,#328545,#328546),(#328547,
#328548,#328549),(#328550,#328551,#328552),(#328553,#328554,#328555),(#328556,
#328557,#328558),(#328559,#328560,#328561),(#328562,#328563,#328564),(#328565,
#328566,#328567),(#328568,#328569,#328570),(#328571,#328572,#328573),(#328574,
#328575,#328576),(#328577,#328578,#328579),(#328580,#328581,#328582),(#328583,
#328584,#328585),(#328586,#328587,#328588),(#328589,#328590,#328591),(#328592,
#328593,#328594),(#328595,#328596,#328597),(#328598,#328599,#328600),(#328601,
#328602,#328603),(#328604,#328605,#328606),(#328607,#328608,#328609),(#328610,
#328611,#328612),(#328613,#328614,#328615),(#328616,#328617,#328618),(#328619,
#328620,#328621),(#328622,#328623,#328624),(#328625,#328626,#328627),(#328628,
#328629,#328630),(#328631,#328632,#328633),(#328634,#328635,#328636),(#328637,
#328638,#328639),(#328640,#328641,#328642),(#328643,#328644,#328645),(#328646,
#328647,#328648),(#328649,#328650,#328651),(#328652,#328653,#328654),(#328655,
#328656,#328657),(#328658,#328659,#328660),(#328661,#328662,#328663),(#328664,
#328665,#328666),(#328667,#328668,#328669),(#328670,#328671,#328672),(#328673,
#328674,#328675),(#328676,#328677,#328678),(#328679,#328680,#328681),(#328682,
#328683,#328684),(#328685,#328686,#328687),(#328688,#328689,#328690),(#328691,
#328692,#328693),(#328694,#328695,#328696),(#328697,#328698,#328699),(#328700,
#328701,#328702),(#328703,#328704,#328705),(#328706,#328707,#328708),(#328709,
#328710,#328711),(#328712,#328713,#328714),(#328715,#328716,#328717),(#328718,
#328719,#328720),(#328721,#328722,#328723),(#328724,#328725,#328726),(#328727,
#328728,#328729),(#328730,#328731,#328732),(#328733,#328734,#328735),(#328736,
#328737,#328738),(#328739,#328740,#328741),(#328742,#328743,#328744),(#328745,
#328746,#328747),(#328748,#328749,#328750),(#328751,#328752,#328753),(#328754,
#328755,#328756),(#328757,#328758,#328759),(#328760,#328761,#328762),(#328763,
#328764,#328765),(#328766,#328767,#328768),(#328769,#328770,#328771),(#328772,
#328773,#328774),(#328775,#328776,#328777),(#328778,#328779,#328780),(#328781,
#328782,#328783),(#328784,#328785,#328786),(#328787,#328788,#328789),(#328790,
#328791,#328792),(#328793,#328794,#328795),(#328796,#328797,#328798),(#328799,
#328800,#328801),(#328802,#328803,#328804),(#328805,#328806,#328807),(#328808,
#328809,#328810),(#328811,#328812,#328813),(#328814,#328815,#328816),(#328817,
#328818,#328819),(#328820,#328821,#328822),(#328823,#328824,#328825),(#328826,
#328827,#328828),(#328829,#328830,#328831),(#328832,#328833,#328834),(#328835,
#328836,#328837),(#328838,#328839,#328840),(#328841,#328842,#328843),(#328844,
#328845,#328846),(#328847,#328848,#328849),(#328850,#328851,#328852),(#328853,
#328854,#328855),(#328856,#328857,#328858),(#328859,#328860,#328861),(#328862,
#328863,#328864),(#328865,#328866,#328867),(#328868,#328869,#328870),(#328871,
#328872,#328873),(#328874,#328875,#328876),(#328877,#328878,#328879),(#328880,
#328881,#328882),(#328883,#328884,#328885),(#328886,#328887,#328888),(#328889,
#328890,#328891),(#328892,#328893,#328894),(#328895,#328896,#328897),(#328898,
#328899,#328900),(#328901,#328902,#328903),(#328904,#328905,#328906),(#328907,
#328908,#328909),(#328910,#328911,#328912),(#328913,#328914,#328915),(#328916,
#328917,#328918),(#328919,#328920,#328921),(#328922,#328923,#328924),(#328925,
#328926,#328927),(#328928,#328929,#328930),(#328931,#328932,#328933),(#328934,
#328935,#328936),(#328937,#328938,#328939),(#328940,#328941,#328942),(#328943,
#328944,#328945),(#328946,#328947,#328948),(#328949,#328950,#328951),(#328952,
#328953,#328954),(#328955,#328956,#328957),(#328958,#328959,#328960),(#328961,
#328962,#328963),(#328964,#328965,#328966),(#328967,#328968,#328969),(#328970,
#328971,#328972),(#328973,#328974,#328975),(#328976,#328977,#328978),(#328979,
#328980,#328981),(#328982,#328983,#328984),(#328985,#328986,#328987),(#328988,
#328989,#328990),(#328991,#328992,#328993),(#328994,#328995,#328996),(#328997,
#328998,#328999),(#329000,#329001,#329002),(#329003,#329004,#329005),(#329006,
#329007,#329008),(#329009,#329010,#329011),(#329012,#329013,#329014),(#329015,
#329016,#329017),(#329018,#329019,#329020),(#329021,#329022,#329023),(#329024,
#329025,#329026),(#329027,#329028,#329029),(#329030,#329031,#329032),(#329033,
#329034,#329035),(#329036,#329037,#329038),(#329039,#329040,#329041),(#329042,
#329043,#329044),(#329045,#329046,#329047),(#329048,#329049,#329050),(#329051,
#329052,#329053),(#329054,#329055,#329056),(#329057,#329058,#329059),(#329060,
#329061,#329062),(#329063,#329064,#329065),(#329066,#329067,#329068),(#329069,
#329070,#329071),(#329072,#329073,#329074),(#329075,#329076,#329077),(#329078,
#329079,#329080),(#329081,#329082,#329083),(#329084,#329085,#329086),(#329087,
#329088,#329089),(#329090,#329091,#329092),(#329093,#329094,#329095),(#329096,
#329097,#329098),(#329099,#329100,#329101),(#329102,#329103,#329104),(#329105,
#329106,#329107),(#329108,#329109,#329110),(#329111,#329112,#329113),(#329114,
#329115,#329116),(#329117,#329118,#329119),(#329120,#329121,#329122),(#329123,
#329124,#329125),(#329126,#329127,#329128),(#329129,#329130,#329131),(#329132,
#329133,#329134),(#329135,#329136,#329137),(#329138,#329139,#329140),(#329141,
#329142,#329143),(#329144,#329145,#329146),(#329147,#329148,#329149),(#329150,
#329151,#329152),(#329153,#329154,#329155),(#329156,#329157,#329158),(#329159,
#329160,#329161),(#329162,#329163,#329164),(#329165,#329166,#329167),(#329168,
#329169,#329170),(#329171,#329172,#329173),(#329174,#329175,#329176),(#329177,
#329178,#329179),(#329180,#329181,#329182),(#329183,#329184,#329185),(#329186,
#329187,#329188),(#329189,#329190,#329191),(#329192,#329193,#329194),(#329195,
#329196,#329197),(#329198,#329199,#329200),(#329201,#329202,#329203),(#329204,
#329205,#329206),(#329207,#329208,#329209),(#329210,#329211,#329212),(#329213,
#329214,#329215),(#329216,#329217,#329218),(#329219,#329220,#329221),(#329222,
#329223,#329224),(#329225,#329226,#329227),(#329228,#329229,#329230),(#329231,
#329232,#329233),(#329234,#329235,#329236),(#329237,#329238,#329239),(#329240,
#329241,#329242),(#329243,#329244,#329245),(#329246,#329247,#329248),(#329249,
#329250,#329251),(#329252,#329253,#329254),(#329255,#329256,#329257),(#329258,
#329259,#329260),(#329261,#329262,#329263),(#329264,#329265,#329266),(#329267,
#329268,#329269),(#329270,#329271,#329272),(#329273,#329274,#329275),(#329276,
#329277,#329278),(#329279,#329280,#329281),(#329282,#329283,#329284),(#329285,
#329286,#329287),(#329288,#329289,#329290),(#329291,#329292,#329293),(#329294,
#329295,#329296),(#329297,#329298,#329299),(#329300,#329301,#329302),(#329303,
#329304,#329305),(#329306,#329307,#329308),(#329309,#329310,#329311),(#329312,
#329313,#329314),(#329315,#329316,#329317),(#329318,#329319,#329320),(#329321,
#329322,#329323),(#329324,#329325,#329326),(#329327,#329328,#329329),(#329330,
#329331,#329332),(#329333,#329334,#329335),(#329336,#329337,#329338),(#329339,
#329340,#329341),(#329342,#329343,#329344),(#329345,#329346,#329347),(#329348,
#329349,#329350),(#329351,#329352,#329353),(#329354,#329355,#329356),(#329357,
#329358,#329359),(#329360,#329361,#329362),(#329363,#329364,#329365),(#329366,
#329367,#329368),(#329369,#329370,#329371),(#329372,#329373,#329374),(#329375,
#329376,#329377),(#329378,#329379,#329380),(#329381,#329382,#329383),(#329384,
#329385,#329386),(#329387,#329388,#329389),(#329390,#329391,#329392),(#329393,
#329394,#329395),(#329396,#329397,#329398),(#329399,#329400,#329401),(#329402,
#329403,#329404),(#329405,#329406,#329407),(#329408,#329409,#329410),(#329411,
#329412,#329413),(#329414,#329415,#329416),(#329417,#329418,#329419),(#329420,
#329421,#329422),(#329423,#329424,#329425),(#329426,#329427,#329428),(#329429,
#329430,#329431),(#329432,#329433,#329434),(#329435,#329436,#329437),(#329438,
#329439,#329440),(#329441,#329442,#329443),(#329444,#329445,#329446),(#329447,
#329448,#329449),(#329450,#329451,#329452),(#329453,#329454,#329455),(#329456,
#329457,#329458),(#329459,#329460,#329461),(#329462,#329463,#329464),(#329465,
#329466,#329467),(#329468,#329469,#329470),(#329471,#329472,#329473),(#329474,
#329475,#329476),(#329477,#329478,#329479),(#329480,#329481,#329482),(#329483,
#329484,#329485),(#329486,#329487,#329488),(#329489,#329490,#329491),(#329492,
#329493,#329494),(#329495,#329496,#329497),(#329498,#329499,#329500),(#329501,
#329502,#329503),(#329504,#329505,#329506),(#329507,#329508,#329509),(#329510,
#329511,#329512),(#329513,#329514,#329515),(#329516,#329517,#329518),(#329519,
#329520,#329521),(#329522,#329523,#329524),(#329525,#329526,#329527),(#329528,
#329529,#329530),(#329531,#329532,#329533),(#329534,#329535,#329536),(#329537,
#329538,#329539),(#329540,#329541,#329542),(#329543,#329544,#329545),(#329546,
#329547,#329548),(#329549,#329550,#329551),(#329552,#329553,#329554),(#329555,
#329556,#329557),(#329558,#329559,#329560),(#329561,#329562,#329563),(#329564,
#329565,#329566),(#329567,#329568,#329569),(#329570,#329571,#329572),(#329573,
#329574,#329575),(#329576,#329577,#329578),(#329579,#329580,#329581),(#329582,
#329583,#329584),(#329585,#329586,#329587),(#329588,#329589,#329590),(#329591,
#329592,#329593),(#329594,#329595,#329596),(#329597,#329598,#329599),(#329600,
#329601,#329602),(#329603,#329604,#329605),(#329606,#329607,#329608),(#329609,
#329610,#329611),(#329612,#329613,#329614),(#329615,#329616,#329617),(#329618,
#329619,#329620),(#329621,#329622,#329623),(#329624,#329625,#329626),(#329627,
#329628,#329629),(#329630,#329631,#329632),(#329633,#329634,#329635),(#329636,
#329637,#329638),(#329639,#329640,#329641),(#329642,#329643,#329644),(#329645,
#329646,#329647),(#329648,#329649,#329650),(#329651,#329652,#329653),(#329654,
#329655,#329656),(#329657,#329658,#329659),(#329660,#329661,#329662),(#329663,
#329664,#329665),(#329666,#329667,#329668),(#329669,#329670,#329671),(#329672,
#329673,#329674),(#329675,#329676,#329677),(#329678,#329679,#329680),(#329681,
#329682,#329683),(#329684,#329685,#329686),(#329687,#329688,#329689),(#329690,
#329691,#329692),(#329693,#329694,#329695),(#329696,#329697,#329698)),
 .UNSPECIFIED.,.F.,.F.,.F.,(6,1,1,1,1,1,1,1,1,1,1,1,1,1,1,1,1,1,1,1,1,1,
1,1,1,1,1,1,1,1,1,1,1,1,1,1,1,1,1,1,1,1,1,1,1,1,1,1,1,1,1,1,1,1,1,1,1,1,
1,1,1,1,1,1,1,1,1,1,1,1,1,1,1,1,1,1,1,1,1,1,1,1,1,1,1,1,1,1,1,1,1,1,1,1,
1,1,1,1,1,1,1,1,1,1,1,1,1,1,1,1,1,1,1,1,1,1,1,1,1,1,1,1,1,1,1,1,1,1,1,1,
1,1,1,1,1,1,1,1,1,1,1,1,1,1,1,1,1,1,1,1,1,1,1,1,1,1,1,1,1,1,1,1,1,1,1,1,
1,1,1,1,1,1,1,1,1,1,1,1,1,1,1,1,1,1,1,1,1,1,1,1,1,1,1,1,1,1,1,1,1,1,1,1,
1,1,1,1,1,1,1,1,1,1,1,1,1,1,1,1,1,1,1,1,1,1,1,1,1,1,1,1,1,1,1,1,1,1,1,1,
1,1,1,1,1,1,1,1,1,1,1,1,1,1,1,1,1,1,1,1,1,1,1,1,1,1,1,1,1,1,1,1,1,1,1,1,
1,1,1,1,1,1,1,1,1,1,1,1,1,1,1,1,1,1,1,1,1,1,1,1,1,1,1,1,1,1,1,1,1,1,1,1,
1,1,1,1,1,1,1,1,1,1,1,1,1,1,1,1,1,1,1,1,1,1,1,1,1,1,1,1,1,1,1,1,1,1,1,1,
1,1,1,1,1,1,1,1,1,1,1,1,1,1,1,1,1,1,1,1,1,1,1,1,1,1,1,1,1,1,1,1,1,1,1,1,
1,1,1,1,1,1,1,1,1,1,1,1,1,1,1,1,1,1,1,1,1,1,1,1,1,1,1,1,1,1,1,1,1,1,1,1,
1,1,1,1,1,1,1,1,1,1,1,1,1,1,1,1,1,1,1,1,1,1,1,1,1,1,1,1,1,1,1,1,1,1,1,1,
1,1,1,1,1,1,1,1,1,1,1,1,1,1,1,1,1,1,1,1,1,1,1,1,1,1,1,1,1,1,1,1,1,1,1,1,
1,1,1,1,1,1,1,1,1,1,1,1,1,1,1,1,1,1,1,1,1,1,1,1,1,1,1,1,1,1,1,1,1,1,1,1,
1,1,1,1,1,1,1,1,1,1,1,1,1,1,1,1,1,1,1,6),(2,1,2),(-1.,-0.998165138,-0.996330275,
-0.994495413,-0.99266055,-0.990825688,-0.988990826,-0.987155963,-0.985321101,
-0.983486239,-0.981651376,-0.979816514,-0.977981651,-0.976146789,-0.974311927,
-0.972477064,-0.970642202,-0.968807339,-0.966972477,-0.965137615,-0.963302752,
-0.96146789,-0.959633028,-0.957798165,-0.955963303,-0.95412844,-0.952293578,
-0.950458716,-0.948623853,-0.946788991,-0.944954128,-0.943119266,-0.941284404,
-0.939449541,-0.937614679,-0.935779817,-0.933944954,-0.932110092,-0.930275229,
-0.928440367,-0.926605505,-0.924770642,-0.92293578,-0.921100917,-0.919266055,
-0.917431193,-0.91559633,-0.913761468,-0.911926606,-0.910091743,-0.908256881,
-0.906422018,-0.904587156,-0.902752294,-0.900917431,-0.899082569,-0.897247706,
-0.895412844,-0.893577982,-0.891743119,-0.889908257,-0.888073394,-0.886238532,
-0.88440367,-0.882568807,-0.880733945,-0.878899083,-0.87706422,-0.875229358,
-0.873394495,-0.871559633,-0.869724771,-0.867889908,-0.866055046,-0.864220183,
-0.862385321,-0.860550459,-0.858715596,-0.856880734,-0.855045872,-0.853211009,
-0.851376147,-0.849541284,-0.847706422,-0.84587156,-0.844036697,-0.842201835,
-0.840366972,-0.83853211,-0.836697248,-0.834862385,-0.833027523,-0.831192661,
-0.829357798,-0.827522936,-0.825688073,-0.823853211,-0.822018349,-0.820183486,
-0.818348624,-0.816513761,-0.814678899,-0.812844037,-0.811009174,-0.809174312,
-0.80733945,-0.805504587,-0.803669725,-0.801834862,-0.8,-0.798165138,-0.796330275,
-0.794495413,-0.79266055,-0.790825688,-0.788990826,-0.787155963,-0.785321101,
-0.783486239,-0.781651376,-0.779816514,-0.777981651,-0.776146789,-0.774311927,
-0.772477064,-0.770642202,-0.768807339,-0.766972477,-0.765137615,-0.763302752,
-0.76146789,-0.759633028,-0.757798165,-0.755963303,-0.75412844,-0.752293578,
-0.750458716,-0.748623853,-0.746788991,-0.744954128,-0.743119266,-0.741284404,
-0.739449541,-0.737614679,-0.735779817,-0.733944954,-0.732110092,-0.730275229,
-0.728440367,-0.726605505,-0.724770642,-0.72293578,-0.721100917,-0.719266055,
-0.717431193,-0.71559633,-0.713761468,-0.711926606,-0.710091743,-0.708256881,
-0.706422018,-0.704587156,-0.702752294,-0.700917431,-0.699082569,-0.697247706,
-0.695412844,-0.693577982,-0.691743119,-0.689908257,-0.688073394,-0.686238532,
-0.68440367,-0.682568807,-0.680733945,-0.678899083,-0.67706422,-0.675229358,
-0.673394495,-0.671559633,-0.669724771,-0.667889908,-0.666055046,-0.664220183,
-0.662385321,-0.660550459,-0.658715596,-0.656880734,-0.655045872,-0.653211009,
-0.651376147,-0.649541284,-0.647706422,-0.64587156,-0.644036697,-0.642201835,
-0.640366972,-0.63853211,-0.636697248,-0.634862385,-0.633027523,-0.631192661,
-0.629357798,-0.627522936,-0.625688073,-0.623853211,-0.622018349,-0.620183486,
-0.618348624,-0.616513761,-0.614678899,-0.612844037,-0.611009174,-0.609174312,
-0.60733945,-0.605504587,-0.603669725,-0.601834862,-0.6,-0.598165138,-0.596330275,
-0.594495413,-0.59266055,-0.590825688,-0.588990826,-0.587155963,-0.585321101,
-0.583486239,-0.581651376,-0.579816514,-0.577981651,-0.576146789,-0.574311927,
-0.572477064,-0.570642202,-0.568807339,-0.566972477,-0.565137615,-0.563302752,
-0.56146789,-0.559633028,-0.557798165,-0.555963303,-0.55412844,-0.552293578,
-0.550458716,-0.548623853,-0.546788991,-0.544954128,-0.543119266,-0.541284404,
-0.539449541,-0.537614679,-0.535779817,-0.533944954,-0.532110092,-0.530275229,
-0.528440367,-0.526605505,-0.524770642,-0.52293578,-0.521100917,-0.519266055,
-0.517431193,-0.51559633,-0.513761468,-0.511926606,-0.510091743,-0.508256881,
-0.506422018,-0.504587156,-0.502752294,-0.500917431,-0.499082569,-0.497247706,
-0.495412844,-0.493577982,-0.491743119,-0.489908257,-0.488073394,-0.486238532,
-0.48440367,-0.482568807,-0.480733945,-0.478899083,-0.47706422,-0.475229358,
-0.473394495,-0.471559633,-0.469724771,-0.467889908,-0.466055046,-0.464220183,
-0.462385321,-0.460550459,-0.458715596,-0.456880734,-0.455045872,-0.453211009,
-0.451376147,-0.449541284,-0.447706422,-0.44587156,-0.444036697,-0.442201835,
-0.440366972,-0.43853211,-0.436697248,-0.434862385,-0.433027523,-0.431192661,
-0.429357798,-0.427522936,-0.425688073,-0.423853211,-0.422018349,-0.420183486,
-0.418348624,-0.416513761,-0.414678899,-0.412844037,-0.411009174,-0.409174312,
-0.40733945,-0.405504587,-0.403669725,-0.401834862,-0.4,-0.398165138,-0.396330275,
-0.394495413,-0.39266055,-0.390825688,-0.388990826,-0.387155963,-0.385321101,
-0.383486239,-0.381651376,-0.379816514,-0.377981651,-0.376146789,-0.374311927,
-0.372477064,-0.370642202,-0.368807339,-0.366972477,-0.365137615,-0.363302752,
-0.36146789,-0.359633028,-0.357798165,-0.355963303,-0.35412844,-0.352293578,
-0.350458716,-0.348623853,-0.346788991,-0.344954128,-0.343119266,-0.341284404,
-0.339449541,-0.337614679,-0.335779817,-0.333944954,-0.332110092,-0.330275229,
-0.328440367,-0.326605505,-0.324770642,-0.32293578,-0.321100917,-0.319266055,
-0.317431193,-0.31559633,-0.313761468,-0.311926606,-0.310091743,-0.308256881,
-0.306422018,-0.304587156,-0.302752294,-0.300917431,-0.299082569,-0.297247706,
-0.295412844,-0.293577982,-0.291743119,-0.289908257,-0.288073394,-0.286238532,
-0.28440367,-0.282568807,-0.280733945,-0.278899083,-0.27706422,-0.275229358,
-0.273394495,-0.271559633,-0.269724771,-0.267889908,-0.266055046,-0.264220183,
-0.262385321,-0.260550459,-0.258715596,-0.256880734,-0.255045872,-0.253211009,
-0.251376147,-0.249541284,-0.247706422,-0.24587156,-0.244036697,-0.242201835,
-0.240366972,-0.23853211,-0.236697248,-0.234862385,-0.233027523,-0.231192661,
-0.229357798,-0.227522936,-0.225688073,-0.223853211,-0.222018349,-0.220183486,
-0.218348624,-0.216513761,-0.214678899,-0.212844037,-0.211009174,-0.209174312,
-0.20733945,-0.205504587,-0.203669725,-0.201834862,-0.2,-0.198165138,-0.196330275,
-0.194495413,-0.19266055,-0.190825688,-0.188990826,-0.187155963,-0.185321101,
-0.183486239,-0.181651376,-0.179816514,-0.177981651,-0.176146789,-0.174311927,
-0.172477064,-0.170642202,-0.168807339,-0.166972477,-0.165137615,-0.163302752,
-0.16146789,-0.159633028,-0.157798165,-0.155963303,-0.15412844,-0.152293578,
-0.150458716,-0.148623853,-0.146788991,-0.144954128,-0.143119266,-0.141284404,
-0.139449541,-0.137614679,-0.135779817,-0.133944954,-0.132110092,-0.130275229,
-0.128440367,-0.126605505,-0.124770642,-0.12293578,-0.121100917,-0.119266055,
-0.117431193,-0.11559633,-0.113761468,-0.111926606,-0.110091743,-0.108256881,
-0.106422018,-0.104587156,-0.102752294,-0.100917431,-0.099082569,-0.097247706,
-0.095412844,-0.093577982,-0.091743119,-0.089908257,-0.088073394,-0.086238532,
-0.08440367,-0.082568807,-0.080733945,-0.078899083,-0.07706422,-0.075229358,
-0.073394495,-0.071559633,-0.069724771,-0.067889908,-0.066055046,-0.064220183,
-0.062385321,-0.060550459,-0.058715596,-0.056880734,-0.055045872,-0.053211009,
-0.051376147,-0.049541284,-0.047706422,-0.04587156,-0.044036697,-0.042201835,
-0.040366972,-0.03853211,-0.036697248,-0.034862385,-0.033027523,-0.031192661,
-0.029357798,-0.027522936,-0.025688073,-0.023853211,-0.022018349,-0.020183486,
-0.018348624,-0.016513761,-0.014678899,-0.012844037,-0.011009174,-0.009174312,
-0.00733945,-0.005504587,-0.003669725,-0.001834862,0.000982137),(0.3,1.,
1.3),.UNSPECIFIED.);
#6320=B_SPLINE_SURFACE_WITH_KNOTS('',5,1,((#329997,#329998,#329999),(#330000,
#330001,#330002),(#330003,#330004,#330005),(#330006,#330007,#330008),(#330009,
#330010,#330011),(#330012,#330013,#330014),(#330015,#330016,#330017),(#330018,
#330019,#330020),(#330021,#330022,#330023),(#330024,#330025,#330026),(#330027,
#330028,#330029),(#330030,#330031,#330032),(#330033,#330034,#330035),(#330036,
#330037,#330038),(#330039,#330040,#330041),(#330042,#330043,#330044),(#330045,
#330046,#330047),(#330048,#330049,#330050),(#330051,#330052,#330053),(#330054,
#330055,#330056),(#330057,#330058,#330059),(#330060,#330061,#330062),(#330063,
#330064,#330065),(#330066,#330067,#330068),(#330069,#330070,#330071),(#330072,
#330073,#330074),(#330075,#330076,#330077),(#330078,#330079,#330080),(#330081,
#330082,#330083),(#330084,#330085,#330086),(#330087,#330088,#330089),(#330090,
#330091,#330092),(#330093,#330094,#330095),(#330096,#330097,#330098),(#330099,
#330100,#330101),(#330102,#330103,#330104),(#330105,#330106,#330107),(#330108,
#330109,#330110),(#330111,#330112,#330113),(#330114,#330115,#330116),(#330117,
#330118,#330119),(#330120,#330121,#330122),(#330123,#330124,#330125),(#330126,
#330127,#330128),(#330129,#330130,#330131),(#330132,#330133,#330134),(#330135,
#330136,#330137),(#330138,#330139,#330140),(#330141,#330142,#330143),(#330144,
#330145,#330146),(#330147,#330148,#330149),(#330150,#330151,#330152),(#330153,
#330154,#330155),(#330156,#330157,#330158),(#330159,#330160,#330161),(#330162,
#330163,#330164),(#330165,#330166,#330167),(#330168,#330169,#330170),(#330171,
#330172,#330173),(#330174,#330175,#330176),(#330177,#330178,#330179),(#330180,
#330181,#330182),(#330183,#330184,#330185),(#330186,#330187,#330188),(#330189,
#330190,#330191),(#330192,#330193,#330194),(#330195,#330196,#330197),(#330198,
#330199,#330200),(#330201,#330202,#330203),(#330204,#330205,#330206),(#330207,
#330208,#330209),(#330210,#330211,#330212),(#330213,#330214,#330215),(#330216,
#330217,#330218),(#330219,#330220,#330221),(#330222,#330223,#330224),(#330225,
#330226,#330227),(#330228,#330229,#330230),(#330231,#330232,#330233),(#330234,
#330235,#330236),(#330237,#330238,#330239),(#330240,#330241,#330242),(#330243,
#330244,#330245),(#330246,#330247,#330248),(#330249,#330250,#330251),(#330252,
#330253,#330254),(#330255,#330256,#330257),(#330258,#330259,#330260),(#330261,
#330262,#330263),(#330264,#330265,#330266),(#330267,#330268,#330269),(#330270,
#330271,#330272),(#330273,#330274,#330275),(#330276,#330277,#330278),(#330279,
#330280,#330281),(#330282,#330283,#330284),(#330285,#330286,#330287),(#330288,
#330289,#330290),(#330291,#330292,#330293),(#330294,#330295,#330296),(#330297,
#330298,#330299),(#330300,#330301,#330302),(#330303,#330304,#330305),(#330306,
#330307,#330308),(#330309,#330310,#330311),(#330312,#330313,#330314),(#330315,
#330316,#330317),(#330318,#330319,#330320),(#330321,#330322,#330323),(#330324,
#330325,#330326),(#330327,#330328,#330329),(#330330,#330331,#330332),(#330333,
#330334,#330335),(#330336,#330337,#330338),(#330339,#330340,#330341),(#330342,
#330343,#330344),(#330345,#330346,#330347),(#330348,#330349,#330350),(#330351,
#330352,#330353),(#330354,#330355,#330356),(#330357,#330358,#330359),(#330360,
#330361,#330362),(#330363,#330364,#330365),(#330366,#330367,#330368),(#330369,
#330370,#330371),(#330372,#330373,#330374),(#330375,#330376,#330377),(#330378,
#330379,#330380),(#330381,#330382,#330383),(#330384,#330385,#330386),(#330387,
#330388,#330389),(#330390,#330391,#330392),(#330393,#330394,#330395),(#330396,
#330397,#330398),(#330399,#330400,#330401),(#330402,#330403,#330404),(#330405,
#330406,#330407),(#330408,#330409,#330410),(#330411,#330412,#330413),(#330414,
#330415,#330416),(#330417,#330418,#330419),(#330420,#330421,#330422),(#330423,
#330424,#330425),(#330426,#330427,#330428),(#330429,#330430,#330431),(#330432,
#330433,#330434),(#330435,#330436,#330437),(#330438,#330439,#330440),(#330441,
#330442,#330443),(#330444,#330445,#330446),(#330447,#330448,#330449),(#330450,
#330451,#330452),(#330453,#330454,#330455),(#330456,#330457,#330458),(#330459,
#330460,#330461),(#330462,#330463,#330464),(#330465,#330466,#330467),(#330468,
#330469,#330470),(#330471,#330472,#330473),(#330474,#330475,#330476),(#330477,
#330478,#330479),(#330480,#330481,#330482),(#330483,#330484,#330485),(#330486,
#330487,#330488),(#330489,#330490,#330491),(#330492,#330493,#330494),(#330495,
#330496,#330497),(#330498,#330499,#330500),(#330501,#330502,#330503),(#330504,
#330505,#330506),(#330507,#330508,#330509),(#330510,#330511,#330512),(#330513,
#330514,#330515),(#330516,#330517,#330518),(#330519,#330520,#330521),(#330522,
#330523,#330524),(#330525,#330526,#330527),(#330528,#330529,#330530),(#330531,
#330532,#330533),(#330534,#330535,#330536),(#330537,#330538,#330539),(#330540,
#330541,#330542),(#330543,#330544,#330545),(#330546,#330547,#330548),(#330549,
#330550,#330551),(#330552,#330553,#330554),(#330555,#330556,#330557),(#330558,
#330559,#330560),(#330561,#330562,#330563),(#330564,#330565,#330566),(#330567,
#330568,#330569),(#330570,#330571,#330572),(#330573,#330574,#330575),(#330576,
#330577,#330578),(#330579,#330580,#330581),(#330582,#330583,#330584),(#330585,
#330586,#330587),(#330588,#330589,#330590),(#330591,#330592,#330593),(#330594,
#330595,#330596),(#330597,#330598,#330599),(#330600,#330601,#330602),(#330603,
#330604,#330605),(#330606,#330607,#330608),(#330609,#330610,#330611),(#330612,
#330613,#330614),(#330615,#330616,#330617),(#330618,#330619,#330620),(#330621,
#330622,#330623),(#330624,#330625,#330626),(#330627,#330628,#330629),(#330630,
#330631,#330632),(#330633,#330634,#330635),(#330636,#330637,#330638),(#330639,
#330640,#330641),(#330642,#330643,#330644),(#330645,#330646,#330647),(#330648,
#330649,#330650),(#330651,#330652,#330653),(#330654,#330655,#330656),(#330657,
#330658,#330659),(#330660,#330661,#330662),(#330663,#330664,#330665),(#330666,
#330667,#330668),(#330669,#330670,#330671),(#330672,#330673,#330674),(#330675,
#330676,#330677),(#330678,#330679,#330680),(#330681,#330682,#330683),(#330684,
#330685,#330686),(#330687,#330688,#330689),(#330690,#330691,#330692),(#330693,
#330694,#330695),(#330696,#330697,#330698),(#330699,#330700,#330701),(#330702,
#330703,#330704),(#330705,#330706,#330707),(#330708,#330709,#330710),(#330711,
#330712,#330713),(#330714,#330715,#330716),(#330717,#330718,#330719),(#330720,
#330721,#330722),(#330723,#330724,#330725),(#330726,#330727,#330728),(#330729,
#330730,#330731),(#330732,#330733,#330734),(#330735,#330736,#330737),(#330738,
#330739,#330740),(#330741,#330742,#330743),(#330744,#330745,#330746),(#330747,
#330748,#330749),(#330750,#330751,#330752),(#330753,#330754,#330755),(#330756,
#330757,#330758),(#330759,#330760,#330761),(#330762,#330763,#330764),(#330765,
#330766,#330767),(#330768,#330769,#330770),(#330771,#330772,#330773),(#330774,
#330775,#330776),(#330777,#330778,#330779),(#330780,#330781,#330782),(#330783,
#330784,#330785),(#330786,#330787,#330788),(#330789,#330790,#330791),(#330792,
#330793,#330794),(#330795,#330796,#330797),(#330798,#330799,#330800),(#330801,
#330802,#330803),(#330804,#330805,#330806),(#330807,#330808,#330809),(#330810,
#330811,#330812),(#330813,#330814,#330815),(#330816,#330817,#330818),(#330819,
#330820,#330821),(#330822,#330823,#330824),(#330825,#330826,#330827),(#330828,
#330829,#330830),(#330831,#330832,#330833),(#330834,#330835,#330836),(#330837,
#330838,#330839),(#330840,#330841,#330842),(#330843,#330844,#330845),(#330846,
#330847,#330848),(#330849,#330850,#330851),(#330852,#330853,#330854),(#330855,
#330856,#330857),(#330858,#330859,#330860),(#330861,#330862,#330863),(#330864,
#330865,#330866),(#330867,#330868,#330869),(#330870,#330871,#330872),(#330873,
#330874,#330875),(#330876,#330877,#330878),(#330879,#330880,#330881),(#330882,
#330883,#330884),(#330885,#330886,#330887),(#330888,#330889,#330890),(#330891,
#330892,#330893),(#330894,#330895,#330896),(#330897,#330898,#330899),(#330900,
#330901,#330902),(#330903,#330904,#330905),(#330906,#330907,#330908),(#330909,
#330910,#330911),(#330912,#330913,#330914),(#330915,#330916,#330917),(#330918,
#330919,#330920),(#330921,#330922,#330923),(#330924,#330925,#330926),(#330927,
#330928,#330929),(#330930,#330931,#330932),(#330933,#330934,#330935),(#330936,
#330937,#330938),(#330939,#330940,#330941),(#330942,#330943,#330944),(#330945,
#330946,#330947),(#330948,#330949,#330950),(#330951,#330952,#330953),(#330954,
#330955,#330956),(#330957,#330958,#330959),(#330960,#330961,#330962),(#330963,
#330964,#330965),(#330966,#330967,#330968),(#330969,#330970,#330971),(#330972,
#330973,#330974),(#330975,#330976,#330977),(#330978,#330979,#330980),(#330981,
#330982,#330983),(#330984,#330985,#330986),(#330987,#330988,#330989),(#330990,
#330991,#330992),(#330993,#330994,#330995),(#330996,#330997,#330998),(#330999,
#331000,#331001),(#331002,#331003,#331004),(#331005,#331006,#331007),(#331008,
#331009,#331010),(#331011,#331012,#331013),(#331014,#331015,#331016),(#331017,
#331018,#331019),(#331020,#331021,#331022),(#331023,#331024,#331025),(#331026,
#331027,#331028),(#331029,#331030,#331031),(#331032,#331033,#331034),(#331035,
#331036,#331037),(#331038,#331039,#331040),(#331041,#331042,#331043),(#331044,
#331045,#331046),(#331047,#331048,#331049),(#331050,#331051,#331052),(#331053,
#331054,#331055),(#331056,#331057,#331058),(#331059,#331060,#331061),(#331062,
#331063,#331064),(#331065,#331066,#331067),(#331068,#331069,#331070),(#331071,
#331072,#331073),(#331074,#331075,#331076),(#331077,#331078,#331079),(#331080,
#331081,#331082),(#331083,#331084,#331085),(#331086,#331087,#331088),(#331089,
#331090,#331091),(#331092,#331093,#331094),(#331095,#331096,#331097),(#331098,
#331099,#331100),(#331101,#331102,#331103),(#331104,#331105,#331106),(#331107,
#331108,#331109),(#331110,#331111,#331112),(#331113,#331114,#331115),(#331116,
#331117,#331118),(#331119,#331120,#331121),(#331122,#331123,#331124),(#331125,
#331126,#331127),(#331128,#331129,#331130),(#331131,#331132,#331133),(#331134,
#331135,#331136),(#331137,#331138,#331139),(#331140,#331141,#331142),(#331143,
#331144,#331145),(#331146,#331147,#331148),(#331149,#331150,#331151),(#331152,
#331153,#331154),(#331155,#331156,#331157),(#331158,#331159,#331160),(#331161,
#331162,#331163),(#331164,#331165,#331166),(#331167,#331168,#331169),(#331170,
#331171,#331172),(#331173,#331174,#331175),(#331176,#331177,#331178),(#331179,
#331180,#331181),(#331182,#331183,#331184),(#331185,#331186,#331187),(#331188,
#331189,#331190),(#331191,#331192,#331193),(#331194,#331195,#331196),(#331197,
#331198,#331199),(#331200,#331201,#331202),(#331203,#331204,#331205),(#331206,
#331207,#331208),(#331209,#331210,#331211),(#331212,#331213,#331214),(#331215,
#331216,#331217),(#331218,#331219,#331220),(#331221,#331222,#331223),(#331224,
#331225,#331226),(#331227,#331228,#331229),(#331230,#331231,#331232),(#331233,
#331234,#331235),(#331236,#331237,#331238),(#331239,#331240,#331241),(#331242,
#331243,#331244),(#331245,#331246,#331247),(#331248,#331249,#331250),(#331251,
#331252,#331253),(#331254,#331255,#331256),(#331257,#331258,#331259),(#331260,
#331261,#331262),(#331263,#331264,#331265),(#331266,#331267,#331268),(#331269,
#331270,#331271),(#331272,#331273,#331274),(#331275,#331276,#331277),(#331278,
#331279,#331280),(#331281,#331282,#331283),(#331284,#331285,#331286),(#331287,
#331288,#331289),(#331290,#331291,#331292),(#331293,#331294,#331295),(#331296,
#331297,#331298),(#331299,#331300,#331301),(#331302,#331303,#331304),(#331305,
#331306,#331307),(#331308,#331309,#331310),(#331311,#331312,#331313),(#331314,
#331315,#331316),(#331317,#331318,#331319),(#331320,#331321,#331322),(#331323,
#331324,#331325),(#331326,#331327,#331328),(#331329,#331330,#331331),(#331332,
#331333,#331334),(#331335,#331336,#331337),(#331338,#331339,#331340),(#331341,
#331342,#331343),(#331344,#331345,#331346),(#331347,#331348,#331349),(#331350,
#331351,#331352),(#331353,#331354,#331355),(#331356,#331357,#331358),(#331359,
#331360,#331361),(#331362,#331363,#331364),(#331365,#331366,#331367),(#331368,
#331369,#331370),(#331371,#331372,#331373),(#331374,#331375,#331376),(#331377,
#331378,#331379),(#331380,#331381,#331382),(#331383,#331384,#331385),(#331386,
#331387,#331388),(#331389,#331390,#331391),(#331392,#331393,#331394),(#331395,
#331396,#331397),(#331398,#331399,#331400),(#331401,#331402,#331403),(#331404,
#331405,#331406),(#331407,#331408,#331409),(#331410,#331411,#331412),(#331413,
#331414,#331415),(#331416,#331417,#331418),(#331419,#331420,#331421),(#331422,
#331423,#331424),(#331425,#331426,#331427),(#331428,#331429,#331430),(#331431,
#331432,#331433),(#331434,#331435,#331436),(#331437,#331438,#331439),(#331440,
#331441,#331442),(#331443,#331444,#331445),(#331446,#331447,#331448),(#331449,
#331450,#331451),(#331452,#331453,#331454),(#331455,#331456,#331457),(#331458,
#331459,#331460),(#331461,#331462,#331463),(#331464,#331465,#331466),(#331467,
#331468,#331469),(#331470,#331471,#331472),(#331473,#331474,#331475),(#331476,
#331477,#331478),(#331479,#331480,#331481),(#331482,#331483,#331484),(#331485,
#331486,#331487),(#331488,#331489,#331490),(#331491,#331492,#331493),(#331494,
#331495,#331496),(#331497,#331498,#331499),(#331500,#331501,#331502),(#331503,
#331504,#331505),(#331506,#331507,#331508),(#331509,#331510,#331511),(#331512,
#331513,#331514),(#331515,#331516,#331517),(#331518,#331519,#331520),(#331521,
#331522,#331523),(#331524,#331525,#331526),(#331527,#331528,#331529),(#331530,
#331531,#331532),(#331533,#331534,#331535),(#331536,#331537,#331538),(#331539,
#331540,#331541),(#331542,#331543,#331544),(#331545,#331546,#331547),(#331548,
#331549,#331550),(#331551,#331552,#331553),(#331554,#331555,#331556),(#331557,
#331558,#331559),(#331560,#331561,#331562),(#331563,#331564,#331565),(#331566,
#331567,#331568),(#331569,#331570,#331571),(#331572,#331573,#331574),(#331575,
#331576,#331577),(#331578,#331579,#331580),(#331581,#331582,#331583),(#331584,
#331585,#331586),(#331587,#331588,#331589),(#331590,#331591,#331592),(#331593,
#331594,#331595),(#331596,#331597,#331598),(#331599,#331600,#331601),(#331602,
#331603,#331604),(#331605,#331606,#331607),(#331608,#331609,#331610),(#331611,
#331612,#331613),(#331614,#331615,#331616),(#331617,#331618,#331619),(#331620,
#331621,#331622),(#331623,#331624,#331625),(#331626,#331627,#331628),(#331629,
#331630,#331631),(#331632,#331633,#331634),(#331635,#331636,#331637),(#331638,
#331639,#331640),(#331641,#331642,#331643),(#331644,#331645,#331646),(#331647,
#331648,#331649)),.UNSPECIFIED.,.F.,.F.,.F.,(6,1,1,1,1,1,1,1,1,1,1,1,1,
1,1,1,1,1,1,1,1,1,1,1,1,1,1,1,1,1,1,1,1,1,1,1,1,1,1,1,1,1,1,1,1,1,1,1,1,
1,1,1,1,1,1,1,1,1,1,1,1,1,1,1,1,1,1,1,1,1,1,1,1,1,1,1,1,1,1,1,1,1,1,1,1,
1,1,1,1,1,1,1,1,1,1,1,1,1,1,1,1,1,1,1,1,1,1,1,1,1,1,1,1,1,1,1,1,1,1,1,1,
1,1,1,1,1,1,1,1,1,1,1,1,1,1,1,1,1,1,1,1,1,1,1,1,1,1,1,1,1,1,1,1,1,1,1,1,
1,1,1,1,1,1,1,1,1,1,1,1,1,1,1,1,1,1,1,1,1,1,1,1,1,1,1,1,1,1,1,1,1,1,1,1,
1,1,1,1,1,1,1,1,1,1,1,1,1,1,1,1,1,1,1,1,1,1,1,1,1,1,1,1,1,1,1,1,1,1,1,1,
1,1,1,1,1,1,1,1,1,1,1,1,1,1,1,1,1,1,1,1,1,1,1,1,1,1,1,1,1,1,1,1,1,1,1,1,
1,1,1,1,1,1,1,1,1,1,1,1,1,1,1,1,1,1,1,1,1,1,1,1,1,1,1,1,1,1,1,1,1,1,1,1,
1,1,1,1,1,1,1,1,1,1,1,1,1,1,1,1,1,1,1,1,1,1,1,1,1,1,1,1,1,1,1,1,1,1,1,1,
1,1,1,1,1,1,1,1,1,1,1,1,1,1,1,1,1,1,1,1,1,1,1,1,1,1,1,1,1,1,1,1,1,1,1,1,
1,1,1,1,1,1,1,1,1,1,1,1,1,1,1,1,1,1,1,1,1,1,1,1,1,1,1,1,1,1,1,1,1,1,1,1,
1,1,1,1,1,1,1,1,1,1,1,1,1,1,1,1,1,1,1,1,1,1,1,1,1,1,1,1,1,1,1,1,1,1,1,1,
1,1,1,1,1,1,1,1,1,1,1,1,1,1,1,1,1,1,1,1,1,1,1,1,1,1,1,1,1,1,1,1,1,1,1,1,
1,1,1,1,1,1,1,1,1,1,1,1,1,1,1,1,1,1,1,1,1,1,1,1,1,1,1,1,1,1,1,1,1,1,1,1,
1,1,1,1,1,1,1,1,1,1,1,1,1,1,1,1,1,1,1,1,1,1,1,1,1,1,1,1,1,6),(2,1,2),(-0.001964159,
0.,0.001834862,0.003669725,0.005504587,0.00733945,0.009174312,0.011009174,
0.012844037,0.014678899,0.016513761,0.018348624,0.020183486,0.022018349,
0.023853211,0.025688073,0.027522936,0.029357798,0.031192661,0.033027523,
0.034862385,0.036697248,0.03853211,0.040366972,0.042201835,0.044036697,
0.04587156,0.047706422,0.049541284,0.051376147,0.053211009,0.055045872,
0.056880734,0.058715596,0.060550459,0.062385321,0.064220183,0.066055046,
0.067889908,0.069724771,0.071559633,0.073394495,0.075229358,0.07706422,
0.078899083,0.080733945,0.082568807,0.08440367,0.086238532,0.088073394,
0.089908257,0.091743119,0.093577982,0.095412844,0.097247706,0.099082569,
0.100917431,0.102752294,0.104587156,0.106422018,0.108256881,0.110091743,
0.111926606,0.113761468,0.11559633,0.117431193,0.119266055,0.121100917,
0.12293578,0.124770642,0.126605505,0.128440367,0.130275229,0.132110092,
0.133944954,0.135779817,0.137614679,0.139449541,0.141284404,0.143119266,
0.144954128,0.146788991,0.148623853,0.150458716,0.152293578,0.15412844,
0.155963303,0.157798165,0.159633028,0.16146789,0.163302752,0.165137615,
0.166972477,0.168807339,0.170642202,0.172477064,0.174311927,0.176146789,
0.177981651,0.179816514,0.181651376,0.183486239,0.185321101,0.187155963,
0.188990826,0.190825688,0.19266055,0.194495413,0.196330275,0.198165138,
0.2,0.201834862,0.203669725,0.205504587,0.20733945,0.209174312,0.211009174,
0.212844037,0.214678899,0.216513761,0.218348624,0.220183486,0.222018349,
0.223853211,0.225688073,0.227522936,0.229357798,0.231192661,0.233027523,
0.234862385,0.236697248,0.23853211,0.240366972,0.242201835,0.244036697,
0.24587156,0.247706422,0.249541284,0.251376147,0.253211009,0.255045872,
0.256880734,0.258715596,0.260550459,0.262385321,0.264220183,0.266055046,
0.267889908,0.269724771,0.271559633,0.273394495,0.275229358,0.27706422,
0.278899083,0.280733945,0.282568807,0.28440367,0.286238532,0.288073394,
0.289908257,0.291743119,0.293577982,0.295412844,0.297247706,0.299082569,
0.300917431,0.302752294,0.304587156,0.306422018,0.308256881,0.310091743,
0.311926606,0.313761468,0.31559633,0.317431193,0.319266055,0.321100917,
0.32293578,0.324770642,0.326605505,0.328440367,0.330275229,0.332110092,
0.333944954,0.335779817,0.337614679,0.339449541,0.341284404,0.343119266,
0.344954128,0.346788991,0.348623853,0.350458716,0.352293578,0.35412844,
0.355963303,0.357798165,0.359633028,0.36146789,0.363302752,0.365137615,
0.366972477,0.368807339,0.370642202,0.372477064,0.374311927,0.376146789,
0.377981651,0.379816514,0.381651376,0.383486239,0.385321101,0.387155963,
0.388990826,0.390825688,0.39266055,0.394495413,0.396330275,0.398165138,
0.4,0.401834862,0.403669725,0.405504587,0.40733945,0.409174312,0.411009174,
0.412844037,0.414678899,0.416513761,0.418348624,0.420183486,0.422018349,
0.423853211,0.425688073,0.427522936,0.429357798,0.431192661,0.433027523,
0.434862385,0.436697248,0.43853211,0.440366972,0.442201835,0.444036697,
0.44587156,0.447706422,0.449541284,0.451376147,0.453211009,0.455045872,
0.456880734,0.458715596,0.460550459,0.462385321,0.464220183,0.466055046,
0.467889908,0.469724771,0.471559633,0.473394495,0.475229358,0.47706422,
0.478899083,0.480733945,0.482568807,0.48440367,0.486238532,0.488073394,
0.489908257,0.491743119,0.493577982,0.495412844,0.497247706,0.499082569,
0.500917431,0.502752294,0.504587156,0.506422018,0.508256881,0.510091743,
0.511926606,0.513761468,0.51559633,0.517431193,0.519266055,0.521100917,
0.52293578,0.524770642,0.526605505,0.528440367,0.530275229,0.532110092,
0.533944954,0.535779817,0.537614679,0.539449541,0.541284404,0.543119266,
0.544954128,0.546788991,0.548623853,0.550458716,0.552293578,0.55412844,
0.555963303,0.557798165,0.559633028,0.56146789,0.563302752,0.565137615,
0.566972477,0.568807339,0.570642202,0.572477064,0.574311927,0.576146789,
0.577981651,0.579816514,0.581651376,0.583486239,0.585321101,0.587155963,
0.588990826,0.590825688,0.59266055,0.594495413,0.596330275,0.598165138,
0.6,0.601834862,0.603669725,0.605504587,0.60733945,0.609174312,0.611009174,
0.612844037,0.614678899,0.616513761,0.618348624,0.620183486,0.622018349,
0.623853211,0.625688073,0.627522936,0.629357798,0.631192661,0.633027523,
0.634862385,0.636697248,0.63853211,0.640366972,0.642201835,0.644036697,
0.64587156,0.647706422,0.649541284,0.651376147,0.653211009,0.655045872,
0.656880734,0.658715596,0.660550459,0.662385321,0.664220183,0.666055046,
0.667889908,0.669724771,0.671559633,0.673394495,0.675229358,0.67706422,
0.678899083,0.680733945,0.682568807,0.68440367,0.686238532,0.688073394,
0.689908257,0.691743119,0.693577982,0.695412844,0.697247706,0.699082569,
0.700917431,0.702752294,0.704587156,0.706422018,0.708256881,0.710091743,
0.711926606,0.713761468,0.71559633,0.717431193,0.719266055,0.721100917,
0.72293578,0.724770642,0.726605505,0.728440367,0.730275229,0.732110092,
0.733944954,0.735779817,0.737614679,0.739449541,0.741284404,0.743119266,
0.744954128,0.746788991,0.748623853,0.750458716,0.752293578,0.75412844,
0.755963303,0.757798165,0.759633028,0.76146789,0.763302752,0.765137615,
0.766972477,0.768807339,0.770642202,0.772477064,0.774311927,0.776146789,
0.777981651,0.779816514,0.781651376,0.783486239,0.785321101,0.787155963,
0.788990826,0.790825688,0.79266055,0.794495413,0.796330275,0.798165138,
0.8,0.801834862,0.803669725,0.805504587,0.80733945,0.809174312,0.811009174,
0.812844037,0.814678899,0.816513761,0.818348624,0.820183486,0.822018349,
0.823853211,0.825688073,0.827522936,0.829357798,0.831192661,0.833027523,
0.834862385,0.836697248,0.83853211,0.840366972,0.842201835,0.844036697,
0.84587156,0.847706422,0.849541284,0.851376147,0.853211009,0.855045872,
0.856880734,0.858715596,0.860550459,0.862385321,0.864220183,0.866055046,
0.867889908,0.869724771,0.871559633,0.873394495,0.875229358,0.87706422,
0.878899083,0.880733945,0.882568807,0.88440367,0.886238532,0.888073394,
0.889908257,0.891743119,0.893577982,0.895412844,0.897247706,0.899082569,
0.900917431,0.902752294,0.904587156,0.906422018,0.908256881,0.910091743,
0.911926606,0.913761468,0.91559633,0.917431193,0.919266055,0.921100917,
0.92293578,0.924770642,0.926605505,0.928440367,0.930275229,0.932110092,
0.933944954,0.935779817,0.937614679,0.939449541,0.941284404,0.943119266,
0.944954128,0.946788991,0.948623853,0.950458716,0.952293578,0.95412844,
0.955963303,0.957798165,0.959633028,0.96146789,0.963302752,0.965137615,
0.966972477,0.968807339,0.970642202,0.972477064,0.974311927,0.976146789,
0.977981651,0.979816514,0.981651376,0.983486239,0.985321101,0.987155963,
0.988990826,0.990825688,0.99266055,0.994495413,0.996330275,0.998165138,
1.000000000385),(0.3,1.,1.3),.UNSPECIFIED.);
#6321=B_SPLINE_SURFACE_WITH_KNOTS('',5,1,((#331654,#331655,#331656),(#331657,
#331658,#331659),(#331660,#331661,#331662),(#331663,#331664,#331665),(#331666,
#331667,#331668),(#331669,#331670,#331671),(#331672,#331673,#331674),(#331675,
#331676,#331677),(#331678,#331679,#331680),(#331681,#331682,#331683),(#331684,
#331685,#331686),(#331687,#331688,#331689),(#331690,#331691,#331692),(#331693,
#331694,#331695),(#331696,#331697,#331698),(#331699,#331700,#331701),(#331702,
#331703,#331704),(#331705,#331706,#331707),(#331708,#331709,#331710),(#331711,
#331712,#331713),(#331714,#331715,#331716),(#331717,#331718,#331719),(#331720,
#331721,#331722),(#331723,#331724,#331725),(#331726,#331727,#331728),(#331729,
#331730,#331731),(#331732,#331733,#331734),(#331735,#331736,#331737),(#331738,
#331739,#331740),(#331741,#331742,#331743),(#331744,#331745,#331746),(#331747,
#331748,#331749),(#331750,#331751,#331752),(#331753,#331754,#331755),(#331756,
#331757,#331758),(#331759,#331760,#331761),(#331762,#331763,#331764),(#331765,
#331766,#331767),(#331768,#331769,#331770),(#331771,#331772,#331773),(#331774,
#331775,#331776),(#331777,#331778,#331779),(#331780,#331781,#331782),(#331783,
#331784,#331785),(#331786,#331787,#331788),(#331789,#331790,#331791),(#331792,
#331793,#331794),(#331795,#331796,#331797),(#331798,#331799,#331800),(#331801,
#331802,#331803),(#331804,#331805,#331806),(#331807,#331808,#331809),(#331810,
#331811,#331812),(#331813,#331814,#331815),(#331816,#331817,#331818),(#331819,
#331820,#331821),(#331822,#331823,#331824),(#331825,#331826,#331827),(#331828,
#331829,#331830),(#331831,#331832,#331833),(#331834,#331835,#331836),(#331837,
#331838,#331839),(#331840,#331841,#331842),(#331843,#331844,#331845),(#331846,
#331847,#331848),(#331849,#331850,#331851),(#331852,#331853,#331854),(#331855,
#331856,#331857),(#331858,#331859,#331860),(#331861,#331862,#331863),(#331864,
#331865,#331866),(#331867,#331868,#331869),(#331870,#331871,#331872),(#331873,
#331874,#331875),(#331876,#331877,#331878),(#331879,#331880,#331881),(#331882,
#331883,#331884),(#331885,#331886,#331887),(#331888,#331889,#331890),(#331891,
#331892,#331893),(#331894,#331895,#331896),(#331897,#331898,#331899),(#331900,
#331901,#331902),(#331903,#331904,#331905),(#331906,#331907,#331908),(#331909,
#331910,#331911),(#331912,#331913,#331914),(#331915,#331916,#331917),(#331918,
#331919,#331920),(#331921,#331922,#331923),(#331924,#331925,#331926),(#331927,
#331928,#331929),(#331930,#331931,#331932),(#331933,#331934,#331935),(#331936,
#331937,#331938),(#331939,#331940,#331941),(#331942,#331943,#331944),(#331945,
#331946,#331947),(#331948,#331949,#331950),(#331951,#331952,#331953),(#331954,
#331955,#331956),(#331957,#331958,#331959),(#331960,#331961,#331962),(#331963,
#331964,#331965),(#331966,#331967,#331968),(#331969,#331970,#331971),(#331972,
#331973,#331974),(#331975,#331976,#331977),(#331978,#331979,#331980),(#331981,
#331982,#331983),(#331984,#331985,#331986),(#331987,#331988,#331989),(#331990,
#331991,#331992),(#331993,#331994,#331995),(#331996,#331997,#331998),(#331999,
#332000,#332001),(#332002,#332003,#332004),(#332005,#332006,#332007),(#332008,
#332009,#332010),(#332011,#332012,#332013),(#332014,#332015,#332016),(#332017,
#332018,#332019),(#332020,#332021,#332022),(#332023,#332024,#332025),(#332026,
#332027,#332028),(#332029,#332030,#332031),(#332032,#332033,#332034),(#332035,
#332036,#332037),(#332038,#332039,#332040),(#332041,#332042,#332043),(#332044,
#332045,#332046),(#332047,#332048,#332049),(#332050,#332051,#332052),(#332053,
#332054,#332055),(#332056,#332057,#332058),(#332059,#332060,#332061),(#332062,
#332063,#332064),(#332065,#332066,#332067),(#332068,#332069,#332070),(#332071,
#332072,#332073),(#332074,#332075,#332076),(#332077,#332078,#332079),(#332080,
#332081,#332082),(#332083,#332084,#332085),(#332086,#332087,#332088),(#332089,
#332090,#332091),(#332092,#332093,#332094),(#332095,#332096,#332097),(#332098,
#332099,#332100),(#332101,#332102,#332103),(#332104,#332105,#332106),(#332107,
#332108,#332109),(#332110,#332111,#332112),(#332113,#332114,#332115),(#332116,
#332117,#332118),(#332119,#332120,#332121),(#332122,#332123,#332124),(#332125,
#332126,#332127),(#332128,#332129,#332130),(#332131,#332132,#332133),(#332134,
#332135,#332136),(#332137,#332138,#332139),(#332140,#332141,#332142),(#332143,
#332144,#332145),(#332146,#332147,#332148),(#332149,#332150,#332151),(#332152,
#332153,#332154),(#332155,#332156,#332157),(#332158,#332159,#332160),(#332161,
#332162,#332163),(#332164,#332165,#332166),(#332167,#332168,#332169),(#332170,
#332171,#332172),(#332173,#332174,#332175),(#332176,#332177,#332178),(#332179,
#332180,#332181),(#332182,#332183,#332184),(#332185,#332186,#332187),(#332188,
#332189,#332190),(#332191,#332192,#332193),(#332194,#332195,#332196),(#332197,
#332198,#332199),(#332200,#332201,#332202),(#332203,#332204,#332205),(#332206,
#332207,#332208),(#332209,#332210,#332211),(#332212,#332213,#332214),(#332215,
#332216,#332217),(#332218,#332219,#332220),(#332221,#332222,#332223),(#332224,
#332225,#332226),(#332227,#332228,#332229),(#332230,#332231,#332232),(#332233,
#332234,#332235),(#332236,#332237,#332238),(#332239,#332240,#332241),(#332242,
#332243,#332244),(#332245,#332246,#332247),(#332248,#332249,#332250),(#332251,
#332252,#332253),(#332254,#332255,#332256),(#332257,#332258,#332259),(#332260,
#332261,#332262),(#332263,#332264,#332265),(#332266,#332267,#332268),(#332269,
#332270,#332271),(#332272,#332273,#332274),(#332275,#332276,#332277),(#332278,
#332279,#332280),(#332281,#332282,#332283),(#332284,#332285,#332286),(#332287,
#332288,#332289),(#332290,#332291,#332292),(#332293,#332294,#332295),(#332296,
#332297,#332298),(#332299,#332300,#332301),(#332302,#332303,#332304),(#332305,
#332306,#332307),(#332308,#332309,#332310),(#332311,#332312,#332313),(#332314,
#332315,#332316),(#332317,#332318,#332319),(#332320,#332321,#332322),(#332323,
#332324,#332325),(#332326,#332327,#332328),(#332329,#332330,#332331),(#332332,
#332333,#332334),(#332335,#332336,#332337),(#332338,#332339,#332340),(#332341,
#332342,#332343),(#332344,#332345,#332346),(#332347,#332348,#332349),(#332350,
#332351,#332352),(#332353,#332354,#332355),(#332356,#332357,#332358),(#332359,
#332360,#332361),(#332362,#332363,#332364),(#332365,#332366,#332367),(#332368,
#332369,#332370),(#332371,#332372,#332373),(#332374,#332375,#332376),(#332377,
#332378,#332379),(#332380,#332381,#332382),(#332383,#332384,#332385),(#332386,
#332387,#332388),(#332389,#332390,#332391),(#332392,#332393,#332394),(#332395,
#332396,#332397),(#332398,#332399,#332400),(#332401,#332402,#332403),(#332404,
#332405,#332406),(#332407,#332408,#332409),(#332410,#332411,#332412),(#332413,
#332414,#332415),(#332416,#332417,#332418),(#332419,#332420,#332421),(#332422,
#332423,#332424),(#332425,#332426,#332427),(#332428,#332429,#332430),(#332431,
#332432,#332433),(#332434,#332435,#332436),(#332437,#332438,#332439),(#332440,
#332441,#332442),(#332443,#332444,#332445),(#332446,#332447,#332448),(#332449,
#332450,#332451),(#332452,#332453,#332454),(#332455,#332456,#332457),(#332458,
#332459,#332460),(#332461,#332462,#332463),(#332464,#332465,#332466),(#332467,
#332468,#332469),(#332470,#332471,#332472),(#332473,#332474,#332475),(#332476,
#332477,#332478),(#332479,#332480,#332481),(#332482,#332483,#332484),(#332485,
#332486,#332487),(#332488,#332489,#332490),(#332491,#332492,#332493),(#332494,
#332495,#332496),(#332497,#332498,#332499),(#332500,#332501,#332502),(#332503,
#332504,#332505),(#332506,#332507,#332508),(#332509,#332510,#332511),(#332512,
#332513,#332514),(#332515,#332516,#332517),(#332518,#332519,#332520),(#332521,
#332522,#332523),(#332524,#332525,#332526),(#332527,#332528,#332529),(#332530,
#332531,#332532),(#332533,#332534,#332535),(#332536,#332537,#332538),(#332539,
#332540,#332541),(#332542,#332543,#332544),(#332545,#332546,#332547),(#332548,
#332549,#332550),(#332551,#332552,#332553),(#332554,#332555,#332556),(#332557,
#332558,#332559),(#332560,#332561,#332562),(#332563,#332564,#332565),(#332566,
#332567,#332568),(#332569,#332570,#332571),(#332572,#332573,#332574),(#332575,
#332576,#332577),(#332578,#332579,#332580),(#332581,#332582,#332583),(#332584,
#332585,#332586),(#332587,#332588,#332589),(#332590,#332591,#332592),(#332593,
#332594,#332595),(#332596,#332597,#332598),(#332599,#332600,#332601),(#332602,
#332603,#332604),(#332605,#332606,#332607),(#332608,#332609,#332610),(#332611,
#332612,#332613),(#332614,#332615,#332616),(#332617,#332618,#332619),(#332620,
#332621,#332622),(#332623,#332624,#332625),(#332626,#332627,#332628),(#332629,
#332630,#332631),(#332632,#332633,#332634),(#332635,#332636,#332637),(#332638,
#332639,#332640),(#332641,#332642,#332643),(#332644,#332645,#332646),(#332647,
#332648,#332649),(#332650,#332651,#332652),(#332653,#332654,#332655),(#332656,
#332657,#332658),(#332659,#332660,#332661),(#332662,#332663,#332664),(#332665,
#332666,#332667),(#332668,#332669,#332670),(#332671,#332672,#332673),(#332674,
#332675,#332676),(#332677,#332678,#332679),(#332680,#332681,#332682),(#332683,
#332684,#332685),(#332686,#332687,#332688),(#332689,#332690,#332691),(#332692,
#332693,#332694),(#332695,#332696,#332697),(#332698,#332699,#332700),(#332701,
#332702,#332703),(#332704,#332705,#332706),(#332707,#332708,#332709),(#332710,
#332711,#332712),(#332713,#332714,#332715),(#332716,#332717,#332718),(#332719,
#332720,#332721),(#332722,#332723,#332724),(#332725,#332726,#332727),(#332728,
#332729,#332730),(#332731,#332732,#332733),(#332734,#332735,#332736),(#332737,
#332738,#332739),(#332740,#332741,#332742),(#332743,#332744,#332745),(#332746,
#332747,#332748),(#332749,#332750,#332751),(#332752,#332753,#332754),(#332755,
#332756,#332757),(#332758,#332759,#332760),(#332761,#332762,#332763),(#332764,
#332765,#332766),(#332767,#332768,#332769),(#332770,#332771,#332772),(#332773,
#332774,#332775),(#332776,#332777,#332778),(#332779,#332780,#332781),(#332782,
#332783,#332784),(#332785,#332786,#332787),(#332788,#332789,#332790),(#332791,
#332792,#332793),(#332794,#332795,#332796),(#332797,#332798,#332799),(#332800,
#332801,#332802),(#332803,#332804,#332805),(#332806,#332807,#332808),(#332809,
#332810,#332811),(#332812,#332813,#332814),(#332815,#332816,#332817),(#332818,
#332819,#332820),(#332821,#332822,#332823),(#332824,#332825,#332826),(#332827,
#332828,#332829),(#332830,#332831,#332832),(#332833,#332834,#332835),(#332836,
#332837,#332838),(#332839,#332840,#332841),(#332842,#332843,#332844),(#332845,
#332846,#332847),(#332848,#332849,#332850),(#332851,#332852,#332853),(#332854,
#332855,#332856),(#332857,#332858,#332859),(#332860,#332861,#332862),(#332863,
#332864,#332865),(#332866,#332867,#332868),(#332869,#332870,#332871),(#332872,
#332873,#332874),(#332875,#332876,#332877),(#332878,#332879,#332880),(#332881,
#332882,#332883),(#332884,#332885,#332886),(#332887,#332888,#332889),(#332890,
#332891,#332892),(#332893,#332894,#332895),(#332896,#332897,#332898),(#332899,
#332900,#332901),(#332902,#332903,#332904),(#332905,#332906,#332907),(#332908,
#332909,#332910),(#332911,#332912,#332913),(#332914,#332915,#332916),(#332917,
#332918,#332919),(#332920,#332921,#332922),(#332923,#332924,#332925),(#332926,
#332927,#332928),(#332929,#332930,#332931),(#332932,#332933,#332934),(#332935,
#332936,#332937),(#332938,#332939,#332940),(#332941,#332942,#332943),(#332944,
#332945,#332946),(#332947,#332948,#332949),(#332950,#332951,#332952),(#332953,
#332954,#332955),(#332956,#332957,#332958),(#332959,#332960,#332961),(#332962,
#332963,#332964),(#332965,#332966,#332967),(#332968,#332969,#332970),(#332971,
#332972,#332973),(#332974,#332975,#332976),(#332977,#332978,#332979),(#332980,
#332981,#332982),(#332983,#332984,#332985),(#332986,#332987,#332988),(#332989,
#332990,#332991),(#332992,#332993,#332994),(#332995,#332996,#332997),(#332998,
#332999,#333000),(#333001,#333002,#333003),(#333004,#333005,#333006),(#333007,
#333008,#333009),(#333010,#333011,#333012),(#333013,#333014,#333015),(#333016,
#333017,#333018),(#333019,#333020,#333021),(#333022,#333023,#333024),(#333025,
#333026,#333027),(#333028,#333029,#333030),(#333031,#333032,#333033),(#333034,
#333035,#333036),(#333037,#333038,#333039),(#333040,#333041,#333042),(#333043,
#333044,#333045),(#333046,#333047,#333048),(#333049,#333050,#333051),(#333052,
#333053,#333054),(#333055,#333056,#333057),(#333058,#333059,#333060),(#333061,
#333062,#333063),(#333064,#333065,#333066),(#333067,#333068,#333069),(#333070,
#333071,#333072),(#333073,#333074,#333075),(#333076,#333077,#333078),(#333079,
#333080,#333081),(#333082,#333083,#333084),(#333085,#333086,#333087),(#333088,
#333089,#333090),(#333091,#333092,#333093),(#333094,#333095,#333096),(#333097,
#333098,#333099),(#333100,#333101,#333102),(#333103,#333104,#333105),(#333106,
#333107,#333108),(#333109,#333110,#333111),(#333112,#333113,#333114),(#333115,
#333116,#333117),(#333118,#333119,#333120),(#333121,#333122,#333123),(#333124,
#333125,#333126),(#333127,#333128,#333129),(#333130,#333131,#333132),(#333133,
#333134,#333135),(#333136,#333137,#333138),(#333139,#333140,#333141),(#333142,
#333143,#333144),(#333145,#333146,#333147),(#333148,#333149,#333150),(#333151,
#333152,#333153),(#333154,#333155,#333156),(#333157,#333158,#333159),(#333160,
#333161,#333162),(#333163,#333164,#333165),(#333166,#333167,#333168),(#333169,
#333170,#333171),(#333172,#333173,#333174),(#333175,#333176,#333177),(#333178,
#333179,#333180),(#333181,#333182,#333183),(#333184,#333185,#333186),(#333187,
#333188,#333189),(#333190,#333191,#333192),(#333193,#333194,#333195),(#333196,
#333197,#333198),(#333199,#333200,#333201),(#333202,#333203,#333204),(#333205,
#333206,#333207),(#333208,#333209,#333210),(#333211,#333212,#333213),(#333214,
#333215,#333216),(#333217,#333218,#333219),(#333220,#333221,#333222),(#333223,
#333224,#333225),(#333226,#333227,#333228),(#333229,#333230,#333231),(#333232,
#333233,#333234),(#333235,#333236,#333237),(#333238,#333239,#333240),(#333241,
#333242,#333243),(#333244,#333245,#333246),(#333247,#333248,#333249),(#333250,
#333251,#333252),(#333253,#333254,#333255),(#333256,#333257,#333258),(#333259,
#333260,#333261),(#333262,#333263,#333264),(#333265,#333266,#333267),(#333268,
#333269,#333270),(#333271,#333272,#333273),(#333274,#333275,#333276),(#333277,
#333278,#333279),(#333280,#333281,#333282),(#333283,#333284,#333285),(#333286,
#333287,#333288),(#333289,#333290,#333291),(#333292,#333293,#333294),(#333295,
#333296,#333297),(#333298,#333299,#333300),(#333301,#333302,#333303)),
 .UNSPECIFIED.,.F.,.F.,.F.,(6,1,1,1,1,1,1,1,1,1,1,1,1,1,1,1,1,1,1,1,1,1,
1,1,1,1,1,1,1,1,1,1,1,1,1,1,1,1,1,1,1,1,1,1,1,1,1,1,1,1,1,1,1,1,1,1,1,1,
1,1,1,1,1,1,1,1,1,1,1,1,1,1,1,1,1,1,1,1,1,1,1,1,1,1,1,1,1,1,1,1,1,1,1,1,
1,1,1,1,1,1,1,1,1,1,1,1,1,1,1,1,1,1,1,1,1,1,1,1,1,1,1,1,1,1,1,1,1,1,1,1,
1,1,1,1,1,1,1,1,1,1,1,1,1,1,1,1,1,1,1,1,1,1,1,1,1,1,1,1,1,1,1,1,1,1,1,1,
1,1,1,1,1,1,1,1,1,1,1,1,1,1,1,1,1,1,1,1,1,1,1,1,1,1,1,1,1,1,1,1,1,1,1,1,
1,1,1,1,1,1,1,1,1,1,1,1,1,1,1,1,1,1,1,1,1,1,1,1,1,1,1,1,1,1,1,1,1,1,1,1,
1,1,1,1,1,1,1,1,1,1,1,1,1,1,1,1,1,1,1,1,1,1,1,1,1,1,1,1,1,1,1,1,1,1,1,1,
1,1,1,1,1,1,1,1,1,1,1,1,1,1,1,1,1,1,1,1,1,1,1,1,1,1,1,1,1,1,1,1,1,1,1,1,
1,1,1,1,1,1,1,1,1,1,1,1,1,1,1,1,1,1,1,1,1,1,1,1,1,1,1,1,1,1,1,1,1,1,1,1,
1,1,1,1,1,1,1,1,1,1,1,1,1,1,1,1,1,1,1,1,1,1,1,1,1,1,1,1,1,1,1,1,1,1,1,1,
1,1,1,1,1,1,1,1,1,1,1,1,1,1,1,1,1,1,1,1,1,1,1,1,1,1,1,1,1,1,1,1,1,1,1,1,
1,1,1,1,1,1,1,1,1,1,1,1,1,1,1,1,1,1,1,1,1,1,1,1,1,1,1,1,1,1,1,1,1,1,1,1,
1,1,1,1,1,1,1,1,1,1,1,1,1,1,1,1,1,1,1,1,1,1,1,1,1,1,1,1,1,1,1,1,1,1,1,1,
1,1,1,1,1,1,1,1,1,1,1,1,1,1,1,1,1,1,1,1,1,1,1,1,1,1,1,1,1,1,1,1,1,1,1,1,
1,1,1,1,1,1,1,1,1,1,1,1,1,1,1,1,1,1,1,6),(2,1,2),(-1.,-0.998165138,-0.996330275,
-0.994495413,-0.99266055,-0.990825688,-0.988990826,-0.987155963,-0.985321101,
-0.983486239,-0.981651376,-0.979816514,-0.977981651,-0.976146789,-0.974311927,
-0.972477064,-0.970642202,-0.968807339,-0.966972477,-0.965137615,-0.963302752,
-0.96146789,-0.959633028,-0.957798165,-0.955963303,-0.95412844,-0.952293578,
-0.950458716,-0.948623853,-0.946788991,-0.944954128,-0.943119266,-0.941284404,
-0.939449541,-0.937614679,-0.935779817,-0.933944954,-0.932110092,-0.930275229,
-0.928440367,-0.926605505,-0.924770642,-0.92293578,-0.921100917,-0.919266055,
-0.917431193,-0.91559633,-0.913761468,-0.911926606,-0.910091743,-0.908256881,
-0.906422018,-0.904587156,-0.902752294,-0.900917431,-0.899082569,-0.897247706,
-0.895412844,-0.893577982,-0.891743119,-0.889908257,-0.888073394,-0.886238532,
-0.88440367,-0.882568807,-0.880733945,-0.878899083,-0.87706422,-0.875229358,
-0.873394495,-0.871559633,-0.869724771,-0.867889908,-0.866055046,-0.864220183,
-0.862385321,-0.860550459,-0.858715596,-0.856880734,-0.855045872,-0.853211009,
-0.851376147,-0.849541284,-0.847706422,-0.84587156,-0.844036697,-0.842201835,
-0.840366972,-0.83853211,-0.836697248,-0.834862385,-0.833027523,-0.831192661,
-0.829357798,-0.827522936,-0.825688073,-0.823853211,-0.822018349,-0.820183486,
-0.818348624,-0.816513761,-0.814678899,-0.812844037,-0.811009174,-0.809174312,
-0.80733945,-0.805504587,-0.803669725,-0.801834862,-0.8,-0.798165138,-0.796330275,
-0.794495413,-0.79266055,-0.790825688,-0.788990826,-0.787155963,-0.785321101,
-0.783486239,-0.781651376,-0.779816514,-0.777981651,-0.776146789,-0.774311927,
-0.772477064,-0.770642202,-0.768807339,-0.766972477,-0.765137615,-0.763302752,
-0.76146789,-0.759633028,-0.757798165,-0.755963303,-0.75412844,-0.752293578,
-0.750458716,-0.748623853,-0.746788991,-0.744954128,-0.743119266,-0.741284404,
-0.739449541,-0.737614679,-0.735779817,-0.733944954,-0.732110092,-0.730275229,
-0.728440367,-0.726605505,-0.724770642,-0.72293578,-0.721100917,-0.719266055,
-0.717431193,-0.71559633,-0.713761468,-0.711926606,-0.710091743,-0.708256881,
-0.706422018,-0.704587156,-0.702752294,-0.700917431,-0.699082569,-0.697247706,
-0.695412844,-0.693577982,-0.691743119,-0.689908257,-0.688073394,-0.686238532,
-0.68440367,-0.682568807,-0.680733945,-0.678899083,-0.67706422,-0.675229358,
-0.673394495,-0.671559633,-0.669724771,-0.667889908,-0.666055046,-0.664220183,
-0.662385321,-0.660550459,-0.658715596,-0.656880734,-0.655045872,-0.653211009,
-0.651376147,-0.649541284,-0.647706422,-0.64587156,-0.644036697,-0.642201835,
-0.640366972,-0.63853211,-0.636697248,-0.634862385,-0.633027523,-0.631192661,
-0.629357798,-0.627522936,-0.625688073,-0.623853211,-0.622018349,-0.620183486,
-0.618348624,-0.616513761,-0.614678899,-0.612844037,-0.611009174,-0.609174312,
-0.60733945,-0.605504587,-0.603669725,-0.601834862,-0.6,-0.598165138,-0.596330275,
-0.594495413,-0.59266055,-0.590825688,-0.588990826,-0.587155963,-0.585321101,
-0.583486239,-0.581651376,-0.579816514,-0.577981651,-0.576146789,-0.574311927,
-0.572477064,-0.570642202,-0.568807339,-0.566972477,-0.565137615,-0.563302752,
-0.56146789,-0.559633028,-0.557798165,-0.555963303,-0.55412844,-0.552293578,
-0.550458716,-0.548623853,-0.546788991,-0.544954128,-0.543119266,-0.541284404,
-0.539449541,-0.537614679,-0.535779817,-0.533944954,-0.532110092,-0.530275229,
-0.528440367,-0.526605505,-0.524770642,-0.52293578,-0.521100917,-0.519266055,
-0.517431193,-0.51559633,-0.513761468,-0.511926606,-0.510091743,-0.508256881,
-0.506422018,-0.504587156,-0.502752294,-0.500917431,-0.499082569,-0.497247706,
-0.495412844,-0.493577982,-0.491743119,-0.489908257,-0.488073394,-0.486238532,
-0.48440367,-0.482568807,-0.480733945,-0.478899083,-0.47706422,-0.475229358,
-0.473394495,-0.471559633,-0.469724771,-0.467889908,-0.466055046,-0.464220183,
-0.462385321,-0.460550459,-0.458715596,-0.456880734,-0.455045872,-0.453211009,
-0.451376147,-0.449541284,-0.447706422,-0.44587156,-0.444036697,-0.442201835,
-0.440366972,-0.43853211,-0.436697248,-0.434862385,-0.433027523,-0.431192661,
-0.429357798,-0.427522936,-0.425688073,-0.423853211,-0.422018349,-0.420183486,
-0.418348624,-0.416513761,-0.414678899,-0.412844037,-0.411009174,-0.409174312,
-0.40733945,-0.405504587,-0.403669725,-0.401834862,-0.4,-0.398165138,-0.396330275,
-0.394495413,-0.39266055,-0.390825688,-0.388990826,-0.387155963,-0.385321101,
-0.383486239,-0.381651376,-0.379816514,-0.377981651,-0.376146789,-0.374311927,
-0.372477064,-0.370642202,-0.368807339,-0.366972477,-0.365137615,-0.363302752,
-0.36146789,-0.359633028,-0.357798165,-0.355963303,-0.35412844,-0.352293578,
-0.350458716,-0.348623853,-0.346788991,-0.344954128,-0.343119266,-0.341284404,
-0.339449541,-0.337614679,-0.335779817,-0.333944954,-0.332110092,-0.330275229,
-0.328440367,-0.326605505,-0.324770642,-0.32293578,-0.321100917,-0.319266055,
-0.317431193,-0.31559633,-0.313761468,-0.311926606,-0.310091743,-0.308256881,
-0.306422018,-0.304587156,-0.302752294,-0.300917431,-0.299082569,-0.297247706,
-0.295412844,-0.293577982,-0.291743119,-0.289908257,-0.288073394,-0.286238532,
-0.28440367,-0.282568807,-0.280733945,-0.278899083,-0.27706422,-0.275229358,
-0.273394495,-0.271559633,-0.269724771,-0.267889908,-0.266055046,-0.264220183,
-0.262385321,-0.260550459,-0.258715596,-0.256880734,-0.255045872,-0.253211009,
-0.251376147,-0.249541284,-0.247706422,-0.24587156,-0.244036697,-0.242201835,
-0.240366972,-0.23853211,-0.236697248,-0.234862385,-0.233027523,-0.231192661,
-0.229357798,-0.227522936,-0.225688073,-0.223853211,-0.222018349,-0.220183486,
-0.218348624,-0.216513761,-0.214678899,-0.212844037,-0.211009174,-0.209174312,
-0.20733945,-0.205504587,-0.203669725,-0.201834862,-0.2,-0.198165138,-0.196330275,
-0.194495413,-0.19266055,-0.190825688,-0.188990826,-0.187155963,-0.185321101,
-0.183486239,-0.181651376,-0.179816514,-0.177981651,-0.176146789,-0.174311927,
-0.172477064,-0.170642202,-0.168807339,-0.166972477,-0.165137615,-0.163302752,
-0.16146789,-0.159633028,-0.157798165,-0.155963303,-0.15412844,-0.152293578,
-0.150458716,-0.148623853,-0.146788991,-0.144954128,-0.143119266,-0.141284404,
-0.139449541,-0.137614679,-0.135779817,-0.133944954,-0.132110092,-0.130275229,
-0.128440367,-0.126605505,-0.124770642,-0.12293578,-0.121100917,-0.119266055,
-0.117431193,-0.11559633,-0.113761468,-0.111926606,-0.110091743,-0.108256881,
-0.106422018,-0.104587156,-0.102752294,-0.100917431,-0.099082569,-0.097247706,
-0.095412844,-0.093577982,-0.091743119,-0.089908257,-0.088073394,-0.086238532,
-0.08440367,-0.082568807,-0.080733945,-0.078899083,-0.07706422,-0.075229358,
-0.073394495,-0.071559633,-0.069724771,-0.067889908,-0.066055046,-0.064220183,
-0.062385321,-0.060550459,-0.058715596,-0.056880734,-0.055045872,-0.053211009,
-0.051376147,-0.049541284,-0.047706422,-0.04587156,-0.044036697,-0.042201835,
-0.040366972,-0.03853211,-0.036697248,-0.034862385,-0.033027523,-0.031192661,
-0.029357798,-0.027522936,-0.025688073,-0.023853211,-0.022018349,-0.020183486,
-0.018348624,-0.016513761,-0.014678899,-0.012844037,-0.011009174,-0.009174312,
-0.00733945,-0.005504587,-0.003669725,-0.001834862,0.000982147),(0.3,1.,
1.3),.UNSPECIFIED.);
#6322=B_SPLINE_SURFACE_WITH_KNOTS('',5,1,((#333307,#333308,#333309),(#333310,
#333311,#333312),(#333313,#333314,#333315),(#333316,#333317,#333318),(#333319,
#333320,#333321),(#333322,#333323,#333324),(#333325,#333326,#333327),(#333328,
#333329,#333330),(#333331,#333332,#333333),(#333334,#333335,#333336),(#333337,
#333338,#333339),(#333340,#333341,#333342),(#333343,#333344,#333345),(#333346,
#333347,#333348),(#333349,#333350,#333351),(#333352,#333353,#333354),(#333355,
#333356,#333357),(#333358,#333359,#333360),(#333361,#333362,#333363),(#333364,
#333365,#333366),(#333367,#333368,#333369),(#333370,#333371,#333372),(#333373,
#333374,#333375),(#333376,#333377,#333378),(#333379,#333380,#333381),(#333382,
#333383,#333384),(#333385,#333386,#333387),(#333388,#333389,#333390),(#333391,
#333392,#333393),(#333394,#333395,#333396),(#333397,#333398,#333399),(#333400,
#333401,#333402),(#333403,#333404,#333405),(#333406,#333407,#333408),(#333409,
#333410,#333411),(#333412,#333413,#333414),(#333415,#333416,#333417),(#333418,
#333419,#333420),(#333421,#333422,#333423),(#333424,#333425,#333426),(#333427,
#333428,#333429),(#333430,#333431,#333432),(#333433,#333434,#333435),(#333436,
#333437,#333438),(#333439,#333440,#333441),(#333442,#333443,#333444),(#333445,
#333446,#333447),(#333448,#333449,#333450),(#333451,#333452,#333453),(#333454,
#333455,#333456),(#333457,#333458,#333459),(#333460,#333461,#333462),(#333463,
#333464,#333465),(#333466,#333467,#333468),(#333469,#333470,#333471),(#333472,
#333473,#333474),(#333475,#333476,#333477),(#333478,#333479,#333480),(#333481,
#333482,#333483),(#333484,#333485,#333486),(#333487,#333488,#333489),(#333490,
#333491,#333492),(#333493,#333494,#333495),(#333496,#333497,#333498),(#333499,
#333500,#333501),(#333502,#333503,#333504),(#333505,#333506,#333507),(#333508,
#333509,#333510),(#333511,#333512,#333513),(#333514,#333515,#333516),(#333517,
#333518,#333519),(#333520,#333521,#333522),(#333523,#333524,#333525),(#333526,
#333527,#333528),(#333529,#333530,#333531),(#333532,#333533,#333534),(#333535,
#333536,#333537),(#333538,#333539,#333540),(#333541,#333542,#333543),(#333544,
#333545,#333546),(#333547,#333548,#333549),(#333550,#333551,#333552),(#333553,
#333554,#333555),(#333556,#333557,#333558),(#333559,#333560,#333561),(#333562,
#333563,#333564),(#333565,#333566,#333567),(#333568,#333569,#333570),(#333571,
#333572,#333573),(#333574,#333575,#333576),(#333577,#333578,#333579),(#333580,
#333581,#333582),(#333583,#333584,#333585),(#333586,#333587,#333588),(#333589,
#333590,#333591),(#333592,#333593,#333594),(#333595,#333596,#333597),(#333598,
#333599,#333600),(#333601,#333602,#333603),(#333604,#333605,#333606),(#333607,
#333608,#333609),(#333610,#333611,#333612),(#333613,#333614,#333615),(#333616,
#333617,#333618),(#333619,#333620,#333621),(#333622,#333623,#333624),(#333625,
#333626,#333627),(#333628,#333629,#333630),(#333631,#333632,#333633),(#333634,
#333635,#333636),(#333637,#333638,#333639),(#333640,#333641,#333642),(#333643,
#333644,#333645),(#333646,#333647,#333648),(#333649,#333650,#333651),(#333652,
#333653,#333654),(#333655,#333656,#333657),(#333658,#333659,#333660),(#333661,
#333662,#333663),(#333664,#333665,#333666),(#333667,#333668,#333669),(#333670,
#333671,#333672),(#333673,#333674,#333675),(#333676,#333677,#333678),(#333679,
#333680,#333681),(#333682,#333683,#333684),(#333685,#333686,#333687),(#333688,
#333689,#333690),(#333691,#333692,#333693),(#333694,#333695,#333696),(#333697,
#333698,#333699),(#333700,#333701,#333702),(#333703,#333704,#333705),(#333706,
#333707,#333708),(#333709,#333710,#333711),(#333712,#333713,#333714),(#333715,
#333716,#333717),(#333718,#333719,#333720),(#333721,#333722,#333723),(#333724,
#333725,#333726),(#333727,#333728,#333729),(#333730,#333731,#333732),(#333733,
#333734,#333735),(#333736,#333737,#333738),(#333739,#333740,#333741),(#333742,
#333743,#333744),(#333745,#333746,#333747),(#333748,#333749,#333750),(#333751,
#333752,#333753),(#333754,#333755,#333756),(#333757,#333758,#333759),(#333760,
#333761,#333762),(#333763,#333764,#333765),(#333766,#333767,#333768),(#333769,
#333770,#333771),(#333772,#333773,#333774),(#333775,#333776,#333777),(#333778,
#333779,#333780),(#333781,#333782,#333783),(#333784,#333785,#333786),(#333787,
#333788,#333789),(#333790,#333791,#333792),(#333793,#333794,#333795),(#333796,
#333797,#333798),(#333799,#333800,#333801),(#333802,#333803,#333804),(#333805,
#333806,#333807),(#333808,#333809,#333810),(#333811,#333812,#333813),(#333814,
#333815,#333816),(#333817,#333818,#333819),(#333820,#333821,#333822),(#333823,
#333824,#333825),(#333826,#333827,#333828),(#333829,#333830,#333831),(#333832,
#333833,#333834),(#333835,#333836,#333837),(#333838,#333839,#333840),(#333841,
#333842,#333843),(#333844,#333845,#333846),(#333847,#333848,#333849),(#333850,
#333851,#333852),(#333853,#333854,#333855),(#333856,#333857,#333858),(#333859,
#333860,#333861),(#333862,#333863,#333864),(#333865,#333866,#333867),(#333868,
#333869,#333870),(#333871,#333872,#333873),(#333874,#333875,#333876),(#333877,
#333878,#333879),(#333880,#333881,#333882),(#333883,#333884,#333885),(#333886,
#333887,#333888),(#333889,#333890,#333891),(#333892,#333893,#333894),(#333895,
#333896,#333897),(#333898,#333899,#333900),(#333901,#333902,#333903),(#333904,
#333905,#333906),(#333907,#333908,#333909),(#333910,#333911,#333912),(#333913,
#333914,#333915),(#333916,#333917,#333918),(#333919,#333920,#333921),(#333922,
#333923,#333924),(#333925,#333926,#333927),(#333928,#333929,#333930),(#333931,
#333932,#333933),(#333934,#333935,#333936),(#333937,#333938,#333939),(#333940,
#333941,#333942),(#333943,#333944,#333945),(#333946,#333947,#333948),(#333949,
#333950,#333951),(#333952,#333953,#333954),(#333955,#333956,#333957),(#333958,
#333959,#333960),(#333961,#333962,#333963),(#333964,#333965,#333966),(#333967,
#333968,#333969),(#333970,#333971,#333972),(#333973,#333974,#333975),(#333976,
#333977,#333978),(#333979,#333980,#333981),(#333982,#333983,#333984),(#333985,
#333986,#333987),(#333988,#333989,#333990),(#333991,#333992,#333993),(#333994,
#333995,#333996),(#333997,#333998,#333999),(#334000,#334001,#334002),(#334003,
#334004,#334005),(#334006,#334007,#334008),(#334009,#334010,#334011),(#334012,
#334013,#334014),(#334015,#334016,#334017),(#334018,#334019,#334020),(#334021,
#334022,#334023),(#334024,#334025,#334026),(#334027,#334028,#334029),(#334030,
#334031,#334032),(#334033,#334034,#334035),(#334036,#334037,#334038),(#334039,
#334040,#334041),(#334042,#334043,#334044),(#334045,#334046,#334047),(#334048,
#334049,#334050),(#334051,#334052,#334053),(#334054,#334055,#334056),(#334057,
#334058,#334059),(#334060,#334061,#334062),(#334063,#334064,#334065),(#334066,
#334067,#334068),(#334069,#334070,#334071),(#334072,#334073,#334074),(#334075,
#334076,#334077),(#334078,#334079,#334080),(#334081,#334082,#334083),(#334084,
#334085,#334086),(#334087,#334088,#334089),(#334090,#334091,#334092),(#334093,
#334094,#334095),(#334096,#334097,#334098),(#334099,#334100,#334101),(#334102,
#334103,#334104),(#334105,#334106,#334107),(#334108,#334109,#334110),(#334111,
#334112,#334113),(#334114,#334115,#334116),(#334117,#334118,#334119),(#334120,
#334121,#334122),(#334123,#334124,#334125),(#334126,#334127,#334128),(#334129,
#334130,#334131),(#334132,#334133,#334134),(#334135,#334136,#334137),(#334138,
#334139,#334140),(#334141,#334142,#334143),(#334144,#334145,#334146),(#334147,
#334148,#334149),(#334150,#334151,#334152),(#334153,#334154,#334155),(#334156,
#334157,#334158),(#334159,#334160,#334161),(#334162,#334163,#334164),(#334165,
#334166,#334167),(#334168,#334169,#334170),(#334171,#334172,#334173),(#334174,
#334175,#334176),(#334177,#334178,#334179),(#334180,#334181,#334182),(#334183,
#334184,#334185),(#334186,#334187,#334188),(#334189,#334190,#334191),(#334192,
#334193,#334194),(#334195,#334196,#334197),(#334198,#334199,#334200),(#334201,
#334202,#334203),(#334204,#334205,#334206),(#334207,#334208,#334209),(#334210,
#334211,#334212),(#334213,#334214,#334215),(#334216,#334217,#334218),(#334219,
#334220,#334221),(#334222,#334223,#334224),(#334225,#334226,#334227),(#334228,
#334229,#334230),(#334231,#334232,#334233),(#334234,#334235,#334236),(#334237,
#334238,#334239),(#334240,#334241,#334242),(#334243,#334244,#334245),(#334246,
#334247,#334248),(#334249,#334250,#334251),(#334252,#334253,#334254),(#334255,
#334256,#334257),(#334258,#334259,#334260),(#334261,#334262,#334263),(#334264,
#334265,#334266),(#334267,#334268,#334269),(#334270,#334271,#334272),(#334273,
#334274,#334275),(#334276,#334277,#334278),(#334279,#334280,#334281),(#334282,
#334283,#334284),(#334285,#334286,#334287),(#334288,#334289,#334290),(#334291,
#334292,#334293),(#334294,#334295,#334296),(#334297,#334298,#334299),(#334300,
#334301,#334302),(#334303,#334304,#334305),(#334306,#334307,#334308),(#334309,
#334310,#334311),(#334312,#334313,#334314),(#334315,#334316,#334317),(#334318,
#334319,#334320),(#334321,#334322,#334323),(#334324,#334325,#334326),(#334327,
#334328,#334329),(#334330,#334331,#334332),(#334333,#334334,#334335),(#334336,
#334337,#334338),(#334339,#334340,#334341),(#334342,#334343,#334344),(#334345,
#334346,#334347),(#334348,#334349,#334350),(#334351,#334352,#334353),(#334354,
#334355,#334356),(#334357,#334358,#334359),(#334360,#334361,#334362),(#334363,
#334364,#334365),(#334366,#334367,#334368),(#334369,#334370,#334371),(#334372,
#334373,#334374),(#334375,#334376,#334377),(#334378,#334379,#334380),(#334381,
#334382,#334383),(#334384,#334385,#334386),(#334387,#334388,#334389),(#334390,
#334391,#334392),(#334393,#334394,#334395),(#334396,#334397,#334398),(#334399,
#334400,#334401),(#334402,#334403,#334404),(#334405,#334406,#334407),(#334408,
#334409,#334410),(#334411,#334412,#334413),(#334414,#334415,#334416),(#334417,
#334418,#334419),(#334420,#334421,#334422),(#334423,#334424,#334425),(#334426,
#334427,#334428),(#334429,#334430,#334431),(#334432,#334433,#334434),(#334435,
#334436,#334437),(#334438,#334439,#334440),(#334441,#334442,#334443),(#334444,
#334445,#334446),(#334447,#334448,#334449),(#334450,#334451,#334452),(#334453,
#334454,#334455),(#334456,#334457,#334458),(#334459,#334460,#334461),(#334462,
#334463,#334464),(#334465,#334466,#334467),(#334468,#334469,#334470),(#334471,
#334472,#334473),(#334474,#334475,#334476),(#334477,#334478,#334479),(#334480,
#334481,#334482),(#334483,#334484,#334485),(#334486,#334487,#334488),(#334489,
#334490,#334491),(#334492,#334493,#334494),(#334495,#334496,#334497),(#334498,
#334499,#334500),(#334501,#334502,#334503),(#334504,#334505,#334506),(#334507,
#334508,#334509),(#334510,#334511,#334512),(#334513,#334514,#334515),(#334516,
#334517,#334518),(#334519,#334520,#334521),(#334522,#334523,#334524),(#334525,
#334526,#334527),(#334528,#334529,#334530),(#334531,#334532,#334533),(#334534,
#334535,#334536),(#334537,#334538,#334539),(#334540,#334541,#334542),(#334543,
#334544,#334545),(#334546,#334547,#334548),(#334549,#334550,#334551),(#334552,
#334553,#334554),(#334555,#334556,#334557),(#334558,#334559,#334560),(#334561,
#334562,#334563),(#334564,#334565,#334566),(#334567,#334568,#334569),(#334570,
#334571,#334572),(#334573,#334574,#334575),(#334576,#334577,#334578),(#334579,
#334580,#334581),(#334582,#334583,#334584),(#334585,#334586,#334587),(#334588,
#334589,#334590),(#334591,#334592,#334593),(#334594,#334595,#334596),(#334597,
#334598,#334599),(#334600,#334601,#334602),(#334603,#334604,#334605),(#334606,
#334607,#334608),(#334609,#334610,#334611),(#334612,#334613,#334614),(#334615,
#334616,#334617),(#334618,#334619,#334620),(#334621,#334622,#334623),(#334624,
#334625,#334626),(#334627,#334628,#334629),(#334630,#334631,#334632),(#334633,
#334634,#334635),(#334636,#334637,#334638),(#334639,#334640,#334641),(#334642,
#334643,#334644),(#334645,#334646,#334647),(#334648,#334649,#334650),(#334651,
#334652,#334653),(#334654,#334655,#334656),(#334657,#334658,#334659),(#334660,
#334661,#334662),(#334663,#334664,#334665),(#334666,#334667,#334668),(#334669,
#334670,#334671),(#334672,#334673,#334674),(#334675,#334676,#334677),(#334678,
#334679,#334680),(#334681,#334682,#334683),(#334684,#334685,#334686),(#334687,
#334688,#334689),(#334690,#334691,#334692),(#334693,#334694,#334695),(#334696,
#334697,#334698),(#334699,#334700,#334701),(#334702,#334703,#334704),(#334705,
#334706,#334707),(#334708,#334709,#334710),(#334711,#334712,#334713),(#334714,
#334715,#334716),(#334717,#334718,#334719),(#334720,#334721,#334722),(#334723,
#334724,#334725),(#334726,#334727,#334728),(#334729,#334730,#334731),(#334732,
#334733,#334734),(#334735,#334736,#334737),(#334738,#334739,#334740),(#334741,
#334742,#334743),(#334744,#334745,#334746),(#334747,#334748,#334749),(#334750,
#334751,#334752),(#334753,#334754,#334755),(#334756,#334757,#334758),(#334759,
#334760,#334761),(#334762,#334763,#334764),(#334765,#334766,#334767),(#334768,
#334769,#334770),(#334771,#334772,#334773),(#334774,#334775,#334776),(#334777,
#334778,#334779),(#334780,#334781,#334782),(#334783,#334784,#334785),(#334786,
#334787,#334788),(#334789,#334790,#334791),(#334792,#334793,#334794),(#334795,
#334796,#334797),(#334798,#334799,#334800),(#334801,#334802,#334803),(#334804,
#334805,#334806),(#334807,#334808,#334809),(#334810,#334811,#334812),(#334813,
#334814,#334815),(#334816,#334817,#334818),(#334819,#334820,#334821),(#334822,
#334823,#334824),(#334825,#334826,#334827),(#334828,#334829,#334830),(#334831,
#334832,#334833),(#334834,#334835,#334836),(#334837,#334838,#334839),(#334840,
#334841,#334842),(#334843,#334844,#334845),(#334846,#334847,#334848),(#334849,
#334850,#334851),(#334852,#334853,#334854),(#334855,#334856,#334857),(#334858,
#334859,#334860),(#334861,#334862,#334863),(#334864,#334865,#334866),(#334867,
#334868,#334869),(#334870,#334871,#334872),(#334873,#334874,#334875),(#334876,
#334877,#334878),(#334879,#334880,#334881),(#334882,#334883,#334884),(#334885,
#334886,#334887),(#334888,#334889,#334890),(#334891,#334892,#334893),(#334894,
#334895,#334896),(#334897,#334898,#334899),(#334900,#334901,#334902),(#334903,
#334904,#334905),(#334906,#334907,#334908),(#334909,#334910,#334911),(#334912,
#334913,#334914),(#334915,#334916,#334917),(#334918,#334919,#334920),(#334921,
#334922,#334923),(#334924,#334925,#334926),(#334927,#334928,#334929),(#334930,
#334931,#334932),(#334933,#334934,#334935),(#334936,#334937,#334938),(#334939,
#334940,#334941),(#334942,#334943,#334944),(#334945,#334946,#334947),(#334948,
#334949,#334950),(#334951,#334952,#334953),(#334954,#334955,#334956),(#334957,
#334958,#334959)),.UNSPECIFIED.,.F.,.F.,.F.,(6,1,1,1,1,1,1,1,1,1,1,1,1,
1,1,1,1,1,1,1,1,1,1,1,1,1,1,1,1,1,1,1,1,1,1,1,1,1,1,1,1,1,1,1,1,1,1,1,1,
1,1,1,1,1,1,1,1,1,1,1,1,1,1,1,1,1,1,1,1,1,1,1,1,1,1,1,1,1,1,1,1,1,1,1,1,
1,1,1,1,1,1,1,1,1,1,1,1,1,1,1,1,1,1,1,1,1,1,1,1,1,1,1,1,1,1,1,1,1,1,1,1,
1,1,1,1,1,1,1,1,1,1,1,1,1,1,1,1,1,1,1,1,1,1,1,1,1,1,1,1,1,1,1,1,1,1,1,1,
1,1,1,1,1,1,1,1,1,1,1,1,1,1,1,1,1,1,1,1,1,1,1,1,1,1,1,1,1,1,1,1,1,1,1,1,
1,1,1,1,1,1,1,1,1,1,1,1,1,1,1,1,1,1,1,1,1,1,1,1,1,1,1,1,1,1,1,1,1,1,1,1,
1,1,1,1,1,1,1,1,1,1,1,1,1,1,1,1,1,1,1,1,1,1,1,1,1,1,1,1,1,1,1,1,1,1,1,1,
1,1,1,1,1,1,1,1,1,1,1,1,1,1,1,1,1,1,1,1,1,1,1,1,1,1,1,1,1,1,1,1,1,1,1,1,
1,1,1,1,1,1,1,1,1,1,1,1,1,1,1,1,1,1,1,1,1,1,1,1,1,1,1,1,1,1,1,1,1,1,1,1,
1,1,1,1,1,1,1,1,1,1,1,1,1,1,1,1,1,1,1,1,1,1,1,1,1,1,1,1,1,1,1,1,1,1,1,1,
1,1,1,1,1,1,1,1,1,1,1,1,1,1,1,1,1,1,1,1,1,1,1,1,1,1,1,1,1,1,1,1,1,1,1,1,
1,1,1,1,1,1,1,1,1,1,1,1,1,1,1,1,1,1,1,1,1,1,1,1,1,1,1,1,1,1,1,1,1,1,1,1,
1,1,1,1,1,1,1,1,1,1,1,1,1,1,1,1,1,1,1,1,1,1,1,1,1,1,1,1,1,1,1,1,1,1,1,1,
1,1,1,1,1,1,1,1,1,1,1,1,1,1,1,1,1,1,1,1,1,1,1,1,1,1,1,1,1,1,1,1,1,1,1,1,
1,1,1,1,1,1,1,1,1,1,1,1,1,1,1,1,1,1,1,1,1,1,1,1,1,1,1,1,1,6),(2,1,2),(-0.001964137,
0.,0.001834862,0.003669725,0.005504587,0.00733945,0.009174312,0.011009174,
0.012844037,0.014678899,0.016513761,0.018348624,0.020183486,0.022018349,
0.023853211,0.025688073,0.027522936,0.029357798,0.031192661,0.033027523,
0.034862385,0.036697248,0.03853211,0.040366972,0.042201835,0.044036697,
0.04587156,0.047706422,0.049541284,0.051376147,0.053211009,0.055045872,
0.056880734,0.058715596,0.060550459,0.062385321,0.064220183,0.066055046,
0.067889908,0.069724771,0.071559633,0.073394495,0.075229358,0.07706422,
0.078899083,0.080733945,0.082568807,0.08440367,0.086238532,0.088073394,
0.089908257,0.091743119,0.093577982,0.095412844,0.097247706,0.099082569,
0.100917431,0.102752294,0.104587156,0.106422018,0.108256881,0.110091743,
0.111926606,0.113761468,0.11559633,0.117431193,0.119266055,0.121100917,
0.12293578,0.124770642,0.126605505,0.128440367,0.130275229,0.132110092,
0.133944954,0.135779817,0.137614679,0.139449541,0.141284404,0.143119266,
0.144954128,0.146788991,0.148623853,0.150458716,0.152293578,0.15412844,
0.155963303,0.157798165,0.159633028,0.16146789,0.163302752,0.165137615,
0.166972477,0.168807339,0.170642202,0.172477064,0.174311927,0.176146789,
0.177981651,0.179816514,0.181651376,0.183486239,0.185321101,0.187155963,
0.188990826,0.190825688,0.19266055,0.194495413,0.196330275,0.198165138,
0.2,0.201834862,0.203669725,0.205504587,0.20733945,0.209174312,0.211009174,
0.212844037,0.214678899,0.216513761,0.218348624,0.220183486,0.222018349,
0.223853211,0.225688073,0.227522936,0.229357798,0.231192661,0.233027523,
0.234862385,0.236697248,0.23853211,0.240366972,0.242201835,0.244036697,
0.24587156,0.247706422,0.249541284,0.251376147,0.253211009,0.255045872,
0.256880734,0.258715596,0.260550459,0.262385321,0.264220183,0.266055046,
0.267889908,0.269724771,0.271559633,0.273394495,0.275229358,0.27706422,
0.278899083,0.280733945,0.282568807,0.28440367,0.286238532,0.288073394,
0.289908257,0.291743119,0.293577982,0.295412844,0.297247706,0.299082569,
0.300917431,0.302752294,0.304587156,0.306422018,0.308256881,0.310091743,
0.311926606,0.313761468,0.31559633,0.317431193,0.319266055,0.321100917,
0.32293578,0.324770642,0.326605505,0.328440367,0.330275229,0.332110092,
0.333944954,0.335779817,0.337614679,0.339449541,0.341284404,0.343119266,
0.344954128,0.346788991,0.348623853,0.350458716,0.352293578,0.35412844,
0.355963303,0.357798165,0.359633028,0.36146789,0.363302752,0.365137615,
0.366972477,0.368807339,0.370642202,0.372477064,0.374311927,0.376146789,
0.377981651,0.379816514,0.381651376,0.383486239,0.385321101,0.387155963,
0.388990826,0.390825688,0.39266055,0.394495413,0.396330275,0.398165138,
0.4,0.401834862,0.403669725,0.405504587,0.40733945,0.409174312,0.411009174,
0.412844037,0.414678899,0.416513761,0.418348624,0.420183486,0.422018349,
0.423853211,0.425688073,0.427522936,0.429357798,0.431192661,0.433027523,
0.434862385,0.436697248,0.43853211,0.440366972,0.442201835,0.444036697,
0.44587156,0.447706422,0.449541284,0.451376147,0.453211009,0.455045872,
0.456880734,0.458715596,0.460550459,0.462385321,0.464220183,0.466055046,
0.467889908,0.469724771,0.471559633,0.473394495,0.475229358,0.47706422,
0.478899083,0.480733945,0.482568807,0.48440367,0.486238532,0.488073394,
0.489908257,0.491743119,0.493577982,0.495412844,0.497247706,0.499082569,
0.500917431,0.502752294,0.504587156,0.506422018,0.508256881,0.510091743,
0.511926606,0.513761468,0.51559633,0.517431193,0.519266055,0.521100917,
0.52293578,0.524770642,0.526605505,0.528440367,0.530275229,0.532110092,
0.533944954,0.535779817,0.537614679,0.539449541,0.541284404,0.543119266,
0.544954128,0.546788991,0.548623853,0.550458716,0.552293578,0.55412844,
0.555963303,0.557798165,0.559633028,0.56146789,0.563302752,0.565137615,
0.566972477,0.568807339,0.570642202,0.572477064,0.574311927,0.576146789,
0.577981651,0.579816514,0.581651376,0.583486239,0.585321101,0.587155963,
0.588990826,0.590825688,0.59266055,0.594495413,0.596330275,0.598165138,
0.6,0.601834862,0.603669725,0.605504587,0.60733945,0.609174312,0.611009174,
0.612844037,0.614678899,0.616513761,0.618348624,0.620183486,0.622018349,
0.623853211,0.625688073,0.627522936,0.629357798,0.631192661,0.633027523,
0.634862385,0.636697248,0.63853211,0.640366972,0.642201835,0.644036697,
0.64587156,0.647706422,0.649541284,0.651376147,0.653211009,0.655045872,
0.656880734,0.658715596,0.660550459,0.662385321,0.664220183,0.666055046,
0.667889908,0.669724771,0.671559633,0.673394495,0.675229358,0.67706422,
0.678899083,0.680733945,0.682568807,0.68440367,0.686238532,0.688073394,
0.689908257,0.691743119,0.693577982,0.695412844,0.697247706,0.699082569,
0.700917431,0.702752294,0.704587156,0.706422018,0.708256881,0.710091743,
0.711926606,0.713761468,0.71559633,0.717431193,0.719266055,0.721100917,
0.72293578,0.724770642,0.726605505,0.728440367,0.730275229,0.732110092,
0.733944954,0.735779817,0.737614679,0.739449541,0.741284404,0.743119266,
0.744954128,0.746788991,0.748623853,0.750458716,0.752293578,0.75412844,
0.755963303,0.757798165,0.759633028,0.76146789,0.763302752,0.765137615,
0.766972477,0.768807339,0.770642202,0.772477064,0.774311927,0.776146789,
0.777981651,0.779816514,0.781651376,0.783486239,0.785321101,0.787155963,
0.788990826,0.790825688,0.79266055,0.794495413,0.796330275,0.798165138,
0.8,0.801834862,0.803669725,0.805504587,0.80733945,0.809174312,0.811009174,
0.812844037,0.814678899,0.816513761,0.818348624,0.820183486,0.822018349,
0.823853211,0.825688073,0.827522936,0.829357798,0.831192661,0.833027523,
0.834862385,0.836697248,0.83853211,0.840366972,0.842201835,0.844036697,
0.84587156,0.847706422,0.849541284,0.851376147,0.853211009,0.855045872,
0.856880734,0.858715596,0.860550459,0.862385321,0.864220183,0.866055046,
0.867889908,0.869724771,0.871559633,0.873394495,0.875229358,0.87706422,
0.878899083,0.880733945,0.882568807,0.88440367,0.886238532,0.888073394,
0.889908257,0.891743119,0.893577982,0.895412844,0.897247706,0.899082569,
0.900917431,0.902752294,0.904587156,0.906422018,0.908256881,0.910091743,
0.911926606,0.913761468,0.91559633,0.917431193,0.919266055,0.921100917,
0.92293578,0.924770642,0.926605505,0.928440367,0.930275229,0.932110092,
0.933944954,0.935779817,0.937614679,0.939449541,0.941284404,0.943119266,
0.944954128,0.946788991,0.948623853,0.950458716,0.952293578,0.95412844,
0.955963303,0.957798165,0.959633028,0.96146789,0.963302752,0.965137615,
0.966972477,0.968807339,0.970642202,0.972477064,0.974311927,0.976146789,
0.977981651,0.979816514,0.981651376,0.983486239,0.985321101,0.987155963,
0.988990826,0.990825688,0.99266055,0.994495413,0.996330275,0.998165138,
1.),(0.3,1.,1.3),.UNSPECIFIED.);
#6323=B_SPLINE_SURFACE_WITH_KNOTS('',5,1,((#334970,#334971,#334972),(#334973,
#334974,#334975),(#334976,#334977,#334978),(#334979,#334980,#334981),(#334982,
#334983,#334984),(#334985,#334986,#334987),(#334988,#334989,#334990),(#334991,
#334992,#334993),(#334994,#334995,#334996),(#334997,#334998,#334999),(#335000,
#335001,#335002),(#335003,#335004,#335005),(#335006,#335007,#335008),(#335009,
#335010,#335011),(#335012,#335013,#335014),(#335015,#335016,#335017),(#335018,
#335019,#335020),(#335021,#335022,#335023),(#335024,#335025,#335026),(#335027,
#335028,#335029),(#335030,#335031,#335032),(#335033,#335034,#335035),(#335036,
#335037,#335038),(#335039,#335040,#335041),(#335042,#335043,#335044),(#335045,
#335046,#335047),(#335048,#335049,#335050),(#335051,#335052,#335053),(#335054,
#335055,#335056),(#335057,#335058,#335059),(#335060,#335061,#335062),(#335063,
#335064,#335065),(#335066,#335067,#335068),(#335069,#335070,#335071),(#335072,
#335073,#335074),(#335075,#335076,#335077),(#335078,#335079,#335080),(#335081,
#335082,#335083),(#335084,#335085,#335086),(#335087,#335088,#335089),(#335090,
#335091,#335092),(#335093,#335094,#335095),(#335096,#335097,#335098),(#335099,
#335100,#335101),(#335102,#335103,#335104),(#335105,#335106,#335107),(#335108,
#335109,#335110),(#335111,#335112,#335113),(#335114,#335115,#335116),(#335117,
#335118,#335119),(#335120,#335121,#335122),(#335123,#335124,#335125),(#335126,
#335127,#335128),(#335129,#335130,#335131),(#335132,#335133,#335134),(#335135,
#335136,#335137),(#335138,#335139,#335140),(#335141,#335142,#335143),(#335144,
#335145,#335146),(#335147,#335148,#335149),(#335150,#335151,#335152),(#335153,
#335154,#335155),(#335156,#335157,#335158),(#335159,#335160,#335161),(#335162,
#335163,#335164),(#335165,#335166,#335167),(#335168,#335169,#335170),(#335171,
#335172,#335173),(#335174,#335175,#335176),(#335177,#335178,#335179),(#335180,
#335181,#335182),(#335183,#335184,#335185),(#335186,#335187,#335188),(#335189,
#335190,#335191),(#335192,#335193,#335194),(#335195,#335196,#335197),(#335198,
#335199,#335200),(#335201,#335202,#335203),(#335204,#335205,#335206),(#335207,
#335208,#335209),(#335210,#335211,#335212),(#335213,#335214,#335215),(#335216,
#335217,#335218),(#335219,#335220,#335221),(#335222,#335223,#335224),(#335225,
#335226,#335227),(#335228,#335229,#335230),(#335231,#335232,#335233),(#335234,
#335235,#335236),(#335237,#335238,#335239),(#335240,#335241,#335242),(#335243,
#335244,#335245),(#335246,#335247,#335248),(#335249,#335250,#335251),(#335252,
#335253,#335254),(#335255,#335256,#335257),(#335258,#335259,#335260),(#335261,
#335262,#335263),(#335264,#335265,#335266),(#335267,#335268,#335269),(#335270,
#335271,#335272),(#335273,#335274,#335275),(#335276,#335277,#335278),(#335279,
#335280,#335281),(#335282,#335283,#335284),(#335285,#335286,#335287),(#335288,
#335289,#335290),(#335291,#335292,#335293),(#335294,#335295,#335296),(#335297,
#335298,#335299),(#335300,#335301,#335302),(#335303,#335304,#335305),(#335306,
#335307,#335308),(#335309,#335310,#335311),(#335312,#335313,#335314),(#335315,
#335316,#335317),(#335318,#335319,#335320),(#335321,#335322,#335323),(#335324,
#335325,#335326),(#335327,#335328,#335329),(#335330,#335331,#335332),(#335333,
#335334,#335335),(#335336,#335337,#335338),(#335339,#335340,#335341),(#335342,
#335343,#335344),(#335345,#335346,#335347),(#335348,#335349,#335350),(#335351,
#335352,#335353),(#335354,#335355,#335356),(#335357,#335358,#335359),(#335360,
#335361,#335362),(#335363,#335364,#335365),(#335366,#335367,#335368),(#335369,
#335370,#335371),(#335372,#335373,#335374),(#335375,#335376,#335377),(#335378,
#335379,#335380),(#335381,#335382,#335383),(#335384,#335385,#335386),(#335387,
#335388,#335389),(#335390,#335391,#335392),(#335393,#335394,#335395),(#335396,
#335397,#335398),(#335399,#335400,#335401),(#335402,#335403,#335404),(#335405,
#335406,#335407),(#335408,#335409,#335410),(#335411,#335412,#335413),(#335414,
#335415,#335416),(#335417,#335418,#335419),(#335420,#335421,#335422),(#335423,
#335424,#335425),(#335426,#335427,#335428),(#335429,#335430,#335431),(#335432,
#335433,#335434),(#335435,#335436,#335437),(#335438,#335439,#335440),(#335441,
#335442,#335443),(#335444,#335445,#335446),(#335447,#335448,#335449),(#335450,
#335451,#335452),(#335453,#335454,#335455),(#335456,#335457,#335458),(#335459,
#335460,#335461),(#335462,#335463,#335464),(#335465,#335466,#335467),(#335468,
#335469,#335470),(#335471,#335472,#335473),(#335474,#335475,#335476),(#335477,
#335478,#335479),(#335480,#335481,#335482),(#335483,#335484,#335485),(#335486,
#335487,#335488),(#335489,#335490,#335491),(#335492,#335493,#335494),(#335495,
#335496,#335497),(#335498,#335499,#335500),(#335501,#335502,#335503),(#335504,
#335505,#335506),(#335507,#335508,#335509),(#335510,#335511,#335512),(#335513,
#335514,#335515),(#335516,#335517,#335518),(#335519,#335520,#335521),(#335522,
#335523,#335524),(#335525,#335526,#335527),(#335528,#335529,#335530),(#335531,
#335532,#335533),(#335534,#335535,#335536),(#335537,#335538,#335539),(#335540,
#335541,#335542),(#335543,#335544,#335545),(#335546,#335547,#335548),(#335549,
#335550,#335551),(#335552,#335553,#335554),(#335555,#335556,#335557),(#335558,
#335559,#335560),(#335561,#335562,#335563),(#335564,#335565,#335566),(#335567,
#335568,#335569),(#335570,#335571,#335572),(#335573,#335574,#335575),(#335576,
#335577,#335578),(#335579,#335580,#335581),(#335582,#335583,#335584),(#335585,
#335586,#335587),(#335588,#335589,#335590),(#335591,#335592,#335593),(#335594,
#335595,#335596),(#335597,#335598,#335599),(#335600,#335601,#335602),(#335603,
#335604,#335605),(#335606,#335607,#335608),(#335609,#335610,#335611),(#335612,
#335613,#335614),(#335615,#335616,#335617),(#335618,#335619,#335620),(#335621,
#335622,#335623),(#335624,#335625,#335626),(#335627,#335628,#335629),(#335630,
#335631,#335632),(#335633,#335634,#335635),(#335636,#335637,#335638),(#335639,
#335640,#335641),(#335642,#335643,#335644),(#335645,#335646,#335647),(#335648,
#335649,#335650),(#335651,#335652,#335653),(#335654,#335655,#335656),(#335657,
#335658,#335659),(#335660,#335661,#335662),(#335663,#335664,#335665),(#335666,
#335667,#335668),(#335669,#335670,#335671),(#335672,#335673,#335674),(#335675,
#335676,#335677),(#335678,#335679,#335680),(#335681,#335682,#335683),(#335684,
#335685,#335686),(#335687,#335688,#335689),(#335690,#335691,#335692),(#335693,
#335694,#335695),(#335696,#335697,#335698),(#335699,#335700,#335701),(#335702,
#335703,#335704),(#335705,#335706,#335707),(#335708,#335709,#335710),(#335711,
#335712,#335713),(#335714,#335715,#335716),(#335717,#335718,#335719),(#335720,
#335721,#335722),(#335723,#335724,#335725),(#335726,#335727,#335728),(#335729,
#335730,#335731),(#335732,#335733,#335734),(#335735,#335736,#335737),(#335738,
#335739,#335740),(#335741,#335742,#335743),(#335744,#335745,#335746),(#335747,
#335748,#335749),(#335750,#335751,#335752),(#335753,#335754,#335755),(#335756,
#335757,#335758),(#335759,#335760,#335761),(#335762,#335763,#335764),(#335765,
#335766,#335767),(#335768,#335769,#335770),(#335771,#335772,#335773),(#335774,
#335775,#335776),(#335777,#335778,#335779),(#335780,#335781,#335782),(#335783,
#335784,#335785),(#335786,#335787,#335788),(#335789,#335790,#335791),(#335792,
#335793,#335794),(#335795,#335796,#335797),(#335798,#335799,#335800),(#335801,
#335802,#335803),(#335804,#335805,#335806),(#335807,#335808,#335809),(#335810,
#335811,#335812),(#335813,#335814,#335815),(#335816,#335817,#335818),(#335819,
#335820,#335821),(#335822,#335823,#335824),(#335825,#335826,#335827),(#335828,
#335829,#335830),(#335831,#335832,#335833),(#335834,#335835,#335836),(#335837,
#335838,#335839),(#335840,#335841,#335842),(#335843,#335844,#335845),(#335846,
#335847,#335848),(#335849,#335850,#335851),(#335852,#335853,#335854),(#335855,
#335856,#335857),(#335858,#335859,#335860),(#335861,#335862,#335863),(#335864,
#335865,#335866),(#335867,#335868,#335869),(#335870,#335871,#335872),(#335873,
#335874,#335875),(#335876,#335877,#335878),(#335879,#335880,#335881),(#335882,
#335883,#335884),(#335885,#335886,#335887),(#335888,#335889,#335890),(#335891,
#335892,#335893),(#335894,#335895,#335896),(#335897,#335898,#335899),(#335900,
#335901,#335902),(#335903,#335904,#335905),(#335906,#335907,#335908),(#335909,
#335910,#335911),(#335912,#335913,#335914),(#335915,#335916,#335917),(#335918,
#335919,#335920),(#335921,#335922,#335923),(#335924,#335925,#335926),(#335927,
#335928,#335929),(#335930,#335931,#335932),(#335933,#335934,#335935),(#335936,
#335937,#335938),(#335939,#335940,#335941),(#335942,#335943,#335944),(#335945,
#335946,#335947),(#335948,#335949,#335950),(#335951,#335952,#335953),(#335954,
#335955,#335956),(#335957,#335958,#335959),(#335960,#335961,#335962),(#335963,
#335964,#335965),(#335966,#335967,#335968),(#335969,#335970,#335971),(#335972,
#335973,#335974),(#335975,#335976,#335977),(#335978,#335979,#335980),(#335981,
#335982,#335983),(#335984,#335985,#335986),(#335987,#335988,#335989),(#335990,
#335991,#335992),(#335993,#335994,#335995),(#335996,#335997,#335998),(#335999,
#336000,#336001),(#336002,#336003,#336004),(#336005,#336006,#336007),(#336008,
#336009,#336010),(#336011,#336012,#336013),(#336014,#336015,#336016),(#336017,
#336018,#336019),(#336020,#336021,#336022),(#336023,#336024,#336025),(#336026,
#336027,#336028),(#336029,#336030,#336031),(#336032,#336033,#336034),(#336035,
#336036,#336037),(#336038,#336039,#336040),(#336041,#336042,#336043),(#336044,
#336045,#336046),(#336047,#336048,#336049),(#336050,#336051,#336052),(#336053,
#336054,#336055),(#336056,#336057,#336058),(#336059,#336060,#336061),(#336062,
#336063,#336064),(#336065,#336066,#336067),(#336068,#336069,#336070),(#336071,
#336072,#336073),(#336074,#336075,#336076),(#336077,#336078,#336079),(#336080,
#336081,#336082),(#336083,#336084,#336085),(#336086,#336087,#336088),(#336089,
#336090,#336091),(#336092,#336093,#336094),(#336095,#336096,#336097),(#336098,
#336099,#336100),(#336101,#336102,#336103),(#336104,#336105,#336106),(#336107,
#336108,#336109),(#336110,#336111,#336112),(#336113,#336114,#336115),(#336116,
#336117,#336118),(#336119,#336120,#336121),(#336122,#336123,#336124),(#336125,
#336126,#336127),(#336128,#336129,#336130),(#336131,#336132,#336133),(#336134,
#336135,#336136),(#336137,#336138,#336139),(#336140,#336141,#336142),(#336143,
#336144,#336145),(#336146,#336147,#336148),(#336149,#336150,#336151),(#336152,
#336153,#336154),(#336155,#336156,#336157),(#336158,#336159,#336160),(#336161,
#336162,#336163),(#336164,#336165,#336166),(#336167,#336168,#336169),(#336170,
#336171,#336172),(#336173,#336174,#336175),(#336176,#336177,#336178),(#336179,
#336180,#336181),(#336182,#336183,#336184),(#336185,#336186,#336187),(#336188,
#336189,#336190),(#336191,#336192,#336193),(#336194,#336195,#336196),(#336197,
#336198,#336199),(#336200,#336201,#336202),(#336203,#336204,#336205),(#336206,
#336207,#336208),(#336209,#336210,#336211),(#336212,#336213,#336214),(#336215,
#336216,#336217),(#336218,#336219,#336220),(#336221,#336222,#336223),(#336224,
#336225,#336226),(#336227,#336228,#336229),(#336230,#336231,#336232),(#336233,
#336234,#336235),(#336236,#336237,#336238),(#336239,#336240,#336241),(#336242,
#336243,#336244),(#336245,#336246,#336247),(#336248,#336249,#336250),(#336251,
#336252,#336253),(#336254,#336255,#336256),(#336257,#336258,#336259),(#336260,
#336261,#336262),(#336263,#336264,#336265),(#336266,#336267,#336268),(#336269,
#336270,#336271),(#336272,#336273,#336274),(#336275,#336276,#336277),(#336278,
#336279,#336280),(#336281,#336282,#336283),(#336284,#336285,#336286),(#336287,
#336288,#336289),(#336290,#336291,#336292),(#336293,#336294,#336295),(#336296,
#336297,#336298),(#336299,#336300,#336301),(#336302,#336303,#336304),(#336305,
#336306,#336307),(#336308,#336309,#336310),(#336311,#336312,#336313),(#336314,
#336315,#336316),(#336317,#336318,#336319),(#336320,#336321,#336322),(#336323,
#336324,#336325),(#336326,#336327,#336328),(#336329,#336330,#336331),(#336332,
#336333,#336334),(#336335,#336336,#336337),(#336338,#336339,#336340),(#336341,
#336342,#336343),(#336344,#336345,#336346),(#336347,#336348,#336349),(#336350,
#336351,#336352),(#336353,#336354,#336355),(#336356,#336357,#336358),(#336359,
#336360,#336361),(#336362,#336363,#336364),(#336365,#336366,#336367),(#336368,
#336369,#336370),(#336371,#336372,#336373),(#336374,#336375,#336376),(#336377,
#336378,#336379),(#336380,#336381,#336382),(#336383,#336384,#336385),(#336386,
#336387,#336388),(#336389,#336390,#336391),(#336392,#336393,#336394),(#336395,
#336396,#336397),(#336398,#336399,#336400),(#336401,#336402,#336403),(#336404,
#336405,#336406),(#336407,#336408,#336409),(#336410,#336411,#336412),(#336413,
#336414,#336415),(#336416,#336417,#336418),(#336419,#336420,#336421),(#336422,
#336423,#336424),(#336425,#336426,#336427),(#336428,#336429,#336430),(#336431,
#336432,#336433),(#336434,#336435,#336436),(#336437,#336438,#336439),(#336440,
#336441,#336442),(#336443,#336444,#336445),(#336446,#336447,#336448),(#336449,
#336450,#336451),(#336452,#336453,#336454),(#336455,#336456,#336457),(#336458,
#336459,#336460),(#336461,#336462,#336463),(#336464,#336465,#336466),(#336467,
#336468,#336469),(#336470,#336471,#336472),(#336473,#336474,#336475),(#336476,
#336477,#336478),(#336479,#336480,#336481),(#336482,#336483,#336484),(#336485,
#336486,#336487),(#336488,#336489,#336490),(#336491,#336492,#336493),(#336494,
#336495,#336496),(#336497,#336498,#336499),(#336500,#336501,#336502),(#336503,
#336504,#336505),(#336506,#336507,#336508),(#336509,#336510,#336511),(#336512,
#336513,#336514),(#336515,#336516,#336517),(#336518,#336519,#336520),(#336521,
#336522,#336523),(#336524,#336525,#336526),(#336527,#336528,#336529),(#336530,
#336531,#336532),(#336533,#336534,#336535),(#336536,#336537,#336538),(#336539,
#336540,#336541),(#336542,#336543,#336544),(#336545,#336546,#336547),(#336548,
#336549,#336550),(#336551,#336552,#336553),(#336554,#336555,#336556),(#336557,
#336558,#336559),(#336560,#336561,#336562),(#336563,#336564,#336565),(#336566,
#336567,#336568),(#336569,#336570,#336571),(#336572,#336573,#336574),(#336575,
#336576,#336577),(#336578,#336579,#336580),(#336581,#336582,#336583),(#336584,
#336585,#336586),(#336587,#336588,#336589),(#336590,#336591,#336592),(#336593,
#336594,#336595),(#336596,#336597,#336598),(#336599,#336600,#336601),(#336602,
#336603,#336604),(#336605,#336606,#336607),(#336608,#336609,#336610),(#336611,
#336612,#336613),(#336614,#336615,#336616),(#336617,#336618,#336619)),
 .UNSPECIFIED.,.F.,.F.,.F.,(6,1,1,1,1,1,1,1,1,1,1,1,1,1,1,1,1,1,1,1,1,1,
1,1,1,1,1,1,1,1,1,1,1,1,1,1,1,1,1,1,1,1,1,1,1,1,1,1,1,1,1,1,1,1,1,1,1,1,
1,1,1,1,1,1,1,1,1,1,1,1,1,1,1,1,1,1,1,1,1,1,1,1,1,1,1,1,1,1,1,1,1,1,1,1,
1,1,1,1,1,1,1,1,1,1,1,1,1,1,1,1,1,1,1,1,1,1,1,1,1,1,1,1,1,1,1,1,1,1,1,1,
1,1,1,1,1,1,1,1,1,1,1,1,1,1,1,1,1,1,1,1,1,1,1,1,1,1,1,1,1,1,1,1,1,1,1,1,
1,1,1,1,1,1,1,1,1,1,1,1,1,1,1,1,1,1,1,1,1,1,1,1,1,1,1,1,1,1,1,1,1,1,1,1,
1,1,1,1,1,1,1,1,1,1,1,1,1,1,1,1,1,1,1,1,1,1,1,1,1,1,1,1,1,1,1,1,1,1,1,1,
1,1,1,1,1,1,1,1,1,1,1,1,1,1,1,1,1,1,1,1,1,1,1,1,1,1,1,1,1,1,1,1,1,1,1,1,
1,1,1,1,1,1,1,1,1,1,1,1,1,1,1,1,1,1,1,1,1,1,1,1,1,1,1,1,1,1,1,1,1,1,1,1,
1,1,1,1,1,1,1,1,1,1,1,1,1,1,1,1,1,1,1,1,1,1,1,1,1,1,1,1,1,1,1,1,1,1,1,1,
1,1,1,1,1,1,1,1,1,1,1,1,1,1,1,1,1,1,1,1,1,1,1,1,1,1,1,1,1,1,1,1,1,1,1,1,
1,1,1,1,1,1,1,1,1,1,1,1,1,1,1,1,1,1,1,1,1,1,1,1,1,1,1,1,1,1,1,1,1,1,1,1,
1,1,1,1,1,1,1,1,1,1,1,1,1,1,1,1,1,1,1,1,1,1,1,1,1,1,1,1,1,1,1,1,1,1,1,1,
1,1,1,1,1,1,1,1,1,1,1,1,1,1,1,1,1,1,1,1,1,1,1,1,1,1,1,1,1,1,1,1,1,1,1,1,
1,1,1,1,1,1,1,1,1,1,1,1,1,1,1,1,1,1,1,1,1,1,1,1,1,1,1,1,1,1,1,1,1,1,1,1,
1,1,1,1,1,1,1,1,1,1,1,1,1,1,1,1,1,1,1,6),(2,1,2),(-1.,-0.998165138,-0.996330275,
-0.994495413,-0.99266055,-0.990825688,-0.988990826,-0.987155963,-0.985321101,
-0.983486239,-0.981651376,-0.979816514,-0.977981651,-0.976146789,-0.974311927,
-0.972477064,-0.970642202,-0.968807339,-0.966972477,-0.965137615,-0.963302752,
-0.96146789,-0.959633028,-0.957798165,-0.955963303,-0.95412844,-0.952293578,
-0.950458716,-0.948623853,-0.946788991,-0.944954128,-0.943119266,-0.941284404,
-0.939449541,-0.937614679,-0.935779817,-0.933944954,-0.932110092,-0.930275229,
-0.928440367,-0.926605505,-0.924770642,-0.92293578,-0.921100917,-0.919266055,
-0.917431193,-0.91559633,-0.913761468,-0.911926606,-0.910091743,-0.908256881,
-0.906422018,-0.904587156,-0.902752294,-0.900917431,-0.899082569,-0.897247706,
-0.895412844,-0.893577982,-0.891743119,-0.889908257,-0.888073394,-0.886238532,
-0.88440367,-0.882568807,-0.880733945,-0.878899083,-0.87706422,-0.875229358,
-0.873394495,-0.871559633,-0.869724771,-0.867889908,-0.866055046,-0.864220183,
-0.862385321,-0.860550459,-0.858715596,-0.856880734,-0.855045872,-0.853211009,
-0.851376147,-0.849541284,-0.847706422,-0.84587156,-0.844036697,-0.842201835,
-0.840366972,-0.83853211,-0.836697248,-0.834862385,-0.833027523,-0.831192661,
-0.829357798,-0.827522936,-0.825688073,-0.823853211,-0.822018349,-0.820183486,
-0.818348624,-0.816513761,-0.814678899,-0.812844037,-0.811009174,-0.809174312,
-0.80733945,-0.805504587,-0.803669725,-0.801834862,-0.8,-0.798165138,-0.796330275,
-0.794495413,-0.79266055,-0.790825688,-0.788990826,-0.787155963,-0.785321101,
-0.783486239,-0.781651376,-0.779816514,-0.777981651,-0.776146789,-0.774311927,
-0.772477064,-0.770642202,-0.768807339,-0.766972477,-0.765137615,-0.763302752,
-0.76146789,-0.759633028,-0.757798165,-0.755963303,-0.75412844,-0.752293578,
-0.750458716,-0.748623853,-0.746788991,-0.744954128,-0.743119266,-0.741284404,
-0.739449541,-0.737614679,-0.735779817,-0.733944954,-0.732110092,-0.730275229,
-0.728440367,-0.726605505,-0.724770642,-0.72293578,-0.721100917,-0.719266055,
-0.717431193,-0.71559633,-0.713761468,-0.711926606,-0.710091743,-0.708256881,
-0.706422018,-0.704587156,-0.702752294,-0.700917431,-0.699082569,-0.697247706,
-0.695412844,-0.693577982,-0.691743119,-0.689908257,-0.688073394,-0.686238532,
-0.68440367,-0.682568807,-0.680733945,-0.678899083,-0.67706422,-0.675229358,
-0.673394495,-0.671559633,-0.669724771,-0.667889908,-0.666055046,-0.664220183,
-0.662385321,-0.660550459,-0.658715596,-0.656880734,-0.655045872,-0.653211009,
-0.651376147,-0.649541284,-0.647706422,-0.64587156,-0.644036697,-0.642201835,
-0.640366972,-0.63853211,-0.636697248,-0.634862385,-0.633027523,-0.631192661,
-0.629357798,-0.627522936,-0.625688073,-0.623853211,-0.622018349,-0.620183486,
-0.618348624,-0.616513761,-0.614678899,-0.612844037,-0.611009174,-0.609174312,
-0.60733945,-0.605504587,-0.603669725,-0.601834862,-0.6,-0.598165138,-0.596330275,
-0.594495413,-0.59266055,-0.590825688,-0.588990826,-0.587155963,-0.585321101,
-0.583486239,-0.581651376,-0.579816514,-0.577981651,-0.576146789,-0.574311927,
-0.572477064,-0.570642202,-0.568807339,-0.566972477,-0.565137615,-0.563302752,
-0.56146789,-0.559633028,-0.557798165,-0.555963303,-0.55412844,-0.552293578,
-0.550458716,-0.548623853,-0.546788991,-0.544954128,-0.543119266,-0.541284404,
-0.539449541,-0.537614679,-0.535779817,-0.533944954,-0.532110092,-0.530275229,
-0.528440367,-0.526605505,-0.524770642,-0.52293578,-0.521100917,-0.519266055,
-0.517431193,-0.51559633,-0.513761468,-0.511926606,-0.510091743,-0.508256881,
-0.506422018,-0.504587156,-0.502752294,-0.500917431,-0.499082569,-0.497247706,
-0.495412844,-0.493577982,-0.491743119,-0.489908257,-0.488073394,-0.486238532,
-0.48440367,-0.482568807,-0.480733945,-0.478899083,-0.47706422,-0.475229358,
-0.473394495,-0.471559633,-0.469724771,-0.467889908,-0.466055046,-0.464220183,
-0.462385321,-0.460550459,-0.458715596,-0.456880734,-0.455045872,-0.453211009,
-0.451376147,-0.449541284,-0.447706422,-0.44587156,-0.444036697,-0.442201835,
-0.440366972,-0.43853211,-0.436697248,-0.434862385,-0.433027523,-0.431192661,
-0.429357798,-0.427522936,-0.425688073,-0.423853211,-0.422018349,-0.420183486,
-0.418348624,-0.416513761,-0.414678899,-0.412844037,-0.411009174,-0.409174312,
-0.40733945,-0.405504587,-0.403669725,-0.401834862,-0.4,-0.398165138,-0.396330275,
-0.394495413,-0.39266055,-0.390825688,-0.388990826,-0.387155963,-0.385321101,
-0.383486239,-0.381651376,-0.379816514,-0.377981651,-0.376146789,-0.374311927,
-0.372477064,-0.370642202,-0.368807339,-0.366972477,-0.365137615,-0.363302752,
-0.36146789,-0.359633028,-0.357798165,-0.355963303,-0.35412844,-0.352293578,
-0.350458716,-0.348623853,-0.346788991,-0.344954128,-0.343119266,-0.341284404,
-0.339449541,-0.337614679,-0.335779817,-0.333944954,-0.332110092,-0.330275229,
-0.328440367,-0.326605505,-0.324770642,-0.32293578,-0.321100917,-0.319266055,
-0.317431193,-0.31559633,-0.313761468,-0.311926606,-0.310091743,-0.308256881,
-0.306422018,-0.304587156,-0.302752294,-0.300917431,-0.299082569,-0.297247706,
-0.295412844,-0.293577982,-0.291743119,-0.289908257,-0.288073394,-0.286238532,
-0.28440367,-0.282568807,-0.280733945,-0.278899083,-0.27706422,-0.275229358,
-0.273394495,-0.271559633,-0.269724771,-0.267889908,-0.266055046,-0.264220183,
-0.262385321,-0.260550459,-0.258715596,-0.256880734,-0.255045872,-0.253211009,
-0.251376147,-0.249541284,-0.247706422,-0.24587156,-0.244036697,-0.242201835,
-0.240366972,-0.23853211,-0.236697248,-0.234862385,-0.233027523,-0.231192661,
-0.229357798,-0.227522936,-0.225688073,-0.223853211,-0.222018349,-0.220183486,
-0.218348624,-0.216513761,-0.214678899,-0.212844037,-0.211009174,-0.209174312,
-0.20733945,-0.205504587,-0.203669725,-0.201834862,-0.2,-0.198165138,-0.196330275,
-0.194495413,-0.19266055,-0.190825688,-0.188990826,-0.187155963,-0.185321101,
-0.183486239,-0.181651376,-0.179816514,-0.177981651,-0.176146789,-0.174311927,
-0.172477064,-0.170642202,-0.168807339,-0.166972477,-0.165137615,-0.163302752,
-0.16146789,-0.159633028,-0.157798165,-0.155963303,-0.15412844,-0.152293578,
-0.150458716,-0.148623853,-0.146788991,-0.144954128,-0.143119266,-0.141284404,
-0.139449541,-0.137614679,-0.135779817,-0.133944954,-0.132110092,-0.130275229,
-0.128440367,-0.126605505,-0.124770642,-0.12293578,-0.121100917,-0.119266055,
-0.117431193,-0.11559633,-0.113761468,-0.111926606,-0.110091743,-0.108256881,
-0.106422018,-0.104587156,-0.102752294,-0.100917431,-0.099082569,-0.097247706,
-0.095412844,-0.093577982,-0.091743119,-0.089908257,-0.088073394,-0.086238532,
-0.08440367,-0.082568807,-0.080733945,-0.078899083,-0.07706422,-0.075229358,
-0.073394495,-0.071559633,-0.069724771,-0.067889908,-0.066055046,-0.064220183,
-0.062385321,-0.060550459,-0.058715596,-0.056880734,-0.055045872,-0.053211009,
-0.051376147,-0.049541284,-0.047706422,-0.04587156,-0.044036697,-0.042201835,
-0.040366972,-0.03853211,-0.036697248,-0.034862385,-0.033027523,-0.031192661,
-0.029357798,-0.027522936,-0.025688073,-0.023853211,-0.022018349,-0.020183486,
-0.018348624,-0.016513761,-0.014678899,-0.012844037,-0.011009174,-0.009174312,
-0.00733945,-0.005504587,-0.003669725,-0.001834862,0.000982116),(0.3,1.,
1.3),.UNSPECIFIED.);
#6324=B_SPLINE_SURFACE_WITH_KNOTS('',5,1,((#336623,#336624,#336625),(#336626,
#336627,#336628),(#336629,#336630,#336631),(#336632,#336633,#336634),(#336635,
#336636,#336637),(#336638,#336639,#336640),(#336641,#336642,#336643),(#336644,
#336645,#336646),(#336647,#336648,#336649),(#336650,#336651,#336652),(#336653,
#336654,#336655),(#336656,#336657,#336658),(#336659,#336660,#336661),(#336662,
#336663,#336664),(#336665,#336666,#336667),(#336668,#336669,#336670),(#336671,
#336672,#336673),(#336674,#336675,#336676),(#336677,#336678,#336679),(#336680,
#336681,#336682),(#336683,#336684,#336685),(#336686,#336687,#336688),(#336689,
#336690,#336691),(#336692,#336693,#336694),(#336695,#336696,#336697),(#336698,
#336699,#336700),(#336701,#336702,#336703),(#336704,#336705,#336706),(#336707,
#336708,#336709),(#336710,#336711,#336712),(#336713,#336714,#336715),(#336716,
#336717,#336718),(#336719,#336720,#336721),(#336722,#336723,#336724),(#336725,
#336726,#336727),(#336728,#336729,#336730),(#336731,#336732,#336733),(#336734,
#336735,#336736),(#336737,#336738,#336739),(#336740,#336741,#336742),(#336743,
#336744,#336745),(#336746,#336747,#336748),(#336749,#336750,#336751),(#336752,
#336753,#336754),(#336755,#336756,#336757),(#336758,#336759,#336760),(#336761,
#336762,#336763),(#336764,#336765,#336766),(#336767,#336768,#336769),(#336770,
#336771,#336772),(#336773,#336774,#336775),(#336776,#336777,#336778),(#336779,
#336780,#336781),(#336782,#336783,#336784),(#336785,#336786,#336787),(#336788,
#336789,#336790),(#336791,#336792,#336793),(#336794,#336795,#336796),(#336797,
#336798,#336799),(#336800,#336801,#336802),(#336803,#336804,#336805),(#336806,
#336807,#336808),(#336809,#336810,#336811),(#336812,#336813,#336814),(#336815,
#336816,#336817),(#336818,#336819,#336820),(#336821,#336822,#336823),(#336824,
#336825,#336826),(#336827,#336828,#336829),(#336830,#336831,#336832),(#336833,
#336834,#336835),(#336836,#336837,#336838),(#336839,#336840,#336841),(#336842,
#336843,#336844),(#336845,#336846,#336847),(#336848,#336849,#336850),(#336851,
#336852,#336853),(#336854,#336855,#336856),(#336857,#336858,#336859),(#336860,
#336861,#336862),(#336863,#336864,#336865),(#336866,#336867,#336868),(#336869,
#336870,#336871),(#336872,#336873,#336874),(#336875,#336876,#336877),(#336878,
#336879,#336880),(#336881,#336882,#336883),(#336884,#336885,#336886),(#336887,
#336888,#336889),(#336890,#336891,#336892),(#336893,#336894,#336895),(#336896,
#336897,#336898),(#336899,#336900,#336901),(#336902,#336903,#336904),(#336905,
#336906,#336907),(#336908,#336909,#336910),(#336911,#336912,#336913),(#336914,
#336915,#336916),(#336917,#336918,#336919),(#336920,#336921,#336922),(#336923,
#336924,#336925),(#336926,#336927,#336928),(#336929,#336930,#336931),(#336932,
#336933,#336934),(#336935,#336936,#336937),(#336938,#336939,#336940),(#336941,
#336942,#336943),(#336944,#336945,#336946),(#336947,#336948,#336949),(#336950,
#336951,#336952),(#336953,#336954,#336955),(#336956,#336957,#336958),(#336959,
#336960,#336961),(#336962,#336963,#336964),(#336965,#336966,#336967),(#336968,
#336969,#336970),(#336971,#336972,#336973),(#336974,#336975,#336976),(#336977,
#336978,#336979),(#336980,#336981,#336982),(#336983,#336984,#336985),(#336986,
#336987,#336988),(#336989,#336990,#336991),(#336992,#336993,#336994),(#336995,
#336996,#336997),(#336998,#336999,#337000),(#337001,#337002,#337003),(#337004,
#337005,#337006),(#337007,#337008,#337009),(#337010,#337011,#337012),(#337013,
#337014,#337015),(#337016,#337017,#337018),(#337019,#337020,#337021),(#337022,
#337023,#337024),(#337025,#337026,#337027),(#337028,#337029,#337030),(#337031,
#337032,#337033),(#337034,#337035,#337036),(#337037,#337038,#337039),(#337040,
#337041,#337042),(#337043,#337044,#337045),(#337046,#337047,#337048),(#337049,
#337050,#337051),(#337052,#337053,#337054),(#337055,#337056,#337057),(#337058,
#337059,#337060),(#337061,#337062,#337063),(#337064,#337065,#337066),(#337067,
#337068,#337069),(#337070,#337071,#337072),(#337073,#337074,#337075),(#337076,
#337077,#337078),(#337079,#337080,#337081),(#337082,#337083,#337084),(#337085,
#337086,#337087),(#337088,#337089,#337090),(#337091,#337092,#337093),(#337094,
#337095,#337096),(#337097,#337098,#337099),(#337100,#337101,#337102),(#337103,
#337104,#337105),(#337106,#337107,#337108),(#337109,#337110,#337111),(#337112,
#337113,#337114),(#337115,#337116,#337117),(#337118,#337119,#337120),(#337121,
#337122,#337123),(#337124,#337125,#337126),(#337127,#337128,#337129),(#337130,
#337131,#337132),(#337133,#337134,#337135),(#337136,#337137,#337138),(#337139,
#337140,#337141),(#337142,#337143,#337144),(#337145,#337146,#337147),(#337148,
#337149,#337150),(#337151,#337152,#337153),(#337154,#337155,#337156),(#337157,
#337158,#337159),(#337160,#337161,#337162),(#337163,#337164,#337165),(#337166,
#337167,#337168),(#337169,#337170,#337171),(#337172,#337173,#337174),(#337175,
#337176,#337177),(#337178,#337179,#337180),(#337181,#337182,#337183),(#337184,
#337185,#337186),(#337187,#337188,#337189),(#337190,#337191,#337192),(#337193,
#337194,#337195),(#337196,#337197,#337198),(#337199,#337200,#337201),(#337202,
#337203,#337204),(#337205,#337206,#337207),(#337208,#337209,#337210),(#337211,
#337212,#337213),(#337214,#337215,#337216),(#337217,#337218,#337219),(#337220,
#337221,#337222),(#337223,#337224,#337225),(#337226,#337227,#337228),(#337229,
#337230,#337231),(#337232,#337233,#337234),(#337235,#337236,#337237),(#337238,
#337239,#337240),(#337241,#337242,#337243),(#337244,#337245,#337246),(#337247,
#337248,#337249),(#337250,#337251,#337252),(#337253,#337254,#337255),(#337256,
#337257,#337258),(#337259,#337260,#337261),(#337262,#337263,#337264),(#337265,
#337266,#337267),(#337268,#337269,#337270),(#337271,#337272,#337273),(#337274,
#337275,#337276),(#337277,#337278,#337279),(#337280,#337281,#337282),(#337283,
#337284,#337285),(#337286,#337287,#337288),(#337289,#337290,#337291),(#337292,
#337293,#337294),(#337295,#337296,#337297),(#337298,#337299,#337300),(#337301,
#337302,#337303),(#337304,#337305,#337306),(#337307,#337308,#337309),(#337310,
#337311,#337312),(#337313,#337314,#337315),(#337316,#337317,#337318),(#337319,
#337320,#337321),(#337322,#337323,#337324),(#337325,#337326,#337327),(#337328,
#337329,#337330),(#337331,#337332,#337333),(#337334,#337335,#337336),(#337337,
#337338,#337339),(#337340,#337341,#337342),(#337343,#337344,#337345),(#337346,
#337347,#337348),(#337349,#337350,#337351),(#337352,#337353,#337354),(#337355,
#337356,#337357),(#337358,#337359,#337360),(#337361,#337362,#337363),(#337364,
#337365,#337366),(#337367,#337368,#337369),(#337370,#337371,#337372),(#337373,
#337374,#337375),(#337376,#337377,#337378),(#337379,#337380,#337381),(#337382,
#337383,#337384),(#337385,#337386,#337387),(#337388,#337389,#337390),(#337391,
#337392,#337393),(#337394,#337395,#337396),(#337397,#337398,#337399),(#337400,
#337401,#337402),(#337403,#337404,#337405),(#337406,#337407,#337408),(#337409,
#337410,#337411),(#337412,#337413,#337414),(#337415,#337416,#337417),(#337418,
#337419,#337420),(#337421,#337422,#337423),(#337424,#337425,#337426),(#337427,
#337428,#337429),(#337430,#337431,#337432),(#337433,#337434,#337435),(#337436,
#337437,#337438),(#337439,#337440,#337441),(#337442,#337443,#337444),(#337445,
#337446,#337447),(#337448,#337449,#337450),(#337451,#337452,#337453),(#337454,
#337455,#337456),(#337457,#337458,#337459),(#337460,#337461,#337462),(#337463,
#337464,#337465),(#337466,#337467,#337468),(#337469,#337470,#337471),(#337472,
#337473,#337474),(#337475,#337476,#337477),(#337478,#337479,#337480),(#337481,
#337482,#337483),(#337484,#337485,#337486),(#337487,#337488,#337489),(#337490,
#337491,#337492),(#337493,#337494,#337495),(#337496,#337497,#337498),(#337499,
#337500,#337501),(#337502,#337503,#337504),(#337505,#337506,#337507),(#337508,
#337509,#337510),(#337511,#337512,#337513),(#337514,#337515,#337516),(#337517,
#337518,#337519),(#337520,#337521,#337522),(#337523,#337524,#337525),(#337526,
#337527,#337528),(#337529,#337530,#337531),(#337532,#337533,#337534),(#337535,
#337536,#337537),(#337538,#337539,#337540),(#337541,#337542,#337543),(#337544,
#337545,#337546),(#337547,#337548,#337549),(#337550,#337551,#337552),(#337553,
#337554,#337555),(#337556,#337557,#337558),(#337559,#337560,#337561),(#337562,
#337563,#337564),(#337565,#337566,#337567),(#337568,#337569,#337570),(#337571,
#337572,#337573),(#337574,#337575,#337576),(#337577,#337578,#337579),(#337580,
#337581,#337582),(#337583,#337584,#337585),(#337586,#337587,#337588),(#337589,
#337590,#337591),(#337592,#337593,#337594),(#337595,#337596,#337597),(#337598,
#337599,#337600),(#337601,#337602,#337603),(#337604,#337605,#337606),(#337607,
#337608,#337609),(#337610,#337611,#337612),(#337613,#337614,#337615),(#337616,
#337617,#337618),(#337619,#337620,#337621),(#337622,#337623,#337624),(#337625,
#337626,#337627),(#337628,#337629,#337630),(#337631,#337632,#337633),(#337634,
#337635,#337636),(#337637,#337638,#337639),(#337640,#337641,#337642),(#337643,
#337644,#337645),(#337646,#337647,#337648),(#337649,#337650,#337651),(#337652,
#337653,#337654),(#337655,#337656,#337657),(#337658,#337659,#337660),(#337661,
#337662,#337663),(#337664,#337665,#337666),(#337667,#337668,#337669),(#337670,
#337671,#337672),(#337673,#337674,#337675),(#337676,#337677,#337678),(#337679,
#337680,#337681),(#337682,#337683,#337684),(#337685,#337686,#337687),(#337688,
#337689,#337690),(#337691,#337692,#337693),(#337694,#337695,#337696),(#337697,
#337698,#337699),(#337700,#337701,#337702),(#337703,#337704,#337705),(#337706,
#337707,#337708),(#337709,#337710,#337711),(#337712,#337713,#337714),(#337715,
#337716,#337717),(#337718,#337719,#337720),(#337721,#337722,#337723),(#337724,
#337725,#337726),(#337727,#337728,#337729),(#337730,#337731,#337732),(#337733,
#337734,#337735),(#337736,#337737,#337738),(#337739,#337740,#337741),(#337742,
#337743,#337744),(#337745,#337746,#337747),(#337748,#337749,#337750),(#337751,
#337752,#337753),(#337754,#337755,#337756),(#337757,#337758,#337759),(#337760,
#337761,#337762),(#337763,#337764,#337765),(#337766,#337767,#337768),(#337769,
#337770,#337771),(#337772,#337773,#337774),(#337775,#337776,#337777),(#337778,
#337779,#337780),(#337781,#337782,#337783),(#337784,#337785,#337786),(#337787,
#337788,#337789),(#337790,#337791,#337792),(#337793,#337794,#337795),(#337796,
#337797,#337798),(#337799,#337800,#337801),(#337802,#337803,#337804),(#337805,
#337806,#337807),(#337808,#337809,#337810),(#337811,#337812,#337813),(#337814,
#337815,#337816),(#337817,#337818,#337819),(#337820,#337821,#337822),(#337823,
#337824,#337825),(#337826,#337827,#337828),(#337829,#337830,#337831),(#337832,
#337833,#337834),(#337835,#337836,#337837),(#337838,#337839,#337840),(#337841,
#337842,#337843),(#337844,#337845,#337846),(#337847,#337848,#337849),(#337850,
#337851,#337852),(#337853,#337854,#337855),(#337856,#337857,#337858),(#337859,
#337860,#337861),(#337862,#337863,#337864),(#337865,#337866,#337867),(#337868,
#337869,#337870),(#337871,#337872,#337873),(#337874,#337875,#337876),(#337877,
#337878,#337879),(#337880,#337881,#337882),(#337883,#337884,#337885),(#337886,
#337887,#337888),(#337889,#337890,#337891),(#337892,#337893,#337894),(#337895,
#337896,#337897),(#337898,#337899,#337900),(#337901,#337902,#337903),(#337904,
#337905,#337906),(#337907,#337908,#337909),(#337910,#337911,#337912),(#337913,
#337914,#337915),(#337916,#337917,#337918),(#337919,#337920,#337921),(#337922,
#337923,#337924),(#337925,#337926,#337927),(#337928,#337929,#337930),(#337931,
#337932,#337933),(#337934,#337935,#337936),(#337937,#337938,#337939),(#337940,
#337941,#337942),(#337943,#337944,#337945),(#337946,#337947,#337948),(#337949,
#337950,#337951),(#337952,#337953,#337954),(#337955,#337956,#337957),(#337958,
#337959,#337960),(#337961,#337962,#337963),(#337964,#337965,#337966),(#337967,
#337968,#337969),(#337970,#337971,#337972),(#337973,#337974,#337975),(#337976,
#337977,#337978),(#337979,#337980,#337981),(#337982,#337983,#337984),(#337985,
#337986,#337987),(#337988,#337989,#337990),(#337991,#337992,#337993),(#337994,
#337995,#337996),(#337997,#337998,#337999),(#338000,#338001,#338002),(#338003,
#338004,#338005),(#338006,#338007,#338008),(#338009,#338010,#338011),(#338012,
#338013,#338014),(#338015,#338016,#338017),(#338018,#338019,#338020),(#338021,
#338022,#338023),(#338024,#338025,#338026),(#338027,#338028,#338029),(#338030,
#338031,#338032),(#338033,#338034,#338035),(#338036,#338037,#338038),(#338039,
#338040,#338041),(#338042,#338043,#338044),(#338045,#338046,#338047),(#338048,
#338049,#338050),(#338051,#338052,#338053),(#338054,#338055,#338056),(#338057,
#338058,#338059),(#338060,#338061,#338062),(#338063,#338064,#338065),(#338066,
#338067,#338068),(#338069,#338070,#338071),(#338072,#338073,#338074),(#338075,
#338076,#338077),(#338078,#338079,#338080),(#338081,#338082,#338083),(#338084,
#338085,#338086),(#338087,#338088,#338089),(#338090,#338091,#338092),(#338093,
#338094,#338095),(#338096,#338097,#338098),(#338099,#338100,#338101),(#338102,
#338103,#338104),(#338105,#338106,#338107),(#338108,#338109,#338110),(#338111,
#338112,#338113),(#338114,#338115,#338116),(#338117,#338118,#338119),(#338120,
#338121,#338122),(#338123,#338124,#338125),(#338126,#338127,#338128),(#338129,
#338130,#338131),(#338132,#338133,#338134),(#338135,#338136,#338137),(#338138,
#338139,#338140),(#338141,#338142,#338143),(#338144,#338145,#338146),(#338147,
#338148,#338149),(#338150,#338151,#338152),(#338153,#338154,#338155),(#338156,
#338157,#338158),(#338159,#338160,#338161),(#338162,#338163,#338164),(#338165,
#338166,#338167),(#338168,#338169,#338170),(#338171,#338172,#338173),(#338174,
#338175,#338176),(#338177,#338178,#338179),(#338180,#338181,#338182),(#338183,
#338184,#338185),(#338186,#338187,#338188),(#338189,#338190,#338191),(#338192,
#338193,#338194),(#338195,#338196,#338197),(#338198,#338199,#338200),(#338201,
#338202,#338203),(#338204,#338205,#338206),(#338207,#338208,#338209),(#338210,
#338211,#338212),(#338213,#338214,#338215),(#338216,#338217,#338218),(#338219,
#338220,#338221),(#338222,#338223,#338224),(#338225,#338226,#338227),(#338228,
#338229,#338230),(#338231,#338232,#338233),(#338234,#338235,#338236),(#338237,
#338238,#338239),(#338240,#338241,#338242),(#338243,#338244,#338245),(#338246,
#338247,#338248),(#338249,#338250,#338251),(#338252,#338253,#338254),(#338255,
#338256,#338257),(#338258,#338259,#338260),(#338261,#338262,#338263),(#338264,
#338265,#338266),(#338267,#338268,#338269),(#338270,#338271,#338272),(#338273,
#338274,#338275)),.UNSPECIFIED.,.F.,.F.,.F.,(6,1,1,1,1,1,1,1,1,1,1,1,1,
1,1,1,1,1,1,1,1,1,1,1,1,1,1,1,1,1,1,1,1,1,1,1,1,1,1,1,1,1,1,1,1,1,1,1,1,
1,1,1,1,1,1,1,1,1,1,1,1,1,1,1,1,1,1,1,1,1,1,1,1,1,1,1,1,1,1,1,1,1,1,1,1,
1,1,1,1,1,1,1,1,1,1,1,1,1,1,1,1,1,1,1,1,1,1,1,1,1,1,1,1,1,1,1,1,1,1,1,1,
1,1,1,1,1,1,1,1,1,1,1,1,1,1,1,1,1,1,1,1,1,1,1,1,1,1,1,1,1,1,1,1,1,1,1,1,
1,1,1,1,1,1,1,1,1,1,1,1,1,1,1,1,1,1,1,1,1,1,1,1,1,1,1,1,1,1,1,1,1,1,1,1,
1,1,1,1,1,1,1,1,1,1,1,1,1,1,1,1,1,1,1,1,1,1,1,1,1,1,1,1,1,1,1,1,1,1,1,1,
1,1,1,1,1,1,1,1,1,1,1,1,1,1,1,1,1,1,1,1,1,1,1,1,1,1,1,1,1,1,1,1,1,1,1,1,
1,1,1,1,1,1,1,1,1,1,1,1,1,1,1,1,1,1,1,1,1,1,1,1,1,1,1,1,1,1,1,1,1,1,1,1,
1,1,1,1,1,1,1,1,1,1,1,1,1,1,1,1,1,1,1,1,1,1,1,1,1,1,1,1,1,1,1,1,1,1,1,1,
1,1,1,1,1,1,1,1,1,1,1,1,1,1,1,1,1,1,1,1,1,1,1,1,1,1,1,1,1,1,1,1,1,1,1,1,
1,1,1,1,1,1,1,1,1,1,1,1,1,1,1,1,1,1,1,1,1,1,1,1,1,1,1,1,1,1,1,1,1,1,1,1,
1,1,1,1,1,1,1,1,1,1,1,1,1,1,1,1,1,1,1,1,1,1,1,1,1,1,1,1,1,1,1,1,1,1,1,1,
1,1,1,1,1,1,1,1,1,1,1,1,1,1,1,1,1,1,1,1,1,1,1,1,1,1,1,1,1,1,1,1,1,1,1,1,
1,1,1,1,1,1,1,1,1,1,1,1,1,1,1,1,1,1,1,1,1,1,1,1,1,1,1,1,1,1,1,1,1,1,1,1,
1,1,1,1,1,1,1,1,1,1,1,1,1,1,1,1,1,1,1,1,1,1,1,1,1,1,1,1,1,6),(2,1,2),(-0.001964156,
0.,0.001834862,0.003669725,0.005504587,0.00733945,0.009174312,0.011009174,
0.012844037,0.014678899,0.016513761,0.018348624,0.020183486,0.022018349,
0.023853211,0.025688073,0.027522936,0.029357798,0.031192661,0.033027523,
0.034862385,0.036697248,0.03853211,0.040366972,0.042201835,0.044036697,
0.04587156,0.047706422,0.049541284,0.051376147,0.053211009,0.055045872,
0.056880734,0.058715596,0.060550459,0.062385321,0.064220183,0.066055046,
0.067889908,0.069724771,0.071559633,0.073394495,0.075229358,0.07706422,
0.078899083,0.080733945,0.082568807,0.08440367,0.086238532,0.088073394,
0.089908257,0.091743119,0.093577982,0.095412844,0.097247706,0.099082569,
0.100917431,0.102752294,0.104587156,0.106422018,0.108256881,0.110091743,
0.111926606,0.113761468,0.11559633,0.117431193,0.119266055,0.121100917,
0.12293578,0.124770642,0.126605505,0.128440367,0.130275229,0.132110092,
0.133944954,0.135779817,0.137614679,0.139449541,0.141284404,0.143119266,
0.144954128,0.146788991,0.148623853,0.150458716,0.152293578,0.15412844,
0.155963303,0.157798165,0.159633028,0.16146789,0.163302752,0.165137615,
0.166972477,0.168807339,0.170642202,0.172477064,0.174311927,0.176146789,
0.177981651,0.179816514,0.181651376,0.183486239,0.185321101,0.187155963,
0.188990826,0.190825688,0.19266055,0.194495413,0.196330275,0.198165138,
0.2,0.201834862,0.203669725,0.205504587,0.20733945,0.209174312,0.211009174,
0.212844037,0.214678899,0.216513761,0.218348624,0.220183486,0.222018349,
0.223853211,0.225688073,0.227522936,0.229357798,0.231192661,0.233027523,
0.234862385,0.236697248,0.23853211,0.240366972,0.242201835,0.244036697,
0.24587156,0.247706422,0.249541284,0.251376147,0.253211009,0.255045872,
0.256880734,0.258715596,0.260550459,0.262385321,0.264220183,0.266055046,
0.267889908,0.269724771,0.271559633,0.273394495,0.275229358,0.27706422,
0.278899083,0.280733945,0.282568807,0.28440367,0.286238532,0.288073394,
0.289908257,0.291743119,0.293577982,0.295412844,0.297247706,0.299082569,
0.300917431,0.302752294,0.304587156,0.306422018,0.308256881,0.310091743,
0.311926606,0.313761468,0.31559633,0.317431193,0.319266055,0.321100917,
0.32293578,0.324770642,0.326605505,0.328440367,0.330275229,0.332110092,
0.333944954,0.335779817,0.337614679,0.339449541,0.341284404,0.343119266,
0.344954128,0.346788991,0.348623853,0.350458716,0.352293578,0.35412844,
0.355963303,0.357798165,0.359633028,0.36146789,0.363302752,0.365137615,
0.366972477,0.368807339,0.370642202,0.372477064,0.374311927,0.376146789,
0.377981651,0.379816514,0.381651376,0.383486239,0.385321101,0.387155963,
0.388990826,0.390825688,0.39266055,0.394495413,0.396330275,0.398165138,
0.4,0.401834862,0.403669725,0.405504587,0.40733945,0.409174312,0.411009174,
0.412844037,0.414678899,0.416513761,0.418348624,0.420183486,0.422018349,
0.423853211,0.425688073,0.427522936,0.429357798,0.431192661,0.433027523,
0.434862385,0.436697248,0.43853211,0.440366972,0.442201835,0.444036697,
0.44587156,0.447706422,0.449541284,0.451376147,0.453211009,0.455045872,
0.456880734,0.458715596,0.460550459,0.462385321,0.464220183,0.466055046,
0.467889908,0.469724771,0.471559633,0.473394495,0.475229358,0.47706422,
0.478899083,0.480733945,0.482568807,0.48440367,0.486238532,0.488073394,
0.489908257,0.491743119,0.493577982,0.495412844,0.497247706,0.499082569,
0.500917431,0.502752294,0.504587156,0.506422018,0.508256881,0.510091743,
0.511926606,0.513761468,0.51559633,0.517431193,0.519266055,0.521100917,
0.52293578,0.524770642,0.526605505,0.528440367,0.530275229,0.532110092,
0.533944954,0.535779817,0.537614679,0.539449541,0.541284404,0.543119266,
0.544954128,0.546788991,0.548623853,0.550458716,0.552293578,0.55412844,
0.555963303,0.557798165,0.559633028,0.56146789,0.563302752,0.565137615,
0.566972477,0.568807339,0.570642202,0.572477064,0.574311927,0.576146789,
0.577981651,0.579816514,0.581651376,0.583486239,0.585321101,0.587155963,
0.588990826,0.590825688,0.59266055,0.594495413,0.596330275,0.598165138,
0.6,0.601834862,0.603669725,0.605504587,0.60733945,0.609174312,0.611009174,
0.612844037,0.614678899,0.616513761,0.618348624,0.620183486,0.622018349,
0.623853211,0.625688073,0.627522936,0.629357798,0.631192661,0.633027523,
0.634862385,0.636697248,0.63853211,0.640366972,0.642201835,0.644036697,
0.64587156,0.647706422,0.649541284,0.651376147,0.653211009,0.655045872,
0.656880734,0.658715596,0.660550459,0.662385321,0.664220183,0.666055046,
0.667889908,0.669724771,0.671559633,0.673394495,0.675229358,0.67706422,
0.678899083,0.680733945,0.682568807,0.68440367,0.686238532,0.688073394,
0.689908257,0.691743119,0.693577982,0.695412844,0.697247706,0.699082569,
0.700917431,0.702752294,0.704587156,0.706422018,0.708256881,0.710091743,
0.711926606,0.713761468,0.71559633,0.717431193,0.719266055,0.721100917,
0.72293578,0.724770642,0.726605505,0.728440367,0.730275229,0.732110092,
0.733944954,0.735779817,0.737614679,0.739449541,0.741284404,0.743119266,
0.744954128,0.746788991,0.748623853,0.750458716,0.752293578,0.75412844,
0.755963303,0.757798165,0.759633028,0.76146789,0.763302752,0.765137615,
0.766972477,0.768807339,0.770642202,0.772477064,0.774311927,0.776146789,
0.777981651,0.779816514,0.781651376,0.783486239,0.785321101,0.787155963,
0.788990826,0.790825688,0.79266055,0.794495413,0.796330275,0.798165138,
0.8,0.801834862,0.803669725,0.805504587,0.80733945,0.809174312,0.811009174,
0.812844037,0.814678899,0.816513761,0.818348624,0.820183486,0.822018349,
0.823853211,0.825688073,0.827522936,0.829357798,0.831192661,0.833027523,
0.834862385,0.836697248,0.83853211,0.840366972,0.842201835,0.844036697,
0.84587156,0.847706422,0.849541284,0.851376147,0.853211009,0.855045872,
0.856880734,0.858715596,0.860550459,0.862385321,0.864220183,0.866055046,
0.867889908,0.869724771,0.871559633,0.873394495,0.875229358,0.87706422,
0.878899083,0.880733945,0.882568807,0.88440367,0.886238532,0.888073394,
0.889908257,0.891743119,0.893577982,0.895412844,0.897247706,0.899082569,
0.900917431,0.902752294,0.904587156,0.906422018,0.908256881,0.910091743,
0.911926606,0.913761468,0.91559633,0.917431193,0.919266055,0.921100917,
0.92293578,0.924770642,0.926605505,0.928440367,0.930275229,0.932110092,
0.933944954,0.935779817,0.937614679,0.939449541,0.941284404,0.943119266,
0.944954128,0.946788991,0.948623853,0.950458716,0.952293578,0.95412844,
0.955963303,0.957798165,0.959633028,0.96146789,0.963302752,0.965137615,
0.966972477,0.968807339,0.970642202,0.972477064,0.974311927,0.976146789,
0.977981651,0.979816514,0.981651376,0.983486239,0.985321101,0.987155963,
0.988990826,0.990825688,0.99266055,0.994495413,0.996330275,0.998165138,
1.000000000264),(0.3,1.,1.3),.UNSPECIFIED.);
#6325=B_SPLINE_SURFACE_WITH_KNOTS('',5,1,((#338282,#338283,#338284),(#338285,
#338286,#338287),(#338288,#338289,#338290),(#338291,#338292,#338293),(#338294,
#338295,#338296),(#338297,#338298,#338299),(#338300,#338301,#338302),(#338303,
#338304,#338305),(#338306,#338307,#338308),(#338309,#338310,#338311),(#338312,
#338313,#338314),(#338315,#338316,#338317),(#338318,#338319,#338320),(#338321,
#338322,#338323),(#338324,#338325,#338326),(#338327,#338328,#338329),(#338330,
#338331,#338332),(#338333,#338334,#338335),(#338336,#338337,#338338),(#338339,
#338340,#338341),(#338342,#338343,#338344),(#338345,#338346,#338347),(#338348,
#338349,#338350),(#338351,#338352,#338353),(#338354,#338355,#338356),(#338357,
#338358,#338359),(#338360,#338361,#338362),(#338363,#338364,#338365),(#338366,
#338367,#338368),(#338369,#338370,#338371),(#338372,#338373,#338374),(#338375,
#338376,#338377),(#338378,#338379,#338380),(#338381,#338382,#338383),(#338384,
#338385,#338386),(#338387,#338388,#338389),(#338390,#338391,#338392),(#338393,
#338394,#338395),(#338396,#338397,#338398),(#338399,#338400,#338401),(#338402,
#338403,#338404),(#338405,#338406,#338407),(#338408,#338409,#338410),(#338411,
#338412,#338413),(#338414,#338415,#338416),(#338417,#338418,#338419),(#338420,
#338421,#338422),(#338423,#338424,#338425),(#338426,#338427,#338428),(#338429,
#338430,#338431),(#338432,#338433,#338434),(#338435,#338436,#338437),(#338438,
#338439,#338440),(#338441,#338442,#338443),(#338444,#338445,#338446),(#338447,
#338448,#338449),(#338450,#338451,#338452),(#338453,#338454,#338455),(#338456,
#338457,#338458),(#338459,#338460,#338461),(#338462,#338463,#338464),(#338465,
#338466,#338467),(#338468,#338469,#338470),(#338471,#338472,#338473),(#338474,
#338475,#338476),(#338477,#338478,#338479),(#338480,#338481,#338482),(#338483,
#338484,#338485),(#338486,#338487,#338488),(#338489,#338490,#338491),(#338492,
#338493,#338494),(#338495,#338496,#338497),(#338498,#338499,#338500),(#338501,
#338502,#338503),(#338504,#338505,#338506),(#338507,#338508,#338509),(#338510,
#338511,#338512),(#338513,#338514,#338515),(#338516,#338517,#338518),(#338519,
#338520,#338521),(#338522,#338523,#338524),(#338525,#338526,#338527),(#338528,
#338529,#338530),(#338531,#338532,#338533),(#338534,#338535,#338536),(#338537,
#338538,#338539),(#338540,#338541,#338542),(#338543,#338544,#338545),(#338546,
#338547,#338548),(#338549,#338550,#338551),(#338552,#338553,#338554),(#338555,
#338556,#338557),(#338558,#338559,#338560),(#338561,#338562,#338563),(#338564,
#338565,#338566),(#338567,#338568,#338569),(#338570,#338571,#338572),(#338573,
#338574,#338575),(#338576,#338577,#338578),(#338579,#338580,#338581),(#338582,
#338583,#338584),(#338585,#338586,#338587),(#338588,#338589,#338590),(#338591,
#338592,#338593),(#338594,#338595,#338596),(#338597,#338598,#338599),(#338600,
#338601,#338602),(#338603,#338604,#338605),(#338606,#338607,#338608),(#338609,
#338610,#338611),(#338612,#338613,#338614),(#338615,#338616,#338617),(#338618,
#338619,#338620),(#338621,#338622,#338623),(#338624,#338625,#338626),(#338627,
#338628,#338629),(#338630,#338631,#338632),(#338633,#338634,#338635),(#338636,
#338637,#338638),(#338639,#338640,#338641),(#338642,#338643,#338644),(#338645,
#338646,#338647),(#338648,#338649,#338650),(#338651,#338652,#338653),(#338654,
#338655,#338656),(#338657,#338658,#338659),(#338660,#338661,#338662),(#338663,
#338664,#338665),(#338666,#338667,#338668),(#338669,#338670,#338671),(#338672,
#338673,#338674),(#338675,#338676,#338677),(#338678,#338679,#338680),(#338681,
#338682,#338683),(#338684,#338685,#338686),(#338687,#338688,#338689),(#338690,
#338691,#338692),(#338693,#338694,#338695),(#338696,#338697,#338698),(#338699,
#338700,#338701),(#338702,#338703,#338704),(#338705,#338706,#338707),(#338708,
#338709,#338710),(#338711,#338712,#338713),(#338714,#338715,#338716),(#338717,
#338718,#338719),(#338720,#338721,#338722),(#338723,#338724,#338725),(#338726,
#338727,#338728),(#338729,#338730,#338731),(#338732,#338733,#338734),(#338735,
#338736,#338737),(#338738,#338739,#338740),(#338741,#338742,#338743),(#338744,
#338745,#338746),(#338747,#338748,#338749),(#338750,#338751,#338752),(#338753,
#338754,#338755),(#338756,#338757,#338758),(#338759,#338760,#338761),(#338762,
#338763,#338764),(#338765,#338766,#338767),(#338768,#338769,#338770),(#338771,
#338772,#338773),(#338774,#338775,#338776),(#338777,#338778,#338779),(#338780,
#338781,#338782),(#338783,#338784,#338785),(#338786,#338787,#338788),(#338789,
#338790,#338791),(#338792,#338793,#338794),(#338795,#338796,#338797),(#338798,
#338799,#338800),(#338801,#338802,#338803),(#338804,#338805,#338806),(#338807,
#338808,#338809),(#338810,#338811,#338812),(#338813,#338814,#338815),(#338816,
#338817,#338818),(#338819,#338820,#338821),(#338822,#338823,#338824),(#338825,
#338826,#338827),(#338828,#338829,#338830),(#338831,#338832,#338833),(#338834,
#338835,#338836),(#338837,#338838,#338839),(#338840,#338841,#338842),(#338843,
#338844,#338845),(#338846,#338847,#338848),(#338849,#338850,#338851),(#338852,
#338853,#338854),(#338855,#338856,#338857),(#338858,#338859,#338860),(#338861,
#338862,#338863),(#338864,#338865,#338866),(#338867,#338868,#338869),(#338870,
#338871,#338872),(#338873,#338874,#338875),(#338876,#338877,#338878),(#338879,
#338880,#338881),(#338882,#338883,#338884),(#338885,#338886,#338887),(#338888,
#338889,#338890),(#338891,#338892,#338893),(#338894,#338895,#338896),(#338897,
#338898,#338899),(#338900,#338901,#338902),(#338903,#338904,#338905),(#338906,
#338907,#338908),(#338909,#338910,#338911),(#338912,#338913,#338914),(#338915,
#338916,#338917),(#338918,#338919,#338920),(#338921,#338922,#338923),(#338924,
#338925,#338926),(#338927,#338928,#338929),(#338930,#338931,#338932),(#338933,
#338934,#338935),(#338936,#338937,#338938),(#338939,#338940,#338941),(#338942,
#338943,#338944),(#338945,#338946,#338947),(#338948,#338949,#338950),(#338951,
#338952,#338953),(#338954,#338955,#338956),(#338957,#338958,#338959),(#338960,
#338961,#338962),(#338963,#338964,#338965),(#338966,#338967,#338968),(#338969,
#338970,#338971),(#338972,#338973,#338974),(#338975,#338976,#338977),(#338978,
#338979,#338980),(#338981,#338982,#338983),(#338984,#338985,#338986),(#338987,
#338988,#338989),(#338990,#338991,#338992),(#338993,#338994,#338995),(#338996,
#338997,#338998),(#338999,#339000,#339001),(#339002,#339003,#339004),(#339005,
#339006,#339007),(#339008,#339009,#339010),(#339011,#339012,#339013),(#339014,
#339015,#339016),(#339017,#339018,#339019),(#339020,#339021,#339022),(#339023,
#339024,#339025),(#339026,#339027,#339028),(#339029,#339030,#339031),(#339032,
#339033,#339034),(#339035,#339036,#339037),(#339038,#339039,#339040),(#339041,
#339042,#339043),(#339044,#339045,#339046),(#339047,#339048,#339049),(#339050,
#339051,#339052),(#339053,#339054,#339055),(#339056,#339057,#339058),(#339059,
#339060,#339061),(#339062,#339063,#339064),(#339065,#339066,#339067),(#339068,
#339069,#339070),(#339071,#339072,#339073),(#339074,#339075,#339076),(#339077,
#339078,#339079),(#339080,#339081,#339082),(#339083,#339084,#339085),(#339086,
#339087,#339088),(#339089,#339090,#339091),(#339092,#339093,#339094),(#339095,
#339096,#339097),(#339098,#339099,#339100),(#339101,#339102,#339103),(#339104,
#339105,#339106),(#339107,#339108,#339109),(#339110,#339111,#339112),(#339113,
#339114,#339115),(#339116,#339117,#339118),(#339119,#339120,#339121),(#339122,
#339123,#339124),(#339125,#339126,#339127),(#339128,#339129,#339130),(#339131,
#339132,#339133),(#339134,#339135,#339136),(#339137,#339138,#339139),(#339140,
#339141,#339142),(#339143,#339144,#339145),(#339146,#339147,#339148),(#339149,
#339150,#339151),(#339152,#339153,#339154),(#339155,#339156,#339157),(#339158,
#339159,#339160),(#339161,#339162,#339163),(#339164,#339165,#339166),(#339167,
#339168,#339169),(#339170,#339171,#339172),(#339173,#339174,#339175),(#339176,
#339177,#339178),(#339179,#339180,#339181),(#339182,#339183,#339184),(#339185,
#339186,#339187),(#339188,#339189,#339190),(#339191,#339192,#339193),(#339194,
#339195,#339196),(#339197,#339198,#339199),(#339200,#339201,#339202),(#339203,
#339204,#339205),(#339206,#339207,#339208),(#339209,#339210,#339211),(#339212,
#339213,#339214),(#339215,#339216,#339217),(#339218,#339219,#339220),(#339221,
#339222,#339223),(#339224,#339225,#339226),(#339227,#339228,#339229),(#339230,
#339231,#339232),(#339233,#339234,#339235),(#339236,#339237,#339238),(#339239,
#339240,#339241),(#339242,#339243,#339244),(#339245,#339246,#339247),(#339248,
#339249,#339250),(#339251,#339252,#339253),(#339254,#339255,#339256),(#339257,
#339258,#339259),(#339260,#339261,#339262),(#339263,#339264,#339265),(#339266,
#339267,#339268),(#339269,#339270,#339271),(#339272,#339273,#339274),(#339275,
#339276,#339277),(#339278,#339279,#339280),(#339281,#339282,#339283),(#339284,
#339285,#339286),(#339287,#339288,#339289),(#339290,#339291,#339292),(#339293,
#339294,#339295),(#339296,#339297,#339298),(#339299,#339300,#339301),(#339302,
#339303,#339304),(#339305,#339306,#339307),(#339308,#339309,#339310),(#339311,
#339312,#339313),(#339314,#339315,#339316),(#339317,#339318,#339319),(#339320,
#339321,#339322),(#339323,#339324,#339325),(#339326,#339327,#339328),(#339329,
#339330,#339331),(#339332,#339333,#339334),(#339335,#339336,#339337),(#339338,
#339339,#339340),(#339341,#339342,#339343),(#339344,#339345,#339346),(#339347,
#339348,#339349),(#339350,#339351,#339352),(#339353,#339354,#339355),(#339356,
#339357,#339358),(#339359,#339360,#339361),(#339362,#339363,#339364),(#339365,
#339366,#339367),(#339368,#339369,#339370),(#339371,#339372,#339373),(#339374,
#339375,#339376),(#339377,#339378,#339379),(#339380,#339381,#339382),(#339383,
#339384,#339385),(#339386,#339387,#339388),(#339389,#339390,#339391),(#339392,
#339393,#339394),(#339395,#339396,#339397),(#339398,#339399,#339400),(#339401,
#339402,#339403),(#339404,#339405,#339406),(#339407,#339408,#339409),(#339410,
#339411,#339412),(#339413,#339414,#339415),(#339416,#339417,#339418),(#339419,
#339420,#339421),(#339422,#339423,#339424),(#339425,#339426,#339427),(#339428,
#339429,#339430),(#339431,#339432,#339433),(#339434,#339435,#339436),(#339437,
#339438,#339439),(#339440,#339441,#339442),(#339443,#339444,#339445),(#339446,
#339447,#339448),(#339449,#339450,#339451),(#339452,#339453,#339454),(#339455,
#339456,#339457),(#339458,#339459,#339460),(#339461,#339462,#339463),(#339464,
#339465,#339466),(#339467,#339468,#339469),(#339470,#339471,#339472),(#339473,
#339474,#339475),(#339476,#339477,#339478),(#339479,#339480,#339481),(#339482,
#339483,#339484),(#339485,#339486,#339487),(#339488,#339489,#339490),(#339491,
#339492,#339493),(#339494,#339495,#339496),(#339497,#339498,#339499),(#339500,
#339501,#339502),(#339503,#339504,#339505),(#339506,#339507,#339508),(#339509,
#339510,#339511),(#339512,#339513,#339514),(#339515,#339516,#339517),(#339518,
#339519,#339520),(#339521,#339522,#339523),(#339524,#339525,#339526),(#339527,
#339528,#339529),(#339530,#339531,#339532),(#339533,#339534,#339535),(#339536,
#339537,#339538),(#339539,#339540,#339541),(#339542,#339543,#339544),(#339545,
#339546,#339547),(#339548,#339549,#339550),(#339551,#339552,#339553),(#339554,
#339555,#339556),(#339557,#339558,#339559),(#339560,#339561,#339562),(#339563,
#339564,#339565),(#339566,#339567,#339568),(#339569,#339570,#339571),(#339572,
#339573,#339574),(#339575,#339576,#339577),(#339578,#339579,#339580),(#339581,
#339582,#339583),(#339584,#339585,#339586),(#339587,#339588,#339589),(#339590,
#339591,#339592),(#339593,#339594,#339595),(#339596,#339597,#339598),(#339599,
#339600,#339601),(#339602,#339603,#339604),(#339605,#339606,#339607),(#339608,
#339609,#339610),(#339611,#339612,#339613),(#339614,#339615,#339616),(#339617,
#339618,#339619),(#339620,#339621,#339622),(#339623,#339624,#339625),(#339626,
#339627,#339628),(#339629,#339630,#339631),(#339632,#339633,#339634),(#339635,
#339636,#339637),(#339638,#339639,#339640),(#339641,#339642,#339643),(#339644,
#339645,#339646),(#339647,#339648,#339649),(#339650,#339651,#339652),(#339653,
#339654,#339655),(#339656,#339657,#339658),(#339659,#339660,#339661),(#339662,
#339663,#339664),(#339665,#339666,#339667),(#339668,#339669,#339670),(#339671,
#339672,#339673),(#339674,#339675,#339676),(#339677,#339678,#339679),(#339680,
#339681,#339682),(#339683,#339684,#339685),(#339686,#339687,#339688),(#339689,
#339690,#339691),(#339692,#339693,#339694),(#339695,#339696,#339697),(#339698,
#339699,#339700),(#339701,#339702,#339703),(#339704,#339705,#339706),(#339707,
#339708,#339709),(#339710,#339711,#339712),(#339713,#339714,#339715),(#339716,
#339717,#339718),(#339719,#339720,#339721),(#339722,#339723,#339724),(#339725,
#339726,#339727),(#339728,#339729,#339730),(#339731,#339732,#339733),(#339734,
#339735,#339736),(#339737,#339738,#339739),(#339740,#339741,#339742),(#339743,
#339744,#339745),(#339746,#339747,#339748),(#339749,#339750,#339751),(#339752,
#339753,#339754),(#339755,#339756,#339757),(#339758,#339759,#339760),(#339761,
#339762,#339763),(#339764,#339765,#339766),(#339767,#339768,#339769),(#339770,
#339771,#339772),(#339773,#339774,#339775),(#339776,#339777,#339778),(#339779,
#339780,#339781),(#339782,#339783,#339784),(#339785,#339786,#339787),(#339788,
#339789,#339790),(#339791,#339792,#339793),(#339794,#339795,#339796),(#339797,
#339798,#339799),(#339800,#339801,#339802),(#339803,#339804,#339805),(#339806,
#339807,#339808),(#339809,#339810,#339811),(#339812,#339813,#339814),(#339815,
#339816,#339817),(#339818,#339819,#339820),(#339821,#339822,#339823),(#339824,
#339825,#339826),(#339827,#339828,#339829),(#339830,#339831,#339832),(#339833,
#339834,#339835),(#339836,#339837,#339838),(#339839,#339840,#339841),(#339842,
#339843,#339844),(#339845,#339846,#339847),(#339848,#339849,#339850),(#339851,
#339852,#339853),(#339854,#339855,#339856),(#339857,#339858,#339859),(#339860,
#339861,#339862),(#339863,#339864,#339865),(#339866,#339867,#339868),(#339869,
#339870,#339871),(#339872,#339873,#339874),(#339875,#339876,#339877),(#339878,
#339879,#339880),(#339881,#339882,#339883),(#339884,#339885,#339886),(#339887,
#339888,#339889),(#339890,#339891,#339892),(#339893,#339894,#339895),(#339896,
#339897,#339898),(#339899,#339900,#339901),(#339902,#339903,#339904),(#339905,
#339906,#339907),(#339908,#339909,#339910),(#339911,#339912,#339913),(#339914,
#339915,#339916),(#339917,#339918,#339919),(#339920,#339921,#339922),(#339923,
#339924,#339925),(#339926,#339927,#339928),(#339929,#339930,#339931)),
 .UNSPECIFIED.,.F.,.F.,.F.,(6,1,1,1,1,1,1,1,1,1,1,1,1,1,1,1,1,1,1,1,1,1,
1,1,1,1,1,1,1,1,1,1,1,1,1,1,1,1,1,1,1,1,1,1,1,1,1,1,1,1,1,1,1,1,1,1,1,1,
1,1,1,1,1,1,1,1,1,1,1,1,1,1,1,1,1,1,1,1,1,1,1,1,1,1,1,1,1,1,1,1,1,1,1,1,
1,1,1,1,1,1,1,1,1,1,1,1,1,1,1,1,1,1,1,1,1,1,1,1,1,1,1,1,1,1,1,1,1,1,1,1,
1,1,1,1,1,1,1,1,1,1,1,1,1,1,1,1,1,1,1,1,1,1,1,1,1,1,1,1,1,1,1,1,1,1,1,1,
1,1,1,1,1,1,1,1,1,1,1,1,1,1,1,1,1,1,1,1,1,1,1,1,1,1,1,1,1,1,1,1,1,1,1,1,
1,1,1,1,1,1,1,1,1,1,1,1,1,1,1,1,1,1,1,1,1,1,1,1,1,1,1,1,1,1,1,1,1,1,1,1,
1,1,1,1,1,1,1,1,1,1,1,1,1,1,1,1,1,1,1,1,1,1,1,1,1,1,1,1,1,1,1,1,1,1,1,1,
1,1,1,1,1,1,1,1,1,1,1,1,1,1,1,1,1,1,1,1,1,1,1,1,1,1,1,1,1,1,1,1,1,1,1,1,
1,1,1,1,1,1,1,1,1,1,1,1,1,1,1,1,1,1,1,1,1,1,1,1,1,1,1,1,1,1,1,1,1,1,1,1,
1,1,1,1,1,1,1,1,1,1,1,1,1,1,1,1,1,1,1,1,1,1,1,1,1,1,1,1,1,1,1,1,1,1,1,1,
1,1,1,1,1,1,1,1,1,1,1,1,1,1,1,1,1,1,1,1,1,1,1,1,1,1,1,1,1,1,1,1,1,1,1,1,
1,1,1,1,1,1,1,1,1,1,1,1,1,1,1,1,1,1,1,1,1,1,1,1,1,1,1,1,1,1,1,1,1,1,1,1,
1,1,1,1,1,1,1,1,1,1,1,1,1,1,1,1,1,1,1,1,1,1,1,1,1,1,1,1,1,1,1,1,1,1,1,1,
1,1,1,1,1,1,1,1,1,1,1,1,1,1,1,1,1,1,1,1,1,1,1,1,1,1,1,1,1,1,1,1,1,1,1,1,
1,1,1,1,1,1,1,1,1,1,1,1,1,1,1,1,1,1,1,6),(2,1,2),(-1.,-0.998165138,-0.996330275,
-0.994495413,-0.99266055,-0.990825688,-0.988990826,-0.987155963,-0.985321101,
-0.983486239,-0.981651376,-0.979816514,-0.977981651,-0.976146789,-0.974311927,
-0.972477064,-0.970642202,-0.968807339,-0.966972477,-0.965137615,-0.963302752,
-0.96146789,-0.959633028,-0.957798165,-0.955963303,-0.95412844,-0.952293578,
-0.950458716,-0.948623853,-0.946788991,-0.944954128,-0.943119266,-0.941284404,
-0.939449541,-0.937614679,-0.935779817,-0.933944954,-0.932110092,-0.930275229,
-0.928440367,-0.926605505,-0.924770642,-0.92293578,-0.921100917,-0.919266055,
-0.917431193,-0.91559633,-0.913761468,-0.911926606,-0.910091743,-0.908256881,
-0.906422018,-0.904587156,-0.902752294,-0.900917431,-0.899082569,-0.897247706,
-0.895412844,-0.893577982,-0.891743119,-0.889908257,-0.888073394,-0.886238532,
-0.88440367,-0.882568807,-0.880733945,-0.878899083,-0.87706422,-0.875229358,
-0.873394495,-0.871559633,-0.869724771,-0.867889908,-0.866055046,-0.864220183,
-0.862385321,-0.860550459,-0.858715596,-0.856880734,-0.855045872,-0.853211009,
-0.851376147,-0.849541284,-0.847706422,-0.84587156,-0.844036697,-0.842201835,
-0.840366972,-0.83853211,-0.836697248,-0.834862385,-0.833027523,-0.831192661,
-0.829357798,-0.827522936,-0.825688073,-0.823853211,-0.822018349,-0.820183486,
-0.818348624,-0.816513761,-0.814678899,-0.812844037,-0.811009174,-0.809174312,
-0.80733945,-0.805504587,-0.803669725,-0.801834862,-0.8,-0.798165138,-0.796330275,
-0.794495413,-0.79266055,-0.790825688,-0.788990826,-0.787155963,-0.785321101,
-0.783486239,-0.781651376,-0.779816514,-0.777981651,-0.776146789,-0.774311927,
-0.772477064,-0.770642202,-0.768807339,-0.766972477,-0.765137615,-0.763302752,
-0.76146789,-0.759633028,-0.757798165,-0.755963303,-0.75412844,-0.752293578,
-0.750458716,-0.748623853,-0.746788991,-0.744954128,-0.743119266,-0.741284404,
-0.739449541,-0.737614679,-0.735779817,-0.733944954,-0.732110092,-0.730275229,
-0.728440367,-0.726605505,-0.724770642,-0.72293578,-0.721100917,-0.719266055,
-0.717431193,-0.71559633,-0.713761468,-0.711926606,-0.710091743,-0.708256881,
-0.706422018,-0.704587156,-0.702752294,-0.700917431,-0.699082569,-0.697247706,
-0.695412844,-0.693577982,-0.691743119,-0.689908257,-0.688073394,-0.686238532,
-0.68440367,-0.682568807,-0.680733945,-0.678899083,-0.67706422,-0.675229358,
-0.673394495,-0.671559633,-0.669724771,-0.667889908,-0.666055046,-0.664220183,
-0.662385321,-0.660550459,-0.658715596,-0.656880734,-0.655045872,-0.653211009,
-0.651376147,-0.649541284,-0.647706422,-0.64587156,-0.644036697,-0.642201835,
-0.640366972,-0.63853211,-0.636697248,-0.634862385,-0.633027523,-0.631192661,
-0.629357798,-0.627522936,-0.625688073,-0.623853211,-0.622018349,-0.620183486,
-0.618348624,-0.616513761,-0.614678899,-0.612844037,-0.611009174,-0.609174312,
-0.60733945,-0.605504587,-0.603669725,-0.601834862,-0.6,-0.598165138,-0.596330275,
-0.594495413,-0.59266055,-0.590825688,-0.588990826,-0.587155963,-0.585321101,
-0.583486239,-0.581651376,-0.579816514,-0.577981651,-0.576146789,-0.574311927,
-0.572477064,-0.570642202,-0.568807339,-0.566972477,-0.565137615,-0.563302752,
-0.56146789,-0.559633028,-0.557798165,-0.555963303,-0.55412844,-0.552293578,
-0.550458716,-0.548623853,-0.546788991,-0.544954128,-0.543119266,-0.541284404,
-0.539449541,-0.537614679,-0.535779817,-0.533944954,-0.532110092,-0.530275229,
-0.528440367,-0.526605505,-0.524770642,-0.52293578,-0.521100917,-0.519266055,
-0.517431193,-0.51559633,-0.513761468,-0.511926606,-0.510091743,-0.508256881,
-0.506422018,-0.504587156,-0.502752294,-0.500917431,-0.499082569,-0.497247706,
-0.495412844,-0.493577982,-0.491743119,-0.489908257,-0.488073394,-0.486238532,
-0.48440367,-0.482568807,-0.480733945,-0.478899083,-0.47706422,-0.475229358,
-0.473394495,-0.471559633,-0.469724771,-0.467889908,-0.466055046,-0.464220183,
-0.462385321,-0.460550459,-0.458715596,-0.456880734,-0.455045872,-0.453211009,
-0.451376147,-0.449541284,-0.447706422,-0.44587156,-0.444036697,-0.442201835,
-0.440366972,-0.43853211,-0.436697248,-0.434862385,-0.433027523,-0.431192661,
-0.429357798,-0.427522936,-0.425688073,-0.423853211,-0.422018349,-0.420183486,
-0.418348624,-0.416513761,-0.414678899,-0.412844037,-0.411009174,-0.409174312,
-0.40733945,-0.405504587,-0.403669725,-0.401834862,-0.4,-0.398165138,-0.396330275,
-0.394495413,-0.39266055,-0.390825688,-0.388990826,-0.387155963,-0.385321101,
-0.383486239,-0.381651376,-0.379816514,-0.377981651,-0.376146789,-0.374311927,
-0.372477064,-0.370642202,-0.368807339,-0.366972477,-0.365137615,-0.363302752,
-0.36146789,-0.359633028,-0.357798165,-0.355963303,-0.35412844,-0.352293578,
-0.350458716,-0.348623853,-0.346788991,-0.344954128,-0.343119266,-0.341284404,
-0.339449541,-0.337614679,-0.335779817,-0.333944954,-0.332110092,-0.330275229,
-0.328440367,-0.326605505,-0.324770642,-0.32293578,-0.321100917,-0.319266055,
-0.317431193,-0.31559633,-0.313761468,-0.311926606,-0.310091743,-0.308256881,
-0.306422018,-0.304587156,-0.302752294,-0.300917431,-0.299082569,-0.297247706,
-0.295412844,-0.293577982,-0.291743119,-0.289908257,-0.288073394,-0.286238532,
-0.28440367,-0.282568807,-0.280733945,-0.278899083,-0.27706422,-0.275229358,
-0.273394495,-0.271559633,-0.269724771,-0.267889908,-0.266055046,-0.264220183,
-0.262385321,-0.260550459,-0.258715596,-0.256880734,-0.255045872,-0.253211009,
-0.251376147,-0.249541284,-0.247706422,-0.24587156,-0.244036697,-0.242201835,
-0.240366972,-0.23853211,-0.236697248,-0.234862385,-0.233027523,-0.231192661,
-0.229357798,-0.227522936,-0.225688073,-0.223853211,-0.222018349,-0.220183486,
-0.218348624,-0.216513761,-0.214678899,-0.212844037,-0.211009174,-0.209174312,
-0.20733945,-0.205504587,-0.203669725,-0.201834862,-0.2,-0.198165138,-0.196330275,
-0.194495413,-0.19266055,-0.190825688,-0.188990826,-0.187155963,-0.185321101,
-0.183486239,-0.181651376,-0.179816514,-0.177981651,-0.176146789,-0.174311927,
-0.172477064,-0.170642202,-0.168807339,-0.166972477,-0.165137615,-0.163302752,
-0.16146789,-0.159633028,-0.157798165,-0.155963303,-0.15412844,-0.152293578,
-0.150458716,-0.148623853,-0.146788991,-0.144954128,-0.143119266,-0.141284404,
-0.139449541,-0.137614679,-0.135779817,-0.133944954,-0.132110092,-0.130275229,
-0.128440367,-0.126605505,-0.124770642,-0.12293578,-0.121100917,-0.119266055,
-0.117431193,-0.11559633,-0.113761468,-0.111926606,-0.110091743,-0.108256881,
-0.106422018,-0.104587156,-0.102752294,-0.100917431,-0.099082569,-0.097247706,
-0.095412844,-0.093577982,-0.091743119,-0.089908257,-0.088073394,-0.086238532,
-0.08440367,-0.082568807,-0.080733945,-0.078899083,-0.07706422,-0.075229358,
-0.073394495,-0.071559633,-0.069724771,-0.067889908,-0.066055046,-0.064220183,
-0.062385321,-0.060550459,-0.058715596,-0.056880734,-0.055045872,-0.053211009,
-0.051376147,-0.049541284,-0.047706422,-0.04587156,-0.044036697,-0.042201835,
-0.040366972,-0.03853211,-0.036697248,-0.034862385,-0.033027523,-0.031192661,
-0.029357798,-0.027522936,-0.025688073,-0.023853211,-0.022018349,-0.020183486,
-0.018348624,-0.016513761,-0.014678899,-0.012844037,-0.011009174,-0.009174312,
-0.00733945,-0.005504587,-0.003669725,-0.001834862,0.000982159),(0.3,1.,
1.3),.UNSPECIFIED.);
#6326=B_SPLINE_SURFACE_WITH_KNOTS('',5,1,((#339935,#339936,#339937),(#339938,
#339939,#339940),(#339941,#339942,#339943),(#339944,#339945,#339946),(#339947,
#339948,#339949),(#339950,#339951,#339952),(#339953,#339954,#339955),(#339956,
#339957,#339958),(#339959,#339960,#339961),(#339962,#339963,#339964),(#339965,
#339966,#339967),(#339968,#339969,#339970),(#339971,#339972,#339973),(#339974,
#339975,#339976),(#339977,#339978,#339979),(#339980,#339981,#339982),(#339983,
#339984,#339985),(#339986,#339987,#339988),(#339989,#339990,#339991),(#339992,
#339993,#339994),(#339995,#339996,#339997),(#339998,#339999,#340000),(#340001,
#340002,#340003),(#340004,#340005,#340006),(#340007,#340008,#340009),(#340010,
#340011,#340012),(#340013,#340014,#340015),(#340016,#340017,#340018),(#340019,
#340020,#340021),(#340022,#340023,#340024),(#340025,#340026,#340027),(#340028,
#340029,#340030),(#340031,#340032,#340033),(#340034,#340035,#340036),(#340037,
#340038,#340039),(#340040,#340041,#340042),(#340043,#340044,#340045),(#340046,
#340047,#340048),(#340049,#340050,#340051),(#340052,#340053,#340054),(#340055,
#340056,#340057),(#340058,#340059,#340060),(#340061,#340062,#340063),(#340064,
#340065,#340066),(#340067,#340068,#340069),(#340070,#340071,#340072),(#340073,
#340074,#340075),(#340076,#340077,#340078),(#340079,#340080,#340081),(#340082,
#340083,#340084),(#340085,#340086,#340087),(#340088,#340089,#340090),(#340091,
#340092,#340093),(#340094,#340095,#340096),(#340097,#340098,#340099),(#340100,
#340101,#340102),(#340103,#340104,#340105),(#340106,#340107,#340108),(#340109,
#340110,#340111),(#340112,#340113,#340114),(#340115,#340116,#340117),(#340118,
#340119,#340120),(#340121,#340122,#340123),(#340124,#340125,#340126),(#340127,
#340128,#340129),(#340130,#340131,#340132),(#340133,#340134,#340135),(#340136,
#340137,#340138),(#340139,#340140,#340141),(#340142,#340143,#340144),(#340145,
#340146,#340147),(#340148,#340149,#340150),(#340151,#340152,#340153),(#340154,
#340155,#340156),(#340157,#340158,#340159),(#340160,#340161,#340162),(#340163,
#340164,#340165),(#340166,#340167,#340168),(#340169,#340170,#340171),(#340172,
#340173,#340174),(#340175,#340176,#340177),(#340178,#340179,#340180),(#340181,
#340182,#340183),(#340184,#340185,#340186),(#340187,#340188,#340189),(#340190,
#340191,#340192),(#340193,#340194,#340195),(#340196,#340197,#340198),(#340199,
#340200,#340201),(#340202,#340203,#340204),(#340205,#340206,#340207),(#340208,
#340209,#340210),(#340211,#340212,#340213),(#340214,#340215,#340216),(#340217,
#340218,#340219),(#340220,#340221,#340222),(#340223,#340224,#340225),(#340226,
#340227,#340228),(#340229,#340230,#340231),(#340232,#340233,#340234),(#340235,
#340236,#340237),(#340238,#340239,#340240),(#340241,#340242,#340243),(#340244,
#340245,#340246),(#340247,#340248,#340249),(#340250,#340251,#340252),(#340253,
#340254,#340255),(#340256,#340257,#340258),(#340259,#340260,#340261),(#340262,
#340263,#340264),(#340265,#340266,#340267),(#340268,#340269,#340270),(#340271,
#340272,#340273),(#340274,#340275,#340276),(#340277,#340278,#340279),(#340280,
#340281,#340282),(#340283,#340284,#340285),(#340286,#340287,#340288),(#340289,
#340290,#340291),(#340292,#340293,#340294),(#340295,#340296,#340297),(#340298,
#340299,#340300),(#340301,#340302,#340303),(#340304,#340305,#340306),(#340307,
#340308,#340309),(#340310,#340311,#340312),(#340313,#340314,#340315),(#340316,
#340317,#340318),(#340319,#340320,#340321),(#340322,#340323,#340324),(#340325,
#340326,#340327),(#340328,#340329,#340330),(#340331,#340332,#340333),(#340334,
#340335,#340336),(#340337,#340338,#340339),(#340340,#340341,#340342),(#340343,
#340344,#340345),(#340346,#340347,#340348),(#340349,#340350,#340351),(#340352,
#340353,#340354),(#340355,#340356,#340357),(#340358,#340359,#340360),(#340361,
#340362,#340363),(#340364,#340365,#340366),(#340367,#340368,#340369),(#340370,
#340371,#340372),(#340373,#340374,#340375),(#340376,#340377,#340378),(#340379,
#340380,#340381),(#340382,#340383,#340384),(#340385,#340386,#340387),(#340388,
#340389,#340390),(#340391,#340392,#340393),(#340394,#340395,#340396),(#340397,
#340398,#340399),(#340400,#340401,#340402),(#340403,#340404,#340405),(#340406,
#340407,#340408),(#340409,#340410,#340411),(#340412,#340413,#340414),(#340415,
#340416,#340417),(#340418,#340419,#340420),(#340421,#340422,#340423),(#340424,
#340425,#340426),(#340427,#340428,#340429),(#340430,#340431,#340432),(#340433,
#340434,#340435),(#340436,#340437,#340438),(#340439,#340440,#340441),(#340442,
#340443,#340444),(#340445,#340446,#340447),(#340448,#340449,#340450),(#340451,
#340452,#340453),(#340454,#340455,#340456),(#340457,#340458,#340459),(#340460,
#340461,#340462),(#340463,#340464,#340465),(#340466,#340467,#340468),(#340469,
#340470,#340471),(#340472,#340473,#340474),(#340475,#340476,#340477),(#340478,
#340479,#340480),(#340481,#340482,#340483),(#340484,#340485,#340486),(#340487,
#340488,#340489),(#340490,#340491,#340492),(#340493,#340494,#340495),(#340496,
#340497,#340498),(#340499,#340500,#340501),(#340502,#340503,#340504),(#340505,
#340506,#340507),(#340508,#340509,#340510),(#340511,#340512,#340513),(#340514,
#340515,#340516),(#340517,#340518,#340519),(#340520,#340521,#340522),(#340523,
#340524,#340525),(#340526,#340527,#340528),(#340529,#340530,#340531),(#340532,
#340533,#340534),(#340535,#340536,#340537),(#340538,#340539,#340540),(#340541,
#340542,#340543),(#340544,#340545,#340546),(#340547,#340548,#340549),(#340550,
#340551,#340552),(#340553,#340554,#340555),(#340556,#340557,#340558),(#340559,
#340560,#340561),(#340562,#340563,#340564),(#340565,#340566,#340567),(#340568,
#340569,#340570),(#340571,#340572,#340573),(#340574,#340575,#340576),(#340577,
#340578,#340579),(#340580,#340581,#340582),(#340583,#340584,#340585),(#340586,
#340587,#340588),(#340589,#340590,#340591),(#340592,#340593,#340594),(#340595,
#340596,#340597),(#340598,#340599,#340600),(#340601,#340602,#340603),(#340604,
#340605,#340606),(#340607,#340608,#340609),(#340610,#340611,#340612),(#340613,
#340614,#340615),(#340616,#340617,#340618),(#340619,#340620,#340621),(#340622,
#340623,#340624),(#340625,#340626,#340627),(#340628,#340629,#340630),(#340631,
#340632,#340633),(#340634,#340635,#340636),(#340637,#340638,#340639),(#340640,
#340641,#340642),(#340643,#340644,#340645),(#340646,#340647,#340648),(#340649,
#340650,#340651),(#340652,#340653,#340654),(#340655,#340656,#340657),(#340658,
#340659,#340660),(#340661,#340662,#340663),(#340664,#340665,#340666),(#340667,
#340668,#340669),(#340670,#340671,#340672),(#340673,#340674,#340675),(#340676,
#340677,#340678),(#340679,#340680,#340681),(#340682,#340683,#340684),(#340685,
#340686,#340687),(#340688,#340689,#340690),(#340691,#340692,#340693),(#340694,
#340695,#340696),(#340697,#340698,#340699),(#340700,#340701,#340702),(#340703,
#340704,#340705),(#340706,#340707,#340708),(#340709,#340710,#340711),(#340712,
#340713,#340714),(#340715,#340716,#340717),(#340718,#340719,#340720),(#340721,
#340722,#340723),(#340724,#340725,#340726),(#340727,#340728,#340729),(#340730,
#340731,#340732),(#340733,#340734,#340735),(#340736,#340737,#340738),(#340739,
#340740,#340741),(#340742,#340743,#340744),(#340745,#340746,#340747),(#340748,
#340749,#340750),(#340751,#340752,#340753),(#340754,#340755,#340756),(#340757,
#340758,#340759),(#340760,#340761,#340762),(#340763,#340764,#340765),(#340766,
#340767,#340768),(#340769,#340770,#340771),(#340772,#340773,#340774),(#340775,
#340776,#340777),(#340778,#340779,#340780),(#340781,#340782,#340783),(#340784,
#340785,#340786),(#340787,#340788,#340789),(#340790,#340791,#340792),(#340793,
#340794,#340795),(#340796,#340797,#340798),(#340799,#340800,#340801),(#340802,
#340803,#340804),(#340805,#340806,#340807),(#340808,#340809,#340810),(#340811,
#340812,#340813),(#340814,#340815,#340816),(#340817,#340818,#340819),(#340820,
#340821,#340822),(#340823,#340824,#340825),(#340826,#340827,#340828),(#340829,
#340830,#340831),(#340832,#340833,#340834),(#340835,#340836,#340837),(#340838,
#340839,#340840),(#340841,#340842,#340843),(#340844,#340845,#340846),(#340847,
#340848,#340849),(#340850,#340851,#340852),(#340853,#340854,#340855),(#340856,
#340857,#340858),(#340859,#340860,#340861),(#340862,#340863,#340864),(#340865,
#340866,#340867),(#340868,#340869,#340870),(#340871,#340872,#340873),(#340874,
#340875,#340876),(#340877,#340878,#340879),(#340880,#340881,#340882),(#340883,
#340884,#340885),(#340886,#340887,#340888),(#340889,#340890,#340891),(#340892,
#340893,#340894),(#340895,#340896,#340897),(#340898,#340899,#340900),(#340901,
#340902,#340903),(#340904,#340905,#340906),(#340907,#340908,#340909),(#340910,
#340911,#340912),(#340913,#340914,#340915),(#340916,#340917,#340918),(#340919,
#340920,#340921),(#340922,#340923,#340924),(#340925,#340926,#340927),(#340928,
#340929,#340930),(#340931,#340932,#340933),(#340934,#340935,#340936),(#340937,
#340938,#340939),(#340940,#340941,#340942),(#340943,#340944,#340945),(#340946,
#340947,#340948),(#340949,#340950,#340951),(#340952,#340953,#340954),(#340955,
#340956,#340957),(#340958,#340959,#340960),(#340961,#340962,#340963),(#340964,
#340965,#340966),(#340967,#340968,#340969),(#340970,#340971,#340972),(#340973,
#340974,#340975),(#340976,#340977,#340978),(#340979,#340980,#340981),(#340982,
#340983,#340984),(#340985,#340986,#340987),(#340988,#340989,#340990),(#340991,
#340992,#340993),(#340994,#340995,#340996),(#340997,#340998,#340999),(#341000,
#341001,#341002),(#341003,#341004,#341005),(#341006,#341007,#341008),(#341009,
#341010,#341011),(#341012,#341013,#341014),(#341015,#341016,#341017),(#341018,
#341019,#341020),(#341021,#341022,#341023),(#341024,#341025,#341026),(#341027,
#341028,#341029),(#341030,#341031,#341032),(#341033,#341034,#341035),(#341036,
#341037,#341038),(#341039,#341040,#341041),(#341042,#341043,#341044),(#341045,
#341046,#341047),(#341048,#341049,#341050),(#341051,#341052,#341053),(#341054,
#341055,#341056),(#341057,#341058,#341059),(#341060,#341061,#341062),(#341063,
#341064,#341065),(#341066,#341067,#341068),(#341069,#341070,#341071),(#341072,
#341073,#341074),(#341075,#341076,#341077),(#341078,#341079,#341080),(#341081,
#341082,#341083),(#341084,#341085,#341086),(#341087,#341088,#341089),(#341090,
#341091,#341092),(#341093,#341094,#341095),(#341096,#341097,#341098),(#341099,
#341100,#341101),(#341102,#341103,#341104),(#341105,#341106,#341107),(#341108,
#341109,#341110),(#341111,#341112,#341113),(#341114,#341115,#341116),(#341117,
#341118,#341119),(#341120,#341121,#341122),(#341123,#341124,#341125),(#341126,
#341127,#341128),(#341129,#341130,#341131),(#341132,#341133,#341134),(#341135,
#341136,#341137),(#341138,#341139,#341140),(#341141,#341142,#341143),(#341144,
#341145,#341146),(#341147,#341148,#341149),(#341150,#341151,#341152),(#341153,
#341154,#341155),(#341156,#341157,#341158),(#341159,#341160,#341161),(#341162,
#341163,#341164),(#341165,#341166,#341167),(#341168,#341169,#341170),(#341171,
#341172,#341173),(#341174,#341175,#341176),(#341177,#341178,#341179),(#341180,
#341181,#341182),(#341183,#341184,#341185),(#341186,#341187,#341188),(#341189,
#341190,#341191),(#341192,#341193,#341194),(#341195,#341196,#341197),(#341198,
#341199,#341200),(#341201,#341202,#341203),(#341204,#341205,#341206),(#341207,
#341208,#341209),(#341210,#341211,#341212),(#341213,#341214,#341215),(#341216,
#341217,#341218),(#341219,#341220,#341221),(#341222,#341223,#341224),(#341225,
#341226,#341227),(#341228,#341229,#341230),(#341231,#341232,#341233),(#341234,
#341235,#341236),(#341237,#341238,#341239),(#341240,#341241,#341242),(#341243,
#341244,#341245),(#341246,#341247,#341248),(#341249,#341250,#341251),(#341252,
#341253,#341254),(#341255,#341256,#341257),(#341258,#341259,#341260),(#341261,
#341262,#341263),(#341264,#341265,#341266),(#341267,#341268,#341269),(#341270,
#341271,#341272),(#341273,#341274,#341275),(#341276,#341277,#341278),(#341279,
#341280,#341281),(#341282,#341283,#341284),(#341285,#341286,#341287),(#341288,
#341289,#341290),(#341291,#341292,#341293),(#341294,#341295,#341296),(#341297,
#341298,#341299),(#341300,#341301,#341302),(#341303,#341304,#341305),(#341306,
#341307,#341308),(#341309,#341310,#341311),(#341312,#341313,#341314),(#341315,
#341316,#341317),(#341318,#341319,#341320),(#341321,#341322,#341323),(#341324,
#341325,#341326),(#341327,#341328,#341329),(#341330,#341331,#341332),(#341333,
#341334,#341335),(#341336,#341337,#341338),(#341339,#341340,#341341),(#341342,
#341343,#341344),(#341345,#341346,#341347),(#341348,#341349,#341350),(#341351,
#341352,#341353),(#341354,#341355,#341356),(#341357,#341358,#341359),(#341360,
#341361,#341362),(#341363,#341364,#341365),(#341366,#341367,#341368),(#341369,
#341370,#341371),(#341372,#341373,#341374),(#341375,#341376,#341377),(#341378,
#341379,#341380),(#341381,#341382,#341383),(#341384,#341385,#341386),(#341387,
#341388,#341389),(#341390,#341391,#341392),(#341393,#341394,#341395),(#341396,
#341397,#341398),(#341399,#341400,#341401),(#341402,#341403,#341404),(#341405,
#341406,#341407),(#341408,#341409,#341410),(#341411,#341412,#341413),(#341414,
#341415,#341416),(#341417,#341418,#341419),(#341420,#341421,#341422),(#341423,
#341424,#341425),(#341426,#341427,#341428),(#341429,#341430,#341431),(#341432,
#341433,#341434),(#341435,#341436,#341437),(#341438,#341439,#341440),(#341441,
#341442,#341443),(#341444,#341445,#341446),(#341447,#341448,#341449),(#341450,
#341451,#341452),(#341453,#341454,#341455),(#341456,#341457,#341458),(#341459,
#341460,#341461),(#341462,#341463,#341464),(#341465,#341466,#341467),(#341468,
#341469,#341470),(#341471,#341472,#341473),(#341474,#341475,#341476),(#341477,
#341478,#341479),(#341480,#341481,#341482),(#341483,#341484,#341485),(#341486,
#341487,#341488),(#341489,#341490,#341491),(#341492,#341493,#341494),(#341495,
#341496,#341497),(#341498,#341499,#341500),(#341501,#341502,#341503),(#341504,
#341505,#341506),(#341507,#341508,#341509),(#341510,#341511,#341512),(#341513,
#341514,#341515),(#341516,#341517,#341518),(#341519,#341520,#341521),(#341522,
#341523,#341524),(#341525,#341526,#341527),(#341528,#341529,#341530),(#341531,
#341532,#341533),(#341534,#341535,#341536),(#341537,#341538,#341539),(#341540,
#341541,#341542),(#341543,#341544,#341545),(#341546,#341547,#341548),(#341549,
#341550,#341551),(#341552,#341553,#341554),(#341555,#341556,#341557),(#341558,
#341559,#341560),(#341561,#341562,#341563),(#341564,#341565,#341566),(#341567,
#341568,#341569),(#341570,#341571,#341572),(#341573,#341574,#341575),(#341576,
#341577,#341578),(#341579,#341580,#341581),(#341582,#341583,#341584),(#341585,
#341586,#341587)),.UNSPECIFIED.,.F.,.F.,.F.,(6,1,1,1,1,1,1,1,1,1,1,1,1,
1,1,1,1,1,1,1,1,1,1,1,1,1,1,1,1,1,1,1,1,1,1,1,1,1,1,1,1,1,1,1,1,1,1,1,1,
1,1,1,1,1,1,1,1,1,1,1,1,1,1,1,1,1,1,1,1,1,1,1,1,1,1,1,1,1,1,1,1,1,1,1,1,
1,1,1,1,1,1,1,1,1,1,1,1,1,1,1,1,1,1,1,1,1,1,1,1,1,1,1,1,1,1,1,1,1,1,1,1,
1,1,1,1,1,1,1,1,1,1,1,1,1,1,1,1,1,1,1,1,1,1,1,1,1,1,1,1,1,1,1,1,1,1,1,1,
1,1,1,1,1,1,1,1,1,1,1,1,1,1,1,1,1,1,1,1,1,1,1,1,1,1,1,1,1,1,1,1,1,1,1,1,
1,1,1,1,1,1,1,1,1,1,1,1,1,1,1,1,1,1,1,1,1,1,1,1,1,1,1,1,1,1,1,1,1,1,1,1,
1,1,1,1,1,1,1,1,1,1,1,1,1,1,1,1,1,1,1,1,1,1,1,1,1,1,1,1,1,1,1,1,1,1,1,1,
1,1,1,1,1,1,1,1,1,1,1,1,1,1,1,1,1,1,1,1,1,1,1,1,1,1,1,1,1,1,1,1,1,1,1,1,
1,1,1,1,1,1,1,1,1,1,1,1,1,1,1,1,1,1,1,1,1,1,1,1,1,1,1,1,1,1,1,1,1,1,1,1,
1,1,1,1,1,1,1,1,1,1,1,1,1,1,1,1,1,1,1,1,1,1,1,1,1,1,1,1,1,1,1,1,1,1,1,1,
1,1,1,1,1,1,1,1,1,1,1,1,1,1,1,1,1,1,1,1,1,1,1,1,1,1,1,1,1,1,1,1,1,1,1,1,
1,1,1,1,1,1,1,1,1,1,1,1,1,1,1,1,1,1,1,1,1,1,1,1,1,1,1,1,1,1,1,1,1,1,1,1,
1,1,1,1,1,1,1,1,1,1,1,1,1,1,1,1,1,1,1,1,1,1,1,1,1,1,1,1,1,1,1,1,1,1,1,1,
1,1,1,1,1,1,1,1,1,1,1,1,1,1,1,1,1,1,1,1,1,1,1,1,1,1,1,1,1,1,1,1,1,1,1,1,
1,1,1,1,1,1,1,1,1,1,1,1,1,1,1,1,1,1,1,1,1,1,1,1,1,1,1,1,1,6),(2,1,2),(-0.001964156,
0.,0.001834862,0.003669725,0.005504587,0.00733945,0.009174312,0.011009174,
0.012844037,0.014678899,0.016513761,0.018348624,0.020183486,0.022018349,
0.023853211,0.025688073,0.027522936,0.029357798,0.031192661,0.033027523,
0.034862385,0.036697248,0.03853211,0.040366972,0.042201835,0.044036697,
0.04587156,0.047706422,0.049541284,0.051376147,0.053211009,0.055045872,
0.056880734,0.058715596,0.060550459,0.062385321,0.064220183,0.066055046,
0.067889908,0.069724771,0.071559633,0.073394495,0.075229358,0.07706422,
0.078899083,0.080733945,0.082568807,0.08440367,0.086238532,0.088073394,
0.089908257,0.091743119,0.093577982,0.095412844,0.097247706,0.099082569,
0.100917431,0.102752294,0.104587156,0.106422018,0.108256881,0.110091743,
0.111926606,0.113761468,0.11559633,0.117431193,0.119266055,0.121100917,
0.12293578,0.124770642,0.126605505,0.128440367,0.130275229,0.132110092,
0.133944954,0.135779817,0.137614679,0.139449541,0.141284404,0.143119266,
0.144954128,0.146788991,0.148623853,0.150458716,0.152293578,0.15412844,
0.155963303,0.157798165,0.159633028,0.16146789,0.163302752,0.165137615,
0.166972477,0.168807339,0.170642202,0.172477064,0.174311927,0.176146789,
0.177981651,0.179816514,0.181651376,0.183486239,0.185321101,0.187155963,
0.188990826,0.190825688,0.19266055,0.194495413,0.196330275,0.198165138,
0.2,0.201834862,0.203669725,0.205504587,0.20733945,0.209174312,0.211009174,
0.212844037,0.214678899,0.216513761,0.218348624,0.220183486,0.222018349,
0.223853211,0.225688073,0.227522936,0.229357798,0.231192661,0.233027523,
0.234862385,0.236697248,0.23853211,0.240366972,0.242201835,0.244036697,
0.24587156,0.247706422,0.249541284,0.251376147,0.253211009,0.255045872,
0.256880734,0.258715596,0.260550459,0.262385321,0.264220183,0.266055046,
0.267889908,0.269724771,0.271559633,0.273394495,0.275229358,0.27706422,
0.278899083,0.280733945,0.282568807,0.28440367,0.286238532,0.288073394,
0.289908257,0.291743119,0.293577982,0.295412844,0.297247706,0.299082569,
0.300917431,0.302752294,0.304587156,0.306422018,0.308256881,0.310091743,
0.311926606,0.313761468,0.31559633,0.317431193,0.319266055,0.321100917,
0.32293578,0.324770642,0.326605505,0.328440367,0.330275229,0.332110092,
0.333944954,0.335779817,0.337614679,0.339449541,0.341284404,0.343119266,
0.344954128,0.346788991,0.348623853,0.350458716,0.352293578,0.35412844,
0.355963303,0.357798165,0.359633028,0.36146789,0.363302752,0.365137615,
0.366972477,0.368807339,0.370642202,0.372477064,0.374311927,0.376146789,
0.377981651,0.379816514,0.381651376,0.383486239,0.385321101,0.387155963,
0.388990826,0.390825688,0.39266055,0.394495413,0.396330275,0.398165138,
0.4,0.401834862,0.403669725,0.405504587,0.40733945,0.409174312,0.411009174,
0.412844037,0.414678899,0.416513761,0.418348624,0.420183486,0.422018349,
0.423853211,0.425688073,0.427522936,0.429357798,0.431192661,0.433027523,
0.434862385,0.436697248,0.43853211,0.440366972,0.442201835,0.444036697,
0.44587156,0.447706422,0.449541284,0.451376147,0.453211009,0.455045872,
0.456880734,0.458715596,0.460550459,0.462385321,0.464220183,0.466055046,
0.467889908,0.469724771,0.471559633,0.473394495,0.475229358,0.47706422,
0.478899083,0.480733945,0.482568807,0.48440367,0.486238532,0.488073394,
0.489908257,0.491743119,0.493577982,0.495412844,0.497247706,0.499082569,
0.500917431,0.502752294,0.504587156,0.506422018,0.508256881,0.510091743,
0.511926606,0.513761468,0.51559633,0.517431193,0.519266055,0.521100917,
0.52293578,0.524770642,0.526605505,0.528440367,0.530275229,0.532110092,
0.533944954,0.535779817,0.537614679,0.539449541,0.541284404,0.543119266,
0.544954128,0.546788991,0.548623853,0.550458716,0.552293578,0.55412844,
0.555963303,0.557798165,0.559633028,0.56146789,0.563302752,0.565137615,
0.566972477,0.568807339,0.570642202,0.572477064,0.574311927,0.576146789,
0.577981651,0.579816514,0.581651376,0.583486239,0.585321101,0.587155963,
0.588990826,0.590825688,0.59266055,0.594495413,0.596330275,0.598165138,
0.6,0.601834862,0.603669725,0.605504587,0.60733945,0.609174312,0.611009174,
0.612844037,0.614678899,0.616513761,0.618348624,0.620183486,0.622018349,
0.623853211,0.625688073,0.627522936,0.629357798,0.631192661,0.633027523,
0.634862385,0.636697248,0.63853211,0.640366972,0.642201835,0.644036697,
0.64587156,0.647706422,0.649541284,0.651376147,0.653211009,0.655045872,
0.656880734,0.658715596,0.660550459,0.662385321,0.664220183,0.666055046,
0.667889908,0.669724771,0.671559633,0.673394495,0.675229358,0.67706422,
0.678899083,0.680733945,0.682568807,0.68440367,0.686238532,0.688073394,
0.689908257,0.691743119,0.693577982,0.695412844,0.697247706,0.699082569,
0.700917431,0.702752294,0.704587156,0.706422018,0.708256881,0.710091743,
0.711926606,0.713761468,0.71559633,0.717431193,0.719266055,0.721100917,
0.72293578,0.724770642,0.726605505,0.728440367,0.730275229,0.732110092,
0.733944954,0.735779817,0.737614679,0.739449541,0.741284404,0.743119266,
0.744954128,0.746788991,0.748623853,0.750458716,0.752293578,0.75412844,
0.755963303,0.757798165,0.759633028,0.76146789,0.763302752,0.765137615,
0.766972477,0.768807339,0.770642202,0.772477064,0.774311927,0.776146789,
0.777981651,0.779816514,0.781651376,0.783486239,0.785321101,0.787155963,
0.788990826,0.790825688,0.79266055,0.794495413,0.796330275,0.798165138,
0.8,0.801834862,0.803669725,0.805504587,0.80733945,0.809174312,0.811009174,
0.812844037,0.814678899,0.816513761,0.818348624,0.820183486,0.822018349,
0.823853211,0.825688073,0.827522936,0.829357798,0.831192661,0.833027523,
0.834862385,0.836697248,0.83853211,0.840366972,0.842201835,0.844036697,
0.84587156,0.847706422,0.849541284,0.851376147,0.853211009,0.855045872,
0.856880734,0.858715596,0.860550459,0.862385321,0.864220183,0.866055046,
0.867889908,0.869724771,0.871559633,0.873394495,0.875229358,0.87706422,
0.878899083,0.880733945,0.882568807,0.88440367,0.886238532,0.888073394,
0.889908257,0.891743119,0.893577982,0.895412844,0.897247706,0.899082569,
0.900917431,0.902752294,0.904587156,0.906422018,0.908256881,0.910091743,
0.911926606,0.913761468,0.91559633,0.917431193,0.919266055,0.921100917,
0.92293578,0.924770642,0.926605505,0.928440367,0.930275229,0.932110092,
0.933944954,0.935779817,0.937614679,0.939449541,0.941284404,0.943119266,
0.944954128,0.946788991,0.948623853,0.950458716,0.952293578,0.95412844,
0.955963303,0.957798165,0.959633028,0.96146789,0.963302752,0.965137615,
0.966972477,0.968807339,0.970642202,0.972477064,0.974311927,0.976146789,
0.977981651,0.979816514,0.981651376,0.983486239,0.985321101,0.987155963,
0.988990826,0.990825688,0.99266055,0.994495413,0.996330275,0.998165138,
1.000000000441),(0.3,1.,1.3),.UNSPECIFIED.);
#6327=B_SPLINE_SURFACE_WITH_KNOTS('',5,1,((#341592,#341593,#341594),(#341595,
#341596,#341597),(#341598,#341599,#341600),(#341601,#341602,#341603),(#341604,
#341605,#341606),(#341607,#341608,#341609),(#341610,#341611,#341612),(#341613,
#341614,#341615),(#341616,#341617,#341618),(#341619,#341620,#341621),(#341622,
#341623,#341624),(#341625,#341626,#341627),(#341628,#341629,#341630),(#341631,
#341632,#341633),(#341634,#341635,#341636),(#341637,#341638,#341639),(#341640,
#341641,#341642),(#341643,#341644,#341645),(#341646,#341647,#341648),(#341649,
#341650,#341651),(#341652,#341653,#341654),(#341655,#341656,#341657),(#341658,
#341659,#341660),(#341661,#341662,#341663),(#341664,#341665,#341666),(#341667,
#341668,#341669),(#341670,#341671,#341672),(#341673,#341674,#341675),(#341676,
#341677,#341678),(#341679,#341680,#341681),(#341682,#341683,#341684),(#341685,
#341686,#341687),(#341688,#341689,#341690),(#341691,#341692,#341693),(#341694,
#341695,#341696),(#341697,#341698,#341699),(#341700,#341701,#341702),(#341703,
#341704,#341705),(#341706,#341707,#341708),(#341709,#341710,#341711),(#341712,
#341713,#341714),(#341715,#341716,#341717),(#341718,#341719,#341720),(#341721,
#341722,#341723),(#341724,#341725,#341726),(#341727,#341728,#341729),(#341730,
#341731,#341732),(#341733,#341734,#341735),(#341736,#341737,#341738),(#341739,
#341740,#341741),(#341742,#341743,#341744),(#341745,#341746,#341747),(#341748,
#341749,#341750),(#341751,#341752,#341753),(#341754,#341755,#341756),(#341757,
#341758,#341759),(#341760,#341761,#341762),(#341763,#341764,#341765),(#341766,
#341767,#341768),(#341769,#341770,#341771),(#341772,#341773,#341774),(#341775,
#341776,#341777),(#341778,#341779,#341780),(#341781,#341782,#341783),(#341784,
#341785,#341786),(#341787,#341788,#341789),(#341790,#341791,#341792),(#341793,
#341794,#341795),(#341796,#341797,#341798),(#341799,#341800,#341801),(#341802,
#341803,#341804),(#341805,#341806,#341807),(#341808,#341809,#341810),(#341811,
#341812,#341813),(#341814,#341815,#341816),(#341817,#341818,#341819),(#341820,
#341821,#341822),(#341823,#341824,#341825),(#341826,#341827,#341828),(#341829,
#341830,#341831),(#341832,#341833,#341834),(#341835,#341836,#341837),(#341838,
#341839,#341840),(#341841,#341842,#341843),(#341844,#341845,#341846),(#341847,
#341848,#341849),(#341850,#341851,#341852),(#341853,#341854,#341855),(#341856,
#341857,#341858),(#341859,#341860,#341861),(#341862,#341863,#341864),(#341865,
#341866,#341867),(#341868,#341869,#341870),(#341871,#341872,#341873),(#341874,
#341875,#341876),(#341877,#341878,#341879),(#341880,#341881,#341882),(#341883,
#341884,#341885),(#341886,#341887,#341888),(#341889,#341890,#341891),(#341892,
#341893,#341894),(#341895,#341896,#341897),(#341898,#341899,#341900),(#341901,
#341902,#341903),(#341904,#341905,#341906),(#341907,#341908,#341909),(#341910,
#341911,#341912),(#341913,#341914,#341915),(#341916,#341917,#341918),(#341919,
#341920,#341921),(#341922,#341923,#341924),(#341925,#341926,#341927),(#341928,
#341929,#341930),(#341931,#341932,#341933),(#341934,#341935,#341936),(#341937,
#341938,#341939),(#341940,#341941,#341942),(#341943,#341944,#341945),(#341946,
#341947,#341948),(#341949,#341950,#341951),(#341952,#341953,#341954),(#341955,
#341956,#341957),(#341958,#341959,#341960),(#341961,#341962,#341963),(#341964,
#341965,#341966),(#341967,#341968,#341969),(#341970,#341971,#341972),(#341973,
#341974,#341975),(#341976,#341977,#341978),(#341979,#341980,#341981),(#341982,
#341983,#341984),(#341985,#341986,#341987),(#341988,#341989,#341990),(#341991,
#341992,#341993),(#341994,#341995,#341996),(#341997,#341998,#341999),(#342000,
#342001,#342002),(#342003,#342004,#342005),(#342006,#342007,#342008),(#342009,
#342010,#342011),(#342012,#342013,#342014),(#342015,#342016,#342017),(#342018,
#342019,#342020),(#342021,#342022,#342023),(#342024,#342025,#342026),(#342027,
#342028,#342029),(#342030,#342031,#342032),(#342033,#342034,#342035),(#342036,
#342037,#342038),(#342039,#342040,#342041),(#342042,#342043,#342044),(#342045,
#342046,#342047),(#342048,#342049,#342050),(#342051,#342052,#342053),(#342054,
#342055,#342056),(#342057,#342058,#342059),(#342060,#342061,#342062),(#342063,
#342064,#342065),(#342066,#342067,#342068),(#342069,#342070,#342071),(#342072,
#342073,#342074),(#342075,#342076,#342077),(#342078,#342079,#342080),(#342081,
#342082,#342083),(#342084,#342085,#342086),(#342087,#342088,#342089),(#342090,
#342091,#342092),(#342093,#342094,#342095),(#342096,#342097,#342098),(#342099,
#342100,#342101),(#342102,#342103,#342104),(#342105,#342106,#342107),(#342108,
#342109,#342110),(#342111,#342112,#342113),(#342114,#342115,#342116),(#342117,
#342118,#342119),(#342120,#342121,#342122),(#342123,#342124,#342125),(#342126,
#342127,#342128),(#342129,#342130,#342131),(#342132,#342133,#342134),(#342135,
#342136,#342137),(#342138,#342139,#342140),(#342141,#342142,#342143),(#342144,
#342145,#342146),(#342147,#342148,#342149),(#342150,#342151,#342152),(#342153,
#342154,#342155),(#342156,#342157,#342158),(#342159,#342160,#342161),(#342162,
#342163,#342164),(#342165,#342166,#342167),(#342168,#342169,#342170),(#342171,
#342172,#342173),(#342174,#342175,#342176),(#342177,#342178,#342179),(#342180,
#342181,#342182),(#342183,#342184,#342185),(#342186,#342187,#342188),(#342189,
#342190,#342191),(#342192,#342193,#342194),(#342195,#342196,#342197),(#342198,
#342199,#342200),(#342201,#342202,#342203),(#342204,#342205,#342206),(#342207,
#342208,#342209),(#342210,#342211,#342212),(#342213,#342214,#342215),(#342216,
#342217,#342218),(#342219,#342220,#342221),(#342222,#342223,#342224),(#342225,
#342226,#342227),(#342228,#342229,#342230),(#342231,#342232,#342233),(#342234,
#342235,#342236),(#342237,#342238,#342239),(#342240,#342241,#342242),(#342243,
#342244,#342245),(#342246,#342247,#342248),(#342249,#342250,#342251),(#342252,
#342253,#342254),(#342255,#342256,#342257),(#342258,#342259,#342260),(#342261,
#342262,#342263),(#342264,#342265,#342266),(#342267,#342268,#342269),(#342270,
#342271,#342272),(#342273,#342274,#342275),(#342276,#342277,#342278),(#342279,
#342280,#342281),(#342282,#342283,#342284),(#342285,#342286,#342287),(#342288,
#342289,#342290),(#342291,#342292,#342293),(#342294,#342295,#342296),(#342297,
#342298,#342299),(#342300,#342301,#342302),(#342303,#342304,#342305),(#342306,
#342307,#342308),(#342309,#342310,#342311),(#342312,#342313,#342314),(#342315,
#342316,#342317),(#342318,#342319,#342320),(#342321,#342322,#342323),(#342324,
#342325,#342326),(#342327,#342328,#342329),(#342330,#342331,#342332),(#342333,
#342334,#342335),(#342336,#342337,#342338),(#342339,#342340,#342341),(#342342,
#342343,#342344),(#342345,#342346,#342347),(#342348,#342349,#342350),(#342351,
#342352,#342353),(#342354,#342355,#342356),(#342357,#342358,#342359),(#342360,
#342361,#342362),(#342363,#342364,#342365),(#342366,#342367,#342368),(#342369,
#342370,#342371),(#342372,#342373,#342374),(#342375,#342376,#342377),(#342378,
#342379,#342380),(#342381,#342382,#342383),(#342384,#342385,#342386),(#342387,
#342388,#342389),(#342390,#342391,#342392),(#342393,#342394,#342395),(#342396,
#342397,#342398),(#342399,#342400,#342401),(#342402,#342403,#342404),(#342405,
#342406,#342407),(#342408,#342409,#342410),(#342411,#342412,#342413),(#342414,
#342415,#342416),(#342417,#342418,#342419),(#342420,#342421,#342422),(#342423,
#342424,#342425),(#342426,#342427,#342428),(#342429,#342430,#342431),(#342432,
#342433,#342434),(#342435,#342436,#342437),(#342438,#342439,#342440),(#342441,
#342442,#342443),(#342444,#342445,#342446),(#342447,#342448,#342449),(#342450,
#342451,#342452),(#342453,#342454,#342455),(#342456,#342457,#342458),(#342459,
#342460,#342461),(#342462,#342463,#342464),(#342465,#342466,#342467),(#342468,
#342469,#342470),(#342471,#342472,#342473),(#342474,#342475,#342476),(#342477,
#342478,#342479),(#342480,#342481,#342482),(#342483,#342484,#342485),(#342486,
#342487,#342488),(#342489,#342490,#342491),(#342492,#342493,#342494),(#342495,
#342496,#342497),(#342498,#342499,#342500),(#342501,#342502,#342503),(#342504,
#342505,#342506),(#342507,#342508,#342509),(#342510,#342511,#342512),(#342513,
#342514,#342515),(#342516,#342517,#342518),(#342519,#342520,#342521),(#342522,
#342523,#342524),(#342525,#342526,#342527),(#342528,#342529,#342530),(#342531,
#342532,#342533),(#342534,#342535,#342536),(#342537,#342538,#342539),(#342540,
#342541,#342542),(#342543,#342544,#342545),(#342546,#342547,#342548),(#342549,
#342550,#342551),(#342552,#342553,#342554),(#342555,#342556,#342557),(#342558,
#342559,#342560),(#342561,#342562,#342563),(#342564,#342565,#342566),(#342567,
#342568,#342569),(#342570,#342571,#342572),(#342573,#342574,#342575),(#342576,
#342577,#342578),(#342579,#342580,#342581),(#342582,#342583,#342584),(#342585,
#342586,#342587),(#342588,#342589,#342590),(#342591,#342592,#342593),(#342594,
#342595,#342596),(#342597,#342598,#342599),(#342600,#342601,#342602),(#342603,
#342604,#342605),(#342606,#342607,#342608),(#342609,#342610,#342611),(#342612,
#342613,#342614),(#342615,#342616,#342617),(#342618,#342619,#342620),(#342621,
#342622,#342623),(#342624,#342625,#342626),(#342627,#342628,#342629),(#342630,
#342631,#342632),(#342633,#342634,#342635),(#342636,#342637,#342638),(#342639,
#342640,#342641),(#342642,#342643,#342644),(#342645,#342646,#342647),(#342648,
#342649,#342650),(#342651,#342652,#342653),(#342654,#342655,#342656),(#342657,
#342658,#342659),(#342660,#342661,#342662),(#342663,#342664,#342665),(#342666,
#342667,#342668),(#342669,#342670,#342671),(#342672,#342673,#342674),(#342675,
#342676,#342677),(#342678,#342679,#342680),(#342681,#342682,#342683),(#342684,
#342685,#342686),(#342687,#342688,#342689),(#342690,#342691,#342692),(#342693,
#342694,#342695),(#342696,#342697,#342698),(#342699,#342700,#342701),(#342702,
#342703,#342704),(#342705,#342706,#342707),(#342708,#342709,#342710),(#342711,
#342712,#342713),(#342714,#342715,#342716),(#342717,#342718,#342719),(#342720,
#342721,#342722),(#342723,#342724,#342725),(#342726,#342727,#342728),(#342729,
#342730,#342731),(#342732,#342733,#342734),(#342735,#342736,#342737),(#342738,
#342739,#342740),(#342741,#342742,#342743),(#342744,#342745,#342746),(#342747,
#342748,#342749),(#342750,#342751,#342752),(#342753,#342754,#342755),(#342756,
#342757,#342758),(#342759,#342760,#342761),(#342762,#342763,#342764),(#342765,
#342766,#342767),(#342768,#342769,#342770),(#342771,#342772,#342773),(#342774,
#342775,#342776),(#342777,#342778,#342779),(#342780,#342781,#342782),(#342783,
#342784,#342785),(#342786,#342787,#342788),(#342789,#342790,#342791),(#342792,
#342793,#342794),(#342795,#342796,#342797),(#342798,#342799,#342800),(#342801,
#342802,#342803),(#342804,#342805,#342806),(#342807,#342808,#342809),(#342810,
#342811,#342812),(#342813,#342814,#342815),(#342816,#342817,#342818),(#342819,
#342820,#342821),(#342822,#342823,#342824),(#342825,#342826,#342827),(#342828,
#342829,#342830),(#342831,#342832,#342833),(#342834,#342835,#342836),(#342837,
#342838,#342839),(#342840,#342841,#342842),(#342843,#342844,#342845),(#342846,
#342847,#342848),(#342849,#342850,#342851),(#342852,#342853,#342854),(#342855,
#342856,#342857),(#342858,#342859,#342860),(#342861,#342862,#342863),(#342864,
#342865,#342866),(#342867,#342868,#342869),(#342870,#342871,#342872),(#342873,
#342874,#342875),(#342876,#342877,#342878),(#342879,#342880,#342881),(#342882,
#342883,#342884),(#342885,#342886,#342887),(#342888,#342889,#342890),(#342891,
#342892,#342893),(#342894,#342895,#342896),(#342897,#342898,#342899),(#342900,
#342901,#342902),(#342903,#342904,#342905),(#342906,#342907,#342908),(#342909,
#342910,#342911),(#342912,#342913,#342914),(#342915,#342916,#342917),(#342918,
#342919,#342920),(#342921,#342922,#342923),(#342924,#342925,#342926),(#342927,
#342928,#342929),(#342930,#342931,#342932),(#342933,#342934,#342935),(#342936,
#342937,#342938),(#342939,#342940,#342941),(#342942,#342943,#342944),(#342945,
#342946,#342947),(#342948,#342949,#342950),(#342951,#342952,#342953),(#342954,
#342955,#342956),(#342957,#342958,#342959),(#342960,#342961,#342962),(#342963,
#342964,#342965),(#342966,#342967,#342968),(#342969,#342970,#342971),(#342972,
#342973,#342974),(#342975,#342976,#342977),(#342978,#342979,#342980),(#342981,
#342982,#342983),(#342984,#342985,#342986),(#342987,#342988,#342989),(#342990,
#342991,#342992),(#342993,#342994,#342995),(#342996,#342997,#342998),(#342999,
#343000,#343001),(#343002,#343003,#343004),(#343005,#343006,#343007),(#343008,
#343009,#343010),(#343011,#343012,#343013),(#343014,#343015,#343016),(#343017,
#343018,#343019),(#343020,#343021,#343022),(#343023,#343024,#343025),(#343026,
#343027,#343028),(#343029,#343030,#343031),(#343032,#343033,#343034),(#343035,
#343036,#343037),(#343038,#343039,#343040),(#343041,#343042,#343043),(#343044,
#343045,#343046),(#343047,#343048,#343049),(#343050,#343051,#343052),(#343053,
#343054,#343055),(#343056,#343057,#343058),(#343059,#343060,#343061),(#343062,
#343063,#343064),(#343065,#343066,#343067),(#343068,#343069,#343070),(#343071,
#343072,#343073),(#343074,#343075,#343076),(#343077,#343078,#343079),(#343080,
#343081,#343082),(#343083,#343084,#343085),(#343086,#343087,#343088),(#343089,
#343090,#343091),(#343092,#343093,#343094),(#343095,#343096,#343097),(#343098,
#343099,#343100),(#343101,#343102,#343103),(#343104,#343105,#343106),(#343107,
#343108,#343109),(#343110,#343111,#343112),(#343113,#343114,#343115),(#343116,
#343117,#343118),(#343119,#343120,#343121),(#343122,#343123,#343124),(#343125,
#343126,#343127),(#343128,#343129,#343130),(#343131,#343132,#343133),(#343134,
#343135,#343136),(#343137,#343138,#343139),(#343140,#343141,#343142),(#343143,
#343144,#343145),(#343146,#343147,#343148),(#343149,#343150,#343151),(#343152,
#343153,#343154),(#343155,#343156,#343157),(#343158,#343159,#343160),(#343161,
#343162,#343163),(#343164,#343165,#343166),(#343167,#343168,#343169),(#343170,
#343171,#343172),(#343173,#343174,#343175),(#343176,#343177,#343178),(#343179,
#343180,#343181),(#343182,#343183,#343184),(#343185,#343186,#343187),(#343188,
#343189,#343190),(#343191,#343192,#343193),(#343194,#343195,#343196),(#343197,
#343198,#343199),(#343200,#343201,#343202),(#343203,#343204,#343205),(#343206,
#343207,#343208),(#343209,#343210,#343211),(#343212,#343213,#343214),(#343215,
#343216,#343217),(#343218,#343219,#343220),(#343221,#343222,#343223),(#343224,
#343225,#343226),(#343227,#343228,#343229),(#343230,#343231,#343232),(#343233,
#343234,#343235),(#343236,#343237,#343238),(#343239,#343240,#343241)),
 .UNSPECIFIED.,.F.,.F.,.F.,(6,1,1,1,1,1,1,1,1,1,1,1,1,1,1,1,1,1,1,1,1,1,
1,1,1,1,1,1,1,1,1,1,1,1,1,1,1,1,1,1,1,1,1,1,1,1,1,1,1,1,1,1,1,1,1,1,1,1,
1,1,1,1,1,1,1,1,1,1,1,1,1,1,1,1,1,1,1,1,1,1,1,1,1,1,1,1,1,1,1,1,1,1,1,1,
1,1,1,1,1,1,1,1,1,1,1,1,1,1,1,1,1,1,1,1,1,1,1,1,1,1,1,1,1,1,1,1,1,1,1,1,
1,1,1,1,1,1,1,1,1,1,1,1,1,1,1,1,1,1,1,1,1,1,1,1,1,1,1,1,1,1,1,1,1,1,1,1,
1,1,1,1,1,1,1,1,1,1,1,1,1,1,1,1,1,1,1,1,1,1,1,1,1,1,1,1,1,1,1,1,1,1,1,1,
1,1,1,1,1,1,1,1,1,1,1,1,1,1,1,1,1,1,1,1,1,1,1,1,1,1,1,1,1,1,1,1,1,1,1,1,
1,1,1,1,1,1,1,1,1,1,1,1,1,1,1,1,1,1,1,1,1,1,1,1,1,1,1,1,1,1,1,1,1,1,1,1,
1,1,1,1,1,1,1,1,1,1,1,1,1,1,1,1,1,1,1,1,1,1,1,1,1,1,1,1,1,1,1,1,1,1,1,1,
1,1,1,1,1,1,1,1,1,1,1,1,1,1,1,1,1,1,1,1,1,1,1,1,1,1,1,1,1,1,1,1,1,1,1,1,
1,1,1,1,1,1,1,1,1,1,1,1,1,1,1,1,1,1,1,1,1,1,1,1,1,1,1,1,1,1,1,1,1,1,1,1,
1,1,1,1,1,1,1,1,1,1,1,1,1,1,1,1,1,1,1,1,1,1,1,1,1,1,1,1,1,1,1,1,1,1,1,1,
1,1,1,1,1,1,1,1,1,1,1,1,1,1,1,1,1,1,1,1,1,1,1,1,1,1,1,1,1,1,1,1,1,1,1,1,
1,1,1,1,1,1,1,1,1,1,1,1,1,1,1,1,1,1,1,1,1,1,1,1,1,1,1,1,1,1,1,1,1,1,1,1,
1,1,1,1,1,1,1,1,1,1,1,1,1,1,1,1,1,1,1,1,1,1,1,1,1,1,1,1,1,1,1,1,1,1,1,1,
1,1,1,1,1,1,1,1,1,1,1,1,1,1,1,1,1,1,1,6),(2,1,2),(-1.,-0.998165138,-0.996330275,
-0.994495413,-0.99266055,-0.990825688,-0.988990826,-0.987155963,-0.985321101,
-0.983486239,-0.981651376,-0.979816514,-0.977981651,-0.976146789,-0.974311927,
-0.972477064,-0.970642202,-0.968807339,-0.966972477,-0.965137615,-0.963302752,
-0.96146789,-0.959633028,-0.957798165,-0.955963303,-0.95412844,-0.952293578,
-0.950458716,-0.948623853,-0.946788991,-0.944954128,-0.943119266,-0.941284404,
-0.939449541,-0.937614679,-0.935779817,-0.933944954,-0.932110092,-0.930275229,
-0.928440367,-0.926605505,-0.924770642,-0.92293578,-0.921100917,-0.919266055,
-0.917431193,-0.91559633,-0.913761468,-0.911926606,-0.910091743,-0.908256881,
-0.906422018,-0.904587156,-0.902752294,-0.900917431,-0.899082569,-0.897247706,
-0.895412844,-0.893577982,-0.891743119,-0.889908257,-0.888073394,-0.886238532,
-0.88440367,-0.882568807,-0.880733945,-0.878899083,-0.87706422,-0.875229358,
-0.873394495,-0.871559633,-0.869724771,-0.867889908,-0.866055046,-0.864220183,
-0.862385321,-0.860550459,-0.858715596,-0.856880734,-0.855045872,-0.853211009,
-0.851376147,-0.849541284,-0.847706422,-0.84587156,-0.844036697,-0.842201835,
-0.840366972,-0.83853211,-0.836697248,-0.834862385,-0.833027523,-0.831192661,
-0.829357798,-0.827522936,-0.825688073,-0.823853211,-0.822018349,-0.820183486,
-0.818348624,-0.816513761,-0.814678899,-0.812844037,-0.811009174,-0.809174312,
-0.80733945,-0.805504587,-0.803669725,-0.801834862,-0.8,-0.798165138,-0.796330275,
-0.794495413,-0.79266055,-0.790825688,-0.788990826,-0.787155963,-0.785321101,
-0.783486239,-0.781651376,-0.779816514,-0.777981651,-0.776146789,-0.774311927,
-0.772477064,-0.770642202,-0.768807339,-0.766972477,-0.765137615,-0.763302752,
-0.76146789,-0.759633028,-0.757798165,-0.755963303,-0.75412844,-0.752293578,
-0.750458716,-0.748623853,-0.746788991,-0.744954128,-0.743119266,-0.741284404,
-0.739449541,-0.737614679,-0.735779817,-0.733944954,-0.732110092,-0.730275229,
-0.728440367,-0.726605505,-0.724770642,-0.72293578,-0.721100917,-0.719266055,
-0.717431193,-0.71559633,-0.713761468,-0.711926606,-0.710091743,-0.708256881,
-0.706422018,-0.704587156,-0.702752294,-0.700917431,-0.699082569,-0.697247706,
-0.695412844,-0.693577982,-0.691743119,-0.689908257,-0.688073394,-0.686238532,
-0.68440367,-0.682568807,-0.680733945,-0.678899083,-0.67706422,-0.675229358,
-0.673394495,-0.671559633,-0.669724771,-0.667889908,-0.666055046,-0.664220183,
-0.662385321,-0.660550459,-0.658715596,-0.656880734,-0.655045872,-0.653211009,
-0.651376147,-0.649541284,-0.647706422,-0.64587156,-0.644036697,-0.642201835,
-0.640366972,-0.63853211,-0.636697248,-0.634862385,-0.633027523,-0.631192661,
-0.629357798,-0.627522936,-0.625688073,-0.623853211,-0.622018349,-0.620183486,
-0.618348624,-0.616513761,-0.614678899,-0.612844037,-0.611009174,-0.609174312,
-0.60733945,-0.605504587,-0.603669725,-0.601834862,-0.6,-0.598165138,-0.596330275,
-0.594495413,-0.59266055,-0.590825688,-0.588990826,-0.587155963,-0.585321101,
-0.583486239,-0.581651376,-0.579816514,-0.577981651,-0.576146789,-0.574311927,
-0.572477064,-0.570642202,-0.568807339,-0.566972477,-0.565137615,-0.563302752,
-0.56146789,-0.559633028,-0.557798165,-0.555963303,-0.55412844,-0.552293578,
-0.550458716,-0.548623853,-0.546788991,-0.544954128,-0.543119266,-0.541284404,
-0.539449541,-0.537614679,-0.535779817,-0.533944954,-0.532110092,-0.530275229,
-0.528440367,-0.526605505,-0.524770642,-0.52293578,-0.521100917,-0.519266055,
-0.517431193,-0.51559633,-0.513761468,-0.511926606,-0.510091743,-0.508256881,
-0.506422018,-0.504587156,-0.502752294,-0.500917431,-0.499082569,-0.497247706,
-0.495412844,-0.493577982,-0.491743119,-0.489908257,-0.488073394,-0.486238532,
-0.48440367,-0.482568807,-0.480733945,-0.478899083,-0.47706422,-0.475229358,
-0.473394495,-0.471559633,-0.469724771,-0.467889908,-0.466055046,-0.464220183,
-0.462385321,-0.460550459,-0.458715596,-0.456880734,-0.455045872,-0.453211009,
-0.451376147,-0.449541284,-0.447706422,-0.44587156,-0.444036697,-0.442201835,
-0.440366972,-0.43853211,-0.436697248,-0.434862385,-0.433027523,-0.431192661,
-0.429357798,-0.427522936,-0.425688073,-0.423853211,-0.422018349,-0.420183486,
-0.418348624,-0.416513761,-0.414678899,-0.412844037,-0.411009174,-0.409174312,
-0.40733945,-0.405504587,-0.403669725,-0.401834862,-0.4,-0.398165138,-0.396330275,
-0.394495413,-0.39266055,-0.390825688,-0.388990826,-0.387155963,-0.385321101,
-0.383486239,-0.381651376,-0.379816514,-0.377981651,-0.376146789,-0.374311927,
-0.372477064,-0.370642202,-0.368807339,-0.366972477,-0.365137615,-0.363302752,
-0.36146789,-0.359633028,-0.357798165,-0.355963303,-0.35412844,-0.352293578,
-0.350458716,-0.348623853,-0.346788991,-0.344954128,-0.343119266,-0.341284404,
-0.339449541,-0.337614679,-0.335779817,-0.333944954,-0.332110092,-0.330275229,
-0.328440367,-0.326605505,-0.324770642,-0.32293578,-0.321100917,-0.319266055,
-0.317431193,-0.31559633,-0.313761468,-0.311926606,-0.310091743,-0.308256881,
-0.306422018,-0.304587156,-0.302752294,-0.300917431,-0.299082569,-0.297247706,
-0.295412844,-0.293577982,-0.291743119,-0.289908257,-0.288073394,-0.286238532,
-0.28440367,-0.282568807,-0.280733945,-0.278899083,-0.27706422,-0.275229358,
-0.273394495,-0.271559633,-0.269724771,-0.267889908,-0.266055046,-0.264220183,
-0.262385321,-0.260550459,-0.258715596,-0.256880734,-0.255045872,-0.253211009,
-0.251376147,-0.249541284,-0.247706422,-0.24587156,-0.244036697,-0.242201835,
-0.240366972,-0.23853211,-0.236697248,-0.234862385,-0.233027523,-0.231192661,
-0.229357798,-0.227522936,-0.225688073,-0.223853211,-0.222018349,-0.220183486,
-0.218348624,-0.216513761,-0.214678899,-0.212844037,-0.211009174,-0.209174312,
-0.20733945,-0.205504587,-0.203669725,-0.201834862,-0.2,-0.198165138,-0.196330275,
-0.194495413,-0.19266055,-0.190825688,-0.188990826,-0.187155963,-0.185321101,
-0.183486239,-0.181651376,-0.179816514,-0.177981651,-0.176146789,-0.174311927,
-0.172477064,-0.170642202,-0.168807339,-0.166972477,-0.165137615,-0.163302752,
-0.16146789,-0.159633028,-0.157798165,-0.155963303,-0.15412844,-0.152293578,
-0.150458716,-0.148623853,-0.146788991,-0.144954128,-0.143119266,-0.141284404,
-0.139449541,-0.137614679,-0.135779817,-0.133944954,-0.132110092,-0.130275229,
-0.128440367,-0.126605505,-0.124770642,-0.12293578,-0.121100917,-0.119266055,
-0.117431193,-0.11559633,-0.113761468,-0.111926606,-0.110091743,-0.108256881,
-0.106422018,-0.104587156,-0.102752294,-0.100917431,-0.099082569,-0.097247706,
-0.095412844,-0.093577982,-0.091743119,-0.089908257,-0.088073394,-0.086238532,
-0.08440367,-0.082568807,-0.080733945,-0.078899083,-0.07706422,-0.075229358,
-0.073394495,-0.071559633,-0.069724771,-0.067889908,-0.066055046,-0.064220183,
-0.062385321,-0.060550459,-0.058715596,-0.056880734,-0.055045872,-0.053211009,
-0.051376147,-0.049541284,-0.047706422,-0.04587156,-0.044036697,-0.042201835,
-0.040366972,-0.03853211,-0.036697248,-0.034862385,-0.033027523,-0.031192661,
-0.029357798,-0.027522936,-0.025688073,-0.023853211,-0.022018349,-0.020183486,
-0.018348624,-0.016513761,-0.014678899,-0.012844037,-0.011009174,-0.009174312,
-0.00733945,-0.005504587,-0.003669725,-0.001834862,0.),(0.3,1.,1.3),
 .UNSPECIFIED.);
#6328=B_SPLINE_SURFACE_WITH_KNOTS('',5,1,((#343245,#343246,#343247),(#343248,
#343249,#343250),(#343251,#343252,#343253),(#343254,#343255,#343256),(#343257,
#343258,#343259),(#343260,#343261,#343262),(#343263,#343264,#343265),(#343266,
#343267,#343268),(#343269,#343270,#343271),(#343272,#343273,#343274),(#343275,
#343276,#343277),(#343278,#343279,#343280),(#343281,#343282,#343283),(#343284,
#343285,#343286),(#343287,#343288,#343289),(#343290,#343291,#343292),(#343293,
#343294,#343295),(#343296,#343297,#343298),(#343299,#343300,#343301),(#343302,
#343303,#343304),(#343305,#343306,#343307),(#343308,#343309,#343310),(#343311,
#343312,#343313),(#343314,#343315,#343316),(#343317,#343318,#343319),(#343320,
#343321,#343322),(#343323,#343324,#343325),(#343326,#343327,#343328),(#343329,
#343330,#343331),(#343332,#343333,#343334),(#343335,#343336,#343337),(#343338,
#343339,#343340),(#343341,#343342,#343343),(#343344,#343345,#343346),(#343347,
#343348,#343349),(#343350,#343351,#343352),(#343353,#343354,#343355),(#343356,
#343357,#343358),(#343359,#343360,#343361),(#343362,#343363,#343364),(#343365,
#343366,#343367),(#343368,#343369,#343370),(#343371,#343372,#343373),(#343374,
#343375,#343376),(#343377,#343378,#343379),(#343380,#343381,#343382),(#343383,
#343384,#343385),(#343386,#343387,#343388),(#343389,#343390,#343391),(#343392,
#343393,#343394),(#343395,#343396,#343397),(#343398,#343399,#343400),(#343401,
#343402,#343403),(#343404,#343405,#343406),(#343407,#343408,#343409),(#343410,
#343411,#343412),(#343413,#343414,#343415),(#343416,#343417,#343418),(#343419,
#343420,#343421),(#343422,#343423,#343424),(#343425,#343426,#343427),(#343428,
#343429,#343430),(#343431,#343432,#343433),(#343434,#343435,#343436),(#343437,
#343438,#343439),(#343440,#343441,#343442),(#343443,#343444,#343445),(#343446,
#343447,#343448),(#343449,#343450,#343451),(#343452,#343453,#343454),(#343455,
#343456,#343457),(#343458,#343459,#343460),(#343461,#343462,#343463),(#343464,
#343465,#343466),(#343467,#343468,#343469),(#343470,#343471,#343472),(#343473,
#343474,#343475),(#343476,#343477,#343478),(#343479,#343480,#343481),(#343482,
#343483,#343484),(#343485,#343486,#343487),(#343488,#343489,#343490),(#343491,
#343492,#343493),(#343494,#343495,#343496),(#343497,#343498,#343499),(#343500,
#343501,#343502),(#343503,#343504,#343505),(#343506,#343507,#343508),(#343509,
#343510,#343511),(#343512,#343513,#343514),(#343515,#343516,#343517),(#343518,
#343519,#343520),(#343521,#343522,#343523),(#343524,#343525,#343526),(#343527,
#343528,#343529),(#343530,#343531,#343532),(#343533,#343534,#343535),(#343536,
#343537,#343538),(#343539,#343540,#343541),(#343542,#343543,#343544),(#343545,
#343546,#343547),(#343548,#343549,#343550),(#343551,#343552,#343553),(#343554,
#343555,#343556),(#343557,#343558,#343559),(#343560,#343561,#343562),(#343563,
#343564,#343565),(#343566,#343567,#343568),(#343569,#343570,#343571),(#343572,
#343573,#343574),(#343575,#343576,#343577),(#343578,#343579,#343580),(#343581,
#343582,#343583),(#343584,#343585,#343586),(#343587,#343588,#343589),(#343590,
#343591,#343592),(#343593,#343594,#343595),(#343596,#343597,#343598),(#343599,
#343600,#343601),(#343602,#343603,#343604),(#343605,#343606,#343607),(#343608,
#343609,#343610),(#343611,#343612,#343613),(#343614,#343615,#343616),(#343617,
#343618,#343619),(#343620,#343621,#343622),(#343623,#343624,#343625),(#343626,
#343627,#343628),(#343629,#343630,#343631),(#343632,#343633,#343634),(#343635,
#343636,#343637),(#343638,#343639,#343640),(#343641,#343642,#343643),(#343644,
#343645,#343646),(#343647,#343648,#343649),(#343650,#343651,#343652),(#343653,
#343654,#343655),(#343656,#343657,#343658),(#343659,#343660,#343661),(#343662,
#343663,#343664),(#343665,#343666,#343667),(#343668,#343669,#343670),(#343671,
#343672,#343673),(#343674,#343675,#343676),(#343677,#343678,#343679),(#343680,
#343681,#343682),(#343683,#343684,#343685),(#343686,#343687,#343688),(#343689,
#343690,#343691),(#343692,#343693,#343694),(#343695,#343696,#343697),(#343698,
#343699,#343700),(#343701,#343702,#343703),(#343704,#343705,#343706),(#343707,
#343708,#343709),(#343710,#343711,#343712),(#343713,#343714,#343715),(#343716,
#343717,#343718),(#343719,#343720,#343721),(#343722,#343723,#343724),(#343725,
#343726,#343727),(#343728,#343729,#343730),(#343731,#343732,#343733),(#343734,
#343735,#343736),(#343737,#343738,#343739),(#343740,#343741,#343742),(#343743,
#343744,#343745),(#343746,#343747,#343748),(#343749,#343750,#343751),(#343752,
#343753,#343754),(#343755,#343756,#343757),(#343758,#343759,#343760),(#343761,
#343762,#343763),(#343764,#343765,#343766),(#343767,#343768,#343769),(#343770,
#343771,#343772),(#343773,#343774,#343775),(#343776,#343777,#343778),(#343779,
#343780,#343781),(#343782,#343783,#343784),(#343785,#343786,#343787),(#343788,
#343789,#343790),(#343791,#343792,#343793),(#343794,#343795,#343796),(#343797,
#343798,#343799),(#343800,#343801,#343802),(#343803,#343804,#343805),(#343806,
#343807,#343808),(#343809,#343810,#343811),(#343812,#343813,#343814),(#343815,
#343816,#343817),(#343818,#343819,#343820),(#343821,#343822,#343823),(#343824,
#343825,#343826),(#343827,#343828,#343829),(#343830,#343831,#343832),(#343833,
#343834,#343835),(#343836,#343837,#343838),(#343839,#343840,#343841),(#343842,
#343843,#343844),(#343845,#343846,#343847),(#343848,#343849,#343850),(#343851,
#343852,#343853),(#343854,#343855,#343856),(#343857,#343858,#343859),(#343860,
#343861,#343862),(#343863,#343864,#343865),(#343866,#343867,#343868),(#343869,
#343870,#343871),(#343872,#343873,#343874),(#343875,#343876,#343877),(#343878,
#343879,#343880),(#343881,#343882,#343883),(#343884,#343885,#343886),(#343887,
#343888,#343889),(#343890,#343891,#343892),(#343893,#343894,#343895),(#343896,
#343897,#343898),(#343899,#343900,#343901),(#343902,#343903,#343904),(#343905,
#343906,#343907),(#343908,#343909,#343910),(#343911,#343912,#343913),(#343914,
#343915,#343916),(#343917,#343918,#343919),(#343920,#343921,#343922),(#343923,
#343924,#343925),(#343926,#343927,#343928),(#343929,#343930,#343931),(#343932,
#343933,#343934),(#343935,#343936,#343937),(#343938,#343939,#343940),(#343941,
#343942,#343943),(#343944,#343945,#343946),(#343947,#343948,#343949),(#343950,
#343951,#343952),(#343953,#343954,#343955),(#343956,#343957,#343958),(#343959,
#343960,#343961),(#343962,#343963,#343964),(#343965,#343966,#343967),(#343968,
#343969,#343970),(#343971,#343972,#343973),(#343974,#343975,#343976),(#343977,
#343978,#343979),(#343980,#343981,#343982),(#343983,#343984,#343985),(#343986,
#343987,#343988),(#343989,#343990,#343991),(#343992,#343993,#343994),(#343995,
#343996,#343997),(#343998,#343999,#344000),(#344001,#344002,#344003),(#344004,
#344005,#344006),(#344007,#344008,#344009),(#344010,#344011,#344012),(#344013,
#344014,#344015),(#344016,#344017,#344018),(#344019,#344020,#344021),(#344022,
#344023,#344024),(#344025,#344026,#344027),(#344028,#344029,#344030),(#344031,
#344032,#344033),(#344034,#344035,#344036),(#344037,#344038,#344039),(#344040,
#344041,#344042),(#344043,#344044,#344045),(#344046,#344047,#344048),(#344049,
#344050,#344051),(#344052,#344053,#344054),(#344055,#344056,#344057),(#344058,
#344059,#344060),(#344061,#344062,#344063),(#344064,#344065,#344066),(#344067,
#344068,#344069),(#344070,#344071,#344072),(#344073,#344074,#344075),(#344076,
#344077,#344078),(#344079,#344080,#344081),(#344082,#344083,#344084),(#344085,
#344086,#344087),(#344088,#344089,#344090),(#344091,#344092,#344093),(#344094,
#344095,#344096),(#344097,#344098,#344099),(#344100,#344101,#344102),(#344103,
#344104,#344105),(#344106,#344107,#344108),(#344109,#344110,#344111),(#344112,
#344113,#344114),(#344115,#344116,#344117),(#344118,#344119,#344120),(#344121,
#344122,#344123),(#344124,#344125,#344126),(#344127,#344128,#344129),(#344130,
#344131,#344132),(#344133,#344134,#344135),(#344136,#344137,#344138),(#344139,
#344140,#344141),(#344142,#344143,#344144),(#344145,#344146,#344147),(#344148,
#344149,#344150),(#344151,#344152,#344153),(#344154,#344155,#344156),(#344157,
#344158,#344159),(#344160,#344161,#344162),(#344163,#344164,#344165),(#344166,
#344167,#344168),(#344169,#344170,#344171),(#344172,#344173,#344174),(#344175,
#344176,#344177),(#344178,#344179,#344180),(#344181,#344182,#344183),(#344184,
#344185,#344186),(#344187,#344188,#344189),(#344190,#344191,#344192),(#344193,
#344194,#344195),(#344196,#344197,#344198),(#344199,#344200,#344201),(#344202,
#344203,#344204),(#344205,#344206,#344207),(#344208,#344209,#344210),(#344211,
#344212,#344213),(#344214,#344215,#344216),(#344217,#344218,#344219),(#344220,
#344221,#344222),(#344223,#344224,#344225),(#344226,#344227,#344228),(#344229,
#344230,#344231),(#344232,#344233,#344234),(#344235,#344236,#344237),(#344238,
#344239,#344240),(#344241,#344242,#344243),(#344244,#344245,#344246),(#344247,
#344248,#344249),(#344250,#344251,#344252),(#344253,#344254,#344255),(#344256,
#344257,#344258),(#344259,#344260,#344261),(#344262,#344263,#344264),(#344265,
#344266,#344267),(#344268,#344269,#344270),(#344271,#344272,#344273),(#344274,
#344275,#344276),(#344277,#344278,#344279),(#344280,#344281,#344282),(#344283,
#344284,#344285),(#344286,#344287,#344288),(#344289,#344290,#344291),(#344292,
#344293,#344294),(#344295,#344296,#344297),(#344298,#344299,#344300),(#344301,
#344302,#344303),(#344304,#344305,#344306),(#344307,#344308,#344309),(#344310,
#344311,#344312),(#344313,#344314,#344315),(#344316,#344317,#344318),(#344319,
#344320,#344321),(#344322,#344323,#344324),(#344325,#344326,#344327),(#344328,
#344329,#344330),(#344331,#344332,#344333),(#344334,#344335,#344336),(#344337,
#344338,#344339),(#344340,#344341,#344342),(#344343,#344344,#344345),(#344346,
#344347,#344348),(#344349,#344350,#344351),(#344352,#344353,#344354),(#344355,
#344356,#344357),(#344358,#344359,#344360),(#344361,#344362,#344363),(#344364,
#344365,#344366),(#344367,#344368,#344369),(#344370,#344371,#344372),(#344373,
#344374,#344375),(#344376,#344377,#344378),(#344379,#344380,#344381),(#344382,
#344383,#344384),(#344385,#344386,#344387),(#344388,#344389,#344390),(#344391,
#344392,#344393),(#344394,#344395,#344396),(#344397,#344398,#344399),(#344400,
#344401,#344402),(#344403,#344404,#344405),(#344406,#344407,#344408),(#344409,
#344410,#344411),(#344412,#344413,#344414),(#344415,#344416,#344417),(#344418,
#344419,#344420),(#344421,#344422,#344423),(#344424,#344425,#344426),(#344427,
#344428,#344429),(#344430,#344431,#344432),(#344433,#344434,#344435),(#344436,
#344437,#344438),(#344439,#344440,#344441),(#344442,#344443,#344444),(#344445,
#344446,#344447),(#344448,#344449,#344450),(#344451,#344452,#344453),(#344454,
#344455,#344456),(#344457,#344458,#344459),(#344460,#344461,#344462),(#344463,
#344464,#344465),(#344466,#344467,#344468),(#344469,#344470,#344471),(#344472,
#344473,#344474),(#344475,#344476,#344477),(#344478,#344479,#344480),(#344481,
#344482,#344483),(#344484,#344485,#344486),(#344487,#344488,#344489),(#344490,
#344491,#344492),(#344493,#344494,#344495),(#344496,#344497,#344498),(#344499,
#344500,#344501),(#344502,#344503,#344504),(#344505,#344506,#344507),(#344508,
#344509,#344510),(#344511,#344512,#344513),(#344514,#344515,#344516),(#344517,
#344518,#344519),(#344520,#344521,#344522),(#344523,#344524,#344525),(#344526,
#344527,#344528),(#344529,#344530,#344531),(#344532,#344533,#344534),(#344535,
#344536,#344537),(#344538,#344539,#344540),(#344541,#344542,#344543),(#344544,
#344545,#344546),(#344547,#344548,#344549),(#344550,#344551,#344552),(#344553,
#344554,#344555),(#344556,#344557,#344558),(#344559,#344560,#344561),(#344562,
#344563,#344564),(#344565,#344566,#344567),(#344568,#344569,#344570),(#344571,
#344572,#344573),(#344574,#344575,#344576),(#344577,#344578,#344579),(#344580,
#344581,#344582),(#344583,#344584,#344585),(#344586,#344587,#344588),(#344589,
#344590,#344591),(#344592,#344593,#344594),(#344595,#344596,#344597),(#344598,
#344599,#344600),(#344601,#344602,#344603),(#344604,#344605,#344606),(#344607,
#344608,#344609),(#344610,#344611,#344612),(#344613,#344614,#344615),(#344616,
#344617,#344618),(#344619,#344620,#344621),(#344622,#344623,#344624),(#344625,
#344626,#344627),(#344628,#344629,#344630),(#344631,#344632,#344633),(#344634,
#344635,#344636),(#344637,#344638,#344639),(#344640,#344641,#344642),(#344643,
#344644,#344645),(#344646,#344647,#344648),(#344649,#344650,#344651),(#344652,
#344653,#344654),(#344655,#344656,#344657),(#344658,#344659,#344660),(#344661,
#344662,#344663),(#344664,#344665,#344666),(#344667,#344668,#344669),(#344670,
#344671,#344672),(#344673,#344674,#344675),(#344676,#344677,#344678),(#344679,
#344680,#344681),(#344682,#344683,#344684),(#344685,#344686,#344687),(#344688,
#344689,#344690),(#344691,#344692,#344693),(#344694,#344695,#344696),(#344697,
#344698,#344699),(#344700,#344701,#344702),(#344703,#344704,#344705),(#344706,
#344707,#344708),(#344709,#344710,#344711),(#344712,#344713,#344714),(#344715,
#344716,#344717),(#344718,#344719,#344720),(#344721,#344722,#344723),(#344724,
#344725,#344726),(#344727,#344728,#344729),(#344730,#344731,#344732),(#344733,
#344734,#344735),(#344736,#344737,#344738),(#344739,#344740,#344741),(#344742,
#344743,#344744),(#344745,#344746,#344747),(#344748,#344749,#344750),(#344751,
#344752,#344753),(#344754,#344755,#344756),(#344757,#344758,#344759),(#344760,
#344761,#344762),(#344763,#344764,#344765),(#344766,#344767,#344768),(#344769,
#344770,#344771),(#344772,#344773,#344774),(#344775,#344776,#344777),(#344778,
#344779,#344780),(#344781,#344782,#344783),(#344784,#344785,#344786),(#344787,
#344788,#344789),(#344790,#344791,#344792),(#344793,#344794,#344795),(#344796,
#344797,#344798),(#344799,#344800,#344801),(#344802,#344803,#344804),(#344805,
#344806,#344807),(#344808,#344809,#344810),(#344811,#344812,#344813),(#344814,
#344815,#344816),(#344817,#344818,#344819),(#344820,#344821,#344822),(#344823,
#344824,#344825),(#344826,#344827,#344828),(#344829,#344830,#344831),(#344832,
#344833,#344834),(#344835,#344836,#344837),(#344838,#344839,#344840),(#344841,
#344842,#344843),(#344844,#344845,#344846),(#344847,#344848,#344849),(#344850,
#344851,#344852),(#344853,#344854,#344855),(#344856,#344857,#344858),(#344859,
#344860,#344861),(#344862,#344863,#344864),(#344865,#344866,#344867),(#344868,
#344869,#344870),(#344871,#344872,#344873),(#344874,#344875,#344876),(#344877,
#344878,#344879),(#344880,#344881,#344882),(#344883,#344884,#344885),(#344886,
#344887,#344888),(#344889,#344890,#344891),(#344892,#344893,#344894),(#344895,
#344896,#344897)),.UNSPECIFIED.,.F.,.F.,.F.,(6,1,1,1,1,1,1,1,1,1,1,1,1,
1,1,1,1,1,1,1,1,1,1,1,1,1,1,1,1,1,1,1,1,1,1,1,1,1,1,1,1,1,1,1,1,1,1,1,1,
1,1,1,1,1,1,1,1,1,1,1,1,1,1,1,1,1,1,1,1,1,1,1,1,1,1,1,1,1,1,1,1,1,1,1,1,
1,1,1,1,1,1,1,1,1,1,1,1,1,1,1,1,1,1,1,1,1,1,1,1,1,1,1,1,1,1,1,1,1,1,1,1,
1,1,1,1,1,1,1,1,1,1,1,1,1,1,1,1,1,1,1,1,1,1,1,1,1,1,1,1,1,1,1,1,1,1,1,1,
1,1,1,1,1,1,1,1,1,1,1,1,1,1,1,1,1,1,1,1,1,1,1,1,1,1,1,1,1,1,1,1,1,1,1,1,
1,1,1,1,1,1,1,1,1,1,1,1,1,1,1,1,1,1,1,1,1,1,1,1,1,1,1,1,1,1,1,1,1,1,1,1,
1,1,1,1,1,1,1,1,1,1,1,1,1,1,1,1,1,1,1,1,1,1,1,1,1,1,1,1,1,1,1,1,1,1,1,1,
1,1,1,1,1,1,1,1,1,1,1,1,1,1,1,1,1,1,1,1,1,1,1,1,1,1,1,1,1,1,1,1,1,1,1,1,
1,1,1,1,1,1,1,1,1,1,1,1,1,1,1,1,1,1,1,1,1,1,1,1,1,1,1,1,1,1,1,1,1,1,1,1,
1,1,1,1,1,1,1,1,1,1,1,1,1,1,1,1,1,1,1,1,1,1,1,1,1,1,1,1,1,1,1,1,1,1,1,1,
1,1,1,1,1,1,1,1,1,1,1,1,1,1,1,1,1,1,1,1,1,1,1,1,1,1,1,1,1,1,1,1,1,1,1,1,
1,1,1,1,1,1,1,1,1,1,1,1,1,1,1,1,1,1,1,1,1,1,1,1,1,1,1,1,1,1,1,1,1,1,1,1,
1,1,1,1,1,1,1,1,1,1,1,1,1,1,1,1,1,1,1,1,1,1,1,1,1,1,1,1,1,1,1,1,1,1,1,1,
1,1,1,1,1,1,1,1,1,1,1,1,1,1,1,1,1,1,1,1,1,1,1,1,1,1,1,1,1,1,1,1,1,1,1,1,
1,1,1,1,1,1,1,1,1,1,1,1,1,1,1,1,1,1,1,1,1,1,1,1,1,1,1,1,1,6),(2,1,2),(-0.00196417,
0.,0.001834862,0.003669725,0.005504587,0.00733945,0.009174312,0.011009174,
0.012844037,0.014678899,0.016513761,0.018348624,0.020183486,0.022018349,
0.023853211,0.025688073,0.027522936,0.029357798,0.031192661,0.033027523,
0.034862385,0.036697248,0.03853211,0.040366972,0.042201835,0.044036697,
0.04587156,0.047706422,0.049541284,0.051376147,0.053211009,0.055045872,
0.056880734,0.058715596,0.060550459,0.062385321,0.064220183,0.066055046,
0.067889908,0.069724771,0.071559633,0.073394495,0.075229358,0.07706422,
0.078899083,0.080733945,0.082568807,0.08440367,0.086238532,0.088073394,
0.089908257,0.091743119,0.093577982,0.095412844,0.097247706,0.099082569,
0.100917431,0.102752294,0.104587156,0.106422018,0.108256881,0.110091743,
0.111926606,0.113761468,0.11559633,0.117431193,0.119266055,0.121100917,
0.12293578,0.124770642,0.126605505,0.128440367,0.130275229,0.132110092,
0.133944954,0.135779817,0.137614679,0.139449541,0.141284404,0.143119266,
0.144954128,0.146788991,0.148623853,0.150458716,0.152293578,0.15412844,
0.155963303,0.157798165,0.159633028,0.16146789,0.163302752,0.165137615,
0.166972477,0.168807339,0.170642202,0.172477064,0.174311927,0.176146789,
0.177981651,0.179816514,0.181651376,0.183486239,0.185321101,0.187155963,
0.188990826,0.190825688,0.19266055,0.194495413,0.196330275,0.198165138,
0.2,0.201834862,0.203669725,0.205504587,0.20733945,0.209174312,0.211009174,
0.212844037,0.214678899,0.216513761,0.218348624,0.220183486,0.222018349,
0.223853211,0.225688073,0.227522936,0.229357798,0.231192661,0.233027523,
0.234862385,0.236697248,0.23853211,0.240366972,0.242201835,0.244036697,
0.24587156,0.247706422,0.249541284,0.251376147,0.253211009,0.255045872,
0.256880734,0.258715596,0.260550459,0.262385321,0.264220183,0.266055046,
0.267889908,0.269724771,0.271559633,0.273394495,0.275229358,0.27706422,
0.278899083,0.280733945,0.282568807,0.28440367,0.286238532,0.288073394,
0.289908257,0.291743119,0.293577982,0.295412844,0.297247706,0.299082569,
0.300917431,0.302752294,0.304587156,0.306422018,0.308256881,0.310091743,
0.311926606,0.313761468,0.31559633,0.317431193,0.319266055,0.321100917,
0.32293578,0.324770642,0.326605505,0.328440367,0.330275229,0.332110092,
0.333944954,0.335779817,0.337614679,0.339449541,0.341284404,0.343119266,
0.344954128,0.346788991,0.348623853,0.350458716,0.352293578,0.35412844,
0.355963303,0.357798165,0.359633028,0.36146789,0.363302752,0.365137615,
0.366972477,0.368807339,0.370642202,0.372477064,0.374311927,0.376146789,
0.377981651,0.379816514,0.381651376,0.383486239,0.385321101,0.387155963,
0.388990826,0.390825688,0.39266055,0.394495413,0.396330275,0.398165138,
0.4,0.401834862,0.403669725,0.405504587,0.40733945,0.409174312,0.411009174,
0.412844037,0.414678899,0.416513761,0.418348624,0.420183486,0.422018349,
0.423853211,0.425688073,0.427522936,0.429357798,0.431192661,0.433027523,
0.434862385,0.436697248,0.43853211,0.440366972,0.442201835,0.444036697,
0.44587156,0.447706422,0.449541284,0.451376147,0.453211009,0.455045872,
0.456880734,0.458715596,0.460550459,0.462385321,0.464220183,0.466055046,
0.467889908,0.469724771,0.471559633,0.473394495,0.475229358,0.47706422,
0.478899083,0.480733945,0.482568807,0.48440367,0.486238532,0.488073394,
0.489908257,0.491743119,0.493577982,0.495412844,0.497247706,0.499082569,
0.500917431,0.502752294,0.504587156,0.506422018,0.508256881,0.510091743,
0.511926606,0.513761468,0.51559633,0.517431193,0.519266055,0.521100917,
0.52293578,0.524770642,0.526605505,0.528440367,0.530275229,0.532110092,
0.533944954,0.535779817,0.537614679,0.539449541,0.541284404,0.543119266,
0.544954128,0.546788991,0.548623853,0.550458716,0.552293578,0.55412844,
0.555963303,0.557798165,0.559633028,0.56146789,0.563302752,0.565137615,
0.566972477,0.568807339,0.570642202,0.572477064,0.574311927,0.576146789,
0.577981651,0.579816514,0.581651376,0.583486239,0.585321101,0.587155963,
0.588990826,0.590825688,0.59266055,0.594495413,0.596330275,0.598165138,
0.6,0.601834862,0.603669725,0.605504587,0.60733945,0.609174312,0.611009174,
0.612844037,0.614678899,0.616513761,0.618348624,0.620183486,0.622018349,
0.623853211,0.625688073,0.627522936,0.629357798,0.631192661,0.633027523,
0.634862385,0.636697248,0.63853211,0.640366972,0.642201835,0.644036697,
0.64587156,0.647706422,0.649541284,0.651376147,0.653211009,0.655045872,
0.656880734,0.658715596,0.660550459,0.662385321,0.664220183,0.666055046,
0.667889908,0.669724771,0.671559633,0.673394495,0.675229358,0.67706422,
0.678899083,0.680733945,0.682568807,0.68440367,0.686238532,0.688073394,
0.689908257,0.691743119,0.693577982,0.695412844,0.697247706,0.699082569,
0.700917431,0.702752294,0.704587156,0.706422018,0.708256881,0.710091743,
0.711926606,0.713761468,0.71559633,0.717431193,0.719266055,0.721100917,
0.72293578,0.724770642,0.726605505,0.728440367,0.730275229,0.732110092,
0.733944954,0.735779817,0.737614679,0.739449541,0.741284404,0.743119266,
0.744954128,0.746788991,0.748623853,0.750458716,0.752293578,0.75412844,
0.755963303,0.757798165,0.759633028,0.76146789,0.763302752,0.765137615,
0.766972477,0.768807339,0.770642202,0.772477064,0.774311927,0.776146789,
0.777981651,0.779816514,0.781651376,0.783486239,0.785321101,0.787155963,
0.788990826,0.790825688,0.79266055,0.794495413,0.796330275,0.798165138,
0.8,0.801834862,0.803669725,0.805504587,0.80733945,0.809174312,0.811009174,
0.812844037,0.814678899,0.816513761,0.818348624,0.820183486,0.822018349,
0.823853211,0.825688073,0.827522936,0.829357798,0.831192661,0.833027523,
0.834862385,0.836697248,0.83853211,0.840366972,0.842201835,0.844036697,
0.84587156,0.847706422,0.849541284,0.851376147,0.853211009,0.855045872,
0.856880734,0.858715596,0.860550459,0.862385321,0.864220183,0.866055046,
0.867889908,0.869724771,0.871559633,0.873394495,0.875229358,0.87706422,
0.878899083,0.880733945,0.882568807,0.88440367,0.886238532,0.888073394,
0.889908257,0.891743119,0.893577982,0.895412844,0.897247706,0.899082569,
0.900917431,0.902752294,0.904587156,0.906422018,0.908256881,0.910091743,
0.911926606,0.913761468,0.91559633,0.917431193,0.919266055,0.921100917,
0.92293578,0.924770642,0.926605505,0.928440367,0.930275229,0.932110092,
0.933944954,0.935779817,0.937614679,0.939449541,0.941284404,0.943119266,
0.944954128,0.946788991,0.948623853,0.950458716,0.952293578,0.95412844,
0.955963303,0.957798165,0.959633028,0.96146789,0.963302752,0.965137615,
0.966972477,0.968807339,0.970642202,0.972477064,0.974311927,0.976146789,
0.977981651,0.979816514,0.981651376,0.983486239,0.985321101,0.987155963,
0.988990826,0.990825688,0.99266055,0.994495413,0.996330275,0.998165138,
1.000000000285),(0.3,1.,1.3),.UNSPECIFIED.);
#6329=B_SPLINE_SURFACE_WITH_KNOTS('',5,1,((#344909,#344910,#344911),(#344912,
#344913,#344914),(#344915,#344916,#344917),(#344918,#344919,#344920),(#344921,
#344922,#344923),(#344924,#344925,#344926),(#344927,#344928,#344929),(#344930,
#344931,#344932),(#344933,#344934,#344935),(#344936,#344937,#344938),(#344939,
#344940,#344941),(#344942,#344943,#344944),(#344945,#344946,#344947),(#344948,
#344949,#344950),(#344951,#344952,#344953),(#344954,#344955,#344956),(#344957,
#344958,#344959),(#344960,#344961,#344962),(#344963,#344964,#344965),(#344966,
#344967,#344968),(#344969,#344970,#344971),(#344972,#344973,#344974),(#344975,
#344976,#344977),(#344978,#344979,#344980),(#344981,#344982,#344983),(#344984,
#344985,#344986),(#344987,#344988,#344989),(#344990,#344991,#344992),(#344993,
#344994,#344995),(#344996,#344997,#344998),(#344999,#345000,#345001),(#345002,
#345003,#345004),(#345005,#345006,#345007),(#345008,#345009,#345010),(#345011,
#345012,#345013),(#345014,#345015,#345016),(#345017,#345018,#345019),(#345020,
#345021,#345022),(#345023,#345024,#345025),(#345026,#345027,#345028),(#345029,
#345030,#345031),(#345032,#345033,#345034),(#345035,#345036,#345037),(#345038,
#345039,#345040),(#345041,#345042,#345043),(#345044,#345045,#345046),(#345047,
#345048,#345049),(#345050,#345051,#345052),(#345053,#345054,#345055),(#345056,
#345057,#345058),(#345059,#345060,#345061),(#345062,#345063,#345064),(#345065,
#345066,#345067),(#345068,#345069,#345070),(#345071,#345072,#345073),(#345074,
#345075,#345076),(#345077,#345078,#345079),(#345080,#345081,#345082),(#345083,
#345084,#345085),(#345086,#345087,#345088),(#345089,#345090,#345091),(#345092,
#345093,#345094),(#345095,#345096,#345097),(#345098,#345099,#345100),(#345101,
#345102,#345103),(#345104,#345105,#345106),(#345107,#345108,#345109),(#345110,
#345111,#345112),(#345113,#345114,#345115),(#345116,#345117,#345118),(#345119,
#345120,#345121),(#345122,#345123,#345124),(#345125,#345126,#345127),(#345128,
#345129,#345130),(#345131,#345132,#345133),(#345134,#345135,#345136),(#345137,
#345138,#345139),(#345140,#345141,#345142),(#345143,#345144,#345145),(#345146,
#345147,#345148),(#345149,#345150,#345151),(#345152,#345153,#345154),(#345155,
#345156,#345157),(#345158,#345159,#345160),(#345161,#345162,#345163),(#345164,
#345165,#345166),(#345167,#345168,#345169),(#345170,#345171,#345172),(#345173,
#345174,#345175),(#345176,#345177,#345178),(#345179,#345180,#345181),(#345182,
#345183,#345184),(#345185,#345186,#345187),(#345188,#345189,#345190),(#345191,
#345192,#345193),(#345194,#345195,#345196),(#345197,#345198,#345199),(#345200,
#345201,#345202),(#345203,#345204,#345205),(#345206,#345207,#345208),(#345209,
#345210,#345211),(#345212,#345213,#345214),(#345215,#345216,#345217),(#345218,
#345219,#345220),(#345221,#345222,#345223),(#345224,#345225,#345226),(#345227,
#345228,#345229),(#345230,#345231,#345232),(#345233,#345234,#345235),(#345236,
#345237,#345238),(#345239,#345240,#345241),(#345242,#345243,#345244),(#345245,
#345246,#345247),(#345248,#345249,#345250),(#345251,#345252,#345253),(#345254,
#345255,#345256),(#345257,#345258,#345259),(#345260,#345261,#345262),(#345263,
#345264,#345265),(#345266,#345267,#345268),(#345269,#345270,#345271),(#345272,
#345273,#345274),(#345275,#345276,#345277),(#345278,#345279,#345280),(#345281,
#345282,#345283),(#345284,#345285,#345286),(#345287,#345288,#345289),(#345290,
#345291,#345292),(#345293,#345294,#345295),(#345296,#345297,#345298),(#345299,
#345300,#345301),(#345302,#345303,#345304),(#345305,#345306,#345307),(#345308,
#345309,#345310),(#345311,#345312,#345313),(#345314,#345315,#345316),(#345317,
#345318,#345319),(#345320,#345321,#345322),(#345323,#345324,#345325),(#345326,
#345327,#345328),(#345329,#345330,#345331),(#345332,#345333,#345334),(#345335,
#345336,#345337),(#345338,#345339,#345340),(#345341,#345342,#345343),(#345344,
#345345,#345346),(#345347,#345348,#345349),(#345350,#345351,#345352),(#345353,
#345354,#345355),(#345356,#345357,#345358),(#345359,#345360,#345361),(#345362,
#345363,#345364),(#345365,#345366,#345367),(#345368,#345369,#345370),(#345371,
#345372,#345373),(#345374,#345375,#345376),(#345377,#345378,#345379),(#345380,
#345381,#345382),(#345383,#345384,#345385),(#345386,#345387,#345388),(#345389,
#345390,#345391),(#345392,#345393,#345394),(#345395,#345396,#345397),(#345398,
#345399,#345400),(#345401,#345402,#345403),(#345404,#345405,#345406),(#345407,
#345408,#345409),(#345410,#345411,#345412),(#345413,#345414,#345415),(#345416,
#345417,#345418),(#345419,#345420,#345421),(#345422,#345423,#345424),(#345425,
#345426,#345427),(#345428,#345429,#345430),(#345431,#345432,#345433),(#345434,
#345435,#345436),(#345437,#345438,#345439),(#345440,#345441,#345442),(#345443,
#345444,#345445),(#345446,#345447,#345448),(#345449,#345450,#345451),(#345452,
#345453,#345454),(#345455,#345456,#345457),(#345458,#345459,#345460),(#345461,
#345462,#345463),(#345464,#345465,#345466),(#345467,#345468,#345469),(#345470,
#345471,#345472),(#345473,#345474,#345475),(#345476,#345477,#345478),(#345479,
#345480,#345481),(#345482,#345483,#345484),(#345485,#345486,#345487),(#345488,
#345489,#345490),(#345491,#345492,#345493),(#345494,#345495,#345496),(#345497,
#345498,#345499),(#345500,#345501,#345502),(#345503,#345504,#345505),(#345506,
#345507,#345508),(#345509,#345510,#345511),(#345512,#345513,#345514),(#345515,
#345516,#345517),(#345518,#345519,#345520),(#345521,#345522,#345523),(#345524,
#345525,#345526),(#345527,#345528,#345529),(#345530,#345531,#345532),(#345533,
#345534,#345535),(#345536,#345537,#345538),(#345539,#345540,#345541),(#345542,
#345543,#345544),(#345545,#345546,#345547),(#345548,#345549,#345550),(#345551,
#345552,#345553),(#345554,#345555,#345556),(#345557,#345558,#345559),(#345560,
#345561,#345562),(#345563,#345564,#345565),(#345566,#345567,#345568),(#345569,
#345570,#345571),(#345572,#345573,#345574),(#345575,#345576,#345577),(#345578,
#345579,#345580),(#345581,#345582,#345583),(#345584,#345585,#345586),(#345587,
#345588,#345589),(#345590,#345591,#345592),(#345593,#345594,#345595),(#345596,
#345597,#345598),(#345599,#345600,#345601),(#345602,#345603,#345604),(#345605,
#345606,#345607),(#345608,#345609,#345610),(#345611,#345612,#345613),(#345614,
#345615,#345616),(#345617,#345618,#345619),(#345620,#345621,#345622),(#345623,
#345624,#345625),(#345626,#345627,#345628),(#345629,#345630,#345631),(#345632,
#345633,#345634),(#345635,#345636,#345637),(#345638,#345639,#345640),(#345641,
#345642,#345643),(#345644,#345645,#345646),(#345647,#345648,#345649),(#345650,
#345651,#345652),(#345653,#345654,#345655),(#345656,#345657,#345658),(#345659,
#345660,#345661),(#345662,#345663,#345664),(#345665,#345666,#345667),(#345668,
#345669,#345670),(#345671,#345672,#345673),(#345674,#345675,#345676),(#345677,
#345678,#345679),(#345680,#345681,#345682),(#345683,#345684,#345685),(#345686,
#345687,#345688),(#345689,#345690,#345691),(#345692,#345693,#345694),(#345695,
#345696,#345697),(#345698,#345699,#345700),(#345701,#345702,#345703),(#345704,
#345705,#345706),(#345707,#345708,#345709),(#345710,#345711,#345712),(#345713,
#345714,#345715),(#345716,#345717,#345718),(#345719,#345720,#345721),(#345722,
#345723,#345724),(#345725,#345726,#345727),(#345728,#345729,#345730),(#345731,
#345732,#345733),(#345734,#345735,#345736),(#345737,#345738,#345739),(#345740,
#345741,#345742),(#345743,#345744,#345745),(#345746,#345747,#345748),(#345749,
#345750,#345751),(#345752,#345753,#345754),(#345755,#345756,#345757),(#345758,
#345759,#345760),(#345761,#345762,#345763),(#345764,#345765,#345766),(#345767,
#345768,#345769),(#345770,#345771,#345772),(#345773,#345774,#345775),(#345776,
#345777,#345778),(#345779,#345780,#345781),(#345782,#345783,#345784),(#345785,
#345786,#345787),(#345788,#345789,#345790),(#345791,#345792,#345793),(#345794,
#345795,#345796),(#345797,#345798,#345799),(#345800,#345801,#345802),(#345803,
#345804,#345805),(#345806,#345807,#345808),(#345809,#345810,#345811),(#345812,
#345813,#345814),(#345815,#345816,#345817),(#345818,#345819,#345820),(#345821,
#345822,#345823),(#345824,#345825,#345826),(#345827,#345828,#345829),(#345830,
#345831,#345832),(#345833,#345834,#345835),(#345836,#345837,#345838),(#345839,
#345840,#345841),(#345842,#345843,#345844),(#345845,#345846,#345847),(#345848,
#345849,#345850),(#345851,#345852,#345853),(#345854,#345855,#345856),(#345857,
#345858,#345859),(#345860,#345861,#345862),(#345863,#345864,#345865),(#345866,
#345867,#345868),(#345869,#345870,#345871),(#345872,#345873,#345874),(#345875,
#345876,#345877),(#345878,#345879,#345880),(#345881,#345882,#345883),(#345884,
#345885,#345886),(#345887,#345888,#345889),(#345890,#345891,#345892),(#345893,
#345894,#345895),(#345896,#345897,#345898),(#345899,#345900,#345901),(#345902,
#345903,#345904),(#345905,#345906,#345907),(#345908,#345909,#345910),(#345911,
#345912,#345913),(#345914,#345915,#345916),(#345917,#345918,#345919),(#345920,
#345921,#345922),(#345923,#345924,#345925),(#345926,#345927,#345928),(#345929,
#345930,#345931),(#345932,#345933,#345934),(#345935,#345936,#345937),(#345938,
#345939,#345940),(#345941,#345942,#345943),(#345944,#345945,#345946),(#345947,
#345948,#345949),(#345950,#345951,#345952),(#345953,#345954,#345955),(#345956,
#345957,#345958),(#345959,#345960,#345961),(#345962,#345963,#345964),(#345965,
#345966,#345967),(#345968,#345969,#345970),(#345971,#345972,#345973),(#345974,
#345975,#345976),(#345977,#345978,#345979),(#345980,#345981,#345982),(#345983,
#345984,#345985),(#345986,#345987,#345988),(#345989,#345990,#345991),(#345992,
#345993,#345994),(#345995,#345996,#345997),(#345998,#345999,#346000),(#346001,
#346002,#346003),(#346004,#346005,#346006),(#346007,#346008,#346009),(#346010,
#346011,#346012),(#346013,#346014,#346015),(#346016,#346017,#346018),(#346019,
#346020,#346021),(#346022,#346023,#346024),(#346025,#346026,#346027),(#346028,
#346029,#346030),(#346031,#346032,#346033),(#346034,#346035,#346036),(#346037,
#346038,#346039),(#346040,#346041,#346042),(#346043,#346044,#346045),(#346046,
#346047,#346048),(#346049,#346050,#346051),(#346052,#346053,#346054),(#346055,
#346056,#346057),(#346058,#346059,#346060),(#346061,#346062,#346063),(#346064,
#346065,#346066),(#346067,#346068,#346069),(#346070,#346071,#346072),(#346073,
#346074,#346075),(#346076,#346077,#346078),(#346079,#346080,#346081),(#346082,
#346083,#346084),(#346085,#346086,#346087),(#346088,#346089,#346090),(#346091,
#346092,#346093),(#346094,#346095,#346096),(#346097,#346098,#346099),(#346100,
#346101,#346102),(#346103,#346104,#346105),(#346106,#346107,#346108),(#346109,
#346110,#346111),(#346112,#346113,#346114),(#346115,#346116,#346117),(#346118,
#346119,#346120),(#346121,#346122,#346123),(#346124,#346125,#346126),(#346127,
#346128,#346129),(#346130,#346131,#346132),(#346133,#346134,#346135),(#346136,
#346137,#346138),(#346139,#346140,#346141),(#346142,#346143,#346144),(#346145,
#346146,#346147),(#346148,#346149,#346150),(#346151,#346152,#346153),(#346154,
#346155,#346156),(#346157,#346158,#346159),(#346160,#346161,#346162),(#346163,
#346164,#346165),(#346166,#346167,#346168),(#346169,#346170,#346171),(#346172,
#346173,#346174),(#346175,#346176,#346177),(#346178,#346179,#346180),(#346181,
#346182,#346183),(#346184,#346185,#346186),(#346187,#346188,#346189),(#346190,
#346191,#346192),(#346193,#346194,#346195),(#346196,#346197,#346198),(#346199,
#346200,#346201),(#346202,#346203,#346204),(#346205,#346206,#346207),(#346208,
#346209,#346210),(#346211,#346212,#346213),(#346214,#346215,#346216),(#346217,
#346218,#346219),(#346220,#346221,#346222),(#346223,#346224,#346225),(#346226,
#346227,#346228),(#346229,#346230,#346231),(#346232,#346233,#346234),(#346235,
#346236,#346237),(#346238,#346239,#346240),(#346241,#346242,#346243),(#346244,
#346245,#346246),(#346247,#346248,#346249),(#346250,#346251,#346252),(#346253,
#346254,#346255),(#346256,#346257,#346258),(#346259,#346260,#346261),(#346262,
#346263,#346264),(#346265,#346266,#346267),(#346268,#346269,#346270),(#346271,
#346272,#346273),(#346274,#346275,#346276),(#346277,#346278,#346279),(#346280,
#346281,#346282),(#346283,#346284,#346285),(#346286,#346287,#346288),(#346289,
#346290,#346291),(#346292,#346293,#346294),(#346295,#346296,#346297),(#346298,
#346299,#346300),(#346301,#346302,#346303),(#346304,#346305,#346306),(#346307,
#346308,#346309),(#346310,#346311,#346312),(#346313,#346314,#346315),(#346316,
#346317,#346318),(#346319,#346320,#346321),(#346322,#346323,#346324),(#346325,
#346326,#346327),(#346328,#346329,#346330),(#346331,#346332,#346333),(#346334,
#346335,#346336),(#346337,#346338,#346339),(#346340,#346341,#346342),(#346343,
#346344,#346345),(#346346,#346347,#346348),(#346349,#346350,#346351),(#346352,
#346353,#346354),(#346355,#346356,#346357),(#346358,#346359,#346360),(#346361,
#346362,#346363),(#346364,#346365,#346366),(#346367,#346368,#346369),(#346370,
#346371,#346372),(#346373,#346374,#346375),(#346376,#346377,#346378),(#346379,
#346380,#346381),(#346382,#346383,#346384),(#346385,#346386,#346387),(#346388,
#346389,#346390),(#346391,#346392,#346393),(#346394,#346395,#346396),(#346397,
#346398,#346399),(#346400,#346401,#346402),(#346403,#346404,#346405),(#346406,
#346407,#346408),(#346409,#346410,#346411),(#346412,#346413,#346414),(#346415,
#346416,#346417),(#346418,#346419,#346420),(#346421,#346422,#346423),(#346424,
#346425,#346426),(#346427,#346428,#346429),(#346430,#346431,#346432),(#346433,
#346434,#346435),(#346436,#346437,#346438),(#346439,#346440,#346441),(#346442,
#346443,#346444),(#346445,#346446,#346447),(#346448,#346449,#346450),(#346451,
#346452,#346453),(#346454,#346455,#346456),(#346457,#346458,#346459),(#346460,
#346461,#346462),(#346463,#346464,#346465),(#346466,#346467,#346468),(#346469,
#346470,#346471),(#346472,#346473,#346474),(#346475,#346476,#346477),(#346478,
#346479,#346480),(#346481,#346482,#346483),(#346484,#346485,#346486),(#346487,
#346488,#346489),(#346490,#346491,#346492),(#346493,#346494,#346495),(#346496,
#346497,#346498),(#346499,#346500,#346501),(#346502,#346503,#346504),(#346505,
#346506,#346507),(#346508,#346509,#346510),(#346511,#346512,#346513),(#346514,
#346515,#346516),(#346517,#346518,#346519),(#346520,#346521,#346522),(#346523,
#346524,#346525),(#346526,#346527,#346528),(#346529,#346530,#346531),(#346532,
#346533,#346534),(#346535,#346536,#346537),(#346538,#346539,#346540),(#346541,
#346542,#346543),(#346544,#346545,#346546),(#346547,#346548,#346549),(#346550,
#346551,#346552),(#346553,#346554,#346555),(#346556,#346557,#346558)),
 .UNSPECIFIED.,.F.,.F.,.F.,(6,1,1,1,1,1,1,1,1,1,1,1,1,1,1,1,1,1,1,1,1,1,
1,1,1,1,1,1,1,1,1,1,1,1,1,1,1,1,1,1,1,1,1,1,1,1,1,1,1,1,1,1,1,1,1,1,1,1,
1,1,1,1,1,1,1,1,1,1,1,1,1,1,1,1,1,1,1,1,1,1,1,1,1,1,1,1,1,1,1,1,1,1,1,1,
1,1,1,1,1,1,1,1,1,1,1,1,1,1,1,1,1,1,1,1,1,1,1,1,1,1,1,1,1,1,1,1,1,1,1,1,
1,1,1,1,1,1,1,1,1,1,1,1,1,1,1,1,1,1,1,1,1,1,1,1,1,1,1,1,1,1,1,1,1,1,1,1,
1,1,1,1,1,1,1,1,1,1,1,1,1,1,1,1,1,1,1,1,1,1,1,1,1,1,1,1,1,1,1,1,1,1,1,1,
1,1,1,1,1,1,1,1,1,1,1,1,1,1,1,1,1,1,1,1,1,1,1,1,1,1,1,1,1,1,1,1,1,1,1,1,
1,1,1,1,1,1,1,1,1,1,1,1,1,1,1,1,1,1,1,1,1,1,1,1,1,1,1,1,1,1,1,1,1,1,1,1,
1,1,1,1,1,1,1,1,1,1,1,1,1,1,1,1,1,1,1,1,1,1,1,1,1,1,1,1,1,1,1,1,1,1,1,1,
1,1,1,1,1,1,1,1,1,1,1,1,1,1,1,1,1,1,1,1,1,1,1,1,1,1,1,1,1,1,1,1,1,1,1,1,
1,1,1,1,1,1,1,1,1,1,1,1,1,1,1,1,1,1,1,1,1,1,1,1,1,1,1,1,1,1,1,1,1,1,1,1,
1,1,1,1,1,1,1,1,1,1,1,1,1,1,1,1,1,1,1,1,1,1,1,1,1,1,1,1,1,1,1,1,1,1,1,1,
1,1,1,1,1,1,1,1,1,1,1,1,1,1,1,1,1,1,1,1,1,1,1,1,1,1,1,1,1,1,1,1,1,1,1,1,
1,1,1,1,1,1,1,1,1,1,1,1,1,1,1,1,1,1,1,1,1,1,1,1,1,1,1,1,1,1,1,1,1,1,1,1,
1,1,1,1,1,1,1,1,1,1,1,1,1,1,1,1,1,1,1,1,1,1,1,1,1,1,1,1,1,1,1,1,1,1,1,1,
1,1,1,1,1,1,1,1,1,1,1,1,1,1,1,1,1,1,1,6),(2,1,2),(-1.,-0.998165138,-0.996330275,
-0.994495413,-0.99266055,-0.990825688,-0.988990826,-0.987155963,-0.985321101,
-0.983486239,-0.981651376,-0.979816514,-0.977981651,-0.976146789,-0.974311927,
-0.972477064,-0.970642202,-0.968807339,-0.966972477,-0.965137615,-0.963302752,
-0.96146789,-0.959633028,-0.957798165,-0.955963303,-0.95412844,-0.952293578,
-0.950458716,-0.948623853,-0.946788991,-0.944954128,-0.943119266,-0.941284404,
-0.939449541,-0.937614679,-0.935779817,-0.933944954,-0.932110092,-0.930275229,
-0.928440367,-0.926605505,-0.924770642,-0.92293578,-0.921100917,-0.919266055,
-0.917431193,-0.91559633,-0.913761468,-0.911926606,-0.910091743,-0.908256881,
-0.906422018,-0.904587156,-0.902752294,-0.900917431,-0.899082569,-0.897247706,
-0.895412844,-0.893577982,-0.891743119,-0.889908257,-0.888073394,-0.886238532,
-0.88440367,-0.882568807,-0.880733945,-0.878899083,-0.87706422,-0.875229358,
-0.873394495,-0.871559633,-0.869724771,-0.867889908,-0.866055046,-0.864220183,
-0.862385321,-0.860550459,-0.858715596,-0.856880734,-0.855045872,-0.853211009,
-0.851376147,-0.849541284,-0.847706422,-0.84587156,-0.844036697,-0.842201835,
-0.840366972,-0.83853211,-0.836697248,-0.834862385,-0.833027523,-0.831192661,
-0.829357798,-0.827522936,-0.825688073,-0.823853211,-0.822018349,-0.820183486,
-0.818348624,-0.816513761,-0.814678899,-0.812844037,-0.811009174,-0.809174312,
-0.80733945,-0.805504587,-0.803669725,-0.801834862,-0.8,-0.798165138,-0.796330275,
-0.794495413,-0.79266055,-0.790825688,-0.788990826,-0.787155963,-0.785321101,
-0.783486239,-0.781651376,-0.779816514,-0.777981651,-0.776146789,-0.774311927,
-0.772477064,-0.770642202,-0.768807339,-0.766972477,-0.765137615,-0.763302752,
-0.76146789,-0.759633028,-0.757798165,-0.755963303,-0.75412844,-0.752293578,
-0.750458716,-0.748623853,-0.746788991,-0.744954128,-0.743119266,-0.741284404,
-0.739449541,-0.737614679,-0.735779817,-0.733944954,-0.732110092,-0.730275229,
-0.728440367,-0.726605505,-0.724770642,-0.72293578,-0.721100917,-0.719266055,
-0.717431193,-0.71559633,-0.713761468,-0.711926606,-0.710091743,-0.708256881,
-0.706422018,-0.704587156,-0.702752294,-0.700917431,-0.699082569,-0.697247706,
-0.695412844,-0.693577982,-0.691743119,-0.689908257,-0.688073394,-0.686238532,
-0.68440367,-0.682568807,-0.680733945,-0.678899083,-0.67706422,-0.675229358,
-0.673394495,-0.671559633,-0.669724771,-0.667889908,-0.666055046,-0.664220183,
-0.662385321,-0.660550459,-0.658715596,-0.656880734,-0.655045872,-0.653211009,
-0.651376147,-0.649541284,-0.647706422,-0.64587156,-0.644036697,-0.642201835,
-0.640366972,-0.63853211,-0.636697248,-0.634862385,-0.633027523,-0.631192661,
-0.629357798,-0.627522936,-0.625688073,-0.623853211,-0.622018349,-0.620183486,
-0.618348624,-0.616513761,-0.614678899,-0.612844037,-0.611009174,-0.609174312,
-0.60733945,-0.605504587,-0.603669725,-0.601834862,-0.6,-0.598165138,-0.596330275,
-0.594495413,-0.59266055,-0.590825688,-0.588990826,-0.587155963,-0.585321101,
-0.583486239,-0.581651376,-0.579816514,-0.577981651,-0.576146789,-0.574311927,
-0.572477064,-0.570642202,-0.568807339,-0.566972477,-0.565137615,-0.563302752,
-0.56146789,-0.559633028,-0.557798165,-0.555963303,-0.55412844,-0.552293578,
-0.550458716,-0.548623853,-0.546788991,-0.544954128,-0.543119266,-0.541284404,
-0.539449541,-0.537614679,-0.535779817,-0.533944954,-0.532110092,-0.530275229,
-0.528440367,-0.526605505,-0.524770642,-0.52293578,-0.521100917,-0.519266055,
-0.517431193,-0.51559633,-0.513761468,-0.511926606,-0.510091743,-0.508256881,
-0.506422018,-0.504587156,-0.502752294,-0.500917431,-0.499082569,-0.497247706,
-0.495412844,-0.493577982,-0.491743119,-0.489908257,-0.488073394,-0.486238532,
-0.48440367,-0.482568807,-0.480733945,-0.478899083,-0.47706422,-0.475229358,
-0.473394495,-0.471559633,-0.469724771,-0.467889908,-0.466055046,-0.464220183,
-0.462385321,-0.460550459,-0.458715596,-0.456880734,-0.455045872,-0.453211009,
-0.451376147,-0.449541284,-0.447706422,-0.44587156,-0.444036697,-0.442201835,
-0.440366972,-0.43853211,-0.436697248,-0.434862385,-0.433027523,-0.431192661,
-0.429357798,-0.427522936,-0.425688073,-0.423853211,-0.422018349,-0.420183486,
-0.418348624,-0.416513761,-0.414678899,-0.412844037,-0.411009174,-0.409174312,
-0.40733945,-0.405504587,-0.403669725,-0.401834862,-0.4,-0.398165138,-0.396330275,
-0.394495413,-0.39266055,-0.390825688,-0.388990826,-0.387155963,-0.385321101,
-0.383486239,-0.381651376,-0.379816514,-0.377981651,-0.376146789,-0.374311927,
-0.372477064,-0.370642202,-0.368807339,-0.366972477,-0.365137615,-0.363302752,
-0.36146789,-0.359633028,-0.357798165,-0.355963303,-0.35412844,-0.352293578,
-0.350458716,-0.348623853,-0.346788991,-0.344954128,-0.343119266,-0.341284404,
-0.339449541,-0.337614679,-0.335779817,-0.333944954,-0.332110092,-0.330275229,
-0.328440367,-0.326605505,-0.324770642,-0.32293578,-0.321100917,-0.319266055,
-0.317431193,-0.31559633,-0.313761468,-0.311926606,-0.310091743,-0.308256881,
-0.306422018,-0.304587156,-0.302752294,-0.300917431,-0.299082569,-0.297247706,
-0.295412844,-0.293577982,-0.291743119,-0.289908257,-0.288073394,-0.286238532,
-0.28440367,-0.282568807,-0.280733945,-0.278899083,-0.27706422,-0.275229358,
-0.273394495,-0.271559633,-0.269724771,-0.267889908,-0.266055046,-0.264220183,
-0.262385321,-0.260550459,-0.258715596,-0.256880734,-0.255045872,-0.253211009,
-0.251376147,-0.249541284,-0.247706422,-0.24587156,-0.244036697,-0.242201835,
-0.240366972,-0.23853211,-0.236697248,-0.234862385,-0.233027523,-0.231192661,
-0.229357798,-0.227522936,-0.225688073,-0.223853211,-0.222018349,-0.220183486,
-0.218348624,-0.216513761,-0.214678899,-0.212844037,-0.211009174,-0.209174312,
-0.20733945,-0.205504587,-0.203669725,-0.201834862,-0.2,-0.198165138,-0.196330275,
-0.194495413,-0.19266055,-0.190825688,-0.188990826,-0.187155963,-0.185321101,
-0.183486239,-0.181651376,-0.179816514,-0.177981651,-0.176146789,-0.174311927,
-0.172477064,-0.170642202,-0.168807339,-0.166972477,-0.165137615,-0.163302752,
-0.16146789,-0.159633028,-0.157798165,-0.155963303,-0.15412844,-0.152293578,
-0.150458716,-0.148623853,-0.146788991,-0.144954128,-0.143119266,-0.141284404,
-0.139449541,-0.137614679,-0.135779817,-0.133944954,-0.132110092,-0.130275229,
-0.128440367,-0.126605505,-0.124770642,-0.12293578,-0.121100917,-0.119266055,
-0.117431193,-0.11559633,-0.113761468,-0.111926606,-0.110091743,-0.108256881,
-0.106422018,-0.104587156,-0.102752294,-0.100917431,-0.099082569,-0.097247706,
-0.095412844,-0.093577982,-0.091743119,-0.089908257,-0.088073394,-0.086238532,
-0.08440367,-0.082568807,-0.080733945,-0.078899083,-0.07706422,-0.075229358,
-0.073394495,-0.071559633,-0.069724771,-0.067889908,-0.066055046,-0.064220183,
-0.062385321,-0.060550459,-0.058715596,-0.056880734,-0.055045872,-0.053211009,
-0.051376147,-0.049541284,-0.047706422,-0.04587156,-0.044036697,-0.042201835,
-0.040366972,-0.03853211,-0.036697248,-0.034862385,-0.033027523,-0.031192661,
-0.029357798,-0.027522936,-0.025688073,-0.023853211,-0.022018349,-0.020183486,
-0.018348624,-0.016513761,-0.014678899,-0.012844037,-0.011009174,-0.009174312,
-0.00733945,-0.005504587,-0.003669725,-0.001834862,0.00098215),(0.3,1.,
1.3),.UNSPECIFIED.);
#6330=B_SPLINE_SURFACE_WITH_KNOTS('',5,1,((#346562,#346563,#346564),(#346565,
#346566,#346567),(#346568,#346569,#346570),(#346571,#346572,#346573),(#346574,
#346575,#346576),(#346577,#346578,#346579),(#346580,#346581,#346582),(#346583,
#346584,#346585),(#346586,#346587,#346588),(#346589,#346590,#346591),(#346592,
#346593,#346594),(#346595,#346596,#346597),(#346598,#346599,#346600),(#346601,
#346602,#346603),(#346604,#346605,#346606),(#346607,#346608,#346609),(#346610,
#346611,#346612),(#346613,#346614,#346615),(#346616,#346617,#346618),(#346619,
#346620,#346621),(#346622,#346623,#346624),(#346625,#346626,#346627),(#346628,
#346629,#346630),(#346631,#346632,#346633),(#346634,#346635,#346636),(#346637,
#346638,#346639),(#346640,#346641,#346642),(#346643,#346644,#346645),(#346646,
#346647,#346648),(#346649,#346650,#346651),(#346652,#346653,#346654),(#346655,
#346656,#346657),(#346658,#346659,#346660),(#346661,#346662,#346663),(#346664,
#346665,#346666),(#346667,#346668,#346669),(#346670,#346671,#346672),(#346673,
#346674,#346675),(#346676,#346677,#346678),(#346679,#346680,#346681),(#346682,
#346683,#346684),(#346685,#346686,#346687),(#346688,#346689,#346690),(#346691,
#346692,#346693),(#346694,#346695,#346696),(#346697,#346698,#346699),(#346700,
#346701,#346702),(#346703,#346704,#346705),(#346706,#346707,#346708),(#346709,
#346710,#346711),(#346712,#346713,#346714),(#346715,#346716,#346717),(#346718,
#346719,#346720),(#346721,#346722,#346723),(#346724,#346725,#346726),(#346727,
#346728,#346729),(#346730,#346731,#346732),(#346733,#346734,#346735),(#346736,
#346737,#346738),(#346739,#346740,#346741),(#346742,#346743,#346744),(#346745,
#346746,#346747),(#346748,#346749,#346750),(#346751,#346752,#346753),(#346754,
#346755,#346756),(#346757,#346758,#346759),(#346760,#346761,#346762),(#346763,
#346764,#346765),(#346766,#346767,#346768),(#346769,#346770,#346771),(#346772,
#346773,#346774),(#346775,#346776,#346777),(#346778,#346779,#346780),(#346781,
#346782,#346783),(#346784,#346785,#346786),(#346787,#346788,#346789),(#346790,
#346791,#346792),(#346793,#346794,#346795),(#346796,#346797,#346798),(#346799,
#346800,#346801),(#346802,#346803,#346804),(#346805,#346806,#346807),(#346808,
#346809,#346810),(#346811,#346812,#346813),(#346814,#346815,#346816),(#346817,
#346818,#346819),(#346820,#346821,#346822),(#346823,#346824,#346825),(#346826,
#346827,#346828),(#346829,#346830,#346831),(#346832,#346833,#346834),(#346835,
#346836,#346837),(#346838,#346839,#346840),(#346841,#346842,#346843),(#346844,
#346845,#346846),(#346847,#346848,#346849),(#346850,#346851,#346852),(#346853,
#346854,#346855),(#346856,#346857,#346858),(#346859,#346860,#346861),(#346862,
#346863,#346864),(#346865,#346866,#346867),(#346868,#346869,#346870),(#346871,
#346872,#346873),(#346874,#346875,#346876),(#346877,#346878,#346879),(#346880,
#346881,#346882),(#346883,#346884,#346885),(#346886,#346887,#346888),(#346889,
#346890,#346891),(#346892,#346893,#346894),(#346895,#346896,#346897),(#346898,
#346899,#346900),(#346901,#346902,#346903),(#346904,#346905,#346906),(#346907,
#346908,#346909),(#346910,#346911,#346912),(#346913,#346914,#346915),(#346916,
#346917,#346918),(#346919,#346920,#346921),(#346922,#346923,#346924),(#346925,
#346926,#346927),(#346928,#346929,#346930),(#346931,#346932,#346933),(#346934,
#346935,#346936),(#346937,#346938,#346939),(#346940,#346941,#346942),(#346943,
#346944,#346945),(#346946,#346947,#346948),(#346949,#346950,#346951),(#346952,
#346953,#346954),(#346955,#346956,#346957),(#346958,#346959,#346960),(#346961,
#346962,#346963),(#346964,#346965,#346966),(#346967,#346968,#346969),(#346970,
#346971,#346972),(#346973,#346974,#346975),(#346976,#346977,#346978),(#346979,
#346980,#346981),(#346982,#346983,#346984),(#346985,#346986,#346987),(#346988,
#346989,#346990),(#346991,#346992,#346993),(#346994,#346995,#346996),(#346997,
#346998,#346999),(#347000,#347001,#347002),(#347003,#347004,#347005),(#347006,
#347007,#347008),(#347009,#347010,#347011),(#347012,#347013,#347014),(#347015,
#347016,#347017),(#347018,#347019,#347020),(#347021,#347022,#347023),(#347024,
#347025,#347026),(#347027,#347028,#347029),(#347030,#347031,#347032),(#347033,
#347034,#347035),(#347036,#347037,#347038),(#347039,#347040,#347041),(#347042,
#347043,#347044),(#347045,#347046,#347047),(#347048,#347049,#347050),(#347051,
#347052,#347053),(#347054,#347055,#347056),(#347057,#347058,#347059),(#347060,
#347061,#347062),(#347063,#347064,#347065),(#347066,#347067,#347068),(#347069,
#347070,#347071),(#347072,#347073,#347074),(#347075,#347076,#347077),(#347078,
#347079,#347080),(#347081,#347082,#347083),(#347084,#347085,#347086),(#347087,
#347088,#347089),(#347090,#347091,#347092),(#347093,#347094,#347095),(#347096,
#347097,#347098),(#347099,#347100,#347101),(#347102,#347103,#347104),(#347105,
#347106,#347107),(#347108,#347109,#347110),(#347111,#347112,#347113),(#347114,
#347115,#347116),(#347117,#347118,#347119),(#347120,#347121,#347122),(#347123,
#347124,#347125),(#347126,#347127,#347128),(#347129,#347130,#347131),(#347132,
#347133,#347134),(#347135,#347136,#347137),(#347138,#347139,#347140),(#347141,
#347142,#347143),(#347144,#347145,#347146),(#347147,#347148,#347149),(#347150,
#347151,#347152),(#347153,#347154,#347155),(#347156,#347157,#347158),(#347159,
#347160,#347161),(#347162,#347163,#347164),(#347165,#347166,#347167),(#347168,
#347169,#347170),(#347171,#347172,#347173),(#347174,#347175,#347176),(#347177,
#347178,#347179),(#347180,#347181,#347182),(#347183,#347184,#347185),(#347186,
#347187,#347188),(#347189,#347190,#347191),(#347192,#347193,#347194),(#347195,
#347196,#347197),(#347198,#347199,#347200),(#347201,#347202,#347203),(#347204,
#347205,#347206),(#347207,#347208,#347209),(#347210,#347211,#347212),(#347213,
#347214,#347215),(#347216,#347217,#347218),(#347219,#347220,#347221),(#347222,
#347223,#347224),(#347225,#347226,#347227),(#347228,#347229,#347230),(#347231,
#347232,#347233),(#347234,#347235,#347236),(#347237,#347238,#347239),(#347240,
#347241,#347242),(#347243,#347244,#347245),(#347246,#347247,#347248),(#347249,
#347250,#347251),(#347252,#347253,#347254),(#347255,#347256,#347257),(#347258,
#347259,#347260),(#347261,#347262,#347263),(#347264,#347265,#347266),(#347267,
#347268,#347269),(#347270,#347271,#347272),(#347273,#347274,#347275),(#347276,
#347277,#347278),(#347279,#347280,#347281),(#347282,#347283,#347284),(#347285,
#347286,#347287),(#347288,#347289,#347290),(#347291,#347292,#347293),(#347294,
#347295,#347296),(#347297,#347298,#347299),(#347300,#347301,#347302),(#347303,
#347304,#347305),(#347306,#347307,#347308),(#347309,#347310,#347311),(#347312,
#347313,#347314),(#347315,#347316,#347317),(#347318,#347319,#347320),(#347321,
#347322,#347323),(#347324,#347325,#347326),(#347327,#347328,#347329),(#347330,
#347331,#347332),(#347333,#347334,#347335),(#347336,#347337,#347338),(#347339,
#347340,#347341),(#347342,#347343,#347344),(#347345,#347346,#347347),(#347348,
#347349,#347350),(#347351,#347352,#347353),(#347354,#347355,#347356),(#347357,
#347358,#347359),(#347360,#347361,#347362),(#347363,#347364,#347365),(#347366,
#347367,#347368),(#347369,#347370,#347371),(#347372,#347373,#347374),(#347375,
#347376,#347377),(#347378,#347379,#347380),(#347381,#347382,#347383),(#347384,
#347385,#347386),(#347387,#347388,#347389),(#347390,#347391,#347392),(#347393,
#347394,#347395),(#347396,#347397,#347398),(#347399,#347400,#347401),(#347402,
#347403,#347404),(#347405,#347406,#347407),(#347408,#347409,#347410),(#347411,
#347412,#347413),(#347414,#347415,#347416),(#347417,#347418,#347419),(#347420,
#347421,#347422),(#347423,#347424,#347425),(#347426,#347427,#347428),(#347429,
#347430,#347431),(#347432,#347433,#347434),(#347435,#347436,#347437),(#347438,
#347439,#347440),(#347441,#347442,#347443),(#347444,#347445,#347446),(#347447,
#347448,#347449),(#347450,#347451,#347452),(#347453,#347454,#347455),(#347456,
#347457,#347458),(#347459,#347460,#347461),(#347462,#347463,#347464),(#347465,
#347466,#347467),(#347468,#347469,#347470),(#347471,#347472,#347473),(#347474,
#347475,#347476),(#347477,#347478,#347479),(#347480,#347481,#347482),(#347483,
#347484,#347485),(#347486,#347487,#347488),(#347489,#347490,#347491),(#347492,
#347493,#347494),(#347495,#347496,#347497),(#347498,#347499,#347500),(#347501,
#347502,#347503),(#347504,#347505,#347506),(#347507,#347508,#347509),(#347510,
#347511,#347512),(#347513,#347514,#347515),(#347516,#347517,#347518),(#347519,
#347520,#347521),(#347522,#347523,#347524),(#347525,#347526,#347527),(#347528,
#347529,#347530),(#347531,#347532,#347533),(#347534,#347535,#347536),(#347537,
#347538,#347539),(#347540,#347541,#347542),(#347543,#347544,#347545),(#347546,
#347547,#347548),(#347549,#347550,#347551),(#347552,#347553,#347554),(#347555,
#347556,#347557),(#347558,#347559,#347560),(#347561,#347562,#347563),(#347564,
#347565,#347566),(#347567,#347568,#347569),(#347570,#347571,#347572),(#347573,
#347574,#347575),(#347576,#347577,#347578),(#347579,#347580,#347581),(#347582,
#347583,#347584),(#347585,#347586,#347587),(#347588,#347589,#347590),(#347591,
#347592,#347593),(#347594,#347595,#347596),(#347597,#347598,#347599),(#347600,
#347601,#347602),(#347603,#347604,#347605),(#347606,#347607,#347608),(#347609,
#347610,#347611),(#347612,#347613,#347614),(#347615,#347616,#347617),(#347618,
#347619,#347620),(#347621,#347622,#347623),(#347624,#347625,#347626),(#347627,
#347628,#347629),(#347630,#347631,#347632),(#347633,#347634,#347635),(#347636,
#347637,#347638),(#347639,#347640,#347641),(#347642,#347643,#347644),(#347645,
#347646,#347647),(#347648,#347649,#347650),(#347651,#347652,#347653),(#347654,
#347655,#347656),(#347657,#347658,#347659),(#347660,#347661,#347662),(#347663,
#347664,#347665),(#347666,#347667,#347668),(#347669,#347670,#347671),(#347672,
#347673,#347674),(#347675,#347676,#347677),(#347678,#347679,#347680),(#347681,
#347682,#347683),(#347684,#347685,#347686),(#347687,#347688,#347689),(#347690,
#347691,#347692),(#347693,#347694,#347695),(#347696,#347697,#347698),(#347699,
#347700,#347701),(#347702,#347703,#347704),(#347705,#347706,#347707),(#347708,
#347709,#347710),(#347711,#347712,#347713),(#347714,#347715,#347716),(#347717,
#347718,#347719),(#347720,#347721,#347722),(#347723,#347724,#347725),(#347726,
#347727,#347728),(#347729,#347730,#347731),(#347732,#347733,#347734),(#347735,
#347736,#347737),(#347738,#347739,#347740),(#347741,#347742,#347743),(#347744,
#347745,#347746),(#347747,#347748,#347749),(#347750,#347751,#347752),(#347753,
#347754,#347755),(#347756,#347757,#347758),(#347759,#347760,#347761),(#347762,
#347763,#347764),(#347765,#347766,#347767),(#347768,#347769,#347770),(#347771,
#347772,#347773),(#347774,#347775,#347776),(#347777,#347778,#347779),(#347780,
#347781,#347782),(#347783,#347784,#347785),(#347786,#347787,#347788),(#347789,
#347790,#347791),(#347792,#347793,#347794),(#347795,#347796,#347797),(#347798,
#347799,#347800),(#347801,#347802,#347803),(#347804,#347805,#347806),(#347807,
#347808,#347809),(#347810,#347811,#347812),(#347813,#347814,#347815),(#347816,
#347817,#347818),(#347819,#347820,#347821),(#347822,#347823,#347824),(#347825,
#347826,#347827),(#347828,#347829,#347830),(#347831,#347832,#347833),(#347834,
#347835,#347836),(#347837,#347838,#347839),(#347840,#347841,#347842),(#347843,
#347844,#347845),(#347846,#347847,#347848),(#347849,#347850,#347851),(#347852,
#347853,#347854),(#347855,#347856,#347857),(#347858,#347859,#347860),(#347861,
#347862,#347863),(#347864,#347865,#347866),(#347867,#347868,#347869),(#347870,
#347871,#347872),(#347873,#347874,#347875),(#347876,#347877,#347878),(#347879,
#347880,#347881),(#347882,#347883,#347884),(#347885,#347886,#347887),(#347888,
#347889,#347890),(#347891,#347892,#347893),(#347894,#347895,#347896),(#347897,
#347898,#347899),(#347900,#347901,#347902),(#347903,#347904,#347905),(#347906,
#347907,#347908),(#347909,#347910,#347911),(#347912,#347913,#347914),(#347915,
#347916,#347917),(#347918,#347919,#347920),(#347921,#347922,#347923),(#347924,
#347925,#347926),(#347927,#347928,#347929),(#347930,#347931,#347932),(#347933,
#347934,#347935),(#347936,#347937,#347938),(#347939,#347940,#347941),(#347942,
#347943,#347944),(#347945,#347946,#347947),(#347948,#347949,#347950),(#347951,
#347952,#347953),(#347954,#347955,#347956),(#347957,#347958,#347959),(#347960,
#347961,#347962),(#347963,#347964,#347965),(#347966,#347967,#347968),(#347969,
#347970,#347971),(#347972,#347973,#347974),(#347975,#347976,#347977),(#347978,
#347979,#347980),(#347981,#347982,#347983),(#347984,#347985,#347986),(#347987,
#347988,#347989),(#347990,#347991,#347992),(#347993,#347994,#347995),(#347996,
#347997,#347998),(#347999,#348000,#348001),(#348002,#348003,#348004),(#348005,
#348006,#348007),(#348008,#348009,#348010),(#348011,#348012,#348013),(#348014,
#348015,#348016),(#348017,#348018,#348019),(#348020,#348021,#348022),(#348023,
#348024,#348025),(#348026,#348027,#348028),(#348029,#348030,#348031),(#348032,
#348033,#348034),(#348035,#348036,#348037),(#348038,#348039,#348040),(#348041,
#348042,#348043),(#348044,#348045,#348046),(#348047,#348048,#348049),(#348050,
#348051,#348052),(#348053,#348054,#348055),(#348056,#348057,#348058),(#348059,
#348060,#348061),(#348062,#348063,#348064),(#348065,#348066,#348067),(#348068,
#348069,#348070),(#348071,#348072,#348073),(#348074,#348075,#348076),(#348077,
#348078,#348079),(#348080,#348081,#348082),(#348083,#348084,#348085),(#348086,
#348087,#348088),(#348089,#348090,#348091),(#348092,#348093,#348094),(#348095,
#348096,#348097),(#348098,#348099,#348100),(#348101,#348102,#348103),(#348104,
#348105,#348106),(#348107,#348108,#348109),(#348110,#348111,#348112),(#348113,
#348114,#348115),(#348116,#348117,#348118),(#348119,#348120,#348121),(#348122,
#348123,#348124),(#348125,#348126,#348127),(#348128,#348129,#348130),(#348131,
#348132,#348133),(#348134,#348135,#348136),(#348137,#348138,#348139),(#348140,
#348141,#348142),(#348143,#348144,#348145),(#348146,#348147,#348148),(#348149,
#348150,#348151),(#348152,#348153,#348154),(#348155,#348156,#348157),(#348158,
#348159,#348160),(#348161,#348162,#348163),(#348164,#348165,#348166),(#348167,
#348168,#348169),(#348170,#348171,#348172),(#348173,#348174,#348175),(#348176,
#348177,#348178),(#348179,#348180,#348181),(#348182,#348183,#348184),(#348185,
#348186,#348187),(#348188,#348189,#348190),(#348191,#348192,#348193),(#348194,
#348195,#348196),(#348197,#348198,#348199),(#348200,#348201,#348202),(#348203,
#348204,#348205),(#348206,#348207,#348208),(#348209,#348210,#348211),(#348212,
#348213,#348214)),.UNSPECIFIED.,.F.,.F.,.F.,(6,1,1,1,1,1,1,1,1,1,1,1,1,
1,1,1,1,1,1,1,1,1,1,1,1,1,1,1,1,1,1,1,1,1,1,1,1,1,1,1,1,1,1,1,1,1,1,1,1,
1,1,1,1,1,1,1,1,1,1,1,1,1,1,1,1,1,1,1,1,1,1,1,1,1,1,1,1,1,1,1,1,1,1,1,1,
1,1,1,1,1,1,1,1,1,1,1,1,1,1,1,1,1,1,1,1,1,1,1,1,1,1,1,1,1,1,1,1,1,1,1,1,
1,1,1,1,1,1,1,1,1,1,1,1,1,1,1,1,1,1,1,1,1,1,1,1,1,1,1,1,1,1,1,1,1,1,1,1,
1,1,1,1,1,1,1,1,1,1,1,1,1,1,1,1,1,1,1,1,1,1,1,1,1,1,1,1,1,1,1,1,1,1,1,1,
1,1,1,1,1,1,1,1,1,1,1,1,1,1,1,1,1,1,1,1,1,1,1,1,1,1,1,1,1,1,1,1,1,1,1,1,
1,1,1,1,1,1,1,1,1,1,1,1,1,1,1,1,1,1,1,1,1,1,1,1,1,1,1,1,1,1,1,1,1,1,1,1,
1,1,1,1,1,1,1,1,1,1,1,1,1,1,1,1,1,1,1,1,1,1,1,1,1,1,1,1,1,1,1,1,1,1,1,1,
1,1,1,1,1,1,1,1,1,1,1,1,1,1,1,1,1,1,1,1,1,1,1,1,1,1,1,1,1,1,1,1,1,1,1,1,
1,1,1,1,1,1,1,1,1,1,1,1,1,1,1,1,1,1,1,1,1,1,1,1,1,1,1,1,1,1,1,1,1,1,1,1,
1,1,1,1,1,1,1,1,1,1,1,1,1,1,1,1,1,1,1,1,1,1,1,1,1,1,1,1,1,1,1,1,1,1,1,1,
1,1,1,1,1,1,1,1,1,1,1,1,1,1,1,1,1,1,1,1,1,1,1,1,1,1,1,1,1,1,1,1,1,1,1,1,
1,1,1,1,1,1,1,1,1,1,1,1,1,1,1,1,1,1,1,1,1,1,1,1,1,1,1,1,1,1,1,1,1,1,1,1,
1,1,1,1,1,1,1,1,1,1,1,1,1,1,1,1,1,1,1,1,1,1,1,1,1,1,1,1,1,1,1,1,1,1,1,1,
1,1,1,1,1,1,1,1,1,1,1,1,1,1,1,1,1,1,1,1,1,1,1,1,1,1,1,1,1,6),(2,1,2),(-0.00196418,
0.,0.001834862,0.003669725,0.005504587,0.00733945,0.009174312,0.011009174,
0.012844037,0.014678899,0.016513761,0.018348624,0.020183486,0.022018349,
0.023853211,0.025688073,0.027522936,0.029357798,0.031192661,0.033027523,
0.034862385,0.036697248,0.03853211,0.040366972,0.042201835,0.044036697,
0.04587156,0.047706422,0.049541284,0.051376147,0.053211009,0.055045872,
0.056880734,0.058715596,0.060550459,0.062385321,0.064220183,0.066055046,
0.067889908,0.069724771,0.071559633,0.073394495,0.075229358,0.07706422,
0.078899083,0.080733945,0.082568807,0.08440367,0.086238532,0.088073394,
0.089908257,0.091743119,0.093577982,0.095412844,0.097247706,0.099082569,
0.100917431,0.102752294,0.104587156,0.106422018,0.108256881,0.110091743,
0.111926606,0.113761468,0.11559633,0.117431193,0.119266055,0.121100917,
0.12293578,0.124770642,0.126605505,0.128440367,0.130275229,0.132110092,
0.133944954,0.135779817,0.137614679,0.139449541,0.141284404,0.143119266,
0.144954128,0.146788991,0.148623853,0.150458716,0.152293578,0.15412844,
0.155963303,0.157798165,0.159633028,0.16146789,0.163302752,0.165137615,
0.166972477,0.168807339,0.170642202,0.172477064,0.174311927,0.176146789,
0.177981651,0.179816514,0.181651376,0.183486239,0.185321101,0.187155963,
0.188990826,0.190825688,0.19266055,0.194495413,0.196330275,0.198165138,
0.2,0.201834862,0.203669725,0.205504587,0.20733945,0.209174312,0.211009174,
0.212844037,0.214678899,0.216513761,0.218348624,0.220183486,0.222018349,
0.223853211,0.225688073,0.227522936,0.229357798,0.231192661,0.233027523,
0.234862385,0.236697248,0.23853211,0.240366972,0.242201835,0.244036697,
0.24587156,0.247706422,0.249541284,0.251376147,0.253211009,0.255045872,
0.256880734,0.258715596,0.260550459,0.262385321,0.264220183,0.266055046,
0.267889908,0.269724771,0.271559633,0.273394495,0.275229358,0.27706422,
0.278899083,0.280733945,0.282568807,0.28440367,0.286238532,0.288073394,
0.289908257,0.291743119,0.293577982,0.295412844,0.297247706,0.299082569,
0.300917431,0.302752294,0.304587156,0.306422018,0.308256881,0.310091743,
0.311926606,0.313761468,0.31559633,0.317431193,0.319266055,0.321100917,
0.32293578,0.324770642,0.326605505,0.328440367,0.330275229,0.332110092,
0.333944954,0.335779817,0.337614679,0.339449541,0.341284404,0.343119266,
0.344954128,0.346788991,0.348623853,0.350458716,0.352293578,0.35412844,
0.355963303,0.357798165,0.359633028,0.36146789,0.363302752,0.365137615,
0.366972477,0.368807339,0.370642202,0.372477064,0.374311927,0.376146789,
0.377981651,0.379816514,0.381651376,0.383486239,0.385321101,0.387155963,
0.388990826,0.390825688,0.39266055,0.394495413,0.396330275,0.398165138,
0.4,0.401834862,0.403669725,0.405504587,0.40733945,0.409174312,0.411009174,
0.412844037,0.414678899,0.416513761,0.418348624,0.420183486,0.422018349,
0.423853211,0.425688073,0.427522936,0.429357798,0.431192661,0.433027523,
0.434862385,0.436697248,0.43853211,0.440366972,0.442201835,0.444036697,
0.44587156,0.447706422,0.449541284,0.451376147,0.453211009,0.455045872,
0.456880734,0.458715596,0.460550459,0.462385321,0.464220183,0.466055046,
0.467889908,0.469724771,0.471559633,0.473394495,0.475229358,0.47706422,
0.478899083,0.480733945,0.482568807,0.48440367,0.486238532,0.488073394,
0.489908257,0.491743119,0.493577982,0.495412844,0.497247706,0.499082569,
0.500917431,0.502752294,0.504587156,0.506422018,0.508256881,0.510091743,
0.511926606,0.513761468,0.51559633,0.517431193,0.519266055,0.521100917,
0.52293578,0.524770642,0.526605505,0.528440367,0.530275229,0.532110092,
0.533944954,0.535779817,0.537614679,0.539449541,0.541284404,0.543119266,
0.544954128,0.546788991,0.548623853,0.550458716,0.552293578,0.55412844,
0.555963303,0.557798165,0.559633028,0.56146789,0.563302752,0.565137615,
0.566972477,0.568807339,0.570642202,0.572477064,0.574311927,0.576146789,
0.577981651,0.579816514,0.581651376,0.583486239,0.585321101,0.587155963,
0.588990826,0.590825688,0.59266055,0.594495413,0.596330275,0.598165138,
0.6,0.601834862,0.603669725,0.605504587,0.60733945,0.609174312,0.611009174,
0.612844037,0.614678899,0.616513761,0.618348624,0.620183486,0.622018349,
0.623853211,0.625688073,0.627522936,0.629357798,0.631192661,0.633027523,
0.634862385,0.636697248,0.63853211,0.640366972,0.642201835,0.644036697,
0.64587156,0.647706422,0.649541284,0.651376147,0.653211009,0.655045872,
0.656880734,0.658715596,0.660550459,0.662385321,0.664220183,0.666055046,
0.667889908,0.669724771,0.671559633,0.673394495,0.675229358,0.67706422,
0.678899083,0.680733945,0.682568807,0.68440367,0.686238532,0.688073394,
0.689908257,0.691743119,0.693577982,0.695412844,0.697247706,0.699082569,
0.700917431,0.702752294,0.704587156,0.706422018,0.708256881,0.710091743,
0.711926606,0.713761468,0.71559633,0.717431193,0.719266055,0.721100917,
0.72293578,0.724770642,0.726605505,0.728440367,0.730275229,0.732110092,
0.733944954,0.735779817,0.737614679,0.739449541,0.741284404,0.743119266,
0.744954128,0.746788991,0.748623853,0.750458716,0.752293578,0.75412844,
0.755963303,0.757798165,0.759633028,0.76146789,0.763302752,0.765137615,
0.766972477,0.768807339,0.770642202,0.772477064,0.774311927,0.776146789,
0.777981651,0.779816514,0.781651376,0.783486239,0.785321101,0.787155963,
0.788990826,0.790825688,0.79266055,0.794495413,0.796330275,0.798165138,
0.8,0.801834862,0.803669725,0.805504587,0.80733945,0.809174312,0.811009174,
0.812844037,0.814678899,0.816513761,0.818348624,0.820183486,0.822018349,
0.823853211,0.825688073,0.827522936,0.829357798,0.831192661,0.833027523,
0.834862385,0.836697248,0.83853211,0.840366972,0.842201835,0.844036697,
0.84587156,0.847706422,0.849541284,0.851376147,0.853211009,0.855045872,
0.856880734,0.858715596,0.860550459,0.862385321,0.864220183,0.866055046,
0.867889908,0.869724771,0.871559633,0.873394495,0.875229358,0.87706422,
0.878899083,0.880733945,0.882568807,0.88440367,0.886238532,0.888073394,
0.889908257,0.891743119,0.893577982,0.895412844,0.897247706,0.899082569,
0.900917431,0.902752294,0.904587156,0.906422018,0.908256881,0.910091743,
0.911926606,0.913761468,0.91559633,0.917431193,0.919266055,0.921100917,
0.92293578,0.924770642,0.926605505,0.928440367,0.930275229,0.932110092,
0.933944954,0.935779817,0.937614679,0.939449541,0.941284404,0.943119266,
0.944954128,0.946788991,0.948623853,0.950458716,0.952293578,0.95412844,
0.955963303,0.957798165,0.959633028,0.96146789,0.963302752,0.965137615,
0.966972477,0.968807339,0.970642202,0.972477064,0.974311927,0.976146789,
0.977981651,0.979816514,0.981651376,0.983486239,0.985321101,0.987155963,
0.988990826,0.990825688,0.99266055,0.994495413,0.996330275,0.998165138,
1.),(0.3,1.,1.3),.UNSPECIFIED.);
#6331=B_SPLINE_SURFACE_WITH_KNOTS('',5,1,((#348221,#348222,#348223),(#348224,
#348225,#348226),(#348227,#348228,#348229),(#348230,#348231,#348232),(#348233,
#348234,#348235),(#348236,#348237,#348238),(#348239,#348240,#348241),(#348242,
#348243,#348244),(#348245,#348246,#348247),(#348248,#348249,#348250),(#348251,
#348252,#348253),(#348254,#348255,#348256),(#348257,#348258,#348259),(#348260,
#348261,#348262),(#348263,#348264,#348265),(#348266,#348267,#348268),(#348269,
#348270,#348271),(#348272,#348273,#348274),(#348275,#348276,#348277),(#348278,
#348279,#348280),(#348281,#348282,#348283),(#348284,#348285,#348286),(#348287,
#348288,#348289),(#348290,#348291,#348292),(#348293,#348294,#348295),(#348296,
#348297,#348298),(#348299,#348300,#348301),(#348302,#348303,#348304),(#348305,
#348306,#348307),(#348308,#348309,#348310),(#348311,#348312,#348313),(#348314,
#348315,#348316),(#348317,#348318,#348319),(#348320,#348321,#348322),(#348323,
#348324,#348325),(#348326,#348327,#348328),(#348329,#348330,#348331),(#348332,
#348333,#348334),(#348335,#348336,#348337),(#348338,#348339,#348340),(#348341,
#348342,#348343),(#348344,#348345,#348346),(#348347,#348348,#348349),(#348350,
#348351,#348352),(#348353,#348354,#348355),(#348356,#348357,#348358),(#348359,
#348360,#348361),(#348362,#348363,#348364),(#348365,#348366,#348367),(#348368,
#348369,#348370),(#348371,#348372,#348373),(#348374,#348375,#348376),(#348377,
#348378,#348379),(#348380,#348381,#348382),(#348383,#348384,#348385),(#348386,
#348387,#348388),(#348389,#348390,#348391),(#348392,#348393,#348394),(#348395,
#348396,#348397),(#348398,#348399,#348400),(#348401,#348402,#348403),(#348404,
#348405,#348406),(#348407,#348408,#348409),(#348410,#348411,#348412),(#348413,
#348414,#348415),(#348416,#348417,#348418),(#348419,#348420,#348421),(#348422,
#348423,#348424),(#348425,#348426,#348427),(#348428,#348429,#348430),(#348431,
#348432,#348433),(#348434,#348435,#348436),(#348437,#348438,#348439),(#348440,
#348441,#348442),(#348443,#348444,#348445),(#348446,#348447,#348448),(#348449,
#348450,#348451),(#348452,#348453,#348454),(#348455,#348456,#348457),(#348458,
#348459,#348460),(#348461,#348462,#348463),(#348464,#348465,#348466),(#348467,
#348468,#348469),(#348470,#348471,#348472),(#348473,#348474,#348475),(#348476,
#348477,#348478),(#348479,#348480,#348481),(#348482,#348483,#348484),(#348485,
#348486,#348487),(#348488,#348489,#348490),(#348491,#348492,#348493),(#348494,
#348495,#348496),(#348497,#348498,#348499),(#348500,#348501,#348502),(#348503,
#348504,#348505),(#348506,#348507,#348508),(#348509,#348510,#348511),(#348512,
#348513,#348514),(#348515,#348516,#348517),(#348518,#348519,#348520),(#348521,
#348522,#348523),(#348524,#348525,#348526),(#348527,#348528,#348529),(#348530,
#348531,#348532),(#348533,#348534,#348535),(#348536,#348537,#348538),(#348539,
#348540,#348541),(#348542,#348543,#348544),(#348545,#348546,#348547),(#348548,
#348549,#348550),(#348551,#348552,#348553),(#348554,#348555,#348556),(#348557,
#348558,#348559),(#348560,#348561,#348562),(#348563,#348564,#348565),(#348566,
#348567,#348568),(#348569,#348570,#348571),(#348572,#348573,#348574),(#348575,
#348576,#348577),(#348578,#348579,#348580),(#348581,#348582,#348583),(#348584,
#348585,#348586),(#348587,#348588,#348589),(#348590,#348591,#348592),(#348593,
#348594,#348595),(#348596,#348597,#348598),(#348599,#348600,#348601),(#348602,
#348603,#348604),(#348605,#348606,#348607),(#348608,#348609,#348610),(#348611,
#348612,#348613),(#348614,#348615,#348616),(#348617,#348618,#348619),(#348620,
#348621,#348622),(#348623,#348624,#348625),(#348626,#348627,#348628),(#348629,
#348630,#348631),(#348632,#348633,#348634),(#348635,#348636,#348637),(#348638,
#348639,#348640),(#348641,#348642,#348643),(#348644,#348645,#348646),(#348647,
#348648,#348649),(#348650,#348651,#348652),(#348653,#348654,#348655),(#348656,
#348657,#348658),(#348659,#348660,#348661),(#348662,#348663,#348664),(#348665,
#348666,#348667),(#348668,#348669,#348670),(#348671,#348672,#348673),(#348674,
#348675,#348676),(#348677,#348678,#348679),(#348680,#348681,#348682),(#348683,
#348684,#348685),(#348686,#348687,#348688),(#348689,#348690,#348691),(#348692,
#348693,#348694),(#348695,#348696,#348697),(#348698,#348699,#348700),(#348701,
#348702,#348703),(#348704,#348705,#348706),(#348707,#348708,#348709),(#348710,
#348711,#348712),(#348713,#348714,#348715),(#348716,#348717,#348718),(#348719,
#348720,#348721),(#348722,#348723,#348724),(#348725,#348726,#348727),(#348728,
#348729,#348730),(#348731,#348732,#348733),(#348734,#348735,#348736),(#348737,
#348738,#348739),(#348740,#348741,#348742),(#348743,#348744,#348745),(#348746,
#348747,#348748),(#348749,#348750,#348751),(#348752,#348753,#348754),(#348755,
#348756,#348757),(#348758,#348759,#348760),(#348761,#348762,#348763),(#348764,
#348765,#348766),(#348767,#348768,#348769),(#348770,#348771,#348772),(#348773,
#348774,#348775),(#348776,#348777,#348778),(#348779,#348780,#348781),(#348782,
#348783,#348784),(#348785,#348786,#348787),(#348788,#348789,#348790),(#348791,
#348792,#348793),(#348794,#348795,#348796),(#348797,#348798,#348799),(#348800,
#348801,#348802),(#348803,#348804,#348805),(#348806,#348807,#348808),(#348809,
#348810,#348811),(#348812,#348813,#348814),(#348815,#348816,#348817),(#348818,
#348819,#348820),(#348821,#348822,#348823),(#348824,#348825,#348826),(#348827,
#348828,#348829),(#348830,#348831,#348832),(#348833,#348834,#348835),(#348836,
#348837,#348838),(#348839,#348840,#348841),(#348842,#348843,#348844),(#348845,
#348846,#348847),(#348848,#348849,#348850),(#348851,#348852,#348853),(#348854,
#348855,#348856),(#348857,#348858,#348859),(#348860,#348861,#348862),(#348863,
#348864,#348865),(#348866,#348867,#348868),(#348869,#348870,#348871),(#348872,
#348873,#348874),(#348875,#348876,#348877),(#348878,#348879,#348880),(#348881,
#348882,#348883),(#348884,#348885,#348886),(#348887,#348888,#348889),(#348890,
#348891,#348892),(#348893,#348894,#348895),(#348896,#348897,#348898),(#348899,
#348900,#348901),(#348902,#348903,#348904),(#348905,#348906,#348907),(#348908,
#348909,#348910),(#348911,#348912,#348913),(#348914,#348915,#348916),(#348917,
#348918,#348919),(#348920,#348921,#348922),(#348923,#348924,#348925),(#348926,
#348927,#348928),(#348929,#348930,#348931),(#348932,#348933,#348934),(#348935,
#348936,#348937),(#348938,#348939,#348940),(#348941,#348942,#348943),(#348944,
#348945,#348946),(#348947,#348948,#348949),(#348950,#348951,#348952),(#348953,
#348954,#348955),(#348956,#348957,#348958),(#348959,#348960,#348961),(#348962,
#348963,#348964),(#348965,#348966,#348967),(#348968,#348969,#348970),(#348971,
#348972,#348973),(#348974,#348975,#348976),(#348977,#348978,#348979),(#348980,
#348981,#348982),(#348983,#348984,#348985),(#348986,#348987,#348988),(#348989,
#348990,#348991),(#348992,#348993,#348994),(#348995,#348996,#348997),(#348998,
#348999,#349000),(#349001,#349002,#349003),(#349004,#349005,#349006),(#349007,
#349008,#349009),(#349010,#349011,#349012),(#349013,#349014,#349015),(#349016,
#349017,#349018),(#349019,#349020,#349021),(#349022,#349023,#349024),(#349025,
#349026,#349027),(#349028,#349029,#349030),(#349031,#349032,#349033),(#349034,
#349035,#349036),(#349037,#349038,#349039),(#349040,#349041,#349042),(#349043,
#349044,#349045),(#349046,#349047,#349048),(#349049,#349050,#349051),(#349052,
#349053,#349054),(#349055,#349056,#349057),(#349058,#349059,#349060),(#349061,
#349062,#349063),(#349064,#349065,#349066),(#349067,#349068,#349069),(#349070,
#349071,#349072),(#349073,#349074,#349075),(#349076,#349077,#349078),(#349079,
#349080,#349081),(#349082,#349083,#349084),(#349085,#349086,#349087),(#349088,
#349089,#349090),(#349091,#349092,#349093),(#349094,#349095,#349096),(#349097,
#349098,#349099),(#349100,#349101,#349102),(#349103,#349104,#349105),(#349106,
#349107,#349108),(#349109,#349110,#349111),(#349112,#349113,#349114),(#349115,
#349116,#349117),(#349118,#349119,#349120),(#349121,#349122,#349123),(#349124,
#349125,#349126),(#349127,#349128,#349129),(#349130,#349131,#349132),(#349133,
#349134,#349135),(#349136,#349137,#349138),(#349139,#349140,#349141),(#349142,
#349143,#349144),(#349145,#349146,#349147),(#349148,#349149,#349150),(#349151,
#349152,#349153),(#349154,#349155,#349156),(#349157,#349158,#349159),(#349160,
#349161,#349162),(#349163,#349164,#349165),(#349166,#349167,#349168),(#349169,
#349170,#349171),(#349172,#349173,#349174),(#349175,#349176,#349177),(#349178,
#349179,#349180),(#349181,#349182,#349183),(#349184,#349185,#349186),(#349187,
#349188,#349189),(#349190,#349191,#349192),(#349193,#349194,#349195),(#349196,
#349197,#349198),(#349199,#349200,#349201),(#349202,#349203,#349204),(#349205,
#349206,#349207),(#349208,#349209,#349210),(#349211,#349212,#349213),(#349214,
#349215,#349216),(#349217,#349218,#349219),(#349220,#349221,#349222),(#349223,
#349224,#349225),(#349226,#349227,#349228),(#349229,#349230,#349231),(#349232,
#349233,#349234),(#349235,#349236,#349237),(#349238,#349239,#349240),(#349241,
#349242,#349243),(#349244,#349245,#349246),(#349247,#349248,#349249),(#349250,
#349251,#349252),(#349253,#349254,#349255),(#349256,#349257,#349258),(#349259,
#349260,#349261),(#349262,#349263,#349264),(#349265,#349266,#349267),(#349268,
#349269,#349270),(#349271,#349272,#349273),(#349274,#349275,#349276),(#349277,
#349278,#349279),(#349280,#349281,#349282),(#349283,#349284,#349285),(#349286,
#349287,#349288),(#349289,#349290,#349291),(#349292,#349293,#349294),(#349295,
#349296,#349297),(#349298,#349299,#349300),(#349301,#349302,#349303),(#349304,
#349305,#349306),(#349307,#349308,#349309),(#349310,#349311,#349312),(#349313,
#349314,#349315),(#349316,#349317,#349318),(#349319,#349320,#349321),(#349322,
#349323,#349324),(#349325,#349326,#349327),(#349328,#349329,#349330),(#349331,
#349332,#349333),(#349334,#349335,#349336),(#349337,#349338,#349339),(#349340,
#349341,#349342),(#349343,#349344,#349345),(#349346,#349347,#349348),(#349349,
#349350,#349351),(#349352,#349353,#349354),(#349355,#349356,#349357),(#349358,
#349359,#349360),(#349361,#349362,#349363),(#349364,#349365,#349366),(#349367,
#349368,#349369),(#349370,#349371,#349372),(#349373,#349374,#349375),(#349376,
#349377,#349378),(#349379,#349380,#349381),(#349382,#349383,#349384),(#349385,
#349386,#349387),(#349388,#349389,#349390),(#349391,#349392,#349393),(#349394,
#349395,#349396),(#349397,#349398,#349399),(#349400,#349401,#349402),(#349403,
#349404,#349405),(#349406,#349407,#349408),(#349409,#349410,#349411),(#349412,
#349413,#349414),(#349415,#349416,#349417),(#349418,#349419,#349420),(#349421,
#349422,#349423),(#349424,#349425,#349426),(#349427,#349428,#349429),(#349430,
#349431,#349432),(#349433,#349434,#349435),(#349436,#349437,#349438),(#349439,
#349440,#349441),(#349442,#349443,#349444),(#349445,#349446,#349447),(#349448,
#349449,#349450),(#349451,#349452,#349453),(#349454,#349455,#349456),(#349457,
#349458,#349459),(#349460,#349461,#349462),(#349463,#349464,#349465),(#349466,
#349467,#349468),(#349469,#349470,#349471),(#349472,#349473,#349474),(#349475,
#349476,#349477),(#349478,#349479,#349480),(#349481,#349482,#349483),(#349484,
#349485,#349486),(#349487,#349488,#349489),(#349490,#349491,#349492),(#349493,
#349494,#349495),(#349496,#349497,#349498),(#349499,#349500,#349501),(#349502,
#349503,#349504),(#349505,#349506,#349507),(#349508,#349509,#349510),(#349511,
#349512,#349513),(#349514,#349515,#349516),(#349517,#349518,#349519),(#349520,
#349521,#349522),(#349523,#349524,#349525),(#349526,#349527,#349528),(#349529,
#349530,#349531),(#349532,#349533,#349534),(#349535,#349536,#349537),(#349538,
#349539,#349540),(#349541,#349542,#349543),(#349544,#349545,#349546),(#349547,
#349548,#349549),(#349550,#349551,#349552),(#349553,#349554,#349555),(#349556,
#349557,#349558),(#349559,#349560,#349561),(#349562,#349563,#349564),(#349565,
#349566,#349567),(#349568,#349569,#349570),(#349571,#349572,#349573),(#349574,
#349575,#349576),(#349577,#349578,#349579),(#349580,#349581,#349582),(#349583,
#349584,#349585),(#349586,#349587,#349588),(#349589,#349590,#349591),(#349592,
#349593,#349594),(#349595,#349596,#349597),(#349598,#349599,#349600),(#349601,
#349602,#349603),(#349604,#349605,#349606),(#349607,#349608,#349609),(#349610,
#349611,#349612),(#349613,#349614,#349615),(#349616,#349617,#349618),(#349619,
#349620,#349621),(#349622,#349623,#349624),(#349625,#349626,#349627),(#349628,
#349629,#349630),(#349631,#349632,#349633),(#349634,#349635,#349636),(#349637,
#349638,#349639),(#349640,#349641,#349642),(#349643,#349644,#349645),(#349646,
#349647,#349648),(#349649,#349650,#349651),(#349652,#349653,#349654),(#349655,
#349656,#349657),(#349658,#349659,#349660),(#349661,#349662,#349663),(#349664,
#349665,#349666),(#349667,#349668,#349669),(#349670,#349671,#349672),(#349673,
#349674,#349675),(#349676,#349677,#349678),(#349679,#349680,#349681),(#349682,
#349683,#349684),(#349685,#349686,#349687),(#349688,#349689,#349690),(#349691,
#349692,#349693),(#349694,#349695,#349696),(#349697,#349698,#349699),(#349700,
#349701,#349702),(#349703,#349704,#349705),(#349706,#349707,#349708),(#349709,
#349710,#349711),(#349712,#349713,#349714),(#349715,#349716,#349717),(#349718,
#349719,#349720),(#349721,#349722,#349723),(#349724,#349725,#349726),(#349727,
#349728,#349729),(#349730,#349731,#349732),(#349733,#349734,#349735),(#349736,
#349737,#349738),(#349739,#349740,#349741),(#349742,#349743,#349744),(#349745,
#349746,#349747),(#349748,#349749,#349750),(#349751,#349752,#349753),(#349754,
#349755,#349756),(#349757,#349758,#349759),(#349760,#349761,#349762),(#349763,
#349764,#349765),(#349766,#349767,#349768),(#349769,#349770,#349771),(#349772,
#349773,#349774),(#349775,#349776,#349777),(#349778,#349779,#349780),(#349781,
#349782,#349783),(#349784,#349785,#349786),(#349787,#349788,#349789),(#349790,
#349791,#349792),(#349793,#349794,#349795),(#349796,#349797,#349798),(#349799,
#349800,#349801),(#349802,#349803,#349804),(#349805,#349806,#349807),(#349808,
#349809,#349810),(#349811,#349812,#349813),(#349814,#349815,#349816),(#349817,
#349818,#349819),(#349820,#349821,#349822),(#349823,#349824,#349825),(#349826,
#349827,#349828),(#349829,#349830,#349831),(#349832,#349833,#349834),(#349835,
#349836,#349837),(#349838,#349839,#349840),(#349841,#349842,#349843),(#349844,
#349845,#349846),(#349847,#349848,#349849),(#349850,#349851,#349852),(#349853,
#349854,#349855),(#349856,#349857,#349858),(#349859,#349860,#349861),(#349862,
#349863,#349864),(#349865,#349866,#349867),(#349868,#349869,#349870)),
 .UNSPECIFIED.,.F.,.F.,.F.,(6,1,1,1,1,1,1,1,1,1,1,1,1,1,1,1,1,1,1,1,1,1,
1,1,1,1,1,1,1,1,1,1,1,1,1,1,1,1,1,1,1,1,1,1,1,1,1,1,1,1,1,1,1,1,1,1,1,1,
1,1,1,1,1,1,1,1,1,1,1,1,1,1,1,1,1,1,1,1,1,1,1,1,1,1,1,1,1,1,1,1,1,1,1,1,
1,1,1,1,1,1,1,1,1,1,1,1,1,1,1,1,1,1,1,1,1,1,1,1,1,1,1,1,1,1,1,1,1,1,1,1,
1,1,1,1,1,1,1,1,1,1,1,1,1,1,1,1,1,1,1,1,1,1,1,1,1,1,1,1,1,1,1,1,1,1,1,1,
1,1,1,1,1,1,1,1,1,1,1,1,1,1,1,1,1,1,1,1,1,1,1,1,1,1,1,1,1,1,1,1,1,1,1,1,
1,1,1,1,1,1,1,1,1,1,1,1,1,1,1,1,1,1,1,1,1,1,1,1,1,1,1,1,1,1,1,1,1,1,1,1,
1,1,1,1,1,1,1,1,1,1,1,1,1,1,1,1,1,1,1,1,1,1,1,1,1,1,1,1,1,1,1,1,1,1,1,1,
1,1,1,1,1,1,1,1,1,1,1,1,1,1,1,1,1,1,1,1,1,1,1,1,1,1,1,1,1,1,1,1,1,1,1,1,
1,1,1,1,1,1,1,1,1,1,1,1,1,1,1,1,1,1,1,1,1,1,1,1,1,1,1,1,1,1,1,1,1,1,1,1,
1,1,1,1,1,1,1,1,1,1,1,1,1,1,1,1,1,1,1,1,1,1,1,1,1,1,1,1,1,1,1,1,1,1,1,1,
1,1,1,1,1,1,1,1,1,1,1,1,1,1,1,1,1,1,1,1,1,1,1,1,1,1,1,1,1,1,1,1,1,1,1,1,
1,1,1,1,1,1,1,1,1,1,1,1,1,1,1,1,1,1,1,1,1,1,1,1,1,1,1,1,1,1,1,1,1,1,1,1,
1,1,1,1,1,1,1,1,1,1,1,1,1,1,1,1,1,1,1,1,1,1,1,1,1,1,1,1,1,1,1,1,1,1,1,1,
1,1,1,1,1,1,1,1,1,1,1,1,1,1,1,1,1,1,1,1,1,1,1,1,1,1,1,1,1,1,1,1,1,1,1,1,
1,1,1,1,1,1,1,1,1,1,1,1,1,1,1,1,1,1,1,6),(2,1,2),(-1.,-0.998165138,-0.996330275,
-0.994495413,-0.99266055,-0.990825688,-0.988990826,-0.987155963,-0.985321101,
-0.983486239,-0.981651376,-0.979816514,-0.977981651,-0.976146789,-0.974311927,
-0.972477064,-0.970642202,-0.968807339,-0.966972477,-0.965137615,-0.963302752,
-0.96146789,-0.959633028,-0.957798165,-0.955963303,-0.95412844,-0.952293578,
-0.950458716,-0.948623853,-0.946788991,-0.944954128,-0.943119266,-0.941284404,
-0.939449541,-0.937614679,-0.935779817,-0.933944954,-0.932110092,-0.930275229,
-0.928440367,-0.926605505,-0.924770642,-0.92293578,-0.921100917,-0.919266055,
-0.917431193,-0.91559633,-0.913761468,-0.911926606,-0.910091743,-0.908256881,
-0.906422018,-0.904587156,-0.902752294,-0.900917431,-0.899082569,-0.897247706,
-0.895412844,-0.893577982,-0.891743119,-0.889908257,-0.888073394,-0.886238532,
-0.88440367,-0.882568807,-0.880733945,-0.878899083,-0.87706422,-0.875229358,
-0.873394495,-0.871559633,-0.869724771,-0.867889908,-0.866055046,-0.864220183,
-0.862385321,-0.860550459,-0.858715596,-0.856880734,-0.855045872,-0.853211009,
-0.851376147,-0.849541284,-0.847706422,-0.84587156,-0.844036697,-0.842201835,
-0.840366972,-0.83853211,-0.836697248,-0.834862385,-0.833027523,-0.831192661,
-0.829357798,-0.827522936,-0.825688073,-0.823853211,-0.822018349,-0.820183486,
-0.818348624,-0.816513761,-0.814678899,-0.812844037,-0.811009174,-0.809174312,
-0.80733945,-0.805504587,-0.803669725,-0.801834862,-0.8,-0.798165138,-0.796330275,
-0.794495413,-0.79266055,-0.790825688,-0.788990826,-0.787155963,-0.785321101,
-0.783486239,-0.781651376,-0.779816514,-0.777981651,-0.776146789,-0.774311927,
-0.772477064,-0.770642202,-0.768807339,-0.766972477,-0.765137615,-0.763302752,
-0.76146789,-0.759633028,-0.757798165,-0.755963303,-0.75412844,-0.752293578,
-0.750458716,-0.748623853,-0.746788991,-0.744954128,-0.743119266,-0.741284404,
-0.739449541,-0.737614679,-0.735779817,-0.733944954,-0.732110092,-0.730275229,
-0.728440367,-0.726605505,-0.724770642,-0.72293578,-0.721100917,-0.719266055,
-0.717431193,-0.71559633,-0.713761468,-0.711926606,-0.710091743,-0.708256881,
-0.706422018,-0.704587156,-0.702752294,-0.700917431,-0.699082569,-0.697247706,
-0.695412844,-0.693577982,-0.691743119,-0.689908257,-0.688073394,-0.686238532,
-0.68440367,-0.682568807,-0.680733945,-0.678899083,-0.67706422,-0.675229358,
-0.673394495,-0.671559633,-0.669724771,-0.667889908,-0.666055046,-0.664220183,
-0.662385321,-0.660550459,-0.658715596,-0.656880734,-0.655045872,-0.653211009,
-0.651376147,-0.649541284,-0.647706422,-0.64587156,-0.644036697,-0.642201835,
-0.640366972,-0.63853211,-0.636697248,-0.634862385,-0.633027523,-0.631192661,
-0.629357798,-0.627522936,-0.625688073,-0.623853211,-0.622018349,-0.620183486,
-0.618348624,-0.616513761,-0.614678899,-0.612844037,-0.611009174,-0.609174312,
-0.60733945,-0.605504587,-0.603669725,-0.601834862,-0.6,-0.598165138,-0.596330275,
-0.594495413,-0.59266055,-0.590825688,-0.588990826,-0.587155963,-0.585321101,
-0.583486239,-0.581651376,-0.579816514,-0.577981651,-0.576146789,-0.574311927,
-0.572477064,-0.570642202,-0.568807339,-0.566972477,-0.565137615,-0.563302752,
-0.56146789,-0.559633028,-0.557798165,-0.555963303,-0.55412844,-0.552293578,
-0.550458716,-0.548623853,-0.546788991,-0.544954128,-0.543119266,-0.541284404,
-0.539449541,-0.537614679,-0.535779817,-0.533944954,-0.532110092,-0.530275229,
-0.528440367,-0.526605505,-0.524770642,-0.52293578,-0.521100917,-0.519266055,
-0.517431193,-0.51559633,-0.513761468,-0.511926606,-0.510091743,-0.508256881,
-0.506422018,-0.504587156,-0.502752294,-0.500917431,-0.499082569,-0.497247706,
-0.495412844,-0.493577982,-0.491743119,-0.489908257,-0.488073394,-0.486238532,
-0.48440367,-0.482568807,-0.480733945,-0.478899083,-0.47706422,-0.475229358,
-0.473394495,-0.471559633,-0.469724771,-0.467889908,-0.466055046,-0.464220183,
-0.462385321,-0.460550459,-0.458715596,-0.456880734,-0.455045872,-0.453211009,
-0.451376147,-0.449541284,-0.447706422,-0.44587156,-0.444036697,-0.442201835,
-0.440366972,-0.43853211,-0.436697248,-0.434862385,-0.433027523,-0.431192661,
-0.429357798,-0.427522936,-0.425688073,-0.423853211,-0.422018349,-0.420183486,
-0.418348624,-0.416513761,-0.414678899,-0.412844037,-0.411009174,-0.409174312,
-0.40733945,-0.405504587,-0.403669725,-0.401834862,-0.4,-0.398165138,-0.396330275,
-0.394495413,-0.39266055,-0.390825688,-0.388990826,-0.387155963,-0.385321101,
-0.383486239,-0.381651376,-0.379816514,-0.377981651,-0.376146789,-0.374311927,
-0.372477064,-0.370642202,-0.368807339,-0.366972477,-0.365137615,-0.363302752,
-0.36146789,-0.359633028,-0.357798165,-0.355963303,-0.35412844,-0.352293578,
-0.350458716,-0.348623853,-0.346788991,-0.344954128,-0.343119266,-0.341284404,
-0.339449541,-0.337614679,-0.335779817,-0.333944954,-0.332110092,-0.330275229,
-0.328440367,-0.326605505,-0.324770642,-0.32293578,-0.321100917,-0.319266055,
-0.317431193,-0.31559633,-0.313761468,-0.311926606,-0.310091743,-0.308256881,
-0.306422018,-0.304587156,-0.302752294,-0.300917431,-0.299082569,-0.297247706,
-0.295412844,-0.293577982,-0.291743119,-0.289908257,-0.288073394,-0.286238532,
-0.28440367,-0.282568807,-0.280733945,-0.278899083,-0.27706422,-0.275229358,
-0.273394495,-0.271559633,-0.269724771,-0.267889908,-0.266055046,-0.264220183,
-0.262385321,-0.260550459,-0.258715596,-0.256880734,-0.255045872,-0.253211009,
-0.251376147,-0.249541284,-0.247706422,-0.24587156,-0.244036697,-0.242201835,
-0.240366972,-0.23853211,-0.236697248,-0.234862385,-0.233027523,-0.231192661,
-0.229357798,-0.227522936,-0.225688073,-0.223853211,-0.222018349,-0.220183486,
-0.218348624,-0.216513761,-0.214678899,-0.212844037,-0.211009174,-0.209174312,
-0.20733945,-0.205504587,-0.203669725,-0.201834862,-0.2,-0.198165138,-0.196330275,
-0.194495413,-0.19266055,-0.190825688,-0.188990826,-0.187155963,-0.185321101,
-0.183486239,-0.181651376,-0.179816514,-0.177981651,-0.176146789,-0.174311927,
-0.172477064,-0.170642202,-0.168807339,-0.166972477,-0.165137615,-0.163302752,
-0.16146789,-0.159633028,-0.157798165,-0.155963303,-0.15412844,-0.152293578,
-0.150458716,-0.148623853,-0.146788991,-0.144954128,-0.143119266,-0.141284404,
-0.139449541,-0.137614679,-0.135779817,-0.133944954,-0.132110092,-0.130275229,
-0.128440367,-0.126605505,-0.124770642,-0.12293578,-0.121100917,-0.119266055,
-0.117431193,-0.11559633,-0.113761468,-0.111926606,-0.110091743,-0.108256881,
-0.106422018,-0.104587156,-0.102752294,-0.100917431,-0.099082569,-0.097247706,
-0.095412844,-0.093577982,-0.091743119,-0.089908257,-0.088073394,-0.086238532,
-0.08440367,-0.082568807,-0.080733945,-0.078899083,-0.07706422,-0.075229358,
-0.073394495,-0.071559633,-0.069724771,-0.067889908,-0.066055046,-0.064220183,
-0.062385321,-0.060550459,-0.058715596,-0.056880734,-0.055045872,-0.053211009,
-0.051376147,-0.049541284,-0.047706422,-0.04587156,-0.044036697,-0.042201835,
-0.040366972,-0.03853211,-0.036697248,-0.034862385,-0.033027523,-0.031192661,
-0.029357798,-0.027522936,-0.025688073,-0.023853211,-0.022018349,-0.020183486,
-0.018348624,-0.016513761,-0.014678899,-0.012844037,-0.011009174,-0.009174312,
-0.00733945,-0.005504587,-0.003669725,-0.001834862,0.000982119),(0.3,1.,
1.3),.UNSPECIFIED.);
#6332=B_SPLINE_SURFACE_WITH_KNOTS('',5,1,((#349874,#349875,#349876),(#349877,
#349878,#349879),(#349880,#349881,#349882),(#349883,#349884,#349885),(#349886,
#349887,#349888),(#349889,#349890,#349891),(#349892,#349893,#349894),(#349895,
#349896,#349897),(#349898,#349899,#349900),(#349901,#349902,#349903),(#349904,
#349905,#349906),(#349907,#349908,#349909),(#349910,#349911,#349912),(#349913,
#349914,#349915),(#349916,#349917,#349918),(#349919,#349920,#349921),(#349922,
#349923,#349924),(#349925,#349926,#349927),(#349928,#349929,#349930),(#349931,
#349932,#349933),(#349934,#349935,#349936),(#349937,#349938,#349939),(#349940,
#349941,#349942),(#349943,#349944,#349945),(#349946,#349947,#349948),(#349949,
#349950,#349951),(#349952,#349953,#349954),(#349955,#349956,#349957),(#349958,
#349959,#349960),(#349961,#349962,#349963),(#349964,#349965,#349966),(#349967,
#349968,#349969),(#349970,#349971,#349972),(#349973,#349974,#349975),(#349976,
#349977,#349978),(#349979,#349980,#349981),(#349982,#349983,#349984),(#349985,
#349986,#349987),(#349988,#349989,#349990),(#349991,#349992,#349993),(#349994,
#349995,#349996),(#349997,#349998,#349999),(#350000,#350001,#350002),(#350003,
#350004,#350005),(#350006,#350007,#350008),(#350009,#350010,#350011),(#350012,
#350013,#350014),(#350015,#350016,#350017),(#350018,#350019,#350020),(#350021,
#350022,#350023),(#350024,#350025,#350026),(#350027,#350028,#350029),(#350030,
#350031,#350032),(#350033,#350034,#350035),(#350036,#350037,#350038),(#350039,
#350040,#350041),(#350042,#350043,#350044),(#350045,#350046,#350047),(#350048,
#350049,#350050),(#350051,#350052,#350053),(#350054,#350055,#350056),(#350057,
#350058,#350059),(#350060,#350061,#350062),(#350063,#350064,#350065),(#350066,
#350067,#350068),(#350069,#350070,#350071),(#350072,#350073,#350074),(#350075,
#350076,#350077),(#350078,#350079,#350080),(#350081,#350082,#350083),(#350084,
#350085,#350086),(#350087,#350088,#350089),(#350090,#350091,#350092),(#350093,
#350094,#350095),(#350096,#350097,#350098),(#350099,#350100,#350101),(#350102,
#350103,#350104),(#350105,#350106,#350107),(#350108,#350109,#350110),(#350111,
#350112,#350113),(#350114,#350115,#350116),(#350117,#350118,#350119),(#350120,
#350121,#350122),(#350123,#350124,#350125),(#350126,#350127,#350128),(#350129,
#350130,#350131),(#350132,#350133,#350134),(#350135,#350136,#350137),(#350138,
#350139,#350140),(#350141,#350142,#350143),(#350144,#350145,#350146),(#350147,
#350148,#350149),(#350150,#350151,#350152),(#350153,#350154,#350155),(#350156,
#350157,#350158),(#350159,#350160,#350161),(#350162,#350163,#350164),(#350165,
#350166,#350167),(#350168,#350169,#350170),(#350171,#350172,#350173),(#350174,
#350175,#350176),(#350177,#350178,#350179),(#350180,#350181,#350182),(#350183,
#350184,#350185),(#350186,#350187,#350188),(#350189,#350190,#350191),(#350192,
#350193,#350194),(#350195,#350196,#350197),(#350198,#350199,#350200),(#350201,
#350202,#350203),(#350204,#350205,#350206),(#350207,#350208,#350209),(#350210,
#350211,#350212),(#350213,#350214,#350215),(#350216,#350217,#350218),(#350219,
#350220,#350221),(#350222,#350223,#350224),(#350225,#350226,#350227),(#350228,
#350229,#350230),(#350231,#350232,#350233),(#350234,#350235,#350236),(#350237,
#350238,#350239),(#350240,#350241,#350242),(#350243,#350244,#350245),(#350246,
#350247,#350248),(#350249,#350250,#350251),(#350252,#350253,#350254),(#350255,
#350256,#350257),(#350258,#350259,#350260),(#350261,#350262,#350263),(#350264,
#350265,#350266),(#350267,#350268,#350269),(#350270,#350271,#350272),(#350273,
#350274,#350275),(#350276,#350277,#350278),(#350279,#350280,#350281),(#350282,
#350283,#350284),(#350285,#350286,#350287),(#350288,#350289,#350290),(#350291,
#350292,#350293),(#350294,#350295,#350296),(#350297,#350298,#350299),(#350300,
#350301,#350302),(#350303,#350304,#350305),(#350306,#350307,#350308),(#350309,
#350310,#350311),(#350312,#350313,#350314),(#350315,#350316,#350317),(#350318,
#350319,#350320),(#350321,#350322,#350323),(#350324,#350325,#350326),(#350327,
#350328,#350329),(#350330,#350331,#350332),(#350333,#350334,#350335),(#350336,
#350337,#350338),(#350339,#350340,#350341),(#350342,#350343,#350344),(#350345,
#350346,#350347),(#350348,#350349,#350350),(#350351,#350352,#350353),(#350354,
#350355,#350356),(#350357,#350358,#350359),(#350360,#350361,#350362),(#350363,
#350364,#350365),(#350366,#350367,#350368),(#350369,#350370,#350371),(#350372,
#350373,#350374),(#350375,#350376,#350377),(#350378,#350379,#350380),(#350381,
#350382,#350383),(#350384,#350385,#350386),(#350387,#350388,#350389),(#350390,
#350391,#350392),(#350393,#350394,#350395),(#350396,#350397,#350398),(#350399,
#350400,#350401),(#350402,#350403,#350404),(#350405,#350406,#350407),(#350408,
#350409,#350410),(#350411,#350412,#350413),(#350414,#350415,#350416),(#350417,
#350418,#350419),(#350420,#350421,#350422),(#350423,#350424,#350425),(#350426,
#350427,#350428),(#350429,#350430,#350431),(#350432,#350433,#350434),(#350435,
#350436,#350437),(#350438,#350439,#350440),(#350441,#350442,#350443),(#350444,
#350445,#350446),(#350447,#350448,#350449),(#350450,#350451,#350452),(#350453,
#350454,#350455),(#350456,#350457,#350458),(#350459,#350460,#350461),(#350462,
#350463,#350464),(#350465,#350466,#350467),(#350468,#350469,#350470),(#350471,
#350472,#350473),(#350474,#350475,#350476),(#350477,#350478,#350479),(#350480,
#350481,#350482),(#350483,#350484,#350485),(#350486,#350487,#350488),(#350489,
#350490,#350491),(#350492,#350493,#350494),(#350495,#350496,#350497),(#350498,
#350499,#350500),(#350501,#350502,#350503),(#350504,#350505,#350506),(#350507,
#350508,#350509),(#350510,#350511,#350512),(#350513,#350514,#350515),(#350516,
#350517,#350518),(#350519,#350520,#350521),(#350522,#350523,#350524),(#350525,
#350526,#350527),(#350528,#350529,#350530),(#350531,#350532,#350533),(#350534,
#350535,#350536),(#350537,#350538,#350539),(#350540,#350541,#350542),(#350543,
#350544,#350545),(#350546,#350547,#350548),(#350549,#350550,#350551),(#350552,
#350553,#350554),(#350555,#350556,#350557),(#350558,#350559,#350560),(#350561,
#350562,#350563),(#350564,#350565,#350566),(#350567,#350568,#350569),(#350570,
#350571,#350572),(#350573,#350574,#350575),(#350576,#350577,#350578),(#350579,
#350580,#350581),(#350582,#350583,#350584),(#350585,#350586,#350587),(#350588,
#350589,#350590),(#350591,#350592,#350593),(#350594,#350595,#350596),(#350597,
#350598,#350599),(#350600,#350601,#350602),(#350603,#350604,#350605),(#350606,
#350607,#350608),(#350609,#350610,#350611),(#350612,#350613,#350614),(#350615,
#350616,#350617),(#350618,#350619,#350620),(#350621,#350622,#350623),(#350624,
#350625,#350626),(#350627,#350628,#350629),(#350630,#350631,#350632),(#350633,
#350634,#350635),(#350636,#350637,#350638),(#350639,#350640,#350641),(#350642,
#350643,#350644),(#350645,#350646,#350647),(#350648,#350649,#350650),(#350651,
#350652,#350653),(#350654,#350655,#350656),(#350657,#350658,#350659),(#350660,
#350661,#350662),(#350663,#350664,#350665),(#350666,#350667,#350668),(#350669,
#350670,#350671),(#350672,#350673,#350674),(#350675,#350676,#350677),(#350678,
#350679,#350680),(#350681,#350682,#350683),(#350684,#350685,#350686),(#350687,
#350688,#350689),(#350690,#350691,#350692),(#350693,#350694,#350695),(#350696,
#350697,#350698),(#350699,#350700,#350701),(#350702,#350703,#350704),(#350705,
#350706,#350707),(#350708,#350709,#350710),(#350711,#350712,#350713),(#350714,
#350715,#350716),(#350717,#350718,#350719),(#350720,#350721,#350722),(#350723,
#350724,#350725),(#350726,#350727,#350728),(#350729,#350730,#350731),(#350732,
#350733,#350734),(#350735,#350736,#350737),(#350738,#350739,#350740),(#350741,
#350742,#350743),(#350744,#350745,#350746),(#350747,#350748,#350749),(#350750,
#350751,#350752),(#350753,#350754,#350755),(#350756,#350757,#350758),(#350759,
#350760,#350761),(#350762,#350763,#350764),(#350765,#350766,#350767),(#350768,
#350769,#350770),(#350771,#350772,#350773),(#350774,#350775,#350776),(#350777,
#350778,#350779),(#350780,#350781,#350782),(#350783,#350784,#350785),(#350786,
#350787,#350788),(#350789,#350790,#350791),(#350792,#350793,#350794),(#350795,
#350796,#350797),(#350798,#350799,#350800),(#350801,#350802,#350803),(#350804,
#350805,#350806),(#350807,#350808,#350809),(#350810,#350811,#350812),(#350813,
#350814,#350815),(#350816,#350817,#350818),(#350819,#350820,#350821),(#350822,
#350823,#350824),(#350825,#350826,#350827),(#350828,#350829,#350830),(#350831,
#350832,#350833),(#350834,#350835,#350836),(#350837,#350838,#350839),(#350840,
#350841,#350842),(#350843,#350844,#350845),(#350846,#350847,#350848),(#350849,
#350850,#350851),(#350852,#350853,#350854),(#350855,#350856,#350857),(#350858,
#350859,#350860),(#350861,#350862,#350863),(#350864,#350865,#350866),(#350867,
#350868,#350869),(#350870,#350871,#350872),(#350873,#350874,#350875),(#350876,
#350877,#350878),(#350879,#350880,#350881),(#350882,#350883,#350884),(#350885,
#350886,#350887),(#350888,#350889,#350890),(#350891,#350892,#350893),(#350894,
#350895,#350896),(#350897,#350898,#350899),(#350900,#350901,#350902),(#350903,
#350904,#350905),(#350906,#350907,#350908),(#350909,#350910,#350911),(#350912,
#350913,#350914),(#350915,#350916,#350917),(#350918,#350919,#350920),(#350921,
#350922,#350923),(#350924,#350925,#350926),(#350927,#350928,#350929),(#350930,
#350931,#350932),(#350933,#350934,#350935),(#350936,#350937,#350938),(#350939,
#350940,#350941),(#350942,#350943,#350944),(#350945,#350946,#350947),(#350948,
#350949,#350950),(#350951,#350952,#350953),(#350954,#350955,#350956),(#350957,
#350958,#350959),(#350960,#350961,#350962),(#350963,#350964,#350965),(#350966,
#350967,#350968),(#350969,#350970,#350971),(#350972,#350973,#350974),(#350975,
#350976,#350977),(#350978,#350979,#350980),(#350981,#350982,#350983),(#350984,
#350985,#350986),(#350987,#350988,#350989),(#350990,#350991,#350992),(#350993,
#350994,#350995),(#350996,#350997,#350998),(#350999,#351000,#351001),(#351002,
#351003,#351004),(#351005,#351006,#351007),(#351008,#351009,#351010),(#351011,
#351012,#351013),(#351014,#351015,#351016),(#351017,#351018,#351019),(#351020,
#351021,#351022),(#351023,#351024,#351025),(#351026,#351027,#351028),(#351029,
#351030,#351031),(#351032,#351033,#351034),(#351035,#351036,#351037),(#351038,
#351039,#351040),(#351041,#351042,#351043),(#351044,#351045,#351046),(#351047,
#351048,#351049),(#351050,#351051,#351052),(#351053,#351054,#351055),(#351056,
#351057,#351058),(#351059,#351060,#351061),(#351062,#351063,#351064),(#351065,
#351066,#351067),(#351068,#351069,#351070),(#351071,#351072,#351073),(#351074,
#351075,#351076),(#351077,#351078,#351079),(#351080,#351081,#351082),(#351083,
#351084,#351085),(#351086,#351087,#351088),(#351089,#351090,#351091),(#351092,
#351093,#351094),(#351095,#351096,#351097),(#351098,#351099,#351100),(#351101,
#351102,#351103),(#351104,#351105,#351106),(#351107,#351108,#351109),(#351110,
#351111,#351112),(#351113,#351114,#351115),(#351116,#351117,#351118),(#351119,
#351120,#351121),(#351122,#351123,#351124),(#351125,#351126,#351127),(#351128,
#351129,#351130),(#351131,#351132,#351133),(#351134,#351135,#351136),(#351137,
#351138,#351139),(#351140,#351141,#351142),(#351143,#351144,#351145),(#351146,
#351147,#351148),(#351149,#351150,#351151),(#351152,#351153,#351154),(#351155,
#351156,#351157),(#351158,#351159,#351160),(#351161,#351162,#351163),(#351164,
#351165,#351166),(#351167,#351168,#351169),(#351170,#351171,#351172),(#351173,
#351174,#351175),(#351176,#351177,#351178),(#351179,#351180,#351181),(#351182,
#351183,#351184),(#351185,#351186,#351187),(#351188,#351189,#351190),(#351191,
#351192,#351193),(#351194,#351195,#351196),(#351197,#351198,#351199),(#351200,
#351201,#351202),(#351203,#351204,#351205),(#351206,#351207,#351208),(#351209,
#351210,#351211),(#351212,#351213,#351214),(#351215,#351216,#351217),(#351218,
#351219,#351220),(#351221,#351222,#351223),(#351224,#351225,#351226),(#351227,
#351228,#351229),(#351230,#351231,#351232),(#351233,#351234,#351235),(#351236,
#351237,#351238),(#351239,#351240,#351241),(#351242,#351243,#351244),(#351245,
#351246,#351247),(#351248,#351249,#351250),(#351251,#351252,#351253),(#351254,
#351255,#351256),(#351257,#351258,#351259),(#351260,#351261,#351262),(#351263,
#351264,#351265),(#351266,#351267,#351268),(#351269,#351270,#351271),(#351272,
#351273,#351274),(#351275,#351276,#351277),(#351278,#351279,#351280),(#351281,
#351282,#351283),(#351284,#351285,#351286),(#351287,#351288,#351289),(#351290,
#351291,#351292),(#351293,#351294,#351295),(#351296,#351297,#351298),(#351299,
#351300,#351301),(#351302,#351303,#351304),(#351305,#351306,#351307),(#351308,
#351309,#351310),(#351311,#351312,#351313),(#351314,#351315,#351316),(#351317,
#351318,#351319),(#351320,#351321,#351322),(#351323,#351324,#351325),(#351326,
#351327,#351328),(#351329,#351330,#351331),(#351332,#351333,#351334),(#351335,
#351336,#351337),(#351338,#351339,#351340),(#351341,#351342,#351343),(#351344,
#351345,#351346),(#351347,#351348,#351349),(#351350,#351351,#351352),(#351353,
#351354,#351355),(#351356,#351357,#351358),(#351359,#351360,#351361),(#351362,
#351363,#351364),(#351365,#351366,#351367),(#351368,#351369,#351370),(#351371,
#351372,#351373),(#351374,#351375,#351376),(#351377,#351378,#351379),(#351380,
#351381,#351382),(#351383,#351384,#351385),(#351386,#351387,#351388),(#351389,
#351390,#351391),(#351392,#351393,#351394),(#351395,#351396,#351397),(#351398,
#351399,#351400),(#351401,#351402,#351403),(#351404,#351405,#351406),(#351407,
#351408,#351409),(#351410,#351411,#351412),(#351413,#351414,#351415),(#351416,
#351417,#351418),(#351419,#351420,#351421),(#351422,#351423,#351424),(#351425,
#351426,#351427),(#351428,#351429,#351430),(#351431,#351432,#351433),(#351434,
#351435,#351436),(#351437,#351438,#351439),(#351440,#351441,#351442),(#351443,
#351444,#351445),(#351446,#351447,#351448),(#351449,#351450,#351451),(#351452,
#351453,#351454),(#351455,#351456,#351457),(#351458,#351459,#351460),(#351461,
#351462,#351463),(#351464,#351465,#351466),(#351467,#351468,#351469),(#351470,
#351471,#351472),(#351473,#351474,#351475),(#351476,#351477,#351478),(#351479,
#351480,#351481),(#351482,#351483,#351484),(#351485,#351486,#351487),(#351488,
#351489,#351490),(#351491,#351492,#351493),(#351494,#351495,#351496),(#351497,
#351498,#351499),(#351500,#351501,#351502),(#351503,#351504,#351505),(#351506,
#351507,#351508),(#351509,#351510,#351511),(#351512,#351513,#351514),(#351515,
#351516,#351517),(#351518,#351519,#351520),(#351521,#351522,#351523),(#351524,
#351525,#351526)),.UNSPECIFIED.,.F.,.F.,.F.,(6,1,1,1,1,1,1,1,1,1,1,1,1,
1,1,1,1,1,1,1,1,1,1,1,1,1,1,1,1,1,1,1,1,1,1,1,1,1,1,1,1,1,1,1,1,1,1,1,1,
1,1,1,1,1,1,1,1,1,1,1,1,1,1,1,1,1,1,1,1,1,1,1,1,1,1,1,1,1,1,1,1,1,1,1,1,
1,1,1,1,1,1,1,1,1,1,1,1,1,1,1,1,1,1,1,1,1,1,1,1,1,1,1,1,1,1,1,1,1,1,1,1,
1,1,1,1,1,1,1,1,1,1,1,1,1,1,1,1,1,1,1,1,1,1,1,1,1,1,1,1,1,1,1,1,1,1,1,1,
1,1,1,1,1,1,1,1,1,1,1,1,1,1,1,1,1,1,1,1,1,1,1,1,1,1,1,1,1,1,1,1,1,1,1,1,
1,1,1,1,1,1,1,1,1,1,1,1,1,1,1,1,1,1,1,1,1,1,1,1,1,1,1,1,1,1,1,1,1,1,1,1,
1,1,1,1,1,1,1,1,1,1,1,1,1,1,1,1,1,1,1,1,1,1,1,1,1,1,1,1,1,1,1,1,1,1,1,1,
1,1,1,1,1,1,1,1,1,1,1,1,1,1,1,1,1,1,1,1,1,1,1,1,1,1,1,1,1,1,1,1,1,1,1,1,
1,1,1,1,1,1,1,1,1,1,1,1,1,1,1,1,1,1,1,1,1,1,1,1,1,1,1,1,1,1,1,1,1,1,1,1,
1,1,1,1,1,1,1,1,1,1,1,1,1,1,1,1,1,1,1,1,1,1,1,1,1,1,1,1,1,1,1,1,1,1,1,1,
1,1,1,1,1,1,1,1,1,1,1,1,1,1,1,1,1,1,1,1,1,1,1,1,1,1,1,1,1,1,1,1,1,1,1,1,
1,1,1,1,1,1,1,1,1,1,1,1,1,1,1,1,1,1,1,1,1,1,1,1,1,1,1,1,1,1,1,1,1,1,1,1,
1,1,1,1,1,1,1,1,1,1,1,1,1,1,1,1,1,1,1,1,1,1,1,1,1,1,1,1,1,1,1,1,1,1,1,1,
1,1,1,1,1,1,1,1,1,1,1,1,1,1,1,1,1,1,1,1,1,1,1,1,1,1,1,1,1,1,1,1,1,1,1,1,
1,1,1,1,1,1,1,1,1,1,1,1,1,1,1,1,1,1,1,1,1,1,1,1,1,1,1,1,1,6),(2,1,2),(-0.001964172,
0.,0.001834862,0.003669725,0.005504587,0.00733945,0.009174312,0.011009174,
0.012844037,0.014678899,0.016513761,0.018348624,0.020183486,0.022018349,
0.023853211,0.025688073,0.027522936,0.029357798,0.031192661,0.033027523,
0.034862385,0.036697248,0.03853211,0.040366972,0.042201835,0.044036697,
0.04587156,0.047706422,0.049541284,0.051376147,0.053211009,0.055045872,
0.056880734,0.058715596,0.060550459,0.062385321,0.064220183,0.066055046,
0.067889908,0.069724771,0.071559633,0.073394495,0.075229358,0.07706422,
0.078899083,0.080733945,0.082568807,0.08440367,0.086238532,0.088073394,
0.089908257,0.091743119,0.093577982,0.095412844,0.097247706,0.099082569,
0.100917431,0.102752294,0.104587156,0.106422018,0.108256881,0.110091743,
0.111926606,0.113761468,0.11559633,0.117431193,0.119266055,0.121100917,
0.12293578,0.124770642,0.126605505,0.128440367,0.130275229,0.132110092,
0.133944954,0.135779817,0.137614679,0.139449541,0.141284404,0.143119266,
0.144954128,0.146788991,0.148623853,0.150458716,0.152293578,0.15412844,
0.155963303,0.157798165,0.159633028,0.16146789,0.163302752,0.165137615,
0.166972477,0.168807339,0.170642202,0.172477064,0.174311927,0.176146789,
0.177981651,0.179816514,0.181651376,0.183486239,0.185321101,0.187155963,
0.188990826,0.190825688,0.19266055,0.194495413,0.196330275,0.198165138,
0.2,0.201834862,0.203669725,0.205504587,0.20733945,0.209174312,0.211009174,
0.212844037,0.214678899,0.216513761,0.218348624,0.220183486,0.222018349,
0.223853211,0.225688073,0.227522936,0.229357798,0.231192661,0.233027523,
0.234862385,0.236697248,0.23853211,0.240366972,0.242201835,0.244036697,
0.24587156,0.247706422,0.249541284,0.251376147,0.253211009,0.255045872,
0.256880734,0.258715596,0.260550459,0.262385321,0.264220183,0.266055046,
0.267889908,0.269724771,0.271559633,0.273394495,0.275229358,0.27706422,
0.278899083,0.280733945,0.282568807,0.28440367,0.286238532,0.288073394,
0.289908257,0.291743119,0.293577982,0.295412844,0.297247706,0.299082569,
0.300917431,0.302752294,0.304587156,0.306422018,0.308256881,0.310091743,
0.311926606,0.313761468,0.31559633,0.317431193,0.319266055,0.321100917,
0.32293578,0.324770642,0.326605505,0.328440367,0.330275229,0.332110092,
0.333944954,0.335779817,0.337614679,0.339449541,0.341284404,0.343119266,
0.344954128,0.346788991,0.348623853,0.350458716,0.352293578,0.35412844,
0.355963303,0.357798165,0.359633028,0.36146789,0.363302752,0.365137615,
0.366972477,0.368807339,0.370642202,0.372477064,0.374311927,0.376146789,
0.377981651,0.379816514,0.381651376,0.383486239,0.385321101,0.387155963,
0.388990826,0.390825688,0.39266055,0.394495413,0.396330275,0.398165138,
0.4,0.401834862,0.403669725,0.405504587,0.40733945,0.409174312,0.411009174,
0.412844037,0.414678899,0.416513761,0.418348624,0.420183486,0.422018349,
0.423853211,0.425688073,0.427522936,0.429357798,0.431192661,0.433027523,
0.434862385,0.436697248,0.43853211,0.440366972,0.442201835,0.444036697,
0.44587156,0.447706422,0.449541284,0.451376147,0.453211009,0.455045872,
0.456880734,0.458715596,0.460550459,0.462385321,0.464220183,0.466055046,
0.467889908,0.469724771,0.471559633,0.473394495,0.475229358,0.47706422,
0.478899083,0.480733945,0.482568807,0.48440367,0.486238532,0.488073394,
0.489908257,0.491743119,0.493577982,0.495412844,0.497247706,0.499082569,
0.500917431,0.502752294,0.504587156,0.506422018,0.508256881,0.510091743,
0.511926606,0.513761468,0.51559633,0.517431193,0.519266055,0.521100917,
0.52293578,0.524770642,0.526605505,0.528440367,0.530275229,0.532110092,
0.533944954,0.535779817,0.537614679,0.539449541,0.541284404,0.543119266,
0.544954128,0.546788991,0.548623853,0.550458716,0.552293578,0.55412844,
0.555963303,0.557798165,0.559633028,0.56146789,0.563302752,0.565137615,
0.566972477,0.568807339,0.570642202,0.572477064,0.574311927,0.576146789,
0.577981651,0.579816514,0.581651376,0.583486239,0.585321101,0.587155963,
0.588990826,0.590825688,0.59266055,0.594495413,0.596330275,0.598165138,
0.6,0.601834862,0.603669725,0.605504587,0.60733945,0.609174312,0.611009174,
0.612844037,0.614678899,0.616513761,0.618348624,0.620183486,0.622018349,
0.623853211,0.625688073,0.627522936,0.629357798,0.631192661,0.633027523,
0.634862385,0.636697248,0.63853211,0.640366972,0.642201835,0.644036697,
0.64587156,0.647706422,0.649541284,0.651376147,0.653211009,0.655045872,
0.656880734,0.658715596,0.660550459,0.662385321,0.664220183,0.666055046,
0.667889908,0.669724771,0.671559633,0.673394495,0.675229358,0.67706422,
0.678899083,0.680733945,0.682568807,0.68440367,0.686238532,0.688073394,
0.689908257,0.691743119,0.693577982,0.695412844,0.697247706,0.699082569,
0.700917431,0.702752294,0.704587156,0.706422018,0.708256881,0.710091743,
0.711926606,0.713761468,0.71559633,0.717431193,0.719266055,0.721100917,
0.72293578,0.724770642,0.726605505,0.728440367,0.730275229,0.732110092,
0.733944954,0.735779817,0.737614679,0.739449541,0.741284404,0.743119266,
0.744954128,0.746788991,0.748623853,0.750458716,0.752293578,0.75412844,
0.755963303,0.757798165,0.759633028,0.76146789,0.763302752,0.765137615,
0.766972477,0.768807339,0.770642202,0.772477064,0.774311927,0.776146789,
0.777981651,0.779816514,0.781651376,0.783486239,0.785321101,0.787155963,
0.788990826,0.790825688,0.79266055,0.794495413,0.796330275,0.798165138,
0.8,0.801834862,0.803669725,0.805504587,0.80733945,0.809174312,0.811009174,
0.812844037,0.814678899,0.816513761,0.818348624,0.820183486,0.822018349,
0.823853211,0.825688073,0.827522936,0.829357798,0.831192661,0.833027523,
0.834862385,0.836697248,0.83853211,0.840366972,0.842201835,0.844036697,
0.84587156,0.847706422,0.849541284,0.851376147,0.853211009,0.855045872,
0.856880734,0.858715596,0.860550459,0.862385321,0.864220183,0.866055046,
0.867889908,0.869724771,0.871559633,0.873394495,0.875229358,0.87706422,
0.878899083,0.880733945,0.882568807,0.88440367,0.886238532,0.888073394,
0.889908257,0.891743119,0.893577982,0.895412844,0.897247706,0.899082569,
0.900917431,0.902752294,0.904587156,0.906422018,0.908256881,0.910091743,
0.911926606,0.913761468,0.91559633,0.917431193,0.919266055,0.921100917,
0.92293578,0.924770642,0.926605505,0.928440367,0.930275229,0.932110092,
0.933944954,0.935779817,0.937614679,0.939449541,0.941284404,0.943119266,
0.944954128,0.946788991,0.948623853,0.950458716,0.952293578,0.95412844,
0.955963303,0.957798165,0.959633028,0.96146789,0.963302752,0.965137615,
0.966972477,0.968807339,0.970642202,0.972477064,0.974311927,0.976146789,
0.977981651,0.979816514,0.981651376,0.983486239,0.985321101,0.987155963,
0.988990826,0.990825688,0.99266055,0.994495413,0.996330275,0.998165138,
1.),(0.3,1.,1.3),.UNSPECIFIED.);
#6333=B_SPLINE_SURFACE_WITH_KNOTS('',5,1,((#351531,#351532,#351533),(#351534,
#351535,#351536),(#351537,#351538,#351539),(#351540,#351541,#351542),(#351543,
#351544,#351545),(#351546,#351547,#351548),(#351549,#351550,#351551),(#351552,
#351553,#351554),(#351555,#351556,#351557),(#351558,#351559,#351560),(#351561,
#351562,#351563),(#351564,#351565,#351566),(#351567,#351568,#351569),(#351570,
#351571,#351572),(#351573,#351574,#351575),(#351576,#351577,#351578),(#351579,
#351580,#351581),(#351582,#351583,#351584),(#351585,#351586,#351587),(#351588,
#351589,#351590),(#351591,#351592,#351593),(#351594,#351595,#351596),(#351597,
#351598,#351599),(#351600,#351601,#351602),(#351603,#351604,#351605),(#351606,
#351607,#351608),(#351609,#351610,#351611),(#351612,#351613,#351614),(#351615,
#351616,#351617),(#351618,#351619,#351620),(#351621,#351622,#351623),(#351624,
#351625,#351626),(#351627,#351628,#351629),(#351630,#351631,#351632),(#351633,
#351634,#351635),(#351636,#351637,#351638),(#351639,#351640,#351641),(#351642,
#351643,#351644),(#351645,#351646,#351647),(#351648,#351649,#351650),(#351651,
#351652,#351653),(#351654,#351655,#351656),(#351657,#351658,#351659),(#351660,
#351661,#351662),(#351663,#351664,#351665),(#351666,#351667,#351668),(#351669,
#351670,#351671),(#351672,#351673,#351674),(#351675,#351676,#351677),(#351678,
#351679,#351680),(#351681,#351682,#351683),(#351684,#351685,#351686),(#351687,
#351688,#351689),(#351690,#351691,#351692),(#351693,#351694,#351695),(#351696,
#351697,#351698),(#351699,#351700,#351701),(#351702,#351703,#351704),(#351705,
#351706,#351707),(#351708,#351709,#351710),(#351711,#351712,#351713),(#351714,
#351715,#351716),(#351717,#351718,#351719),(#351720,#351721,#351722),(#351723,
#351724,#351725),(#351726,#351727,#351728),(#351729,#351730,#351731),(#351732,
#351733,#351734),(#351735,#351736,#351737),(#351738,#351739,#351740),(#351741,
#351742,#351743),(#351744,#351745,#351746),(#351747,#351748,#351749),(#351750,
#351751,#351752),(#351753,#351754,#351755),(#351756,#351757,#351758),(#351759,
#351760,#351761),(#351762,#351763,#351764),(#351765,#351766,#351767),(#351768,
#351769,#351770),(#351771,#351772,#351773),(#351774,#351775,#351776),(#351777,
#351778,#351779),(#351780,#351781,#351782),(#351783,#351784,#351785),(#351786,
#351787,#351788),(#351789,#351790,#351791),(#351792,#351793,#351794),(#351795,
#351796,#351797),(#351798,#351799,#351800),(#351801,#351802,#351803),(#351804,
#351805,#351806),(#351807,#351808,#351809),(#351810,#351811,#351812),(#351813,
#351814,#351815),(#351816,#351817,#351818),(#351819,#351820,#351821),(#351822,
#351823,#351824),(#351825,#351826,#351827),(#351828,#351829,#351830),(#351831,
#351832,#351833),(#351834,#351835,#351836),(#351837,#351838,#351839),(#351840,
#351841,#351842),(#351843,#351844,#351845),(#351846,#351847,#351848),(#351849,
#351850,#351851),(#351852,#351853,#351854),(#351855,#351856,#351857),(#351858,
#351859,#351860),(#351861,#351862,#351863),(#351864,#351865,#351866),(#351867,
#351868,#351869),(#351870,#351871,#351872),(#351873,#351874,#351875),(#351876,
#351877,#351878),(#351879,#351880,#351881),(#351882,#351883,#351884),(#351885,
#351886,#351887),(#351888,#351889,#351890),(#351891,#351892,#351893),(#351894,
#351895,#351896),(#351897,#351898,#351899),(#351900,#351901,#351902),(#351903,
#351904,#351905),(#351906,#351907,#351908),(#351909,#351910,#351911),(#351912,
#351913,#351914),(#351915,#351916,#351917),(#351918,#351919,#351920),(#351921,
#351922,#351923),(#351924,#351925,#351926),(#351927,#351928,#351929),(#351930,
#351931,#351932),(#351933,#351934,#351935),(#351936,#351937,#351938),(#351939,
#351940,#351941),(#351942,#351943,#351944),(#351945,#351946,#351947),(#351948,
#351949,#351950),(#351951,#351952,#351953),(#351954,#351955,#351956),(#351957,
#351958,#351959),(#351960,#351961,#351962),(#351963,#351964,#351965),(#351966,
#351967,#351968),(#351969,#351970,#351971),(#351972,#351973,#351974),(#351975,
#351976,#351977),(#351978,#351979,#351980),(#351981,#351982,#351983),(#351984,
#351985,#351986),(#351987,#351988,#351989),(#351990,#351991,#351992),(#351993,
#351994,#351995),(#351996,#351997,#351998),(#351999,#352000,#352001),(#352002,
#352003,#352004),(#352005,#352006,#352007),(#352008,#352009,#352010),(#352011,
#352012,#352013),(#352014,#352015,#352016),(#352017,#352018,#352019),(#352020,
#352021,#352022),(#352023,#352024,#352025),(#352026,#352027,#352028),(#352029,
#352030,#352031),(#352032,#352033,#352034),(#352035,#352036,#352037),(#352038,
#352039,#352040),(#352041,#352042,#352043),(#352044,#352045,#352046),(#352047,
#352048,#352049),(#352050,#352051,#352052),(#352053,#352054,#352055),(#352056,
#352057,#352058),(#352059,#352060,#352061),(#352062,#352063,#352064),(#352065,
#352066,#352067),(#352068,#352069,#352070),(#352071,#352072,#352073),(#352074,
#352075,#352076),(#352077,#352078,#352079),(#352080,#352081,#352082),(#352083,
#352084,#352085),(#352086,#352087,#352088),(#352089,#352090,#352091),(#352092,
#352093,#352094),(#352095,#352096,#352097),(#352098,#352099,#352100),(#352101,
#352102,#352103),(#352104,#352105,#352106),(#352107,#352108,#352109),(#352110,
#352111,#352112),(#352113,#352114,#352115),(#352116,#352117,#352118),(#352119,
#352120,#352121),(#352122,#352123,#352124),(#352125,#352126,#352127),(#352128,
#352129,#352130),(#352131,#352132,#352133),(#352134,#352135,#352136),(#352137,
#352138,#352139),(#352140,#352141,#352142),(#352143,#352144,#352145),(#352146,
#352147,#352148),(#352149,#352150,#352151),(#352152,#352153,#352154),(#352155,
#352156,#352157),(#352158,#352159,#352160),(#352161,#352162,#352163),(#352164,
#352165,#352166),(#352167,#352168,#352169),(#352170,#352171,#352172),(#352173,
#352174,#352175),(#352176,#352177,#352178),(#352179,#352180,#352181),(#352182,
#352183,#352184),(#352185,#352186,#352187),(#352188,#352189,#352190),(#352191,
#352192,#352193),(#352194,#352195,#352196),(#352197,#352198,#352199),(#352200,
#352201,#352202),(#352203,#352204,#352205),(#352206,#352207,#352208),(#352209,
#352210,#352211),(#352212,#352213,#352214),(#352215,#352216,#352217),(#352218,
#352219,#352220),(#352221,#352222,#352223),(#352224,#352225,#352226),(#352227,
#352228,#352229),(#352230,#352231,#352232),(#352233,#352234,#352235),(#352236,
#352237,#352238),(#352239,#352240,#352241),(#352242,#352243,#352244),(#352245,
#352246,#352247),(#352248,#352249,#352250),(#352251,#352252,#352253),(#352254,
#352255,#352256),(#352257,#352258,#352259),(#352260,#352261,#352262),(#352263,
#352264,#352265),(#352266,#352267,#352268),(#352269,#352270,#352271),(#352272,
#352273,#352274),(#352275,#352276,#352277),(#352278,#352279,#352280),(#352281,
#352282,#352283),(#352284,#352285,#352286),(#352287,#352288,#352289),(#352290,
#352291,#352292),(#352293,#352294,#352295),(#352296,#352297,#352298),(#352299,
#352300,#352301),(#352302,#352303,#352304),(#352305,#352306,#352307),(#352308,
#352309,#352310),(#352311,#352312,#352313),(#352314,#352315,#352316),(#352317,
#352318,#352319),(#352320,#352321,#352322),(#352323,#352324,#352325),(#352326,
#352327,#352328),(#352329,#352330,#352331),(#352332,#352333,#352334),(#352335,
#352336,#352337),(#352338,#352339,#352340),(#352341,#352342,#352343),(#352344,
#352345,#352346),(#352347,#352348,#352349),(#352350,#352351,#352352),(#352353,
#352354,#352355),(#352356,#352357,#352358),(#352359,#352360,#352361),(#352362,
#352363,#352364),(#352365,#352366,#352367),(#352368,#352369,#352370),(#352371,
#352372,#352373),(#352374,#352375,#352376),(#352377,#352378,#352379),(#352380,
#352381,#352382),(#352383,#352384,#352385),(#352386,#352387,#352388),(#352389,
#352390,#352391),(#352392,#352393,#352394),(#352395,#352396,#352397),(#352398,
#352399,#352400),(#352401,#352402,#352403),(#352404,#352405,#352406),(#352407,
#352408,#352409),(#352410,#352411,#352412),(#352413,#352414,#352415),(#352416,
#352417,#352418),(#352419,#352420,#352421),(#352422,#352423,#352424),(#352425,
#352426,#352427),(#352428,#352429,#352430),(#352431,#352432,#352433),(#352434,
#352435,#352436),(#352437,#352438,#352439),(#352440,#352441,#352442),(#352443,
#352444,#352445),(#352446,#352447,#352448),(#352449,#352450,#352451),(#352452,
#352453,#352454),(#352455,#352456,#352457),(#352458,#352459,#352460),(#352461,
#352462,#352463),(#352464,#352465,#352466),(#352467,#352468,#352469),(#352470,
#352471,#352472),(#352473,#352474,#352475),(#352476,#352477,#352478),(#352479,
#352480,#352481),(#352482,#352483,#352484),(#352485,#352486,#352487),(#352488,
#352489,#352490),(#352491,#352492,#352493),(#352494,#352495,#352496),(#352497,
#352498,#352499),(#352500,#352501,#352502),(#352503,#352504,#352505),(#352506,
#352507,#352508),(#352509,#352510,#352511),(#352512,#352513,#352514),(#352515,
#352516,#352517),(#352518,#352519,#352520),(#352521,#352522,#352523),(#352524,
#352525,#352526),(#352527,#352528,#352529),(#352530,#352531,#352532),(#352533,
#352534,#352535),(#352536,#352537,#352538),(#352539,#352540,#352541),(#352542,
#352543,#352544),(#352545,#352546,#352547),(#352548,#352549,#352550),(#352551,
#352552,#352553),(#352554,#352555,#352556),(#352557,#352558,#352559),(#352560,
#352561,#352562),(#352563,#352564,#352565),(#352566,#352567,#352568),(#352569,
#352570,#352571),(#352572,#352573,#352574),(#352575,#352576,#352577),(#352578,
#352579,#352580),(#352581,#352582,#352583),(#352584,#352585,#352586),(#352587,
#352588,#352589),(#352590,#352591,#352592),(#352593,#352594,#352595),(#352596,
#352597,#352598),(#352599,#352600,#352601),(#352602,#352603,#352604),(#352605,
#352606,#352607),(#352608,#352609,#352610),(#352611,#352612,#352613),(#352614,
#352615,#352616),(#352617,#352618,#352619),(#352620,#352621,#352622),(#352623,
#352624,#352625),(#352626,#352627,#352628),(#352629,#352630,#352631),(#352632,
#352633,#352634),(#352635,#352636,#352637),(#352638,#352639,#352640),(#352641,
#352642,#352643),(#352644,#352645,#352646),(#352647,#352648,#352649),(#352650,
#352651,#352652),(#352653,#352654,#352655),(#352656,#352657,#352658),(#352659,
#352660,#352661),(#352662,#352663,#352664),(#352665,#352666,#352667),(#352668,
#352669,#352670),(#352671,#352672,#352673),(#352674,#352675,#352676),(#352677,
#352678,#352679),(#352680,#352681,#352682),(#352683,#352684,#352685),(#352686,
#352687,#352688),(#352689,#352690,#352691),(#352692,#352693,#352694),(#352695,
#352696,#352697),(#352698,#352699,#352700),(#352701,#352702,#352703),(#352704,
#352705,#352706),(#352707,#352708,#352709),(#352710,#352711,#352712),(#352713,
#352714,#352715),(#352716,#352717,#352718),(#352719,#352720,#352721),(#352722,
#352723,#352724),(#352725,#352726,#352727),(#352728,#352729,#352730),(#352731,
#352732,#352733),(#352734,#352735,#352736),(#352737,#352738,#352739),(#352740,
#352741,#352742),(#352743,#352744,#352745),(#352746,#352747,#352748),(#352749,
#352750,#352751),(#352752,#352753,#352754),(#352755,#352756,#352757),(#352758,
#352759,#352760),(#352761,#352762,#352763),(#352764,#352765,#352766),(#352767,
#352768,#352769),(#352770,#352771,#352772),(#352773,#352774,#352775),(#352776,
#352777,#352778),(#352779,#352780,#352781),(#352782,#352783,#352784),(#352785,
#352786,#352787),(#352788,#352789,#352790),(#352791,#352792,#352793),(#352794,
#352795,#352796),(#352797,#352798,#352799),(#352800,#352801,#352802),(#352803,
#352804,#352805),(#352806,#352807,#352808),(#352809,#352810,#352811),(#352812,
#352813,#352814),(#352815,#352816,#352817),(#352818,#352819,#352820),(#352821,
#352822,#352823),(#352824,#352825,#352826),(#352827,#352828,#352829),(#352830,
#352831,#352832),(#352833,#352834,#352835),(#352836,#352837,#352838),(#352839,
#352840,#352841),(#352842,#352843,#352844),(#352845,#352846,#352847),(#352848,
#352849,#352850),(#352851,#352852,#352853),(#352854,#352855,#352856),(#352857,
#352858,#352859),(#352860,#352861,#352862),(#352863,#352864,#352865),(#352866,
#352867,#352868),(#352869,#352870,#352871),(#352872,#352873,#352874),(#352875,
#352876,#352877),(#352878,#352879,#352880),(#352881,#352882,#352883),(#352884,
#352885,#352886),(#352887,#352888,#352889),(#352890,#352891,#352892),(#352893,
#352894,#352895),(#352896,#352897,#352898),(#352899,#352900,#352901),(#352902,
#352903,#352904),(#352905,#352906,#352907),(#352908,#352909,#352910),(#352911,
#352912,#352913),(#352914,#352915,#352916),(#352917,#352918,#352919),(#352920,
#352921,#352922),(#352923,#352924,#352925),(#352926,#352927,#352928),(#352929,
#352930,#352931),(#352932,#352933,#352934),(#352935,#352936,#352937),(#352938,
#352939,#352940),(#352941,#352942,#352943),(#352944,#352945,#352946),(#352947,
#352948,#352949),(#352950,#352951,#352952),(#352953,#352954,#352955),(#352956,
#352957,#352958),(#352959,#352960,#352961),(#352962,#352963,#352964),(#352965,
#352966,#352967),(#352968,#352969,#352970),(#352971,#352972,#352973),(#352974,
#352975,#352976),(#352977,#352978,#352979),(#352980,#352981,#352982),(#352983,
#352984,#352985),(#352986,#352987,#352988),(#352989,#352990,#352991),(#352992,
#352993,#352994),(#352995,#352996,#352997),(#352998,#352999,#353000),(#353001,
#353002,#353003),(#353004,#353005,#353006),(#353007,#353008,#353009),(#353010,
#353011,#353012),(#353013,#353014,#353015),(#353016,#353017,#353018),(#353019,
#353020,#353021),(#353022,#353023,#353024),(#353025,#353026,#353027),(#353028,
#353029,#353030),(#353031,#353032,#353033),(#353034,#353035,#353036),(#353037,
#353038,#353039),(#353040,#353041,#353042),(#353043,#353044,#353045),(#353046,
#353047,#353048),(#353049,#353050,#353051),(#353052,#353053,#353054),(#353055,
#353056,#353057),(#353058,#353059,#353060),(#353061,#353062,#353063),(#353064,
#353065,#353066),(#353067,#353068,#353069),(#353070,#353071,#353072),(#353073,
#353074,#353075),(#353076,#353077,#353078),(#353079,#353080,#353081),(#353082,
#353083,#353084),(#353085,#353086,#353087),(#353088,#353089,#353090),(#353091,
#353092,#353093),(#353094,#353095,#353096),(#353097,#353098,#353099),(#353100,
#353101,#353102),(#353103,#353104,#353105),(#353106,#353107,#353108),(#353109,
#353110,#353111),(#353112,#353113,#353114),(#353115,#353116,#353117),(#353118,
#353119,#353120),(#353121,#353122,#353123),(#353124,#353125,#353126),(#353127,
#353128,#353129),(#353130,#353131,#353132),(#353133,#353134,#353135),(#353136,
#353137,#353138),(#353139,#353140,#353141),(#353142,#353143,#353144),(#353145,
#353146,#353147),(#353148,#353149,#353150),(#353151,#353152,#353153),(#353154,
#353155,#353156),(#353157,#353158,#353159),(#353160,#353161,#353162),(#353163,
#353164,#353165),(#353166,#353167,#353168),(#353169,#353170,#353171),(#353172,
#353173,#353174),(#353175,#353176,#353177),(#353178,#353179,#353180)),
 .UNSPECIFIED.,.F.,.F.,.F.,(6,1,1,1,1,1,1,1,1,1,1,1,1,1,1,1,1,1,1,1,1,1,
1,1,1,1,1,1,1,1,1,1,1,1,1,1,1,1,1,1,1,1,1,1,1,1,1,1,1,1,1,1,1,1,1,1,1,1,
1,1,1,1,1,1,1,1,1,1,1,1,1,1,1,1,1,1,1,1,1,1,1,1,1,1,1,1,1,1,1,1,1,1,1,1,
1,1,1,1,1,1,1,1,1,1,1,1,1,1,1,1,1,1,1,1,1,1,1,1,1,1,1,1,1,1,1,1,1,1,1,1,
1,1,1,1,1,1,1,1,1,1,1,1,1,1,1,1,1,1,1,1,1,1,1,1,1,1,1,1,1,1,1,1,1,1,1,1,
1,1,1,1,1,1,1,1,1,1,1,1,1,1,1,1,1,1,1,1,1,1,1,1,1,1,1,1,1,1,1,1,1,1,1,1,
1,1,1,1,1,1,1,1,1,1,1,1,1,1,1,1,1,1,1,1,1,1,1,1,1,1,1,1,1,1,1,1,1,1,1,1,
1,1,1,1,1,1,1,1,1,1,1,1,1,1,1,1,1,1,1,1,1,1,1,1,1,1,1,1,1,1,1,1,1,1,1,1,
1,1,1,1,1,1,1,1,1,1,1,1,1,1,1,1,1,1,1,1,1,1,1,1,1,1,1,1,1,1,1,1,1,1,1,1,
1,1,1,1,1,1,1,1,1,1,1,1,1,1,1,1,1,1,1,1,1,1,1,1,1,1,1,1,1,1,1,1,1,1,1,1,
1,1,1,1,1,1,1,1,1,1,1,1,1,1,1,1,1,1,1,1,1,1,1,1,1,1,1,1,1,1,1,1,1,1,1,1,
1,1,1,1,1,1,1,1,1,1,1,1,1,1,1,1,1,1,1,1,1,1,1,1,1,1,1,1,1,1,1,1,1,1,1,1,
1,1,1,1,1,1,1,1,1,1,1,1,1,1,1,1,1,1,1,1,1,1,1,1,1,1,1,1,1,1,1,1,1,1,1,1,
1,1,1,1,1,1,1,1,1,1,1,1,1,1,1,1,1,1,1,1,1,1,1,1,1,1,1,1,1,1,1,1,1,1,1,1,
1,1,1,1,1,1,1,1,1,1,1,1,1,1,1,1,1,1,1,1,1,1,1,1,1,1,1,1,1,1,1,1,1,1,1,1,
1,1,1,1,1,1,1,1,1,1,1,1,1,1,1,1,1,1,1,6),(2,1,2),(-1.,-0.998165138,-0.996330275,
-0.994495413,-0.99266055,-0.990825688,-0.988990826,-0.987155963,-0.985321101,
-0.983486239,-0.981651376,-0.979816514,-0.977981651,-0.976146789,-0.974311927,
-0.972477064,-0.970642202,-0.968807339,-0.966972477,-0.965137615,-0.963302752,
-0.96146789,-0.959633028,-0.957798165,-0.955963303,-0.95412844,-0.952293578,
-0.950458716,-0.948623853,-0.946788991,-0.944954128,-0.943119266,-0.941284404,
-0.939449541,-0.937614679,-0.935779817,-0.933944954,-0.932110092,-0.930275229,
-0.928440367,-0.926605505,-0.924770642,-0.92293578,-0.921100917,-0.919266055,
-0.917431193,-0.91559633,-0.913761468,-0.911926606,-0.910091743,-0.908256881,
-0.906422018,-0.904587156,-0.902752294,-0.900917431,-0.899082569,-0.897247706,
-0.895412844,-0.893577982,-0.891743119,-0.889908257,-0.888073394,-0.886238532,
-0.88440367,-0.882568807,-0.880733945,-0.878899083,-0.87706422,-0.875229358,
-0.873394495,-0.871559633,-0.869724771,-0.867889908,-0.866055046,-0.864220183,
-0.862385321,-0.860550459,-0.858715596,-0.856880734,-0.855045872,-0.853211009,
-0.851376147,-0.849541284,-0.847706422,-0.84587156,-0.844036697,-0.842201835,
-0.840366972,-0.83853211,-0.836697248,-0.834862385,-0.833027523,-0.831192661,
-0.829357798,-0.827522936,-0.825688073,-0.823853211,-0.822018349,-0.820183486,
-0.818348624,-0.816513761,-0.814678899,-0.812844037,-0.811009174,-0.809174312,
-0.80733945,-0.805504587,-0.803669725,-0.801834862,-0.8,-0.798165138,-0.796330275,
-0.794495413,-0.79266055,-0.790825688,-0.788990826,-0.787155963,-0.785321101,
-0.783486239,-0.781651376,-0.779816514,-0.777981651,-0.776146789,-0.774311927,
-0.772477064,-0.770642202,-0.768807339,-0.766972477,-0.765137615,-0.763302752,
-0.76146789,-0.759633028,-0.757798165,-0.755963303,-0.75412844,-0.752293578,
-0.750458716,-0.748623853,-0.746788991,-0.744954128,-0.743119266,-0.741284404,
-0.739449541,-0.737614679,-0.735779817,-0.733944954,-0.732110092,-0.730275229,
-0.728440367,-0.726605505,-0.724770642,-0.72293578,-0.721100917,-0.719266055,
-0.717431193,-0.71559633,-0.713761468,-0.711926606,-0.710091743,-0.708256881,
-0.706422018,-0.704587156,-0.702752294,-0.700917431,-0.699082569,-0.697247706,
-0.695412844,-0.693577982,-0.691743119,-0.689908257,-0.688073394,-0.686238532,
-0.68440367,-0.682568807,-0.680733945,-0.678899083,-0.67706422,-0.675229358,
-0.673394495,-0.671559633,-0.669724771,-0.667889908,-0.666055046,-0.664220183,
-0.662385321,-0.660550459,-0.658715596,-0.656880734,-0.655045872,-0.653211009,
-0.651376147,-0.649541284,-0.647706422,-0.64587156,-0.644036697,-0.642201835,
-0.640366972,-0.63853211,-0.636697248,-0.634862385,-0.633027523,-0.631192661,
-0.629357798,-0.627522936,-0.625688073,-0.623853211,-0.622018349,-0.620183486,
-0.618348624,-0.616513761,-0.614678899,-0.612844037,-0.611009174,-0.609174312,
-0.60733945,-0.605504587,-0.603669725,-0.601834862,-0.6,-0.598165138,-0.596330275,
-0.594495413,-0.59266055,-0.590825688,-0.588990826,-0.587155963,-0.585321101,
-0.583486239,-0.581651376,-0.579816514,-0.577981651,-0.576146789,-0.574311927,
-0.572477064,-0.570642202,-0.568807339,-0.566972477,-0.565137615,-0.563302752,
-0.56146789,-0.559633028,-0.557798165,-0.555963303,-0.55412844,-0.552293578,
-0.550458716,-0.548623853,-0.546788991,-0.544954128,-0.543119266,-0.541284404,
-0.539449541,-0.537614679,-0.535779817,-0.533944954,-0.532110092,-0.530275229,
-0.528440367,-0.526605505,-0.524770642,-0.52293578,-0.521100917,-0.519266055,
-0.517431193,-0.51559633,-0.513761468,-0.511926606,-0.510091743,-0.508256881,
-0.506422018,-0.504587156,-0.502752294,-0.500917431,-0.499082569,-0.497247706,
-0.495412844,-0.493577982,-0.491743119,-0.489908257,-0.488073394,-0.486238532,
-0.48440367,-0.482568807,-0.480733945,-0.478899083,-0.47706422,-0.475229358,
-0.473394495,-0.471559633,-0.469724771,-0.467889908,-0.466055046,-0.464220183,
-0.462385321,-0.460550459,-0.458715596,-0.456880734,-0.455045872,-0.453211009,
-0.451376147,-0.449541284,-0.447706422,-0.44587156,-0.444036697,-0.442201835,
-0.440366972,-0.43853211,-0.436697248,-0.434862385,-0.433027523,-0.431192661,
-0.429357798,-0.427522936,-0.425688073,-0.423853211,-0.422018349,-0.420183486,
-0.418348624,-0.416513761,-0.414678899,-0.412844037,-0.411009174,-0.409174312,
-0.40733945,-0.405504587,-0.403669725,-0.401834862,-0.4,-0.398165138,-0.396330275,
-0.394495413,-0.39266055,-0.390825688,-0.388990826,-0.387155963,-0.385321101,
-0.383486239,-0.381651376,-0.379816514,-0.377981651,-0.376146789,-0.374311927,
-0.372477064,-0.370642202,-0.368807339,-0.366972477,-0.365137615,-0.363302752,
-0.36146789,-0.359633028,-0.357798165,-0.355963303,-0.35412844,-0.352293578,
-0.350458716,-0.348623853,-0.346788991,-0.344954128,-0.343119266,-0.341284404,
-0.339449541,-0.337614679,-0.335779817,-0.333944954,-0.332110092,-0.330275229,
-0.328440367,-0.326605505,-0.324770642,-0.32293578,-0.321100917,-0.319266055,
-0.317431193,-0.31559633,-0.313761468,-0.311926606,-0.310091743,-0.308256881,
-0.306422018,-0.304587156,-0.302752294,-0.300917431,-0.299082569,-0.297247706,
-0.295412844,-0.293577982,-0.291743119,-0.289908257,-0.288073394,-0.286238532,
-0.28440367,-0.282568807,-0.280733945,-0.278899083,-0.27706422,-0.275229358,
-0.273394495,-0.271559633,-0.269724771,-0.267889908,-0.266055046,-0.264220183,
-0.262385321,-0.260550459,-0.258715596,-0.256880734,-0.255045872,-0.253211009,
-0.251376147,-0.249541284,-0.247706422,-0.24587156,-0.244036697,-0.242201835,
-0.240366972,-0.23853211,-0.236697248,-0.234862385,-0.233027523,-0.231192661,
-0.229357798,-0.227522936,-0.225688073,-0.223853211,-0.222018349,-0.220183486,
-0.218348624,-0.216513761,-0.214678899,-0.212844037,-0.211009174,-0.209174312,
-0.20733945,-0.205504587,-0.203669725,-0.201834862,-0.2,-0.198165138,-0.196330275,
-0.194495413,-0.19266055,-0.190825688,-0.188990826,-0.187155963,-0.185321101,
-0.183486239,-0.181651376,-0.179816514,-0.177981651,-0.176146789,-0.174311927,
-0.172477064,-0.170642202,-0.168807339,-0.166972477,-0.165137615,-0.163302752,
-0.16146789,-0.159633028,-0.157798165,-0.155963303,-0.15412844,-0.152293578,
-0.150458716,-0.148623853,-0.146788991,-0.144954128,-0.143119266,-0.141284404,
-0.139449541,-0.137614679,-0.135779817,-0.133944954,-0.132110092,-0.130275229,
-0.128440367,-0.126605505,-0.124770642,-0.12293578,-0.121100917,-0.119266055,
-0.117431193,-0.11559633,-0.113761468,-0.111926606,-0.110091743,-0.108256881,
-0.106422018,-0.104587156,-0.102752294,-0.100917431,-0.099082569,-0.097247706,
-0.095412844,-0.093577982,-0.091743119,-0.089908257,-0.088073394,-0.086238532,
-0.08440367,-0.082568807,-0.080733945,-0.078899083,-0.07706422,-0.075229358,
-0.073394495,-0.071559633,-0.069724771,-0.067889908,-0.066055046,-0.064220183,
-0.062385321,-0.060550459,-0.058715596,-0.056880734,-0.055045872,-0.053211009,
-0.051376147,-0.049541284,-0.047706422,-0.04587156,-0.044036697,-0.042201835,
-0.040366972,-0.03853211,-0.036697248,-0.034862385,-0.033027523,-0.031192661,
-0.029357798,-0.027522936,-0.025688073,-0.023853211,-0.022018349,-0.020183486,
-0.018348624,-0.016513761,-0.014678899,-0.012844037,-0.011009174,-0.009174312,
-0.00733945,-0.005504587,-0.003669725,-0.001834862,0.000982134),(0.3,1.,
1.3),.UNSPECIFIED.);
#6334=B_SPLINE_SURFACE_WITH_KNOTS('',5,1,((#353184,#353185,#353186),(#353187,
#353188,#353189),(#353190,#353191,#353192),(#353193,#353194,#353195),(#353196,
#353197,#353198),(#353199,#353200,#353201),(#353202,#353203,#353204),(#353205,
#353206,#353207),(#353208,#353209,#353210),(#353211,#353212,#353213),(#353214,
#353215,#353216),(#353217,#353218,#353219),(#353220,#353221,#353222),(#353223,
#353224,#353225),(#353226,#353227,#353228),(#353229,#353230,#353231),(#353232,
#353233,#353234),(#353235,#353236,#353237),(#353238,#353239,#353240),(#353241,
#353242,#353243),(#353244,#353245,#353246),(#353247,#353248,#353249),(#353250,
#353251,#353252),(#353253,#353254,#353255),(#353256,#353257,#353258),(#353259,
#353260,#353261),(#353262,#353263,#353264),(#353265,#353266,#353267),(#353268,
#353269,#353270),(#353271,#353272,#353273),(#353274,#353275,#353276),(#353277,
#353278,#353279),(#353280,#353281,#353282),(#353283,#353284,#353285),(#353286,
#353287,#353288),(#353289,#353290,#353291),(#353292,#353293,#353294),(#353295,
#353296,#353297),(#353298,#353299,#353300),(#353301,#353302,#353303),(#353304,
#353305,#353306),(#353307,#353308,#353309),(#353310,#353311,#353312),(#353313,
#353314,#353315),(#353316,#353317,#353318),(#353319,#353320,#353321),(#353322,
#353323,#353324),(#353325,#353326,#353327),(#353328,#353329,#353330),(#353331,
#353332,#353333),(#353334,#353335,#353336),(#353337,#353338,#353339),(#353340,
#353341,#353342),(#353343,#353344,#353345),(#353346,#353347,#353348),(#353349,
#353350,#353351),(#353352,#353353,#353354),(#353355,#353356,#353357),(#353358,
#353359,#353360),(#353361,#353362,#353363),(#353364,#353365,#353366),(#353367,
#353368,#353369),(#353370,#353371,#353372),(#353373,#353374,#353375),(#353376,
#353377,#353378),(#353379,#353380,#353381),(#353382,#353383,#353384),(#353385,
#353386,#353387),(#353388,#353389,#353390),(#353391,#353392,#353393),(#353394,
#353395,#353396),(#353397,#353398,#353399),(#353400,#353401,#353402),(#353403,
#353404,#353405),(#353406,#353407,#353408),(#353409,#353410,#353411),(#353412,
#353413,#353414),(#353415,#353416,#353417),(#353418,#353419,#353420),(#353421,
#353422,#353423),(#353424,#353425,#353426),(#353427,#353428,#353429),(#353430,
#353431,#353432),(#353433,#353434,#353435),(#353436,#353437,#353438),(#353439,
#353440,#353441),(#353442,#353443,#353444),(#353445,#353446,#353447),(#353448,
#353449,#353450),(#353451,#353452,#353453),(#353454,#353455,#353456),(#353457,
#353458,#353459),(#353460,#353461,#353462),(#353463,#353464,#353465),(#353466,
#353467,#353468),(#353469,#353470,#353471),(#353472,#353473,#353474),(#353475,
#353476,#353477),(#353478,#353479,#353480),(#353481,#353482,#353483),(#353484,
#353485,#353486),(#353487,#353488,#353489),(#353490,#353491,#353492),(#353493,
#353494,#353495),(#353496,#353497,#353498),(#353499,#353500,#353501),(#353502,
#353503,#353504),(#353505,#353506,#353507),(#353508,#353509,#353510),(#353511,
#353512,#353513),(#353514,#353515,#353516),(#353517,#353518,#353519),(#353520,
#353521,#353522),(#353523,#353524,#353525),(#353526,#353527,#353528),(#353529,
#353530,#353531),(#353532,#353533,#353534),(#353535,#353536,#353537),(#353538,
#353539,#353540),(#353541,#353542,#353543),(#353544,#353545,#353546),(#353547,
#353548,#353549),(#353550,#353551,#353552),(#353553,#353554,#353555),(#353556,
#353557,#353558),(#353559,#353560,#353561),(#353562,#353563,#353564),(#353565,
#353566,#353567),(#353568,#353569,#353570),(#353571,#353572,#353573),(#353574,
#353575,#353576),(#353577,#353578,#353579),(#353580,#353581,#353582),(#353583,
#353584,#353585),(#353586,#353587,#353588),(#353589,#353590,#353591),(#353592,
#353593,#353594),(#353595,#353596,#353597),(#353598,#353599,#353600),(#353601,
#353602,#353603),(#353604,#353605,#353606),(#353607,#353608,#353609),(#353610,
#353611,#353612),(#353613,#353614,#353615),(#353616,#353617,#353618),(#353619,
#353620,#353621),(#353622,#353623,#353624),(#353625,#353626,#353627),(#353628,
#353629,#353630),(#353631,#353632,#353633),(#353634,#353635,#353636),(#353637,
#353638,#353639),(#353640,#353641,#353642),(#353643,#353644,#353645),(#353646,
#353647,#353648),(#353649,#353650,#353651),(#353652,#353653,#353654),(#353655,
#353656,#353657),(#353658,#353659,#353660),(#353661,#353662,#353663),(#353664,
#353665,#353666),(#353667,#353668,#353669),(#353670,#353671,#353672),(#353673,
#353674,#353675),(#353676,#353677,#353678),(#353679,#353680,#353681),(#353682,
#353683,#353684),(#353685,#353686,#353687),(#353688,#353689,#353690),(#353691,
#353692,#353693),(#353694,#353695,#353696),(#353697,#353698,#353699),(#353700,
#353701,#353702),(#353703,#353704,#353705),(#353706,#353707,#353708),(#353709,
#353710,#353711),(#353712,#353713,#353714),(#353715,#353716,#353717),(#353718,
#353719,#353720),(#353721,#353722,#353723),(#353724,#353725,#353726),(#353727,
#353728,#353729),(#353730,#353731,#353732),(#353733,#353734,#353735),(#353736,
#353737,#353738),(#353739,#353740,#353741),(#353742,#353743,#353744),(#353745,
#353746,#353747),(#353748,#353749,#353750),(#353751,#353752,#353753),(#353754,
#353755,#353756),(#353757,#353758,#353759),(#353760,#353761,#353762),(#353763,
#353764,#353765),(#353766,#353767,#353768),(#353769,#353770,#353771),(#353772,
#353773,#353774),(#353775,#353776,#353777),(#353778,#353779,#353780),(#353781,
#353782,#353783),(#353784,#353785,#353786),(#353787,#353788,#353789),(#353790,
#353791,#353792),(#353793,#353794,#353795),(#353796,#353797,#353798),(#353799,
#353800,#353801),(#353802,#353803,#353804),(#353805,#353806,#353807),(#353808,
#353809,#353810),(#353811,#353812,#353813),(#353814,#353815,#353816),(#353817,
#353818,#353819),(#353820,#353821,#353822),(#353823,#353824,#353825),(#353826,
#353827,#353828),(#353829,#353830,#353831),(#353832,#353833,#353834),(#353835,
#353836,#353837),(#353838,#353839,#353840),(#353841,#353842,#353843),(#353844,
#353845,#353846),(#353847,#353848,#353849),(#353850,#353851,#353852),(#353853,
#353854,#353855),(#353856,#353857,#353858),(#353859,#353860,#353861),(#353862,
#353863,#353864),(#353865,#353866,#353867),(#353868,#353869,#353870),(#353871,
#353872,#353873),(#353874,#353875,#353876),(#353877,#353878,#353879),(#353880,
#353881,#353882),(#353883,#353884,#353885),(#353886,#353887,#353888),(#353889,
#353890,#353891),(#353892,#353893,#353894),(#353895,#353896,#353897),(#353898,
#353899,#353900),(#353901,#353902,#353903),(#353904,#353905,#353906),(#353907,
#353908,#353909),(#353910,#353911,#353912),(#353913,#353914,#353915),(#353916,
#353917,#353918),(#353919,#353920,#353921),(#353922,#353923,#353924),(#353925,
#353926,#353927),(#353928,#353929,#353930),(#353931,#353932,#353933),(#353934,
#353935,#353936),(#353937,#353938,#353939),(#353940,#353941,#353942),(#353943,
#353944,#353945),(#353946,#353947,#353948),(#353949,#353950,#353951),(#353952,
#353953,#353954),(#353955,#353956,#353957),(#353958,#353959,#353960),(#353961,
#353962,#353963),(#353964,#353965,#353966),(#353967,#353968,#353969),(#353970,
#353971,#353972),(#353973,#353974,#353975),(#353976,#353977,#353978),(#353979,
#353980,#353981),(#353982,#353983,#353984),(#353985,#353986,#353987),(#353988,
#353989,#353990),(#353991,#353992,#353993),(#353994,#353995,#353996),(#353997,
#353998,#353999),(#354000,#354001,#354002),(#354003,#354004,#354005),(#354006,
#354007,#354008),(#354009,#354010,#354011),(#354012,#354013,#354014),(#354015,
#354016,#354017),(#354018,#354019,#354020),(#354021,#354022,#354023),(#354024,
#354025,#354026),(#354027,#354028,#354029),(#354030,#354031,#354032),(#354033,
#354034,#354035),(#354036,#354037,#354038),(#354039,#354040,#354041),(#354042,
#354043,#354044),(#354045,#354046,#354047),(#354048,#354049,#354050),(#354051,
#354052,#354053),(#354054,#354055,#354056),(#354057,#354058,#354059),(#354060,
#354061,#354062),(#354063,#354064,#354065),(#354066,#354067,#354068),(#354069,
#354070,#354071),(#354072,#354073,#354074),(#354075,#354076,#354077),(#354078,
#354079,#354080),(#354081,#354082,#354083),(#354084,#354085,#354086),(#354087,
#354088,#354089),(#354090,#354091,#354092),(#354093,#354094,#354095),(#354096,
#354097,#354098),(#354099,#354100,#354101),(#354102,#354103,#354104),(#354105,
#354106,#354107),(#354108,#354109,#354110),(#354111,#354112,#354113),(#354114,
#354115,#354116),(#354117,#354118,#354119),(#354120,#354121,#354122),(#354123,
#354124,#354125),(#354126,#354127,#354128),(#354129,#354130,#354131),(#354132,
#354133,#354134),(#354135,#354136,#354137),(#354138,#354139,#354140),(#354141,
#354142,#354143),(#354144,#354145,#354146),(#354147,#354148,#354149),(#354150,
#354151,#354152),(#354153,#354154,#354155),(#354156,#354157,#354158),(#354159,
#354160,#354161),(#354162,#354163,#354164),(#354165,#354166,#354167),(#354168,
#354169,#354170),(#354171,#354172,#354173),(#354174,#354175,#354176),(#354177,
#354178,#354179),(#354180,#354181,#354182),(#354183,#354184,#354185),(#354186,
#354187,#354188),(#354189,#354190,#354191),(#354192,#354193,#354194),(#354195,
#354196,#354197),(#354198,#354199,#354200),(#354201,#354202,#354203),(#354204,
#354205,#354206),(#354207,#354208,#354209),(#354210,#354211,#354212),(#354213,
#354214,#354215),(#354216,#354217,#354218),(#354219,#354220,#354221),(#354222,
#354223,#354224),(#354225,#354226,#354227),(#354228,#354229,#354230),(#354231,
#354232,#354233),(#354234,#354235,#354236),(#354237,#354238,#354239),(#354240,
#354241,#354242),(#354243,#354244,#354245),(#354246,#354247,#354248),(#354249,
#354250,#354251),(#354252,#354253,#354254),(#354255,#354256,#354257),(#354258,
#354259,#354260),(#354261,#354262,#354263),(#354264,#354265,#354266),(#354267,
#354268,#354269),(#354270,#354271,#354272),(#354273,#354274,#354275),(#354276,
#354277,#354278),(#354279,#354280,#354281),(#354282,#354283,#354284),(#354285,
#354286,#354287),(#354288,#354289,#354290),(#354291,#354292,#354293),(#354294,
#354295,#354296),(#354297,#354298,#354299),(#354300,#354301,#354302),(#354303,
#354304,#354305),(#354306,#354307,#354308),(#354309,#354310,#354311),(#354312,
#354313,#354314),(#354315,#354316,#354317),(#354318,#354319,#354320),(#354321,
#354322,#354323),(#354324,#354325,#354326),(#354327,#354328,#354329),(#354330,
#354331,#354332),(#354333,#354334,#354335),(#354336,#354337,#354338),(#354339,
#354340,#354341),(#354342,#354343,#354344),(#354345,#354346,#354347),(#354348,
#354349,#354350),(#354351,#354352,#354353),(#354354,#354355,#354356),(#354357,
#354358,#354359),(#354360,#354361,#354362),(#354363,#354364,#354365),(#354366,
#354367,#354368),(#354369,#354370,#354371),(#354372,#354373,#354374),(#354375,
#354376,#354377),(#354378,#354379,#354380),(#354381,#354382,#354383),(#354384,
#354385,#354386),(#354387,#354388,#354389),(#354390,#354391,#354392),(#354393,
#354394,#354395),(#354396,#354397,#354398),(#354399,#354400,#354401),(#354402,
#354403,#354404),(#354405,#354406,#354407),(#354408,#354409,#354410),(#354411,
#354412,#354413),(#354414,#354415,#354416),(#354417,#354418,#354419),(#354420,
#354421,#354422),(#354423,#354424,#354425),(#354426,#354427,#354428),(#354429,
#354430,#354431),(#354432,#354433,#354434),(#354435,#354436,#354437),(#354438,
#354439,#354440),(#354441,#354442,#354443),(#354444,#354445,#354446),(#354447,
#354448,#354449),(#354450,#354451,#354452),(#354453,#354454,#354455),(#354456,
#354457,#354458),(#354459,#354460,#354461),(#354462,#354463,#354464),(#354465,
#354466,#354467),(#354468,#354469,#354470),(#354471,#354472,#354473),(#354474,
#354475,#354476),(#354477,#354478,#354479),(#354480,#354481,#354482),(#354483,
#354484,#354485),(#354486,#354487,#354488),(#354489,#354490,#354491),(#354492,
#354493,#354494),(#354495,#354496,#354497),(#354498,#354499,#354500),(#354501,
#354502,#354503),(#354504,#354505,#354506),(#354507,#354508,#354509),(#354510,
#354511,#354512),(#354513,#354514,#354515),(#354516,#354517,#354518),(#354519,
#354520,#354521),(#354522,#354523,#354524),(#354525,#354526,#354527),(#354528,
#354529,#354530),(#354531,#354532,#354533),(#354534,#354535,#354536),(#354537,
#354538,#354539),(#354540,#354541,#354542),(#354543,#354544,#354545),(#354546,
#354547,#354548),(#354549,#354550,#354551),(#354552,#354553,#354554),(#354555,
#354556,#354557),(#354558,#354559,#354560),(#354561,#354562,#354563),(#354564,
#354565,#354566),(#354567,#354568,#354569),(#354570,#354571,#354572),(#354573,
#354574,#354575),(#354576,#354577,#354578),(#354579,#354580,#354581),(#354582,
#354583,#354584),(#354585,#354586,#354587),(#354588,#354589,#354590),(#354591,
#354592,#354593),(#354594,#354595,#354596),(#354597,#354598,#354599),(#354600,
#354601,#354602),(#354603,#354604,#354605),(#354606,#354607,#354608),(#354609,
#354610,#354611),(#354612,#354613,#354614),(#354615,#354616,#354617),(#354618,
#354619,#354620),(#354621,#354622,#354623),(#354624,#354625,#354626),(#354627,
#354628,#354629),(#354630,#354631,#354632),(#354633,#354634,#354635),(#354636,
#354637,#354638),(#354639,#354640,#354641),(#354642,#354643,#354644),(#354645,
#354646,#354647),(#354648,#354649,#354650),(#354651,#354652,#354653),(#354654,
#354655,#354656),(#354657,#354658,#354659),(#354660,#354661,#354662),(#354663,
#354664,#354665),(#354666,#354667,#354668),(#354669,#354670,#354671),(#354672,
#354673,#354674),(#354675,#354676,#354677),(#354678,#354679,#354680),(#354681,
#354682,#354683),(#354684,#354685,#354686),(#354687,#354688,#354689),(#354690,
#354691,#354692),(#354693,#354694,#354695),(#354696,#354697,#354698),(#354699,
#354700,#354701),(#354702,#354703,#354704),(#354705,#354706,#354707),(#354708,
#354709,#354710),(#354711,#354712,#354713),(#354714,#354715,#354716),(#354717,
#354718,#354719),(#354720,#354721,#354722),(#354723,#354724,#354725),(#354726,
#354727,#354728),(#354729,#354730,#354731),(#354732,#354733,#354734),(#354735,
#354736,#354737),(#354738,#354739,#354740),(#354741,#354742,#354743),(#354744,
#354745,#354746),(#354747,#354748,#354749),(#354750,#354751,#354752),(#354753,
#354754,#354755),(#354756,#354757,#354758),(#354759,#354760,#354761),(#354762,
#354763,#354764),(#354765,#354766,#354767),(#354768,#354769,#354770),(#354771,
#354772,#354773),(#354774,#354775,#354776),(#354777,#354778,#354779),(#354780,
#354781,#354782),(#354783,#354784,#354785),(#354786,#354787,#354788),(#354789,
#354790,#354791),(#354792,#354793,#354794),(#354795,#354796,#354797),(#354798,
#354799,#354800),(#354801,#354802,#354803),(#354804,#354805,#354806),(#354807,
#354808,#354809),(#354810,#354811,#354812),(#354813,#354814,#354815),(#354816,
#354817,#354818),(#354819,#354820,#354821),(#354822,#354823,#354824),(#354825,
#354826,#354827),(#354828,#354829,#354830),(#354831,#354832,#354833),(#354834,
#354835,#354836)),.UNSPECIFIED.,.F.,.F.,.F.,(6,1,1,1,1,1,1,1,1,1,1,1,1,
1,1,1,1,1,1,1,1,1,1,1,1,1,1,1,1,1,1,1,1,1,1,1,1,1,1,1,1,1,1,1,1,1,1,1,1,
1,1,1,1,1,1,1,1,1,1,1,1,1,1,1,1,1,1,1,1,1,1,1,1,1,1,1,1,1,1,1,1,1,1,1,1,
1,1,1,1,1,1,1,1,1,1,1,1,1,1,1,1,1,1,1,1,1,1,1,1,1,1,1,1,1,1,1,1,1,1,1,1,
1,1,1,1,1,1,1,1,1,1,1,1,1,1,1,1,1,1,1,1,1,1,1,1,1,1,1,1,1,1,1,1,1,1,1,1,
1,1,1,1,1,1,1,1,1,1,1,1,1,1,1,1,1,1,1,1,1,1,1,1,1,1,1,1,1,1,1,1,1,1,1,1,
1,1,1,1,1,1,1,1,1,1,1,1,1,1,1,1,1,1,1,1,1,1,1,1,1,1,1,1,1,1,1,1,1,1,1,1,
1,1,1,1,1,1,1,1,1,1,1,1,1,1,1,1,1,1,1,1,1,1,1,1,1,1,1,1,1,1,1,1,1,1,1,1,
1,1,1,1,1,1,1,1,1,1,1,1,1,1,1,1,1,1,1,1,1,1,1,1,1,1,1,1,1,1,1,1,1,1,1,1,
1,1,1,1,1,1,1,1,1,1,1,1,1,1,1,1,1,1,1,1,1,1,1,1,1,1,1,1,1,1,1,1,1,1,1,1,
1,1,1,1,1,1,1,1,1,1,1,1,1,1,1,1,1,1,1,1,1,1,1,1,1,1,1,1,1,1,1,1,1,1,1,1,
1,1,1,1,1,1,1,1,1,1,1,1,1,1,1,1,1,1,1,1,1,1,1,1,1,1,1,1,1,1,1,1,1,1,1,1,
1,1,1,1,1,1,1,1,1,1,1,1,1,1,1,1,1,1,1,1,1,1,1,1,1,1,1,1,1,1,1,1,1,1,1,1,
1,1,1,1,1,1,1,1,1,1,1,1,1,1,1,1,1,1,1,1,1,1,1,1,1,1,1,1,1,1,1,1,1,1,1,1,
1,1,1,1,1,1,1,1,1,1,1,1,1,1,1,1,1,1,1,1,1,1,1,1,1,1,1,1,1,1,1,1,1,1,1,1,
1,1,1,1,1,1,1,1,1,1,1,1,1,1,1,1,1,1,1,1,1,1,1,1,1,1,1,1,1,6),(2,1,2),(-0.001964168,
0.,0.001834862,0.003669725,0.005504587,0.00733945,0.009174312,0.011009174,
0.012844037,0.014678899,0.016513761,0.018348624,0.020183486,0.022018349,
0.023853211,0.025688073,0.027522936,0.029357798,0.031192661,0.033027523,
0.034862385,0.036697248,0.03853211,0.040366972,0.042201835,0.044036697,
0.04587156,0.047706422,0.049541284,0.051376147,0.053211009,0.055045872,
0.056880734,0.058715596,0.060550459,0.062385321,0.064220183,0.066055046,
0.067889908,0.069724771,0.071559633,0.073394495,0.075229358,0.07706422,
0.078899083,0.080733945,0.082568807,0.08440367,0.086238532,0.088073394,
0.089908257,0.091743119,0.093577982,0.095412844,0.097247706,0.099082569,
0.100917431,0.102752294,0.104587156,0.106422018,0.108256881,0.110091743,
0.111926606,0.113761468,0.11559633,0.117431193,0.119266055,0.121100917,
0.12293578,0.124770642,0.126605505,0.128440367,0.130275229,0.132110092,
0.133944954,0.135779817,0.137614679,0.139449541,0.141284404,0.143119266,
0.144954128,0.146788991,0.148623853,0.150458716,0.152293578,0.15412844,
0.155963303,0.157798165,0.159633028,0.16146789,0.163302752,0.165137615,
0.166972477,0.168807339,0.170642202,0.172477064,0.174311927,0.176146789,
0.177981651,0.179816514,0.181651376,0.183486239,0.185321101,0.187155963,
0.188990826,0.190825688,0.19266055,0.194495413,0.196330275,0.198165138,
0.2,0.201834862,0.203669725,0.205504587,0.20733945,0.209174312,0.211009174,
0.212844037,0.214678899,0.216513761,0.218348624,0.220183486,0.222018349,
0.223853211,0.225688073,0.227522936,0.229357798,0.231192661,0.233027523,
0.234862385,0.236697248,0.23853211,0.240366972,0.242201835,0.244036697,
0.24587156,0.247706422,0.249541284,0.251376147,0.253211009,0.255045872,
0.256880734,0.258715596,0.260550459,0.262385321,0.264220183,0.266055046,
0.267889908,0.269724771,0.271559633,0.273394495,0.275229358,0.27706422,
0.278899083,0.280733945,0.282568807,0.28440367,0.286238532,0.288073394,
0.289908257,0.291743119,0.293577982,0.295412844,0.297247706,0.299082569,
0.300917431,0.302752294,0.304587156,0.306422018,0.308256881,0.310091743,
0.311926606,0.313761468,0.31559633,0.317431193,0.319266055,0.321100917,
0.32293578,0.324770642,0.326605505,0.328440367,0.330275229,0.332110092,
0.333944954,0.335779817,0.337614679,0.339449541,0.341284404,0.343119266,
0.344954128,0.346788991,0.348623853,0.350458716,0.352293578,0.35412844,
0.355963303,0.357798165,0.359633028,0.36146789,0.363302752,0.365137615,
0.366972477,0.368807339,0.370642202,0.372477064,0.374311927,0.376146789,
0.377981651,0.379816514,0.381651376,0.383486239,0.385321101,0.387155963,
0.388990826,0.390825688,0.39266055,0.394495413,0.396330275,0.398165138,
0.4,0.401834862,0.403669725,0.405504587,0.40733945,0.409174312,0.411009174,
0.412844037,0.414678899,0.416513761,0.418348624,0.420183486,0.422018349,
0.423853211,0.425688073,0.427522936,0.429357798,0.431192661,0.433027523,
0.434862385,0.436697248,0.43853211,0.440366972,0.442201835,0.444036697,
0.44587156,0.447706422,0.449541284,0.451376147,0.453211009,0.455045872,
0.456880734,0.458715596,0.460550459,0.462385321,0.464220183,0.466055046,
0.467889908,0.469724771,0.471559633,0.473394495,0.475229358,0.47706422,
0.478899083,0.480733945,0.482568807,0.48440367,0.486238532,0.488073394,
0.489908257,0.491743119,0.493577982,0.495412844,0.497247706,0.499082569,
0.500917431,0.502752294,0.504587156,0.506422018,0.508256881,0.510091743,
0.511926606,0.513761468,0.51559633,0.517431193,0.519266055,0.521100917,
0.52293578,0.524770642,0.526605505,0.528440367,0.530275229,0.532110092,
0.533944954,0.535779817,0.537614679,0.539449541,0.541284404,0.543119266,
0.544954128,0.546788991,0.548623853,0.550458716,0.552293578,0.55412844,
0.555963303,0.557798165,0.559633028,0.56146789,0.563302752,0.565137615,
0.566972477,0.568807339,0.570642202,0.572477064,0.574311927,0.576146789,
0.577981651,0.579816514,0.581651376,0.583486239,0.585321101,0.587155963,
0.588990826,0.590825688,0.59266055,0.594495413,0.596330275,0.598165138,
0.6,0.601834862,0.603669725,0.605504587,0.60733945,0.609174312,0.611009174,
0.612844037,0.614678899,0.616513761,0.618348624,0.620183486,0.622018349,
0.623853211,0.625688073,0.627522936,0.629357798,0.631192661,0.633027523,
0.634862385,0.636697248,0.63853211,0.640366972,0.642201835,0.644036697,
0.64587156,0.647706422,0.649541284,0.651376147,0.653211009,0.655045872,
0.656880734,0.658715596,0.660550459,0.662385321,0.664220183,0.666055046,
0.667889908,0.669724771,0.671559633,0.673394495,0.675229358,0.67706422,
0.678899083,0.680733945,0.682568807,0.68440367,0.686238532,0.688073394,
0.689908257,0.691743119,0.693577982,0.695412844,0.697247706,0.699082569,
0.700917431,0.702752294,0.704587156,0.706422018,0.708256881,0.710091743,
0.711926606,0.713761468,0.71559633,0.717431193,0.719266055,0.721100917,
0.72293578,0.724770642,0.726605505,0.728440367,0.730275229,0.732110092,
0.733944954,0.735779817,0.737614679,0.739449541,0.741284404,0.743119266,
0.744954128,0.746788991,0.748623853,0.750458716,0.752293578,0.75412844,
0.755963303,0.757798165,0.759633028,0.76146789,0.763302752,0.765137615,
0.766972477,0.768807339,0.770642202,0.772477064,0.774311927,0.776146789,
0.777981651,0.779816514,0.781651376,0.783486239,0.785321101,0.787155963,
0.788990826,0.790825688,0.79266055,0.794495413,0.796330275,0.798165138,
0.8,0.801834862,0.803669725,0.805504587,0.80733945,0.809174312,0.811009174,
0.812844037,0.814678899,0.816513761,0.818348624,0.820183486,0.822018349,
0.823853211,0.825688073,0.827522936,0.829357798,0.831192661,0.833027523,
0.834862385,0.836697248,0.83853211,0.840366972,0.842201835,0.844036697,
0.84587156,0.847706422,0.849541284,0.851376147,0.853211009,0.855045872,
0.856880734,0.858715596,0.860550459,0.862385321,0.864220183,0.866055046,
0.867889908,0.869724771,0.871559633,0.873394495,0.875229358,0.87706422,
0.878899083,0.880733945,0.882568807,0.88440367,0.886238532,0.888073394,
0.889908257,0.891743119,0.893577982,0.895412844,0.897247706,0.899082569,
0.900917431,0.902752294,0.904587156,0.906422018,0.908256881,0.910091743,
0.911926606,0.913761468,0.91559633,0.917431193,0.919266055,0.921100917,
0.92293578,0.924770642,0.926605505,0.928440367,0.930275229,0.932110092,
0.933944954,0.935779817,0.937614679,0.939449541,0.941284404,0.943119266,
0.944954128,0.946788991,0.948623853,0.950458716,0.952293578,0.95412844,
0.955963303,0.957798165,0.959633028,0.96146789,0.963302752,0.965137615,
0.966972477,0.968807339,0.970642202,0.972477064,0.974311927,0.976146789,
0.977981651,0.979816514,0.981651376,0.983486239,0.985321101,0.987155963,
0.988990826,0.990825688,0.99266055,0.994495413,0.996330275,0.998165138,
1.),(0.3,1.,1.3),.UNSPECIFIED.);
#6335=B_SPLINE_SURFACE_WITH_KNOTS('',5,1,((#354848,#354849,#354850),(#354851,
#354852,#354853),(#354854,#354855,#354856),(#354857,#354858,#354859),(#354860,
#354861,#354862),(#354863,#354864,#354865),(#354866,#354867,#354868),(#354869,
#354870,#354871),(#354872,#354873,#354874),(#354875,#354876,#354877),(#354878,
#354879,#354880),(#354881,#354882,#354883),(#354884,#354885,#354886),(#354887,
#354888,#354889),(#354890,#354891,#354892),(#354893,#354894,#354895),(#354896,
#354897,#354898),(#354899,#354900,#354901),(#354902,#354903,#354904),(#354905,
#354906,#354907),(#354908,#354909,#354910),(#354911,#354912,#354913),(#354914,
#354915,#354916),(#354917,#354918,#354919),(#354920,#354921,#354922),(#354923,
#354924,#354925),(#354926,#354927,#354928),(#354929,#354930,#354931),(#354932,
#354933,#354934),(#354935,#354936,#354937),(#354938,#354939,#354940),(#354941,
#354942,#354943),(#354944,#354945,#354946),(#354947,#354948,#354949),(#354950,
#354951,#354952),(#354953,#354954,#354955),(#354956,#354957,#354958),(#354959,
#354960,#354961),(#354962,#354963,#354964),(#354965,#354966,#354967),(#354968,
#354969,#354970),(#354971,#354972,#354973),(#354974,#354975,#354976),(#354977,
#354978,#354979),(#354980,#354981,#354982),(#354983,#354984,#354985),(#354986,
#354987,#354988),(#354989,#354990,#354991),(#354992,#354993,#354994),(#354995,
#354996,#354997),(#354998,#354999,#355000),(#355001,#355002,#355003),(#355004,
#355005,#355006),(#355007,#355008,#355009),(#355010,#355011,#355012),(#355013,
#355014,#355015),(#355016,#355017,#355018),(#355019,#355020,#355021),(#355022,
#355023,#355024),(#355025,#355026,#355027),(#355028,#355029,#355030),(#355031,
#355032,#355033),(#355034,#355035,#355036),(#355037,#355038,#355039),(#355040,
#355041,#355042),(#355043,#355044,#355045),(#355046,#355047,#355048),(#355049,
#355050,#355051),(#355052,#355053,#355054),(#355055,#355056,#355057),(#355058,
#355059,#355060),(#355061,#355062,#355063),(#355064,#355065,#355066),(#355067,
#355068,#355069),(#355070,#355071,#355072),(#355073,#355074,#355075),(#355076,
#355077,#355078),(#355079,#355080,#355081),(#355082,#355083,#355084),(#355085,
#355086,#355087),(#355088,#355089,#355090),(#355091,#355092,#355093),(#355094,
#355095,#355096),(#355097,#355098,#355099),(#355100,#355101,#355102),(#355103,
#355104,#355105),(#355106,#355107,#355108),(#355109,#355110,#355111),(#355112,
#355113,#355114),(#355115,#355116,#355117),(#355118,#355119,#355120),(#355121,
#355122,#355123),(#355124,#355125,#355126),(#355127,#355128,#355129),(#355130,
#355131,#355132),(#355133,#355134,#355135),(#355136,#355137,#355138),(#355139,
#355140,#355141),(#355142,#355143,#355144),(#355145,#355146,#355147),(#355148,
#355149,#355150),(#355151,#355152,#355153),(#355154,#355155,#355156),(#355157,
#355158,#355159),(#355160,#355161,#355162),(#355163,#355164,#355165),(#355166,
#355167,#355168),(#355169,#355170,#355171),(#355172,#355173,#355174),(#355175,
#355176,#355177),(#355178,#355179,#355180),(#355181,#355182,#355183),(#355184,
#355185,#355186),(#355187,#355188,#355189),(#355190,#355191,#355192),(#355193,
#355194,#355195),(#355196,#355197,#355198),(#355199,#355200,#355201),(#355202,
#355203,#355204),(#355205,#355206,#355207),(#355208,#355209,#355210),(#355211,
#355212,#355213),(#355214,#355215,#355216),(#355217,#355218,#355219),(#355220,
#355221,#355222),(#355223,#355224,#355225),(#355226,#355227,#355228),(#355229,
#355230,#355231),(#355232,#355233,#355234),(#355235,#355236,#355237),(#355238,
#355239,#355240),(#355241,#355242,#355243),(#355244,#355245,#355246),(#355247,
#355248,#355249),(#355250,#355251,#355252),(#355253,#355254,#355255),(#355256,
#355257,#355258),(#355259,#355260,#355261),(#355262,#355263,#355264),(#355265,
#355266,#355267),(#355268,#355269,#355270),(#355271,#355272,#355273),(#355274,
#355275,#355276),(#355277,#355278,#355279),(#355280,#355281,#355282),(#355283,
#355284,#355285),(#355286,#355287,#355288),(#355289,#355290,#355291),(#355292,
#355293,#355294),(#355295,#355296,#355297),(#355298,#355299,#355300),(#355301,
#355302,#355303),(#355304,#355305,#355306),(#355307,#355308,#355309),(#355310,
#355311,#355312),(#355313,#355314,#355315),(#355316,#355317,#355318),(#355319,
#355320,#355321),(#355322,#355323,#355324),(#355325,#355326,#355327),(#355328,
#355329,#355330),(#355331,#355332,#355333),(#355334,#355335,#355336),(#355337,
#355338,#355339),(#355340,#355341,#355342),(#355343,#355344,#355345),(#355346,
#355347,#355348),(#355349,#355350,#355351),(#355352,#355353,#355354),(#355355,
#355356,#355357),(#355358,#355359,#355360),(#355361,#355362,#355363),(#355364,
#355365,#355366),(#355367,#355368,#355369),(#355370,#355371,#355372),(#355373,
#355374,#355375),(#355376,#355377,#355378),(#355379,#355380,#355381),(#355382,
#355383,#355384),(#355385,#355386,#355387),(#355388,#355389,#355390),(#355391,
#355392,#355393),(#355394,#355395,#355396),(#355397,#355398,#355399),(#355400,
#355401,#355402),(#355403,#355404,#355405),(#355406,#355407,#355408),(#355409,
#355410,#355411),(#355412,#355413,#355414),(#355415,#355416,#355417),(#355418,
#355419,#355420),(#355421,#355422,#355423),(#355424,#355425,#355426),(#355427,
#355428,#355429),(#355430,#355431,#355432),(#355433,#355434,#355435),(#355436,
#355437,#355438),(#355439,#355440,#355441),(#355442,#355443,#355444),(#355445,
#355446,#355447),(#355448,#355449,#355450),(#355451,#355452,#355453),(#355454,
#355455,#355456),(#355457,#355458,#355459),(#355460,#355461,#355462),(#355463,
#355464,#355465),(#355466,#355467,#355468),(#355469,#355470,#355471),(#355472,
#355473,#355474),(#355475,#355476,#355477),(#355478,#355479,#355480),(#355481,
#355482,#355483),(#355484,#355485,#355486),(#355487,#355488,#355489),(#355490,
#355491,#355492),(#355493,#355494,#355495),(#355496,#355497,#355498),(#355499,
#355500,#355501),(#355502,#355503,#355504),(#355505,#355506,#355507),(#355508,
#355509,#355510),(#355511,#355512,#355513),(#355514,#355515,#355516),(#355517,
#355518,#355519),(#355520,#355521,#355522),(#355523,#355524,#355525),(#355526,
#355527,#355528),(#355529,#355530,#355531),(#355532,#355533,#355534),(#355535,
#355536,#355537),(#355538,#355539,#355540),(#355541,#355542,#355543),(#355544,
#355545,#355546),(#355547,#355548,#355549),(#355550,#355551,#355552),(#355553,
#355554,#355555),(#355556,#355557,#355558),(#355559,#355560,#355561),(#355562,
#355563,#355564),(#355565,#355566,#355567),(#355568,#355569,#355570),(#355571,
#355572,#355573),(#355574,#355575,#355576),(#355577,#355578,#355579),(#355580,
#355581,#355582),(#355583,#355584,#355585),(#355586,#355587,#355588),(#355589,
#355590,#355591),(#355592,#355593,#355594),(#355595,#355596,#355597),(#355598,
#355599,#355600),(#355601,#355602,#355603),(#355604,#355605,#355606),(#355607,
#355608,#355609),(#355610,#355611,#355612),(#355613,#355614,#355615),(#355616,
#355617,#355618),(#355619,#355620,#355621),(#355622,#355623,#355624),(#355625,
#355626,#355627),(#355628,#355629,#355630),(#355631,#355632,#355633),(#355634,
#355635,#355636),(#355637,#355638,#355639),(#355640,#355641,#355642),(#355643,
#355644,#355645),(#355646,#355647,#355648),(#355649,#355650,#355651),(#355652,
#355653,#355654),(#355655,#355656,#355657),(#355658,#355659,#355660),(#355661,
#355662,#355663),(#355664,#355665,#355666),(#355667,#355668,#355669),(#355670,
#355671,#355672),(#355673,#355674,#355675),(#355676,#355677,#355678),(#355679,
#355680,#355681),(#355682,#355683,#355684),(#355685,#355686,#355687),(#355688,
#355689,#355690),(#355691,#355692,#355693),(#355694,#355695,#355696),(#355697,
#355698,#355699),(#355700,#355701,#355702),(#355703,#355704,#355705),(#355706,
#355707,#355708),(#355709,#355710,#355711),(#355712,#355713,#355714),(#355715,
#355716,#355717),(#355718,#355719,#355720),(#355721,#355722,#355723),(#355724,
#355725,#355726),(#355727,#355728,#355729),(#355730,#355731,#355732),(#355733,
#355734,#355735),(#355736,#355737,#355738),(#355739,#355740,#355741),(#355742,
#355743,#355744),(#355745,#355746,#355747),(#355748,#355749,#355750),(#355751,
#355752,#355753),(#355754,#355755,#355756),(#355757,#355758,#355759),(#355760,
#355761,#355762),(#355763,#355764,#355765),(#355766,#355767,#355768),(#355769,
#355770,#355771),(#355772,#355773,#355774),(#355775,#355776,#355777),(#355778,
#355779,#355780),(#355781,#355782,#355783),(#355784,#355785,#355786),(#355787,
#355788,#355789),(#355790,#355791,#355792),(#355793,#355794,#355795),(#355796,
#355797,#355798),(#355799,#355800,#355801),(#355802,#355803,#355804),(#355805,
#355806,#355807),(#355808,#355809,#355810),(#355811,#355812,#355813),(#355814,
#355815,#355816),(#355817,#355818,#355819),(#355820,#355821,#355822),(#355823,
#355824,#355825),(#355826,#355827,#355828),(#355829,#355830,#355831),(#355832,
#355833,#355834),(#355835,#355836,#355837),(#355838,#355839,#355840),(#355841,
#355842,#355843),(#355844,#355845,#355846),(#355847,#355848,#355849),(#355850,
#355851,#355852),(#355853,#355854,#355855),(#355856,#355857,#355858),(#355859,
#355860,#355861),(#355862,#355863,#355864),(#355865,#355866,#355867),(#355868,
#355869,#355870),(#355871,#355872,#355873),(#355874,#355875,#355876),(#355877,
#355878,#355879),(#355880,#355881,#355882),(#355883,#355884,#355885),(#355886,
#355887,#355888),(#355889,#355890,#355891),(#355892,#355893,#355894),(#355895,
#355896,#355897),(#355898,#355899,#355900),(#355901,#355902,#355903),(#355904,
#355905,#355906),(#355907,#355908,#355909),(#355910,#355911,#355912),(#355913,
#355914,#355915),(#355916,#355917,#355918),(#355919,#355920,#355921),(#355922,
#355923,#355924),(#355925,#355926,#355927),(#355928,#355929,#355930),(#355931,
#355932,#355933),(#355934,#355935,#355936),(#355937,#355938,#355939),(#355940,
#355941,#355942),(#355943,#355944,#355945),(#355946,#355947,#355948),(#355949,
#355950,#355951),(#355952,#355953,#355954),(#355955,#355956,#355957),(#355958,
#355959,#355960),(#355961,#355962,#355963),(#355964,#355965,#355966),(#355967,
#355968,#355969),(#355970,#355971,#355972),(#355973,#355974,#355975),(#355976,
#355977,#355978),(#355979,#355980,#355981),(#355982,#355983,#355984),(#355985,
#355986,#355987),(#355988,#355989,#355990),(#355991,#355992,#355993),(#355994,
#355995,#355996),(#355997,#355998,#355999),(#356000,#356001,#356002),(#356003,
#356004,#356005),(#356006,#356007,#356008),(#356009,#356010,#356011),(#356012,
#356013,#356014),(#356015,#356016,#356017),(#356018,#356019,#356020),(#356021,
#356022,#356023),(#356024,#356025,#356026),(#356027,#356028,#356029),(#356030,
#356031,#356032),(#356033,#356034,#356035),(#356036,#356037,#356038),(#356039,
#356040,#356041),(#356042,#356043,#356044),(#356045,#356046,#356047),(#356048,
#356049,#356050),(#356051,#356052,#356053),(#356054,#356055,#356056),(#356057,
#356058,#356059),(#356060,#356061,#356062),(#356063,#356064,#356065),(#356066,
#356067,#356068),(#356069,#356070,#356071),(#356072,#356073,#356074),(#356075,
#356076,#356077),(#356078,#356079,#356080),(#356081,#356082,#356083),(#356084,
#356085,#356086),(#356087,#356088,#356089),(#356090,#356091,#356092),(#356093,
#356094,#356095),(#356096,#356097,#356098),(#356099,#356100,#356101),(#356102,
#356103,#356104),(#356105,#356106,#356107),(#356108,#356109,#356110),(#356111,
#356112,#356113),(#356114,#356115,#356116),(#356117,#356118,#356119),(#356120,
#356121,#356122),(#356123,#356124,#356125),(#356126,#356127,#356128),(#356129,
#356130,#356131),(#356132,#356133,#356134),(#356135,#356136,#356137),(#356138,
#356139,#356140),(#356141,#356142,#356143),(#356144,#356145,#356146),(#356147,
#356148,#356149),(#356150,#356151,#356152),(#356153,#356154,#356155),(#356156,
#356157,#356158),(#356159,#356160,#356161),(#356162,#356163,#356164),(#356165,
#356166,#356167),(#356168,#356169,#356170),(#356171,#356172,#356173),(#356174,
#356175,#356176),(#356177,#356178,#356179),(#356180,#356181,#356182),(#356183,
#356184,#356185),(#356186,#356187,#356188),(#356189,#356190,#356191),(#356192,
#356193,#356194),(#356195,#356196,#356197),(#356198,#356199,#356200),(#356201,
#356202,#356203),(#356204,#356205,#356206),(#356207,#356208,#356209),(#356210,
#356211,#356212),(#356213,#356214,#356215),(#356216,#356217,#356218),(#356219,
#356220,#356221),(#356222,#356223,#356224),(#356225,#356226,#356227),(#356228,
#356229,#356230),(#356231,#356232,#356233),(#356234,#356235,#356236),(#356237,
#356238,#356239),(#356240,#356241,#356242),(#356243,#356244,#356245),(#356246,
#356247,#356248),(#356249,#356250,#356251),(#356252,#356253,#356254),(#356255,
#356256,#356257),(#356258,#356259,#356260),(#356261,#356262,#356263),(#356264,
#356265,#356266),(#356267,#356268,#356269),(#356270,#356271,#356272),(#356273,
#356274,#356275),(#356276,#356277,#356278),(#356279,#356280,#356281),(#356282,
#356283,#356284),(#356285,#356286,#356287),(#356288,#356289,#356290),(#356291,
#356292,#356293),(#356294,#356295,#356296),(#356297,#356298,#356299),(#356300,
#356301,#356302),(#356303,#356304,#356305),(#356306,#356307,#356308),(#356309,
#356310,#356311),(#356312,#356313,#356314),(#356315,#356316,#356317),(#356318,
#356319,#356320),(#356321,#356322,#356323),(#356324,#356325,#356326),(#356327,
#356328,#356329),(#356330,#356331,#356332),(#356333,#356334,#356335),(#356336,
#356337,#356338),(#356339,#356340,#356341),(#356342,#356343,#356344),(#356345,
#356346,#356347),(#356348,#356349,#356350),(#356351,#356352,#356353),(#356354,
#356355,#356356),(#356357,#356358,#356359),(#356360,#356361,#356362),(#356363,
#356364,#356365),(#356366,#356367,#356368),(#356369,#356370,#356371),(#356372,
#356373,#356374),(#356375,#356376,#356377),(#356378,#356379,#356380),(#356381,
#356382,#356383),(#356384,#356385,#356386),(#356387,#356388,#356389),(#356390,
#356391,#356392),(#356393,#356394,#356395),(#356396,#356397,#356398),(#356399,
#356400,#356401),(#356402,#356403,#356404),(#356405,#356406,#356407),(#356408,
#356409,#356410),(#356411,#356412,#356413),(#356414,#356415,#356416),(#356417,
#356418,#356419),(#356420,#356421,#356422),(#356423,#356424,#356425),(#356426,
#356427,#356428),(#356429,#356430,#356431),(#356432,#356433,#356434),(#356435,
#356436,#356437),(#356438,#356439,#356440),(#356441,#356442,#356443),(#356444,
#356445,#356446),(#356447,#356448,#356449),(#356450,#356451,#356452),(#356453,
#356454,#356455),(#356456,#356457,#356458),(#356459,#356460,#356461),(#356462,
#356463,#356464),(#356465,#356466,#356467),(#356468,#356469,#356470),(#356471,
#356472,#356473),(#356474,#356475,#356476),(#356477,#356478,#356479),(#356480,
#356481,#356482),(#356483,#356484,#356485),(#356486,#356487,#356488),(#356489,
#356490,#356491),(#356492,#356493,#356494),(#356495,#356496,#356497)),
 .UNSPECIFIED.,.F.,.F.,.F.,(6,1,1,1,1,1,1,1,1,1,1,1,1,1,1,1,1,1,1,1,1,1,
1,1,1,1,1,1,1,1,1,1,1,1,1,1,1,1,1,1,1,1,1,1,1,1,1,1,1,1,1,1,1,1,1,1,1,1,
1,1,1,1,1,1,1,1,1,1,1,1,1,1,1,1,1,1,1,1,1,1,1,1,1,1,1,1,1,1,1,1,1,1,1,1,
1,1,1,1,1,1,1,1,1,1,1,1,1,1,1,1,1,1,1,1,1,1,1,1,1,1,1,1,1,1,1,1,1,1,1,1,
1,1,1,1,1,1,1,1,1,1,1,1,1,1,1,1,1,1,1,1,1,1,1,1,1,1,1,1,1,1,1,1,1,1,1,1,
1,1,1,1,1,1,1,1,1,1,1,1,1,1,1,1,1,1,1,1,1,1,1,1,1,1,1,1,1,1,1,1,1,1,1,1,
1,1,1,1,1,1,1,1,1,1,1,1,1,1,1,1,1,1,1,1,1,1,1,1,1,1,1,1,1,1,1,1,1,1,1,1,
1,1,1,1,1,1,1,1,1,1,1,1,1,1,1,1,1,1,1,1,1,1,1,1,1,1,1,1,1,1,1,1,1,1,1,1,
1,1,1,1,1,1,1,1,1,1,1,1,1,1,1,1,1,1,1,1,1,1,1,1,1,1,1,1,1,1,1,1,1,1,1,1,
1,1,1,1,1,1,1,1,1,1,1,1,1,1,1,1,1,1,1,1,1,1,1,1,1,1,1,1,1,1,1,1,1,1,1,1,
1,1,1,1,1,1,1,1,1,1,1,1,1,1,1,1,1,1,1,1,1,1,1,1,1,1,1,1,1,1,1,1,1,1,1,1,
1,1,1,1,1,1,1,1,1,1,1,1,1,1,1,1,1,1,1,1,1,1,1,1,1,1,1,1,1,1,1,1,1,1,1,1,
1,1,1,1,1,1,1,1,1,1,1,1,1,1,1,1,1,1,1,1,1,1,1,1,1,1,1,1,1,1,1,1,1,1,1,1,
1,1,1,1,1,1,1,1,1,1,1,1,1,1,1,1,1,1,1,1,1,1,1,1,1,1,1,1,1,1,1,1,1,1,1,1,
1,1,1,1,1,1,1,1,1,1,1,1,1,1,1,1,1,1,1,1,1,1,1,1,1,1,1,1,1,1,1,1,1,1,1,1,
1,1,1,1,1,1,1,1,1,1,1,1,1,1,1,1,1,1,1,6),(2,1,2),(-1.,-0.998165138,-0.996330275,
-0.994495413,-0.99266055,-0.990825688,-0.988990826,-0.987155963,-0.985321101,
-0.983486239,-0.981651376,-0.979816514,-0.977981651,-0.976146789,-0.974311927,
-0.972477064,-0.970642202,-0.968807339,-0.966972477,-0.965137615,-0.963302752,
-0.96146789,-0.959633028,-0.957798165,-0.955963303,-0.95412844,-0.952293578,
-0.950458716,-0.948623853,-0.946788991,-0.944954128,-0.943119266,-0.941284404,
-0.939449541,-0.937614679,-0.935779817,-0.933944954,-0.932110092,-0.930275229,
-0.928440367,-0.926605505,-0.924770642,-0.92293578,-0.921100917,-0.919266055,
-0.917431193,-0.91559633,-0.913761468,-0.911926606,-0.910091743,-0.908256881,
-0.906422018,-0.904587156,-0.902752294,-0.900917431,-0.899082569,-0.897247706,
-0.895412844,-0.893577982,-0.891743119,-0.889908257,-0.888073394,-0.886238532,
-0.88440367,-0.882568807,-0.880733945,-0.878899083,-0.87706422,-0.875229358,
-0.873394495,-0.871559633,-0.869724771,-0.867889908,-0.866055046,-0.864220183,
-0.862385321,-0.860550459,-0.858715596,-0.856880734,-0.855045872,-0.853211009,
-0.851376147,-0.849541284,-0.847706422,-0.84587156,-0.844036697,-0.842201835,
-0.840366972,-0.83853211,-0.836697248,-0.834862385,-0.833027523,-0.831192661,
-0.829357798,-0.827522936,-0.825688073,-0.823853211,-0.822018349,-0.820183486,
-0.818348624,-0.816513761,-0.814678899,-0.812844037,-0.811009174,-0.809174312,
-0.80733945,-0.805504587,-0.803669725,-0.801834862,-0.8,-0.798165138,-0.796330275,
-0.794495413,-0.79266055,-0.790825688,-0.788990826,-0.787155963,-0.785321101,
-0.783486239,-0.781651376,-0.779816514,-0.777981651,-0.776146789,-0.774311927,
-0.772477064,-0.770642202,-0.768807339,-0.766972477,-0.765137615,-0.763302752,
-0.76146789,-0.759633028,-0.757798165,-0.755963303,-0.75412844,-0.752293578,
-0.750458716,-0.748623853,-0.746788991,-0.744954128,-0.743119266,-0.741284404,
-0.739449541,-0.737614679,-0.735779817,-0.733944954,-0.732110092,-0.730275229,
-0.728440367,-0.726605505,-0.724770642,-0.72293578,-0.721100917,-0.719266055,
-0.717431193,-0.71559633,-0.713761468,-0.711926606,-0.710091743,-0.708256881,
-0.706422018,-0.704587156,-0.702752294,-0.700917431,-0.699082569,-0.697247706,
-0.695412844,-0.693577982,-0.691743119,-0.689908257,-0.688073394,-0.686238532,
-0.68440367,-0.682568807,-0.680733945,-0.678899083,-0.67706422,-0.675229358,
-0.673394495,-0.671559633,-0.669724771,-0.667889908,-0.666055046,-0.664220183,
-0.662385321,-0.660550459,-0.658715596,-0.656880734,-0.655045872,-0.653211009,
-0.651376147,-0.649541284,-0.647706422,-0.64587156,-0.644036697,-0.642201835,
-0.640366972,-0.63853211,-0.636697248,-0.634862385,-0.633027523,-0.631192661,
-0.629357798,-0.627522936,-0.625688073,-0.623853211,-0.622018349,-0.620183486,
-0.618348624,-0.616513761,-0.614678899,-0.612844037,-0.611009174,-0.609174312,
-0.60733945,-0.605504587,-0.603669725,-0.601834862,-0.6,-0.598165138,-0.596330275,
-0.594495413,-0.59266055,-0.590825688,-0.588990826,-0.587155963,-0.585321101,
-0.583486239,-0.581651376,-0.579816514,-0.577981651,-0.576146789,-0.574311927,
-0.572477064,-0.570642202,-0.568807339,-0.566972477,-0.565137615,-0.563302752,
-0.56146789,-0.559633028,-0.557798165,-0.555963303,-0.55412844,-0.552293578,
-0.550458716,-0.548623853,-0.546788991,-0.544954128,-0.543119266,-0.541284404,
-0.539449541,-0.537614679,-0.535779817,-0.533944954,-0.532110092,-0.530275229,
-0.528440367,-0.526605505,-0.524770642,-0.52293578,-0.521100917,-0.519266055,
-0.517431193,-0.51559633,-0.513761468,-0.511926606,-0.510091743,-0.508256881,
-0.506422018,-0.504587156,-0.502752294,-0.500917431,-0.499082569,-0.497247706,
-0.495412844,-0.493577982,-0.491743119,-0.489908257,-0.488073394,-0.486238532,
-0.48440367,-0.482568807,-0.480733945,-0.478899083,-0.47706422,-0.475229358,
-0.473394495,-0.471559633,-0.469724771,-0.467889908,-0.466055046,-0.464220183,
-0.462385321,-0.460550459,-0.458715596,-0.456880734,-0.455045872,-0.453211009,
-0.451376147,-0.449541284,-0.447706422,-0.44587156,-0.444036697,-0.442201835,
-0.440366972,-0.43853211,-0.436697248,-0.434862385,-0.433027523,-0.431192661,
-0.429357798,-0.427522936,-0.425688073,-0.423853211,-0.422018349,-0.420183486,
-0.418348624,-0.416513761,-0.414678899,-0.412844037,-0.411009174,-0.409174312,
-0.40733945,-0.405504587,-0.403669725,-0.401834862,-0.4,-0.398165138,-0.396330275,
-0.394495413,-0.39266055,-0.390825688,-0.388990826,-0.387155963,-0.385321101,
-0.383486239,-0.381651376,-0.379816514,-0.377981651,-0.376146789,-0.374311927,
-0.372477064,-0.370642202,-0.368807339,-0.366972477,-0.365137615,-0.363302752,
-0.36146789,-0.359633028,-0.357798165,-0.355963303,-0.35412844,-0.352293578,
-0.350458716,-0.348623853,-0.346788991,-0.344954128,-0.343119266,-0.341284404,
-0.339449541,-0.337614679,-0.335779817,-0.333944954,-0.332110092,-0.330275229,
-0.328440367,-0.326605505,-0.324770642,-0.32293578,-0.321100917,-0.319266055,
-0.317431193,-0.31559633,-0.313761468,-0.311926606,-0.310091743,-0.308256881,
-0.306422018,-0.304587156,-0.302752294,-0.300917431,-0.299082569,-0.297247706,
-0.295412844,-0.293577982,-0.291743119,-0.289908257,-0.288073394,-0.286238532,
-0.28440367,-0.282568807,-0.280733945,-0.278899083,-0.27706422,-0.275229358,
-0.273394495,-0.271559633,-0.269724771,-0.267889908,-0.266055046,-0.264220183,
-0.262385321,-0.260550459,-0.258715596,-0.256880734,-0.255045872,-0.253211009,
-0.251376147,-0.249541284,-0.247706422,-0.24587156,-0.244036697,-0.242201835,
-0.240366972,-0.23853211,-0.236697248,-0.234862385,-0.233027523,-0.231192661,
-0.229357798,-0.227522936,-0.225688073,-0.223853211,-0.222018349,-0.220183486,
-0.218348624,-0.216513761,-0.214678899,-0.212844037,-0.211009174,-0.209174312,
-0.20733945,-0.205504587,-0.203669725,-0.201834862,-0.2,-0.198165138,-0.196330275,
-0.194495413,-0.19266055,-0.190825688,-0.188990826,-0.187155963,-0.185321101,
-0.183486239,-0.181651376,-0.179816514,-0.177981651,-0.176146789,-0.174311927,
-0.172477064,-0.170642202,-0.168807339,-0.166972477,-0.165137615,-0.163302752,
-0.16146789,-0.159633028,-0.157798165,-0.155963303,-0.15412844,-0.152293578,
-0.150458716,-0.148623853,-0.146788991,-0.144954128,-0.143119266,-0.141284404,
-0.139449541,-0.137614679,-0.135779817,-0.133944954,-0.132110092,-0.130275229,
-0.128440367,-0.126605505,-0.124770642,-0.12293578,-0.121100917,-0.119266055,
-0.117431193,-0.11559633,-0.113761468,-0.111926606,-0.110091743,-0.108256881,
-0.106422018,-0.104587156,-0.102752294,-0.100917431,-0.099082569,-0.097247706,
-0.095412844,-0.093577982,-0.091743119,-0.089908257,-0.088073394,-0.086238532,
-0.08440367,-0.082568807,-0.080733945,-0.078899083,-0.07706422,-0.075229358,
-0.073394495,-0.071559633,-0.069724771,-0.067889908,-0.066055046,-0.064220183,
-0.062385321,-0.060550459,-0.058715596,-0.056880734,-0.055045872,-0.053211009,
-0.051376147,-0.049541284,-0.047706422,-0.04587156,-0.044036697,-0.042201835,
-0.040366972,-0.03853211,-0.036697248,-0.034862385,-0.033027523,-0.031192661,
-0.029357798,-0.027522936,-0.025688073,-0.023853211,-0.022018349,-0.020183486,
-0.018348624,-0.016513761,-0.014678899,-0.012844037,-0.011009174,-0.009174312,
-0.00733945,-0.005504587,-0.003669725,-0.001834862,0.000982074616),(0.3,
1.,1.3),.UNSPECIFIED.);
#6336=B_SPLINE_SURFACE_WITH_KNOTS('',5,1,((#356501,#356502,#356503),(#356504,
#356505,#356506),(#356507,#356508,#356509),(#356510,#356511,#356512),(#356513,
#356514,#356515),(#356516,#356517,#356518),(#356519,#356520,#356521),(#356522,
#356523,#356524),(#356525,#356526,#356527),(#356528,#356529,#356530),(#356531,
#356532,#356533),(#356534,#356535,#356536),(#356537,#356538,#356539),(#356540,
#356541,#356542),(#356543,#356544,#356545),(#356546,#356547,#356548),(#356549,
#356550,#356551),(#356552,#356553,#356554),(#356555,#356556,#356557),(#356558,
#356559,#356560),(#356561,#356562,#356563),(#356564,#356565,#356566),(#356567,
#356568,#356569),(#356570,#356571,#356572),(#356573,#356574,#356575),(#356576,
#356577,#356578),(#356579,#356580,#356581),(#356582,#356583,#356584),(#356585,
#356586,#356587),(#356588,#356589,#356590),(#356591,#356592,#356593),(#356594,
#356595,#356596),(#356597,#356598,#356599),(#356600,#356601,#356602),(#356603,
#356604,#356605),(#356606,#356607,#356608),(#356609,#356610,#356611),(#356612,
#356613,#356614),(#356615,#356616,#356617),(#356618,#356619,#356620),(#356621,
#356622,#356623),(#356624,#356625,#356626),(#356627,#356628,#356629),(#356630,
#356631,#356632),(#356633,#356634,#356635),(#356636,#356637,#356638),(#356639,
#356640,#356641),(#356642,#356643,#356644),(#356645,#356646,#356647),(#356648,
#356649,#356650),(#356651,#356652,#356653),(#356654,#356655,#356656),(#356657,
#356658,#356659),(#356660,#356661,#356662),(#356663,#356664,#356665),(#356666,
#356667,#356668),(#356669,#356670,#356671),(#356672,#356673,#356674),(#356675,
#356676,#356677),(#356678,#356679,#356680),(#356681,#356682,#356683),(#356684,
#356685,#356686),(#356687,#356688,#356689),(#356690,#356691,#356692),(#356693,
#356694,#356695),(#356696,#356697,#356698),(#356699,#356700,#356701),(#356702,
#356703,#356704),(#356705,#356706,#356707),(#356708,#356709,#356710),(#356711,
#356712,#356713),(#356714,#356715,#356716),(#356717,#356718,#356719),(#356720,
#356721,#356722),(#356723,#356724,#356725),(#356726,#356727,#356728),(#356729,
#356730,#356731),(#356732,#356733,#356734),(#356735,#356736,#356737),(#356738,
#356739,#356740),(#356741,#356742,#356743),(#356744,#356745,#356746),(#356747,
#356748,#356749),(#356750,#356751,#356752),(#356753,#356754,#356755),(#356756,
#356757,#356758),(#356759,#356760,#356761),(#356762,#356763,#356764),(#356765,
#356766,#356767),(#356768,#356769,#356770),(#356771,#356772,#356773),(#356774,
#356775,#356776),(#356777,#356778,#356779),(#356780,#356781,#356782),(#356783,
#356784,#356785),(#356786,#356787,#356788),(#356789,#356790,#356791),(#356792,
#356793,#356794),(#356795,#356796,#356797),(#356798,#356799,#356800),(#356801,
#356802,#356803),(#356804,#356805,#356806),(#356807,#356808,#356809),(#356810,
#356811,#356812),(#356813,#356814,#356815),(#356816,#356817,#356818),(#356819,
#356820,#356821),(#356822,#356823,#356824),(#356825,#356826,#356827),(#356828,
#356829,#356830),(#356831,#356832,#356833),(#356834,#356835,#356836),(#356837,
#356838,#356839),(#356840,#356841,#356842),(#356843,#356844,#356845),(#356846,
#356847,#356848),(#356849,#356850,#356851),(#356852,#356853,#356854),(#356855,
#356856,#356857),(#356858,#356859,#356860),(#356861,#356862,#356863),(#356864,
#356865,#356866),(#356867,#356868,#356869),(#356870,#356871,#356872),(#356873,
#356874,#356875),(#356876,#356877,#356878),(#356879,#356880,#356881),(#356882,
#356883,#356884),(#356885,#356886,#356887),(#356888,#356889,#356890),(#356891,
#356892,#356893),(#356894,#356895,#356896),(#356897,#356898,#356899),(#356900,
#356901,#356902),(#356903,#356904,#356905),(#356906,#356907,#356908),(#356909,
#356910,#356911),(#356912,#356913,#356914),(#356915,#356916,#356917),(#356918,
#356919,#356920),(#356921,#356922,#356923),(#356924,#356925,#356926),(#356927,
#356928,#356929),(#356930,#356931,#356932),(#356933,#356934,#356935),(#356936,
#356937,#356938),(#356939,#356940,#356941),(#356942,#356943,#356944),(#356945,
#356946,#356947),(#356948,#356949,#356950),(#356951,#356952,#356953),(#356954,
#356955,#356956),(#356957,#356958,#356959),(#356960,#356961,#356962),(#356963,
#356964,#356965),(#356966,#356967,#356968),(#356969,#356970,#356971),(#356972,
#356973,#356974),(#356975,#356976,#356977),(#356978,#356979,#356980),(#356981,
#356982,#356983),(#356984,#356985,#356986),(#356987,#356988,#356989),(#356990,
#356991,#356992),(#356993,#356994,#356995),(#356996,#356997,#356998),(#356999,
#357000,#357001),(#357002,#357003,#357004),(#357005,#357006,#357007),(#357008,
#357009,#357010),(#357011,#357012,#357013),(#357014,#357015,#357016),(#357017,
#357018,#357019),(#357020,#357021,#357022),(#357023,#357024,#357025),(#357026,
#357027,#357028),(#357029,#357030,#357031),(#357032,#357033,#357034),(#357035,
#357036,#357037),(#357038,#357039,#357040),(#357041,#357042,#357043),(#357044,
#357045,#357046),(#357047,#357048,#357049),(#357050,#357051,#357052),(#357053,
#357054,#357055),(#357056,#357057,#357058),(#357059,#357060,#357061),(#357062,
#357063,#357064),(#357065,#357066,#357067),(#357068,#357069,#357070),(#357071,
#357072,#357073),(#357074,#357075,#357076),(#357077,#357078,#357079),(#357080,
#357081,#357082),(#357083,#357084,#357085),(#357086,#357087,#357088),(#357089,
#357090,#357091),(#357092,#357093,#357094),(#357095,#357096,#357097),(#357098,
#357099,#357100),(#357101,#357102,#357103),(#357104,#357105,#357106),(#357107,
#357108,#357109),(#357110,#357111,#357112),(#357113,#357114,#357115),(#357116,
#357117,#357118),(#357119,#357120,#357121),(#357122,#357123,#357124),(#357125,
#357126,#357127),(#357128,#357129,#357130),(#357131,#357132,#357133),(#357134,
#357135,#357136),(#357137,#357138,#357139),(#357140,#357141,#357142),(#357143,
#357144,#357145),(#357146,#357147,#357148),(#357149,#357150,#357151),(#357152,
#357153,#357154),(#357155,#357156,#357157),(#357158,#357159,#357160),(#357161,
#357162,#357163),(#357164,#357165,#357166),(#357167,#357168,#357169),(#357170,
#357171,#357172),(#357173,#357174,#357175),(#357176,#357177,#357178),(#357179,
#357180,#357181),(#357182,#357183,#357184),(#357185,#357186,#357187),(#357188,
#357189,#357190),(#357191,#357192,#357193),(#357194,#357195,#357196),(#357197,
#357198,#357199),(#357200,#357201,#357202),(#357203,#357204,#357205),(#357206,
#357207,#357208),(#357209,#357210,#357211),(#357212,#357213,#357214),(#357215,
#357216,#357217),(#357218,#357219,#357220),(#357221,#357222,#357223),(#357224,
#357225,#357226),(#357227,#357228,#357229),(#357230,#357231,#357232),(#357233,
#357234,#357235),(#357236,#357237,#357238),(#357239,#357240,#357241),(#357242,
#357243,#357244),(#357245,#357246,#357247),(#357248,#357249,#357250),(#357251,
#357252,#357253),(#357254,#357255,#357256),(#357257,#357258,#357259),(#357260,
#357261,#357262),(#357263,#357264,#357265),(#357266,#357267,#357268),(#357269,
#357270,#357271),(#357272,#357273,#357274),(#357275,#357276,#357277),(#357278,
#357279,#357280),(#357281,#357282,#357283),(#357284,#357285,#357286),(#357287,
#357288,#357289),(#357290,#357291,#357292),(#357293,#357294,#357295),(#357296,
#357297,#357298),(#357299,#357300,#357301),(#357302,#357303,#357304),(#357305,
#357306,#357307),(#357308,#357309,#357310),(#357311,#357312,#357313),(#357314,
#357315,#357316),(#357317,#357318,#357319),(#357320,#357321,#357322),(#357323,
#357324,#357325),(#357326,#357327,#357328),(#357329,#357330,#357331),(#357332,
#357333,#357334),(#357335,#357336,#357337),(#357338,#357339,#357340),(#357341,
#357342,#357343),(#357344,#357345,#357346),(#357347,#357348,#357349),(#357350,
#357351,#357352),(#357353,#357354,#357355),(#357356,#357357,#357358),(#357359,
#357360,#357361),(#357362,#357363,#357364),(#357365,#357366,#357367),(#357368,
#357369,#357370),(#357371,#357372,#357373),(#357374,#357375,#357376),(#357377,
#357378,#357379),(#357380,#357381,#357382),(#357383,#357384,#357385),(#357386,
#357387,#357388),(#357389,#357390,#357391),(#357392,#357393,#357394),(#357395,
#357396,#357397),(#357398,#357399,#357400),(#357401,#357402,#357403),(#357404,
#357405,#357406),(#357407,#357408,#357409),(#357410,#357411,#357412),(#357413,
#357414,#357415),(#357416,#357417,#357418),(#357419,#357420,#357421),(#357422,
#357423,#357424),(#357425,#357426,#357427),(#357428,#357429,#357430),(#357431,
#357432,#357433),(#357434,#357435,#357436),(#357437,#357438,#357439),(#357440,
#357441,#357442),(#357443,#357444,#357445),(#357446,#357447,#357448),(#357449,
#357450,#357451),(#357452,#357453,#357454),(#357455,#357456,#357457),(#357458,
#357459,#357460),(#357461,#357462,#357463),(#357464,#357465,#357466),(#357467,
#357468,#357469),(#357470,#357471,#357472),(#357473,#357474,#357475),(#357476,
#357477,#357478),(#357479,#357480,#357481),(#357482,#357483,#357484),(#357485,
#357486,#357487),(#357488,#357489,#357490),(#357491,#357492,#357493),(#357494,
#357495,#357496),(#357497,#357498,#357499),(#357500,#357501,#357502),(#357503,
#357504,#357505),(#357506,#357507,#357508),(#357509,#357510,#357511),(#357512,
#357513,#357514),(#357515,#357516,#357517),(#357518,#357519,#357520),(#357521,
#357522,#357523),(#357524,#357525,#357526),(#357527,#357528,#357529),(#357530,
#357531,#357532),(#357533,#357534,#357535),(#357536,#357537,#357538),(#357539,
#357540,#357541),(#357542,#357543,#357544),(#357545,#357546,#357547),(#357548,
#357549,#357550),(#357551,#357552,#357553),(#357554,#357555,#357556),(#357557,
#357558,#357559),(#357560,#357561,#357562),(#357563,#357564,#357565),(#357566,
#357567,#357568),(#357569,#357570,#357571),(#357572,#357573,#357574),(#357575,
#357576,#357577),(#357578,#357579,#357580),(#357581,#357582,#357583),(#357584,
#357585,#357586),(#357587,#357588,#357589),(#357590,#357591,#357592),(#357593,
#357594,#357595),(#357596,#357597,#357598),(#357599,#357600,#357601),(#357602,
#357603,#357604),(#357605,#357606,#357607),(#357608,#357609,#357610),(#357611,
#357612,#357613),(#357614,#357615,#357616),(#357617,#357618,#357619),(#357620,
#357621,#357622),(#357623,#357624,#357625),(#357626,#357627,#357628),(#357629,
#357630,#357631),(#357632,#357633,#357634),(#357635,#357636,#357637),(#357638,
#357639,#357640),(#357641,#357642,#357643),(#357644,#357645,#357646),(#357647,
#357648,#357649),(#357650,#357651,#357652),(#357653,#357654,#357655),(#357656,
#357657,#357658),(#357659,#357660,#357661),(#357662,#357663,#357664),(#357665,
#357666,#357667),(#357668,#357669,#357670),(#357671,#357672,#357673),(#357674,
#357675,#357676),(#357677,#357678,#357679),(#357680,#357681,#357682),(#357683,
#357684,#357685),(#357686,#357687,#357688),(#357689,#357690,#357691),(#357692,
#357693,#357694),(#357695,#357696,#357697),(#357698,#357699,#357700),(#357701,
#357702,#357703),(#357704,#357705,#357706),(#357707,#357708,#357709),(#357710,
#357711,#357712),(#357713,#357714,#357715),(#357716,#357717,#357718),(#357719,
#357720,#357721),(#357722,#357723,#357724),(#357725,#357726,#357727),(#357728,
#357729,#357730),(#357731,#357732,#357733),(#357734,#357735,#357736),(#357737,
#357738,#357739),(#357740,#357741,#357742),(#357743,#357744,#357745),(#357746,
#357747,#357748),(#357749,#357750,#357751),(#357752,#357753,#357754),(#357755,
#357756,#357757),(#357758,#357759,#357760),(#357761,#357762,#357763),(#357764,
#357765,#357766),(#357767,#357768,#357769),(#357770,#357771,#357772),(#357773,
#357774,#357775),(#357776,#357777,#357778),(#357779,#357780,#357781),(#357782,
#357783,#357784),(#357785,#357786,#357787),(#357788,#357789,#357790),(#357791,
#357792,#357793),(#357794,#357795,#357796),(#357797,#357798,#357799),(#357800,
#357801,#357802),(#357803,#357804,#357805),(#357806,#357807,#357808),(#357809,
#357810,#357811),(#357812,#357813,#357814),(#357815,#357816,#357817),(#357818,
#357819,#357820),(#357821,#357822,#357823),(#357824,#357825,#357826),(#357827,
#357828,#357829),(#357830,#357831,#357832),(#357833,#357834,#357835),(#357836,
#357837,#357838),(#357839,#357840,#357841),(#357842,#357843,#357844),(#357845,
#357846,#357847),(#357848,#357849,#357850),(#357851,#357852,#357853),(#357854,
#357855,#357856),(#357857,#357858,#357859),(#357860,#357861,#357862),(#357863,
#357864,#357865),(#357866,#357867,#357868),(#357869,#357870,#357871),(#357872,
#357873,#357874),(#357875,#357876,#357877),(#357878,#357879,#357880),(#357881,
#357882,#357883),(#357884,#357885,#357886),(#357887,#357888,#357889),(#357890,
#357891,#357892),(#357893,#357894,#357895),(#357896,#357897,#357898),(#357899,
#357900,#357901),(#357902,#357903,#357904),(#357905,#357906,#357907),(#357908,
#357909,#357910),(#357911,#357912,#357913),(#357914,#357915,#357916),(#357917,
#357918,#357919),(#357920,#357921,#357922),(#357923,#357924,#357925),(#357926,
#357927,#357928),(#357929,#357930,#357931),(#357932,#357933,#357934),(#357935,
#357936,#357937),(#357938,#357939,#357940),(#357941,#357942,#357943),(#357944,
#357945,#357946),(#357947,#357948,#357949),(#357950,#357951,#357952),(#357953,
#357954,#357955),(#357956,#357957,#357958),(#357959,#357960,#357961),(#357962,
#357963,#357964),(#357965,#357966,#357967),(#357968,#357969,#357970),(#357971,
#357972,#357973),(#357974,#357975,#357976),(#357977,#357978,#357979),(#357980,
#357981,#357982),(#357983,#357984,#357985),(#357986,#357987,#357988),(#357989,
#357990,#357991),(#357992,#357993,#357994),(#357995,#357996,#357997),(#357998,
#357999,#358000),(#358001,#358002,#358003),(#358004,#358005,#358006),(#358007,
#358008,#358009),(#358010,#358011,#358012),(#358013,#358014,#358015),(#358016,
#358017,#358018),(#358019,#358020,#358021),(#358022,#358023,#358024),(#358025,
#358026,#358027),(#358028,#358029,#358030),(#358031,#358032,#358033),(#358034,
#358035,#358036),(#358037,#358038,#358039),(#358040,#358041,#358042),(#358043,
#358044,#358045),(#358046,#358047,#358048),(#358049,#358050,#358051),(#358052,
#358053,#358054),(#358055,#358056,#358057),(#358058,#358059,#358060),(#358061,
#358062,#358063),(#358064,#358065,#358066),(#358067,#358068,#358069),(#358070,
#358071,#358072),(#358073,#358074,#358075),(#358076,#358077,#358078),(#358079,
#358080,#358081),(#358082,#358083,#358084),(#358085,#358086,#358087),(#358088,
#358089,#358090),(#358091,#358092,#358093),(#358094,#358095,#358096),(#358097,
#358098,#358099),(#358100,#358101,#358102),(#358103,#358104,#358105),(#358106,
#358107,#358108),(#358109,#358110,#358111),(#358112,#358113,#358114),(#358115,
#358116,#358117),(#358118,#358119,#358120),(#358121,#358122,#358123),(#358124,
#358125,#358126),(#358127,#358128,#358129),(#358130,#358131,#358132),(#358133,
#358134,#358135),(#358136,#358137,#358138),(#358139,#358140,#358141),(#358142,
#358143,#358144),(#358145,#358146,#358147),(#358148,#358149,#358150),(#358151,
#358152,#358153)),.UNSPECIFIED.,.F.,.F.,.F.,(6,1,1,1,1,1,1,1,1,1,1,1,1,
1,1,1,1,1,1,1,1,1,1,1,1,1,1,1,1,1,1,1,1,1,1,1,1,1,1,1,1,1,1,1,1,1,1,1,1,
1,1,1,1,1,1,1,1,1,1,1,1,1,1,1,1,1,1,1,1,1,1,1,1,1,1,1,1,1,1,1,1,1,1,1,1,
1,1,1,1,1,1,1,1,1,1,1,1,1,1,1,1,1,1,1,1,1,1,1,1,1,1,1,1,1,1,1,1,1,1,1,1,
1,1,1,1,1,1,1,1,1,1,1,1,1,1,1,1,1,1,1,1,1,1,1,1,1,1,1,1,1,1,1,1,1,1,1,1,
1,1,1,1,1,1,1,1,1,1,1,1,1,1,1,1,1,1,1,1,1,1,1,1,1,1,1,1,1,1,1,1,1,1,1,1,
1,1,1,1,1,1,1,1,1,1,1,1,1,1,1,1,1,1,1,1,1,1,1,1,1,1,1,1,1,1,1,1,1,1,1,1,
1,1,1,1,1,1,1,1,1,1,1,1,1,1,1,1,1,1,1,1,1,1,1,1,1,1,1,1,1,1,1,1,1,1,1,1,
1,1,1,1,1,1,1,1,1,1,1,1,1,1,1,1,1,1,1,1,1,1,1,1,1,1,1,1,1,1,1,1,1,1,1,1,
1,1,1,1,1,1,1,1,1,1,1,1,1,1,1,1,1,1,1,1,1,1,1,1,1,1,1,1,1,1,1,1,1,1,1,1,
1,1,1,1,1,1,1,1,1,1,1,1,1,1,1,1,1,1,1,1,1,1,1,1,1,1,1,1,1,1,1,1,1,1,1,1,
1,1,1,1,1,1,1,1,1,1,1,1,1,1,1,1,1,1,1,1,1,1,1,1,1,1,1,1,1,1,1,1,1,1,1,1,
1,1,1,1,1,1,1,1,1,1,1,1,1,1,1,1,1,1,1,1,1,1,1,1,1,1,1,1,1,1,1,1,1,1,1,1,
1,1,1,1,1,1,1,1,1,1,1,1,1,1,1,1,1,1,1,1,1,1,1,1,1,1,1,1,1,1,1,1,1,1,1,1,
1,1,1,1,1,1,1,1,1,1,1,1,1,1,1,1,1,1,1,1,1,1,1,1,1,1,1,1,1,1,1,1,1,1,1,1,
1,1,1,1,1,1,1,1,1,1,1,1,1,1,1,1,1,1,1,1,1,1,1,1,1,1,1,1,1,6),(2,1,2),(-0.001964179,
0.,0.001834862,0.003669725,0.005504587,0.00733945,0.009174312,0.011009174,
0.012844037,0.014678899,0.016513761,0.018348624,0.020183486,0.022018349,
0.023853211,0.025688073,0.027522936,0.029357798,0.031192661,0.033027523,
0.034862385,0.036697248,0.03853211,0.040366972,0.042201835,0.044036697,
0.04587156,0.047706422,0.049541284,0.051376147,0.053211009,0.055045872,
0.056880734,0.058715596,0.060550459,0.062385321,0.064220183,0.066055046,
0.067889908,0.069724771,0.071559633,0.073394495,0.075229358,0.07706422,
0.078899083,0.080733945,0.082568807,0.08440367,0.086238532,0.088073394,
0.089908257,0.091743119,0.093577982,0.095412844,0.097247706,0.099082569,
0.100917431,0.102752294,0.104587156,0.106422018,0.108256881,0.110091743,
0.111926606,0.113761468,0.11559633,0.117431193,0.119266055,0.121100917,
0.12293578,0.124770642,0.126605505,0.128440367,0.130275229,0.132110092,
0.133944954,0.135779817,0.137614679,0.139449541,0.141284404,0.143119266,
0.144954128,0.146788991,0.148623853,0.150458716,0.152293578,0.15412844,
0.155963303,0.157798165,0.159633028,0.16146789,0.163302752,0.165137615,
0.166972477,0.168807339,0.170642202,0.172477064,0.174311927,0.176146789,
0.177981651,0.179816514,0.181651376,0.183486239,0.185321101,0.187155963,
0.188990826,0.190825688,0.19266055,0.194495413,0.196330275,0.198165138,
0.2,0.201834862,0.203669725,0.205504587,0.20733945,0.209174312,0.211009174,
0.212844037,0.214678899,0.216513761,0.218348624,0.220183486,0.222018349,
0.223853211,0.225688073,0.227522936,0.229357798,0.231192661,0.233027523,
0.234862385,0.236697248,0.23853211,0.240366972,0.242201835,0.244036697,
0.24587156,0.247706422,0.249541284,0.251376147,0.253211009,0.255045872,
0.256880734,0.258715596,0.260550459,0.262385321,0.264220183,0.266055046,
0.267889908,0.269724771,0.271559633,0.273394495,0.275229358,0.27706422,
0.278899083,0.280733945,0.282568807,0.28440367,0.286238532,0.288073394,
0.289908257,0.291743119,0.293577982,0.295412844,0.297247706,0.299082569,
0.300917431,0.302752294,0.304587156,0.306422018,0.308256881,0.310091743,
0.311926606,0.313761468,0.31559633,0.317431193,0.319266055,0.321100917,
0.32293578,0.324770642,0.326605505,0.328440367,0.330275229,0.332110092,
0.333944954,0.335779817,0.337614679,0.339449541,0.341284404,0.343119266,
0.344954128,0.346788991,0.348623853,0.350458716,0.352293578,0.35412844,
0.355963303,0.357798165,0.359633028,0.36146789,0.363302752,0.365137615,
0.366972477,0.368807339,0.370642202,0.372477064,0.374311927,0.376146789,
0.377981651,0.379816514,0.381651376,0.383486239,0.385321101,0.387155963,
0.388990826,0.390825688,0.39266055,0.394495413,0.396330275,0.398165138,
0.4,0.401834862,0.403669725,0.405504587,0.40733945,0.409174312,0.411009174,
0.412844037,0.414678899,0.416513761,0.418348624,0.420183486,0.422018349,
0.423853211,0.425688073,0.427522936,0.429357798,0.431192661,0.433027523,
0.434862385,0.436697248,0.43853211,0.440366972,0.442201835,0.444036697,
0.44587156,0.447706422,0.449541284,0.451376147,0.453211009,0.455045872,
0.456880734,0.458715596,0.460550459,0.462385321,0.464220183,0.466055046,
0.467889908,0.469724771,0.471559633,0.473394495,0.475229358,0.47706422,
0.478899083,0.480733945,0.482568807,0.48440367,0.486238532,0.488073394,
0.489908257,0.491743119,0.493577982,0.495412844,0.497247706,0.499082569,
0.500917431,0.502752294,0.504587156,0.506422018,0.508256881,0.510091743,
0.511926606,0.513761468,0.51559633,0.517431193,0.519266055,0.521100917,
0.52293578,0.524770642,0.526605505,0.528440367,0.530275229,0.532110092,
0.533944954,0.535779817,0.537614679,0.539449541,0.541284404,0.543119266,
0.544954128,0.546788991,0.548623853,0.550458716,0.552293578,0.55412844,
0.555963303,0.557798165,0.559633028,0.56146789,0.563302752,0.565137615,
0.566972477,0.568807339,0.570642202,0.572477064,0.574311927,0.576146789,
0.577981651,0.579816514,0.581651376,0.583486239,0.585321101,0.587155963,
0.588990826,0.590825688,0.59266055,0.594495413,0.596330275,0.598165138,
0.6,0.601834862,0.603669725,0.605504587,0.60733945,0.609174312,0.611009174,
0.612844037,0.614678899,0.616513761,0.618348624,0.620183486,0.622018349,
0.623853211,0.625688073,0.627522936,0.629357798,0.631192661,0.633027523,
0.634862385,0.636697248,0.63853211,0.640366972,0.642201835,0.644036697,
0.64587156,0.647706422,0.649541284,0.651376147,0.653211009,0.655045872,
0.656880734,0.658715596,0.660550459,0.662385321,0.664220183,0.666055046,
0.667889908,0.669724771,0.671559633,0.673394495,0.675229358,0.67706422,
0.678899083,0.680733945,0.682568807,0.68440367,0.686238532,0.688073394,
0.689908257,0.691743119,0.693577982,0.695412844,0.697247706,0.699082569,
0.700917431,0.702752294,0.704587156,0.706422018,0.708256881,0.710091743,
0.711926606,0.713761468,0.71559633,0.717431193,0.719266055,0.721100917,
0.72293578,0.724770642,0.726605505,0.728440367,0.730275229,0.732110092,
0.733944954,0.735779817,0.737614679,0.739449541,0.741284404,0.743119266,
0.744954128,0.746788991,0.748623853,0.750458716,0.752293578,0.75412844,
0.755963303,0.757798165,0.759633028,0.76146789,0.763302752,0.765137615,
0.766972477,0.768807339,0.770642202,0.772477064,0.774311927,0.776146789,
0.777981651,0.779816514,0.781651376,0.783486239,0.785321101,0.787155963,
0.788990826,0.790825688,0.79266055,0.794495413,0.796330275,0.798165138,
0.8,0.801834862,0.803669725,0.805504587,0.80733945,0.809174312,0.811009174,
0.812844037,0.814678899,0.816513761,0.818348624,0.820183486,0.822018349,
0.823853211,0.825688073,0.827522936,0.829357798,0.831192661,0.833027523,
0.834862385,0.836697248,0.83853211,0.840366972,0.842201835,0.844036697,
0.84587156,0.847706422,0.849541284,0.851376147,0.853211009,0.855045872,
0.856880734,0.858715596,0.860550459,0.862385321,0.864220183,0.866055046,
0.867889908,0.869724771,0.871559633,0.873394495,0.875229358,0.87706422,
0.878899083,0.880733945,0.882568807,0.88440367,0.886238532,0.888073394,
0.889908257,0.891743119,0.893577982,0.895412844,0.897247706,0.899082569,
0.900917431,0.902752294,0.904587156,0.906422018,0.908256881,0.910091743,
0.911926606,0.913761468,0.91559633,0.917431193,0.919266055,0.921100917,
0.92293578,0.924770642,0.926605505,0.928440367,0.930275229,0.932110092,
0.933944954,0.935779817,0.937614679,0.939449541,0.941284404,0.943119266,
0.944954128,0.946788991,0.948623853,0.950458716,0.952293578,0.95412844,
0.955963303,0.957798165,0.959633028,0.96146789,0.963302752,0.965137615,
0.966972477,0.968807339,0.970642202,0.972477064,0.974311927,0.976146789,
0.977981651,0.979816514,0.981651376,0.983486239,0.985321101,0.987155963,
0.988990826,0.990825688,0.99266055,0.994495413,0.996330275,0.998165138,
1.),(0.3,1.,1.3),.UNSPECIFIED.);
#6337=B_SPLINE_SURFACE_WITH_KNOTS('',3,3,((#452194,#452195,#452196,#452197,
#452198,#452199,#452200,#452201,#452202,#452203,#452204,#452205,#452206,
#452207,#452208,#452209,#452210,#452211,#452212,#452213,#452214,#452215,
#452216,#452217,#452218,#452219,#452220,#452221,#452222,#452223,#452224,
#452225,#452226,#452227,#452228,#452229,#452230,#452231,#452232,#452233,
#452234,#452235,#452236,#452237,#452238,#452239,#452240,#452241,#452242,
#452243,#452244,#452245,#452246,#452247),(#452248,#452249,#452250,#452251,
#452252,#452253,#452254,#452255,#452256,#452257,#452258,#452259,#452260,
#452261,#452262,#452263,#452264,#452265,#452266,#452267,#452268,#452269,
#452270,#452271,#452272,#452273,#452274,#452275,#452276,#452277,#452278,
#452279,#452280,#452281,#452282,#452283,#452284,#452285,#452286,#452287,
#452288,#452289,#452290,#452291,#452292,#452293,#452294,#452295,#452296,
#452297,#452298,#452299,#452300,#452301),(#452302,#452303,#452304,#452305,
#452306,#452307,#452308,#452309,#452310,#452311,#452312,#452313,#452314,
#452315,#452316,#452317,#452318,#452319,#452320,#452321,#452322,#452323,
#452324,#452325,#452326,#452327,#452328,#452329,#452330,#452331,#452332,
#452333,#452334,#452335,#452336,#452337,#452338,#452339,#452340,#452341,
#452342,#452343,#452344,#452345,#452346,#452347,#452348,#452349,#452350,
#452351,#452352,#452353,#452354,#452355),(#452356,#452357,#452358,#452359,
#452360,#452361,#452362,#452363,#452364,#452365,#452366,#452367,#452368,
#452369,#452370,#452371,#452372,#452373,#452374,#452375,#452376,#452377,
#452378,#452379,#452380,#452381,#452382,#452383,#452384,#452385,#452386,
#452387,#452388,#452389,#452390,#452391,#452392,#452393,#452394,#452395,
#452396,#452397,#452398,#452399,#452400,#452401,#452402,#452403,#452404,
#452405,#452406,#452407,#452408,#452409)),.UNSPECIFIED.,.F.,.F.,.F.,(4,
4),(4,1,1,1,1,1,1,1,1,1,1,1,1,1,1,1,1,1,1,1,1,1,1,1,1,1,1,1,1,1,1,1,1,1,
1,1,1,1,1,1,1,1,1,1,1,1,1,1,1,1,1,4),(0.,0.0291273210806165),(11.8408508686654,
12.8389428231049,13.8370347775443,14.8351267319837,15.8332186864231,16.8313106408625,
17.829402595302,18.8274945497414,19.8255865041808,20.8236784586202,21.8217704130596,
22.8198623674991,23.8179543219385,24.8160462763779,25.8141382308173,26.8122301852567,
27.8103221396962,28.8084140941356,29.806506048575,30.8045980030144,31.8026899574538,
32.8007819118933,33.7988738663327,34.7969658207721,35.7950577752115,36.7931497296509,
37.7912416840904,38.7893336385298,39.7874255929692,40.7855175474086,41.783609501848,
42.7817014562875,43.7797934107269,44.7778853651663,45.7759773196057,46.7740692740451,
47.7721612284846,48.770253182924,49.7683451373634,50.7664370918028,51.7645290462422,
52.7626210006817,53.7607129551211,54.7588049095605,55.7568968639999,56.7549888184393,
57.7530807728788,58.7511727273182,59.7492646817576,60.747356636197,61.7454485906364,
62.7435405450759),.UNSPECIFIED.);
#6338=B_SPLINE_SURFACE_WITH_KNOTS('',3,3,((#452514,#452515,#452516,#452517,
#452518,#452519,#452520,#452521,#452522,#452523,#452524,#452525,#452526,
#452527,#452528,#452529,#452530,#452531,#452532,#452533,#452534,#452535,
#452536,#452537,#452538,#452539,#452540,#452541,#452542,#452543,#452544,
#452545,#452546,#452547,#452548,#452549,#452550,#452551,#452552,#452553,
#452554,#452555,#452556,#452557,#452558,#452559,#452560,#452561,#452562,
#452563,#452564,#452565,#452566,#452567),(#452568,#452569,#452570,#452571,
#452572,#452573,#452574,#452575,#452576,#452577,#452578,#452579,#452580,
#452581,#452582,#452583,#452584,#452585,#452586,#452587,#452588,#452589,
#452590,#452591,#452592,#452593,#452594,#452595,#452596,#452597,#452598,
#452599,#452600,#452601,#452602,#452603,#452604,#452605,#452606,#452607,
#452608,#452609,#452610,#452611,#452612,#452613,#452614,#452615,#452616,
#452617,#452618,#452619,#452620,#452621),(#452622,#452623,#452624,#452625,
#452626,#452627,#452628,#452629,#452630,#452631,#452632,#452633,#452634,
#452635,#452636,#452637,#452638,#452639,#452640,#452641,#452642,#452643,
#452644,#452645,#452646,#452647,#452648,#452649,#452650,#452651,#452652,
#452653,#452654,#452655,#452656,#452657,#452658,#452659,#452660,#452661,
#452662,#452663,#452664,#452665,#452666,#452667,#452668,#452669,#452670,
#452671,#452672,#452673,#452674,#452675),(#452676,#452677,#452678,#452679,
#452680,#452681,#452682,#452683,#452684,#452685,#452686,#452687,#452688,
#452689,#452690,#452691,#452692,#452693,#452694,#452695,#452696,#452697,
#452698,#452699,#452700,#452701,#452702,#452703,#452704,#452705,#452706,
#452707,#452708,#452709,#452710,#452711,#452712,#452713,#452714,#452715,
#452716,#452717,#452718,#452719,#452720,#452721,#452722,#452723,#452724,
#452725,#452726,#452727,#452728,#452729)),.UNSPECIFIED.,.F.,.F.,.F.,(4,
4),(4,1,1,1,1,1,1,1,1,1,1,1,1,1,1,1,1,1,1,1,1,1,1,1,1,1,1,1,1,1,1,1,1,1,
1,1,1,1,1,1,1,1,1,1,1,1,1,1,1,1,1,4),(0.,0.0291273210806165),(14.4000123930734,
15.3981043475128,16.3961963019522,17.3942882563917,18.3923802108311,19.3904721652705,
20.3885641197099,21.3866560741493,22.3847480285887,23.3828399830282,24.3809319374676,
25.379023891907,26.3771158463464,27.3752078007858,28.3732997552253,29.3713917096647,
30.3694836641041,31.3675756185435,32.3656675729829,33.3637595274224,34.3618514818618,
35.3599434363012,36.3580353907406,37.35612734518,38.3542192996195,39.3523112540589,
40.3504032084983,41.3484951629377,42.3465871173771,43.3446790718166,44.342771026256,
45.3408629806954,46.3389549351348,47.3370468895742,48.3351388440137,49.3332307984531,
50.3313227528925,51.3294147073319,52.3275066617713,53.3255986162108,54.3236905706502,
55.3217825250896,56.319874479529,57.3179664339684,58.3160583884079,59.3141503428473,
60.3122422972867,61.3103342517261,62.3084262061655,63.306518160605,64.3046101150444,
65.3027020694838),.UNSPECIFIED.);
#6339=B_SPLINE_SURFACE_WITH_KNOTS('',3,3,((#453481,#453482,#453483,#453484,
#453485,#453486,#453487,#453488,#453489,#453490,#453491,#453492,#453493,
#453494,#453495,#453496,#453497,#453498,#453499,#453500,#453501,#453502,
#453503,#453504,#453505,#453506,#453507,#453508,#453509,#453510,#453511,
#453512,#453513,#453514,#453515,#453516,#453517,#453518,#453519,#453520,
#453521,#453522,#453523,#453524,#453525,#453526,#453527,#453528,#453529,
#453530,#453531,#453532,#453533,#453534),(#453535,#453536,#453537,#453538,
#453539,#453540,#453541,#453542,#453543,#453544,#453545,#453546,#453547,
#453548,#453549,#453550,#453551,#453552,#453553,#453554,#453555,#453556,
#453557,#453558,#453559,#453560,#453561,#453562,#453563,#453564,#453565,
#453566,#453567,#453568,#453569,#453570,#453571,#453572,#453573,#453574,
#453575,#453576,#453577,#453578,#453579,#453580,#453581,#453582,#453583,
#453584,#453585,#453586,#453587,#453588),(#453589,#453590,#453591,#453592,
#453593,#453594,#453595,#453596,#453597,#453598,#453599,#453600,#453601,
#453602,#453603,#453604,#453605,#453606,#453607,#453608,#453609,#453610,
#453611,#453612,#453613,#453614,#453615,#453616,#453617,#453618,#453619,
#453620,#453621,#453622,#453623,#453624,#453625,#453626,#453627,#453628,
#453629,#453630,#453631,#453632,#453633,#453634,#453635,#453636,#453637,
#453638,#453639,#453640,#453641,#453642),(#453643,#453644,#453645,#453646,
#453647,#453648,#453649,#453650,#453651,#453652,#453653,#453654,#453655,
#453656,#453657,#453658,#453659,#453660,#453661,#453662,#453663,#453664,
#453665,#453666,#453667,#453668,#453669,#453670,#453671,#453672,#453673,
#453674,#453675,#453676,#453677,#453678,#453679,#453680,#453681,#453682,
#453683,#453684,#453685,#453686,#453687,#453688,#453689,#453690,#453691,
#453692,#453693,#453694,#453695,#453696)),.UNSPECIFIED.,.F.,.F.,.F.,(4,
4),(4,1,1,1,1,1,1,1,1,1,1,1,1,1,1,1,1,1,1,1,1,1,1,1,1,1,1,1,1,1,1,1,1,1,
1,1,1,1,1,1,1,1,1,1,1,1,1,1,1,1,1,4),(0.,0.0291273210806165),(11.8408508686654,
12.8389428231049,13.8370347775443,14.8351267319837,15.8332186864231,16.8313106408625,
17.829402595302,18.8274945497414,19.8255865041808,20.8236784586202,21.8217704130596,
22.8198623674991,23.8179543219385,24.8160462763779,25.8141382308173,26.8122301852567,
27.8103221396962,28.8084140941356,29.806506048575,30.8045980030144,31.8026899574538,
32.8007819118933,33.7988738663327,34.7969658207721,35.7950577752115,36.7931497296509,
37.7912416840904,38.7893336385298,39.7874255929692,40.7855175474086,41.783609501848,
42.7817014562875,43.7797934107269,44.7778853651663,45.7759773196057,46.7740692740451,
47.7721612284846,48.770253182924,49.7683451373634,50.7664370918028,51.7645290462422,
52.7626210006817,53.7607129551211,54.7588049095605,55.7568968639999,56.7549888184393,
57.7530807728788,58.7511727273182,59.7492646817576,60.747356636197,61.7454485906364,
62.7435405450759),.UNSPECIFIED.);
#6340=B_SPLINE_SURFACE_WITH_KNOTS('',3,3,((#453722,#453723,#453724,#453725,
#453726,#453727,#453728,#453729,#453730,#453731,#453732,#453733,#453734,
#453735,#453736,#453737,#453738,#453739,#453740,#453741,#453742,#453743,
#453744,#453745,#453746,#453747,#453748,#453749,#453750,#453751,#453752,
#453753,#453754,#453755,#453756,#453757,#453758,#453759,#453760,#453761,
#453762,#453763,#453764,#453765,#453766,#453767,#453768,#453769,#453770,
#453771,#453772,#453773,#453774,#453775),(#453776,#453777,#453778,#453779,
#453780,#453781,#453782,#453783,#453784,#453785,#453786,#453787,#453788,
#453789,#453790,#453791,#453792,#453793,#453794,#453795,#453796,#453797,
#453798,#453799,#453800,#453801,#453802,#453803,#453804,#453805,#453806,
#453807,#453808,#453809,#453810,#453811,#453812,#453813,#453814,#453815,
#453816,#453817,#453818,#453819,#453820,#453821,#453822,#453823,#453824,
#453825,#453826,#453827,#453828,#453829),(#453830,#453831,#453832,#453833,
#453834,#453835,#453836,#453837,#453838,#453839,#453840,#453841,#453842,
#453843,#453844,#453845,#453846,#453847,#453848,#453849,#453850,#453851,
#453852,#453853,#453854,#453855,#453856,#453857,#453858,#453859,#453860,
#453861,#453862,#453863,#453864,#453865,#453866,#453867,#453868,#453869,
#453870,#453871,#453872,#453873,#453874,#453875,#453876,#453877,#453878,
#453879,#453880,#453881,#453882,#453883),(#453884,#453885,#453886,#453887,
#453888,#453889,#453890,#453891,#453892,#453893,#453894,#453895,#453896,
#453897,#453898,#453899,#453900,#453901,#453902,#453903,#453904,#453905,
#453906,#453907,#453908,#453909,#453910,#453911,#453912,#453913,#453914,
#453915,#453916,#453917,#453918,#453919,#453920,#453921,#453922,#453923,
#453924,#453925,#453926,#453927,#453928,#453929,#453930,#453931,#453932,
#453933,#453934,#453935,#453936,#453937)),.UNSPECIFIED.,.F.,.F.,.F.,(4,
4),(4,1,1,1,1,1,1,1,1,1,1,1,1,1,1,1,1,1,1,1,1,1,1,1,1,1,1,1,1,1,1,1,1,1,
1,1,1,1,1,1,1,1,1,1,1,1,1,1,1,1,1,4),(0.,0.0291273210806165),(14.4000123930734,
15.3981043475128,16.3961963019522,17.3942882563917,18.3923802108311,19.3904721652705,
20.3885641197099,21.3866560741493,22.3847480285887,23.3828399830282,24.3809319374676,
25.379023891907,26.3771158463464,27.3752078007858,28.3732997552253,29.3713917096647,
30.3694836641041,31.3675756185435,32.3656675729829,33.3637595274224,34.3618514818618,
35.3599434363012,36.3580353907406,37.35612734518,38.3542192996195,39.3523112540589,
40.3504032084983,41.3484951629377,42.3465871173771,43.3446790718166,44.342771026256,
45.3408629806954,46.3389549351348,47.3370468895742,48.3351388440137,49.3332307984531,
50.3313227528925,51.3294147073319,52.3275066617713,53.3255986162108,54.3236905706502,
55.3217825250896,56.319874479529,57.3179664339684,58.3160583884079,59.3141503428473,
60.3122422972867,61.3103342517261,62.3084262061655,63.306518160605,64.3046101150444,
65.3027020694838),.UNSPECIFIED.);
#6341=B_SPLINE_SURFACE_WITH_KNOTS('',3,3,((#453983,#453984,#453985,#453986,
#453987,#453988,#453989,#453990,#453991,#453992,#453993,#453994,#453995,
#453996,#453997,#453998,#453999,#454000,#454001,#454002,#454003,#454004,
#454005,#454006,#454007,#454008,#454009,#454010,#454011,#454012,#454013,
#454014,#454015,#454016,#454017,#454018,#454019,#454020,#454021,#454022,
#454023,#454024,#454025,#454026,#454027,#454028,#454029,#454030,#454031,
#454032,#454033,#454034,#454035,#454036),(#454037,#454038,#454039,#454040,
#454041,#454042,#454043,#454044,#454045,#454046,#454047,#454048,#454049,
#454050,#454051,#454052,#454053,#454054,#454055,#454056,#454057,#454058,
#454059,#454060,#454061,#454062,#454063,#454064,#454065,#454066,#454067,
#454068,#454069,#454070,#454071,#454072,#454073,#454074,#454075,#454076,
#454077,#454078,#454079,#454080,#454081,#454082,#454083,#454084,#454085,
#454086,#454087,#454088,#454089,#454090),(#454091,#454092,#454093,#454094,
#454095,#454096,#454097,#454098,#454099,#454100,#454101,#454102,#454103,
#454104,#454105,#454106,#454107,#454108,#454109,#454110,#454111,#454112,
#454113,#454114,#454115,#454116,#454117,#454118,#454119,#454120,#454121,
#454122,#454123,#454124,#454125,#454126,#454127,#454128,#454129,#454130,
#454131,#454132,#454133,#454134,#454135,#454136,#454137,#454138,#454139,
#454140,#454141,#454142,#454143,#454144),(#454145,#454146,#454147,#454148,
#454149,#454150,#454151,#454152,#454153,#454154,#454155,#454156,#454157,
#454158,#454159,#454160,#454161,#454162,#454163,#454164,#454165,#454166,
#454167,#454168,#454169,#454170,#454171,#454172,#454173,#454174,#454175,
#454176,#454177,#454178,#454179,#454180,#454181,#454182,#454183,#454184,
#454185,#454186,#454187,#454188,#454189,#454190,#454191,#454192,#454193,
#454194,#454195,#454196,#454197,#454198)),.UNSPECIFIED.,.F.,.F.,.F.,(4,
4),(4,1,1,1,1,1,1,1,1,1,1,1,1,1,1,1,1,1,1,1,1,1,1,1,1,1,1,1,1,1,1,1,1,1,
1,1,1,1,1,1,1,1,1,1,1,1,1,1,1,1,1,4),(0.,0.0291273210806165),(11.8408508686654,
12.8389428231049,13.8370347775443,14.8351267319837,15.8332186864231,16.8313106408625,
17.829402595302,18.8274945497414,19.8255865041808,20.8236784586202,21.8217704130596,
22.8198623674991,23.8179543219385,24.8160462763779,25.8141382308173,26.8122301852567,
27.8103221396962,28.8084140941356,29.806506048575,30.8045980030144,31.8026899574538,
32.8007819118933,33.7988738663327,34.7969658207721,35.7950577752115,36.7931497296509,
37.7912416840904,38.7893336385298,39.7874255929692,40.7855175474086,41.783609501848,
42.7817014562875,43.7797934107269,44.7778853651663,45.7759773196057,46.7740692740451,
47.7721612284846,48.770253182924,49.7683451373634,50.7664370918028,51.7645290462422,
52.7626210006817,53.7607129551211,54.7588049095605,55.7568968639999,56.7549888184393,
57.7530807728788,58.7511727273182,59.7492646817576,60.747356636197,61.7454485906364,
62.7435405450759),.UNSPECIFIED.);
#6342=B_SPLINE_SURFACE_WITH_KNOTS('',3,3,((#454224,#454225,#454226,#454227,
#454228,#454229,#454230,#454231,#454232,#454233,#454234,#454235,#454236,
#454237,#454238,#454239,#454240,#454241,#454242,#454243,#454244,#454245,
#454246,#454247,#454248,#454249,#454250,#454251,#454252,#454253,#454254,
#454255,#454256,#454257,#454258,#454259,#454260,#454261,#454262,#454263,
#454264,#454265,#454266,#454267,#454268,#454269,#454270,#454271,#454272,
#454273,#454274,#454275,#454276,#454277),(#454278,#454279,#454280,#454281,
#454282,#454283,#454284,#454285,#454286,#454287,#454288,#454289,#454290,
#454291,#454292,#454293,#454294,#454295,#454296,#454297,#454298,#454299,
#454300,#454301,#454302,#454303,#454304,#454305,#454306,#454307,#454308,
#454309,#454310,#454311,#454312,#454313,#454314,#454315,#454316,#454317,
#454318,#454319,#454320,#454321,#454322,#454323,#454324,#454325,#454326,
#454327,#454328,#454329,#454330,#454331),(#454332,#454333,#454334,#454335,
#454336,#454337,#454338,#454339,#454340,#454341,#454342,#454343,#454344,
#454345,#454346,#454347,#454348,#454349,#454350,#454351,#454352,#454353,
#454354,#454355,#454356,#454357,#454358,#454359,#454360,#454361,#454362,
#454363,#454364,#454365,#454366,#454367,#454368,#454369,#454370,#454371,
#454372,#454373,#454374,#454375,#454376,#454377,#454378,#454379,#454380,
#454381,#454382,#454383,#454384,#454385),(#454386,#454387,#454388,#454389,
#454390,#454391,#454392,#454393,#454394,#454395,#454396,#454397,#454398,
#454399,#454400,#454401,#454402,#454403,#454404,#454405,#454406,#454407,
#454408,#454409,#454410,#454411,#454412,#454413,#454414,#454415,#454416,
#454417,#454418,#454419,#454420,#454421,#454422,#454423,#454424,#454425,
#454426,#454427,#454428,#454429,#454430,#454431,#454432,#454433,#454434,
#454435,#454436,#454437,#454438,#454439)),.UNSPECIFIED.,.F.,.F.,.F.,(4,
4),(4,1,1,1,1,1,1,1,1,1,1,1,1,1,1,1,1,1,1,1,1,1,1,1,1,1,1,1,1,1,1,1,1,1,
1,1,1,1,1,1,1,1,1,1,1,1,1,1,1,1,1,4),(0.,0.0291273210806165),(14.4000123930734,
15.3981043475128,16.3961963019522,17.3942882563917,18.3923802108311,19.3904721652705,
20.3885641197099,21.3866560741493,22.3847480285887,23.3828399830282,24.3809319374676,
25.379023891907,26.3771158463464,27.3752078007858,28.3732997552253,29.3713917096647,
30.3694836641041,31.3675756185435,32.3656675729829,33.3637595274224,34.3618514818618,
35.3599434363012,36.3580353907406,37.35612734518,38.3542192996195,39.3523112540589,
40.3504032084983,41.3484951629377,42.3465871173771,43.3446790718166,44.342771026256,
45.3408629806954,46.3389549351348,47.3370468895742,48.3351388440137,49.3332307984531,
50.3313227528925,51.3294147073319,52.3275066617713,53.3255986162108,54.3236905706502,
55.3217825250896,56.319874479529,57.3179664339684,58.3160583884079,59.3141503428473,
60.3122422972867,61.3103342517261,62.3084262061655,63.306518160605,64.3046101150444,
65.3027020694838),.UNSPECIFIED.);
#6343=B_SPLINE_SURFACE_WITH_KNOTS('',3,3,((#454485,#454486,#454487,#454488,
#454489,#454490,#454491,#454492,#454493,#454494,#454495,#454496,#454497,
#454498,#454499,#454500,#454501,#454502,#454503,#454504,#454505,#454506,
#454507,#454508,#454509,#454510,#454511,#454512,#454513,#454514,#454515,
#454516,#454517,#454518,#454519,#454520,#454521,#454522,#454523,#454524,
#454525,#454526,#454527,#454528,#454529,#454530,#454531,#454532,#454533,
#454534,#454535,#454536,#454537,#454538),(#454539,#454540,#454541,#454542,
#454543,#454544,#454545,#454546,#454547,#454548,#454549,#454550,#454551,
#454552,#454553,#454554,#454555,#454556,#454557,#454558,#454559,#454560,
#454561,#454562,#454563,#454564,#454565,#454566,#454567,#454568,#454569,
#454570,#454571,#454572,#454573,#454574,#454575,#454576,#454577,#454578,
#454579,#454580,#454581,#454582,#454583,#454584,#454585,#454586,#454587,
#454588,#454589,#454590,#454591,#454592),(#454593,#454594,#454595,#454596,
#454597,#454598,#454599,#454600,#454601,#454602,#454603,#454604,#454605,
#454606,#454607,#454608,#454609,#454610,#454611,#454612,#454613,#454614,
#454615,#454616,#454617,#454618,#454619,#454620,#454621,#454622,#454623,
#454624,#454625,#454626,#454627,#454628,#454629,#454630,#454631,#454632,
#454633,#454634,#454635,#454636,#454637,#454638,#454639,#454640,#454641,
#454642,#454643,#454644,#454645,#454646),(#454647,#454648,#454649,#454650,
#454651,#454652,#454653,#454654,#454655,#454656,#454657,#454658,#454659,
#454660,#454661,#454662,#454663,#454664,#454665,#454666,#454667,#454668,
#454669,#454670,#454671,#454672,#454673,#454674,#454675,#454676,#454677,
#454678,#454679,#454680,#454681,#454682,#454683,#454684,#454685,#454686,
#454687,#454688,#454689,#454690,#454691,#454692,#454693,#454694,#454695,
#454696,#454697,#454698,#454699,#454700)),.UNSPECIFIED.,.F.,.F.,.F.,(4,
4),(4,1,1,1,1,1,1,1,1,1,1,1,1,1,1,1,1,1,1,1,1,1,1,1,1,1,1,1,1,1,1,1,1,1,
1,1,1,1,1,1,1,1,1,1,1,1,1,1,1,1,1,4),(0.,0.0291273210806165),(11.8408508686654,
12.8389428231049,13.8370347775443,14.8351267319837,15.8332186864231,16.8313106408625,
17.829402595302,18.8274945497414,19.8255865041808,20.8236784586202,21.8217704130596,
22.8198623674991,23.8179543219385,24.8160462763779,25.8141382308173,26.8122301852567,
27.8103221396962,28.8084140941356,29.806506048575,30.8045980030144,31.8026899574538,
32.8007819118933,33.7988738663327,34.7969658207721,35.7950577752115,36.7931497296509,
37.7912416840904,38.7893336385298,39.7874255929692,40.7855175474086,41.783609501848,
42.7817014562875,43.7797934107269,44.7778853651663,45.7759773196057,46.7740692740451,
47.7721612284846,48.770253182924,49.7683451373634,50.7664370918028,51.7645290462422,
52.7626210006817,53.7607129551211,54.7588049095605,55.7568968639999,56.7549888184393,
57.7530807728788,58.7511727273182,59.7492646817576,60.747356636197,61.7454485906364,
62.7435405450759),.UNSPECIFIED.);
#6344=B_SPLINE_SURFACE_WITH_KNOTS('',3,3,((#454726,#454727,#454728,#454729,
#454730,#454731,#454732,#454733,#454734,#454735,#454736,#454737,#454738,
#454739,#454740,#454741,#454742,#454743,#454744,#454745,#454746,#454747,
#454748,#454749,#454750,#454751,#454752,#454753,#454754,#454755,#454756,
#454757,#454758,#454759,#454760,#454761,#454762,#454763,#454764,#454765,
#454766,#454767,#454768,#454769,#454770,#454771,#454772,#454773,#454774,
#454775,#454776,#454777,#454778,#454779),(#454780,#454781,#454782,#454783,
#454784,#454785,#454786,#454787,#454788,#454789,#454790,#454791,#454792,
#454793,#454794,#454795,#454796,#454797,#454798,#454799,#454800,#454801,
#454802,#454803,#454804,#454805,#454806,#454807,#454808,#454809,#454810,
#454811,#454812,#454813,#454814,#454815,#454816,#454817,#454818,#454819,
#454820,#454821,#454822,#454823,#454824,#454825,#454826,#454827,#454828,
#454829,#454830,#454831,#454832,#454833),(#454834,#454835,#454836,#454837,
#454838,#454839,#454840,#454841,#454842,#454843,#454844,#454845,#454846,
#454847,#454848,#454849,#454850,#454851,#454852,#454853,#454854,#454855,
#454856,#454857,#454858,#454859,#454860,#454861,#454862,#454863,#454864,
#454865,#454866,#454867,#454868,#454869,#454870,#454871,#454872,#454873,
#454874,#454875,#454876,#454877,#454878,#454879,#454880,#454881,#454882,
#454883,#454884,#454885,#454886,#454887),(#454888,#454889,#454890,#454891,
#454892,#454893,#454894,#454895,#454896,#454897,#454898,#454899,#454900,
#454901,#454902,#454903,#454904,#454905,#454906,#454907,#454908,#454909,
#454910,#454911,#454912,#454913,#454914,#454915,#454916,#454917,#454918,
#454919,#454920,#454921,#454922,#454923,#454924,#454925,#454926,#454927,
#454928,#454929,#454930,#454931,#454932,#454933,#454934,#454935,#454936,
#454937,#454938,#454939,#454940,#454941)),.UNSPECIFIED.,.F.,.F.,.F.,(4,
4),(4,1,1,1,1,1,1,1,1,1,1,1,1,1,1,1,1,1,1,1,1,1,1,1,1,1,1,1,1,1,1,1,1,1,
1,1,1,1,1,1,1,1,1,1,1,1,1,1,1,1,1,4),(0.,0.0291273210806165),(14.4000123930734,
15.3981043475128,16.3961963019522,17.3942882563917,18.3923802108311,19.3904721652705,
20.3885641197099,21.3866560741493,22.3847480285887,23.3828399830282,24.3809319374676,
25.379023891907,26.3771158463464,27.3752078007858,28.3732997552253,29.3713917096647,
30.3694836641041,31.3675756185435,32.3656675729829,33.3637595274224,34.3618514818618,
35.3599434363012,36.3580353907406,37.35612734518,38.3542192996195,39.3523112540589,
40.3504032084983,41.3484951629377,42.3465871173771,43.3446790718166,44.342771026256,
45.3408629806954,46.3389549351348,47.3370468895742,48.3351388440137,49.3332307984531,
50.3313227528925,51.3294147073319,52.3275066617713,53.3255986162108,54.3236905706502,
55.3217825250896,56.319874479529,57.3179664339684,58.3160583884079,59.3141503428473,
60.3122422972867,61.3103342517261,62.3084262061655,63.306518160605,64.3046101150444,
65.3027020694838),.UNSPECIFIED.);
#6345=B_SPLINE_SURFACE_WITH_KNOTS('',3,3,((#456005,#456006,#456007,#456008,
#456009,#456010,#456011,#456012,#456013,#456014,#456015,#456016,#456017,
#456018,#456019,#456020,#456021,#456022,#456023,#456024,#456025,#456026,
#456027,#456028,#456029,#456030,#456031,#456032,#456033,#456034,#456035,
#456036,#456037,#456038,#456039,#456040,#456041),(#456042,#456043,#456044,
#456045,#456046,#456047,#456048,#456049,#456050,#456051,#456052,#456053,
#456054,#456055,#456056,#456057,#456058,#456059,#456060,#456061,#456062,
#456063,#456064,#456065,#456066,#456067,#456068,#456069,#456070,#456071,
#456072,#456073,#456074,#456075,#456076,#456077,#456078),(#456079,#456080,
#456081,#456082,#456083,#456084,#456085,#456086,#456087,#456088,#456089,
#456090,#456091,#456092,#456093,#456094,#456095,#456096,#456097,#456098,
#456099,#456100,#456101,#456102,#456103,#456104,#456105,#456106,#456107,
#456108,#456109,#456110,#456111,#456112,#456113,#456114,#456115),(#456116,
#456117,#456118,#456119,#456120,#456121,#456122,#456123,#456124,#456125,
#456126,#456127,#456128,#456129,#456130,#456131,#456132,#456133,#456134,
#456135,#456136,#456137,#456138,#456139,#456140,#456141,#456142,#456143,
#456144,#456145,#456146,#456147,#456148,#456149,#456150,#456151,#456152)),
 .UNSPECIFIED.,.F.,.F.,.F.,(4,4),(4,1,1,1,1,1,1,1,1,1,1,1,1,1,1,1,1,1,1,
1,1,1,1,1,1,1,1,1,1,1,1,1,1,1,4),(0.,0.0658467982010768),(8.3074775524011,
9.29231769095425,10.2771578295074,11.2619979680605,12.2468381066137,13.2316782451668,
14.21651838372,15.2013585222731,16.1861986608263,17.1710387993794,18.1558789379326,
19.1407190764857,20.1255592150389,21.110399353592,22.0952394921452,23.0800796306983,
24.0649197692515,25.0497599078046,26.0346000463578,27.0194401849109,28.0042803234641,
28.9891204620172,29.9739606005704,30.9588007391235,31.9436408776767,32.9284810162298,
33.913321154783,34.8981612933361,35.8830014318893,36.8678415704424,37.8526817089956,
38.8375218475487,39.8223619861019,40.807202124655,41.7920422632082),
 .UNSPECIFIED.);
#6346=B_SPLINE_SURFACE_WITH_KNOTS('',3,3,((#456376,#456377,#456378,#456379,
#456380,#456381,#456382,#456383,#456384,#456385,#456386,#456387,#456388,
#456389,#456390,#456391,#456392,#456393,#456394,#456395,#456396,#456397,
#456398,#456399,#456400,#456401,#456402,#456403,#456404,#456405,#456406,
#456407,#456408,#456409,#456410,#456411,#456412),(#456413,#456414,#456415,
#456416,#456417,#456418,#456419,#456420,#456421,#456422,#456423,#456424,
#456425,#456426,#456427,#456428,#456429,#456430,#456431,#456432,#456433,
#456434,#456435,#456436,#456437,#456438,#456439,#456440,#456441,#456442,
#456443,#456444,#456445,#456446,#456447,#456448,#456449),(#456450,#456451,
#456452,#456453,#456454,#456455,#456456,#456457,#456458,#456459,#456460,
#456461,#456462,#456463,#456464,#456465,#456466,#456467,#456468,#456469,
#456470,#456471,#456472,#456473,#456474,#456475,#456476,#456477,#456478,
#456479,#456480,#456481,#456482,#456483,#456484,#456485,#456486),(#456487,
#456488,#456489,#456490,#456491,#456492,#456493,#456494,#456495,#456496,
#456497,#456498,#456499,#456500,#456501,#456502,#456503,#456504,#456505,
#456506,#456507,#456508,#456509,#456510,#456511,#456512,#456513,#456514,
#456515,#456516,#456517,#456518,#456519,#456520,#456521,#456522,#456523)),
 .UNSPECIFIED.,.F.,.F.,.F.,(4,4),(4,1,1,1,1,1,1,1,1,1,1,1,1,1,1,1,1,1,1,
1,1,1,1,1,1,1,1,1,1,1,1,1,1,1,4),(0.,0.0658467982010768),(11.6150328478183,
12.5998729863715,13.5847131249246,14.5695532634778,15.5543934020309,16.5392335405841,
17.5240736791372,18.5089138176904,19.4937539562435,20.4785940947967,21.4634342333498,
22.448274371903,23.4331145104561,24.4179546490093,25.4027947875624,26.3876349261156,
27.3724750646687,28.3573152032219,29.342155341775,30.3269954803282,31.3118356188813,
32.2966757574344,33.2815158959876,34.2663560345407,35.2511961730939,36.236036311647,
37.2208764502002,38.2057165887533,39.1905567273065,40.1753968658596,41.1602370044128,
42.1450771429659,43.1299172815191,44.1147574200722,45.0995975586254),
 .UNSPECIFIED.);
#6347=B_SPLINE_SURFACE_WITH_KNOTS('',3,3,((#456775,#456776,#456777,#456778,
#456779,#456780,#456781,#456782,#456783,#456784,#456785,#456786,#456787,
#456788,#456789,#456790,#456791,#456792,#456793,#456794,#456795,#456796,
#456797,#456798,#456799,#456800,#456801,#456802,#456803,#456804,#456805,
#456806,#456807,#456808,#456809,#456810,#456811,#456812,#456813,#456814,
#456815,#456816,#456817,#456818,#456819,#456820,#456821,#456822,#456823,
#456824,#456825,#456826,#456827,#456828,#456829,#456830,#456831,#456832,
#456833,#456834,#456835,#456836,#456837,#456838,#456839,#456840,#456841),
(#456842,#456843,#456844,#456845,#456846,#456847,#456848,#456849,#456850,
#456851,#456852,#456853,#456854,#456855,#456856,#456857,#456858,#456859,
#456860,#456861,#456862,#456863,#456864,#456865,#456866,#456867,#456868,
#456869,#456870,#456871,#456872,#456873,#456874,#456875,#456876,#456877,
#456878,#456879,#456880,#456881,#456882,#456883,#456884,#456885,#456886,
#456887,#456888,#456889,#456890,#456891,#456892,#456893,#456894,#456895,
#456896,#456897,#456898,#456899,#456900,#456901,#456902,#456903,#456904,
#456905,#456906,#456907,#456908),(#456909,#456910,#456911,#456912,#456913,
#456914,#456915,#456916,#456917,#456918,#456919,#456920,#456921,#456922,
#456923,#456924,#456925,#456926,#456927,#456928,#456929,#456930,#456931,
#456932,#456933,#456934,#456935,#456936,#456937,#456938,#456939,#456940,
#456941,#456942,#456943,#456944,#456945,#456946,#456947,#456948,#456949,
#456950,#456951,#456952,#456953,#456954,#456955,#456956,#456957,#456958,
#456959,#456960,#456961,#456962,#456963,#456964,#456965,#456966,#456967,
#456968,#456969,#456970,#456971,#456972,#456973,#456974,#456975),(#456976,
#456977,#456978,#456979,#456980,#456981,#456982,#456983,#456984,#456985,
#456986,#456987,#456988,#456989,#456990,#456991,#456992,#456993,#456994,
#456995,#456996,#456997,#456998,#456999,#457000,#457001,#457002,#457003,
#457004,#457005,#457006,#457007,#457008,#457009,#457010,#457011,#457012,
#457013,#457014,#457015,#457016,#457017,#457018,#457019,#457020,#457021,
#457022,#457023,#457024,#457025,#457026,#457027,#457028,#457029,#457030,
#457031,#457032,#457033,#457034,#457035,#457036,#457037,#457038,#457039,
#457040,#457041,#457042)),.UNSPECIFIED.,.F.,.F.,.F.,(4,4),(4,1,1,1,1,1,
1,1,1,1,1,1,1,1,1,1,1,1,1,1,1,1,1,1,1,1,1,1,1,1,1,1,1,1,1,1,1,1,1,1,1,1,
1,1,1,1,1,1,1,1,1,1,1,1,1,1,1,1,1,1,1,1,1,1,4),(0.,0.0658179306876173),
(8.30838445208317,9.30280550342046,10.2972265547578,11.2916476060951,12.2860686574324,
13.2804897087697,14.2749107601069,15.2693318114442,16.2637528627815,17.2581739141188,
18.2525949654561,19.2470160167934,20.2414370681307,21.235858119468,22.2302791708053,
23.2247002221426,24.2191212734799,25.2135423248172,26.2079633761545,27.2023844274918,
28.1968054788291,29.1912265301664,30.1856475815037,31.180068632841,32.1744896841783,
33.1689107355156,34.1633317868529,35.1577528381902,36.1521738895275,37.1465949408648,
38.1410159922021,39.1354370435394,40.1298580948767,41.1242791462139,42.1187001975512,
43.1131212488885,44.1075423002258,45.1019633515631,46.0963844029004,47.0908054542377,
48.085226505575,49.0796475569123,50.0740686082496,51.0684896595869,52.0629107109242,
53.0573317622615,54.0517528135988,55.0461738649361,56.0405949162734,57.0350159676107,
58.029437018948,59.0238580702853,60.0182791216226,61.0127001729599,62.0071212242972,
63.0015422756345,63.9959633269718,64.9903843783091,65.9848054296463,66.9792264809836,
67.9736475323209,68.9680685836582,69.9624896349955,70.9569106863328,71.9513317376701),
 .UNSPECIFIED.);
#6348=B_SPLINE_SURFACE_WITH_KNOTS('',3,3,((#457239,#457240,#457241,#457242,
#457243,#457244,#457245,#457246,#457247,#457248,#457249,#457250,#457251,
#457252,#457253,#457254,#457255,#457256,#457257,#457258,#457259,#457260,
#457261,#457262,#457263,#457264,#457265,#457266,#457267,#457268,#457269,
#457270,#457271,#457272,#457273,#457274,#457275,#457276,#457277,#457278,
#457279,#457280,#457281,#457282,#457283,#457284,#457285,#457286,#457287,
#457288,#457289,#457290,#457291,#457292,#457293,#457294,#457295,#457296,
#457297,#457298,#457299,#457300,#457301,#457302,#457303,#457304,#457305),
(#457306,#457307,#457308,#457309,#457310,#457311,#457312,#457313,#457314,
#457315,#457316,#457317,#457318,#457319,#457320,#457321,#457322,#457323,
#457324,#457325,#457326,#457327,#457328,#457329,#457330,#457331,#457332,
#457333,#457334,#457335,#457336,#457337,#457338,#457339,#457340,#457341,
#457342,#457343,#457344,#457345,#457346,#457347,#457348,#457349,#457350,
#457351,#457352,#457353,#457354,#457355,#457356,#457357,#457358,#457359,
#457360,#457361,#457362,#457363,#457364,#457365,#457366,#457367,#457368,
#457369,#457370,#457371,#457372),(#457373,#457374,#457375,#457376,#457377,
#457378,#457379,#457380,#457381,#457382,#457383,#457384,#457385,#457386,
#457387,#457388,#457389,#457390,#457391,#457392,#457393,#457394,#457395,
#457396,#457397,#457398,#457399,#457400,#457401,#457402,#457403,#457404,
#457405,#457406,#457407,#457408,#457409,#457410,#457411,#457412,#457413,
#457414,#457415,#457416,#457417,#457418,#457419,#457420,#457421,#457422,
#457423,#457424,#457425,#457426,#457427,#457428,#457429,#457430,#457431,
#457432,#457433,#457434,#457435,#457436,#457437,#457438,#457439),(#457440,
#457441,#457442,#457443,#457444,#457445,#457446,#457447,#457448,#457449,
#457450,#457451,#457452,#457453,#457454,#457455,#457456,#457457,#457458,
#457459,#457460,#457461,#457462,#457463,#457464,#457465,#457466,#457467,
#457468,#457469,#457470,#457471,#457472,#457473,#457474,#457475,#457476,
#457477,#457478,#457479,#457480,#457481,#457482,#457483,#457484,#457485,
#457486,#457487,#457488,#457489,#457490,#457491,#457492,#457493,#457494,
#457495,#457496,#457497,#457498,#457499,#457500,#457501,#457502,#457503,
#457504,#457505,#457506)),.UNSPECIFIED.,.F.,.F.,.F.,(4,4),(4,1,1,1,1,1,
1,1,1,1,1,1,1,1,1,1,1,1,1,1,1,1,1,1,1,1,1,1,1,1,1,1,1,1,1,1,1,1,1,1,1,1,
1,1,1,1,1,1,1,1,1,1,1,1,1,1,1,1,1,1,1,1,1,1,4),(0.,0.0658179306876173),
(11.6150328478183,12.6094538991556,13.6038749504929,14.5982960018302,15.5927170531675,
16.5871381045047,17.581559155842,18.5759802071793,19.5704012585166,20.5648223098539,
21.5592433611912,22.5536644125285,23.5480854638658,24.5425065152031,25.5369275665404,
26.5313486178777,27.525769669215,28.5201907205523,29.5146117718896,30.5090328232269,
31.5034538745642,32.4978749259015,33.4922959772388,34.4867170285761,35.4811380799134,
36.4755591312507,37.469980182588,38.4644012339253,39.4588222852626,40.4532433365999,
41.4476643879372,42.4420854392745,43.4365064906117,44.430927541949,45.4253485932863,
46.4197696446236,47.4141906959609,48.4086117472982,49.4030327986355,50.3974538499728,
51.3918749013101,52.3862959526474,53.3807170039847,54.375138055322,55.3695591066593,
56.3639801579966,57.3584012093339,58.3528222606712,59.3472433120085,60.3416643633458,
61.3360854146831,62.3305064660204,63.3249275173577,64.319348568695,65.3137696200323,
66.3081906713696,67.3026117227069,68.2970327740442,69.2914538253815,70.2858748767188,
71.280295928056,72.2747169793933,73.2691380307306,74.2635590820679,75.2579801334052),
 .UNSPECIFIED.);
#6349=B_SPLINE_SURFACE_WITH_KNOTS('',3,3,((#458143,#458144,#458145,#458146,
#458147,#458148,#458149,#458150,#458151,#458152,#458153,#458154,#458155,
#458156,#458157,#458158,#458159,#458160,#458161,#458162,#458163,#458164,
#458165,#458166,#458167,#458168,#458169,#458170,#458171,#458172,#458173,
#458174,#458175,#458176,#458177,#458178,#458179,#458180,#458181,#458182,
#458183,#458184,#458185),(#458186,#458187,#458188,#458189,#458190,#458191,
#458192,#458193,#458194,#458195,#458196,#458197,#458198,#458199,#458200,
#458201,#458202,#458203,#458204,#458205,#458206,#458207,#458208,#458209,
#458210,#458211,#458212,#458213,#458214,#458215,#458216,#458217,#458218,
#458219,#458220,#458221,#458222,#458223,#458224,#458225,#458226,#458227,
#458228),(#458229,#458230,#458231,#458232,#458233,#458234,#458235,#458236,
#458237,#458238,#458239,#458240,#458241,#458242,#458243,#458244,#458245,
#458246,#458247,#458248,#458249,#458250,#458251,#458252,#458253,#458254,
#458255,#458256,#458257,#458258,#458259,#458260,#458261,#458262,#458263,
#458264,#458265,#458266,#458267,#458268,#458269,#458270,#458271),(#458272,
#458273,#458274,#458275,#458276,#458277,#458278,#458279,#458280,#458281,
#458282,#458283,#458284,#458285,#458286,#458287,#458288,#458289,#458290,
#458291,#458292,#458293,#458294,#458295,#458296,#458297,#458298,#458299,
#458300,#458301,#458302,#458303,#458304,#458305,#458306,#458307,#458308,
#458309,#458310,#458311,#458312,#458313,#458314)),.UNSPECIFIED.,.F.,.F.,
 .F.,(4,4),(4,1,1,1,1,1,1,1,1,1,1,1,1,1,1,1,1,1,1,1,1,1,1,1,1,1,1,1,1,1,
1,1,1,1,1,1,1,1,1,1,4),(0.,0.0658467982010768),(8.30747755240108,9.30167130285074,
10.2958650533004,11.2900588037501,12.2842525541997,13.2784463046494,14.2726400550991,
15.2668338055487,16.2610275559984,17.2552213064481,18.2494150568977,19.2436088073474,
20.2378025577971,21.2319963082467,22.2261900586964,23.2203838091461,24.2145775595957,
25.2087713100454,26.2029650604951,27.1971588109447,28.1913525613944,29.1855463118441,
30.1797400622937,31.1739338127434,32.1681275631931,33.1623213136427,34.1565150640924,
35.1507088145421,36.1449025649917,37.1390963154414,38.1332900658911,39.1274838163407,
40.1216775667904,41.1158713172401,42.1100650676897,43.1042588181394,44.0984525685891,
45.0926463190387,46.0868400694884,47.081033819938,48.0752275703877),
 .UNSPECIFIED.);
#6350=B_SPLINE_SURFACE_WITH_KNOTS('',3,3,((#458565,#458566,#458567,#458568,
#458569,#458570,#458571,#458572,#458573,#458574,#458575,#458576,#458577,
#458578,#458579,#458580,#458581,#458582,#458583,#458584,#458585,#458586,
#458587,#458588,#458589,#458590,#458591,#458592,#458593,#458594,#458595,
#458596,#458597,#458598,#458599,#458600,#458601,#458602,#458603,#458604,
#458605,#458606,#458607),(#458608,#458609,#458610,#458611,#458612,#458613,
#458614,#458615,#458616,#458617,#458618,#458619,#458620,#458621,#458622,
#458623,#458624,#458625,#458626,#458627,#458628,#458629,#458630,#458631,
#458632,#458633,#458634,#458635,#458636,#458637,#458638,#458639,#458640,
#458641,#458642,#458643,#458644,#458645,#458646,#458647,#458648,#458649,
#458650),(#458651,#458652,#458653,#458654,#458655,#458656,#458657,#458658,
#458659,#458660,#458661,#458662,#458663,#458664,#458665,#458666,#458667,
#458668,#458669,#458670,#458671,#458672,#458673,#458674,#458675,#458676,
#458677,#458678,#458679,#458680,#458681,#458682,#458683,#458684,#458685,
#458686,#458687,#458688,#458689,#458690,#458691,#458692,#458693),(#458694,
#458695,#458696,#458697,#458698,#458699,#458700,#458701,#458702,#458703,
#458704,#458705,#458706,#458707,#458708,#458709,#458710,#458711,#458712,
#458713,#458714,#458715,#458716,#458717,#458718,#458719,#458720,#458721,
#458722,#458723,#458724,#458725,#458726,#458727,#458728,#458729,#458730,
#458731,#458732,#458733,#458734,#458735,#458736)),.UNSPECIFIED.,.F.,.F.,
 .F.,(4,4),(4,1,1,1,1,1,1,1,1,1,1,1,1,1,1,1,1,1,1,1,1,1,1,1,1,1,1,1,1,1,
1,1,1,1,1,1,1,1,1,1,4),(0.,0.0658467982010768),(11.6150328478183,12.609226598268,
13.6034203487176,14.5976140991673,15.591807849617,16.5860016000666,17.5801953505163,
18.574389100966,19.5685828514156,20.5627766018653,21.556970352315,22.5511641027646,
23.5453578532143,24.539551603664,25.5337453541136,26.5279391045633,27.522132855013,
28.5163266054626,29.5105203559123,30.504714106362,31.4989078568116,32.4931016072613,
33.487295357711,34.4814891081606,35.4756828586103,36.46987660906,37.4640703595096,
38.4582641099593,39.452457860409,40.4466516108586,41.4408453613083,42.4350391117579,
43.4292328622076,44.4234266126573,45.4176203631069,46.4118141135566,47.4060078640063,
48.400201614456,49.3943953649056,50.3885891153553,51.3827828658049),
 .UNSPECIFIED.);
#6351=FACE_OUTER_BOUND('',#12159,.T.);
#6352=FACE_OUTER_BOUND('',#12160,.T.);
#6353=FACE_OUTER_BOUND('',#12161,.T.);
#6354=FACE_OUTER_BOUND('',#12162,.T.);
#6355=FACE_OUTER_BOUND('',#12163,.T.);
#6356=FACE_OUTER_BOUND('',#12164,.T.);
#6357=FACE_OUTER_BOUND('',#12165,.T.);
#6358=FACE_OUTER_BOUND('',#12166,.T.);
#6359=FACE_OUTER_BOUND('',#12167,.T.);
#6360=FACE_OUTER_BOUND('',#12168,.T.);
#6361=FACE_OUTER_BOUND('',#12169,.T.);
#6362=FACE_OUTER_BOUND('',#12170,.T.);
#6363=FACE_OUTER_BOUND('',#12171,.T.);
#6364=FACE_OUTER_BOUND('',#12172,.T.);
#6365=FACE_OUTER_BOUND('',#12173,.T.);
#6366=FACE_OUTER_BOUND('',#12174,.T.);
#6367=FACE_OUTER_BOUND('',#12175,.T.);
#6368=FACE_OUTER_BOUND('',#12176,.T.);
#6369=FACE_OUTER_BOUND('',#12177,.T.);
#6370=FACE_OUTER_BOUND('',#12178,.T.);
#6371=FACE_OUTER_BOUND('',#12179,.T.);
#6372=FACE_OUTER_BOUND('',#12180,.T.);
#6373=FACE_OUTER_BOUND('',#12181,.T.);
#6374=FACE_OUTER_BOUND('',#12183,.T.);
#6375=FACE_OUTER_BOUND('',#12184,.T.);
#6376=FACE_OUTER_BOUND('',#12185,.T.);
#6377=FACE_OUTER_BOUND('',#12187,.T.);
#6378=FACE_OUTER_BOUND('',#12188,.T.);
#6379=FACE_OUTER_BOUND('',#12189,.T.);
#6380=FACE_OUTER_BOUND('',#12191,.T.);
#6381=FACE_OUTER_BOUND('',#12192,.T.);
#6382=FACE_OUTER_BOUND('',#12193,.T.);
#6383=FACE_OUTER_BOUND('',#12195,.T.);
#6384=FACE_OUTER_BOUND('',#12196,.T.);
#6385=FACE_OUTER_BOUND('',#12197,.T.);
#6386=FACE_OUTER_BOUND('',#12199,.T.);
#6387=FACE_OUTER_BOUND('',#12200,.T.);
#6388=FACE_OUTER_BOUND('',#12202,.T.);
#6389=FACE_OUTER_BOUND('',#12203,.T.);
#6390=FACE_OUTER_BOUND('',#12204,.T.);
#6391=FACE_OUTER_BOUND('',#12205,.T.);
#6392=FACE_OUTER_BOUND('',#12206,.T.);
#6393=FACE_OUTER_BOUND('',#12207,.T.);
#6394=FACE_OUTER_BOUND('',#12208,.T.);
#6395=FACE_OUTER_BOUND('',#12209,.T.);
#6396=FACE_OUTER_BOUND('',#12210,.T.);
#6397=FACE_OUTER_BOUND('',#12211,.T.);
#6398=FACE_OUTER_BOUND('',#12212,.T.);
#6399=FACE_OUTER_BOUND('',#12213,.T.);
#6400=FACE_OUTER_BOUND('',#12214,.T.);
#6401=FACE_OUTER_BOUND('',#12215,.T.);
#6402=FACE_OUTER_BOUND('',#12216,.T.);
#6403=FACE_OUTER_BOUND('',#12217,.T.);
#6404=FACE_OUTER_BOUND('',#12218,.T.);
#6405=FACE_OUTER_BOUND('',#12219,.T.);
#6406=FACE_OUTER_BOUND('',#12220,.T.);
#6407=FACE_OUTER_BOUND('',#12221,.T.);
#6408=FACE_OUTER_BOUND('',#12222,.T.);
#6409=FACE_OUTER_BOUND('',#12223,.T.);
#6410=FACE_OUTER_BOUND('',#12224,.T.);
#6411=FACE_OUTER_BOUND('',#12225,.T.);
#6412=FACE_OUTER_BOUND('',#12226,.T.);
#6413=FACE_OUTER_BOUND('',#12227,.T.);
#6414=FACE_OUTER_BOUND('',#12228,.T.);
#6415=FACE_OUTER_BOUND('',#12229,.T.);
#6416=FACE_OUTER_BOUND('',#12230,.T.);
#6417=FACE_OUTER_BOUND('',#12231,.T.);
#6418=FACE_OUTER_BOUND('',#12235,.T.);
#6419=FACE_OUTER_BOUND('',#12236,.T.);
#6420=FACE_OUTER_BOUND('',#12237,.T.);
#6421=FACE_OUTER_BOUND('',#12238,.T.);
#6422=FACE_OUTER_BOUND('',#12239,.T.);
#6423=FACE_OUTER_BOUND('',#12240,.T.);
#6424=FACE_OUTER_BOUND('',#12242,.T.);
#6425=FACE_OUTER_BOUND('',#12243,.T.);
#6426=FACE_OUTER_BOUND('',#12245,.T.);
#6427=FACE_OUTER_BOUND('',#12246,.T.);
#6428=FACE_OUTER_BOUND('',#12247,.T.);
#6429=FACE_OUTER_BOUND('',#12248,.T.);
#6430=FACE_OUTER_BOUND('',#12249,.T.);
#6431=FACE_OUTER_BOUND('',#12250,.T.);
#6432=FACE_OUTER_BOUND('',#12251,.T.);
#6433=FACE_OUTER_BOUND('',#12252,.T.);
#6434=FACE_OUTER_BOUND('',#12253,.T.);
#6435=FACE_OUTER_BOUND('',#12254,.T.);
#6436=FACE_OUTER_BOUND('',#12255,.T.);
#6437=FACE_OUTER_BOUND('',#12256,.T.);
#6438=FACE_OUTER_BOUND('',#12257,.T.);
#6439=FACE_OUTER_BOUND('',#12258,.T.);
#6440=FACE_OUTER_BOUND('',#12259,.T.);
#6441=FACE_OUTER_BOUND('',#12260,.T.);
#6442=FACE_OUTER_BOUND('',#12261,.T.);
#6443=FACE_OUTER_BOUND('',#12262,.T.);
#6444=FACE_OUTER_BOUND('',#12263,.T.);
#6445=FACE_OUTER_BOUND('',#12264,.T.);
#6446=FACE_OUTER_BOUND('',#12265,.T.);
#6447=FACE_OUTER_BOUND('',#12266,.T.);
#6448=FACE_OUTER_BOUND('',#12267,.T.);
#6449=FACE_OUTER_BOUND('',#12268,.T.);
#6450=FACE_OUTER_BOUND('',#12269,.T.);
#6451=FACE_OUTER_BOUND('',#12270,.T.);
#6452=FACE_OUTER_BOUND('',#12271,.T.);
#6453=FACE_OUTER_BOUND('',#12272,.T.);
#6454=FACE_OUTER_BOUND('',#12273,.T.);
#6455=FACE_OUTER_BOUND('',#12274,.T.);
#6456=FACE_OUTER_BOUND('',#12275,.T.);
#6457=FACE_OUTER_BOUND('',#12276,.T.);
#6458=FACE_OUTER_BOUND('',#12277,.T.);
#6459=FACE_OUTER_BOUND('',#12278,.T.);
#6460=FACE_OUTER_BOUND('',#12279,.T.);
#6461=FACE_OUTER_BOUND('',#12280,.T.);
#6462=FACE_OUTER_BOUND('',#12281,.T.);
#6463=FACE_OUTER_BOUND('',#12282,.T.);
#6464=FACE_OUTER_BOUND('',#12283,.T.);
#6465=FACE_OUTER_BOUND('',#12284,.T.);
#6466=FACE_OUTER_BOUND('',#12285,.T.);
#6467=FACE_OUTER_BOUND('',#12286,.T.);
#6468=FACE_OUTER_BOUND('',#12287,.T.);
#6469=FACE_OUTER_BOUND('',#12288,.T.);
#6470=FACE_OUTER_BOUND('',#12289,.T.);
#6471=FACE_OUTER_BOUND('',#12290,.T.);
#6472=FACE_OUTER_BOUND('',#12291,.T.);
#6473=FACE_OUTER_BOUND('',#12292,.T.);
#6474=FACE_OUTER_BOUND('',#12293,.T.);
#6475=FACE_OUTER_BOUND('',#12294,.T.);
#6476=FACE_OUTER_BOUND('',#12295,.T.);
#6477=FACE_OUTER_BOUND('',#12296,.T.);
#6478=FACE_OUTER_BOUND('',#12297,.T.);
#6479=FACE_OUTER_BOUND('',#12298,.T.);
#6480=FACE_OUTER_BOUND('',#12299,.T.);
#6481=FACE_OUTER_BOUND('',#12300,.T.);
#6482=FACE_OUTER_BOUND('',#12301,.T.);
#6483=FACE_OUTER_BOUND('',#12302,.T.);
#6484=FACE_OUTER_BOUND('',#12303,.T.);
#6485=FACE_OUTER_BOUND('',#12304,.T.);
#6486=FACE_OUTER_BOUND('',#12305,.T.);
#6487=FACE_OUTER_BOUND('',#12306,.T.);
#6488=FACE_OUTER_BOUND('',#12307,.T.);
#6489=FACE_OUTER_BOUND('',#12308,.T.);
#6490=FACE_OUTER_BOUND('',#12309,.T.);
#6491=FACE_OUTER_BOUND('',#12310,.T.);
#6492=FACE_OUTER_BOUND('',#12311,.T.);
#6493=FACE_OUTER_BOUND('',#12312,.T.);
#6494=FACE_OUTER_BOUND('',#12313,.T.);
#6495=FACE_OUTER_BOUND('',#12314,.T.);
#6496=FACE_OUTER_BOUND('',#12315,.T.);
#6497=FACE_OUTER_BOUND('',#12316,.T.);
#6498=FACE_OUTER_BOUND('',#12317,.T.);
#6499=FACE_OUTER_BOUND('',#12318,.T.);
#6500=FACE_OUTER_BOUND('',#12319,.T.);
#6501=FACE_OUTER_BOUND('',#12320,.T.);
#6502=FACE_OUTER_BOUND('',#12321,.T.);
#6503=FACE_OUTER_BOUND('',#12322,.T.);
#6504=FACE_OUTER_BOUND('',#12323,.T.);
#6505=FACE_OUTER_BOUND('',#12324,.T.);
#6506=FACE_OUTER_BOUND('',#12325,.T.);
#6507=FACE_OUTER_BOUND('',#12326,.T.);
#6508=FACE_OUTER_BOUND('',#12327,.T.);
#6509=FACE_OUTER_BOUND('',#12328,.T.);
#6510=FACE_OUTER_BOUND('',#12329,.T.);
#6511=FACE_OUTER_BOUND('',#12330,.T.);
#6512=FACE_OUTER_BOUND('',#12331,.T.);
#6513=FACE_OUTER_BOUND('',#12332,.T.);
#6514=FACE_OUTER_BOUND('',#12333,.T.);
#6515=FACE_OUTER_BOUND('',#12334,.T.);
#6516=FACE_OUTER_BOUND('',#12335,.T.);
#6517=FACE_OUTER_BOUND('',#12336,.T.);
#6518=FACE_OUTER_BOUND('',#12337,.T.);
#6519=FACE_OUTER_BOUND('',#12338,.T.);
#6520=FACE_OUTER_BOUND('',#12339,.T.);
#6521=FACE_OUTER_BOUND('',#12340,.T.);
#6522=FACE_OUTER_BOUND('',#12341,.T.);
#6523=FACE_OUTER_BOUND('',#12342,.T.);
#6524=FACE_OUTER_BOUND('',#12343,.T.);
#6525=FACE_OUTER_BOUND('',#12344,.T.);
#6526=FACE_OUTER_BOUND('',#12345,.T.);
#6527=FACE_OUTER_BOUND('',#12346,.T.);
#6528=FACE_OUTER_BOUND('',#12347,.T.);
#6529=FACE_OUTER_BOUND('',#12348,.T.);
#6530=FACE_OUTER_BOUND('',#12349,.T.);
#6531=FACE_OUTER_BOUND('',#12350,.T.);
#6532=FACE_OUTER_BOUND('',#12351,.T.);
#6533=FACE_OUTER_BOUND('',#12352,.T.);
#6534=FACE_OUTER_BOUND('',#12353,.T.);
#6535=FACE_OUTER_BOUND('',#12354,.T.);
#6536=FACE_OUTER_BOUND('',#12355,.T.);
#6537=FACE_OUTER_BOUND('',#12356,.T.);
#6538=FACE_OUTER_BOUND('',#12357,.T.);
#6539=FACE_OUTER_BOUND('',#12358,.T.);
#6540=FACE_OUTER_BOUND('',#12359,.T.);
#6541=FACE_OUTER_BOUND('',#12360,.T.);
#6542=FACE_OUTER_BOUND('',#12361,.T.);
#6543=FACE_OUTER_BOUND('',#12362,.T.);
#6544=FACE_OUTER_BOUND('',#12363,.T.);
#6545=FACE_OUTER_BOUND('',#12364,.T.);
#6546=FACE_OUTER_BOUND('',#12365,.T.);
#6547=FACE_OUTER_BOUND('',#12366,.T.);
#6548=FACE_OUTER_BOUND('',#12367,.T.);
#6549=FACE_OUTER_BOUND('',#12368,.T.);
#6550=FACE_OUTER_BOUND('',#12369,.T.);
#6551=FACE_OUTER_BOUND('',#12370,.T.);
#6552=FACE_OUTER_BOUND('',#12371,.T.);
#6553=FACE_OUTER_BOUND('',#12372,.T.);
#6554=FACE_OUTER_BOUND('',#12373,.T.);
#6555=FACE_OUTER_BOUND('',#12375,.T.);
#6556=FACE_OUTER_BOUND('',#12376,.T.);
#6557=FACE_OUTER_BOUND('',#12378,.T.);
#6558=FACE_OUTER_BOUND('',#12379,.T.);
#6559=FACE_OUTER_BOUND('',#12380,.T.);
#6560=FACE_OUTER_BOUND('',#12381,.T.);
#6561=FACE_OUTER_BOUND('',#12382,.T.);
#6562=FACE_OUTER_BOUND('',#12383,.T.);
#6563=FACE_OUTER_BOUND('',#12384,.T.);
#6564=FACE_OUTER_BOUND('',#12385,.T.);
#6565=FACE_OUTER_BOUND('',#12386,.T.);
#6566=FACE_OUTER_BOUND('',#12387,.T.);
#6567=FACE_OUTER_BOUND('',#12388,.T.);
#6568=FACE_OUTER_BOUND('',#12389,.T.);
#6569=FACE_OUTER_BOUND('',#12390,.T.);
#6570=FACE_OUTER_BOUND('',#12391,.T.);
#6571=FACE_OUTER_BOUND('',#12392,.T.);
#6572=FACE_OUTER_BOUND('',#12393,.T.);
#6573=FACE_OUTER_BOUND('',#12394,.T.);
#6574=FACE_OUTER_BOUND('',#12395,.T.);
#6575=FACE_OUTER_BOUND('',#12396,.T.);
#6576=FACE_OUTER_BOUND('',#12397,.T.);
#6577=FACE_OUTER_BOUND('',#12398,.T.);
#6578=FACE_OUTER_BOUND('',#12399,.T.);
#6579=FACE_OUTER_BOUND('',#12400,.T.);
#6580=FACE_OUTER_BOUND('',#12401,.T.);
#6581=FACE_OUTER_BOUND('',#12402,.T.);
#6582=FACE_OUTER_BOUND('',#12403,.T.);
#6583=FACE_OUTER_BOUND('',#12404,.T.);
#6584=FACE_OUTER_BOUND('',#12405,.T.);
#6585=FACE_OUTER_BOUND('',#12406,.T.);
#6586=FACE_OUTER_BOUND('',#12407,.T.);
#6587=FACE_OUTER_BOUND('',#12408,.T.);
#6588=FACE_OUTER_BOUND('',#12409,.T.);
#6589=FACE_OUTER_BOUND('',#12410,.T.);
#6590=FACE_OUTER_BOUND('',#12411,.T.);
#6591=FACE_OUTER_BOUND('',#12412,.T.);
#6592=FACE_OUTER_BOUND('',#12413,.T.);
#6593=FACE_OUTER_BOUND('',#12414,.T.);
#6594=FACE_OUTER_BOUND('',#12415,.T.);
#6595=FACE_OUTER_BOUND('',#12416,.T.);
#6596=FACE_OUTER_BOUND('',#12417,.T.);
#6597=FACE_OUTER_BOUND('',#12418,.T.);
#6598=FACE_OUTER_BOUND('',#12419,.T.);
#6599=FACE_OUTER_BOUND('',#12420,.T.);
#6600=FACE_OUTER_BOUND('',#12421,.T.);
#6601=FACE_OUTER_BOUND('',#12422,.T.);
#6602=FACE_OUTER_BOUND('',#12423,.T.);
#6603=FACE_OUTER_BOUND('',#12424,.T.);
#6604=FACE_OUTER_BOUND('',#12425,.T.);
#6605=FACE_OUTER_BOUND('',#12426,.T.);
#6606=FACE_OUTER_BOUND('',#12427,.T.);
#6607=FACE_OUTER_BOUND('',#12428,.T.);
#6608=FACE_OUTER_BOUND('',#12429,.T.);
#6609=FACE_OUTER_BOUND('',#12430,.T.);
#6610=FACE_OUTER_BOUND('',#12431,.T.);
#6611=FACE_OUTER_BOUND('',#12432,.T.);
#6612=FACE_OUTER_BOUND('',#12433,.T.);
#6613=FACE_OUTER_BOUND('',#12434,.T.);
#6614=FACE_OUTER_BOUND('',#12435,.T.);
#6615=FACE_OUTER_BOUND('',#12436,.T.);
#6616=FACE_OUTER_BOUND('',#12437,.T.);
#6617=FACE_OUTER_BOUND('',#12438,.T.);
#6618=FACE_OUTER_BOUND('',#12439,.T.);
#6619=FACE_OUTER_BOUND('',#12440,.T.);
#6620=FACE_OUTER_BOUND('',#12441,.T.);
#6621=FACE_OUTER_BOUND('',#12442,.T.);
#6622=FACE_OUTER_BOUND('',#12443,.T.);
#6623=FACE_OUTER_BOUND('',#12444,.T.);
#6624=FACE_OUTER_BOUND('',#12445,.T.);
#6625=FACE_OUTER_BOUND('',#12446,.T.);
#6626=FACE_OUTER_BOUND('',#12447,.T.);
#6627=FACE_OUTER_BOUND('',#12448,.T.);
#6628=FACE_OUTER_BOUND('',#12449,.T.);
#6629=FACE_OUTER_BOUND('',#12450,.T.);
#6630=FACE_OUTER_BOUND('',#12451,.T.);
#6631=FACE_OUTER_BOUND('',#12452,.T.);
#6632=FACE_OUTER_BOUND('',#12453,.T.);
#6633=FACE_OUTER_BOUND('',#12454,.T.);
#6634=FACE_OUTER_BOUND('',#12455,.T.);
#6635=FACE_OUTER_BOUND('',#12456,.T.);
#6636=FACE_OUTER_BOUND('',#12457,.T.);
#6637=FACE_OUTER_BOUND('',#12458,.T.);
#6638=FACE_OUTER_BOUND('',#12459,.T.);
#6639=FACE_OUTER_BOUND('',#12460,.T.);
#6640=FACE_OUTER_BOUND('',#12461,.T.);
#6641=FACE_OUTER_BOUND('',#12462,.T.);
#6642=FACE_OUTER_BOUND('',#12463,.T.);
#6643=FACE_OUTER_BOUND('',#12464,.T.);
#6644=FACE_OUTER_BOUND('',#12465,.T.);
#6645=FACE_OUTER_BOUND('',#12466,.T.);
#6646=FACE_OUTER_BOUND('',#12467,.T.);
#6647=FACE_OUTER_BOUND('',#12468,.T.);
#6648=FACE_OUTER_BOUND('',#12469,.T.);
#6649=FACE_OUTER_BOUND('',#12470,.T.);
#6650=FACE_OUTER_BOUND('',#12471,.T.);
#6651=FACE_OUTER_BOUND('',#12472,.T.);
#6652=FACE_OUTER_BOUND('',#12473,.T.);
#6653=FACE_OUTER_BOUND('',#12474,.T.);
#6654=FACE_OUTER_BOUND('',#12475,.T.);
#6655=FACE_OUTER_BOUND('',#12476,.T.);
#6656=FACE_OUTER_BOUND('',#12477,.T.);
#6657=FACE_OUTER_BOUND('',#12478,.T.);
#6658=FACE_OUTER_BOUND('',#12479,.T.);
#6659=FACE_OUTER_BOUND('',#12480,.T.);
#6660=FACE_OUTER_BOUND('',#12481,.T.);
#6661=FACE_OUTER_BOUND('',#12482,.T.);
#6662=FACE_OUTER_BOUND('',#12483,.T.);
#6663=FACE_OUTER_BOUND('',#12484,.T.);
#6664=FACE_OUTER_BOUND('',#12485,.T.);
#6665=FACE_OUTER_BOUND('',#12486,.T.);
#6666=FACE_OUTER_BOUND('',#12487,.T.);
#6667=FACE_OUTER_BOUND('',#12488,.T.);
#6668=FACE_OUTER_BOUND('',#12489,.T.);
#6669=FACE_OUTER_BOUND('',#12490,.T.);
#6670=FACE_OUTER_BOUND('',#12491,.T.);
#6671=FACE_OUTER_BOUND('',#12492,.T.);
#6672=FACE_OUTER_BOUND('',#12493,.T.);
#6673=FACE_OUTER_BOUND('',#12494,.T.);
#6674=FACE_OUTER_BOUND('',#12495,.T.);
#6675=FACE_OUTER_BOUND('',#12496,.T.);
#6676=FACE_OUTER_BOUND('',#12497,.T.);
#6677=FACE_OUTER_BOUND('',#12498,.T.);
#6678=FACE_OUTER_BOUND('',#12499,.T.);
#6679=FACE_OUTER_BOUND('',#12500,.T.);
#6680=FACE_OUTER_BOUND('',#12501,.T.);
#6681=FACE_OUTER_BOUND('',#12502,.T.);
#6682=FACE_OUTER_BOUND('',#12503,.T.);
#6683=FACE_OUTER_BOUND('',#12504,.T.);
#6684=FACE_OUTER_BOUND('',#12505,.T.);
#6685=FACE_OUTER_BOUND('',#12506,.T.);
#6686=FACE_OUTER_BOUND('',#12507,.T.);
#6687=FACE_OUTER_BOUND('',#12508,.T.);
#6688=FACE_OUTER_BOUND('',#12509,.T.);
#6689=FACE_OUTER_BOUND('',#12510,.T.);
#6690=FACE_OUTER_BOUND('',#12511,.T.);
#6691=FACE_OUTER_BOUND('',#12512,.T.);
#6692=FACE_OUTER_BOUND('',#12513,.T.);
#6693=FACE_OUTER_BOUND('',#12514,.T.);
#6694=FACE_OUTER_BOUND('',#12515,.T.);
#6695=FACE_OUTER_BOUND('',#12516,.T.);
#6696=FACE_OUTER_BOUND('',#12517,.T.);
#6697=FACE_OUTER_BOUND('',#12518,.T.);
#6698=FACE_OUTER_BOUND('',#12519,.T.);
#6699=FACE_OUTER_BOUND('',#12520,.T.);
#6700=FACE_OUTER_BOUND('',#12521,.T.);
#6701=FACE_OUTER_BOUND('',#12522,.T.);
#6702=FACE_OUTER_BOUND('',#12523,.T.);
#6703=FACE_OUTER_BOUND('',#12524,.T.);
#6704=FACE_OUTER_BOUND('',#12525,.T.);
#6705=FACE_OUTER_BOUND('',#12526,.T.);
#6706=FACE_OUTER_BOUND('',#12527,.T.);
#6707=FACE_OUTER_BOUND('',#12528,.T.);
#6708=FACE_OUTER_BOUND('',#12529,.T.);
#6709=FACE_OUTER_BOUND('',#12530,.T.);
#6710=FACE_OUTER_BOUND('',#12531,.T.);
#6711=FACE_OUTER_BOUND('',#12532,.T.);
#6712=FACE_OUTER_BOUND('',#12533,.T.);
#6713=FACE_OUTER_BOUND('',#12534,.T.);
#6714=FACE_OUTER_BOUND('',#12535,.T.);
#6715=FACE_OUTER_BOUND('',#12536,.T.);
#6716=FACE_OUTER_BOUND('',#12537,.T.);
#6717=FACE_OUTER_BOUND('',#12538,.T.);
#6718=FACE_OUTER_BOUND('',#12539,.T.);
#6719=FACE_OUTER_BOUND('',#12540,.T.);
#6720=FACE_OUTER_BOUND('',#12541,.T.);
#6721=FACE_OUTER_BOUND('',#12542,.T.);
#6722=FACE_OUTER_BOUND('',#12543,.T.);
#6723=FACE_OUTER_BOUND('',#12544,.T.);
#6724=FACE_OUTER_BOUND('',#12545,.T.);
#6725=FACE_OUTER_BOUND('',#12546,.T.);
#6726=FACE_OUTER_BOUND('',#12547,.T.);
#6727=FACE_OUTER_BOUND('',#12548,.T.);
#6728=FACE_OUTER_BOUND('',#12549,.T.);
#6729=FACE_OUTER_BOUND('',#12550,.T.);
#6730=FACE_OUTER_BOUND('',#12551,.T.);
#6731=FACE_OUTER_BOUND('',#12552,.T.);
#6732=FACE_OUTER_BOUND('',#12553,.T.);
#6733=FACE_OUTER_BOUND('',#12554,.T.);
#6734=FACE_OUTER_BOUND('',#12555,.T.);
#6735=FACE_OUTER_BOUND('',#12556,.T.);
#6736=FACE_OUTER_BOUND('',#12557,.T.);
#6737=FACE_OUTER_BOUND('',#12558,.T.);
#6738=FACE_OUTER_BOUND('',#12559,.T.);
#6739=FACE_OUTER_BOUND('',#12560,.T.);
#6740=FACE_OUTER_BOUND('',#12561,.T.);
#6741=FACE_OUTER_BOUND('',#12562,.T.);
#6742=FACE_OUTER_BOUND('',#12563,.T.);
#6743=FACE_OUTER_BOUND('',#12564,.T.);
#6744=FACE_OUTER_BOUND('',#12565,.T.);
#6745=FACE_OUTER_BOUND('',#12566,.T.);
#6746=FACE_OUTER_BOUND('',#12567,.T.);
#6747=FACE_OUTER_BOUND('',#12568,.T.);
#6748=FACE_OUTER_BOUND('',#12569,.T.);
#6749=FACE_OUTER_BOUND('',#12570,.T.);
#6750=FACE_OUTER_BOUND('',#12571,.T.);
#6751=FACE_OUTER_BOUND('',#12572,.T.);
#6752=FACE_OUTER_BOUND('',#12573,.T.);
#6753=FACE_OUTER_BOUND('',#12574,.T.);
#6754=FACE_OUTER_BOUND('',#12575,.T.);
#6755=FACE_OUTER_BOUND('',#12576,.T.);
#6756=FACE_OUTER_BOUND('',#12577,.T.);
#6757=FACE_OUTER_BOUND('',#12578,.T.);
#6758=FACE_OUTER_BOUND('',#12579,.T.);
#6759=FACE_OUTER_BOUND('',#12580,.T.);
#6760=FACE_OUTER_BOUND('',#12582,.T.);
#6761=FACE_OUTER_BOUND('',#12583,.T.);
#6762=FACE_OUTER_BOUND('',#12586,.T.);
#6763=FACE_OUTER_BOUND('',#12587,.T.);
#6764=FACE_OUTER_BOUND('',#12588,.T.);
#6765=FACE_OUTER_BOUND('',#12589,.T.);
#6766=FACE_OUTER_BOUND('',#12595,.T.);
#6767=FACE_OUTER_BOUND('',#12596,.T.);
#6768=FACE_OUTER_BOUND('',#12597,.T.);
#6769=FACE_OUTER_BOUND('',#12598,.T.);
#6770=FACE_OUTER_BOUND('',#12599,.T.);
#6771=FACE_OUTER_BOUND('',#12600,.T.);
#6772=FACE_OUTER_BOUND('',#12601,.T.);
#6773=FACE_OUTER_BOUND('',#12602,.T.);
#6774=FACE_OUTER_BOUND('',#12603,.T.);
#6775=FACE_OUTER_BOUND('',#12604,.T.);
#6776=FACE_OUTER_BOUND('',#12606,.T.);
#6777=FACE_OUTER_BOUND('',#12607,.T.);
#6778=FACE_OUTER_BOUND('',#12608,.T.);
#6779=FACE_OUTER_BOUND('',#12609,.T.);
#6780=FACE_OUTER_BOUND('',#12610,.T.);
#6781=FACE_OUTER_BOUND('',#12611,.T.);
#6782=FACE_OUTER_BOUND('',#12612,.T.);
#6783=FACE_OUTER_BOUND('',#12613,.T.);
#6784=FACE_OUTER_BOUND('',#12614,.T.);
#6785=FACE_OUTER_BOUND('',#12615,.T.);
#6786=FACE_OUTER_BOUND('',#12616,.T.);
#6787=FACE_OUTER_BOUND('',#12617,.T.);
#6788=FACE_OUTER_BOUND('',#12618,.T.);
#6789=FACE_OUTER_BOUND('',#12619,.T.);
#6790=FACE_OUTER_BOUND('',#12620,.T.);
#6791=FACE_OUTER_BOUND('',#12621,.T.);
#6792=FACE_OUTER_BOUND('',#12622,.T.);
#6793=FACE_OUTER_BOUND('',#12623,.T.);
#6794=FACE_OUTER_BOUND('',#12624,.T.);
#6795=FACE_OUTER_BOUND('',#12625,.T.);
#6796=FACE_OUTER_BOUND('',#12626,.T.);
#6797=FACE_OUTER_BOUND('',#12627,.T.);
#6798=FACE_OUTER_BOUND('',#12628,.T.);
#6799=FACE_OUTER_BOUND('',#12629,.T.);
#6800=FACE_OUTER_BOUND('',#12630,.T.);
#6801=FACE_OUTER_BOUND('',#12631,.T.);
#6802=FACE_OUTER_BOUND('',#12632,.T.);
#6803=FACE_OUTER_BOUND('',#12633,.T.);
#6804=FACE_OUTER_BOUND('',#12634,.T.);
#6805=FACE_OUTER_BOUND('',#12635,.T.);
#6806=FACE_OUTER_BOUND('',#12636,.T.);
#6807=FACE_OUTER_BOUND('',#12637,.T.);
#6808=FACE_OUTER_BOUND('',#12638,.T.);
#6809=FACE_OUTER_BOUND('',#12639,.T.);
#6810=FACE_OUTER_BOUND('',#12640,.T.);
#6811=FACE_OUTER_BOUND('',#12641,.T.);
#6812=FACE_OUTER_BOUND('',#12642,.T.);
#6813=FACE_OUTER_BOUND('',#12643,.T.);
#6814=FACE_OUTER_BOUND('',#12644,.T.);
#6815=FACE_OUTER_BOUND('',#12645,.T.);
#6816=FACE_OUTER_BOUND('',#12646,.T.);
#6817=FACE_OUTER_BOUND('',#12647,.T.);
#6818=FACE_OUTER_BOUND('',#12649,.T.);
#6819=FACE_OUTER_BOUND('',#12650,.T.);
#6820=FACE_OUTER_BOUND('',#12651,.T.);
#6821=FACE_OUTER_BOUND('',#12652,.T.);
#6822=FACE_OUTER_BOUND('',#12653,.T.);
#6823=FACE_OUTER_BOUND('',#12654,.T.);
#6824=FACE_OUTER_BOUND('',#12655,.T.);
#6825=FACE_OUTER_BOUND('',#12656,.T.);
#6826=FACE_OUTER_BOUND('',#12657,.T.);
#6827=FACE_OUTER_BOUND('',#12658,.T.);
#6828=FACE_OUTER_BOUND('',#12659,.T.);
#6829=FACE_OUTER_BOUND('',#12660,.T.);
#6830=FACE_OUTER_BOUND('',#12661,.T.);
#6831=FACE_OUTER_BOUND('',#12662,.T.);
#6832=FACE_OUTER_BOUND('',#12663,.T.);
#6833=FACE_OUTER_BOUND('',#12664,.T.);
#6834=FACE_OUTER_BOUND('',#12665,.T.);
#6835=FACE_OUTER_BOUND('',#12666,.T.);
#6836=FACE_OUTER_BOUND('',#12667,.T.);
#6837=FACE_OUTER_BOUND('',#12668,.T.);
#6838=FACE_OUTER_BOUND('',#12669,.T.);
#6839=FACE_OUTER_BOUND('',#12670,.T.);
#6840=FACE_OUTER_BOUND('',#12671,.T.);
#6841=FACE_OUTER_BOUND('',#12672,.T.);
#6842=FACE_OUTER_BOUND('',#12673,.T.);
#6843=FACE_OUTER_BOUND('',#12674,.T.);
#6844=FACE_OUTER_BOUND('',#12675,.T.);
#6845=FACE_OUTER_BOUND('',#12678,.T.);
#6846=FACE_OUTER_BOUND('',#12679,.T.);
#6847=FACE_OUTER_BOUND('',#12680,.T.);
#6848=FACE_OUTER_BOUND('',#12681,.T.);
#6849=FACE_OUTER_BOUND('',#12682,.T.);
#6850=FACE_OUTER_BOUND('',#12683,.T.);
#6851=FACE_OUTER_BOUND('',#12684,.T.);
#6852=FACE_OUTER_BOUND('',#12685,.T.);
#6853=FACE_OUTER_BOUND('',#12686,.T.);
#6854=FACE_OUTER_BOUND('',#12687,.T.);
#6855=FACE_OUTER_BOUND('',#12688,.T.);
#6856=FACE_OUTER_BOUND('',#12690,.T.);
#6857=FACE_OUTER_BOUND('',#12691,.T.);
#6858=FACE_OUTER_BOUND('',#12692,.T.);
#6859=FACE_OUTER_BOUND('',#12693,.T.);
#6860=FACE_OUTER_BOUND('',#12694,.T.);
#6861=FACE_OUTER_BOUND('',#12695,.T.);
#6862=FACE_OUTER_BOUND('',#12696,.T.);
#6863=FACE_OUTER_BOUND('',#12697,.T.);
#6864=FACE_OUTER_BOUND('',#12698,.T.);
#6865=FACE_OUTER_BOUND('',#12699,.T.);
#6866=FACE_OUTER_BOUND('',#12700,.T.);
#6867=FACE_OUTER_BOUND('',#12701,.T.);
#6868=FACE_OUTER_BOUND('',#12702,.T.);
#6869=FACE_OUTER_BOUND('',#12703,.T.);
#6870=FACE_OUTER_BOUND('',#12704,.T.);
#6871=FACE_OUTER_BOUND('',#12705,.T.);
#6872=FACE_OUTER_BOUND('',#12706,.T.);
#6873=FACE_OUTER_BOUND('',#12707,.T.);
#6874=FACE_OUTER_BOUND('',#12709,.T.);
#6875=FACE_OUTER_BOUND('',#12710,.T.);
#6876=FACE_OUTER_BOUND('',#12711,.T.);
#6877=FACE_OUTER_BOUND('',#12712,.T.);
#6878=FACE_OUTER_BOUND('',#12713,.T.);
#6879=FACE_OUTER_BOUND('',#12714,.T.);
#6880=FACE_OUTER_BOUND('',#12715,.T.);
#6881=FACE_OUTER_BOUND('',#12716,.T.);
#6882=FACE_OUTER_BOUND('',#12717,.T.);
#6883=FACE_OUTER_BOUND('',#12718,.T.);
#6884=FACE_OUTER_BOUND('',#12719,.T.);
#6885=FACE_OUTER_BOUND('',#12720,.T.);
#6886=FACE_OUTER_BOUND('',#12721,.T.);
#6887=FACE_OUTER_BOUND('',#12722,.T.);
#6888=FACE_OUTER_BOUND('',#12723,.T.);
#6889=FACE_OUTER_BOUND('',#12724,.T.);
#6890=FACE_OUTER_BOUND('',#12725,.T.);
#6891=FACE_OUTER_BOUND('',#12726,.T.);
#6892=FACE_OUTER_BOUND('',#12727,.T.);
#6893=FACE_OUTER_BOUND('',#12728,.T.);
#6894=FACE_OUTER_BOUND('',#12729,.T.);
#6895=FACE_OUTER_BOUND('',#12730,.T.);
#6896=FACE_OUTER_BOUND('',#12731,.T.);
#6897=FACE_OUTER_BOUND('',#12732,.T.);
#6898=FACE_OUTER_BOUND('',#12733,.T.);
#6899=FACE_OUTER_BOUND('',#12734,.T.);
#6900=FACE_OUTER_BOUND('',#12735,.T.);
#6901=FACE_OUTER_BOUND('',#12736,.T.);
#6902=FACE_OUTER_BOUND('',#12737,.T.);
#6903=FACE_OUTER_BOUND('',#12738,.T.);
#6904=FACE_OUTER_BOUND('',#12739,.T.);
#6905=FACE_OUTER_BOUND('',#12740,.T.);
#6906=FACE_OUTER_BOUND('',#12741,.T.);
#6907=FACE_OUTER_BOUND('',#12742,.T.);
#6908=FACE_OUTER_BOUND('',#12743,.T.);
#6909=FACE_OUTER_BOUND('',#12744,.T.);
#6910=FACE_OUTER_BOUND('',#12745,.T.);
#6911=FACE_OUTER_BOUND('',#12746,.T.);
#6912=FACE_OUTER_BOUND('',#12747,.T.);
#6913=FACE_OUTER_BOUND('',#12748,.T.);
#6914=FACE_OUTER_BOUND('',#12749,.T.);
#6915=FACE_OUTER_BOUND('',#12750,.T.);
#6916=FACE_OUTER_BOUND('',#12751,.T.);
#6917=FACE_OUTER_BOUND('',#12752,.T.);
#6918=FACE_OUTER_BOUND('',#12753,.T.);
#6919=FACE_OUTER_BOUND('',#12754,.T.);
#6920=FACE_OUTER_BOUND('',#12755,.T.);
#6921=FACE_OUTER_BOUND('',#12756,.T.);
#6922=FACE_OUTER_BOUND('',#12757,.T.);
#6923=FACE_OUTER_BOUND('',#12758,.T.);
#6924=FACE_OUTER_BOUND('',#12759,.T.);
#6925=FACE_OUTER_BOUND('',#12760,.T.);
#6926=FACE_OUTER_BOUND('',#12761,.T.);
#6927=FACE_OUTER_BOUND('',#12762,.T.);
#6928=FACE_OUTER_BOUND('',#12763,.T.);
#6929=FACE_OUTER_BOUND('',#12764,.T.);
#6930=FACE_OUTER_BOUND('',#12765,.T.);
#6931=FACE_OUTER_BOUND('',#12766,.T.);
#6932=FACE_OUTER_BOUND('',#12767,.T.);
#6933=FACE_OUTER_BOUND('',#12769,.T.);
#6934=FACE_OUTER_BOUND('',#12770,.T.);
#6935=FACE_OUTER_BOUND('',#12771,.T.);
#6936=FACE_OUTER_BOUND('',#12772,.T.);
#6937=FACE_OUTER_BOUND('',#12773,.T.);
#6938=FACE_OUTER_BOUND('',#12774,.T.);
#6939=FACE_OUTER_BOUND('',#12775,.T.);
#6940=FACE_OUTER_BOUND('',#12776,.T.);
#6941=FACE_OUTER_BOUND('',#12777,.T.);
#6942=FACE_OUTER_BOUND('',#12778,.T.);
#6943=FACE_OUTER_BOUND('',#12779,.T.);
#6944=FACE_OUTER_BOUND('',#12780,.T.);
#6945=FACE_OUTER_BOUND('',#12781,.T.);
#6946=FACE_OUTER_BOUND('',#12782,.T.);
#6947=FACE_OUTER_BOUND('',#12783,.T.);
#6948=FACE_OUTER_BOUND('',#12784,.T.);
#6949=FACE_OUTER_BOUND('',#12785,.T.);
#6950=FACE_OUTER_BOUND('',#12786,.T.);
#6951=FACE_OUTER_BOUND('',#12787,.T.);
#6952=FACE_OUTER_BOUND('',#12788,.T.);
#6953=FACE_OUTER_BOUND('',#12789,.T.);
#6954=FACE_OUTER_BOUND('',#12790,.T.);
#6955=FACE_OUTER_BOUND('',#12791,.T.);
#6956=FACE_OUTER_BOUND('',#12792,.T.);
#6957=FACE_OUTER_BOUND('',#12793,.T.);
#6958=FACE_OUTER_BOUND('',#12794,.T.);
#6959=FACE_OUTER_BOUND('',#12795,.T.);
#6960=FACE_OUTER_BOUND('',#12796,.T.);
#6961=FACE_OUTER_BOUND('',#12797,.T.);
#6962=FACE_OUTER_BOUND('',#12798,.T.);
#6963=FACE_OUTER_BOUND('',#12799,.T.);
#6964=FACE_OUTER_BOUND('',#12800,.T.);
#6965=FACE_OUTER_BOUND('',#12801,.T.);
#6966=FACE_OUTER_BOUND('',#12802,.T.);
#6967=FACE_OUTER_BOUND('',#12803,.T.);
#6968=FACE_OUTER_BOUND('',#12804,.T.);
#6969=FACE_OUTER_BOUND('',#12805,.T.);
#6970=FACE_OUTER_BOUND('',#12806,.T.);
#6971=FACE_OUTER_BOUND('',#12807,.T.);
#6972=FACE_OUTER_BOUND('',#12808,.T.);
#6973=FACE_OUTER_BOUND('',#12809,.T.);
#6974=FACE_OUTER_BOUND('',#12810,.T.);
#6975=FACE_OUTER_BOUND('',#12811,.T.);
#6976=FACE_OUTER_BOUND('',#12812,.T.);
#6977=FACE_OUTER_BOUND('',#12813,.T.);
#6978=FACE_OUTER_BOUND('',#12814,.T.);
#6979=FACE_OUTER_BOUND('',#12815,.T.);
#6980=FACE_OUTER_BOUND('',#12816,.T.);
#6981=FACE_OUTER_BOUND('',#12817,.T.);
#6982=FACE_OUTER_BOUND('',#12818,.T.);
#6983=FACE_OUTER_BOUND('',#12819,.T.);
#6984=FACE_OUTER_BOUND('',#12820,.T.);
#6985=FACE_OUTER_BOUND('',#12821,.T.);
#6986=FACE_OUTER_BOUND('',#12822,.T.);
#6987=FACE_OUTER_BOUND('',#12823,.T.);
#6988=FACE_OUTER_BOUND('',#12824,.T.);
#6989=FACE_OUTER_BOUND('',#12825,.T.);
#6990=FACE_OUTER_BOUND('',#12826,.T.);
#6991=FACE_OUTER_BOUND('',#12827,.T.);
#6992=FACE_OUTER_BOUND('',#12828,.T.);
#6993=FACE_OUTER_BOUND('',#12829,.T.);
#6994=FACE_OUTER_BOUND('',#12830,.T.);
#6995=FACE_OUTER_BOUND('',#12831,.T.);
#6996=FACE_OUTER_BOUND('',#12832,.T.);
#6997=FACE_OUTER_BOUND('',#12833,.T.);
#6998=FACE_OUTER_BOUND('',#12834,.T.);
#6999=FACE_OUTER_BOUND('',#12835,.T.);
#7000=FACE_OUTER_BOUND('',#12836,.T.);
#7001=FACE_OUTER_BOUND('',#12837,.T.);
#7002=FACE_OUTER_BOUND('',#12838,.T.);
#7003=FACE_OUTER_BOUND('',#12839,.T.);
#7004=FACE_OUTER_BOUND('',#12840,.T.);
#7005=FACE_OUTER_BOUND('',#12841,.T.);
#7006=FACE_OUTER_BOUND('',#12842,.T.);
#7007=FACE_OUTER_BOUND('',#12843,.T.);
#7008=FACE_OUTER_BOUND('',#12844,.T.);
#7009=FACE_OUTER_BOUND('',#12845,.T.);
#7010=FACE_OUTER_BOUND('',#12846,.T.);
#7011=FACE_OUTER_BOUND('',#12847,.T.);
#7012=FACE_OUTER_BOUND('',#12848,.T.);
#7013=FACE_OUTER_BOUND('',#12849,.T.);
#7014=FACE_OUTER_BOUND('',#12850,.T.);
#7015=FACE_OUTER_BOUND('',#12851,.T.);
#7016=FACE_OUTER_BOUND('',#12852,.T.);
#7017=FACE_OUTER_BOUND('',#12853,.T.);
#7018=FACE_OUTER_BOUND('',#12854,.T.);
#7019=FACE_OUTER_BOUND('',#12855,.T.);
#7020=FACE_OUTER_BOUND('',#12856,.T.);
#7021=FACE_OUTER_BOUND('',#12857,.T.);
#7022=FACE_OUTER_BOUND('',#12858,.T.);
#7023=FACE_OUTER_BOUND('',#12859,.T.);
#7024=FACE_OUTER_BOUND('',#12860,.T.);
#7025=FACE_OUTER_BOUND('',#12861,.T.);
#7026=FACE_OUTER_BOUND('',#12862,.T.);
#7027=FACE_OUTER_BOUND('',#12863,.T.);
#7028=FACE_OUTER_BOUND('',#12864,.T.);
#7029=FACE_OUTER_BOUND('',#12865,.T.);
#7030=FACE_OUTER_BOUND('',#12866,.T.);
#7031=FACE_OUTER_BOUND('',#12867,.T.);
#7032=FACE_OUTER_BOUND('',#12868,.T.);
#7033=FACE_OUTER_BOUND('',#12869,.T.);
#7034=FACE_OUTER_BOUND('',#12870,.T.);
#7035=FACE_OUTER_BOUND('',#12871,.T.);
#7036=FACE_OUTER_BOUND('',#12872,.T.);
#7037=FACE_OUTER_BOUND('',#12873,.T.);
#7038=FACE_OUTER_BOUND('',#12874,.T.);
#7039=FACE_OUTER_BOUND('',#12875,.T.);
#7040=FACE_OUTER_BOUND('',#12876,.T.);
#7041=FACE_OUTER_BOUND('',#12877,.T.);
#7042=FACE_OUTER_BOUND('',#12878,.T.);
#7043=FACE_OUTER_BOUND('',#12879,.T.);
#7044=FACE_OUTER_BOUND('',#12880,.T.);
#7045=FACE_OUTER_BOUND('',#12881,.T.);
#7046=FACE_OUTER_BOUND('',#12882,.T.);
#7047=FACE_OUTER_BOUND('',#12883,.T.);
#7048=FACE_OUTER_BOUND('',#12884,.T.);
#7049=FACE_OUTER_BOUND('',#12885,.T.);
#7050=FACE_OUTER_BOUND('',#12886,.T.);
#7051=FACE_OUTER_BOUND('',#12887,.T.);
#7052=FACE_OUTER_BOUND('',#12888,.T.);
#7053=FACE_OUTER_BOUND('',#12889,.T.);
#7054=FACE_OUTER_BOUND('',#12890,.T.);
#7055=FACE_OUTER_BOUND('',#12891,.T.);
#7056=FACE_OUTER_BOUND('',#12892,.T.);
#7057=FACE_OUTER_BOUND('',#12893,.T.);
#7058=FACE_OUTER_BOUND('',#12894,.T.);
#7059=FACE_OUTER_BOUND('',#12895,.T.);
#7060=FACE_OUTER_BOUND('',#12896,.T.);
#7061=FACE_OUTER_BOUND('',#12897,.T.);
#7062=FACE_OUTER_BOUND('',#12898,.T.);
#7063=FACE_OUTER_BOUND('',#12899,.T.);
#7064=FACE_OUTER_BOUND('',#12900,.T.);
#7065=FACE_OUTER_BOUND('',#12901,.T.);
#7066=FACE_OUTER_BOUND('',#12902,.T.);
#7067=FACE_OUTER_BOUND('',#12903,.T.);
#7068=FACE_OUTER_BOUND('',#12904,.T.);
#7069=FACE_OUTER_BOUND('',#12905,.T.);
#7070=FACE_OUTER_BOUND('',#12906,.T.);
#7071=FACE_OUTER_BOUND('',#12907,.T.);
#7072=FACE_OUTER_BOUND('',#12908,.T.);
#7073=FACE_OUTER_BOUND('',#12909,.T.);
#7074=FACE_OUTER_BOUND('',#12910,.T.);
#7075=FACE_OUTER_BOUND('',#12911,.T.);
#7076=FACE_OUTER_BOUND('',#12912,.T.);
#7077=FACE_OUTER_BOUND('',#12913,.T.);
#7078=FACE_OUTER_BOUND('',#12914,.T.);
#7079=FACE_OUTER_BOUND('',#12915,.T.);
#7080=FACE_OUTER_BOUND('',#12916,.T.);
#7081=FACE_OUTER_BOUND('',#12917,.T.);
#7082=FACE_OUTER_BOUND('',#12918,.T.);
#7083=FACE_OUTER_BOUND('',#12919,.T.);
#7084=FACE_OUTER_BOUND('',#12920,.T.);
#7085=FACE_OUTER_BOUND('',#12921,.T.);
#7086=FACE_OUTER_BOUND('',#12922,.T.);
#7087=FACE_OUTER_BOUND('',#12923,.T.);
#7088=FACE_OUTER_BOUND('',#12924,.T.);
#7089=FACE_OUTER_BOUND('',#12925,.T.);
#7090=FACE_OUTER_BOUND('',#12926,.T.);
#7091=FACE_OUTER_BOUND('',#12927,.T.);
#7092=FACE_OUTER_BOUND('',#12928,.T.);
#7093=FACE_OUTER_BOUND('',#12929,.T.);
#7094=FACE_OUTER_BOUND('',#12930,.T.);
#7095=FACE_OUTER_BOUND('',#12931,.T.);
#7096=FACE_OUTER_BOUND('',#12932,.T.);
#7097=FACE_OUTER_BOUND('',#12933,.T.);
#7098=FACE_OUTER_BOUND('',#12934,.T.);
#7099=FACE_OUTER_BOUND('',#12935,.T.);
#7100=FACE_OUTER_BOUND('',#12936,.T.);
#7101=FACE_OUTER_BOUND('',#12937,.T.);
#7102=FACE_OUTER_BOUND('',#12938,.T.);
#7103=FACE_OUTER_BOUND('',#12939,.T.);
#7104=FACE_OUTER_BOUND('',#12940,.T.);
#7105=FACE_OUTER_BOUND('',#12941,.T.);
#7106=FACE_OUTER_BOUND('',#12942,.T.);
#7107=FACE_OUTER_BOUND('',#12944,.T.);
#7108=FACE_OUTER_BOUND('',#12945,.T.);
#7109=FACE_OUTER_BOUND('',#12946,.T.);
#7110=FACE_OUTER_BOUND('',#12947,.T.);
#7111=FACE_OUTER_BOUND('',#12948,.T.);
#7112=FACE_OUTER_BOUND('',#12949,.T.);
#7113=FACE_OUTER_BOUND('',#12950,.T.);
#7114=FACE_OUTER_BOUND('',#12951,.T.);
#7115=FACE_OUTER_BOUND('',#12952,.T.);
#7116=FACE_OUTER_BOUND('',#12953,.T.);
#7117=FACE_OUTER_BOUND('',#12954,.T.);
#7118=FACE_OUTER_BOUND('',#12955,.T.);
#7119=FACE_OUTER_BOUND('',#12956,.T.);
#7120=FACE_OUTER_BOUND('',#12957,.T.);
#7121=FACE_OUTER_BOUND('',#12958,.T.);
#7122=FACE_OUTER_BOUND('',#12959,.T.);
#7123=FACE_OUTER_BOUND('',#12960,.T.);
#7124=FACE_OUTER_BOUND('',#12961,.T.);
#7125=FACE_OUTER_BOUND('',#12962,.T.);
#7126=FACE_OUTER_BOUND('',#12963,.T.);
#7127=FACE_OUTER_BOUND('',#12964,.T.);
#7128=FACE_OUTER_BOUND('',#12966,.T.);
#7129=FACE_OUTER_BOUND('',#12967,.T.);
#7130=FACE_OUTER_BOUND('',#12968,.T.);
#7131=FACE_OUTER_BOUND('',#12970,.T.);
#7132=FACE_OUTER_BOUND('',#12971,.T.);
#7133=FACE_OUTER_BOUND('',#12972,.T.);
#7134=FACE_OUTER_BOUND('',#12973,.T.);
#7135=FACE_OUTER_BOUND('',#12974,.T.);
#7136=FACE_OUTER_BOUND('',#12975,.T.);
#7137=FACE_OUTER_BOUND('',#12976,.T.);
#7138=FACE_OUTER_BOUND('',#12977,.T.);
#7139=FACE_OUTER_BOUND('',#12978,.T.);
#7140=FACE_OUTER_BOUND('',#12979,.T.);
#7141=FACE_OUTER_BOUND('',#12980,.T.);
#7142=FACE_OUTER_BOUND('',#12981,.T.);
#7143=FACE_OUTER_BOUND('',#12982,.T.);
#7144=FACE_OUTER_BOUND('',#12983,.T.);
#7145=FACE_OUTER_BOUND('',#12984,.T.);
#7146=FACE_OUTER_BOUND('',#12985,.T.);
#7147=FACE_OUTER_BOUND('',#12986,.T.);
#7148=FACE_OUTER_BOUND('',#12987,.T.);
#7149=FACE_OUTER_BOUND('',#12988,.T.);
#7150=FACE_OUTER_BOUND('',#12989,.T.);
#7151=FACE_OUTER_BOUND('',#12990,.T.);
#7152=FACE_OUTER_BOUND('',#12991,.T.);
#7153=FACE_OUTER_BOUND('',#12992,.T.);
#7154=FACE_OUTER_BOUND('',#12993,.T.);
#7155=FACE_OUTER_BOUND('',#12994,.T.);
#7156=FACE_OUTER_BOUND('',#12995,.T.);
#7157=FACE_OUTER_BOUND('',#12996,.T.);
#7158=FACE_OUTER_BOUND('',#12997,.T.);
#7159=FACE_OUTER_BOUND('',#12998,.T.);
#7160=FACE_OUTER_BOUND('',#12999,.T.);
#7161=FACE_OUTER_BOUND('',#13000,.T.);
#7162=FACE_OUTER_BOUND('',#13001,.T.);
#7163=FACE_OUTER_BOUND('',#13003,.T.);
#7164=FACE_OUTER_BOUND('',#13004,.T.);
#7165=FACE_OUTER_BOUND('',#13005,.T.);
#7166=FACE_OUTER_BOUND('',#13006,.T.);
#7167=FACE_OUTER_BOUND('',#13007,.T.);
#7168=FACE_OUTER_BOUND('',#13008,.T.);
#7169=FACE_OUTER_BOUND('',#13009,.T.);
#7170=FACE_OUTER_BOUND('',#13010,.T.);
#7171=FACE_OUTER_BOUND('',#13011,.T.);
#7172=FACE_OUTER_BOUND('',#13012,.T.);
#7173=FACE_OUTER_BOUND('',#13013,.T.);
#7174=FACE_OUTER_BOUND('',#13014,.T.);
#7175=FACE_OUTER_BOUND('',#13015,.T.);
#7176=FACE_OUTER_BOUND('',#13016,.T.);
#7177=FACE_OUTER_BOUND('',#13017,.T.);
#7178=FACE_OUTER_BOUND('',#13018,.T.);
#7179=FACE_OUTER_BOUND('',#13019,.T.);
#7180=FACE_OUTER_BOUND('',#13020,.T.);
#7181=FACE_OUTER_BOUND('',#13021,.T.);
#7182=FACE_OUTER_BOUND('',#13022,.T.);
#7183=FACE_OUTER_BOUND('',#13023,.T.);
#7184=FACE_OUTER_BOUND('',#13024,.T.);
#7185=FACE_OUTER_BOUND('',#13025,.T.);
#7186=FACE_OUTER_BOUND('',#13026,.T.);
#7187=FACE_OUTER_BOUND('',#13028,.T.);
#7188=FACE_OUTER_BOUND('',#13032,.T.);
#7189=FACE_OUTER_BOUND('',#13033,.T.);
#7190=FACE_OUTER_BOUND('',#13034,.T.);
#7191=FACE_OUTER_BOUND('',#13035,.T.);
#7192=FACE_OUTER_BOUND('',#13036,.T.);
#7193=FACE_OUTER_BOUND('',#13037,.T.);
#7194=FACE_OUTER_BOUND('',#13038,.T.);
#7195=FACE_OUTER_BOUND('',#13039,.T.);
#7196=FACE_OUTER_BOUND('',#13040,.T.);
#7197=FACE_OUTER_BOUND('',#13041,.T.);
#7198=FACE_OUTER_BOUND('',#13042,.T.);
#7199=FACE_OUTER_BOUND('',#13043,.T.);
#7200=FACE_OUTER_BOUND('',#13044,.T.);
#7201=FACE_OUTER_BOUND('',#13046,.T.);
#7202=FACE_OUTER_BOUND('',#13047,.T.);
#7203=FACE_OUTER_BOUND('',#13048,.T.);
#7204=FACE_OUTER_BOUND('',#13049,.T.);
#7205=FACE_OUTER_BOUND('',#13050,.T.);
#7206=FACE_OUTER_BOUND('',#13051,.T.);
#7207=FACE_OUTER_BOUND('',#13052,.T.);
#7208=FACE_OUTER_BOUND('',#13053,.T.);
#7209=FACE_OUTER_BOUND('',#13054,.T.);
#7210=FACE_OUTER_BOUND('',#13055,.T.);
#7211=FACE_OUTER_BOUND('',#13056,.T.);
#7212=FACE_OUTER_BOUND('',#13057,.T.);
#7213=FACE_OUTER_BOUND('',#13058,.T.);
#7214=FACE_OUTER_BOUND('',#13059,.T.);
#7215=FACE_OUTER_BOUND('',#13060,.T.);
#7216=FACE_OUTER_BOUND('',#13061,.T.);
#7217=FACE_OUTER_BOUND('',#13062,.T.);
#7218=FACE_OUTER_BOUND('',#13063,.T.);
#7219=FACE_OUTER_BOUND('',#13064,.T.);
#7220=FACE_OUTER_BOUND('',#13065,.T.);
#7221=FACE_OUTER_BOUND('',#13066,.T.);
#7222=FACE_OUTER_BOUND('',#13067,.T.);
#7223=FACE_OUTER_BOUND('',#13068,.T.);
#7224=FACE_OUTER_BOUND('',#13070,.T.);
#7225=FACE_OUTER_BOUND('',#13072,.T.);
#7226=FACE_OUTER_BOUND('',#13073,.T.);
#7227=FACE_OUTER_BOUND('',#13074,.T.);
#7228=FACE_OUTER_BOUND('',#13075,.T.);
#7229=FACE_OUTER_BOUND('',#13076,.T.);
#7230=FACE_OUTER_BOUND('',#13077,.T.);
#7231=FACE_OUTER_BOUND('',#13078,.T.);
#7232=FACE_OUTER_BOUND('',#13079,.T.);
#7233=FACE_OUTER_BOUND('',#13081,.T.);
#7234=FACE_OUTER_BOUND('',#13082,.T.);
#7235=FACE_OUTER_BOUND('',#13084,.T.);
#7236=FACE_OUTER_BOUND('',#13085,.T.);
#7237=FACE_OUTER_BOUND('',#13086,.T.);
#7238=FACE_OUTER_BOUND('',#13087,.T.);
#7239=FACE_OUTER_BOUND('',#13088,.T.);
#7240=FACE_OUTER_BOUND('',#13090,.T.);
#7241=FACE_OUTER_BOUND('',#13091,.T.);
#7242=FACE_OUTER_BOUND('',#13092,.T.);
#7243=FACE_OUTER_BOUND('',#13093,.T.);
#7244=FACE_OUTER_BOUND('',#13094,.T.);
#7245=FACE_OUTER_BOUND('',#13095,.T.);
#7246=FACE_OUTER_BOUND('',#13096,.T.);
#7247=FACE_OUTER_BOUND('',#13097,.T.);
#7248=FACE_OUTER_BOUND('',#13098,.T.);
#7249=FACE_OUTER_BOUND('',#13099,.T.);
#7250=FACE_OUTER_BOUND('',#13100,.T.);
#7251=FACE_OUTER_BOUND('',#13101,.T.);
#7252=FACE_OUTER_BOUND('',#13102,.T.);
#7253=FACE_OUTER_BOUND('',#13103,.T.);
#7254=FACE_OUTER_BOUND('',#13104,.T.);
#7255=FACE_OUTER_BOUND('',#13105,.T.);
#7256=FACE_OUTER_BOUND('',#13106,.T.);
#7257=FACE_OUTER_BOUND('',#13107,.T.);
#7258=FACE_OUTER_BOUND('',#13108,.T.);
#7259=FACE_OUTER_BOUND('',#13109,.T.);
#7260=FACE_OUTER_BOUND('',#13110,.T.);
#7261=FACE_OUTER_BOUND('',#13111,.T.);
#7262=FACE_OUTER_BOUND('',#13112,.T.);
#7263=FACE_OUTER_BOUND('',#13113,.T.);
#7264=FACE_OUTER_BOUND('',#13114,.T.);
#7265=FACE_OUTER_BOUND('',#13115,.T.);
#7266=FACE_OUTER_BOUND('',#13116,.T.);
#7267=FACE_OUTER_BOUND('',#13117,.T.);
#7268=FACE_OUTER_BOUND('',#13118,.T.);
#7269=FACE_OUTER_BOUND('',#13119,.T.);
#7270=FACE_OUTER_BOUND('',#13120,.T.);
#7271=FACE_OUTER_BOUND('',#13121,.T.);
#7272=FACE_OUTER_BOUND('',#13122,.T.);
#7273=FACE_OUTER_BOUND('',#13124,.T.);
#7274=FACE_OUTER_BOUND('',#13125,.T.);
#7275=FACE_OUTER_BOUND('',#13126,.T.);
#7276=FACE_OUTER_BOUND('',#13127,.T.);
#7277=FACE_OUTER_BOUND('',#13128,.T.);
#7278=FACE_OUTER_BOUND('',#13129,.T.);
#7279=FACE_OUTER_BOUND('',#13131,.T.);
#7280=FACE_OUTER_BOUND('',#13132,.T.);
#7281=FACE_OUTER_BOUND('',#13133,.T.);
#7282=FACE_OUTER_BOUND('',#13134,.T.);
#7283=FACE_OUTER_BOUND('',#13135,.T.);
#7284=FACE_OUTER_BOUND('',#13136,.T.);
#7285=FACE_OUTER_BOUND('',#13137,.T.);
#7286=FACE_OUTER_BOUND('',#13138,.T.);
#7287=FACE_OUTER_BOUND('',#13139,.T.);
#7288=FACE_OUTER_BOUND('',#13140,.T.);
#7289=FACE_OUTER_BOUND('',#13141,.T.);
#7290=FACE_OUTER_BOUND('',#13142,.T.);
#7291=FACE_OUTER_BOUND('',#13143,.T.);
#7292=FACE_OUTER_BOUND('',#13144,.T.);
#7293=FACE_OUTER_BOUND('',#13145,.T.);
#7294=FACE_OUTER_BOUND('',#13146,.T.);
#7295=FACE_OUTER_BOUND('',#13148,.T.);
#7296=FACE_OUTER_BOUND('',#13149,.T.);
#7297=FACE_OUTER_BOUND('',#13150,.T.);
#7298=FACE_OUTER_BOUND('',#13151,.T.);
#7299=FACE_OUTER_BOUND('',#13152,.T.);
#7300=FACE_OUTER_BOUND('',#13153,.T.);
#7301=FACE_OUTER_BOUND('',#13154,.T.);
#7302=FACE_OUTER_BOUND('',#13155,.T.);
#7303=FACE_OUTER_BOUND('',#13156,.T.);
#7304=FACE_OUTER_BOUND('',#13157,.T.);
#7305=FACE_OUTER_BOUND('',#13158,.T.);
#7306=FACE_OUTER_BOUND('',#13159,.T.);
#7307=FACE_OUTER_BOUND('',#13160,.T.);
#7308=FACE_OUTER_BOUND('',#13161,.T.);
#7309=FACE_OUTER_BOUND('',#13162,.T.);
#7310=FACE_OUTER_BOUND('',#13163,.T.);
#7311=FACE_OUTER_BOUND('',#13164,.T.);
#7312=FACE_OUTER_BOUND('',#13165,.T.);
#7313=FACE_OUTER_BOUND('',#13166,.T.);
#7314=FACE_OUTER_BOUND('',#13167,.T.);
#7315=FACE_OUTER_BOUND('',#13168,.T.);
#7316=FACE_OUTER_BOUND('',#13169,.T.);
#7317=FACE_OUTER_BOUND('',#13170,.T.);
#7318=FACE_OUTER_BOUND('',#13171,.T.);
#7319=FACE_OUTER_BOUND('',#13172,.T.);
#7320=FACE_OUTER_BOUND('',#13173,.T.);
#7321=FACE_OUTER_BOUND('',#13174,.T.);
#7322=FACE_OUTER_BOUND('',#13175,.T.);
#7323=FACE_OUTER_BOUND('',#13176,.T.);
#7324=FACE_OUTER_BOUND('',#13177,.T.);
#7325=FACE_OUTER_BOUND('',#13178,.T.);
#7326=FACE_OUTER_BOUND('',#13179,.T.);
#7327=FACE_OUTER_BOUND('',#13180,.T.);
#7328=FACE_OUTER_BOUND('',#13181,.T.);
#7329=FACE_OUTER_BOUND('',#13182,.T.);
#7330=FACE_OUTER_BOUND('',#13183,.T.);
#7331=FACE_OUTER_BOUND('',#13184,.T.);
#7332=FACE_OUTER_BOUND('',#13185,.T.);
#7333=FACE_OUTER_BOUND('',#13186,.T.);
#7334=FACE_OUTER_BOUND('',#13187,.T.);
#7335=FACE_OUTER_BOUND('',#13188,.T.);
#7336=FACE_OUTER_BOUND('',#13189,.T.);
#7337=FACE_OUTER_BOUND('',#13190,.T.);
#7338=FACE_OUTER_BOUND('',#13191,.T.);
#7339=FACE_OUTER_BOUND('',#13192,.T.);
#7340=FACE_OUTER_BOUND('',#13193,.T.);
#7341=FACE_OUTER_BOUND('',#13194,.T.);
#7342=FACE_OUTER_BOUND('',#13195,.T.);
#7343=FACE_OUTER_BOUND('',#13196,.T.);
#7344=FACE_OUTER_BOUND('',#13197,.T.);
#7345=FACE_OUTER_BOUND('',#13198,.T.);
#7346=FACE_OUTER_BOUND('',#13200,.T.);
#7347=FACE_OUTER_BOUND('',#13201,.T.);
#7348=FACE_OUTER_BOUND('',#13202,.T.);
#7349=FACE_OUTER_BOUND('',#13203,.T.);
#7350=FACE_OUTER_BOUND('',#13204,.T.);
#7351=FACE_OUTER_BOUND('',#13205,.T.);
#7352=FACE_OUTER_BOUND('',#13206,.T.);
#7353=FACE_OUTER_BOUND('',#13207,.T.);
#7354=FACE_OUTER_BOUND('',#13208,.T.);
#7355=FACE_OUTER_BOUND('',#13209,.T.);
#7356=FACE_OUTER_BOUND('',#13210,.T.);
#7357=FACE_OUTER_BOUND('',#13211,.T.);
#7358=FACE_OUTER_BOUND('',#13212,.T.);
#7359=FACE_OUTER_BOUND('',#13216,.T.);
#7360=FACE_OUTER_BOUND('',#13217,.T.);
#7361=FACE_OUTER_BOUND('',#13218,.T.);
#7362=FACE_OUTER_BOUND('',#13219,.T.);
#7363=FACE_OUTER_BOUND('',#13220,.T.);
#7364=FACE_OUTER_BOUND('',#13221,.T.);
#7365=FACE_OUTER_BOUND('',#13222,.T.);
#7366=FACE_OUTER_BOUND('',#13223,.T.);
#7367=FACE_OUTER_BOUND('',#13224,.T.);
#7368=FACE_OUTER_BOUND('',#13225,.T.);
#7369=FACE_OUTER_BOUND('',#13226,.T.);
#7370=FACE_OUTER_BOUND('',#13227,.T.);
#7371=FACE_OUTER_BOUND('',#13228,.T.);
#7372=FACE_OUTER_BOUND('',#13229,.T.);
#7373=FACE_OUTER_BOUND('',#13231,.T.);
#7374=FACE_OUTER_BOUND('',#13232,.T.);
#7375=FACE_OUTER_BOUND('',#13233,.T.);
#7376=FACE_OUTER_BOUND('',#13234,.T.);
#7377=FACE_OUTER_BOUND('',#13235,.T.);
#7378=FACE_OUTER_BOUND('',#13236,.T.);
#7379=FACE_OUTER_BOUND('',#13237,.T.);
#7380=FACE_OUTER_BOUND('',#13238,.T.);
#7381=FACE_OUTER_BOUND('',#13239,.T.);
#7382=FACE_OUTER_BOUND('',#13240,.T.);
#7383=FACE_OUTER_BOUND('',#13241,.T.);
#7384=FACE_OUTER_BOUND('',#13242,.T.);
#7385=FACE_OUTER_BOUND('',#13243,.T.);
#7386=FACE_OUTER_BOUND('',#13244,.T.);
#7387=FACE_OUTER_BOUND('',#13245,.T.);
#7388=FACE_OUTER_BOUND('',#13246,.T.);
#7389=FACE_OUTER_BOUND('',#13247,.T.);
#7390=FACE_OUTER_BOUND('',#13248,.T.);
#7391=FACE_OUTER_BOUND('',#13249,.T.);
#7392=FACE_OUTER_BOUND('',#13250,.T.);
#7393=FACE_OUTER_BOUND('',#13251,.T.);
#7394=FACE_OUTER_BOUND('',#13252,.T.);
#7395=FACE_OUTER_BOUND('',#13253,.T.);
#7396=FACE_OUTER_BOUND('',#13254,.T.);
#7397=FACE_OUTER_BOUND('',#13255,.T.);
#7398=FACE_OUTER_BOUND('',#13256,.T.);
#7399=FACE_OUTER_BOUND('',#13258,.T.);
#7400=FACE_OUTER_BOUND('',#13259,.T.);
#7401=FACE_OUTER_BOUND('',#13260,.T.);
#7402=FACE_OUTER_BOUND('',#13261,.T.);
#7403=FACE_OUTER_BOUND('',#13262,.T.);
#7404=FACE_OUTER_BOUND('',#13263,.T.);
#7405=FACE_OUTER_BOUND('',#13265,.T.);
#7406=FACE_OUTER_BOUND('',#13267,.T.);
#7407=FACE_OUTER_BOUND('',#13268,.T.);
#7408=FACE_OUTER_BOUND('',#13269,.T.);
#7409=FACE_OUTER_BOUND('',#13271,.T.);
#7410=FACE_OUTER_BOUND('',#13273,.T.);
#7411=FACE_OUTER_BOUND('',#13274,.T.);
#7412=FACE_OUTER_BOUND('',#13275,.T.);
#7413=FACE_OUTER_BOUND('',#13276,.T.);
#7414=FACE_OUTER_BOUND('',#13277,.T.);
#7415=FACE_OUTER_BOUND('',#13279,.T.);
#7416=FACE_OUTER_BOUND('',#13280,.T.);
#7417=FACE_OUTER_BOUND('',#13282,.T.);
#7418=FACE_OUTER_BOUND('',#13283,.T.);
#7419=FACE_OUTER_BOUND('',#13284,.T.);
#7420=FACE_OUTER_BOUND('',#13285,.T.);
#7421=FACE_OUTER_BOUND('',#13286,.T.);
#7422=FACE_OUTER_BOUND('',#13287,.T.);
#7423=FACE_OUTER_BOUND('',#13288,.T.);
#7424=FACE_OUTER_BOUND('',#13289,.T.);
#7425=FACE_OUTER_BOUND('',#13290,.T.);
#7426=FACE_OUTER_BOUND('',#13291,.T.);
#7427=FACE_OUTER_BOUND('',#13292,.T.);
#7428=FACE_OUTER_BOUND('',#13293,.T.);
#7429=FACE_OUTER_BOUND('',#13294,.T.);
#7430=FACE_OUTER_BOUND('',#13295,.T.);
#7431=FACE_OUTER_BOUND('',#13296,.T.);
#7432=FACE_OUTER_BOUND('',#13297,.T.);
#7433=FACE_OUTER_BOUND('',#13298,.T.);
#7434=FACE_OUTER_BOUND('',#13299,.T.);
#7435=FACE_OUTER_BOUND('',#13300,.T.);
#7436=FACE_OUTER_BOUND('',#13301,.T.);
#7437=FACE_OUTER_BOUND('',#13302,.T.);
#7438=FACE_OUTER_BOUND('',#13303,.T.);
#7439=FACE_OUTER_BOUND('',#13304,.T.);
#7440=FACE_OUTER_BOUND('',#13305,.T.);
#7441=FACE_OUTER_BOUND('',#13306,.T.);
#7442=FACE_OUTER_BOUND('',#13307,.T.);
#7443=FACE_OUTER_BOUND('',#13308,.T.);
#7444=FACE_OUTER_BOUND('',#13309,.T.);
#7445=FACE_OUTER_BOUND('',#13310,.T.);
#7446=FACE_OUTER_BOUND('',#13311,.T.);
#7447=FACE_OUTER_BOUND('',#13312,.T.);
#7448=FACE_OUTER_BOUND('',#13313,.T.);
#7449=FACE_OUTER_BOUND('',#13314,.T.);
#7450=FACE_OUTER_BOUND('',#13315,.T.);
#7451=FACE_OUTER_BOUND('',#13316,.T.);
#7452=FACE_OUTER_BOUND('',#13317,.T.);
#7453=FACE_OUTER_BOUND('',#13318,.T.);
#7454=FACE_OUTER_BOUND('',#13319,.T.);
#7455=FACE_OUTER_BOUND('',#13320,.T.);
#7456=FACE_OUTER_BOUND('',#13321,.T.);
#7457=FACE_OUTER_BOUND('',#13322,.T.);
#7458=FACE_OUTER_BOUND('',#13323,.T.);
#7459=FACE_OUTER_BOUND('',#13324,.T.);
#7460=FACE_OUTER_BOUND('',#13325,.T.);
#7461=FACE_OUTER_BOUND('',#13326,.T.);
#7462=FACE_OUTER_BOUND('',#13327,.T.);
#7463=FACE_OUTER_BOUND('',#13328,.T.);
#7464=FACE_OUTER_BOUND('',#13329,.T.);
#7465=FACE_OUTER_BOUND('',#13330,.T.);
#7466=FACE_OUTER_BOUND('',#13331,.T.);
#7467=FACE_OUTER_BOUND('',#13332,.T.);
#7468=FACE_OUTER_BOUND('',#13333,.T.);
#7469=FACE_OUTER_BOUND('',#13334,.T.);
#7470=FACE_OUTER_BOUND('',#13335,.T.);
#7471=FACE_OUTER_BOUND('',#13336,.T.);
#7472=FACE_OUTER_BOUND('',#13337,.T.);
#7473=FACE_OUTER_BOUND('',#13338,.T.);
#7474=FACE_OUTER_BOUND('',#13339,.T.);
#7475=FACE_OUTER_BOUND('',#13340,.T.);
#7476=FACE_OUTER_BOUND('',#13341,.T.);
#7477=FACE_OUTER_BOUND('',#13342,.T.);
#7478=FACE_OUTER_BOUND('',#13343,.T.);
#7479=FACE_OUTER_BOUND('',#13344,.T.);
#7480=FACE_OUTER_BOUND('',#13345,.T.);
#7481=FACE_OUTER_BOUND('',#13346,.T.);
#7482=FACE_OUTER_BOUND('',#13347,.T.);
#7483=FACE_OUTER_BOUND('',#13348,.T.);
#7484=FACE_OUTER_BOUND('',#13349,.T.);
#7485=FACE_OUTER_BOUND('',#13350,.T.);
#7486=FACE_OUTER_BOUND('',#13351,.T.);
#7487=FACE_OUTER_BOUND('',#13352,.T.);
#7488=FACE_OUTER_BOUND('',#13353,.T.);
#7489=FACE_OUTER_BOUND('',#13354,.T.);
#7490=FACE_OUTER_BOUND('',#13355,.T.);
#7491=FACE_OUTER_BOUND('',#13356,.T.);
#7492=FACE_OUTER_BOUND('',#13357,.T.);
#7493=FACE_OUTER_BOUND('',#13358,.T.);
#7494=FACE_OUTER_BOUND('',#13359,.T.);
#7495=FACE_OUTER_BOUND('',#13360,.T.);
#7496=FACE_OUTER_BOUND('',#13361,.T.);
#7497=FACE_OUTER_BOUND('',#13362,.T.);
#7498=FACE_OUTER_BOUND('',#13363,.T.);
#7499=FACE_OUTER_BOUND('',#13364,.T.);
#7500=FACE_OUTER_BOUND('',#13365,.T.);
#7501=FACE_OUTER_BOUND('',#13366,.T.);
#7502=FACE_OUTER_BOUND('',#13367,.T.);
#7503=FACE_OUTER_BOUND('',#13368,.T.);
#7504=FACE_OUTER_BOUND('',#13369,.T.);
#7505=FACE_OUTER_BOUND('',#13370,.T.);
#7506=FACE_OUTER_BOUND('',#13371,.T.);
#7507=FACE_OUTER_BOUND('',#13372,.T.);
#7508=FACE_OUTER_BOUND('',#13373,.T.);
#7509=FACE_OUTER_BOUND('',#13374,.T.);
#7510=FACE_OUTER_BOUND('',#13375,.T.);
#7511=FACE_OUTER_BOUND('',#13376,.T.);
#7512=FACE_OUTER_BOUND('',#13377,.T.);
#7513=FACE_OUTER_BOUND('',#13378,.T.);
#7514=FACE_OUTER_BOUND('',#13379,.T.);
#7515=FACE_OUTER_BOUND('',#13380,.T.);
#7516=FACE_OUTER_BOUND('',#13381,.T.);
#7517=FACE_OUTER_BOUND('',#13382,.T.);
#7518=FACE_OUTER_BOUND('',#13383,.T.);
#7519=FACE_OUTER_BOUND('',#13384,.T.);
#7520=FACE_OUTER_BOUND('',#13385,.T.);
#7521=FACE_OUTER_BOUND('',#13386,.T.);
#7522=FACE_OUTER_BOUND('',#13387,.T.);
#7523=FACE_OUTER_BOUND('',#13388,.T.);
#7524=FACE_OUTER_BOUND('',#13389,.T.);
#7525=FACE_OUTER_BOUND('',#13391,.T.);
#7526=FACE_OUTER_BOUND('',#13395,.T.);
#7527=FACE_OUTER_BOUND('',#13399,.T.);
#7528=FACE_OUTER_BOUND('',#13400,.T.);
#7529=FACE_OUTER_BOUND('',#13401,.T.);
#7530=FACE_OUTER_BOUND('',#13402,.T.);
#7531=FACE_OUTER_BOUND('',#13403,.T.);
#7532=FACE_OUTER_BOUND('',#13404,.T.);
#7533=FACE_OUTER_BOUND('',#13405,.T.);
#7534=FACE_OUTER_BOUND('',#13406,.T.);
#7535=FACE_OUTER_BOUND('',#13407,.T.);
#7536=FACE_OUTER_BOUND('',#13408,.T.);
#7537=FACE_OUTER_BOUND('',#13409,.T.);
#7538=FACE_OUTER_BOUND('',#13410,.T.);
#7539=FACE_OUTER_BOUND('',#13411,.T.);
#7540=FACE_OUTER_BOUND('',#13412,.T.);
#7541=FACE_OUTER_BOUND('',#13413,.T.);
#7542=FACE_OUTER_BOUND('',#13414,.T.);
#7543=FACE_OUTER_BOUND('',#13415,.T.);
#7544=FACE_OUTER_BOUND('',#13416,.T.);
#7545=FACE_OUTER_BOUND('',#13417,.T.);
#7546=FACE_OUTER_BOUND('',#13418,.T.);
#7547=FACE_OUTER_BOUND('',#13419,.T.);
#7548=FACE_OUTER_BOUND('',#13420,.T.);
#7549=FACE_OUTER_BOUND('',#13421,.T.);
#7550=FACE_OUTER_BOUND('',#13422,.T.);
#7551=FACE_OUTER_BOUND('',#13423,.T.);
#7552=FACE_OUTER_BOUND('',#13424,.T.);
#7553=FACE_OUTER_BOUND('',#13425,.T.);
#7554=FACE_OUTER_BOUND('',#13426,.T.);
#7555=FACE_OUTER_BOUND('',#13427,.T.);
#7556=FACE_OUTER_BOUND('',#13428,.T.);
#7557=FACE_OUTER_BOUND('',#13429,.T.);
#7558=FACE_OUTER_BOUND('',#13430,.T.);
#7559=FACE_OUTER_BOUND('',#13431,.T.);
#7560=FACE_OUTER_BOUND('',#13432,.T.);
#7561=FACE_OUTER_BOUND('',#13433,.T.);
#7562=FACE_OUTER_BOUND('',#13434,.T.);
#7563=FACE_OUTER_BOUND('',#13435,.T.);
#7564=FACE_OUTER_BOUND('',#13436,.T.);
#7565=FACE_OUTER_BOUND('',#13437,.T.);
#7566=FACE_OUTER_BOUND('',#13438,.T.);
#7567=FACE_OUTER_BOUND('',#13439,.T.);
#7568=FACE_OUTER_BOUND('',#13440,.T.);
#7569=FACE_OUTER_BOUND('',#13441,.T.);
#7570=FACE_OUTER_BOUND('',#13442,.T.);
#7571=FACE_OUTER_BOUND('',#13443,.T.);
#7572=FACE_OUTER_BOUND('',#13444,.T.);
#7573=FACE_OUTER_BOUND('',#13445,.T.);
#7574=FACE_OUTER_BOUND('',#13446,.T.);
#7575=FACE_OUTER_BOUND('',#13447,.T.);
#7576=FACE_OUTER_BOUND('',#13448,.T.);
#7577=FACE_OUTER_BOUND('',#13449,.T.);
#7578=FACE_OUTER_BOUND('',#13450,.T.);
#7579=FACE_OUTER_BOUND('',#13451,.T.);
#7580=FACE_OUTER_BOUND('',#13452,.T.);
#7581=FACE_OUTER_BOUND('',#13453,.T.);
#7582=FACE_OUTER_BOUND('',#13454,.T.);
#7583=FACE_OUTER_BOUND('',#13455,.T.);
#7584=FACE_OUTER_BOUND('',#13456,.T.);
#7585=FACE_OUTER_BOUND('',#13457,.T.);
#7586=FACE_OUTER_BOUND('',#13458,.T.);
#7587=FACE_OUTER_BOUND('',#13459,.T.);
#7588=FACE_OUTER_BOUND('',#13460,.T.);
#7589=FACE_OUTER_BOUND('',#13461,.T.);
#7590=FACE_OUTER_BOUND('',#13462,.T.);
#7591=FACE_OUTER_BOUND('',#13463,.T.);
#7592=FACE_OUTER_BOUND('',#13464,.T.);
#7593=FACE_OUTER_BOUND('',#13465,.T.);
#7594=FACE_OUTER_BOUND('',#13466,.T.);
#7595=FACE_OUTER_BOUND('',#13467,.T.);
#7596=FACE_OUTER_BOUND('',#13468,.T.);
#7597=FACE_OUTER_BOUND('',#13469,.T.);
#7598=FACE_OUTER_BOUND('',#13470,.T.);
#7599=FACE_OUTER_BOUND('',#13471,.T.);
#7600=FACE_OUTER_BOUND('',#13472,.T.);
#7601=FACE_OUTER_BOUND('',#13473,.T.);
#7602=FACE_OUTER_BOUND('',#13474,.T.);
#7603=FACE_OUTER_BOUND('',#13475,.T.);
#7604=FACE_OUTER_BOUND('',#13476,.T.);
#7605=FACE_OUTER_BOUND('',#13477,.T.);
#7606=FACE_OUTER_BOUND('',#13478,.T.);
#7607=FACE_OUTER_BOUND('',#13479,.T.);
#7608=FACE_OUTER_BOUND('',#13480,.T.);
#7609=FACE_OUTER_BOUND('',#13481,.T.);
#7610=FACE_OUTER_BOUND('',#13482,.T.);
#7611=FACE_OUTER_BOUND('',#13483,.T.);
#7612=FACE_OUTER_BOUND('',#13484,.T.);
#7613=FACE_OUTER_BOUND('',#13485,.T.);
#7614=FACE_OUTER_BOUND('',#13486,.T.);
#7615=FACE_OUTER_BOUND('',#13487,.T.);
#7616=FACE_OUTER_BOUND('',#13488,.T.);
#7617=FACE_OUTER_BOUND('',#13489,.T.);
#7618=FACE_OUTER_BOUND('',#13490,.T.);
#7619=FACE_OUTER_BOUND('',#13491,.T.);
#7620=FACE_OUTER_BOUND('',#13492,.T.);
#7621=FACE_OUTER_BOUND('',#13493,.T.);
#7622=FACE_OUTER_BOUND('',#13494,.T.);
#7623=FACE_OUTER_BOUND('',#13495,.T.);
#7624=FACE_OUTER_BOUND('',#13496,.T.);
#7625=FACE_OUTER_BOUND('',#13497,.T.);
#7626=FACE_OUTER_BOUND('',#13498,.T.);
#7627=FACE_OUTER_BOUND('',#13499,.T.);
#7628=FACE_OUTER_BOUND('',#13500,.T.);
#7629=FACE_OUTER_BOUND('',#13501,.T.);
#7630=FACE_OUTER_BOUND('',#13502,.T.);
#7631=FACE_OUTER_BOUND('',#13503,.T.);
#7632=FACE_OUTER_BOUND('',#13504,.T.);
#7633=FACE_OUTER_BOUND('',#13505,.T.);
#7634=FACE_OUTER_BOUND('',#13506,.T.);
#7635=FACE_OUTER_BOUND('',#13507,.T.);
#7636=FACE_OUTER_BOUND('',#13508,.T.);
#7637=FACE_OUTER_BOUND('',#13509,.T.);
#7638=FACE_OUTER_BOUND('',#13510,.T.);
#7639=FACE_OUTER_BOUND('',#13511,.T.);
#7640=FACE_OUTER_BOUND('',#13512,.T.);
#7641=FACE_OUTER_BOUND('',#13513,.T.);
#7642=FACE_OUTER_BOUND('',#13514,.T.);
#7643=FACE_OUTER_BOUND('',#13515,.T.);
#7644=FACE_OUTER_BOUND('',#13516,.T.);
#7645=FACE_OUTER_BOUND('',#13517,.T.);
#7646=FACE_OUTER_BOUND('',#13518,.T.);
#7647=FACE_OUTER_BOUND('',#13519,.T.);
#7648=FACE_OUTER_BOUND('',#13520,.T.);
#7649=FACE_OUTER_BOUND('',#13521,.T.);
#7650=FACE_OUTER_BOUND('',#13522,.T.);
#7651=FACE_OUTER_BOUND('',#13523,.T.);
#7652=FACE_OUTER_BOUND('',#13524,.T.);
#7653=FACE_OUTER_BOUND('',#13525,.T.);
#7654=FACE_OUTER_BOUND('',#13526,.T.);
#7655=FACE_OUTER_BOUND('',#13527,.T.);
#7656=FACE_OUTER_BOUND('',#13528,.T.);
#7657=FACE_OUTER_BOUND('',#13529,.T.);
#7658=FACE_OUTER_BOUND('',#13530,.T.);
#7659=FACE_OUTER_BOUND('',#13531,.T.);
#7660=FACE_OUTER_BOUND('',#13532,.T.);
#7661=FACE_OUTER_BOUND('',#13533,.T.);
#7662=FACE_OUTER_BOUND('',#13534,.T.);
#7663=FACE_OUTER_BOUND('',#13535,.T.);
#7664=FACE_OUTER_BOUND('',#13536,.T.);
#7665=FACE_OUTER_BOUND('',#13537,.T.);
#7666=FACE_OUTER_BOUND('',#13538,.T.);
#7667=FACE_OUTER_BOUND('',#13539,.T.);
#7668=FACE_OUTER_BOUND('',#13540,.T.);
#7669=FACE_OUTER_BOUND('',#13541,.T.);
#7670=FACE_OUTER_BOUND('',#13542,.T.);
#7671=FACE_OUTER_BOUND('',#13543,.T.);
#7672=FACE_OUTER_BOUND('',#13544,.T.);
#7673=FACE_OUTER_BOUND('',#13545,.T.);
#7674=FACE_OUTER_BOUND('',#13546,.T.);
#7675=FACE_OUTER_BOUND('',#13547,.T.);
#7676=FACE_OUTER_BOUND('',#13548,.T.);
#7677=FACE_OUTER_BOUND('',#13549,.T.);
#7678=FACE_OUTER_BOUND('',#13550,.T.);
#7679=FACE_OUTER_BOUND('',#13551,.T.);
#7680=FACE_OUTER_BOUND('',#13552,.T.);
#7681=FACE_OUTER_BOUND('',#13553,.T.);
#7682=FACE_OUTER_BOUND('',#13554,.T.);
#7683=FACE_OUTER_BOUND('',#13555,.T.);
#7684=FACE_OUTER_BOUND('',#13556,.T.);
#7685=FACE_OUTER_BOUND('',#13557,.T.);
#7686=FACE_OUTER_BOUND('',#13558,.T.);
#7687=FACE_OUTER_BOUND('',#13559,.T.);
#7688=FACE_OUTER_BOUND('',#13560,.T.);
#7689=FACE_OUTER_BOUND('',#13561,.T.);
#7690=FACE_OUTER_BOUND('',#13562,.T.);
#7691=FACE_OUTER_BOUND('',#13563,.T.);
#7692=FACE_OUTER_BOUND('',#13564,.T.);
#7693=FACE_OUTER_BOUND('',#13565,.T.);
#7694=FACE_OUTER_BOUND('',#13566,.T.);
#7695=FACE_OUTER_BOUND('',#13567,.T.);
#7696=FACE_OUTER_BOUND('',#13568,.T.);
#7697=FACE_OUTER_BOUND('',#13569,.T.);
#7698=FACE_OUTER_BOUND('',#13570,.T.);
#7699=FACE_OUTER_BOUND('',#13571,.T.);
#7700=FACE_OUTER_BOUND('',#13572,.T.);
#7701=FACE_OUTER_BOUND('',#13573,.T.);
#7702=FACE_OUTER_BOUND('',#13574,.T.);
#7703=FACE_OUTER_BOUND('',#13575,.T.);
#7704=FACE_OUTER_BOUND('',#13576,.T.);
#7705=FACE_OUTER_BOUND('',#13577,.T.);
#7706=FACE_OUTER_BOUND('',#13578,.T.);
#7707=FACE_OUTER_BOUND('',#13579,.T.);
#7708=FACE_OUTER_BOUND('',#13580,.T.);
#7709=FACE_OUTER_BOUND('',#13581,.T.);
#7710=FACE_OUTER_BOUND('',#13582,.T.);
#7711=FACE_OUTER_BOUND('',#13583,.T.);
#7712=FACE_OUTER_BOUND('',#13584,.T.);
#7713=FACE_OUTER_BOUND('',#13585,.T.);
#7714=FACE_OUTER_BOUND('',#13586,.T.);
#7715=FACE_OUTER_BOUND('',#13587,.T.);
#7716=FACE_OUTER_BOUND('',#13588,.T.);
#7717=FACE_OUTER_BOUND('',#13589,.T.);
#7718=FACE_OUTER_BOUND('',#13590,.T.);
#7719=FACE_OUTER_BOUND('',#13591,.T.);
#7720=FACE_OUTER_BOUND('',#13592,.T.);
#7721=FACE_OUTER_BOUND('',#13593,.T.);
#7722=FACE_OUTER_BOUND('',#13594,.T.);
#7723=FACE_OUTER_BOUND('',#13595,.T.);
#7724=FACE_OUTER_BOUND('',#13596,.T.);
#7725=FACE_OUTER_BOUND('',#13597,.T.);
#7726=FACE_OUTER_BOUND('',#13598,.T.);
#7727=FACE_OUTER_BOUND('',#13599,.T.);
#7728=FACE_OUTER_BOUND('',#13600,.T.);
#7729=FACE_OUTER_BOUND('',#13601,.T.);
#7730=FACE_OUTER_BOUND('',#13602,.T.);
#7731=FACE_OUTER_BOUND('',#13603,.T.);
#7732=FACE_OUTER_BOUND('',#13604,.T.);
#7733=FACE_OUTER_BOUND('',#13605,.T.);
#7734=FACE_OUTER_BOUND('',#13606,.T.);
#7735=FACE_OUTER_BOUND('',#13607,.T.);
#7736=FACE_OUTER_BOUND('',#13608,.T.);
#7737=FACE_OUTER_BOUND('',#13609,.T.);
#7738=FACE_OUTER_BOUND('',#13610,.T.);
#7739=FACE_OUTER_BOUND('',#13611,.T.);
#7740=FACE_OUTER_BOUND('',#13612,.T.);
#7741=FACE_OUTER_BOUND('',#13613,.T.);
#7742=FACE_OUTER_BOUND('',#13614,.T.);
#7743=FACE_OUTER_BOUND('',#13615,.T.);
#7744=FACE_OUTER_BOUND('',#13616,.T.);
#7745=FACE_OUTER_BOUND('',#13617,.T.);
#7746=FACE_OUTER_BOUND('',#13618,.T.);
#7747=FACE_OUTER_BOUND('',#13619,.T.);
#7748=FACE_OUTER_BOUND('',#13620,.T.);
#7749=FACE_OUTER_BOUND('',#13621,.T.);
#7750=FACE_OUTER_BOUND('',#13622,.T.);
#7751=FACE_OUTER_BOUND('',#13623,.T.);
#7752=FACE_OUTER_BOUND('',#13624,.T.);
#7753=FACE_OUTER_BOUND('',#13625,.T.);
#7754=FACE_OUTER_BOUND('',#13626,.T.);
#7755=FACE_OUTER_BOUND('',#13627,.T.);
#7756=FACE_OUTER_BOUND('',#13628,.T.);
#7757=FACE_OUTER_BOUND('',#13629,.T.);
#7758=FACE_OUTER_BOUND('',#13630,.T.);
#7759=FACE_OUTER_BOUND('',#13631,.T.);
#7760=FACE_OUTER_BOUND('',#13632,.T.);
#7761=FACE_OUTER_BOUND('',#13638,.T.);
#7762=FACE_OUTER_BOUND('',#13639,.T.);
#7763=FACE_OUTER_BOUND('',#13640,.T.);
#7764=FACE_OUTER_BOUND('',#13641,.T.);
#7765=FACE_OUTER_BOUND('',#13642,.T.);
#7766=FACE_OUTER_BOUND('',#13643,.T.);
#7767=FACE_OUTER_BOUND('',#13644,.T.);
#7768=FACE_OUTER_BOUND('',#13645,.T.);
#7769=FACE_OUTER_BOUND('',#13646,.T.);
#7770=FACE_OUTER_BOUND('',#13647,.T.);
#7771=FACE_OUTER_BOUND('',#13648,.T.);
#7772=FACE_OUTER_BOUND('',#13649,.T.);
#7773=FACE_OUTER_BOUND('',#13650,.T.);
#7774=FACE_OUTER_BOUND('',#13651,.T.);
#7775=FACE_OUTER_BOUND('',#13652,.T.);
#7776=FACE_OUTER_BOUND('',#13653,.T.);
#7777=FACE_OUTER_BOUND('',#13654,.T.);
#7778=FACE_OUTER_BOUND('',#13655,.T.);
#7779=FACE_OUTER_BOUND('',#13656,.T.);
#7780=FACE_OUTER_BOUND('',#13657,.T.);
#7781=FACE_OUTER_BOUND('',#13658,.T.);
#7782=FACE_OUTER_BOUND('',#13659,.T.);
#7783=FACE_OUTER_BOUND('',#13660,.T.);
#7784=FACE_OUTER_BOUND('',#13661,.T.);
#7785=FACE_OUTER_BOUND('',#13662,.T.);
#7786=FACE_OUTER_BOUND('',#13663,.T.);
#7787=FACE_OUTER_BOUND('',#13664,.T.);
#7788=FACE_OUTER_BOUND('',#13665,.T.);
#7789=FACE_OUTER_BOUND('',#13666,.T.);
#7790=FACE_OUTER_BOUND('',#13667,.T.);
#7791=FACE_OUTER_BOUND('',#13668,.T.);
#7792=FACE_OUTER_BOUND('',#13669,.T.);
#7793=FACE_OUTER_BOUND('',#13670,.T.);
#7794=FACE_OUTER_BOUND('',#13671,.T.);
#7795=FACE_OUTER_BOUND('',#13672,.T.);
#7796=FACE_OUTER_BOUND('',#13673,.T.);
#7797=FACE_OUTER_BOUND('',#13674,.T.);
#7798=FACE_OUTER_BOUND('',#13678,.T.);
#7799=FACE_OUTER_BOUND('',#13679,.T.);
#7800=FACE_OUTER_BOUND('',#13680,.T.);
#7801=FACE_OUTER_BOUND('',#13681,.T.);
#7802=FACE_OUTER_BOUND('',#13682,.T.);
#7803=FACE_OUTER_BOUND('',#13683,.T.);
#7804=FACE_OUTER_BOUND('',#13684,.T.);
#7805=FACE_OUTER_BOUND('',#13685,.T.);
#7806=FACE_OUTER_BOUND('',#13686,.T.);
#7807=FACE_OUTER_BOUND('',#13687,.T.);
#7808=FACE_OUTER_BOUND('',#13688,.T.);
#7809=FACE_OUTER_BOUND('',#13689,.T.);
#7810=FACE_OUTER_BOUND('',#13690,.T.);
#7811=FACE_OUTER_BOUND('',#13691,.T.);
#7812=FACE_OUTER_BOUND('',#13692,.T.);
#7813=FACE_OUTER_BOUND('',#13693,.T.);
#7814=FACE_OUTER_BOUND('',#13694,.T.);
#7815=FACE_OUTER_BOUND('',#13695,.T.);
#7816=FACE_OUTER_BOUND('',#13696,.T.);
#7817=FACE_OUTER_BOUND('',#13697,.T.);
#7818=FACE_OUTER_BOUND('',#13698,.T.);
#7819=FACE_OUTER_BOUND('',#13699,.T.);
#7820=FACE_OUTER_BOUND('',#13700,.T.);
#7821=FACE_OUTER_BOUND('',#13701,.T.);
#7822=FACE_OUTER_BOUND('',#13702,.T.);
#7823=FACE_OUTER_BOUND('',#13703,.T.);
#7824=FACE_OUTER_BOUND('',#13704,.T.);
#7825=FACE_OUTER_BOUND('',#13705,.T.);
#7826=FACE_OUTER_BOUND('',#13706,.T.);
#7827=FACE_OUTER_BOUND('',#13707,.T.);
#7828=FACE_OUTER_BOUND('',#13708,.T.);
#7829=FACE_OUTER_BOUND('',#13709,.T.);
#7830=FACE_OUTER_BOUND('',#13710,.T.);
#7831=FACE_OUTER_BOUND('',#13711,.T.);
#7832=FACE_OUTER_BOUND('',#13712,.T.);
#7833=FACE_OUTER_BOUND('',#13713,.T.);
#7834=FACE_OUTER_BOUND('',#13714,.T.);
#7835=FACE_OUTER_BOUND('',#13715,.T.);
#7836=FACE_OUTER_BOUND('',#13716,.T.);
#7837=FACE_OUTER_BOUND('',#13717,.T.);
#7838=FACE_OUTER_BOUND('',#13718,.T.);
#7839=FACE_OUTER_BOUND('',#13719,.T.);
#7840=FACE_OUTER_BOUND('',#13720,.T.);
#7841=FACE_OUTER_BOUND('',#13721,.T.);
#7842=FACE_OUTER_BOUND('',#13722,.T.);
#7843=FACE_OUTER_BOUND('',#13723,.T.);
#7844=FACE_OUTER_BOUND('',#13724,.T.);
#7845=FACE_OUTER_BOUND('',#13725,.T.);
#7846=FACE_OUTER_BOUND('',#13726,.T.);
#7847=FACE_OUTER_BOUND('',#13727,.T.);
#7848=FACE_OUTER_BOUND('',#13728,.T.);
#7849=FACE_OUTER_BOUND('',#13729,.T.);
#7850=FACE_OUTER_BOUND('',#13730,.T.);
#7851=FACE_OUTER_BOUND('',#13731,.T.);
#7852=FACE_OUTER_BOUND('',#13732,.T.);
#7853=FACE_OUTER_BOUND('',#13733,.T.);
#7854=FACE_OUTER_BOUND('',#13734,.T.);
#7855=FACE_OUTER_BOUND('',#13735,.T.);
#7856=FACE_OUTER_BOUND('',#13736,.T.);
#7857=FACE_OUTER_BOUND('',#13737,.T.);
#7858=FACE_OUTER_BOUND('',#13738,.T.);
#7859=FACE_OUTER_BOUND('',#13739,.T.);
#7860=FACE_OUTER_BOUND('',#13740,.T.);
#7861=FACE_OUTER_BOUND('',#13741,.T.);
#7862=FACE_OUTER_BOUND('',#13742,.T.);
#7863=FACE_OUTER_BOUND('',#13743,.T.);
#7864=FACE_OUTER_BOUND('',#13744,.T.);
#7865=FACE_OUTER_BOUND('',#13745,.T.);
#7866=FACE_OUTER_BOUND('',#13746,.T.);
#7867=FACE_OUTER_BOUND('',#13747,.T.);
#7868=FACE_OUTER_BOUND('',#13748,.T.);
#7869=FACE_OUTER_BOUND('',#13749,.T.);
#7870=FACE_OUTER_BOUND('',#13750,.T.);
#7871=FACE_OUTER_BOUND('',#13751,.T.);
#7872=FACE_OUTER_BOUND('',#13752,.T.);
#7873=FACE_OUTER_BOUND('',#13753,.T.);
#7874=FACE_OUTER_BOUND('',#13754,.T.);
#7875=FACE_OUTER_BOUND('',#13755,.T.);
#7876=FACE_OUTER_BOUND('',#13756,.T.);
#7877=FACE_OUTER_BOUND('',#13757,.T.);
#7878=FACE_OUTER_BOUND('',#13758,.T.);
#7879=FACE_OUTER_BOUND('',#13759,.T.);
#7880=FACE_OUTER_BOUND('',#13760,.T.);
#7881=FACE_OUTER_BOUND('',#13761,.T.);
#7882=FACE_OUTER_BOUND('',#13762,.T.);
#7883=FACE_OUTER_BOUND('',#13763,.T.);
#7884=FACE_OUTER_BOUND('',#13764,.T.);
#7885=FACE_OUTER_BOUND('',#13765,.T.);
#7886=FACE_OUTER_BOUND('',#13766,.T.);
#7887=FACE_OUTER_BOUND('',#13767,.T.);
#7888=FACE_OUTER_BOUND('',#13768,.T.);
#7889=FACE_OUTER_BOUND('',#13769,.T.);
#7890=FACE_OUTER_BOUND('',#13770,.T.);
#7891=FACE_OUTER_BOUND('',#13771,.T.);
#7892=FACE_OUTER_BOUND('',#13772,.T.);
#7893=FACE_OUTER_BOUND('',#13773,.T.);
#7894=FACE_OUTER_BOUND('',#13774,.T.);
#7895=FACE_OUTER_BOUND('',#13775,.T.);
#7896=FACE_OUTER_BOUND('',#13776,.T.);
#7897=FACE_OUTER_BOUND('',#13777,.T.);
#7898=FACE_OUTER_BOUND('',#13778,.T.);
#7899=FACE_OUTER_BOUND('',#13779,.T.);
#7900=FACE_OUTER_BOUND('',#13780,.T.);
#7901=FACE_OUTER_BOUND('',#13781,.T.);
#7902=FACE_OUTER_BOUND('',#13782,.T.);
#7903=FACE_OUTER_BOUND('',#13783,.T.);
#7904=FACE_OUTER_BOUND('',#13784,.T.);
#7905=FACE_OUTER_BOUND('',#13785,.T.);
#7906=FACE_OUTER_BOUND('',#13786,.T.);
#7907=FACE_OUTER_BOUND('',#13788,.T.);
#7908=FACE_OUTER_BOUND('',#13789,.T.);
#7909=FACE_OUTER_BOUND('',#13790,.T.);
#7910=FACE_OUTER_BOUND('',#13792,.T.);
#7911=FACE_OUTER_BOUND('',#13793,.T.);
#7912=FACE_OUTER_BOUND('',#13794,.T.);
#7913=FACE_OUTER_BOUND('',#13795,.T.);
#7914=FACE_OUTER_BOUND('',#13796,.T.);
#7915=FACE_OUTER_BOUND('',#13797,.T.);
#7916=FACE_OUTER_BOUND('',#13798,.T.);
#7917=FACE_OUTER_BOUND('',#13799,.T.);
#7918=FACE_OUTER_BOUND('',#13800,.T.);
#7919=FACE_OUTER_BOUND('',#13801,.T.);
#7920=FACE_OUTER_BOUND('',#13802,.T.);
#7921=FACE_OUTER_BOUND('',#13803,.T.);
#7922=FACE_OUTER_BOUND('',#13804,.T.);
#7923=FACE_OUTER_BOUND('',#13805,.T.);
#7924=FACE_OUTER_BOUND('',#13806,.T.);
#7925=FACE_OUTER_BOUND('',#13807,.T.);
#7926=FACE_OUTER_BOUND('',#13808,.T.);
#7927=FACE_OUTER_BOUND('',#13809,.T.);
#7928=FACE_OUTER_BOUND('',#13810,.T.);
#7929=FACE_OUTER_BOUND('',#13811,.T.);
#7930=FACE_OUTER_BOUND('',#13812,.T.);
#7931=FACE_OUTER_BOUND('',#13813,.T.);
#7932=FACE_OUTER_BOUND('',#13814,.T.);
#7933=FACE_OUTER_BOUND('',#13815,.T.);
#7934=FACE_OUTER_BOUND('',#13816,.T.);
#7935=FACE_OUTER_BOUND('',#13817,.T.);
#7936=FACE_OUTER_BOUND('',#13818,.T.);
#7937=FACE_OUTER_BOUND('',#13819,.T.);
#7938=FACE_OUTER_BOUND('',#13820,.T.);
#7939=FACE_OUTER_BOUND('',#13821,.T.);
#7940=FACE_OUTER_BOUND('',#13822,.T.);
#7941=FACE_OUTER_BOUND('',#13823,.T.);
#7942=FACE_OUTER_BOUND('',#13824,.T.);
#7943=FACE_OUTER_BOUND('',#13825,.T.);
#7944=FACE_OUTER_BOUND('',#13826,.T.);
#7945=FACE_OUTER_BOUND('',#13827,.T.);
#7946=FACE_OUTER_BOUND('',#13828,.T.);
#7947=FACE_OUTER_BOUND('',#13829,.T.);
#7948=FACE_OUTER_BOUND('',#13830,.T.);
#7949=FACE_OUTER_BOUND('',#13831,.T.);
#7950=FACE_OUTER_BOUND('',#13832,.T.);
#7951=FACE_OUTER_BOUND('',#13833,.T.);
#7952=FACE_OUTER_BOUND('',#13834,.T.);
#7953=FACE_OUTER_BOUND('',#13835,.T.);
#7954=FACE_OUTER_BOUND('',#13836,.T.);
#7955=FACE_OUTER_BOUND('',#13837,.T.);
#7956=FACE_OUTER_BOUND('',#13838,.T.);
#7957=FACE_OUTER_BOUND('',#13839,.T.);
#7958=FACE_OUTER_BOUND('',#13840,.T.);
#7959=FACE_OUTER_BOUND('',#13841,.T.);
#7960=FACE_OUTER_BOUND('',#13842,.T.);
#7961=FACE_OUTER_BOUND('',#13843,.T.);
#7962=FACE_OUTER_BOUND('',#13844,.T.);
#7963=FACE_OUTER_BOUND('',#13845,.T.);
#7964=FACE_OUTER_BOUND('',#13846,.T.);
#7965=FACE_OUTER_BOUND('',#13847,.T.);
#7966=FACE_OUTER_BOUND('',#13848,.T.);
#7967=FACE_OUTER_BOUND('',#13849,.T.);
#7968=FACE_OUTER_BOUND('',#13850,.T.);
#7969=FACE_OUTER_BOUND('',#13851,.T.);
#7970=FACE_OUTER_BOUND('',#13852,.T.);
#7971=FACE_OUTER_BOUND('',#13853,.T.);
#7972=FACE_OUTER_BOUND('',#13854,.T.);
#7973=FACE_OUTER_BOUND('',#13855,.T.);
#7974=FACE_OUTER_BOUND('',#13856,.T.);
#7975=FACE_OUTER_BOUND('',#13857,.T.);
#7976=FACE_OUTER_BOUND('',#13858,.T.);
#7977=FACE_OUTER_BOUND('',#13859,.T.);
#7978=FACE_OUTER_BOUND('',#13860,.T.);
#7979=FACE_OUTER_BOUND('',#13861,.T.);
#7980=FACE_OUTER_BOUND('',#13862,.T.);
#7981=FACE_OUTER_BOUND('',#13863,.T.);
#7982=FACE_OUTER_BOUND('',#13864,.T.);
#7983=FACE_OUTER_BOUND('',#13865,.T.);
#7984=FACE_OUTER_BOUND('',#13866,.T.);
#7985=FACE_OUTER_BOUND('',#13867,.T.);
#7986=FACE_OUTER_BOUND('',#13868,.T.);
#7987=FACE_OUTER_BOUND('',#13869,.T.);
#7988=FACE_OUTER_BOUND('',#13870,.T.);
#7989=FACE_OUTER_BOUND('',#13871,.T.);
#7990=FACE_OUTER_BOUND('',#13872,.T.);
#7991=FACE_OUTER_BOUND('',#13873,.T.);
#7992=FACE_OUTER_BOUND('',#13874,.T.);
#7993=FACE_OUTER_BOUND('',#13875,.T.);
#7994=FACE_OUTER_BOUND('',#13876,.T.);
#7995=FACE_OUTER_BOUND('',#13877,.T.);
#7996=FACE_OUTER_BOUND('',#13878,.T.);
#7997=FACE_OUTER_BOUND('',#13879,.T.);
#7998=FACE_OUTER_BOUND('',#13880,.T.);
#7999=FACE_OUTER_BOUND('',#13881,.T.);
#8000=FACE_OUTER_BOUND('',#13882,.T.);
#8001=FACE_OUTER_BOUND('',#13883,.T.);
#8002=FACE_OUTER_BOUND('',#13884,.T.);
#8003=FACE_OUTER_BOUND('',#13885,.T.);
#8004=FACE_OUTER_BOUND('',#13886,.T.);
#8005=FACE_OUTER_BOUND('',#13887,.T.);
#8006=FACE_OUTER_BOUND('',#13888,.T.);
#8007=FACE_OUTER_BOUND('',#13889,.T.);
#8008=FACE_OUTER_BOUND('',#13890,.T.);
#8009=FACE_OUTER_BOUND('',#13891,.T.);
#8010=FACE_OUTER_BOUND('',#13892,.T.);
#8011=FACE_OUTER_BOUND('',#13893,.T.);
#8012=FACE_OUTER_BOUND('',#13894,.T.);
#8013=FACE_OUTER_BOUND('',#13895,.T.);
#8014=FACE_OUTER_BOUND('',#13896,.T.);
#8015=FACE_OUTER_BOUND('',#13897,.T.);
#8016=FACE_OUTER_BOUND('',#13898,.T.);
#8017=FACE_OUTER_BOUND('',#13899,.T.);
#8018=FACE_OUTER_BOUND('',#13900,.T.);
#8019=FACE_OUTER_BOUND('',#13901,.T.);
#8020=FACE_OUTER_BOUND('',#13902,.T.);
#8021=FACE_OUTER_BOUND('',#13903,.T.);
#8022=FACE_OUTER_BOUND('',#13904,.T.);
#8023=FACE_OUTER_BOUND('',#13905,.T.);
#8024=FACE_OUTER_BOUND('',#13906,.T.);
#8025=FACE_OUTER_BOUND('',#13907,.T.);
#8026=FACE_OUTER_BOUND('',#13908,.T.);
#8027=FACE_OUTER_BOUND('',#13909,.T.);
#8028=FACE_OUTER_BOUND('',#13910,.T.);
#8029=FACE_OUTER_BOUND('',#13911,.T.);
#8030=FACE_OUTER_BOUND('',#13912,.T.);
#8031=FACE_OUTER_BOUND('',#13913,.T.);
#8032=FACE_OUTER_BOUND('',#13914,.T.);
#8033=FACE_OUTER_BOUND('',#13915,.T.);
#8034=FACE_OUTER_BOUND('',#13916,.T.);
#8035=FACE_OUTER_BOUND('',#13917,.T.);
#8036=FACE_OUTER_BOUND('',#13918,.T.);
#8037=FACE_OUTER_BOUND('',#13919,.T.);
#8038=FACE_OUTER_BOUND('',#13920,.T.);
#8039=FACE_OUTER_BOUND('',#13921,.T.);
#8040=FACE_OUTER_BOUND('',#13922,.T.);
#8041=FACE_OUTER_BOUND('',#13923,.T.);
#8042=FACE_OUTER_BOUND('',#13924,.T.);
#8043=FACE_OUTER_BOUND('',#13925,.T.);
#8044=FACE_OUTER_BOUND('',#13926,.T.);
#8045=FACE_OUTER_BOUND('',#13927,.T.);
#8046=FACE_OUTER_BOUND('',#13928,.T.);
#8047=FACE_OUTER_BOUND('',#13929,.T.);
#8048=FACE_OUTER_BOUND('',#13930,.T.);
#8049=FACE_OUTER_BOUND('',#13931,.T.);
#8050=FACE_OUTER_BOUND('',#13932,.T.);
#8051=FACE_OUTER_BOUND('',#13933,.T.);
#8052=FACE_OUTER_BOUND('',#13934,.T.);
#8053=FACE_OUTER_BOUND('',#13935,.T.);
#8054=FACE_OUTER_BOUND('',#13936,.T.);
#8055=FACE_OUTER_BOUND('',#13937,.T.);
#8056=FACE_OUTER_BOUND('',#13938,.T.);
#8057=FACE_OUTER_BOUND('',#13939,.T.);
#8058=FACE_OUTER_BOUND('',#13940,.T.);
#8059=FACE_OUTER_BOUND('',#13941,.T.);
#8060=FACE_OUTER_BOUND('',#13942,.T.);
#8061=FACE_OUTER_BOUND('',#13943,.T.);
#8062=FACE_OUTER_BOUND('',#13944,.T.);
#8063=FACE_OUTER_BOUND('',#13945,.T.);
#8064=FACE_OUTER_BOUND('',#13946,.T.);
#8065=FACE_OUTER_BOUND('',#13947,.T.);
#8066=FACE_OUTER_BOUND('',#13948,.T.);
#8067=FACE_OUTER_BOUND('',#13949,.T.);
#8068=FACE_OUTER_BOUND('',#13950,.T.);
#8069=FACE_OUTER_BOUND('',#13951,.T.);
#8070=FACE_OUTER_BOUND('',#13952,.T.);
#8071=FACE_OUTER_BOUND('',#13953,.T.);
#8072=FACE_OUTER_BOUND('',#13954,.T.);
#8073=FACE_OUTER_BOUND('',#13955,.T.);
#8074=FACE_OUTER_BOUND('',#13956,.T.);
#8075=FACE_OUTER_BOUND('',#13957,.T.);
#8076=FACE_OUTER_BOUND('',#13958,.T.);
#8077=FACE_OUTER_BOUND('',#13959,.T.);
#8078=FACE_OUTER_BOUND('',#13960,.T.);
#8079=FACE_OUTER_BOUND('',#13961,.T.);
#8080=FACE_OUTER_BOUND('',#13962,.T.);
#8081=FACE_OUTER_BOUND('',#13963,.T.);
#8082=FACE_OUTER_BOUND('',#13964,.T.);
#8083=FACE_OUTER_BOUND('',#13965,.T.);
#8084=FACE_OUTER_BOUND('',#13966,.T.);
#8085=FACE_OUTER_BOUND('',#13967,.T.);
#8086=FACE_OUTER_BOUND('',#13968,.T.);
#8087=FACE_OUTER_BOUND('',#13969,.T.);
#8088=FACE_OUTER_BOUND('',#13970,.T.);
#8089=FACE_OUTER_BOUND('',#13971,.T.);
#8090=FACE_OUTER_BOUND('',#13972,.T.);
#8091=FACE_OUTER_BOUND('',#13973,.T.);
#8092=FACE_OUTER_BOUND('',#13974,.T.);
#8093=FACE_OUTER_BOUND('',#13975,.T.);
#8094=FACE_OUTER_BOUND('',#13976,.T.);
#8095=FACE_OUTER_BOUND('',#13977,.T.);
#8096=FACE_OUTER_BOUND('',#13978,.T.);
#8097=FACE_OUTER_BOUND('',#13979,.T.);
#8098=FACE_OUTER_BOUND('',#13980,.T.);
#8099=FACE_OUTER_BOUND('',#13981,.T.);
#8100=FACE_OUTER_BOUND('',#13982,.T.);
#8101=FACE_OUTER_BOUND('',#13983,.T.);
#8102=FACE_OUTER_BOUND('',#13984,.T.);
#8103=FACE_OUTER_BOUND('',#13985,.T.);
#8104=FACE_OUTER_BOUND('',#13986,.T.);
#8105=FACE_OUTER_BOUND('',#13987,.T.);
#8106=FACE_OUTER_BOUND('',#13988,.T.);
#8107=FACE_OUTER_BOUND('',#13989,.T.);
#8108=FACE_OUTER_BOUND('',#13990,.T.);
#8109=FACE_OUTER_BOUND('',#13991,.T.);
#8110=FACE_OUTER_BOUND('',#13992,.T.);
#8111=FACE_OUTER_BOUND('',#13993,.T.);
#8112=FACE_OUTER_BOUND('',#13994,.T.);
#8113=FACE_OUTER_BOUND('',#13995,.T.);
#8114=FACE_OUTER_BOUND('',#13997,.T.);
#8115=FACE_OUTER_BOUND('',#13998,.T.);
#8116=FACE_OUTER_BOUND('',#13999,.T.);
#8117=FACE_OUTER_BOUND('',#14000,.T.);
#8118=FACE_OUTER_BOUND('',#14001,.T.);
#8119=FACE_OUTER_BOUND('',#14002,.T.);
#8120=FACE_OUTER_BOUND('',#14003,.T.);
#8121=FACE_OUTER_BOUND('',#14005,.T.);
#8122=FACE_OUTER_BOUND('',#14006,.T.);
#8123=FACE_OUTER_BOUND('',#14007,.T.);
#8124=FACE_OUTER_BOUND('',#14008,.T.);
#8125=FACE_OUTER_BOUND('',#14009,.T.);
#8126=FACE_OUTER_BOUND('',#14011,.T.);
#8127=FACE_OUTER_BOUND('',#14012,.T.);
#8128=FACE_OUTER_BOUND('',#14014,.T.);
#8129=FACE_OUTER_BOUND('',#14015,.T.);
#8130=FACE_OUTER_BOUND('',#14016,.T.);
#8131=FACE_OUTER_BOUND('',#14017,.T.);
#8132=FACE_OUTER_BOUND('',#14018,.T.);
#8133=FACE_OUTER_BOUND('',#14019,.T.);
#8134=FACE_OUTER_BOUND('',#14020,.T.);
#8135=FACE_OUTER_BOUND('',#14021,.T.);
#8136=FACE_OUTER_BOUND('',#14022,.T.);
#8137=FACE_OUTER_BOUND('',#14023,.T.);
#8138=FACE_OUTER_BOUND('',#14024,.T.);
#8139=FACE_OUTER_BOUND('',#14025,.T.);
#8140=FACE_OUTER_BOUND('',#14026,.T.);
#8141=FACE_OUTER_BOUND('',#14027,.T.);
#8142=FACE_OUTER_BOUND('',#14028,.T.);
#8143=FACE_OUTER_BOUND('',#14029,.T.);
#8144=FACE_OUTER_BOUND('',#14030,.T.);
#8145=FACE_OUTER_BOUND('',#14031,.T.);
#8146=FACE_OUTER_BOUND('',#14032,.T.);
#8147=FACE_OUTER_BOUND('',#14033,.T.);
#8148=FACE_OUTER_BOUND('',#14034,.T.);
#8149=FACE_OUTER_BOUND('',#14035,.T.);
#8150=FACE_OUTER_BOUND('',#14036,.T.);
#8151=FACE_OUTER_BOUND('',#14037,.T.);
#8152=FACE_OUTER_BOUND('',#14038,.T.);
#8153=FACE_OUTER_BOUND('',#14039,.T.);
#8154=FACE_OUTER_BOUND('',#14040,.T.);
#8155=FACE_OUTER_BOUND('',#14041,.T.);
#8156=FACE_OUTER_BOUND('',#14042,.T.);
#8157=FACE_OUTER_BOUND('',#14043,.T.);
#8158=FACE_OUTER_BOUND('',#14044,.T.);
#8159=FACE_OUTER_BOUND('',#14045,.T.);
#8160=FACE_OUTER_BOUND('',#14046,.T.);
#8161=FACE_OUTER_BOUND('',#14047,.T.);
#8162=FACE_OUTER_BOUND('',#14048,.T.);
#8163=FACE_OUTER_BOUND('',#14049,.T.);
#8164=FACE_OUTER_BOUND('',#14050,.T.);
#8165=FACE_OUTER_BOUND('',#14051,.T.);
#8166=FACE_OUTER_BOUND('',#14052,.T.);
#8167=FACE_OUTER_BOUND('',#14053,.T.);
#8168=FACE_OUTER_BOUND('',#14054,.T.);
#8169=FACE_OUTER_BOUND('',#14055,.T.);
#8170=FACE_OUTER_BOUND('',#14056,.T.);
#8171=FACE_OUTER_BOUND('',#14057,.T.);
#8172=FACE_OUTER_BOUND('',#14058,.T.);
#8173=FACE_OUTER_BOUND('',#14059,.T.);
#8174=FACE_OUTER_BOUND('',#14060,.T.);
#8175=FACE_OUTER_BOUND('',#14061,.T.);
#8176=FACE_OUTER_BOUND('',#14062,.T.);
#8177=FACE_OUTER_BOUND('',#14063,.T.);
#8178=FACE_OUTER_BOUND('',#14064,.T.);
#8179=FACE_OUTER_BOUND('',#14065,.T.);
#8180=FACE_OUTER_BOUND('',#14067,.T.);
#8181=FACE_OUTER_BOUND('',#14068,.T.);
#8182=FACE_OUTER_BOUND('',#14069,.T.);
#8183=FACE_OUTER_BOUND('',#14070,.T.);
#8184=FACE_OUTER_BOUND('',#14071,.T.);
#8185=FACE_OUTER_BOUND('',#14072,.T.);
#8186=FACE_OUTER_BOUND('',#14073,.T.);
#8187=FACE_OUTER_BOUND('',#14074,.T.);
#8188=FACE_OUTER_BOUND('',#14075,.T.);
#8189=FACE_OUTER_BOUND('',#14076,.T.);
#8190=FACE_OUTER_BOUND('',#14077,.T.);
#8191=FACE_OUTER_BOUND('',#14078,.T.);
#8192=FACE_OUTER_BOUND('',#14079,.T.);
#8193=FACE_OUTER_BOUND('',#14080,.T.);
#8194=FACE_OUTER_BOUND('',#14081,.T.);
#8195=FACE_OUTER_BOUND('',#14082,.T.);
#8196=FACE_OUTER_BOUND('',#14083,.T.);
#8197=FACE_OUTER_BOUND('',#14084,.T.);
#8198=FACE_OUTER_BOUND('',#14085,.T.);
#8199=FACE_OUTER_BOUND('',#14086,.T.);
#8200=FACE_OUTER_BOUND('',#14087,.T.);
#8201=FACE_OUTER_BOUND('',#14088,.T.);
#8202=FACE_OUTER_BOUND('',#14089,.T.);
#8203=FACE_OUTER_BOUND('',#14090,.T.);
#8204=FACE_OUTER_BOUND('',#14091,.T.);
#8205=FACE_OUTER_BOUND('',#14092,.T.);
#8206=FACE_OUTER_BOUND('',#14093,.T.);
#8207=FACE_OUTER_BOUND('',#14094,.T.);
#8208=FACE_OUTER_BOUND('',#14095,.T.);
#8209=FACE_OUTER_BOUND('',#14096,.T.);
#8210=FACE_OUTER_BOUND('',#14097,.T.);
#8211=FACE_OUTER_BOUND('',#14098,.T.);
#8212=FACE_OUTER_BOUND('',#14099,.T.);
#8213=FACE_OUTER_BOUND('',#14100,.T.);
#8214=FACE_OUTER_BOUND('',#14101,.T.);
#8215=FACE_OUTER_BOUND('',#14102,.T.);
#8216=FACE_OUTER_BOUND('',#14103,.T.);
#8217=FACE_OUTER_BOUND('',#14104,.T.);
#8218=FACE_OUTER_BOUND('',#14105,.T.);
#8219=FACE_OUTER_BOUND('',#14106,.T.);
#8220=FACE_OUTER_BOUND('',#14107,.T.);
#8221=FACE_OUTER_BOUND('',#14108,.T.);
#8222=FACE_OUTER_BOUND('',#14109,.T.);
#8223=FACE_OUTER_BOUND('',#14110,.T.);
#8224=FACE_OUTER_BOUND('',#14111,.T.);
#8225=FACE_OUTER_BOUND('',#14112,.T.);
#8226=FACE_OUTER_BOUND('',#14113,.T.);
#8227=FACE_OUTER_BOUND('',#14114,.T.);
#8228=FACE_OUTER_BOUND('',#14115,.T.);
#8229=FACE_OUTER_BOUND('',#14116,.T.);
#8230=FACE_OUTER_BOUND('',#14117,.T.);
#8231=FACE_OUTER_BOUND('',#14118,.T.);
#8232=FACE_OUTER_BOUND('',#14119,.T.);
#8233=FACE_OUTER_BOUND('',#14121,.T.);
#8234=FACE_OUTER_BOUND('',#14122,.T.);
#8235=FACE_OUTER_BOUND('',#14124,.T.);
#8236=FACE_OUTER_BOUND('',#14132,.T.);
#8237=FACE_OUTER_BOUND('',#14133,.T.);
#8238=FACE_OUTER_BOUND('',#14141,.T.);
#8239=FACE_OUTER_BOUND('',#14142,.T.);
#8240=FACE_OUTER_BOUND('',#14144,.T.);
#8241=FACE_OUTER_BOUND('',#14145,.T.);
#8242=FACE_OUTER_BOUND('',#14146,.T.);
#8243=FACE_OUTER_BOUND('',#14147,.T.);
#8244=FACE_OUTER_BOUND('',#14148,.T.);
#8245=FACE_OUTER_BOUND('',#14149,.T.);
#8246=FACE_OUTER_BOUND('',#14150,.T.);
#8247=FACE_OUTER_BOUND('',#14151,.T.);
#8248=FACE_OUTER_BOUND('',#14152,.T.);
#8249=FACE_OUTER_BOUND('',#14153,.T.);
#8250=FACE_OUTER_BOUND('',#14154,.T.);
#8251=FACE_OUTER_BOUND('',#14155,.T.);
#8252=FACE_OUTER_BOUND('',#14156,.T.);
#8253=FACE_OUTER_BOUND('',#14157,.T.);
#8254=FACE_OUTER_BOUND('',#14158,.T.);
#8255=FACE_OUTER_BOUND('',#14159,.T.);
#8256=FACE_OUTER_BOUND('',#14160,.T.);
#8257=FACE_OUTER_BOUND('',#14161,.T.);
#8258=FACE_OUTER_BOUND('',#14162,.T.);
#8259=FACE_OUTER_BOUND('',#14163,.T.);
#8260=FACE_OUTER_BOUND('',#14164,.T.);
#8261=FACE_OUTER_BOUND('',#14165,.T.);
#8262=FACE_OUTER_BOUND('',#14166,.T.);
#8263=FACE_OUTER_BOUND('',#14167,.T.);
#8264=FACE_OUTER_BOUND('',#14168,.T.);
#8265=FACE_OUTER_BOUND('',#14169,.T.);
#8266=FACE_OUTER_BOUND('',#14170,.T.);
#8267=FACE_OUTER_BOUND('',#14171,.T.);
#8268=FACE_OUTER_BOUND('',#14172,.T.);
#8269=FACE_OUTER_BOUND('',#14173,.T.);
#8270=FACE_OUTER_BOUND('',#14174,.T.);
#8271=FACE_OUTER_BOUND('',#14175,.T.);
#8272=FACE_OUTER_BOUND('',#14176,.T.);
#8273=FACE_OUTER_BOUND('',#14177,.T.);
#8274=FACE_OUTER_BOUND('',#14178,.T.);
#8275=FACE_OUTER_BOUND('',#14179,.T.);
#8276=FACE_OUTER_BOUND('',#14180,.T.);
#8277=FACE_OUTER_BOUND('',#14181,.T.);
#8278=FACE_OUTER_BOUND('',#14182,.T.);
#8279=FACE_OUTER_BOUND('',#14183,.T.);
#8280=FACE_OUTER_BOUND('',#14184,.T.);
#8281=FACE_OUTER_BOUND('',#14185,.T.);
#8282=FACE_OUTER_BOUND('',#14186,.T.);
#8283=FACE_OUTER_BOUND('',#14187,.T.);
#8284=FACE_OUTER_BOUND('',#14188,.T.);
#8285=FACE_OUTER_BOUND('',#14189,.T.);
#8286=FACE_OUTER_BOUND('',#14190,.T.);
#8287=FACE_OUTER_BOUND('',#14191,.T.);
#8288=FACE_OUTER_BOUND('',#14192,.T.);
#8289=FACE_OUTER_BOUND('',#14193,.T.);
#8290=FACE_OUTER_BOUND('',#14194,.T.);
#8291=FACE_OUTER_BOUND('',#14195,.T.);
#8292=FACE_OUTER_BOUND('',#14196,.T.);
#8293=FACE_OUTER_BOUND('',#14197,.T.);
#8294=FACE_OUTER_BOUND('',#14198,.T.);
#8295=FACE_OUTER_BOUND('',#14199,.T.);
#8296=FACE_OUTER_BOUND('',#14200,.T.);
#8297=FACE_OUTER_BOUND('',#14201,.T.);
#8298=FACE_OUTER_BOUND('',#14202,.T.);
#8299=FACE_OUTER_BOUND('',#14203,.T.);
#8300=FACE_OUTER_BOUND('',#14204,.T.);
#8301=FACE_OUTER_BOUND('',#14205,.T.);
#8302=FACE_OUTER_BOUND('',#14206,.T.);
#8303=FACE_OUTER_BOUND('',#14207,.T.);
#8304=FACE_OUTER_BOUND('',#14208,.T.);
#8305=FACE_OUTER_BOUND('',#14209,.T.);
#8306=FACE_OUTER_BOUND('',#14210,.T.);
#8307=FACE_OUTER_BOUND('',#14211,.T.);
#8308=FACE_OUTER_BOUND('',#14212,.T.);
#8309=FACE_OUTER_BOUND('',#14213,.T.);
#8310=FACE_OUTER_BOUND('',#14214,.T.);
#8311=FACE_OUTER_BOUND('',#14215,.T.);
#8312=FACE_OUTER_BOUND('',#14216,.T.);
#8313=FACE_OUTER_BOUND('',#14217,.T.);
#8314=FACE_OUTER_BOUND('',#14218,.T.);
#8315=FACE_OUTER_BOUND('',#14219,.T.);
#8316=FACE_OUTER_BOUND('',#14220,.T.);
#8317=FACE_OUTER_BOUND('',#14221,.T.);
#8318=FACE_OUTER_BOUND('',#14222,.T.);
#8319=FACE_OUTER_BOUND('',#14223,.T.);
#8320=FACE_OUTER_BOUND('',#14224,.T.);
#8321=FACE_OUTER_BOUND('',#14225,.T.);
#8322=FACE_OUTER_BOUND('',#14226,.T.);
#8323=FACE_OUTER_BOUND('',#14227,.T.);
#8324=FACE_OUTER_BOUND('',#14228,.T.);
#8325=FACE_OUTER_BOUND('',#14229,.T.);
#8326=FACE_OUTER_BOUND('',#14230,.T.);
#8327=FACE_OUTER_BOUND('',#14231,.T.);
#8328=FACE_OUTER_BOUND('',#14232,.T.);
#8329=FACE_OUTER_BOUND('',#14233,.T.);
#8330=FACE_OUTER_BOUND('',#14234,.T.);
#8331=FACE_OUTER_BOUND('',#14235,.T.);
#8332=FACE_OUTER_BOUND('',#14236,.T.);
#8333=FACE_OUTER_BOUND('',#14237,.T.);
#8334=FACE_OUTER_BOUND('',#14238,.T.);
#8335=FACE_OUTER_BOUND('',#14239,.T.);
#8336=FACE_OUTER_BOUND('',#14240,.T.);
#8337=FACE_OUTER_BOUND('',#14241,.T.);
#8338=FACE_OUTER_BOUND('',#14242,.T.);
#8339=FACE_OUTER_BOUND('',#14243,.T.);
#8340=FACE_OUTER_BOUND('',#14244,.T.);
#8341=FACE_OUTER_BOUND('',#14245,.T.);
#8342=FACE_OUTER_BOUND('',#14246,.T.);
#8343=FACE_OUTER_BOUND('',#14247,.T.);
#8344=FACE_OUTER_BOUND('',#14248,.T.);
#8345=FACE_OUTER_BOUND('',#14249,.T.);
#8346=FACE_OUTER_BOUND('',#14250,.T.);
#8347=FACE_OUTER_BOUND('',#14251,.T.);
#8348=FACE_OUTER_BOUND('',#14252,.T.);
#8349=FACE_OUTER_BOUND('',#14253,.T.);
#8350=FACE_OUTER_BOUND('',#14254,.T.);
#8351=FACE_OUTER_BOUND('',#14255,.T.);
#8352=FACE_OUTER_BOUND('',#14256,.T.);
#8353=FACE_OUTER_BOUND('',#14257,.T.);
#8354=FACE_OUTER_BOUND('',#14258,.T.);
#8355=FACE_OUTER_BOUND('',#14259,.T.);
#8356=FACE_OUTER_BOUND('',#14260,.T.);
#8357=FACE_OUTER_BOUND('',#14261,.T.);
#8358=FACE_OUTER_BOUND('',#14262,.T.);
#8359=FACE_OUTER_BOUND('',#14263,.T.);
#8360=FACE_OUTER_BOUND('',#14264,.T.);
#8361=FACE_OUTER_BOUND('',#14265,.T.);
#8362=FACE_OUTER_BOUND('',#14266,.T.);
#8363=FACE_OUTER_BOUND('',#14267,.T.);
#8364=FACE_OUTER_BOUND('',#14268,.T.);
#8365=FACE_OUTER_BOUND('',#14269,.T.);
#8366=FACE_OUTER_BOUND('',#14270,.T.);
#8367=FACE_OUTER_BOUND('',#14271,.T.);
#8368=FACE_OUTER_BOUND('',#14272,.T.);
#8369=FACE_OUTER_BOUND('',#14273,.T.);
#8370=FACE_OUTER_BOUND('',#14274,.T.);
#8371=FACE_OUTER_BOUND('',#14275,.T.);
#8372=FACE_OUTER_BOUND('',#14276,.T.);
#8373=FACE_OUTER_BOUND('',#14277,.T.);
#8374=FACE_OUTER_BOUND('',#14278,.T.);
#8375=FACE_OUTER_BOUND('',#14279,.T.);
#8376=FACE_OUTER_BOUND('',#14280,.T.);
#8377=FACE_OUTER_BOUND('',#14281,.T.);
#8378=FACE_OUTER_BOUND('',#14283,.T.);
#8379=FACE_OUTER_BOUND('',#14284,.T.);
#8380=FACE_OUTER_BOUND('',#14285,.T.);
#8381=FACE_OUTER_BOUND('',#14286,.T.);
#8382=FACE_OUTER_BOUND('',#14287,.T.);
#8383=FACE_OUTER_BOUND('',#14289,.T.);
#8384=FACE_OUTER_BOUND('',#14291,.T.);
#8385=FACE_OUTER_BOUND('',#14293,.T.);
#8386=FACE_OUTER_BOUND('',#14294,.T.);
#8387=FACE_OUTER_BOUND('',#14295,.T.);
#8388=FACE_OUTER_BOUND('',#14296,.T.);
#8389=FACE_OUTER_BOUND('',#14297,.T.);
#8390=FACE_OUTER_BOUND('',#14298,.T.);
#8391=FACE_OUTER_BOUND('',#14299,.T.);
#8392=FACE_OUTER_BOUND('',#14300,.T.);
#8393=FACE_OUTER_BOUND('',#14301,.T.);
#8394=FACE_OUTER_BOUND('',#14302,.T.);
#8395=FACE_OUTER_BOUND('',#14303,.T.);
#8396=FACE_OUTER_BOUND('',#14304,.T.);
#8397=FACE_OUTER_BOUND('',#14305,.T.);
#8398=FACE_OUTER_BOUND('',#14306,.T.);
#8399=FACE_OUTER_BOUND('',#14307,.T.);
#8400=FACE_OUTER_BOUND('',#14308,.T.);
#8401=FACE_OUTER_BOUND('',#14309,.T.);
#8402=FACE_OUTER_BOUND('',#14310,.T.);
#8403=FACE_OUTER_BOUND('',#14311,.T.);
#8404=FACE_OUTER_BOUND('',#14312,.T.);
#8405=FACE_OUTER_BOUND('',#14313,.T.);
#8406=FACE_OUTER_BOUND('',#14314,.T.);
#8407=FACE_OUTER_BOUND('',#14315,.T.);
#8408=FACE_OUTER_BOUND('',#14316,.T.);
#8409=FACE_OUTER_BOUND('',#14317,.T.);
#8410=FACE_OUTER_BOUND('',#14318,.T.);
#8411=FACE_OUTER_BOUND('',#14319,.T.);
#8412=FACE_OUTER_BOUND('',#14320,.T.);
#8413=FACE_OUTER_BOUND('',#14321,.T.);
#8414=FACE_OUTER_BOUND('',#14322,.T.);
#8415=FACE_OUTER_BOUND('',#14324,.T.);
#8416=FACE_OUTER_BOUND('',#14326,.T.);
#8417=FACE_OUTER_BOUND('',#14327,.T.);
#8418=FACE_OUTER_BOUND('',#14328,.T.);
#8419=FACE_OUTER_BOUND('',#14329,.T.);
#8420=FACE_OUTER_BOUND('',#14330,.T.);
#8421=FACE_OUTER_BOUND('',#14331,.T.);
#8422=FACE_OUTER_BOUND('',#14332,.T.);
#8423=FACE_OUTER_BOUND('',#14334,.T.);
#8424=FACE_OUTER_BOUND('',#14336,.T.);
#8425=FACE_OUTER_BOUND('',#14337,.T.);
#8426=FACE_OUTER_BOUND('',#14338,.T.);
#8427=FACE_OUTER_BOUND('',#14339,.T.);
#8428=FACE_OUTER_BOUND('',#14340,.T.);
#8429=FACE_OUTER_BOUND('',#14341,.T.);
#8430=FACE_OUTER_BOUND('',#14342,.T.);
#8431=FACE_OUTER_BOUND('',#14343,.T.);
#8432=FACE_OUTER_BOUND('',#14344,.T.);
#8433=FACE_OUTER_BOUND('',#14345,.T.);
#8434=FACE_OUTER_BOUND('',#14346,.T.);
#8435=FACE_OUTER_BOUND('',#14347,.T.);
#8436=FACE_OUTER_BOUND('',#14348,.T.);
#8437=FACE_OUTER_BOUND('',#14349,.T.);
#8438=FACE_OUTER_BOUND('',#14350,.T.);
#8439=FACE_OUTER_BOUND('',#14352,.T.);
#8440=FACE_OUTER_BOUND('',#14354,.T.);
#8441=FACE_OUTER_BOUND('',#14355,.T.);
#8442=FACE_OUTER_BOUND('',#14356,.T.);
#8443=FACE_OUTER_BOUND('',#14358,.T.);
#8444=FACE_OUTER_BOUND('',#14360,.T.);
#8445=FACE_OUTER_BOUND('',#14361,.T.);
#8446=FACE_OUTER_BOUND('',#14362,.T.);
#8447=FACE_OUTER_BOUND('',#14363,.T.);
#8448=FACE_OUTER_BOUND('',#14364,.T.);
#8449=FACE_OUTER_BOUND('',#14365,.T.);
#8450=FACE_OUTER_BOUND('',#14366,.T.);
#8451=FACE_OUTER_BOUND('',#14367,.T.);
#8452=FACE_OUTER_BOUND('',#14368,.T.);
#8453=FACE_OUTER_BOUND('',#14369,.T.);
#8454=FACE_OUTER_BOUND('',#14370,.T.);
#8455=FACE_OUTER_BOUND('',#14371,.T.);
#8456=FACE_OUTER_BOUND('',#14372,.T.);
#8457=FACE_OUTER_BOUND('',#14373,.T.);
#8458=FACE_OUTER_BOUND('',#14374,.T.);
#8459=FACE_OUTER_BOUND('',#14375,.T.);
#8460=FACE_OUTER_BOUND('',#14376,.T.);
#8461=FACE_OUTER_BOUND('',#14377,.T.);
#8462=FACE_OUTER_BOUND('',#14378,.T.);
#8463=FACE_OUTER_BOUND('',#14379,.T.);
#8464=FACE_OUTER_BOUND('',#14380,.T.);
#8465=FACE_OUTER_BOUND('',#14381,.T.);
#8466=FACE_OUTER_BOUND('',#14382,.T.);
#8467=FACE_OUTER_BOUND('',#14383,.T.);
#8468=FACE_OUTER_BOUND('',#14384,.T.);
#8469=FACE_OUTER_BOUND('',#14385,.T.);
#8470=FACE_OUTER_BOUND('',#14386,.T.);
#8471=FACE_OUTER_BOUND('',#14387,.T.);
#8472=FACE_OUTER_BOUND('',#14388,.T.);
#8473=FACE_OUTER_BOUND('',#14389,.T.);
#8474=FACE_OUTER_BOUND('',#14390,.T.);
#8475=FACE_OUTER_BOUND('',#14391,.T.);
#8476=FACE_OUTER_BOUND('',#14392,.T.);
#8477=FACE_OUTER_BOUND('',#14394,.T.);
#8478=FACE_OUTER_BOUND('',#14395,.T.);
#8479=FACE_OUTER_BOUND('',#14396,.T.);
#8480=FACE_OUTER_BOUND('',#14397,.T.);
#8481=FACE_OUTER_BOUND('',#14398,.T.);
#8482=FACE_OUTER_BOUND('',#14400,.T.);
#8483=FACE_OUTER_BOUND('',#14402,.T.);
#8484=FACE_OUTER_BOUND('',#14404,.T.);
#8485=FACE_OUTER_BOUND('',#14405,.T.);
#8486=FACE_OUTER_BOUND('',#14406,.T.);
#8487=FACE_OUTER_BOUND('',#14407,.T.);
#8488=FACE_OUTER_BOUND('',#14408,.T.);
#8489=FACE_OUTER_BOUND('',#14409,.T.);
#8490=FACE_OUTER_BOUND('',#14410,.T.);
#8491=FACE_OUTER_BOUND('',#14411,.T.);
#8492=FACE_OUTER_BOUND('',#14412,.T.);
#8493=FACE_OUTER_BOUND('',#14413,.T.);
#8494=FACE_OUTER_BOUND('',#14414,.T.);
#8495=FACE_OUTER_BOUND('',#14415,.T.);
#8496=FACE_OUTER_BOUND('',#14416,.T.);
#8497=FACE_OUTER_BOUND('',#14417,.T.);
#8498=FACE_OUTER_BOUND('',#14418,.T.);
#8499=FACE_OUTER_BOUND('',#14419,.T.);
#8500=FACE_OUTER_BOUND('',#14420,.T.);
#8501=FACE_OUTER_BOUND('',#14421,.T.);
#8502=FACE_OUTER_BOUND('',#14422,.T.);
#8503=FACE_OUTER_BOUND('',#14423,.T.);
#8504=FACE_OUTER_BOUND('',#14424,.T.);
#8505=FACE_OUTER_BOUND('',#14425,.T.);
#8506=FACE_OUTER_BOUND('',#14426,.T.);
#8507=FACE_OUTER_BOUND('',#14427,.T.);
#8508=FACE_OUTER_BOUND('',#14428,.T.);
#8509=FACE_OUTER_BOUND('',#14429,.T.);
#8510=FACE_OUTER_BOUND('',#14430,.T.);
#8511=FACE_OUTER_BOUND('',#14431,.T.);
#8512=FACE_OUTER_BOUND('',#14432,.T.);
#8513=FACE_OUTER_BOUND('',#14433,.T.);
#8514=FACE_OUTER_BOUND('',#14434,.T.);
#8515=FACE_OUTER_BOUND('',#14435,.T.);
#8516=FACE_OUTER_BOUND('',#14436,.T.);
#8517=FACE_OUTER_BOUND('',#14437,.T.);
#8518=FACE_OUTER_BOUND('',#14438,.T.);
#8519=FACE_OUTER_BOUND('',#14439,.T.);
#8520=FACE_OUTER_BOUND('',#14440,.T.);
#8521=FACE_OUTER_BOUND('',#14441,.T.);
#8522=FACE_OUTER_BOUND('',#14442,.T.);
#8523=FACE_OUTER_BOUND('',#14443,.T.);
#8524=FACE_OUTER_BOUND('',#14444,.T.);
#8525=FACE_OUTER_BOUND('',#14445,.T.);
#8526=FACE_OUTER_BOUND('',#14446,.T.);
#8527=FACE_OUTER_BOUND('',#14447,.T.);
#8528=FACE_OUTER_BOUND('',#14448,.T.);
#8529=FACE_OUTER_BOUND('',#14449,.T.);
#8530=FACE_OUTER_BOUND('',#14450,.T.);
#8531=FACE_OUTER_BOUND('',#14451,.T.);
#8532=FACE_OUTER_BOUND('',#14452,.T.);
#8533=FACE_OUTER_BOUND('',#14453,.T.);
#8534=FACE_OUTER_BOUND('',#14455,.T.);
#8535=FACE_OUTER_BOUND('',#14456,.T.);
#8536=FACE_OUTER_BOUND('',#14457,.T.);
#8537=FACE_OUTER_BOUND('',#14458,.T.);
#8538=FACE_OUTER_BOUND('',#14459,.T.);
#8539=FACE_OUTER_BOUND('',#14460,.T.);
#8540=FACE_OUTER_BOUND('',#14461,.T.);
#8541=FACE_OUTER_BOUND('',#14462,.T.);
#8542=FACE_OUTER_BOUND('',#14463,.T.);
#8543=FACE_OUTER_BOUND('',#14464,.T.);
#8544=FACE_OUTER_BOUND('',#14465,.T.);
#8545=FACE_OUTER_BOUND('',#14466,.T.);
#8546=FACE_OUTER_BOUND('',#14467,.T.);
#8547=FACE_OUTER_BOUND('',#14468,.T.);
#8548=FACE_OUTER_BOUND('',#14469,.T.);
#8549=FACE_OUTER_BOUND('',#14470,.T.);
#8550=FACE_OUTER_BOUND('',#14471,.T.);
#8551=FACE_OUTER_BOUND('',#14472,.T.);
#8552=FACE_OUTER_BOUND('',#14473,.T.);
#8553=FACE_OUTER_BOUND('',#14474,.T.);
#8554=FACE_OUTER_BOUND('',#14475,.T.);
#8555=FACE_OUTER_BOUND('',#14476,.T.);
#8556=FACE_OUTER_BOUND('',#14477,.T.);
#8557=FACE_OUTER_BOUND('',#14478,.T.);
#8558=FACE_OUTER_BOUND('',#14479,.T.);
#8559=FACE_OUTER_BOUND('',#14480,.T.);
#8560=FACE_OUTER_BOUND('',#14481,.T.);
#8561=FACE_OUTER_BOUND('',#14482,.T.);
#8562=FACE_OUTER_BOUND('',#14483,.T.);
#8563=FACE_OUTER_BOUND('',#14484,.T.);
#8564=FACE_OUTER_BOUND('',#14485,.T.);
#8565=FACE_OUTER_BOUND('',#14486,.T.);
#8566=FACE_OUTER_BOUND('',#14487,.T.);
#8567=FACE_OUTER_BOUND('',#14488,.T.);
#8568=FACE_OUTER_BOUND('',#14489,.T.);
#8569=FACE_OUTER_BOUND('',#14490,.T.);
#8570=FACE_OUTER_BOUND('',#14491,.T.);
#8571=FACE_OUTER_BOUND('',#14492,.T.);
#8572=FACE_OUTER_BOUND('',#14493,.T.);
#8573=FACE_OUTER_BOUND('',#14494,.T.);
#8574=FACE_OUTER_BOUND('',#14495,.T.);
#8575=FACE_OUTER_BOUND('',#14496,.T.);
#8576=FACE_OUTER_BOUND('',#14497,.T.);
#8577=FACE_OUTER_BOUND('',#14498,.T.);
#8578=FACE_OUTER_BOUND('',#14499,.T.);
#8579=FACE_OUTER_BOUND('',#14500,.T.);
#8580=FACE_OUTER_BOUND('',#14501,.T.);
#8581=FACE_OUTER_BOUND('',#14502,.T.);
#8582=FACE_OUTER_BOUND('',#14503,.T.);
#8583=FACE_OUTER_BOUND('',#14504,.T.);
#8584=FACE_OUTER_BOUND('',#14505,.T.);
#8585=FACE_OUTER_BOUND('',#14506,.T.);
#8586=FACE_OUTER_BOUND('',#14507,.T.);
#8587=FACE_OUTER_BOUND('',#14508,.T.);
#8588=FACE_OUTER_BOUND('',#14509,.T.);
#8589=FACE_OUTER_BOUND('',#14510,.T.);
#8590=FACE_OUTER_BOUND('',#14511,.T.);
#8591=FACE_OUTER_BOUND('',#14512,.T.);
#8592=FACE_OUTER_BOUND('',#14513,.T.);
#8593=FACE_OUTER_BOUND('',#14514,.T.);
#8594=FACE_OUTER_BOUND('',#14515,.T.);
#8595=FACE_OUTER_BOUND('',#14516,.T.);
#8596=FACE_OUTER_BOUND('',#14517,.T.);
#8597=FACE_OUTER_BOUND('',#14518,.T.);
#8598=FACE_OUTER_BOUND('',#14519,.T.);
#8599=FACE_OUTER_BOUND('',#14520,.T.);
#8600=FACE_OUTER_BOUND('',#14521,.T.);
#8601=FACE_OUTER_BOUND('',#14522,.T.);
#8602=FACE_OUTER_BOUND('',#14523,.T.);
#8603=FACE_OUTER_BOUND('',#14524,.T.);
#8604=FACE_OUTER_BOUND('',#14525,.T.);
#8605=FACE_OUTER_BOUND('',#14526,.T.);
#8606=FACE_OUTER_BOUND('',#14527,.T.);
#8607=FACE_OUTER_BOUND('',#14528,.T.);
#8608=FACE_OUTER_BOUND('',#14529,.T.);
#8609=FACE_OUTER_BOUND('',#14530,.T.);
#8610=FACE_OUTER_BOUND('',#14531,.T.);
#8611=FACE_OUTER_BOUND('',#14532,.T.);
#8612=FACE_OUTER_BOUND('',#14533,.T.);
#8613=FACE_OUTER_BOUND('',#14534,.T.);
#8614=FACE_OUTER_BOUND('',#14535,.T.);
#8615=FACE_OUTER_BOUND('',#14536,.T.);
#8616=FACE_OUTER_BOUND('',#14537,.T.);
#8617=FACE_OUTER_BOUND('',#14538,.T.);
#8618=FACE_OUTER_BOUND('',#14539,.T.);
#8619=FACE_OUTER_BOUND('',#14540,.T.);
#8620=FACE_OUTER_BOUND('',#14541,.T.);
#8621=FACE_OUTER_BOUND('',#14542,.T.);
#8622=FACE_OUTER_BOUND('',#14543,.T.);
#8623=FACE_OUTER_BOUND('',#14544,.T.);
#8624=FACE_OUTER_BOUND('',#14545,.T.);
#8625=FACE_OUTER_BOUND('',#14546,.T.);
#8626=FACE_OUTER_BOUND('',#14547,.T.);
#8627=FACE_OUTER_BOUND('',#14548,.T.);
#8628=FACE_OUTER_BOUND('',#14549,.T.);
#8629=FACE_OUTER_BOUND('',#14550,.T.);
#8630=FACE_OUTER_BOUND('',#14551,.T.);
#8631=FACE_OUTER_BOUND('',#14552,.T.);
#8632=FACE_OUTER_BOUND('',#14553,.T.);
#8633=FACE_OUTER_BOUND('',#14554,.T.);
#8634=FACE_OUTER_BOUND('',#14555,.T.);
#8635=FACE_OUTER_BOUND('',#14556,.T.);
#8636=FACE_OUTER_BOUND('',#14557,.T.);
#8637=FACE_OUTER_BOUND('',#14558,.T.);
#8638=FACE_OUTER_BOUND('',#14559,.T.);
#8639=FACE_OUTER_BOUND('',#14560,.T.);
#8640=FACE_OUTER_BOUND('',#14561,.T.);
#8641=FACE_OUTER_BOUND('',#14562,.T.);
#8642=FACE_OUTER_BOUND('',#14563,.T.);
#8643=FACE_OUTER_BOUND('',#14564,.T.);
#8644=FACE_OUTER_BOUND('',#14565,.T.);
#8645=FACE_OUTER_BOUND('',#14566,.T.);
#8646=FACE_OUTER_BOUND('',#14567,.T.);
#8647=FACE_OUTER_BOUND('',#14568,.T.);
#8648=FACE_OUTER_BOUND('',#14569,.T.);
#8649=FACE_OUTER_BOUND('',#14570,.T.);
#8650=FACE_OUTER_BOUND('',#14571,.T.);
#8651=FACE_OUTER_BOUND('',#14572,.T.);
#8652=FACE_OUTER_BOUND('',#14573,.T.);
#8653=FACE_OUTER_BOUND('',#14574,.T.);
#8654=FACE_OUTER_BOUND('',#14575,.T.);
#8655=FACE_OUTER_BOUND('',#14576,.T.);
#8656=FACE_OUTER_BOUND('',#14577,.T.);
#8657=FACE_OUTER_BOUND('',#14578,.T.);
#8658=FACE_OUTER_BOUND('',#14579,.T.);
#8659=FACE_OUTER_BOUND('',#14580,.T.);
#8660=FACE_OUTER_BOUND('',#14581,.T.);
#8661=FACE_OUTER_BOUND('',#14582,.T.);
#8662=FACE_OUTER_BOUND('',#14583,.T.);
#8663=FACE_OUTER_BOUND('',#14584,.T.);
#8664=FACE_OUTER_BOUND('',#14585,.T.);
#8665=FACE_OUTER_BOUND('',#14586,.T.);
#8666=FACE_OUTER_BOUND('',#14587,.T.);
#8667=FACE_OUTER_BOUND('',#14588,.T.);
#8668=FACE_OUTER_BOUND('',#14589,.T.);
#8669=FACE_OUTER_BOUND('',#14590,.T.);
#8670=FACE_OUTER_BOUND('',#14591,.T.);
#8671=FACE_OUTER_BOUND('',#14592,.T.);
#8672=FACE_OUTER_BOUND('',#14593,.T.);
#8673=FACE_OUTER_BOUND('',#14594,.T.);
#8674=FACE_OUTER_BOUND('',#14595,.T.);
#8675=FACE_OUTER_BOUND('',#14596,.T.);
#8676=FACE_OUTER_BOUND('',#14597,.T.);
#8677=FACE_OUTER_BOUND('',#14598,.T.);
#8678=FACE_OUTER_BOUND('',#14599,.T.);
#8679=FACE_OUTER_BOUND('',#14600,.T.);
#8680=FACE_OUTER_BOUND('',#14601,.T.);
#8681=FACE_OUTER_BOUND('',#14602,.T.);
#8682=FACE_OUTER_BOUND('',#14603,.T.);
#8683=FACE_OUTER_BOUND('',#14604,.T.);
#8684=FACE_OUTER_BOUND('',#14605,.T.);
#8685=FACE_OUTER_BOUND('',#14606,.T.);
#8686=FACE_OUTER_BOUND('',#14607,.T.);
#8687=FACE_OUTER_BOUND('',#14608,.T.);
#8688=FACE_OUTER_BOUND('',#14609,.T.);
#8689=FACE_OUTER_BOUND('',#14610,.T.);
#8690=FACE_OUTER_BOUND('',#14611,.T.);
#8691=FACE_OUTER_BOUND('',#14612,.T.);
#8692=FACE_OUTER_BOUND('',#14613,.T.);
#8693=FACE_OUTER_BOUND('',#14614,.T.);
#8694=FACE_OUTER_BOUND('',#14615,.T.);
#8695=FACE_OUTER_BOUND('',#14616,.T.);
#8696=FACE_OUTER_BOUND('',#14617,.T.);
#8697=FACE_OUTER_BOUND('',#14618,.T.);
#8698=FACE_OUTER_BOUND('',#14619,.T.);
#8699=FACE_OUTER_BOUND('',#14620,.T.);
#8700=FACE_OUTER_BOUND('',#14621,.T.);
#8701=FACE_OUTER_BOUND('',#14622,.T.);
#8702=FACE_OUTER_BOUND('',#14623,.T.);
#8703=FACE_OUTER_BOUND('',#14624,.T.);
#8704=FACE_OUTER_BOUND('',#14625,.T.);
#8705=FACE_OUTER_BOUND('',#14626,.T.);
#8706=FACE_OUTER_BOUND('',#14627,.T.);
#8707=FACE_OUTER_BOUND('',#14628,.T.);
#8708=FACE_OUTER_BOUND('',#14629,.T.);
#8709=FACE_OUTER_BOUND('',#14630,.T.);
#8710=FACE_OUTER_BOUND('',#14631,.T.);
#8711=FACE_OUTER_BOUND('',#14632,.T.);
#8712=FACE_OUTER_BOUND('',#14633,.T.);
#8713=FACE_OUTER_BOUND('',#14634,.T.);
#8714=FACE_OUTER_BOUND('',#14635,.T.);
#8715=FACE_OUTER_BOUND('',#14636,.T.);
#8716=FACE_OUTER_BOUND('',#14637,.T.);
#8717=FACE_OUTER_BOUND('',#14638,.T.);
#8718=FACE_OUTER_BOUND('',#14639,.T.);
#8719=FACE_OUTER_BOUND('',#14640,.T.);
#8720=FACE_OUTER_BOUND('',#14641,.T.);
#8721=FACE_OUTER_BOUND('',#14642,.T.);
#8722=FACE_OUTER_BOUND('',#14643,.T.);
#8723=FACE_OUTER_BOUND('',#14644,.T.);
#8724=FACE_OUTER_BOUND('',#14645,.T.);
#8725=FACE_OUTER_BOUND('',#14646,.T.);
#8726=FACE_OUTER_BOUND('',#14647,.T.);
#8727=FACE_OUTER_BOUND('',#14648,.T.);
#8728=FACE_OUTER_BOUND('',#14650,.T.);
#8729=FACE_OUTER_BOUND('',#14651,.T.);
#8730=FACE_OUTER_BOUND('',#14652,.T.);
#8731=FACE_OUTER_BOUND('',#14653,.T.);
#8732=FACE_OUTER_BOUND('',#14654,.T.);
#8733=FACE_OUTER_BOUND('',#14655,.T.);
#8734=FACE_OUTER_BOUND('',#14656,.T.);
#8735=FACE_OUTER_BOUND('',#14657,.T.);
#8736=FACE_OUTER_BOUND('',#14658,.T.);
#8737=FACE_OUTER_BOUND('',#14659,.T.);
#8738=FACE_OUTER_BOUND('',#14660,.T.);
#8739=FACE_OUTER_BOUND('',#14661,.T.);
#8740=FACE_OUTER_BOUND('',#14662,.T.);
#8741=FACE_OUTER_BOUND('',#14663,.T.);
#8742=FACE_OUTER_BOUND('',#14665,.T.);
#8743=FACE_OUTER_BOUND('',#14666,.T.);
#8744=FACE_OUTER_BOUND('',#14667,.T.);
#8745=FACE_OUTER_BOUND('',#14668,.T.);
#8746=FACE_OUTER_BOUND('',#14669,.T.);
#8747=FACE_OUTER_BOUND('',#14670,.T.);
#8748=FACE_OUTER_BOUND('',#14671,.T.);
#8749=FACE_OUTER_BOUND('',#14672,.T.);
#8750=FACE_OUTER_BOUND('',#14673,.T.);
#8751=FACE_OUTER_BOUND('',#14674,.T.);
#8752=FACE_OUTER_BOUND('',#14675,.T.);
#8753=FACE_OUTER_BOUND('',#14676,.T.);
#8754=FACE_OUTER_BOUND('',#14677,.T.);
#8755=FACE_OUTER_BOUND('',#14678,.T.);
#8756=FACE_OUTER_BOUND('',#14679,.T.);
#8757=FACE_OUTER_BOUND('',#14680,.T.);
#8758=FACE_OUTER_BOUND('',#14681,.T.);
#8759=FACE_OUTER_BOUND('',#14682,.T.);
#8760=FACE_OUTER_BOUND('',#14683,.T.);
#8761=FACE_OUTER_BOUND('',#14684,.T.);
#8762=FACE_OUTER_BOUND('',#14685,.T.);
#8763=FACE_OUTER_BOUND('',#14686,.T.);
#8764=FACE_OUTER_BOUND('',#14687,.T.);
#8765=FACE_OUTER_BOUND('',#14688,.T.);
#8766=FACE_OUTER_BOUND('',#14689,.T.);
#8767=FACE_OUTER_BOUND('',#14690,.T.);
#8768=FACE_OUTER_BOUND('',#14691,.T.);
#8769=FACE_OUTER_BOUND('',#14692,.T.);
#8770=FACE_OUTER_BOUND('',#14693,.T.);
#8771=FACE_OUTER_BOUND('',#14694,.T.);
#8772=FACE_OUTER_BOUND('',#14695,.T.);
#8773=FACE_OUTER_BOUND('',#14696,.T.);
#8774=FACE_OUTER_BOUND('',#14697,.T.);
#8775=FACE_OUTER_BOUND('',#14698,.T.);
#8776=FACE_OUTER_BOUND('',#14699,.T.);
#8777=FACE_OUTER_BOUND('',#14700,.T.);
#8778=FACE_OUTER_BOUND('',#14701,.T.);
#8779=FACE_OUTER_BOUND('',#14702,.T.);
#8780=FACE_OUTER_BOUND('',#14703,.T.);
#8781=FACE_OUTER_BOUND('',#14704,.T.);
#8782=FACE_OUTER_BOUND('',#14705,.T.);
#8783=FACE_OUTER_BOUND('',#14706,.T.);
#8784=FACE_OUTER_BOUND('',#14707,.T.);
#8785=FACE_OUTER_BOUND('',#14708,.T.);
#8786=FACE_OUTER_BOUND('',#14709,.T.);
#8787=FACE_OUTER_BOUND('',#14710,.T.);
#8788=FACE_OUTER_BOUND('',#14711,.T.);
#8789=FACE_OUTER_BOUND('',#14712,.T.);
#8790=FACE_OUTER_BOUND('',#14713,.T.);
#8791=FACE_OUTER_BOUND('',#14714,.T.);
#8792=FACE_OUTER_BOUND('',#14715,.T.);
#8793=FACE_OUTER_BOUND('',#14716,.T.);
#8794=FACE_OUTER_BOUND('',#14717,.T.);
#8795=FACE_OUTER_BOUND('',#14718,.T.);
#8796=FACE_OUTER_BOUND('',#14719,.T.);
#8797=FACE_OUTER_BOUND('',#14720,.T.);
#8798=FACE_OUTER_BOUND('',#14721,.T.);
#8799=FACE_OUTER_BOUND('',#14722,.T.);
#8800=FACE_OUTER_BOUND('',#14723,.T.);
#8801=FACE_OUTER_BOUND('',#14724,.T.);
#8802=FACE_OUTER_BOUND('',#14725,.T.);
#8803=FACE_OUTER_BOUND('',#14726,.T.);
#8804=FACE_OUTER_BOUND('',#14727,.T.);
#8805=FACE_OUTER_BOUND('',#14728,.T.);
#8806=FACE_OUTER_BOUND('',#14729,.T.);
#8807=FACE_OUTER_BOUND('',#14730,.T.);
#8808=FACE_OUTER_BOUND('',#14731,.T.);
#8809=FACE_OUTER_BOUND('',#14732,.T.);
#8810=FACE_OUTER_BOUND('',#14733,.T.);
#8811=FACE_OUTER_BOUND('',#14734,.T.);
#8812=FACE_OUTER_BOUND('',#14735,.T.);
#8813=FACE_OUTER_BOUND('',#14736,.T.);
#8814=FACE_OUTER_BOUND('',#14737,.T.);
#8815=FACE_OUTER_BOUND('',#14738,.T.);
#8816=FACE_OUTER_BOUND('',#14739,.T.);
#8817=FACE_OUTER_BOUND('',#14740,.T.);
#8818=FACE_OUTER_BOUND('',#14741,.T.);
#8819=FACE_OUTER_BOUND('',#14742,.T.);
#8820=FACE_OUTER_BOUND('',#14743,.T.);
#8821=FACE_OUTER_BOUND('',#14744,.T.);
#8822=FACE_OUTER_BOUND('',#14745,.T.);
#8823=FACE_OUTER_BOUND('',#14746,.T.);
#8824=FACE_OUTER_BOUND('',#14747,.T.);
#8825=FACE_OUTER_BOUND('',#14748,.T.);
#8826=FACE_OUTER_BOUND('',#14749,.T.);
#8827=FACE_OUTER_BOUND('',#14750,.T.);
#8828=FACE_OUTER_BOUND('',#14751,.T.);
#8829=FACE_OUTER_BOUND('',#14752,.T.);
#8830=FACE_OUTER_BOUND('',#14753,.T.);
#8831=FACE_OUTER_BOUND('',#14754,.T.);
#8832=FACE_OUTER_BOUND('',#14755,.T.);
#8833=FACE_OUTER_BOUND('',#14756,.T.);
#8834=FACE_OUTER_BOUND('',#14757,.T.);
#8835=FACE_OUTER_BOUND('',#14758,.T.);
#8836=FACE_OUTER_BOUND('',#14759,.T.);
#8837=FACE_OUTER_BOUND('',#14760,.T.);
#8838=FACE_OUTER_BOUND('',#14761,.T.);
#8839=FACE_OUTER_BOUND('',#14762,.T.);
#8840=FACE_OUTER_BOUND('',#14763,.T.);
#8841=FACE_OUTER_BOUND('',#14764,.T.);
#8842=FACE_OUTER_BOUND('',#14765,.T.);
#8843=FACE_OUTER_BOUND('',#14766,.T.);
#8844=FACE_OUTER_BOUND('',#14767,.T.);
#8845=FACE_OUTER_BOUND('',#14768,.T.);
#8846=FACE_OUTER_BOUND('',#14769,.T.);
#8847=FACE_OUTER_BOUND('',#14770,.T.);
#8848=FACE_OUTER_BOUND('',#14771,.T.);
#8849=FACE_OUTER_BOUND('',#14772,.T.);
#8850=FACE_OUTER_BOUND('',#14773,.T.);
#8851=FACE_OUTER_BOUND('',#14774,.T.);
#8852=FACE_OUTER_BOUND('',#14775,.T.);
#8853=FACE_OUTER_BOUND('',#14776,.T.);
#8854=FACE_OUTER_BOUND('',#14777,.T.);
#8855=FACE_OUTER_BOUND('',#14778,.T.);
#8856=FACE_OUTER_BOUND('',#14779,.T.);
#8857=FACE_OUTER_BOUND('',#14780,.T.);
#8858=FACE_OUTER_BOUND('',#14781,.T.);
#8859=FACE_OUTER_BOUND('',#14782,.T.);
#8860=FACE_OUTER_BOUND('',#14783,.T.);
#8861=FACE_OUTER_BOUND('',#14784,.T.);
#8862=FACE_OUTER_BOUND('',#14785,.T.);
#8863=FACE_OUTER_BOUND('',#14786,.T.);
#8864=FACE_OUTER_BOUND('',#14787,.T.);
#8865=FACE_OUTER_BOUND('',#14788,.T.);
#8866=FACE_OUTER_BOUND('',#14789,.T.);
#8867=FACE_OUTER_BOUND('',#14790,.T.);
#8868=FACE_OUTER_BOUND('',#14791,.T.);
#8869=FACE_OUTER_BOUND('',#14792,.T.);
#8870=FACE_OUTER_BOUND('',#14793,.T.);
#8871=FACE_OUTER_BOUND('',#14794,.T.);
#8872=FACE_OUTER_BOUND('',#14795,.T.);
#8873=FACE_OUTER_BOUND('',#14796,.T.);
#8874=FACE_OUTER_BOUND('',#14797,.T.);
#8875=FACE_OUTER_BOUND('',#14798,.T.);
#8876=FACE_OUTER_BOUND('',#14799,.T.);
#8877=FACE_OUTER_BOUND('',#14800,.T.);
#8878=FACE_OUTER_BOUND('',#14801,.T.);
#8879=FACE_OUTER_BOUND('',#14802,.T.);
#8880=FACE_OUTER_BOUND('',#14803,.T.);
#8881=FACE_OUTER_BOUND('',#14804,.T.);
#8882=FACE_OUTER_BOUND('',#14805,.T.);
#8883=FACE_OUTER_BOUND('',#14806,.T.);
#8884=FACE_OUTER_BOUND('',#14807,.T.);
#8885=FACE_OUTER_BOUND('',#14808,.T.);
#8886=FACE_OUTER_BOUND('',#14809,.T.);
#8887=FACE_OUTER_BOUND('',#14810,.T.);
#8888=FACE_OUTER_BOUND('',#14811,.T.);
#8889=FACE_OUTER_BOUND('',#14812,.T.);
#8890=FACE_OUTER_BOUND('',#14813,.T.);
#8891=FACE_OUTER_BOUND('',#14814,.T.);
#8892=FACE_OUTER_BOUND('',#14815,.T.);
#8893=FACE_OUTER_BOUND('',#14816,.T.);
#8894=FACE_OUTER_BOUND('',#14817,.T.);
#8895=FACE_OUTER_BOUND('',#14818,.T.);
#8896=FACE_OUTER_BOUND('',#14819,.T.);
#8897=FACE_OUTER_BOUND('',#14820,.T.);
#8898=FACE_OUTER_BOUND('',#14821,.T.);
#8899=FACE_OUTER_BOUND('',#14822,.T.);
#8900=FACE_OUTER_BOUND('',#14823,.T.);
#8901=FACE_OUTER_BOUND('',#14824,.T.);
#8902=FACE_OUTER_BOUND('',#14825,.T.);
#8903=FACE_OUTER_BOUND('',#14826,.T.);
#8904=FACE_OUTER_BOUND('',#14827,.T.);
#8905=FACE_OUTER_BOUND('',#14828,.T.);
#8906=FACE_OUTER_BOUND('',#14829,.T.);
#8907=FACE_OUTER_BOUND('',#14830,.T.);
#8908=FACE_OUTER_BOUND('',#14831,.T.);
#8909=FACE_OUTER_BOUND('',#14832,.T.);
#8910=FACE_OUTER_BOUND('',#14833,.T.);
#8911=FACE_OUTER_BOUND('',#14834,.T.);
#8912=FACE_OUTER_BOUND('',#14835,.T.);
#8913=FACE_OUTER_BOUND('',#14836,.T.);
#8914=FACE_OUTER_BOUND('',#14837,.T.);
#8915=FACE_OUTER_BOUND('',#14838,.T.);
#8916=FACE_OUTER_BOUND('',#14839,.T.);
#8917=FACE_OUTER_BOUND('',#14840,.T.);
#8918=FACE_OUTER_BOUND('',#14841,.T.);
#8919=FACE_OUTER_BOUND('',#14842,.T.);
#8920=FACE_OUTER_BOUND('',#14843,.T.);
#8921=FACE_OUTER_BOUND('',#14844,.T.);
#8922=FACE_OUTER_BOUND('',#14845,.T.);
#8923=FACE_OUTER_BOUND('',#14846,.T.);
#8924=FACE_OUTER_BOUND('',#14847,.T.);
#8925=FACE_OUTER_BOUND('',#14848,.T.);
#8926=FACE_OUTER_BOUND('',#14849,.T.);
#8927=FACE_OUTER_BOUND('',#14850,.T.);
#8928=FACE_OUTER_BOUND('',#14851,.T.);
#8929=FACE_OUTER_BOUND('',#14852,.T.);
#8930=FACE_OUTER_BOUND('',#14853,.T.);
#8931=FACE_OUTER_BOUND('',#14854,.T.);
#8932=FACE_OUTER_BOUND('',#14855,.T.);
#8933=FACE_OUTER_BOUND('',#14856,.T.);
#8934=FACE_OUTER_BOUND('',#14857,.T.);
#8935=FACE_OUTER_BOUND('',#14858,.T.);
#8936=FACE_OUTER_BOUND('',#14859,.T.);
#8937=FACE_OUTER_BOUND('',#14860,.T.);
#8938=FACE_OUTER_BOUND('',#14861,.T.);
#8939=FACE_OUTER_BOUND('',#14862,.T.);
#8940=FACE_OUTER_BOUND('',#14863,.T.);
#8941=FACE_OUTER_BOUND('',#14864,.T.);
#8942=FACE_OUTER_BOUND('',#14865,.T.);
#8943=FACE_OUTER_BOUND('',#14866,.T.);
#8944=FACE_OUTER_BOUND('',#14867,.T.);
#8945=FACE_OUTER_BOUND('',#14868,.T.);
#8946=FACE_OUTER_BOUND('',#14869,.T.);
#8947=FACE_OUTER_BOUND('',#14870,.T.);
#8948=FACE_OUTER_BOUND('',#14871,.T.);
#8949=FACE_OUTER_BOUND('',#14872,.T.);
#8950=FACE_OUTER_BOUND('',#14873,.T.);
#8951=FACE_OUTER_BOUND('',#14874,.T.);
#8952=FACE_OUTER_BOUND('',#14875,.T.);
#8953=FACE_OUTER_BOUND('',#14876,.T.);
#8954=FACE_OUTER_BOUND('',#14877,.T.);
#8955=FACE_OUTER_BOUND('',#14878,.T.);
#8956=FACE_OUTER_BOUND('',#14879,.T.);
#8957=FACE_OUTER_BOUND('',#14880,.T.);
#8958=FACE_OUTER_BOUND('',#14881,.T.);
#8959=FACE_OUTER_BOUND('',#14882,.T.);
#8960=FACE_OUTER_BOUND('',#14883,.T.);
#8961=FACE_OUTER_BOUND('',#14884,.T.);
#8962=FACE_OUTER_BOUND('',#14885,.T.);
#8963=FACE_OUTER_BOUND('',#14886,.T.);
#8964=FACE_OUTER_BOUND('',#14887,.T.);
#8965=FACE_OUTER_BOUND('',#14888,.T.);
#8966=FACE_OUTER_BOUND('',#14889,.T.);
#8967=FACE_OUTER_BOUND('',#14890,.T.);
#8968=FACE_OUTER_BOUND('',#14891,.T.);
#8969=FACE_OUTER_BOUND('',#14892,.T.);
#8970=FACE_OUTER_BOUND('',#14893,.T.);
#8971=FACE_OUTER_BOUND('',#14894,.T.);
#8972=FACE_OUTER_BOUND('',#14895,.T.);
#8973=FACE_OUTER_BOUND('',#14896,.T.);
#8974=FACE_OUTER_BOUND('',#14897,.T.);
#8975=FACE_OUTER_BOUND('',#14898,.T.);
#8976=FACE_OUTER_BOUND('',#14899,.T.);
#8977=FACE_OUTER_BOUND('',#14900,.T.);
#8978=FACE_OUTER_BOUND('',#14901,.T.);
#8979=FACE_OUTER_BOUND('',#14902,.T.);
#8980=FACE_OUTER_BOUND('',#14903,.T.);
#8981=FACE_OUTER_BOUND('',#14904,.T.);
#8982=FACE_OUTER_BOUND('',#14905,.T.);
#8983=FACE_OUTER_BOUND('',#14906,.T.);
#8984=FACE_OUTER_BOUND('',#14907,.T.);
#8985=FACE_OUTER_BOUND('',#14908,.T.);
#8986=FACE_OUTER_BOUND('',#14909,.T.);
#8987=FACE_OUTER_BOUND('',#14910,.T.);
#8988=FACE_OUTER_BOUND('',#14911,.T.);
#8989=FACE_OUTER_BOUND('',#14912,.T.);
#8990=FACE_OUTER_BOUND('',#14913,.T.);
#8991=FACE_OUTER_BOUND('',#14914,.T.);
#8992=FACE_OUTER_BOUND('',#14915,.T.);
#8993=FACE_OUTER_BOUND('',#14916,.T.);
#8994=FACE_OUTER_BOUND('',#14917,.T.);
#8995=FACE_OUTER_BOUND('',#14918,.T.);
#8996=FACE_OUTER_BOUND('',#14919,.T.);
#8997=FACE_OUTER_BOUND('',#14920,.T.);
#8998=FACE_OUTER_BOUND('',#14921,.T.);
#8999=FACE_OUTER_BOUND('',#14922,.T.);
#9000=FACE_OUTER_BOUND('',#14923,.T.);
#9001=FACE_OUTER_BOUND('',#14924,.T.);
#9002=FACE_OUTER_BOUND('',#14925,.T.);
#9003=FACE_OUTER_BOUND('',#14926,.T.);
#9004=FACE_OUTER_BOUND('',#14927,.T.);
#9005=FACE_OUTER_BOUND('',#14928,.T.);
#9006=FACE_OUTER_BOUND('',#14929,.T.);
#9007=FACE_OUTER_BOUND('',#14930,.T.);
#9008=FACE_OUTER_BOUND('',#14931,.T.);
#9009=FACE_OUTER_BOUND('',#14932,.T.);
#9010=FACE_OUTER_BOUND('',#14933,.T.);
#9011=FACE_OUTER_BOUND('',#14934,.T.);
#9012=FACE_OUTER_BOUND('',#14935,.T.);
#9013=FACE_OUTER_BOUND('',#14936,.T.);
#9014=FACE_OUTER_BOUND('',#14937,.T.);
#9015=FACE_OUTER_BOUND('',#14938,.T.);
#9016=FACE_OUTER_BOUND('',#14939,.T.);
#9017=FACE_OUTER_BOUND('',#14940,.T.);
#9018=FACE_OUTER_BOUND('',#14941,.T.);
#9019=FACE_OUTER_BOUND('',#14942,.T.);
#9020=FACE_OUTER_BOUND('',#14943,.T.);
#9021=FACE_OUTER_BOUND('',#14944,.T.);
#9022=FACE_OUTER_BOUND('',#14945,.T.);
#9023=FACE_OUTER_BOUND('',#14946,.T.);
#9024=FACE_OUTER_BOUND('',#14947,.T.);
#9025=FACE_OUTER_BOUND('',#14948,.T.);
#9026=FACE_OUTER_BOUND('',#14949,.T.);
#9027=FACE_OUTER_BOUND('',#14950,.T.);
#9028=FACE_OUTER_BOUND('',#14951,.T.);
#9029=FACE_OUTER_BOUND('',#14952,.T.);
#9030=FACE_OUTER_BOUND('',#14953,.T.);
#9031=FACE_OUTER_BOUND('',#14954,.T.);
#9032=FACE_OUTER_BOUND('',#14955,.T.);
#9033=FACE_OUTER_BOUND('',#14956,.T.);
#9034=FACE_OUTER_BOUND('',#14957,.T.);
#9035=FACE_OUTER_BOUND('',#14958,.T.);
#9036=FACE_OUTER_BOUND('',#14959,.T.);
#9037=FACE_OUTER_BOUND('',#14960,.T.);
#9038=FACE_OUTER_BOUND('',#14961,.T.);
#9039=FACE_OUTER_BOUND('',#14962,.T.);
#9040=FACE_OUTER_BOUND('',#14963,.T.);
#9041=FACE_OUTER_BOUND('',#14964,.T.);
#9042=FACE_OUTER_BOUND('',#14965,.T.);
#9043=FACE_OUTER_BOUND('',#14966,.T.);
#9044=FACE_OUTER_BOUND('',#14967,.T.);
#9045=FACE_OUTER_BOUND('',#14968,.T.);
#9046=FACE_OUTER_BOUND('',#14969,.T.);
#9047=FACE_OUTER_BOUND('',#14970,.T.);
#9048=FACE_OUTER_BOUND('',#14971,.T.);
#9049=FACE_OUTER_BOUND('',#14972,.T.);
#9050=FACE_OUTER_BOUND('',#14973,.T.);
#9051=FACE_OUTER_BOUND('',#14974,.T.);
#9052=FACE_OUTER_BOUND('',#14975,.T.);
#9053=FACE_OUTER_BOUND('',#14976,.T.);
#9054=FACE_OUTER_BOUND('',#14977,.T.);
#9055=FACE_OUTER_BOUND('',#14978,.T.);
#9056=FACE_OUTER_BOUND('',#14979,.T.);
#9057=FACE_OUTER_BOUND('',#14980,.T.);
#9058=FACE_OUTER_BOUND('',#14981,.T.);
#9059=FACE_OUTER_BOUND('',#14982,.T.);
#9060=FACE_OUTER_BOUND('',#14983,.T.);
#9061=FACE_OUTER_BOUND('',#14984,.T.);
#9062=FACE_OUTER_BOUND('',#14985,.T.);
#9063=FACE_OUTER_BOUND('',#14986,.T.);
#9064=FACE_OUTER_BOUND('',#14987,.T.);
#9065=FACE_OUTER_BOUND('',#14988,.T.);
#9066=FACE_OUTER_BOUND('',#14989,.T.);
#9067=FACE_OUTER_BOUND('',#14990,.T.);
#9068=FACE_OUTER_BOUND('',#14991,.T.);
#9069=FACE_OUTER_BOUND('',#14992,.T.);
#9070=FACE_OUTER_BOUND('',#14993,.T.);
#9071=FACE_OUTER_BOUND('',#14994,.T.);
#9072=FACE_OUTER_BOUND('',#14995,.T.);
#9073=FACE_OUTER_BOUND('',#14996,.T.);
#9074=FACE_OUTER_BOUND('',#14997,.T.);
#9075=FACE_OUTER_BOUND('',#14998,.T.);
#9076=FACE_OUTER_BOUND('',#14999,.T.);
#9077=FACE_OUTER_BOUND('',#15000,.T.);
#9078=FACE_OUTER_BOUND('',#15001,.T.);
#9079=FACE_OUTER_BOUND('',#15002,.T.);
#9080=FACE_OUTER_BOUND('',#15003,.T.);
#9081=FACE_OUTER_BOUND('',#15004,.T.);
#9082=FACE_OUTER_BOUND('',#15005,.T.);
#9083=FACE_OUTER_BOUND('',#15006,.T.);
#9084=FACE_OUTER_BOUND('',#15007,.T.);
#9085=FACE_OUTER_BOUND('',#15008,.T.);
#9086=FACE_OUTER_BOUND('',#15009,.T.);
#9087=FACE_OUTER_BOUND('',#15010,.T.);
#9088=FACE_OUTER_BOUND('',#15011,.T.);
#9089=FACE_OUTER_BOUND('',#15012,.T.);
#9090=FACE_OUTER_BOUND('',#15013,.T.);
#9091=FACE_OUTER_BOUND('',#15014,.T.);
#9092=FACE_OUTER_BOUND('',#15015,.T.);
#9093=FACE_OUTER_BOUND('',#15016,.T.);
#9094=FACE_OUTER_BOUND('',#15017,.T.);
#9095=FACE_OUTER_BOUND('',#15018,.T.);
#9096=FACE_OUTER_BOUND('',#15019,.T.);
#9097=FACE_OUTER_BOUND('',#15020,.T.);
#9098=FACE_OUTER_BOUND('',#15021,.T.);
#9099=FACE_OUTER_BOUND('',#15022,.T.);
#9100=FACE_OUTER_BOUND('',#15023,.T.);
#9101=FACE_OUTER_BOUND('',#15024,.T.);
#9102=FACE_OUTER_BOUND('',#15025,.T.);
#9103=FACE_OUTER_BOUND('',#15026,.T.);
#9104=FACE_OUTER_BOUND('',#15027,.T.);
#9105=FACE_OUTER_BOUND('',#15028,.T.);
#9106=FACE_OUTER_BOUND('',#15029,.T.);
#9107=FACE_OUTER_BOUND('',#15030,.T.);
#9108=FACE_OUTER_BOUND('',#15031,.T.);
#9109=FACE_OUTER_BOUND('',#15032,.T.);
#9110=FACE_OUTER_BOUND('',#15033,.T.);
#9111=FACE_OUTER_BOUND('',#15034,.T.);
#9112=FACE_OUTER_BOUND('',#15035,.T.);
#9113=FACE_OUTER_BOUND('',#15036,.T.);
#9114=FACE_OUTER_BOUND('',#15037,.T.);
#9115=FACE_OUTER_BOUND('',#15038,.T.);
#9116=FACE_OUTER_BOUND('',#15039,.T.);
#9117=FACE_OUTER_BOUND('',#15040,.T.);
#9118=FACE_OUTER_BOUND('',#15041,.T.);
#9119=FACE_OUTER_BOUND('',#15042,.T.);
#9120=FACE_OUTER_BOUND('',#15043,.T.);
#9121=FACE_OUTER_BOUND('',#15044,.T.);
#9122=FACE_OUTER_BOUND('',#15045,.T.);
#9123=FACE_OUTER_BOUND('',#15046,.T.);
#9124=FACE_OUTER_BOUND('',#15047,.T.);
#9125=FACE_OUTER_BOUND('',#15048,.T.);
#9126=FACE_OUTER_BOUND('',#15049,.T.);
#9127=FACE_OUTER_BOUND('',#15050,.T.);
#9128=FACE_OUTER_BOUND('',#15051,.T.);
#9129=FACE_OUTER_BOUND('',#15052,.T.);
#9130=FACE_OUTER_BOUND('',#15053,.T.);
#9131=FACE_OUTER_BOUND('',#15054,.T.);
#9132=FACE_OUTER_BOUND('',#15055,.T.);
#9133=FACE_OUTER_BOUND('',#15056,.T.);
#9134=FACE_OUTER_BOUND('',#15057,.T.);
#9135=FACE_OUTER_BOUND('',#15058,.T.);
#9136=FACE_OUTER_BOUND('',#15059,.T.);
#9137=FACE_OUTER_BOUND('',#15060,.T.);
#9138=FACE_OUTER_BOUND('',#15061,.T.);
#9139=FACE_OUTER_BOUND('',#15062,.T.);
#9140=FACE_OUTER_BOUND('',#15063,.T.);
#9141=FACE_OUTER_BOUND('',#15064,.T.);
#9142=FACE_OUTER_BOUND('',#15065,.T.);
#9143=FACE_OUTER_BOUND('',#15066,.T.);
#9144=FACE_OUTER_BOUND('',#15067,.T.);
#9145=FACE_OUTER_BOUND('',#15068,.T.);
#9146=FACE_OUTER_BOUND('',#15069,.T.);
#9147=FACE_OUTER_BOUND('',#15070,.T.);
#9148=FACE_OUTER_BOUND('',#15071,.T.);
#9149=FACE_OUTER_BOUND('',#15072,.T.);
#9150=FACE_OUTER_BOUND('',#15073,.T.);
#9151=FACE_OUTER_BOUND('',#15074,.T.);
#9152=FACE_OUTER_BOUND('',#15075,.T.);
#9153=FACE_OUTER_BOUND('',#15076,.T.);
#9154=FACE_OUTER_BOUND('',#15077,.T.);
#9155=FACE_OUTER_BOUND('',#15078,.T.);
#9156=FACE_OUTER_BOUND('',#15079,.T.);
#9157=FACE_OUTER_BOUND('',#15080,.T.);
#9158=FACE_OUTER_BOUND('',#15081,.T.);
#9159=FACE_OUTER_BOUND('',#15082,.T.);
#9160=FACE_OUTER_BOUND('',#15083,.T.);
#9161=FACE_OUTER_BOUND('',#15084,.T.);
#9162=FACE_OUTER_BOUND('',#15085,.T.);
#9163=FACE_OUTER_BOUND('',#15086,.T.);
#9164=FACE_OUTER_BOUND('',#15087,.T.);
#9165=FACE_OUTER_BOUND('',#15088,.T.);
#9166=FACE_OUTER_BOUND('',#15089,.T.);
#9167=FACE_OUTER_BOUND('',#15090,.T.);
#9168=FACE_OUTER_BOUND('',#15091,.T.);
#9169=FACE_OUTER_BOUND('',#15092,.T.);
#9170=FACE_OUTER_BOUND('',#15093,.T.);
#9171=FACE_OUTER_BOUND('',#15094,.T.);
#9172=FACE_OUTER_BOUND('',#15095,.T.);
#9173=FACE_OUTER_BOUND('',#15096,.T.);
#9174=FACE_OUTER_BOUND('',#15097,.T.);
#9175=FACE_OUTER_BOUND('',#15098,.T.);
#9176=FACE_OUTER_BOUND('',#15099,.T.);
#9177=FACE_OUTER_BOUND('',#15100,.T.);
#9178=FACE_OUTER_BOUND('',#15101,.T.);
#9179=FACE_OUTER_BOUND('',#15102,.T.);
#9180=FACE_OUTER_BOUND('',#15103,.T.);
#9181=FACE_OUTER_BOUND('',#15104,.T.);
#9182=FACE_OUTER_BOUND('',#15105,.T.);
#9183=FACE_OUTER_BOUND('',#15106,.T.);
#9184=FACE_OUTER_BOUND('',#15107,.T.);
#9185=FACE_OUTER_BOUND('',#15108,.T.);
#9186=FACE_OUTER_BOUND('',#15109,.T.);
#9187=FACE_OUTER_BOUND('',#15110,.T.);
#9188=FACE_OUTER_BOUND('',#15111,.T.);
#9189=FACE_OUTER_BOUND('',#15112,.T.);
#9190=FACE_OUTER_BOUND('',#15113,.T.);
#9191=FACE_OUTER_BOUND('',#15114,.T.);
#9192=FACE_OUTER_BOUND('',#15115,.T.);
#9193=FACE_OUTER_BOUND('',#15116,.T.);
#9194=FACE_OUTER_BOUND('',#15117,.T.);
#9195=FACE_OUTER_BOUND('',#15118,.T.);
#9196=FACE_OUTER_BOUND('',#15119,.T.);
#9197=FACE_OUTER_BOUND('',#15120,.T.);
#9198=FACE_OUTER_BOUND('',#15121,.T.);
#9199=FACE_OUTER_BOUND('',#15122,.T.);
#9200=FACE_OUTER_BOUND('',#15123,.T.);
#9201=FACE_OUTER_BOUND('',#15124,.T.);
#9202=FACE_OUTER_BOUND('',#15125,.T.);
#9203=FACE_OUTER_BOUND('',#15126,.T.);
#9204=FACE_OUTER_BOUND('',#15127,.T.);
#9205=FACE_OUTER_BOUND('',#15128,.T.);
#9206=FACE_OUTER_BOUND('',#15129,.T.);
#9207=FACE_OUTER_BOUND('',#15130,.T.);
#9208=FACE_OUTER_BOUND('',#15131,.T.);
#9209=FACE_OUTER_BOUND('',#15132,.T.);
#9210=FACE_OUTER_BOUND('',#15133,.T.);
#9211=FACE_OUTER_BOUND('',#15134,.T.);
#9212=FACE_OUTER_BOUND('',#15135,.T.);
#9213=FACE_OUTER_BOUND('',#15136,.T.);
#9214=FACE_OUTER_BOUND('',#15137,.T.);
#9215=FACE_OUTER_BOUND('',#15138,.T.);
#9216=FACE_OUTER_BOUND('',#15139,.T.);
#9217=FACE_OUTER_BOUND('',#15140,.T.);
#9218=FACE_OUTER_BOUND('',#15141,.T.);
#9219=FACE_OUTER_BOUND('',#15142,.T.);
#9220=FACE_OUTER_BOUND('',#15143,.T.);
#9221=FACE_OUTER_BOUND('',#15144,.T.);
#9222=FACE_OUTER_BOUND('',#15145,.T.);
#9223=FACE_OUTER_BOUND('',#15146,.T.);
#9224=FACE_OUTER_BOUND('',#15147,.T.);
#9225=FACE_OUTER_BOUND('',#15148,.T.);
#9226=FACE_OUTER_BOUND('',#15149,.T.);
#9227=FACE_OUTER_BOUND('',#15150,.T.);
#9228=FACE_OUTER_BOUND('',#15151,.T.);
#9229=FACE_OUTER_BOUND('',#15152,.T.);
#9230=FACE_OUTER_BOUND('',#15153,.T.);
#9231=FACE_OUTER_BOUND('',#15154,.T.);
#9232=FACE_OUTER_BOUND('',#15155,.T.);
#9233=FACE_OUTER_BOUND('',#15156,.T.);
#9234=FACE_OUTER_BOUND('',#15157,.T.);
#9235=FACE_OUTER_BOUND('',#15158,.T.);
#9236=FACE_OUTER_BOUND('',#15159,.T.);
#9237=FACE_OUTER_BOUND('',#15160,.T.);
#9238=FACE_OUTER_BOUND('',#15161,.T.);
#9239=FACE_OUTER_BOUND('',#15162,.T.);
#9240=FACE_OUTER_BOUND('',#15163,.T.);
#9241=FACE_OUTER_BOUND('',#15164,.T.);
#9242=FACE_OUTER_BOUND('',#15165,.T.);
#9243=FACE_OUTER_BOUND('',#15166,.T.);
#9244=FACE_OUTER_BOUND('',#15167,.T.);
#9245=FACE_OUTER_BOUND('',#15168,.T.);
#9246=FACE_OUTER_BOUND('',#15169,.T.);
#9247=FACE_OUTER_BOUND('',#15170,.T.);
#9248=FACE_OUTER_BOUND('',#15171,.T.);
#9249=FACE_OUTER_BOUND('',#15172,.T.);
#9250=FACE_OUTER_BOUND('',#15173,.T.);
#9251=FACE_OUTER_BOUND('',#15174,.T.);
#9252=FACE_OUTER_BOUND('',#15175,.T.);
#9253=FACE_OUTER_BOUND('',#15176,.T.);
#9254=FACE_OUTER_BOUND('',#15177,.T.);
#9255=FACE_OUTER_BOUND('',#15178,.T.);
#9256=FACE_OUTER_BOUND('',#15179,.T.);
#9257=FACE_OUTER_BOUND('',#15180,.T.);
#9258=FACE_OUTER_BOUND('',#15181,.T.);
#9259=FACE_OUTER_BOUND('',#15182,.T.);
#9260=FACE_OUTER_BOUND('',#15183,.T.);
#9261=FACE_OUTER_BOUND('',#15184,.T.);
#9262=FACE_OUTER_BOUND('',#15185,.T.);
#9263=FACE_OUTER_BOUND('',#15186,.T.);
#9264=FACE_OUTER_BOUND('',#15187,.T.);
#9265=FACE_OUTER_BOUND('',#15188,.T.);
#9266=FACE_OUTER_BOUND('',#15189,.T.);
#9267=FACE_OUTER_BOUND('',#15190,.T.);
#9268=FACE_OUTER_BOUND('',#15191,.T.);
#9269=FACE_OUTER_BOUND('',#15192,.T.);
#9270=FACE_OUTER_BOUND('',#15193,.T.);
#9271=FACE_OUTER_BOUND('',#15194,.T.);
#9272=FACE_OUTER_BOUND('',#15195,.T.);
#9273=FACE_OUTER_BOUND('',#15196,.T.);
#9274=FACE_OUTER_BOUND('',#15197,.T.);
#9275=FACE_OUTER_BOUND('',#15198,.T.);
#9276=FACE_OUTER_BOUND('',#15199,.T.);
#9277=FACE_OUTER_BOUND('',#15200,.T.);
#9278=FACE_OUTER_BOUND('',#15201,.T.);
#9279=FACE_OUTER_BOUND('',#15202,.T.);
#9280=FACE_OUTER_BOUND('',#15203,.T.);
#9281=FACE_OUTER_BOUND('',#15204,.T.);
#9282=FACE_OUTER_BOUND('',#15205,.T.);
#9283=FACE_OUTER_BOUND('',#15206,.T.);
#9284=FACE_OUTER_BOUND('',#15207,.T.);
#9285=FACE_OUTER_BOUND('',#15208,.T.);
#9286=FACE_OUTER_BOUND('',#15209,.T.);
#9287=FACE_OUTER_BOUND('',#15210,.T.);
#9288=FACE_OUTER_BOUND('',#15211,.T.);
#9289=FACE_OUTER_BOUND('',#15212,.T.);
#9290=FACE_OUTER_BOUND('',#15213,.T.);
#9291=FACE_OUTER_BOUND('',#15214,.T.);
#9292=FACE_OUTER_BOUND('',#15215,.T.);
#9293=FACE_OUTER_BOUND('',#15216,.T.);
#9294=FACE_OUTER_BOUND('',#15217,.T.);
#9295=FACE_OUTER_BOUND('',#15218,.T.);
#9296=FACE_OUTER_BOUND('',#15219,.T.);
#9297=FACE_OUTER_BOUND('',#15220,.T.);
#9298=FACE_OUTER_BOUND('',#15221,.T.);
#9299=FACE_OUTER_BOUND('',#15222,.T.);
#9300=FACE_OUTER_BOUND('',#15223,.T.);
#9301=FACE_OUTER_BOUND('',#15224,.T.);
#9302=FACE_OUTER_BOUND('',#15225,.T.);
#9303=FACE_OUTER_BOUND('',#15226,.T.);
#9304=FACE_OUTER_BOUND('',#15227,.T.);
#9305=FACE_OUTER_BOUND('',#15228,.T.);
#9306=FACE_OUTER_BOUND('',#15229,.T.);
#9307=FACE_OUTER_BOUND('',#15230,.T.);
#9308=FACE_OUTER_BOUND('',#15231,.T.);
#9309=FACE_OUTER_BOUND('',#15232,.T.);
#9310=FACE_OUTER_BOUND('',#15233,.T.);
#9311=FACE_OUTER_BOUND('',#15234,.T.);
#9312=FACE_OUTER_BOUND('',#15235,.T.);
#9313=FACE_OUTER_BOUND('',#15236,.T.);
#9314=FACE_OUTER_BOUND('',#15237,.T.);
#9315=FACE_OUTER_BOUND('',#15238,.T.);
#9316=FACE_OUTER_BOUND('',#15239,.T.);
#9317=FACE_OUTER_BOUND('',#15240,.T.);
#9318=FACE_OUTER_BOUND('',#15241,.T.);
#9319=FACE_OUTER_BOUND('',#15242,.T.);
#9320=FACE_OUTER_BOUND('',#15243,.T.);
#9321=FACE_OUTER_BOUND('',#15244,.T.);
#9322=FACE_OUTER_BOUND('',#15245,.T.);
#9323=FACE_OUTER_BOUND('',#15246,.T.);
#9324=FACE_OUTER_BOUND('',#15247,.T.);
#9325=FACE_OUTER_BOUND('',#15248,.T.);
#9326=FACE_OUTER_BOUND('',#15249,.T.);
#9327=FACE_OUTER_BOUND('',#15250,.T.);
#9328=FACE_OUTER_BOUND('',#15251,.T.);
#9329=FACE_OUTER_BOUND('',#15252,.T.);
#9330=FACE_OUTER_BOUND('',#15253,.T.);
#9331=FACE_OUTER_BOUND('',#15254,.T.);
#9332=FACE_OUTER_BOUND('',#15255,.T.);
#9333=FACE_OUTER_BOUND('',#15256,.T.);
#9334=FACE_OUTER_BOUND('',#15257,.T.);
#9335=FACE_OUTER_BOUND('',#15258,.T.);
#9336=FACE_OUTER_BOUND('',#15259,.T.);
#9337=FACE_OUTER_BOUND('',#15260,.T.);
#9338=FACE_OUTER_BOUND('',#15261,.T.);
#9339=FACE_OUTER_BOUND('',#15262,.T.);
#9340=FACE_OUTER_BOUND('',#15263,.T.);
#9341=FACE_OUTER_BOUND('',#15264,.T.);
#9342=FACE_OUTER_BOUND('',#15265,.T.);
#9343=FACE_OUTER_BOUND('',#15266,.T.);
#9344=FACE_OUTER_BOUND('',#15267,.T.);
#9345=FACE_OUTER_BOUND('',#15268,.T.);
#9346=FACE_OUTER_BOUND('',#15269,.T.);
#9347=FACE_OUTER_BOUND('',#15270,.T.);
#9348=FACE_OUTER_BOUND('',#15271,.T.);
#9349=FACE_OUTER_BOUND('',#15272,.T.);
#9350=FACE_OUTER_BOUND('',#15273,.T.);
#9351=FACE_OUTER_BOUND('',#15274,.T.);
#9352=FACE_OUTER_BOUND('',#15275,.T.);
#9353=FACE_OUTER_BOUND('',#15276,.T.);
#9354=FACE_OUTER_BOUND('',#15277,.T.);
#9355=FACE_OUTER_BOUND('',#15278,.T.);
#9356=FACE_OUTER_BOUND('',#15279,.T.);
#9357=FACE_OUTER_BOUND('',#15280,.T.);
#9358=FACE_OUTER_BOUND('',#15281,.T.);
#9359=FACE_OUTER_BOUND('',#15282,.T.);
#9360=FACE_OUTER_BOUND('',#15283,.T.);
#9361=FACE_OUTER_BOUND('',#15284,.T.);
#9362=FACE_OUTER_BOUND('',#15285,.T.);
#9363=FACE_OUTER_BOUND('',#15286,.T.);
#9364=FACE_OUTER_BOUND('',#15287,.T.);
#9365=FACE_OUTER_BOUND('',#15288,.T.);
#9366=FACE_OUTER_BOUND('',#15289,.T.);
#9367=FACE_OUTER_BOUND('',#15290,.T.);
#9368=FACE_OUTER_BOUND('',#15291,.T.);
#9369=FACE_OUTER_BOUND('',#15292,.T.);
#9370=FACE_OUTER_BOUND('',#15293,.T.);
#9371=FACE_OUTER_BOUND('',#15294,.T.);
#9372=FACE_OUTER_BOUND('',#15295,.T.);
#9373=FACE_OUTER_BOUND('',#15296,.T.);
#9374=FACE_OUTER_BOUND('',#15297,.T.);
#9375=FACE_OUTER_BOUND('',#15298,.T.);
#9376=FACE_OUTER_BOUND('',#15299,.T.);
#9377=FACE_OUTER_BOUND('',#15300,.T.);
#9378=FACE_OUTER_BOUND('',#15301,.T.);
#9379=FACE_OUTER_BOUND('',#15302,.T.);
#9380=FACE_OUTER_BOUND('',#15303,.T.);
#9381=FACE_OUTER_BOUND('',#15304,.T.);
#9382=FACE_OUTER_BOUND('',#15305,.T.);
#9383=FACE_OUTER_BOUND('',#15306,.T.);
#9384=FACE_OUTER_BOUND('',#15307,.T.);
#9385=FACE_OUTER_BOUND('',#15308,.T.);
#9386=FACE_OUTER_BOUND('',#15309,.T.);
#9387=FACE_OUTER_BOUND('',#15310,.T.);
#9388=FACE_OUTER_BOUND('',#15311,.T.);
#9389=FACE_OUTER_BOUND('',#15312,.T.);
#9390=FACE_OUTER_BOUND('',#15313,.T.);
#9391=FACE_OUTER_BOUND('',#15314,.T.);
#9392=FACE_OUTER_BOUND('',#15315,.T.);
#9393=FACE_OUTER_BOUND('',#15316,.T.);
#9394=FACE_OUTER_BOUND('',#15317,.T.);
#9395=FACE_OUTER_BOUND('',#15318,.T.);
#9396=FACE_OUTER_BOUND('',#15319,.T.);
#9397=FACE_OUTER_BOUND('',#15320,.T.);
#9398=FACE_OUTER_BOUND('',#15321,.T.);
#9399=FACE_OUTER_BOUND('',#15322,.T.);
#9400=FACE_OUTER_BOUND('',#15323,.T.);
#9401=FACE_OUTER_BOUND('',#15324,.T.);
#9402=FACE_OUTER_BOUND('',#15325,.T.);
#9403=FACE_OUTER_BOUND('',#15326,.T.);
#9404=FACE_OUTER_BOUND('',#15327,.T.);
#9405=FACE_OUTER_BOUND('',#15328,.T.);
#9406=FACE_OUTER_BOUND('',#15329,.T.);
#9407=FACE_OUTER_BOUND('',#15330,.T.);
#9408=FACE_OUTER_BOUND('',#15331,.T.);
#9409=FACE_OUTER_BOUND('',#15332,.T.);
#9410=FACE_OUTER_BOUND('',#15333,.T.);
#9411=FACE_OUTER_BOUND('',#15334,.T.);
#9412=FACE_OUTER_BOUND('',#15335,.T.);
#9413=FACE_OUTER_BOUND('',#15336,.T.);
#9414=FACE_OUTER_BOUND('',#15337,.T.);
#9415=FACE_OUTER_BOUND('',#15338,.T.);
#9416=FACE_OUTER_BOUND('',#15339,.T.);
#9417=FACE_OUTER_BOUND('',#15340,.T.);
#9418=FACE_OUTER_BOUND('',#15341,.T.);
#9419=FACE_OUTER_BOUND('',#15342,.T.);
#9420=FACE_OUTER_BOUND('',#15343,.T.);
#9421=FACE_OUTER_BOUND('',#15344,.T.);
#9422=FACE_OUTER_BOUND('',#15345,.T.);
#9423=FACE_OUTER_BOUND('',#15346,.T.);
#9424=FACE_OUTER_BOUND('',#15347,.T.);
#9425=FACE_OUTER_BOUND('',#15348,.T.);
#9426=FACE_OUTER_BOUND('',#15349,.T.);
#9427=FACE_OUTER_BOUND('',#15350,.T.);
#9428=FACE_OUTER_BOUND('',#15351,.T.);
#9429=FACE_OUTER_BOUND('',#15352,.T.);
#9430=FACE_OUTER_BOUND('',#15353,.T.);
#9431=FACE_OUTER_BOUND('',#15354,.T.);
#9432=FACE_OUTER_BOUND('',#15355,.T.);
#9433=FACE_OUTER_BOUND('',#15356,.T.);
#9434=FACE_OUTER_BOUND('',#15357,.T.);
#9435=FACE_OUTER_BOUND('',#15358,.T.);
#9436=FACE_OUTER_BOUND('',#15359,.T.);
#9437=FACE_OUTER_BOUND('',#15360,.T.);
#9438=FACE_OUTER_BOUND('',#15361,.T.);
#9439=FACE_OUTER_BOUND('',#15362,.T.);
#9440=FACE_OUTER_BOUND('',#15363,.T.);
#9441=FACE_OUTER_BOUND('',#15364,.T.);
#9442=FACE_OUTER_BOUND('',#15365,.T.);
#9443=FACE_OUTER_BOUND('',#15366,.T.);
#9444=FACE_OUTER_BOUND('',#15367,.T.);
#9445=FACE_OUTER_BOUND('',#15368,.T.);
#9446=FACE_OUTER_BOUND('',#15369,.T.);
#9447=FACE_OUTER_BOUND('',#15370,.T.);
#9448=FACE_OUTER_BOUND('',#15371,.T.);
#9449=FACE_OUTER_BOUND('',#15372,.T.);
#9450=FACE_OUTER_BOUND('',#15373,.T.);
#9451=FACE_OUTER_BOUND('',#15374,.T.);
#9452=FACE_OUTER_BOUND('',#15375,.T.);
#9453=FACE_OUTER_BOUND('',#15376,.T.);
#9454=FACE_OUTER_BOUND('',#15377,.T.);
#9455=FACE_OUTER_BOUND('',#15378,.T.);
#9456=FACE_OUTER_BOUND('',#15379,.T.);
#9457=FACE_OUTER_BOUND('',#15380,.T.);
#9458=FACE_OUTER_BOUND('',#15381,.T.);
#9459=FACE_OUTER_BOUND('',#15382,.T.);
#9460=FACE_OUTER_BOUND('',#15383,.T.);
#9461=FACE_OUTER_BOUND('',#15384,.T.);
#9462=FACE_OUTER_BOUND('',#15385,.T.);
#9463=FACE_OUTER_BOUND('',#15386,.T.);
#9464=FACE_OUTER_BOUND('',#15387,.T.);
#9465=FACE_OUTER_BOUND('',#15388,.T.);
#9466=FACE_OUTER_BOUND('',#15389,.T.);
#9467=FACE_OUTER_BOUND('',#15390,.T.);
#9468=FACE_OUTER_BOUND('',#15391,.T.);
#9469=FACE_OUTER_BOUND('',#15392,.T.);
#9470=FACE_OUTER_BOUND('',#15393,.T.);
#9471=FACE_OUTER_BOUND('',#15394,.T.);
#9472=FACE_OUTER_BOUND('',#15395,.T.);
#9473=FACE_OUTER_BOUND('',#15396,.T.);
#9474=FACE_OUTER_BOUND('',#15397,.T.);
#9475=FACE_OUTER_BOUND('',#15398,.T.);
#9476=FACE_OUTER_BOUND('',#15399,.T.);
#9477=FACE_OUTER_BOUND('',#15400,.T.);
#9478=FACE_OUTER_BOUND('',#15401,.T.);
#9479=FACE_OUTER_BOUND('',#15402,.T.);
#9480=FACE_OUTER_BOUND('',#15403,.T.);
#9481=FACE_OUTER_BOUND('',#15404,.T.);
#9482=FACE_OUTER_BOUND('',#15405,.T.);
#9483=FACE_OUTER_BOUND('',#15406,.T.);
#9484=FACE_OUTER_BOUND('',#15407,.T.);
#9485=FACE_OUTER_BOUND('',#15408,.T.);
#9486=FACE_OUTER_BOUND('',#15409,.T.);
#9487=FACE_OUTER_BOUND('',#15410,.T.);
#9488=FACE_OUTER_BOUND('',#15411,.T.);
#9489=FACE_OUTER_BOUND('',#15412,.T.);
#9490=FACE_OUTER_BOUND('',#15413,.T.);
#9491=FACE_OUTER_BOUND('',#15414,.T.);
#9492=FACE_OUTER_BOUND('',#15415,.T.);
#9493=FACE_OUTER_BOUND('',#15416,.T.);
#9494=FACE_OUTER_BOUND('',#15417,.T.);
#9495=FACE_OUTER_BOUND('',#15418,.T.);
#9496=FACE_OUTER_BOUND('',#15419,.T.);
#9497=FACE_OUTER_BOUND('',#15420,.T.);
#9498=FACE_OUTER_BOUND('',#15421,.T.);
#9499=FACE_OUTER_BOUND('',#15422,.T.);
#9500=FACE_OUTER_BOUND('',#15423,.T.);
#9501=FACE_OUTER_BOUND('',#15424,.T.);
#9502=FACE_OUTER_BOUND('',#15425,.T.);
#9503=FACE_OUTER_BOUND('',#15426,.T.);
#9504=FACE_OUTER_BOUND('',#15427,.T.);
#9505=FACE_OUTER_BOUND('',#15428,.T.);
#9506=FACE_OUTER_BOUND('',#15429,.T.);
#9507=FACE_OUTER_BOUND('',#15430,.T.);
#9508=FACE_OUTER_BOUND('',#15431,.T.);
#9509=FACE_OUTER_BOUND('',#15432,.T.);
#9510=FACE_OUTER_BOUND('',#15433,.T.);
#9511=FACE_OUTER_BOUND('',#15434,.T.);
#9512=FACE_OUTER_BOUND('',#15435,.T.);
#9513=FACE_OUTER_BOUND('',#15436,.T.);
#9514=FACE_OUTER_BOUND('',#15437,.T.);
#9515=FACE_OUTER_BOUND('',#15438,.T.);
#9516=FACE_OUTER_BOUND('',#15439,.T.);
#9517=FACE_OUTER_BOUND('',#15440,.T.);
#9518=FACE_OUTER_BOUND('',#15441,.T.);
#9519=FACE_OUTER_BOUND('',#15442,.T.);
#9520=FACE_OUTER_BOUND('',#15443,.T.);
#9521=FACE_OUTER_BOUND('',#15444,.T.);
#9522=FACE_OUTER_BOUND('',#15445,.T.);
#9523=FACE_OUTER_BOUND('',#15446,.T.);
#9524=FACE_OUTER_BOUND('',#15447,.T.);
#9525=FACE_OUTER_BOUND('',#15448,.T.);
#9526=FACE_OUTER_BOUND('',#15449,.T.);
#9527=FACE_OUTER_BOUND('',#15450,.T.);
#9528=FACE_OUTER_BOUND('',#15451,.T.);
#9529=FACE_OUTER_BOUND('',#15452,.T.);
#9530=FACE_OUTER_BOUND('',#15453,.T.);
#9531=FACE_OUTER_BOUND('',#15454,.T.);
#9532=FACE_OUTER_BOUND('',#15455,.T.);
#9533=FACE_OUTER_BOUND('',#15456,.T.);
#9534=FACE_OUTER_BOUND('',#15457,.T.);
#9535=FACE_OUTER_BOUND('',#15458,.T.);
#9536=FACE_OUTER_BOUND('',#15459,.T.);
#9537=FACE_OUTER_BOUND('',#15460,.T.);
#9538=FACE_OUTER_BOUND('',#15461,.T.);
#9539=FACE_OUTER_BOUND('',#15462,.T.);
#9540=FACE_OUTER_BOUND('',#15463,.T.);
#9541=FACE_OUTER_BOUND('',#15464,.T.);
#9542=FACE_OUTER_BOUND('',#15465,.T.);
#9543=FACE_OUTER_BOUND('',#15466,.T.);
#9544=FACE_OUTER_BOUND('',#15467,.T.);
#9545=FACE_OUTER_BOUND('',#15468,.T.);
#9546=FACE_OUTER_BOUND('',#15469,.T.);
#9547=FACE_OUTER_BOUND('',#15470,.T.);
#9548=FACE_OUTER_BOUND('',#15471,.T.);
#9549=FACE_OUTER_BOUND('',#15472,.T.);
#9550=FACE_OUTER_BOUND('',#15473,.T.);
#9551=FACE_OUTER_BOUND('',#15474,.T.);
#9552=FACE_OUTER_BOUND('',#15475,.T.);
#9553=FACE_OUTER_BOUND('',#15476,.T.);
#9554=FACE_OUTER_BOUND('',#15477,.T.);
#9555=FACE_OUTER_BOUND('',#15478,.T.);
#9556=FACE_OUTER_BOUND('',#15479,.T.);
#9557=FACE_OUTER_BOUND('',#15480,.T.);
#9558=FACE_OUTER_BOUND('',#15481,.T.);
#9559=FACE_OUTER_BOUND('',#15482,.T.);
#9560=FACE_OUTER_BOUND('',#15483,.T.);
#9561=FACE_OUTER_BOUND('',#15484,.T.);
#9562=FACE_OUTER_BOUND('',#15485,.T.);
#9563=FACE_OUTER_BOUND('',#15486,.T.);
#9564=FACE_OUTER_BOUND('',#15487,.T.);
#9565=FACE_OUTER_BOUND('',#15488,.T.);
#9566=FACE_OUTER_BOUND('',#15489,.T.);
#9567=FACE_OUTER_BOUND('',#15490,.T.);
#9568=FACE_OUTER_BOUND('',#15491,.T.);
#9569=FACE_OUTER_BOUND('',#15492,.T.);
#9570=FACE_OUTER_BOUND('',#15493,.T.);
#9571=FACE_OUTER_BOUND('',#15494,.T.);
#9572=FACE_OUTER_BOUND('',#15495,.T.);
#9573=FACE_OUTER_BOUND('',#15496,.T.);
#9574=FACE_OUTER_BOUND('',#15497,.T.);
#9575=FACE_OUTER_BOUND('',#15498,.T.);
#9576=FACE_OUTER_BOUND('',#15499,.T.);
#9577=FACE_OUTER_BOUND('',#15500,.T.);
#9578=FACE_OUTER_BOUND('',#15501,.T.);
#9579=FACE_OUTER_BOUND('',#15502,.T.);
#9580=FACE_OUTER_BOUND('',#15503,.T.);
#9581=FACE_OUTER_BOUND('',#15504,.T.);
#9582=FACE_OUTER_BOUND('',#15505,.T.);
#9583=FACE_OUTER_BOUND('',#15506,.T.);
#9584=FACE_OUTER_BOUND('',#15507,.T.);
#9585=FACE_OUTER_BOUND('',#15508,.T.);
#9586=FACE_OUTER_BOUND('',#15509,.T.);
#9587=FACE_OUTER_BOUND('',#15510,.T.);
#9588=FACE_OUTER_BOUND('',#15511,.T.);
#9589=FACE_OUTER_BOUND('',#15512,.T.);
#9590=FACE_OUTER_BOUND('',#15513,.T.);
#9591=FACE_OUTER_BOUND('',#15514,.T.);
#9592=FACE_OUTER_BOUND('',#15515,.T.);
#9593=FACE_OUTER_BOUND('',#15516,.T.);
#9594=FACE_OUTER_BOUND('',#15517,.T.);
#9595=FACE_OUTER_BOUND('',#15518,.T.);
#9596=FACE_OUTER_BOUND('',#15519,.T.);
#9597=FACE_OUTER_BOUND('',#15520,.T.);
#9598=FACE_OUTER_BOUND('',#15521,.T.);
#9599=FACE_OUTER_BOUND('',#15522,.T.);
#9600=FACE_OUTER_BOUND('',#15523,.T.);
#9601=FACE_OUTER_BOUND('',#15524,.T.);
#9602=FACE_OUTER_BOUND('',#15525,.T.);
#9603=FACE_OUTER_BOUND('',#15526,.T.);
#9604=FACE_OUTER_BOUND('',#15527,.T.);
#9605=FACE_OUTER_BOUND('',#15528,.T.);
#9606=FACE_OUTER_BOUND('',#15529,.T.);
#9607=FACE_OUTER_BOUND('',#15530,.T.);
#9608=FACE_OUTER_BOUND('',#15531,.T.);
#9609=FACE_OUTER_BOUND('',#15532,.T.);
#9610=FACE_OUTER_BOUND('',#15533,.T.);
#9611=FACE_OUTER_BOUND('',#15534,.T.);
#9612=FACE_OUTER_BOUND('',#15535,.T.);
#9613=FACE_OUTER_BOUND('',#15536,.T.);
#9614=FACE_OUTER_BOUND('',#15537,.T.);
#9615=FACE_OUTER_BOUND('',#15538,.T.);
#9616=FACE_OUTER_BOUND('',#15539,.T.);
#9617=FACE_OUTER_BOUND('',#15540,.T.);
#9618=FACE_OUTER_BOUND('',#15541,.T.);
#9619=FACE_OUTER_BOUND('',#15542,.T.);
#9620=FACE_OUTER_BOUND('',#15543,.T.);
#9621=FACE_OUTER_BOUND('',#15544,.T.);
#9622=FACE_OUTER_BOUND('',#15545,.T.);
#9623=FACE_OUTER_BOUND('',#15546,.T.);
#9624=FACE_OUTER_BOUND('',#15547,.T.);
#9625=FACE_OUTER_BOUND('',#15548,.T.);
#9626=FACE_OUTER_BOUND('',#15549,.T.);
#9627=FACE_OUTER_BOUND('',#15550,.T.);
#9628=FACE_OUTER_BOUND('',#15551,.T.);
#9629=FACE_OUTER_BOUND('',#15552,.T.);
#9630=FACE_OUTER_BOUND('',#15553,.T.);
#9631=FACE_OUTER_BOUND('',#15554,.T.);
#9632=FACE_OUTER_BOUND('',#15555,.T.);
#9633=FACE_OUTER_BOUND('',#15556,.T.);
#9634=FACE_OUTER_BOUND('',#15557,.T.);
#9635=FACE_OUTER_BOUND('',#15558,.T.);
#9636=FACE_OUTER_BOUND('',#15559,.T.);
#9637=FACE_OUTER_BOUND('',#15560,.T.);
#9638=FACE_OUTER_BOUND('',#15561,.T.);
#9639=FACE_OUTER_BOUND('',#15562,.T.);
#9640=FACE_OUTER_BOUND('',#15563,.T.);
#9641=FACE_OUTER_BOUND('',#15564,.T.);
#9642=FACE_OUTER_BOUND('',#15565,.T.);
#9643=FACE_OUTER_BOUND('',#15566,.T.);
#9644=FACE_OUTER_BOUND('',#15567,.T.);
#9645=FACE_OUTER_BOUND('',#15568,.T.);
#9646=FACE_OUTER_BOUND('',#15569,.T.);
#9647=FACE_OUTER_BOUND('',#15570,.T.);
#9648=FACE_OUTER_BOUND('',#15571,.T.);
#9649=FACE_OUTER_BOUND('',#15572,.T.);
#9650=FACE_OUTER_BOUND('',#15573,.T.);
#9651=FACE_OUTER_BOUND('',#15574,.T.);
#9652=FACE_OUTER_BOUND('',#15575,.T.);
#9653=FACE_OUTER_BOUND('',#15576,.T.);
#9654=FACE_OUTER_BOUND('',#15577,.T.);
#9655=FACE_OUTER_BOUND('',#15578,.T.);
#9656=FACE_OUTER_BOUND('',#15579,.T.);
#9657=FACE_OUTER_BOUND('',#15580,.T.);
#9658=FACE_OUTER_BOUND('',#15581,.T.);
#9659=FACE_OUTER_BOUND('',#15582,.T.);
#9660=FACE_OUTER_BOUND('',#15583,.T.);
#9661=FACE_OUTER_BOUND('',#15584,.T.);
#9662=FACE_OUTER_BOUND('',#15585,.T.);
#9663=FACE_OUTER_BOUND('',#15586,.T.);
#9664=FACE_OUTER_BOUND('',#15587,.T.);
#9665=FACE_OUTER_BOUND('',#15588,.T.);
#9666=FACE_OUTER_BOUND('',#15589,.T.);
#9667=FACE_OUTER_BOUND('',#15590,.T.);
#9668=FACE_OUTER_BOUND('',#15591,.T.);
#9669=FACE_OUTER_BOUND('',#15592,.T.);
#9670=FACE_OUTER_BOUND('',#15593,.T.);
#9671=FACE_OUTER_BOUND('',#15594,.T.);
#9672=FACE_OUTER_BOUND('',#15595,.T.);
#9673=FACE_OUTER_BOUND('',#15596,.T.);
#9674=FACE_OUTER_BOUND('',#15597,.T.);
#9675=FACE_OUTER_BOUND('',#15598,.T.);
#9676=FACE_OUTER_BOUND('',#15599,.T.);
#9677=FACE_OUTER_BOUND('',#15600,.T.);
#9678=FACE_OUTER_BOUND('',#15601,.T.);
#9679=FACE_OUTER_BOUND('',#15602,.T.);
#9680=FACE_OUTER_BOUND('',#15603,.T.);
#9681=FACE_OUTER_BOUND('',#15604,.T.);
#9682=FACE_OUTER_BOUND('',#15605,.T.);
#9683=FACE_OUTER_BOUND('',#15606,.T.);
#9684=FACE_OUTER_BOUND('',#15607,.T.);
#9685=FACE_OUTER_BOUND('',#15608,.T.);
#9686=FACE_OUTER_BOUND('',#15609,.T.);
#9687=FACE_OUTER_BOUND('',#15610,.T.);
#9688=FACE_OUTER_BOUND('',#15611,.T.);
#9689=FACE_OUTER_BOUND('',#15612,.T.);
#9690=FACE_OUTER_BOUND('',#15613,.T.);
#9691=FACE_OUTER_BOUND('',#15614,.T.);
#9692=FACE_OUTER_BOUND('',#15615,.T.);
#9693=FACE_OUTER_BOUND('',#15616,.T.);
#9694=FACE_OUTER_BOUND('',#15617,.T.);
#9695=FACE_OUTER_BOUND('',#15618,.T.);
#9696=FACE_OUTER_BOUND('',#15619,.T.);
#9697=FACE_OUTER_BOUND('',#15620,.T.);
#9698=FACE_OUTER_BOUND('',#15621,.T.);
#9699=FACE_OUTER_BOUND('',#15622,.T.);
#9700=FACE_OUTER_BOUND('',#15623,.T.);
#9701=FACE_OUTER_BOUND('',#15624,.T.);
#9702=FACE_OUTER_BOUND('',#15625,.T.);
#9703=FACE_OUTER_BOUND('',#15626,.T.);
#9704=FACE_OUTER_BOUND('',#15627,.T.);
#9705=FACE_OUTER_BOUND('',#15628,.T.);
#9706=FACE_OUTER_BOUND('',#15629,.T.);
#9707=FACE_OUTER_BOUND('',#15630,.T.);
#9708=FACE_OUTER_BOUND('',#15631,.T.);
#9709=FACE_OUTER_BOUND('',#15632,.T.);
#9710=FACE_OUTER_BOUND('',#15633,.T.);
#9711=FACE_OUTER_BOUND('',#15634,.T.);
#9712=FACE_OUTER_BOUND('',#15635,.T.);
#9713=FACE_OUTER_BOUND('',#15636,.T.);
#9714=FACE_OUTER_BOUND('',#15637,.T.);
#9715=FACE_OUTER_BOUND('',#15638,.T.);
#9716=FACE_OUTER_BOUND('',#15639,.T.);
#9717=FACE_OUTER_BOUND('',#15640,.T.);
#9718=FACE_OUTER_BOUND('',#15641,.T.);
#9719=FACE_OUTER_BOUND('',#15642,.T.);
#9720=FACE_OUTER_BOUND('',#15643,.T.);
#9721=FACE_OUTER_BOUND('',#15644,.T.);
#9722=FACE_OUTER_BOUND('',#15645,.T.);
#9723=FACE_OUTER_BOUND('',#15646,.T.);
#9724=FACE_OUTER_BOUND('',#15647,.T.);
#9725=FACE_OUTER_BOUND('',#15648,.T.);
#9726=FACE_OUTER_BOUND('',#15649,.T.);
#9727=FACE_OUTER_BOUND('',#15650,.T.);
#9728=FACE_OUTER_BOUND('',#15651,.T.);
#9729=FACE_OUTER_BOUND('',#15652,.T.);
#9730=FACE_OUTER_BOUND('',#15653,.T.);
#9731=FACE_OUTER_BOUND('',#15654,.T.);
#9732=FACE_OUTER_BOUND('',#15655,.T.);
#9733=FACE_OUTER_BOUND('',#15656,.T.);
#9734=FACE_OUTER_BOUND('',#15657,.T.);
#9735=FACE_OUTER_BOUND('',#15658,.T.);
#9736=FACE_OUTER_BOUND('',#15659,.T.);
#9737=FACE_OUTER_BOUND('',#15660,.T.);
#9738=FACE_OUTER_BOUND('',#15661,.T.);
#9739=FACE_OUTER_BOUND('',#15662,.T.);
#9740=FACE_OUTER_BOUND('',#15663,.T.);
#9741=FACE_OUTER_BOUND('',#15664,.T.);
#9742=FACE_OUTER_BOUND('',#15665,.T.);
#9743=FACE_OUTER_BOUND('',#15666,.T.);
#9744=FACE_OUTER_BOUND('',#15667,.T.);
#9745=FACE_OUTER_BOUND('',#15668,.T.);
#9746=FACE_OUTER_BOUND('',#15669,.T.);
#9747=FACE_OUTER_BOUND('',#15670,.T.);
#9748=FACE_OUTER_BOUND('',#15671,.T.);
#9749=FACE_OUTER_BOUND('',#15672,.T.);
#9750=FACE_OUTER_BOUND('',#15673,.T.);
#9751=FACE_OUTER_BOUND('',#15674,.T.);
#9752=FACE_OUTER_BOUND('',#15675,.T.);
#9753=FACE_OUTER_BOUND('',#15676,.T.);
#9754=FACE_OUTER_BOUND('',#15677,.T.);
#9755=FACE_OUTER_BOUND('',#15678,.T.);
#9756=FACE_OUTER_BOUND('',#15679,.T.);
#9757=FACE_OUTER_BOUND('',#15680,.T.);
#9758=FACE_OUTER_BOUND('',#15681,.T.);
#9759=FACE_OUTER_BOUND('',#15682,.T.);
#9760=FACE_OUTER_BOUND('',#15683,.T.);
#9761=FACE_OUTER_BOUND('',#15684,.T.);
#9762=FACE_OUTER_BOUND('',#15685,.T.);
#9763=FACE_OUTER_BOUND('',#15686,.T.);
#9764=FACE_OUTER_BOUND('',#15687,.T.);
#9765=FACE_OUTER_BOUND('',#15688,.T.);
#9766=FACE_OUTER_BOUND('',#15689,.T.);
#9767=FACE_OUTER_BOUND('',#15690,.T.);
#9768=FACE_OUTER_BOUND('',#15691,.T.);
#9769=FACE_OUTER_BOUND('',#15692,.T.);
#9770=FACE_OUTER_BOUND('',#15693,.T.);
#9771=FACE_OUTER_BOUND('',#15694,.T.);
#9772=FACE_OUTER_BOUND('',#15695,.T.);
#9773=FACE_OUTER_BOUND('',#15696,.T.);
#9774=FACE_OUTER_BOUND('',#15697,.T.);
#9775=FACE_OUTER_BOUND('',#15698,.T.);
#9776=FACE_OUTER_BOUND('',#15699,.T.);
#9777=FACE_OUTER_BOUND('',#15700,.T.);
#9778=FACE_OUTER_BOUND('',#15701,.T.);
#9779=FACE_OUTER_BOUND('',#15702,.T.);
#9780=FACE_OUTER_BOUND('',#15703,.T.);
#9781=FACE_OUTER_BOUND('',#15704,.T.);
#9782=FACE_OUTER_BOUND('',#15705,.T.);
#9783=FACE_OUTER_BOUND('',#15706,.T.);
#9784=FACE_OUTER_BOUND('',#15707,.T.);
#9785=FACE_OUTER_BOUND('',#15708,.T.);
#9786=FACE_OUTER_BOUND('',#15709,.T.);
#9787=FACE_OUTER_BOUND('',#15710,.T.);
#9788=FACE_OUTER_BOUND('',#15711,.T.);
#9789=FACE_OUTER_BOUND('',#15712,.T.);
#9790=FACE_OUTER_BOUND('',#15713,.T.);
#9791=FACE_OUTER_BOUND('',#15714,.T.);
#9792=FACE_OUTER_BOUND('',#15715,.T.);
#9793=FACE_OUTER_BOUND('',#15716,.T.);
#9794=FACE_OUTER_BOUND('',#15717,.T.);
#9795=FACE_OUTER_BOUND('',#15718,.T.);
#9796=FACE_OUTER_BOUND('',#15719,.T.);
#9797=FACE_OUTER_BOUND('',#15720,.T.);
#9798=FACE_OUTER_BOUND('',#15721,.T.);
#9799=FACE_OUTER_BOUND('',#15722,.T.);
#9800=FACE_OUTER_BOUND('',#15723,.T.);
#9801=FACE_OUTER_BOUND('',#15724,.T.);
#9802=FACE_OUTER_BOUND('',#15725,.T.);
#9803=FACE_OUTER_BOUND('',#15726,.T.);
#9804=FACE_OUTER_BOUND('',#15727,.T.);
#9805=FACE_OUTER_BOUND('',#15728,.T.);
#9806=FACE_OUTER_BOUND('',#15729,.T.);
#9807=FACE_OUTER_BOUND('',#15730,.T.);
#9808=FACE_OUTER_BOUND('',#15731,.T.);
#9809=FACE_OUTER_BOUND('',#15732,.T.);
#9810=FACE_OUTER_BOUND('',#15733,.T.);
#9811=FACE_OUTER_BOUND('',#15734,.T.);
#9812=FACE_OUTER_BOUND('',#15735,.T.);
#9813=FACE_OUTER_BOUND('',#15736,.T.);
#9814=FACE_OUTER_BOUND('',#15737,.T.);
#9815=FACE_OUTER_BOUND('',#15738,.T.);
#9816=FACE_OUTER_BOUND('',#15739,.T.);
#9817=FACE_OUTER_BOUND('',#15740,.T.);
#9818=FACE_OUTER_BOUND('',#15741,.T.);
#9819=FACE_OUTER_BOUND('',#15742,.T.);
#9820=FACE_OUTER_BOUND('',#15743,.T.);
#9821=FACE_OUTER_BOUND('',#15744,.T.);
#9822=FACE_OUTER_BOUND('',#15745,.T.);
#9823=FACE_OUTER_BOUND('',#15746,.T.);
#9824=FACE_OUTER_BOUND('',#15747,.T.);
#9825=FACE_OUTER_BOUND('',#15748,.T.);
#9826=FACE_OUTER_BOUND('',#15749,.T.);
#9827=FACE_OUTER_BOUND('',#15750,.T.);
#9828=FACE_OUTER_BOUND('',#15751,.T.);
#9829=FACE_OUTER_BOUND('',#15752,.T.);
#9830=FACE_OUTER_BOUND('',#15753,.T.);
#9831=FACE_OUTER_BOUND('',#15754,.T.);
#9832=FACE_OUTER_BOUND('',#15755,.T.);
#9833=FACE_OUTER_BOUND('',#15756,.T.);
#9834=FACE_OUTER_BOUND('',#15757,.T.);
#9835=FACE_OUTER_BOUND('',#15758,.T.);
#9836=FACE_OUTER_BOUND('',#15759,.T.);
#9837=FACE_OUTER_BOUND('',#15760,.T.);
#9838=FACE_OUTER_BOUND('',#15761,.T.);
#9839=FACE_OUTER_BOUND('',#15762,.T.);
#9840=FACE_OUTER_BOUND('',#15763,.T.);
#9841=FACE_OUTER_BOUND('',#15764,.T.);
#9842=FACE_OUTER_BOUND('',#15765,.T.);
#9843=FACE_OUTER_BOUND('',#15766,.T.);
#9844=FACE_OUTER_BOUND('',#15767,.T.);
#9845=FACE_OUTER_BOUND('',#15768,.T.);
#9846=FACE_OUTER_BOUND('',#15769,.T.);
#9847=FACE_OUTER_BOUND('',#15770,.T.);
#9848=FACE_OUTER_BOUND('',#15771,.T.);
#9849=FACE_OUTER_BOUND('',#15772,.T.);
#9850=FACE_OUTER_BOUND('',#15773,.T.);
#9851=FACE_OUTER_BOUND('',#15774,.T.);
#9852=FACE_OUTER_BOUND('',#15775,.T.);
#9853=FACE_OUTER_BOUND('',#15776,.T.);
#9854=FACE_OUTER_BOUND('',#15777,.T.);
#9855=FACE_OUTER_BOUND('',#15778,.T.);
#9856=FACE_OUTER_BOUND('',#15779,.T.);
#9857=FACE_OUTER_BOUND('',#15780,.T.);
#9858=FACE_OUTER_BOUND('',#15781,.T.);
#9859=FACE_OUTER_BOUND('',#15782,.T.);
#9860=FACE_OUTER_BOUND('',#15783,.T.);
#9861=FACE_OUTER_BOUND('',#15784,.T.);
#9862=FACE_OUTER_BOUND('',#15785,.T.);
#9863=FACE_OUTER_BOUND('',#15786,.T.);
#9864=FACE_OUTER_BOUND('',#15787,.T.);
#9865=FACE_OUTER_BOUND('',#15788,.T.);
#9866=FACE_OUTER_BOUND('',#15789,.T.);
#9867=FACE_OUTER_BOUND('',#15790,.T.);
#9868=FACE_OUTER_BOUND('',#15791,.T.);
#9869=FACE_OUTER_BOUND('',#15792,.T.);
#9870=FACE_OUTER_BOUND('',#15793,.T.);
#9871=FACE_OUTER_BOUND('',#15794,.T.);
#9872=FACE_OUTER_BOUND('',#15795,.T.);
#9873=FACE_OUTER_BOUND('',#15796,.T.);
#9874=FACE_OUTER_BOUND('',#15797,.T.);
#9875=FACE_OUTER_BOUND('',#15798,.T.);
#9876=FACE_OUTER_BOUND('',#15799,.T.);
#9877=FACE_OUTER_BOUND('',#15800,.T.);
#9878=FACE_OUTER_BOUND('',#15801,.T.);
#9879=FACE_OUTER_BOUND('',#15802,.T.);
#9880=FACE_OUTER_BOUND('',#15803,.T.);
#9881=FACE_OUTER_BOUND('',#15804,.T.);
#9882=FACE_OUTER_BOUND('',#15805,.T.);
#9883=FACE_OUTER_BOUND('',#15806,.T.);
#9884=FACE_OUTER_BOUND('',#15807,.T.);
#9885=FACE_OUTER_BOUND('',#15808,.T.);
#9886=FACE_OUTER_BOUND('',#15809,.T.);
#9887=FACE_OUTER_BOUND('',#15810,.T.);
#9888=FACE_OUTER_BOUND('',#15811,.T.);
#9889=FACE_OUTER_BOUND('',#15812,.T.);
#9890=FACE_OUTER_BOUND('',#15813,.T.);
#9891=FACE_OUTER_BOUND('',#15814,.T.);
#9892=FACE_OUTER_BOUND('',#15815,.T.);
#9893=FACE_OUTER_BOUND('',#15816,.T.);
#9894=FACE_OUTER_BOUND('',#15817,.T.);
#9895=FACE_OUTER_BOUND('',#15818,.T.);
#9896=FACE_OUTER_BOUND('',#15819,.T.);
#9897=FACE_OUTER_BOUND('',#15820,.T.);
#9898=FACE_OUTER_BOUND('',#15821,.T.);
#9899=FACE_OUTER_BOUND('',#15822,.T.);
#9900=FACE_OUTER_BOUND('',#15823,.T.);
#9901=FACE_OUTER_BOUND('',#15824,.T.);
#9902=FACE_OUTER_BOUND('',#15825,.T.);
#9903=FACE_OUTER_BOUND('',#15826,.T.);
#9904=FACE_OUTER_BOUND('',#15827,.T.);
#9905=FACE_OUTER_BOUND('',#15828,.T.);
#9906=FACE_OUTER_BOUND('',#15829,.T.);
#9907=FACE_OUTER_BOUND('',#15830,.T.);
#9908=FACE_OUTER_BOUND('',#15831,.T.);
#9909=FACE_OUTER_BOUND('',#15832,.T.);
#9910=FACE_OUTER_BOUND('',#15833,.T.);
#9911=FACE_OUTER_BOUND('',#15834,.T.);
#9912=FACE_OUTER_BOUND('',#15835,.T.);
#9913=FACE_OUTER_BOUND('',#15836,.T.);
#9914=FACE_OUTER_BOUND('',#15837,.T.);
#9915=FACE_OUTER_BOUND('',#15838,.T.);
#9916=FACE_OUTER_BOUND('',#15839,.T.);
#9917=FACE_OUTER_BOUND('',#15840,.T.);
#9918=FACE_OUTER_BOUND('',#15841,.T.);
#9919=FACE_OUTER_BOUND('',#15842,.T.);
#9920=FACE_OUTER_BOUND('',#15843,.T.);
#9921=FACE_OUTER_BOUND('',#15844,.T.);
#9922=FACE_OUTER_BOUND('',#15845,.T.);
#9923=FACE_OUTER_BOUND('',#15846,.T.);
#9924=FACE_OUTER_BOUND('',#15847,.T.);
#9925=FACE_OUTER_BOUND('',#15848,.T.);
#9926=FACE_OUTER_BOUND('',#15849,.T.);
#9927=FACE_OUTER_BOUND('',#15850,.T.);
#9928=FACE_OUTER_BOUND('',#15851,.T.);
#9929=FACE_OUTER_BOUND('',#15852,.T.);
#9930=FACE_OUTER_BOUND('',#15853,.T.);
#9931=FACE_OUTER_BOUND('',#15854,.T.);
#9932=FACE_OUTER_BOUND('',#15855,.T.);
#9933=FACE_OUTER_BOUND('',#15856,.T.);
#9934=FACE_OUTER_BOUND('',#15857,.T.);
#9935=FACE_OUTER_BOUND('',#15858,.T.);
#9936=FACE_OUTER_BOUND('',#15859,.T.);
#9937=FACE_OUTER_BOUND('',#15860,.T.);
#9938=FACE_OUTER_BOUND('',#15861,.T.);
#9939=FACE_OUTER_BOUND('',#15862,.T.);
#9940=FACE_OUTER_BOUND('',#15863,.T.);
#9941=FACE_OUTER_BOUND('',#15864,.T.);
#9942=FACE_OUTER_BOUND('',#15865,.T.);
#9943=FACE_OUTER_BOUND('',#15866,.T.);
#9944=FACE_OUTER_BOUND('',#15867,.T.);
#9945=FACE_OUTER_BOUND('',#15868,.T.);
#9946=FACE_OUTER_BOUND('',#15869,.T.);
#9947=FACE_OUTER_BOUND('',#15870,.T.);
#9948=FACE_OUTER_BOUND('',#15871,.T.);
#9949=FACE_OUTER_BOUND('',#15872,.T.);
#9950=FACE_OUTER_BOUND('',#15873,.T.);
#9951=FACE_OUTER_BOUND('',#15874,.T.);
#9952=FACE_OUTER_BOUND('',#15875,.T.);
#9953=FACE_OUTER_BOUND('',#15876,.T.);
#9954=FACE_OUTER_BOUND('',#15877,.T.);
#9955=FACE_OUTER_BOUND('',#15878,.T.);
#9956=FACE_OUTER_BOUND('',#15879,.T.);
#9957=FACE_OUTER_BOUND('',#15880,.T.);
#9958=FACE_OUTER_BOUND('',#15881,.T.);
#9959=FACE_OUTER_BOUND('',#15882,.T.);
#9960=FACE_OUTER_BOUND('',#15883,.T.);
#9961=FACE_OUTER_BOUND('',#15884,.T.);
#9962=FACE_OUTER_BOUND('',#15885,.T.);
#9963=FACE_OUTER_BOUND('',#15886,.T.);
#9964=FACE_OUTER_BOUND('',#15887,.T.);
#9965=FACE_OUTER_BOUND('',#15888,.T.);
#9966=FACE_OUTER_BOUND('',#15889,.T.);
#9967=FACE_OUTER_BOUND('',#15890,.T.);
#9968=FACE_OUTER_BOUND('',#15891,.T.);
#9969=FACE_OUTER_BOUND('',#15892,.T.);
#9970=FACE_OUTER_BOUND('',#15893,.T.);
#9971=FACE_OUTER_BOUND('',#15894,.T.);
#9972=FACE_OUTER_BOUND('',#15895,.T.);
#9973=FACE_OUTER_BOUND('',#15896,.T.);
#9974=FACE_OUTER_BOUND('',#15897,.T.);
#9975=FACE_OUTER_BOUND('',#15898,.T.);
#9976=FACE_OUTER_BOUND('',#15899,.T.);
#9977=FACE_OUTER_BOUND('',#15900,.T.);
#9978=FACE_OUTER_BOUND('',#15901,.T.);
#9979=FACE_OUTER_BOUND('',#15902,.T.);
#9980=FACE_OUTER_BOUND('',#15903,.T.);
#9981=FACE_OUTER_BOUND('',#15904,.T.);
#9982=FACE_OUTER_BOUND('',#15905,.T.);
#9983=FACE_OUTER_BOUND('',#15906,.T.);
#9984=FACE_OUTER_BOUND('',#15907,.T.);
#9985=FACE_OUTER_BOUND('',#15908,.T.);
#9986=FACE_OUTER_BOUND('',#15909,.T.);
#9987=FACE_OUTER_BOUND('',#15910,.T.);
#9988=FACE_OUTER_BOUND('',#15911,.T.);
#9989=FACE_OUTER_BOUND('',#15912,.T.);
#9990=FACE_OUTER_BOUND('',#15913,.T.);
#9991=FACE_OUTER_BOUND('',#15914,.T.);
#9992=FACE_OUTER_BOUND('',#15915,.T.);
#9993=FACE_OUTER_BOUND('',#15916,.T.);
#9994=FACE_OUTER_BOUND('',#15917,.T.);
#9995=FACE_OUTER_BOUND('',#15918,.T.);
#9996=FACE_OUTER_BOUND('',#15919,.T.);
#9997=FACE_OUTER_BOUND('',#15920,.T.);
#9998=FACE_OUTER_BOUND('',#15921,.T.);
#9999=FACE_OUTER_BOUND('',#15922,.T.);
#10000=FACE_OUTER_BOUND('',#15923,.T.);
#10001=FACE_OUTER_BOUND('',#15924,.T.);
#10002=FACE_OUTER_BOUND('',#15925,.T.);
#10003=FACE_OUTER_BOUND('',#15926,.T.);
#10004=FACE_OUTER_BOUND('',#15927,.T.);
#10005=FACE_OUTER_BOUND('',#15928,.T.);
#10006=FACE_OUTER_BOUND('',#15929,.T.);
#10007=FACE_OUTER_BOUND('',#15930,.T.);
#10008=FACE_OUTER_BOUND('',#15931,.T.);
#10009=FACE_OUTER_BOUND('',#15932,.T.);
#10010=FACE_OUTER_BOUND('',#15933,.T.);
#10011=FACE_OUTER_BOUND('',#15934,.T.);
#10012=FACE_OUTER_BOUND('',#15935,.T.);
#10013=FACE_OUTER_BOUND('',#15936,.T.);
#10014=FACE_OUTER_BOUND('',#15937,.T.);
#10015=FACE_OUTER_BOUND('',#15938,.T.);
#10016=FACE_OUTER_BOUND('',#15939,.T.);
#10017=FACE_OUTER_BOUND('',#15940,.T.);
#10018=FACE_OUTER_BOUND('',#15941,.T.);
#10019=FACE_OUTER_BOUND('',#15942,.T.);
#10020=FACE_OUTER_BOUND('',#15943,.T.);
#10021=FACE_OUTER_BOUND('',#15944,.T.);
#10022=FACE_OUTER_BOUND('',#15945,.T.);
#10023=FACE_OUTER_BOUND('',#15946,.T.);
#10024=FACE_OUTER_BOUND('',#15947,.T.);
#10025=FACE_OUTER_BOUND('',#15948,.T.);
#10026=FACE_OUTER_BOUND('',#15949,.T.);
#10027=FACE_OUTER_BOUND('',#15950,.T.);
#10028=FACE_OUTER_BOUND('',#15951,.T.);
#10029=FACE_OUTER_BOUND('',#15952,.T.);
#10030=FACE_OUTER_BOUND('',#15953,.T.);
#10031=FACE_OUTER_BOUND('',#15954,.T.);
#10032=FACE_OUTER_BOUND('',#15955,.T.);
#10033=FACE_OUTER_BOUND('',#15956,.T.);
#10034=FACE_OUTER_BOUND('',#15957,.T.);
#10035=FACE_OUTER_BOUND('',#15958,.T.);
#10036=FACE_OUTER_BOUND('',#15959,.T.);
#10037=FACE_OUTER_BOUND('',#15960,.T.);
#10038=FACE_OUTER_BOUND('',#15961,.T.);
#10039=FACE_OUTER_BOUND('',#15962,.T.);
#10040=FACE_OUTER_BOUND('',#15963,.T.);
#10041=FACE_OUTER_BOUND('',#15964,.T.);
#10042=FACE_OUTER_BOUND('',#15965,.T.);
#10043=FACE_OUTER_BOUND('',#15966,.T.);
#10044=FACE_OUTER_BOUND('',#15967,.T.);
#10045=FACE_OUTER_BOUND('',#15968,.T.);
#10046=FACE_OUTER_BOUND('',#15969,.T.);
#10047=FACE_OUTER_BOUND('',#15970,.T.);
#10048=FACE_OUTER_BOUND('',#15971,.T.);
#10049=FACE_OUTER_BOUND('',#15972,.T.);
#10050=FACE_OUTER_BOUND('',#15973,.T.);
#10051=FACE_OUTER_BOUND('',#15974,.T.);
#10052=FACE_OUTER_BOUND('',#15975,.T.);
#10053=FACE_OUTER_BOUND('',#15976,.T.);
#10054=FACE_OUTER_BOUND('',#15977,.T.);
#10055=FACE_OUTER_BOUND('',#15978,.T.);
#10056=FACE_OUTER_BOUND('',#15979,.T.);
#10057=FACE_OUTER_BOUND('',#15980,.T.);
#10058=FACE_OUTER_BOUND('',#15981,.T.);
#10059=FACE_OUTER_BOUND('',#15982,.T.);
#10060=FACE_OUTER_BOUND('',#15983,.T.);
#10061=FACE_OUTER_BOUND('',#15984,.T.);
#10062=FACE_OUTER_BOUND('',#15985,.T.);
#10063=FACE_OUTER_BOUND('',#15986,.T.);
#10064=FACE_OUTER_BOUND('',#15987,.T.);
#10065=FACE_OUTER_BOUND('',#15988,.T.);
#10066=FACE_OUTER_BOUND('',#15989,.T.);
#10067=FACE_OUTER_BOUND('',#15990,.T.);
#10068=FACE_OUTER_BOUND('',#15991,.T.);
#10069=FACE_OUTER_BOUND('',#15992,.T.);
#10070=FACE_OUTER_BOUND('',#15993,.T.);
#10071=FACE_OUTER_BOUND('',#15994,.T.);
#10072=FACE_OUTER_BOUND('',#15995,.T.);
#10073=FACE_OUTER_BOUND('',#15996,.T.);
#10074=FACE_OUTER_BOUND('',#15997,.T.);
#10075=FACE_OUTER_BOUND('',#15998,.T.);
#10076=FACE_OUTER_BOUND('',#15999,.T.);
#10077=FACE_OUTER_BOUND('',#16000,.T.);
#10078=FACE_OUTER_BOUND('',#16001,.T.);
#10079=FACE_OUTER_BOUND('',#16002,.T.);
#10080=FACE_OUTER_BOUND('',#16003,.T.);
#10081=FACE_OUTER_BOUND('',#16004,.T.);
#10082=FACE_OUTER_BOUND('',#16005,.T.);
#10083=FACE_OUTER_BOUND('',#16006,.T.);
#10084=FACE_OUTER_BOUND('',#16007,.T.);
#10085=FACE_OUTER_BOUND('',#16008,.T.);
#10086=FACE_OUTER_BOUND('',#16009,.T.);
#10087=FACE_OUTER_BOUND('',#16010,.T.);
#10088=FACE_OUTER_BOUND('',#16011,.T.);
#10089=FACE_OUTER_BOUND('',#16012,.T.);
#10090=FACE_OUTER_BOUND('',#16013,.T.);
#10091=FACE_OUTER_BOUND('',#16014,.T.);
#10092=FACE_OUTER_BOUND('',#16015,.T.);
#10093=FACE_OUTER_BOUND('',#16016,.T.);
#10094=FACE_OUTER_BOUND('',#16017,.T.);
#10095=FACE_OUTER_BOUND('',#16018,.T.);
#10096=FACE_OUTER_BOUND('',#16019,.T.);
#10097=FACE_OUTER_BOUND('',#16020,.T.);
#10098=FACE_OUTER_BOUND('',#16021,.T.);
#10099=FACE_OUTER_BOUND('',#16022,.T.);
#10100=FACE_OUTER_BOUND('',#16023,.T.);
#10101=FACE_OUTER_BOUND('',#16024,.T.);
#10102=FACE_OUTER_BOUND('',#16025,.T.);
#10103=FACE_OUTER_BOUND('',#16026,.T.);
#10104=FACE_OUTER_BOUND('',#16027,.T.);
#10105=FACE_OUTER_BOUND('',#16028,.T.);
#10106=FACE_OUTER_BOUND('',#16029,.T.);
#10107=FACE_OUTER_BOUND('',#16030,.T.);
#10108=FACE_OUTER_BOUND('',#16031,.T.);
#10109=FACE_OUTER_BOUND('',#16032,.T.);
#10110=FACE_OUTER_BOUND('',#16033,.T.);
#10111=FACE_OUTER_BOUND('',#16034,.T.);
#10112=FACE_OUTER_BOUND('',#16035,.T.);
#10113=FACE_OUTER_BOUND('',#16036,.T.);
#10114=FACE_OUTER_BOUND('',#16037,.T.);
#10115=FACE_OUTER_BOUND('',#16038,.T.);
#10116=FACE_OUTER_BOUND('',#16039,.T.);
#10117=FACE_OUTER_BOUND('',#16040,.T.);
#10118=FACE_OUTER_BOUND('',#16041,.T.);
#10119=FACE_OUTER_BOUND('',#16042,.T.);
#10120=FACE_OUTER_BOUND('',#16043,.T.);
#10121=FACE_OUTER_BOUND('',#16044,.T.);
#10122=FACE_OUTER_BOUND('',#16045,.T.);
#10123=FACE_OUTER_BOUND('',#16046,.T.);
#10124=FACE_OUTER_BOUND('',#16047,.T.);
#10125=FACE_OUTER_BOUND('',#16048,.T.);
#10126=FACE_OUTER_BOUND('',#16049,.T.);
#10127=FACE_OUTER_BOUND('',#16050,.T.);
#10128=FACE_OUTER_BOUND('',#16051,.T.);
#10129=FACE_OUTER_BOUND('',#16052,.T.);
#10130=FACE_OUTER_BOUND('',#16053,.T.);
#10131=FACE_OUTER_BOUND('',#16054,.T.);
#10132=FACE_OUTER_BOUND('',#16055,.T.);
#10133=FACE_OUTER_BOUND('',#16056,.T.);
#10134=FACE_OUTER_BOUND('',#16057,.T.);
#10135=FACE_OUTER_BOUND('',#16058,.T.);
#10136=FACE_OUTER_BOUND('',#16059,.T.);
#10137=FACE_OUTER_BOUND('',#16060,.T.);
#10138=FACE_OUTER_BOUND('',#16061,.T.);
#10139=FACE_OUTER_BOUND('',#16062,.T.);
#10140=FACE_OUTER_BOUND('',#16063,.T.);
#10141=FACE_OUTER_BOUND('',#16064,.T.);
#10142=FACE_OUTER_BOUND('',#16065,.T.);
#10143=FACE_OUTER_BOUND('',#16066,.T.);
#10144=FACE_OUTER_BOUND('',#16067,.T.);
#10145=FACE_OUTER_BOUND('',#16068,.T.);
#10146=FACE_OUTER_BOUND('',#16069,.T.);
#10147=FACE_OUTER_BOUND('',#16070,.T.);
#10148=FACE_OUTER_BOUND('',#16071,.T.);
#10149=FACE_OUTER_BOUND('',#16072,.T.);
#10150=FACE_OUTER_BOUND('',#16073,.T.);
#10151=FACE_OUTER_BOUND('',#16074,.T.);
#10152=FACE_OUTER_BOUND('',#16075,.T.);
#10153=FACE_OUTER_BOUND('',#16076,.T.);
#10154=FACE_OUTER_BOUND('',#16077,.T.);
#10155=FACE_OUTER_BOUND('',#16078,.T.);
#10156=FACE_OUTER_BOUND('',#16079,.T.);
#10157=FACE_OUTER_BOUND('',#16080,.T.);
#10158=FACE_OUTER_BOUND('',#16081,.T.);
#10159=FACE_OUTER_BOUND('',#16082,.T.);
#10160=FACE_OUTER_BOUND('',#16083,.T.);
#10161=FACE_OUTER_BOUND('',#16084,.T.);
#10162=FACE_OUTER_BOUND('',#16085,.T.);
#10163=FACE_OUTER_BOUND('',#16086,.T.);
#10164=FACE_OUTER_BOUND('',#16087,.T.);
#10165=FACE_OUTER_BOUND('',#16088,.T.);
#10166=FACE_OUTER_BOUND('',#16089,.T.);
#10167=FACE_OUTER_BOUND('',#16090,.T.);
#10168=FACE_OUTER_BOUND('',#16091,.T.);
#10169=FACE_OUTER_BOUND('',#16092,.T.);
#10170=FACE_OUTER_BOUND('',#16093,.T.);
#10171=FACE_OUTER_BOUND('',#16094,.T.);
#10172=FACE_OUTER_BOUND('',#16095,.T.);
#10173=FACE_OUTER_BOUND('',#16096,.T.);
#10174=FACE_OUTER_BOUND('',#16097,.T.);
#10175=FACE_OUTER_BOUND('',#16098,.T.);
#10176=FACE_OUTER_BOUND('',#16099,.T.);
#10177=FACE_OUTER_BOUND('',#16100,.T.);
#10178=FACE_OUTER_BOUND('',#16101,.T.);
#10179=FACE_OUTER_BOUND('',#16102,.T.);
#10180=FACE_OUTER_BOUND('',#16103,.T.);
#10181=FACE_OUTER_BOUND('',#16104,.T.);
#10182=FACE_OUTER_BOUND('',#16105,.T.);
#10183=FACE_OUTER_BOUND('',#16106,.T.);
#10184=FACE_OUTER_BOUND('',#16107,.T.);
#10185=FACE_OUTER_BOUND('',#16108,.T.);
#10186=FACE_OUTER_BOUND('',#16109,.T.);
#10187=FACE_OUTER_BOUND('',#16110,.T.);
#10188=FACE_OUTER_BOUND('',#16111,.T.);
#10189=FACE_OUTER_BOUND('',#16112,.T.);
#10190=FACE_OUTER_BOUND('',#16113,.T.);
#10191=FACE_OUTER_BOUND('',#16114,.T.);
#10192=FACE_OUTER_BOUND('',#16115,.T.);
#10193=FACE_OUTER_BOUND('',#16116,.T.);
#10194=FACE_OUTER_BOUND('',#16117,.T.);
#10195=FACE_OUTER_BOUND('',#16118,.T.);
#10196=FACE_OUTER_BOUND('',#16119,.T.);
#10197=FACE_OUTER_BOUND('',#16120,.T.);
#10198=FACE_OUTER_BOUND('',#16121,.T.);
#10199=FACE_OUTER_BOUND('',#16122,.T.);
#10200=FACE_OUTER_BOUND('',#16123,.T.);
#10201=FACE_OUTER_BOUND('',#16124,.T.);
#10202=FACE_OUTER_BOUND('',#16125,.T.);
#10203=FACE_OUTER_BOUND('',#16126,.T.);
#10204=FACE_OUTER_BOUND('',#16127,.T.);
#10205=FACE_OUTER_BOUND('',#16128,.T.);
#10206=FACE_OUTER_BOUND('',#16129,.T.);
#10207=FACE_OUTER_BOUND('',#16130,.T.);
#10208=FACE_OUTER_BOUND('',#16131,.T.);
#10209=FACE_OUTER_BOUND('',#16132,.T.);
#10210=FACE_OUTER_BOUND('',#16133,.T.);
#10211=FACE_OUTER_BOUND('',#16134,.T.);
#10212=FACE_OUTER_BOUND('',#16135,.T.);
#10213=FACE_OUTER_BOUND('',#16136,.T.);
#10214=FACE_OUTER_BOUND('',#16137,.T.);
#10215=FACE_OUTER_BOUND('',#16138,.T.);
#10216=FACE_OUTER_BOUND('',#16139,.T.);
#10217=FACE_OUTER_BOUND('',#16140,.T.);
#10218=FACE_OUTER_BOUND('',#16141,.T.);
#10219=FACE_OUTER_BOUND('',#16142,.T.);
#10220=FACE_OUTER_BOUND('',#16143,.T.);
#10221=FACE_OUTER_BOUND('',#16144,.T.);
#10222=FACE_OUTER_BOUND('',#16145,.T.);
#10223=FACE_OUTER_BOUND('',#16146,.T.);
#10224=FACE_OUTER_BOUND('',#16147,.T.);
#10225=FACE_OUTER_BOUND('',#16148,.T.);
#10226=FACE_OUTER_BOUND('',#16149,.T.);
#10227=FACE_OUTER_BOUND('',#16150,.T.);
#10228=FACE_OUTER_BOUND('',#16151,.T.);
#10229=FACE_OUTER_BOUND('',#16152,.T.);
#10230=FACE_OUTER_BOUND('',#16153,.T.);
#10231=FACE_OUTER_BOUND('',#16154,.T.);
#10232=FACE_OUTER_BOUND('',#16155,.T.);
#10233=FACE_OUTER_BOUND('',#16156,.T.);
#10234=FACE_OUTER_BOUND('',#16157,.T.);
#10235=FACE_OUTER_BOUND('',#16158,.T.);
#10236=FACE_OUTER_BOUND('',#16159,.T.);
#10237=FACE_OUTER_BOUND('',#16160,.T.);
#10238=FACE_OUTER_BOUND('',#16161,.T.);
#10239=FACE_OUTER_BOUND('',#16162,.T.);
#10240=FACE_OUTER_BOUND('',#16163,.T.);
#10241=FACE_OUTER_BOUND('',#16164,.T.);
#10242=FACE_OUTER_BOUND('',#16165,.T.);
#10243=FACE_OUTER_BOUND('',#16166,.T.);
#10244=FACE_OUTER_BOUND('',#16167,.T.);
#10245=FACE_OUTER_BOUND('',#16168,.T.);
#10246=FACE_OUTER_BOUND('',#16169,.T.);
#10247=FACE_OUTER_BOUND('',#16170,.T.);
#10248=FACE_OUTER_BOUND('',#16171,.T.);
#10249=FACE_OUTER_BOUND('',#16172,.T.);
#10250=FACE_OUTER_BOUND('',#16173,.T.);
#10251=FACE_OUTER_BOUND('',#16174,.T.);
#10252=FACE_OUTER_BOUND('',#16175,.T.);
#10253=FACE_OUTER_BOUND('',#16176,.T.);
#10254=FACE_OUTER_BOUND('',#16177,.T.);
#10255=FACE_OUTER_BOUND('',#16178,.T.);
#10256=FACE_OUTER_BOUND('',#16179,.T.);
#10257=FACE_OUTER_BOUND('',#16180,.T.);
#10258=FACE_OUTER_BOUND('',#16181,.T.);
#10259=FACE_OUTER_BOUND('',#16182,.T.);
#10260=FACE_OUTER_BOUND('',#16183,.T.);
#10261=FACE_OUTER_BOUND('',#16184,.T.);
#10262=FACE_OUTER_BOUND('',#16185,.T.);
#10263=FACE_OUTER_BOUND('',#16186,.T.);
#10264=FACE_OUTER_BOUND('',#16187,.T.);
#10265=FACE_OUTER_BOUND('',#16188,.T.);
#10266=FACE_OUTER_BOUND('',#16189,.T.);
#10267=FACE_OUTER_BOUND('',#16190,.T.);
#10268=FACE_OUTER_BOUND('',#16191,.T.);
#10269=FACE_OUTER_BOUND('',#16192,.T.);
#10270=FACE_OUTER_BOUND('',#16193,.T.);
#10271=FACE_OUTER_BOUND('',#16194,.T.);
#10272=FACE_OUTER_BOUND('',#16195,.T.);
#10273=FACE_OUTER_BOUND('',#16196,.T.);
#10274=FACE_OUTER_BOUND('',#16197,.T.);
#10275=FACE_OUTER_BOUND('',#16198,.T.);
#10276=FACE_OUTER_BOUND('',#16199,.T.);
#10277=FACE_OUTER_BOUND('',#16200,.T.);
#10278=FACE_OUTER_BOUND('',#16201,.T.);
#10279=FACE_OUTER_BOUND('',#16202,.T.);
#10280=FACE_OUTER_BOUND('',#16203,.T.);
#10281=FACE_OUTER_BOUND('',#16204,.T.);
#10282=FACE_OUTER_BOUND('',#16205,.T.);
#10283=FACE_OUTER_BOUND('',#16206,.T.);
#10284=FACE_OUTER_BOUND('',#16207,.T.);
#10285=FACE_OUTER_BOUND('',#16208,.T.);
#10286=FACE_OUTER_BOUND('',#16209,.T.);
#10287=FACE_OUTER_BOUND('',#16210,.T.);
#10288=FACE_OUTER_BOUND('',#16211,.T.);
#10289=FACE_OUTER_BOUND('',#16212,.T.);
#10290=FACE_OUTER_BOUND('',#16213,.T.);
#10291=FACE_OUTER_BOUND('',#16214,.T.);
#10292=FACE_OUTER_BOUND('',#16215,.T.);
#10293=FACE_OUTER_BOUND('',#16216,.T.);
#10294=FACE_OUTER_BOUND('',#16217,.T.);
#10295=FACE_OUTER_BOUND('',#16218,.T.);
#10296=FACE_OUTER_BOUND('',#16219,.T.);
#10297=FACE_OUTER_BOUND('',#16220,.T.);
#10298=FACE_OUTER_BOUND('',#16221,.T.);
#10299=FACE_OUTER_BOUND('',#16222,.T.);
#10300=FACE_OUTER_BOUND('',#16223,.T.);
#10301=FACE_OUTER_BOUND('',#16224,.T.);
#10302=FACE_OUTER_BOUND('',#16225,.T.);
#10303=FACE_OUTER_BOUND('',#16226,.T.);
#10304=FACE_OUTER_BOUND('',#16227,.T.);
#10305=FACE_OUTER_BOUND('',#16228,.T.);
#10306=FACE_OUTER_BOUND('',#16229,.T.);
#10307=FACE_OUTER_BOUND('',#16230,.T.);
#10308=FACE_OUTER_BOUND('',#16231,.T.);
#10309=FACE_OUTER_BOUND('',#16232,.T.);
#10310=FACE_OUTER_BOUND('',#16233,.T.);
#10311=FACE_OUTER_BOUND('',#16234,.T.);
#10312=FACE_OUTER_BOUND('',#16235,.T.);
#10313=FACE_OUTER_BOUND('',#16236,.T.);
#10314=FACE_OUTER_BOUND('',#16237,.T.);
#10315=FACE_OUTER_BOUND('',#16238,.T.);
#10316=FACE_OUTER_BOUND('',#16239,.T.);
#10317=FACE_OUTER_BOUND('',#16240,.T.);
#10318=FACE_OUTER_BOUND('',#16241,.T.);
#10319=FACE_OUTER_BOUND('',#16242,.T.);
#10320=FACE_OUTER_BOUND('',#16243,.T.);
#10321=FACE_OUTER_BOUND('',#16244,.T.);
#10322=FACE_OUTER_BOUND('',#16245,.T.);
#10323=FACE_OUTER_BOUND('',#16246,.T.);
#10324=FACE_OUTER_BOUND('',#16247,.T.);
#10325=FACE_OUTER_BOUND('',#16248,.T.);
#10326=FACE_OUTER_BOUND('',#16249,.T.);
#10327=FACE_OUTER_BOUND('',#16250,.T.);
#10328=FACE_OUTER_BOUND('',#16251,.T.);
#10329=FACE_OUTER_BOUND('',#16252,.T.);
#10330=FACE_OUTER_BOUND('',#16253,.T.);
#10331=FACE_OUTER_BOUND('',#16254,.T.);
#10332=FACE_OUTER_BOUND('',#16255,.T.);
#10333=FACE_OUTER_BOUND('',#16256,.T.);
#10334=FACE_OUTER_BOUND('',#16257,.T.);
#10335=FACE_OUTER_BOUND('',#16258,.T.);
#10336=FACE_OUTER_BOUND('',#16259,.T.);
#10337=FACE_OUTER_BOUND('',#16260,.T.);
#10338=FACE_OUTER_BOUND('',#16261,.T.);
#10339=FACE_OUTER_BOUND('',#16262,.T.);
#10340=FACE_OUTER_BOUND('',#16263,.T.);
#10341=FACE_OUTER_BOUND('',#16264,.T.);
#10342=FACE_OUTER_BOUND('',#16265,.T.);
#10343=FACE_OUTER_BOUND('',#16266,.T.);
#10344=FACE_OUTER_BOUND('',#16267,.T.);
#10345=FACE_OUTER_BOUND('',#16268,.T.);
#10346=FACE_OUTER_BOUND('',#16269,.T.);
#10347=FACE_OUTER_BOUND('',#16270,.T.);
#10348=FACE_OUTER_BOUND('',#16271,.T.);
#10349=FACE_OUTER_BOUND('',#16272,.T.);
#10350=FACE_OUTER_BOUND('',#16273,.T.);
#10351=FACE_OUTER_BOUND('',#16274,.T.);
#10352=FACE_OUTER_BOUND('',#16275,.T.);
#10353=FACE_OUTER_BOUND('',#16276,.T.);
#10354=FACE_OUTER_BOUND('',#16277,.T.);
#10355=FACE_OUTER_BOUND('',#16278,.T.);
#10356=FACE_OUTER_BOUND('',#16279,.T.);
#10357=FACE_OUTER_BOUND('',#16280,.T.);
#10358=FACE_OUTER_BOUND('',#16281,.T.);
#10359=FACE_OUTER_BOUND('',#16282,.T.);
#10360=FACE_OUTER_BOUND('',#16283,.T.);
#10361=FACE_OUTER_BOUND('',#16284,.T.);
#10362=FACE_OUTER_BOUND('',#16285,.T.);
#10363=FACE_OUTER_BOUND('',#16286,.T.);
#10364=FACE_OUTER_BOUND('',#16287,.T.);
#10365=FACE_OUTER_BOUND('',#16288,.T.);
#10366=FACE_OUTER_BOUND('',#16289,.T.);
#10367=FACE_OUTER_BOUND('',#16290,.T.);
#10368=FACE_OUTER_BOUND('',#16291,.T.);
#10369=FACE_OUTER_BOUND('',#16292,.T.);
#10370=FACE_OUTER_BOUND('',#16293,.T.);
#10371=FACE_OUTER_BOUND('',#16294,.T.);
#10372=FACE_OUTER_BOUND('',#16295,.T.);
#10373=FACE_OUTER_BOUND('',#16296,.T.);
#10374=FACE_OUTER_BOUND('',#16297,.T.);
#10375=FACE_OUTER_BOUND('',#16298,.T.);
#10376=FACE_OUTER_BOUND('',#16299,.T.);
#10377=FACE_OUTER_BOUND('',#16300,.T.);
#10378=FACE_OUTER_BOUND('',#16301,.T.);
#10379=FACE_OUTER_BOUND('',#16302,.T.);
#10380=FACE_OUTER_BOUND('',#16303,.T.);
#10381=FACE_OUTER_BOUND('',#16304,.T.);
#10382=FACE_OUTER_BOUND('',#16305,.T.);
#10383=FACE_OUTER_BOUND('',#16306,.T.);
#10384=FACE_OUTER_BOUND('',#16307,.T.);
#10385=FACE_OUTER_BOUND('',#16308,.T.);
#10386=FACE_OUTER_BOUND('',#16309,.T.);
#10387=FACE_OUTER_BOUND('',#16310,.T.);
#10388=FACE_OUTER_BOUND('',#16311,.T.);
#10389=FACE_OUTER_BOUND('',#16312,.T.);
#10390=FACE_OUTER_BOUND('',#16313,.T.);
#10391=FACE_OUTER_BOUND('',#16314,.T.);
#10392=FACE_OUTER_BOUND('',#16315,.T.);
#10393=FACE_OUTER_BOUND('',#16316,.T.);
#10394=FACE_OUTER_BOUND('',#16317,.T.);
#10395=FACE_OUTER_BOUND('',#16318,.T.);
#10396=FACE_OUTER_BOUND('',#16319,.T.);
#10397=FACE_OUTER_BOUND('',#16320,.T.);
#10398=FACE_OUTER_BOUND('',#16321,.T.);
#10399=FACE_OUTER_BOUND('',#16322,.T.);
#10400=FACE_OUTER_BOUND('',#16323,.T.);
#10401=FACE_OUTER_BOUND('',#16324,.T.);
#10402=FACE_OUTER_BOUND('',#16325,.T.);
#10403=FACE_OUTER_BOUND('',#16326,.T.);
#10404=FACE_OUTER_BOUND('',#16327,.T.);
#10405=FACE_OUTER_BOUND('',#16328,.T.);
#10406=FACE_OUTER_BOUND('',#16329,.T.);
#10407=FACE_OUTER_BOUND('',#16330,.T.);
#10408=FACE_OUTER_BOUND('',#16331,.T.);
#10409=FACE_OUTER_BOUND('',#16332,.T.);
#10410=FACE_OUTER_BOUND('',#16333,.T.);
#10411=FACE_OUTER_BOUND('',#16334,.T.);
#10412=FACE_OUTER_BOUND('',#16335,.T.);
#10413=FACE_OUTER_BOUND('',#16336,.T.);
#10414=FACE_OUTER_BOUND('',#16337,.T.);
#10415=FACE_OUTER_BOUND('',#16338,.T.);
#10416=FACE_OUTER_BOUND('',#16339,.T.);
#10417=FACE_OUTER_BOUND('',#16340,.T.);
#10418=FACE_OUTER_BOUND('',#16341,.T.);
#10419=FACE_OUTER_BOUND('',#16342,.T.);
#10420=FACE_OUTER_BOUND('',#16343,.T.);
#10421=FACE_OUTER_BOUND('',#16344,.T.);
#10422=FACE_OUTER_BOUND('',#16345,.T.);
#10423=FACE_OUTER_BOUND('',#16346,.T.);
#10424=FACE_OUTER_BOUND('',#16347,.T.);
#10425=FACE_OUTER_BOUND('',#16348,.T.);
#10426=FACE_OUTER_BOUND('',#16349,.T.);
#10427=FACE_OUTER_BOUND('',#16350,.T.);
#10428=FACE_OUTER_BOUND('',#16351,.T.);
#10429=FACE_OUTER_BOUND('',#16352,.T.);
#10430=FACE_OUTER_BOUND('',#16353,.T.);
#10431=FACE_OUTER_BOUND('',#16354,.T.);
#10432=FACE_OUTER_BOUND('',#16355,.T.);
#10433=FACE_OUTER_BOUND('',#16356,.T.);
#10434=FACE_OUTER_BOUND('',#16357,.T.);
#10435=FACE_OUTER_BOUND('',#16358,.T.);
#10436=FACE_OUTER_BOUND('',#16359,.T.);
#10437=FACE_OUTER_BOUND('',#16360,.T.);
#10438=FACE_OUTER_BOUND('',#16361,.T.);
#10439=FACE_OUTER_BOUND('',#16362,.T.);
#10440=FACE_OUTER_BOUND('',#16363,.T.);
#10441=FACE_OUTER_BOUND('',#16364,.T.);
#10442=FACE_OUTER_BOUND('',#16365,.T.);
#10443=FACE_OUTER_BOUND('',#16366,.T.);
#10444=FACE_OUTER_BOUND('',#16367,.T.);
#10445=FACE_OUTER_BOUND('',#16368,.T.);
#10446=FACE_OUTER_BOUND('',#16369,.T.);
#10447=FACE_OUTER_BOUND('',#16370,.T.);
#10448=FACE_OUTER_BOUND('',#16371,.T.);
#10449=FACE_OUTER_BOUND('',#16372,.T.);
#10450=FACE_OUTER_BOUND('',#16373,.T.);
#10451=FACE_OUTER_BOUND('',#16374,.T.);
#10452=FACE_OUTER_BOUND('',#16375,.T.);
#10453=FACE_OUTER_BOUND('',#16376,.T.);
#10454=FACE_OUTER_BOUND('',#16377,.T.);
#10455=FACE_OUTER_BOUND('',#16378,.T.);
#10456=FACE_OUTER_BOUND('',#16379,.T.);
#10457=FACE_OUTER_BOUND('',#16380,.T.);
#10458=FACE_OUTER_BOUND('',#16381,.T.);
#10459=FACE_OUTER_BOUND('',#16382,.T.);
#10460=FACE_OUTER_BOUND('',#16383,.T.);
#10461=FACE_OUTER_BOUND('',#16384,.T.);
#10462=FACE_OUTER_BOUND('',#16385,.T.);
#10463=FACE_OUTER_BOUND('',#16386,.T.);
#10464=FACE_OUTER_BOUND('',#16387,.T.);
#10465=FACE_OUTER_BOUND('',#16388,.T.);
#10466=FACE_OUTER_BOUND('',#16389,.T.);
#10467=FACE_OUTER_BOUND('',#16390,.T.);
#10468=FACE_OUTER_BOUND('',#16391,.T.);
#10469=FACE_OUTER_BOUND('',#16392,.T.);
#10470=FACE_OUTER_BOUND('',#16393,.T.);
#10471=FACE_OUTER_BOUND('',#16394,.T.);
#10472=FACE_OUTER_BOUND('',#16395,.T.);
#10473=FACE_OUTER_BOUND('',#16396,.T.);
#10474=FACE_OUTER_BOUND('',#16397,.T.);
#10475=FACE_OUTER_BOUND('',#16398,.T.);
#10476=FACE_OUTER_BOUND('',#16399,.T.);
#10477=FACE_OUTER_BOUND('',#16400,.T.);
#10478=FACE_OUTER_BOUND('',#16401,.T.);
#10479=FACE_OUTER_BOUND('',#16402,.T.);
#10480=FACE_OUTER_BOUND('',#16403,.T.);
#10481=FACE_OUTER_BOUND('',#16404,.T.);
#10482=FACE_OUTER_BOUND('',#16405,.T.);
#10483=FACE_OUTER_BOUND('',#16406,.T.);
#10484=FACE_OUTER_BOUND('',#16407,.T.);
#10485=FACE_OUTER_BOUND('',#16408,.T.);
#10486=FACE_OUTER_BOUND('',#16409,.T.);
#10487=FACE_OUTER_BOUND('',#16410,.T.);
#10488=FACE_OUTER_BOUND('',#16411,.T.);
#10489=FACE_OUTER_BOUND('',#16412,.T.);
#10490=FACE_OUTER_BOUND('',#16413,.T.);
#10491=FACE_OUTER_BOUND('',#16414,.T.);
#10492=FACE_OUTER_BOUND('',#16415,.T.);
#10493=FACE_OUTER_BOUND('',#16416,.T.);
#10494=FACE_OUTER_BOUND('',#16417,.T.);
#10495=FACE_OUTER_BOUND('',#16418,.T.);
#10496=FACE_OUTER_BOUND('',#16419,.T.);
#10497=FACE_OUTER_BOUND('',#16420,.T.);
#10498=FACE_OUTER_BOUND('',#16421,.T.);
#10499=FACE_OUTER_BOUND('',#16422,.T.);
#10500=FACE_OUTER_BOUND('',#16423,.T.);
#10501=FACE_OUTER_BOUND('',#16424,.T.);
#10502=FACE_OUTER_BOUND('',#16425,.T.);
#10503=FACE_OUTER_BOUND('',#16426,.T.);
#10504=FACE_OUTER_BOUND('',#16427,.T.);
#10505=FACE_OUTER_BOUND('',#16428,.T.);
#10506=FACE_OUTER_BOUND('',#16429,.T.);
#10507=FACE_OUTER_BOUND('',#16430,.T.);
#10508=FACE_OUTER_BOUND('',#16431,.T.);
#10509=FACE_OUTER_BOUND('',#16432,.T.);
#10510=FACE_OUTER_BOUND('',#16433,.T.);
#10511=FACE_OUTER_BOUND('',#16434,.T.);
#10512=FACE_OUTER_BOUND('',#16435,.T.);
#10513=FACE_OUTER_BOUND('',#16436,.T.);
#10514=FACE_OUTER_BOUND('',#16437,.T.);
#10515=FACE_OUTER_BOUND('',#16438,.T.);
#10516=FACE_OUTER_BOUND('',#16439,.T.);
#10517=FACE_OUTER_BOUND('',#16440,.T.);
#10518=FACE_OUTER_BOUND('',#16441,.T.);
#10519=FACE_OUTER_BOUND('',#16442,.T.);
#10520=FACE_OUTER_BOUND('',#16443,.T.);
#10521=FACE_OUTER_BOUND('',#16444,.T.);
#10522=FACE_OUTER_BOUND('',#16445,.T.);
#10523=FACE_OUTER_BOUND('',#16446,.T.);
#10524=FACE_OUTER_BOUND('',#16447,.T.);
#10525=FACE_OUTER_BOUND('',#16448,.T.);
#10526=FACE_OUTER_BOUND('',#16449,.T.);
#10527=FACE_OUTER_BOUND('',#16450,.T.);
#10528=FACE_OUTER_BOUND('',#16451,.T.);
#10529=FACE_OUTER_BOUND('',#16452,.T.);
#10530=FACE_OUTER_BOUND('',#16453,.T.);
#10531=FACE_OUTER_BOUND('',#16454,.T.);
#10532=FACE_OUTER_BOUND('',#16455,.T.);
#10533=FACE_OUTER_BOUND('',#16456,.T.);
#10534=FACE_OUTER_BOUND('',#16457,.T.);
#10535=FACE_OUTER_BOUND('',#16458,.T.);
#10536=FACE_OUTER_BOUND('',#16459,.T.);
#10537=FACE_OUTER_BOUND('',#16460,.T.);
#10538=FACE_OUTER_BOUND('',#16461,.T.);
#10539=FACE_OUTER_BOUND('',#16462,.T.);
#10540=FACE_OUTER_BOUND('',#16463,.T.);
#10541=FACE_OUTER_BOUND('',#16464,.T.);
#10542=FACE_OUTER_BOUND('',#16465,.T.);
#10543=FACE_OUTER_BOUND('',#16466,.T.);
#10544=FACE_OUTER_BOUND('',#16467,.T.);
#10545=FACE_OUTER_BOUND('',#16468,.T.);
#10546=FACE_OUTER_BOUND('',#16469,.T.);
#10547=FACE_OUTER_BOUND('',#16470,.T.);
#10548=FACE_OUTER_BOUND('',#16471,.T.);
#10549=FACE_OUTER_BOUND('',#16472,.T.);
#10550=FACE_OUTER_BOUND('',#16473,.T.);
#10551=FACE_OUTER_BOUND('',#16474,.T.);
#10552=FACE_OUTER_BOUND('',#16475,.T.);
#10553=FACE_OUTER_BOUND('',#16476,.T.);
#10554=FACE_OUTER_BOUND('',#16477,.T.);
#10555=FACE_OUTER_BOUND('',#16478,.T.);
#10556=FACE_OUTER_BOUND('',#16479,.T.);
#10557=FACE_OUTER_BOUND('',#16480,.T.);
#10558=FACE_OUTER_BOUND('',#16481,.T.);
#10559=FACE_OUTER_BOUND('',#16482,.T.);
#10560=FACE_OUTER_BOUND('',#16483,.T.);
#10561=FACE_OUTER_BOUND('',#16484,.T.);
#10562=FACE_OUTER_BOUND('',#16485,.T.);
#10563=FACE_OUTER_BOUND('',#16486,.T.);
#10564=FACE_OUTER_BOUND('',#16487,.T.);
#10565=FACE_OUTER_BOUND('',#16488,.T.);
#10566=FACE_OUTER_BOUND('',#16489,.T.);
#10567=FACE_OUTER_BOUND('',#16490,.T.);
#10568=FACE_OUTER_BOUND('',#16491,.T.);
#10569=FACE_OUTER_BOUND('',#16492,.T.);
#10570=FACE_OUTER_BOUND('',#16493,.T.);
#10571=FACE_OUTER_BOUND('',#16494,.T.);
#10572=FACE_OUTER_BOUND('',#16495,.T.);
#10573=FACE_OUTER_BOUND('',#16496,.T.);
#10574=FACE_OUTER_BOUND('',#16497,.T.);
#10575=FACE_OUTER_BOUND('',#16498,.T.);
#10576=FACE_OUTER_BOUND('',#16499,.T.);
#10577=FACE_OUTER_BOUND('',#16500,.T.);
#10578=FACE_OUTER_BOUND('',#16501,.T.);
#10579=FACE_OUTER_BOUND('',#16502,.T.);
#10580=FACE_OUTER_BOUND('',#16503,.T.);
#10581=FACE_OUTER_BOUND('',#16504,.T.);
#10582=FACE_OUTER_BOUND('',#16505,.T.);
#10583=FACE_OUTER_BOUND('',#16506,.T.);
#10584=FACE_OUTER_BOUND('',#16507,.T.);
#10585=FACE_OUTER_BOUND('',#16508,.T.);
#10586=FACE_OUTER_BOUND('',#16509,.T.);
#10587=FACE_OUTER_BOUND('',#16510,.T.);
#10588=FACE_OUTER_BOUND('',#16511,.T.);
#10589=FACE_OUTER_BOUND('',#16512,.T.);
#10590=FACE_OUTER_BOUND('',#16513,.T.);
#10591=FACE_OUTER_BOUND('',#16514,.T.);
#10592=FACE_OUTER_BOUND('',#16515,.T.);
#10593=FACE_OUTER_BOUND('',#16516,.T.);
#10594=FACE_OUTER_BOUND('',#16517,.T.);
#10595=FACE_OUTER_BOUND('',#16518,.T.);
#10596=FACE_OUTER_BOUND('',#16519,.T.);
#10597=FACE_OUTER_BOUND('',#16520,.T.);
#10598=FACE_OUTER_BOUND('',#16521,.T.);
#10599=FACE_OUTER_BOUND('',#16522,.T.);
#10600=FACE_OUTER_BOUND('',#16523,.T.);
#10601=FACE_OUTER_BOUND('',#16524,.T.);
#10602=FACE_OUTER_BOUND('',#16525,.T.);
#10603=FACE_OUTER_BOUND('',#16526,.T.);
#10604=FACE_OUTER_BOUND('',#16527,.T.);
#10605=FACE_OUTER_BOUND('',#16528,.T.);
#10606=FACE_OUTER_BOUND('',#16529,.T.);
#10607=FACE_OUTER_BOUND('',#16530,.T.);
#10608=FACE_OUTER_BOUND('',#16531,.T.);
#10609=FACE_OUTER_BOUND('',#16532,.T.);
#10610=FACE_OUTER_BOUND('',#16533,.T.);
#10611=FACE_OUTER_BOUND('',#16534,.T.);
#10612=FACE_OUTER_BOUND('',#16535,.T.);
#10613=FACE_OUTER_BOUND('',#16536,.T.);
#10614=FACE_OUTER_BOUND('',#16537,.T.);
#10615=FACE_OUTER_BOUND('',#16538,.T.);
#10616=FACE_OUTER_BOUND('',#16539,.T.);
#10617=FACE_OUTER_BOUND('',#16540,.T.);
#10618=FACE_OUTER_BOUND('',#16541,.T.);
#10619=FACE_OUTER_BOUND('',#16542,.T.);
#10620=FACE_OUTER_BOUND('',#16543,.T.);
#10621=FACE_OUTER_BOUND('',#16544,.T.);
#10622=FACE_OUTER_BOUND('',#16545,.T.);
#10623=FACE_OUTER_BOUND('',#16546,.T.);
#10624=FACE_OUTER_BOUND('',#16547,.T.);
#10625=FACE_OUTER_BOUND('',#16548,.T.);
#10626=FACE_OUTER_BOUND('',#16549,.T.);
#10627=FACE_OUTER_BOUND('',#16550,.T.);
#10628=FACE_OUTER_BOUND('',#16551,.T.);
#10629=FACE_OUTER_BOUND('',#16552,.T.);
#10630=FACE_OUTER_BOUND('',#16553,.T.);
#10631=FACE_OUTER_BOUND('',#16554,.T.);
#10632=FACE_OUTER_BOUND('',#16555,.T.);
#10633=FACE_OUTER_BOUND('',#16556,.T.);
#10634=FACE_OUTER_BOUND('',#16557,.T.);
#10635=FACE_OUTER_BOUND('',#16558,.T.);
#10636=FACE_OUTER_BOUND('',#16559,.T.);
#10637=FACE_OUTER_BOUND('',#16560,.T.);
#10638=FACE_OUTER_BOUND('',#16561,.T.);
#10639=FACE_OUTER_BOUND('',#16562,.T.);
#10640=FACE_OUTER_BOUND('',#16563,.T.);
#10641=FACE_OUTER_BOUND('',#16564,.T.);
#10642=FACE_OUTER_BOUND('',#16565,.T.);
#10643=FACE_OUTER_BOUND('',#16566,.T.);
#10644=FACE_OUTER_BOUND('',#16567,.T.);
#10645=FACE_OUTER_BOUND('',#16568,.T.);
#10646=FACE_OUTER_BOUND('',#16569,.T.);
#10647=FACE_OUTER_BOUND('',#16570,.T.);
#10648=FACE_OUTER_BOUND('',#16571,.T.);
#10649=FACE_OUTER_BOUND('',#16572,.T.);
#10650=FACE_OUTER_BOUND('',#16573,.T.);
#10651=FACE_OUTER_BOUND('',#16575,.T.);
#10652=FACE_OUTER_BOUND('',#16576,.T.);
#10653=FACE_OUTER_BOUND('',#16577,.T.);
#10654=FACE_OUTER_BOUND('',#16578,.T.);
#10655=FACE_OUTER_BOUND('',#16579,.T.);
#10656=FACE_OUTER_BOUND('',#16580,.T.);
#10657=FACE_OUTER_BOUND('',#16582,.T.);
#10658=FACE_OUTER_BOUND('',#16583,.T.);
#10659=FACE_OUTER_BOUND('',#16584,.T.);
#10660=FACE_OUTER_BOUND('',#16585,.T.);
#10661=FACE_OUTER_BOUND('',#16586,.T.);
#10662=FACE_OUTER_BOUND('',#16587,.T.);
#10663=FACE_OUTER_BOUND('',#16588,.T.);
#10664=FACE_OUTER_BOUND('',#16589,.T.);
#10665=FACE_OUTER_BOUND('',#16590,.T.);
#10666=FACE_OUTER_BOUND('',#16591,.T.);
#10667=FACE_OUTER_BOUND('',#16592,.T.);
#10668=FACE_OUTER_BOUND('',#16593,.T.);
#10669=FACE_OUTER_BOUND('',#16594,.T.);
#10670=FACE_OUTER_BOUND('',#16595,.T.);
#10671=FACE_OUTER_BOUND('',#16596,.T.);
#10672=FACE_OUTER_BOUND('',#16597,.T.);
#10673=FACE_OUTER_BOUND('',#16598,.T.);
#10674=FACE_OUTER_BOUND('',#16599,.T.);
#10675=FACE_OUTER_BOUND('',#16600,.T.);
#10676=FACE_OUTER_BOUND('',#16601,.T.);
#10677=FACE_OUTER_BOUND('',#16602,.T.);
#10678=FACE_OUTER_BOUND('',#16603,.T.);
#10679=FACE_OUTER_BOUND('',#16604,.T.);
#10680=FACE_OUTER_BOUND('',#16605,.T.);
#10681=FACE_OUTER_BOUND('',#16606,.T.);
#10682=FACE_OUTER_BOUND('',#16607,.T.);
#10683=FACE_OUTER_BOUND('',#16608,.T.);
#10684=FACE_OUTER_BOUND('',#16609,.T.);
#10685=FACE_OUTER_BOUND('',#16610,.T.);
#10686=FACE_OUTER_BOUND('',#16611,.T.);
#10687=FACE_OUTER_BOUND('',#16612,.T.);
#10688=FACE_OUTER_BOUND('',#16613,.T.);
#10689=FACE_OUTER_BOUND('',#16614,.T.);
#10690=FACE_OUTER_BOUND('',#16615,.T.);
#10691=FACE_OUTER_BOUND('',#16616,.T.);
#10692=FACE_OUTER_BOUND('',#16617,.T.);
#10693=FACE_OUTER_BOUND('',#16618,.T.);
#10694=FACE_OUTER_BOUND('',#16619,.T.);
#10695=FACE_OUTER_BOUND('',#16620,.T.);
#10696=FACE_OUTER_BOUND('',#16621,.T.);
#10697=FACE_OUTER_BOUND('',#16622,.T.);
#10698=FACE_OUTER_BOUND('',#16623,.T.);
#10699=FACE_OUTER_BOUND('',#16624,.T.);
#10700=FACE_OUTER_BOUND('',#16625,.T.);
#10701=FACE_OUTER_BOUND('',#16626,.T.);
#10702=FACE_OUTER_BOUND('',#16627,.T.);
#10703=FACE_OUTER_BOUND('',#16628,.T.);
#10704=FACE_OUTER_BOUND('',#16629,.T.);
#10705=FACE_OUTER_BOUND('',#16630,.T.);
#10706=FACE_OUTER_BOUND('',#16631,.T.);
#10707=FACE_OUTER_BOUND('',#16632,.T.);
#10708=FACE_OUTER_BOUND('',#16633,.T.);
#10709=FACE_OUTER_BOUND('',#16634,.T.);
#10710=FACE_OUTER_BOUND('',#16635,.T.);
#10711=FACE_OUTER_BOUND('',#16636,.T.);
#10712=FACE_OUTER_BOUND('',#16637,.T.);
#10713=FACE_OUTER_BOUND('',#16638,.T.);
#10714=FACE_OUTER_BOUND('',#16639,.T.);
#10715=FACE_OUTER_BOUND('',#16640,.T.);
#10716=FACE_OUTER_BOUND('',#16641,.T.);
#10717=FACE_OUTER_BOUND('',#16642,.T.);
#10718=FACE_OUTER_BOUND('',#16643,.T.);
#10719=FACE_OUTER_BOUND('',#16644,.T.);
#10720=FACE_OUTER_BOUND('',#16645,.T.);
#10721=FACE_OUTER_BOUND('',#16646,.T.);
#10722=FACE_OUTER_BOUND('',#16647,.T.);
#10723=FACE_OUTER_BOUND('',#16648,.T.);
#10724=FACE_OUTER_BOUND('',#16649,.T.);
#10725=FACE_OUTER_BOUND('',#16650,.T.);
#10726=FACE_OUTER_BOUND('',#16651,.T.);
#10727=FACE_OUTER_BOUND('',#16652,.T.);
#10728=FACE_OUTER_BOUND('',#16653,.T.);
#10729=FACE_OUTER_BOUND('',#16654,.T.);
#10730=FACE_OUTER_BOUND('',#16655,.T.);
#10731=FACE_OUTER_BOUND('',#16656,.T.);
#10732=FACE_OUTER_BOUND('',#16657,.T.);
#10733=FACE_OUTER_BOUND('',#16658,.T.);
#10734=FACE_OUTER_BOUND('',#16659,.T.);
#10735=FACE_OUTER_BOUND('',#16660,.T.);
#10736=FACE_OUTER_BOUND('',#16661,.T.);
#10737=FACE_OUTER_BOUND('',#16662,.T.);
#10738=FACE_OUTER_BOUND('',#16663,.T.);
#10739=FACE_OUTER_BOUND('',#16664,.T.);
#10740=FACE_OUTER_BOUND('',#16665,.T.);
#10741=FACE_OUTER_BOUND('',#16666,.T.);
#10742=FACE_OUTER_BOUND('',#16667,.T.);
#10743=FACE_OUTER_BOUND('',#16668,.T.);
#10744=FACE_OUTER_BOUND('',#16669,.T.);
#10745=FACE_OUTER_BOUND('',#16670,.T.);
#10746=FACE_OUTER_BOUND('',#16671,.T.);
#10747=FACE_OUTER_BOUND('',#16672,.T.);
#10748=FACE_OUTER_BOUND('',#16673,.T.);
#10749=FACE_OUTER_BOUND('',#16674,.T.);
#10750=FACE_OUTER_BOUND('',#16675,.T.);
#10751=FACE_OUTER_BOUND('',#16676,.T.);
#10752=FACE_OUTER_BOUND('',#16677,.T.);
#10753=FACE_OUTER_BOUND('',#16678,.T.);
#10754=FACE_OUTER_BOUND('',#16679,.T.);
#10755=FACE_OUTER_BOUND('',#16680,.T.);
#10756=FACE_OUTER_BOUND('',#16681,.T.);
#10757=FACE_OUTER_BOUND('',#16682,.T.);
#10758=FACE_OUTER_BOUND('',#16683,.T.);
#10759=FACE_OUTER_BOUND('',#16684,.T.);
#10760=FACE_OUTER_BOUND('',#16685,.T.);
#10761=FACE_OUTER_BOUND('',#16686,.T.);
#10762=FACE_OUTER_BOUND('',#16687,.T.);
#10763=FACE_OUTER_BOUND('',#16688,.T.);
#10764=FACE_OUTER_BOUND('',#16689,.T.);
#10765=FACE_OUTER_BOUND('',#16690,.T.);
#10766=FACE_OUTER_BOUND('',#16691,.T.);
#10767=FACE_OUTER_BOUND('',#16692,.T.);
#10768=FACE_OUTER_BOUND('',#16693,.T.);
#10769=FACE_OUTER_BOUND('',#16694,.T.);
#10770=FACE_OUTER_BOUND('',#16695,.T.);
#10771=FACE_OUTER_BOUND('',#16696,.T.);
#10772=FACE_OUTER_BOUND('',#16697,.T.);
#10773=FACE_OUTER_BOUND('',#16698,.T.);
#10774=FACE_OUTER_BOUND('',#16699,.T.);
#10775=FACE_OUTER_BOUND('',#16700,.T.);
#10776=FACE_OUTER_BOUND('',#16701,.T.);
#10777=FACE_OUTER_BOUND('',#16702,.T.);
#10778=FACE_OUTER_BOUND('',#16703,.T.);
#10779=FACE_OUTER_BOUND('',#16704,.T.);
#10780=FACE_OUTER_BOUND('',#16705,.T.);
#10781=FACE_OUTER_BOUND('',#16706,.T.);
#10782=FACE_OUTER_BOUND('',#16707,.T.);
#10783=FACE_OUTER_BOUND('',#16708,.T.);
#10784=FACE_OUTER_BOUND('',#16709,.T.);
#10785=FACE_OUTER_BOUND('',#16710,.T.);
#10786=FACE_OUTER_BOUND('',#16711,.T.);
#10787=FACE_OUTER_BOUND('',#16712,.T.);
#10788=FACE_OUTER_BOUND('',#16713,.T.);
#10789=FACE_OUTER_BOUND('',#16714,.T.);
#10790=FACE_OUTER_BOUND('',#16715,.T.);
#10791=FACE_OUTER_BOUND('',#16716,.T.);
#10792=FACE_OUTER_BOUND('',#16717,.T.);
#10793=FACE_OUTER_BOUND('',#16718,.T.);
#10794=FACE_OUTER_BOUND('',#16719,.T.);
#10795=FACE_OUTER_BOUND('',#16720,.T.);
#10796=FACE_OUTER_BOUND('',#16721,.T.);
#10797=FACE_OUTER_BOUND('',#16722,.T.);
#10798=FACE_OUTER_BOUND('',#16723,.T.);
#10799=FACE_OUTER_BOUND('',#16724,.T.);
#10800=FACE_OUTER_BOUND('',#16725,.T.);
#10801=FACE_OUTER_BOUND('',#16726,.T.);
#10802=FACE_OUTER_BOUND('',#16727,.T.);
#10803=FACE_OUTER_BOUND('',#16728,.T.);
#10804=FACE_OUTER_BOUND('',#16729,.T.);
#10805=FACE_OUTER_BOUND('',#16730,.T.);
#10806=FACE_OUTER_BOUND('',#16731,.T.);
#10807=FACE_OUTER_BOUND('',#16732,.T.);
#10808=FACE_OUTER_BOUND('',#16733,.T.);
#10809=FACE_OUTER_BOUND('',#16734,.T.);
#10810=FACE_OUTER_BOUND('',#16735,.T.);
#10811=FACE_OUTER_BOUND('',#16736,.T.);
#10812=FACE_OUTER_BOUND('',#16737,.T.);
#10813=FACE_OUTER_BOUND('',#16738,.T.);
#10814=FACE_OUTER_BOUND('',#16739,.T.);
#10815=FACE_OUTER_BOUND('',#16740,.T.);
#10816=FACE_OUTER_BOUND('',#16741,.T.);
#10817=FACE_OUTER_BOUND('',#16742,.T.);
#10818=FACE_OUTER_BOUND('',#16743,.T.);
#10819=FACE_OUTER_BOUND('',#16744,.T.);
#10820=FACE_OUTER_BOUND('',#16745,.T.);
#10821=FACE_OUTER_BOUND('',#16746,.T.);
#10822=FACE_OUTER_BOUND('',#16747,.T.);
#10823=FACE_OUTER_BOUND('',#16748,.T.);
#10824=FACE_OUTER_BOUND('',#16749,.T.);
#10825=FACE_OUTER_BOUND('',#16750,.T.);
#10826=FACE_OUTER_BOUND('',#16751,.T.);
#10827=FACE_OUTER_BOUND('',#16752,.T.);
#10828=FACE_OUTER_BOUND('',#16753,.T.);
#10829=FACE_OUTER_BOUND('',#16754,.T.);
#10830=FACE_OUTER_BOUND('',#16755,.T.);
#10831=FACE_OUTER_BOUND('',#16756,.T.);
#10832=FACE_OUTER_BOUND('',#16757,.T.);
#10833=FACE_OUTER_BOUND('',#16758,.T.);
#10834=FACE_OUTER_BOUND('',#16759,.T.);
#10835=FACE_OUTER_BOUND('',#16760,.T.);
#10836=FACE_OUTER_BOUND('',#16761,.T.);
#10837=FACE_OUTER_BOUND('',#16762,.T.);
#10838=FACE_OUTER_BOUND('',#16763,.T.);
#10839=FACE_OUTER_BOUND('',#16764,.T.);
#10840=FACE_OUTER_BOUND('',#16765,.T.);
#10841=FACE_OUTER_BOUND('',#16766,.T.);
#10842=FACE_OUTER_BOUND('',#16767,.T.);
#10843=FACE_OUTER_BOUND('',#16768,.T.);
#10844=FACE_OUTER_BOUND('',#16769,.T.);
#10845=FACE_OUTER_BOUND('',#16770,.T.);
#10846=FACE_OUTER_BOUND('',#16771,.T.);
#10847=FACE_OUTER_BOUND('',#16772,.T.);
#10848=FACE_OUTER_BOUND('',#16773,.T.);
#10849=FACE_OUTER_BOUND('',#16774,.T.);
#10850=FACE_OUTER_BOUND('',#16775,.T.);
#10851=FACE_OUTER_BOUND('',#16776,.T.);
#10852=FACE_OUTER_BOUND('',#16777,.T.);
#10853=FACE_OUTER_BOUND('',#16778,.T.);
#10854=FACE_OUTER_BOUND('',#16779,.T.);
#10855=FACE_OUTER_BOUND('',#16780,.T.);
#10856=FACE_OUTER_BOUND('',#16781,.T.);
#10857=FACE_OUTER_BOUND('',#16782,.T.);
#10858=FACE_OUTER_BOUND('',#16783,.T.);
#10859=FACE_OUTER_BOUND('',#16784,.T.);
#10860=FACE_OUTER_BOUND('',#16785,.T.);
#10861=FACE_OUTER_BOUND('',#16786,.T.);
#10862=FACE_OUTER_BOUND('',#16787,.T.);
#10863=FACE_OUTER_BOUND('',#16788,.T.);
#10864=FACE_OUTER_BOUND('',#16789,.T.);
#10865=FACE_OUTER_BOUND('',#16790,.T.);
#10866=FACE_OUTER_BOUND('',#16791,.T.);
#10867=FACE_OUTER_BOUND('',#16792,.T.);
#10868=FACE_OUTER_BOUND('',#16793,.T.);
#10869=FACE_OUTER_BOUND('',#16794,.T.);
#10870=FACE_OUTER_BOUND('',#16795,.T.);
#10871=FACE_OUTER_BOUND('',#16796,.T.);
#10872=FACE_OUTER_BOUND('',#16797,.T.);
#10873=FACE_OUTER_BOUND('',#16798,.T.);
#10874=FACE_OUTER_BOUND('',#16799,.T.);
#10875=FACE_OUTER_BOUND('',#16800,.T.);
#10876=FACE_OUTER_BOUND('',#16801,.T.);
#10877=FACE_OUTER_BOUND('',#16802,.T.);
#10878=FACE_OUTER_BOUND('',#16803,.T.);
#10879=FACE_OUTER_BOUND('',#16804,.T.);
#10880=FACE_OUTER_BOUND('',#16805,.T.);
#10881=FACE_OUTER_BOUND('',#16806,.T.);
#10882=FACE_OUTER_BOUND('',#16807,.T.);
#10883=FACE_OUTER_BOUND('',#16808,.T.);
#10884=FACE_OUTER_BOUND('',#16809,.T.);
#10885=FACE_OUTER_BOUND('',#16810,.T.);
#10886=FACE_OUTER_BOUND('',#16811,.T.);
#10887=FACE_OUTER_BOUND('',#16812,.T.);
#10888=FACE_OUTER_BOUND('',#16813,.T.);
#10889=FACE_OUTER_BOUND('',#16814,.T.);
#10890=FACE_OUTER_BOUND('',#16815,.T.);
#10891=FACE_OUTER_BOUND('',#16816,.T.);
#10892=FACE_OUTER_BOUND('',#16817,.T.);
#10893=FACE_OUTER_BOUND('',#16818,.T.);
#10894=FACE_OUTER_BOUND('',#16819,.T.);
#10895=FACE_OUTER_BOUND('',#16820,.T.);
#10896=FACE_OUTER_BOUND('',#16821,.T.);
#10897=FACE_OUTER_BOUND('',#16822,.T.);
#10898=FACE_OUTER_BOUND('',#16823,.T.);
#10899=FACE_OUTER_BOUND('',#16824,.T.);
#10900=FACE_OUTER_BOUND('',#16825,.T.);
#10901=FACE_OUTER_BOUND('',#16826,.T.);
#10902=FACE_OUTER_BOUND('',#16827,.T.);
#10903=FACE_OUTER_BOUND('',#16828,.T.);
#10904=FACE_OUTER_BOUND('',#16829,.T.);
#10905=FACE_OUTER_BOUND('',#16830,.T.);
#10906=FACE_OUTER_BOUND('',#16831,.T.);
#10907=FACE_OUTER_BOUND('',#16832,.T.);
#10908=FACE_OUTER_BOUND('',#16833,.T.);
#10909=FACE_OUTER_BOUND('',#16834,.T.);
#10910=FACE_OUTER_BOUND('',#16835,.T.);
#10911=FACE_OUTER_BOUND('',#16836,.T.);
#10912=FACE_OUTER_BOUND('',#16837,.T.);
#10913=FACE_OUTER_BOUND('',#16838,.T.);
#10914=FACE_OUTER_BOUND('',#16839,.T.);
#10915=FACE_OUTER_BOUND('',#16840,.T.);
#10916=FACE_OUTER_BOUND('',#16841,.T.);
#10917=FACE_OUTER_BOUND('',#16842,.T.);
#10918=FACE_OUTER_BOUND('',#16843,.T.);
#10919=FACE_OUTER_BOUND('',#16844,.T.);
#10920=FACE_OUTER_BOUND('',#16845,.T.);
#10921=FACE_OUTER_BOUND('',#16846,.T.);
#10922=FACE_OUTER_BOUND('',#16847,.T.);
#10923=FACE_OUTER_BOUND('',#16848,.T.);
#10924=FACE_OUTER_BOUND('',#16849,.T.);
#10925=FACE_OUTER_BOUND('',#16850,.T.);
#10926=FACE_OUTER_BOUND('',#16851,.T.);
#10927=FACE_OUTER_BOUND('',#16852,.T.);
#10928=FACE_OUTER_BOUND('',#16853,.T.);
#10929=FACE_OUTER_BOUND('',#16854,.T.);
#10930=FACE_OUTER_BOUND('',#16855,.T.);
#10931=FACE_OUTER_BOUND('',#16856,.T.);
#10932=FACE_OUTER_BOUND('',#16857,.T.);
#10933=FACE_OUTER_BOUND('',#16858,.T.);
#10934=FACE_OUTER_BOUND('',#16859,.T.);
#10935=FACE_OUTER_BOUND('',#16860,.T.);
#10936=FACE_OUTER_BOUND('',#16861,.T.);
#10937=FACE_OUTER_BOUND('',#16862,.T.);
#10938=FACE_OUTER_BOUND('',#16863,.T.);
#10939=FACE_OUTER_BOUND('',#16864,.T.);
#10940=FACE_OUTER_BOUND('',#16865,.T.);
#10941=FACE_OUTER_BOUND('',#16866,.T.);
#10942=FACE_OUTER_BOUND('',#16867,.T.);
#10943=FACE_OUTER_BOUND('',#16868,.T.);
#10944=FACE_OUTER_BOUND('',#16869,.T.);
#10945=FACE_OUTER_BOUND('',#16870,.T.);
#10946=FACE_OUTER_BOUND('',#16871,.T.);
#10947=FACE_OUTER_BOUND('',#16872,.T.);
#10948=FACE_OUTER_BOUND('',#16873,.T.);
#10949=FACE_OUTER_BOUND('',#16874,.T.);
#10950=FACE_OUTER_BOUND('',#16875,.T.);
#10951=FACE_OUTER_BOUND('',#16876,.T.);
#10952=FACE_OUTER_BOUND('',#16877,.T.);
#10953=FACE_OUTER_BOUND('',#16878,.T.);
#10954=FACE_OUTER_BOUND('',#16879,.T.);
#10955=FACE_OUTER_BOUND('',#16880,.T.);
#10956=FACE_OUTER_BOUND('',#16881,.T.);
#10957=FACE_OUTER_BOUND('',#16882,.T.);
#10958=FACE_OUTER_BOUND('',#16883,.T.);
#10959=FACE_OUTER_BOUND('',#16884,.T.);
#10960=FACE_OUTER_BOUND('',#16885,.T.);
#10961=FACE_OUTER_BOUND('',#16886,.T.);
#10962=FACE_OUTER_BOUND('',#16887,.T.);
#10963=FACE_OUTER_BOUND('',#16888,.T.);
#10964=FACE_OUTER_BOUND('',#16889,.T.);
#10965=FACE_OUTER_BOUND('',#16890,.T.);
#10966=FACE_OUTER_BOUND('',#16891,.T.);
#10967=FACE_OUTER_BOUND('',#16892,.T.);
#10968=FACE_OUTER_BOUND('',#16893,.T.);
#10969=FACE_OUTER_BOUND('',#16894,.T.);
#10970=FACE_OUTER_BOUND('',#16895,.T.);
#10971=FACE_OUTER_BOUND('',#16896,.T.);
#10972=FACE_OUTER_BOUND('',#16897,.T.);
#10973=FACE_OUTER_BOUND('',#16898,.T.);
#10974=FACE_OUTER_BOUND('',#16899,.T.);
#10975=FACE_OUTER_BOUND('',#16900,.T.);
#10976=FACE_OUTER_BOUND('',#16901,.T.);
#10977=FACE_OUTER_BOUND('',#16902,.T.);
#10978=FACE_OUTER_BOUND('',#16903,.T.);
#10979=FACE_OUTER_BOUND('',#16904,.T.);
#10980=FACE_OUTER_BOUND('',#16905,.T.);
#10981=FACE_OUTER_BOUND('',#16906,.T.);
#10982=FACE_OUTER_BOUND('',#16907,.T.);
#10983=FACE_OUTER_BOUND('',#16908,.T.);
#10984=FACE_OUTER_BOUND('',#16909,.T.);
#10985=FACE_OUTER_BOUND('',#16910,.T.);
#10986=FACE_OUTER_BOUND('',#16911,.T.);
#10987=FACE_OUTER_BOUND('',#16912,.T.);
#10988=FACE_OUTER_BOUND('',#16913,.T.);
#10989=FACE_OUTER_BOUND('',#16914,.T.);
#10990=FACE_OUTER_BOUND('',#16915,.T.);
#10991=FACE_OUTER_BOUND('',#16916,.T.);
#10992=FACE_OUTER_BOUND('',#16917,.T.);
#10993=FACE_OUTER_BOUND('',#16918,.T.);
#10994=FACE_OUTER_BOUND('',#16919,.T.);
#10995=FACE_OUTER_BOUND('',#16920,.T.);
#10996=FACE_OUTER_BOUND('',#16921,.T.);
#10997=FACE_OUTER_BOUND('',#16922,.T.);
#10998=FACE_OUTER_BOUND('',#16923,.T.);
#10999=FACE_OUTER_BOUND('',#16924,.T.);
#11000=FACE_OUTER_BOUND('',#16925,.T.);
#11001=FACE_OUTER_BOUND('',#16926,.T.);
#11002=FACE_OUTER_BOUND('',#16927,.T.);
#11003=FACE_OUTER_BOUND('',#16928,.T.);
#11004=FACE_OUTER_BOUND('',#16929,.T.);
#11005=FACE_OUTER_BOUND('',#16930,.T.);
#11006=FACE_OUTER_BOUND('',#16931,.T.);
#11007=FACE_OUTER_BOUND('',#16932,.T.);
#11008=FACE_OUTER_BOUND('',#16933,.T.);
#11009=FACE_OUTER_BOUND('',#16934,.T.);
#11010=FACE_OUTER_BOUND('',#16935,.T.);
#11011=FACE_OUTER_BOUND('',#16936,.T.);
#11012=FACE_OUTER_BOUND('',#16937,.T.);
#11013=FACE_OUTER_BOUND('',#16938,.T.);
#11014=FACE_OUTER_BOUND('',#16939,.T.);
#11015=FACE_OUTER_BOUND('',#16940,.T.);
#11016=FACE_OUTER_BOUND('',#16941,.T.);
#11017=FACE_OUTER_BOUND('',#16942,.T.);
#11018=FACE_OUTER_BOUND('',#16943,.T.);
#11019=FACE_OUTER_BOUND('',#16944,.T.);
#11020=FACE_OUTER_BOUND('',#16945,.T.);
#11021=FACE_OUTER_BOUND('',#16946,.T.);
#11022=FACE_OUTER_BOUND('',#16947,.T.);
#11023=FACE_OUTER_BOUND('',#16948,.T.);
#11024=FACE_OUTER_BOUND('',#16949,.T.);
#11025=FACE_OUTER_BOUND('',#16950,.T.);
#11026=FACE_OUTER_BOUND('',#16951,.T.);
#11027=FACE_OUTER_BOUND('',#16952,.T.);
#11028=FACE_OUTER_BOUND('',#16953,.T.);
#11029=FACE_OUTER_BOUND('',#16954,.T.);
#11030=FACE_OUTER_BOUND('',#16955,.T.);
#11031=FACE_OUTER_BOUND('',#16956,.T.);
#11032=FACE_OUTER_BOUND('',#16957,.T.);
#11033=FACE_OUTER_BOUND('',#16958,.T.);
#11034=FACE_OUTER_BOUND('',#16959,.T.);
#11035=FACE_OUTER_BOUND('',#16960,.T.);
#11036=FACE_OUTER_BOUND('',#16961,.T.);
#11037=FACE_OUTER_BOUND('',#16962,.T.);
#11038=FACE_OUTER_BOUND('',#16963,.T.);
#11039=FACE_OUTER_BOUND('',#16964,.T.);
#11040=FACE_OUTER_BOUND('',#16965,.T.);
#11041=FACE_OUTER_BOUND('',#16966,.T.);
#11042=FACE_OUTER_BOUND('',#16967,.T.);
#11043=FACE_OUTER_BOUND('',#16968,.T.);
#11044=FACE_OUTER_BOUND('',#16969,.T.);
#11045=FACE_OUTER_BOUND('',#16970,.T.);
#11046=FACE_OUTER_BOUND('',#16971,.T.);
#11047=FACE_OUTER_BOUND('',#16972,.T.);
#11048=FACE_OUTER_BOUND('',#16973,.T.);
#11049=FACE_OUTER_BOUND('',#16974,.T.);
#11050=FACE_OUTER_BOUND('',#16975,.T.);
#11051=FACE_OUTER_BOUND('',#16976,.T.);
#11052=FACE_OUTER_BOUND('',#16977,.T.);
#11053=FACE_OUTER_BOUND('',#16978,.T.);
#11054=FACE_OUTER_BOUND('',#16979,.T.);
#11055=FACE_OUTER_BOUND('',#16980,.T.);
#11056=FACE_OUTER_BOUND('',#16981,.T.);
#11057=FACE_OUTER_BOUND('',#16982,.T.);
#11058=FACE_OUTER_BOUND('',#16983,.T.);
#11059=FACE_OUTER_BOUND('',#16984,.T.);
#11060=FACE_OUTER_BOUND('',#16985,.T.);
#11061=FACE_OUTER_BOUND('',#16986,.T.);
#11062=FACE_OUTER_BOUND('',#16987,.T.);
#11063=FACE_OUTER_BOUND('',#16988,.T.);
#11064=FACE_OUTER_BOUND('',#16989,.T.);
#11065=FACE_OUTER_BOUND('',#16990,.T.);
#11066=FACE_OUTER_BOUND('',#16991,.T.);
#11067=FACE_OUTER_BOUND('',#16992,.T.);
#11068=FACE_OUTER_BOUND('',#16993,.T.);
#11069=FACE_OUTER_BOUND('',#16994,.T.);
#11070=FACE_OUTER_BOUND('',#16995,.T.);
#11071=FACE_OUTER_BOUND('',#16996,.T.);
#11072=FACE_OUTER_BOUND('',#16997,.T.);
#11073=FACE_OUTER_BOUND('',#16998,.T.);
#11074=FACE_OUTER_BOUND('',#16999,.T.);
#11075=FACE_OUTER_BOUND('',#17000,.T.);
#11076=FACE_OUTER_BOUND('',#17001,.T.);
#11077=FACE_OUTER_BOUND('',#17002,.T.);
#11078=FACE_OUTER_BOUND('',#17003,.T.);
#11079=FACE_OUTER_BOUND('',#17004,.T.);
#11080=FACE_OUTER_BOUND('',#17005,.T.);
#11081=FACE_OUTER_BOUND('',#17006,.T.);
#11082=FACE_OUTER_BOUND('',#17007,.T.);
#11083=FACE_OUTER_BOUND('',#17008,.T.);
#11084=FACE_OUTER_BOUND('',#17009,.T.);
#11085=FACE_OUTER_BOUND('',#17010,.T.);
#11086=FACE_OUTER_BOUND('',#17011,.T.);
#11087=FACE_OUTER_BOUND('',#17012,.T.);
#11088=FACE_OUTER_BOUND('',#17013,.T.);
#11089=FACE_OUTER_BOUND('',#17014,.T.);
#11090=FACE_OUTER_BOUND('',#17015,.T.);
#11091=FACE_OUTER_BOUND('',#17016,.T.);
#11092=FACE_OUTER_BOUND('',#17017,.T.);
#11093=FACE_OUTER_BOUND('',#17018,.T.);
#11094=FACE_OUTER_BOUND('',#17019,.T.);
#11095=FACE_OUTER_BOUND('',#17020,.T.);
#11096=FACE_OUTER_BOUND('',#17021,.T.);
#11097=FACE_OUTER_BOUND('',#17022,.T.);
#11098=FACE_OUTER_BOUND('',#17023,.T.);
#11099=FACE_OUTER_BOUND('',#17024,.T.);
#11100=FACE_OUTER_BOUND('',#17025,.T.);
#11101=FACE_OUTER_BOUND('',#17026,.T.);
#11102=FACE_OUTER_BOUND('',#17027,.T.);
#11103=FACE_OUTER_BOUND('',#17028,.T.);
#11104=FACE_OUTER_BOUND('',#17029,.T.);
#11105=FACE_OUTER_BOUND('',#17030,.T.);
#11106=FACE_OUTER_BOUND('',#17031,.T.);
#11107=FACE_OUTER_BOUND('',#17032,.T.);
#11108=FACE_OUTER_BOUND('',#17033,.T.);
#11109=FACE_OUTER_BOUND('',#17034,.T.);
#11110=FACE_OUTER_BOUND('',#17035,.T.);
#11111=FACE_OUTER_BOUND('',#17036,.T.);
#11112=FACE_OUTER_BOUND('',#17037,.T.);
#11113=FACE_OUTER_BOUND('',#17038,.T.);
#11114=FACE_OUTER_BOUND('',#17039,.T.);
#11115=FACE_OUTER_BOUND('',#17040,.T.);
#11116=FACE_OUTER_BOUND('',#17041,.T.);
#11117=FACE_OUTER_BOUND('',#17042,.T.);
#11118=FACE_OUTER_BOUND('',#17043,.T.);
#11119=FACE_OUTER_BOUND('',#17044,.T.);
#11120=FACE_OUTER_BOUND('',#17045,.T.);
#11121=FACE_OUTER_BOUND('',#17046,.T.);
#11122=FACE_OUTER_BOUND('',#17047,.T.);
#11123=FACE_OUTER_BOUND('',#17048,.T.);
#11124=FACE_OUTER_BOUND('',#17049,.T.);
#11125=FACE_OUTER_BOUND('',#17050,.T.);
#11126=FACE_OUTER_BOUND('',#17051,.T.);
#11127=FACE_OUTER_BOUND('',#17052,.T.);
#11128=FACE_OUTER_BOUND('',#17053,.T.);
#11129=FACE_OUTER_BOUND('',#17054,.T.);
#11130=FACE_OUTER_BOUND('',#17055,.T.);
#11131=FACE_OUTER_BOUND('',#17056,.T.);
#11132=FACE_OUTER_BOUND('',#17057,.T.);
#11133=FACE_OUTER_BOUND('',#17058,.T.);
#11134=FACE_OUTER_BOUND('',#17059,.T.);
#11135=FACE_OUTER_BOUND('',#17060,.T.);
#11136=FACE_OUTER_BOUND('',#17061,.T.);
#11137=FACE_OUTER_BOUND('',#17062,.T.);
#11138=FACE_OUTER_BOUND('',#17063,.T.);
#11139=FACE_OUTER_BOUND('',#17064,.T.);
#11140=FACE_OUTER_BOUND('',#17065,.T.);
#11141=FACE_OUTER_BOUND('',#17066,.T.);
#11142=FACE_OUTER_BOUND('',#17067,.T.);
#11143=FACE_OUTER_BOUND('',#17068,.T.);
#11144=FACE_OUTER_BOUND('',#17069,.T.);
#11145=FACE_OUTER_BOUND('',#17070,.T.);
#11146=FACE_OUTER_BOUND('',#17071,.T.);
#11147=FACE_OUTER_BOUND('',#17072,.T.);
#11148=FACE_OUTER_BOUND('',#17073,.T.);
#11149=FACE_OUTER_BOUND('',#17074,.T.);
#11150=FACE_OUTER_BOUND('',#17075,.T.);
#11151=FACE_OUTER_BOUND('',#17076,.T.);
#11152=FACE_OUTER_BOUND('',#17077,.T.);
#11153=FACE_OUTER_BOUND('',#17078,.T.);
#11154=FACE_OUTER_BOUND('',#17079,.T.);
#11155=FACE_OUTER_BOUND('',#17080,.T.);
#11156=FACE_OUTER_BOUND('',#17081,.T.);
#11157=FACE_OUTER_BOUND('',#17082,.T.);
#11158=FACE_OUTER_BOUND('',#17083,.T.);
#11159=FACE_OUTER_BOUND('',#17084,.T.);
#11160=FACE_OUTER_BOUND('',#17085,.T.);
#11161=FACE_OUTER_BOUND('',#17086,.T.);
#11162=FACE_OUTER_BOUND('',#17087,.T.);
#11163=FACE_OUTER_BOUND('',#17088,.T.);
#11164=FACE_OUTER_BOUND('',#17089,.T.);
#11165=FACE_OUTER_BOUND('',#17090,.T.);
#11166=FACE_OUTER_BOUND('',#17091,.T.);
#11167=FACE_OUTER_BOUND('',#17092,.T.);
#11168=FACE_OUTER_BOUND('',#17093,.T.);
#11169=FACE_OUTER_BOUND('',#17094,.T.);
#11170=FACE_OUTER_BOUND('',#17095,.T.);
#11171=FACE_OUTER_BOUND('',#17096,.T.);
#11172=FACE_OUTER_BOUND('',#17097,.T.);
#11173=FACE_OUTER_BOUND('',#17098,.T.);
#11174=FACE_OUTER_BOUND('',#17099,.T.);
#11175=FACE_OUTER_BOUND('',#17100,.T.);
#11176=FACE_OUTER_BOUND('',#17101,.T.);
#11177=FACE_OUTER_BOUND('',#17102,.T.);
#11178=FACE_OUTER_BOUND('',#17103,.T.);
#11179=FACE_OUTER_BOUND('',#17104,.T.);
#11180=FACE_OUTER_BOUND('',#17105,.T.);
#11181=FACE_OUTER_BOUND('',#17106,.T.);
#11182=FACE_OUTER_BOUND('',#17107,.T.);
#11183=FACE_OUTER_BOUND('',#17108,.T.);
#11184=FACE_OUTER_BOUND('',#17109,.T.);
#11185=FACE_OUTER_BOUND('',#17110,.T.);
#11186=FACE_OUTER_BOUND('',#17111,.T.);
#11187=FACE_OUTER_BOUND('',#17112,.T.);
#11188=FACE_OUTER_BOUND('',#17113,.T.);
#11189=FACE_OUTER_BOUND('',#17114,.T.);
#11190=FACE_OUTER_BOUND('',#17115,.T.);
#11191=FACE_OUTER_BOUND('',#17116,.T.);
#11192=FACE_OUTER_BOUND('',#17117,.T.);
#11193=FACE_OUTER_BOUND('',#17118,.T.);
#11194=FACE_OUTER_BOUND('',#17119,.T.);
#11195=FACE_OUTER_BOUND('',#17120,.T.);
#11196=FACE_OUTER_BOUND('',#17121,.T.);
#11197=FACE_OUTER_BOUND('',#17122,.T.);
#11198=FACE_OUTER_BOUND('',#17123,.T.);
#11199=FACE_OUTER_BOUND('',#17124,.T.);
#11200=FACE_OUTER_BOUND('',#17125,.T.);
#11201=FACE_OUTER_BOUND('',#17126,.T.);
#11202=FACE_OUTER_BOUND('',#17127,.T.);
#11203=FACE_OUTER_BOUND('',#17128,.T.);
#11204=FACE_OUTER_BOUND('',#17129,.T.);
#11205=FACE_OUTER_BOUND('',#17130,.T.);
#11206=FACE_OUTER_BOUND('',#17131,.T.);
#11207=FACE_OUTER_BOUND('',#17132,.T.);
#11208=FACE_OUTER_BOUND('',#17133,.T.);
#11209=FACE_OUTER_BOUND('',#17134,.T.);
#11210=FACE_OUTER_BOUND('',#17135,.T.);
#11211=FACE_OUTER_BOUND('',#17136,.T.);
#11212=FACE_OUTER_BOUND('',#17137,.T.);
#11213=FACE_OUTER_BOUND('',#17138,.T.);
#11214=FACE_OUTER_BOUND('',#17139,.T.);
#11215=FACE_OUTER_BOUND('',#17140,.T.);
#11216=FACE_OUTER_BOUND('',#17141,.T.);
#11217=FACE_OUTER_BOUND('',#17142,.T.);
#11218=FACE_OUTER_BOUND('',#17143,.T.);
#11219=FACE_OUTER_BOUND('',#17144,.T.);
#11220=FACE_OUTER_BOUND('',#17145,.T.);
#11221=FACE_OUTER_BOUND('',#17146,.T.);
#11222=FACE_OUTER_BOUND('',#17147,.T.);
#11223=FACE_OUTER_BOUND('',#17148,.T.);
#11224=FACE_OUTER_BOUND('',#17149,.T.);
#11225=FACE_OUTER_BOUND('',#17150,.T.);
#11226=FACE_OUTER_BOUND('',#17151,.T.);
#11227=FACE_OUTER_BOUND('',#17152,.T.);
#11228=FACE_OUTER_BOUND('',#17153,.T.);
#11229=FACE_OUTER_BOUND('',#17154,.T.);
#11230=FACE_OUTER_BOUND('',#17155,.T.);
#11231=FACE_OUTER_BOUND('',#17156,.T.);
#11232=FACE_OUTER_BOUND('',#17157,.T.);
#11233=FACE_OUTER_BOUND('',#17158,.T.);
#11234=FACE_OUTER_BOUND('',#17159,.T.);
#11235=FACE_OUTER_BOUND('',#17160,.T.);
#11236=FACE_OUTER_BOUND('',#17161,.T.);
#11237=FACE_OUTER_BOUND('',#17162,.T.);
#11238=FACE_OUTER_BOUND('',#17163,.T.);
#11239=FACE_OUTER_BOUND('',#17164,.T.);
#11240=FACE_OUTER_BOUND('',#17165,.T.);
#11241=FACE_OUTER_BOUND('',#17166,.T.);
#11242=FACE_OUTER_BOUND('',#17167,.T.);
#11243=FACE_OUTER_BOUND('',#17168,.T.);
#11244=FACE_OUTER_BOUND('',#17169,.T.);
#11245=FACE_OUTER_BOUND('',#17170,.T.);
#11246=FACE_OUTER_BOUND('',#17171,.T.);
#11247=FACE_OUTER_BOUND('',#17172,.T.);
#11248=FACE_OUTER_BOUND('',#17173,.T.);
#11249=FACE_OUTER_BOUND('',#17174,.T.);
#11250=FACE_OUTER_BOUND('',#17175,.T.);
#11251=FACE_OUTER_BOUND('',#17176,.T.);
#11252=FACE_OUTER_BOUND('',#17177,.T.);
#11253=FACE_OUTER_BOUND('',#17178,.T.);
#11254=FACE_OUTER_BOUND('',#17179,.T.);
#11255=FACE_OUTER_BOUND('',#17180,.T.);
#11256=FACE_OUTER_BOUND('',#17181,.T.);
#11257=FACE_OUTER_BOUND('',#17182,.T.);
#11258=FACE_OUTER_BOUND('',#17183,.T.);
#11259=FACE_OUTER_BOUND('',#17184,.T.);
#11260=FACE_OUTER_BOUND('',#17185,.T.);
#11261=FACE_OUTER_BOUND('',#17186,.T.);
#11262=FACE_OUTER_BOUND('',#17187,.T.);
#11263=FACE_OUTER_BOUND('',#17188,.T.);
#11264=FACE_OUTER_BOUND('',#17189,.T.);
#11265=FACE_OUTER_BOUND('',#17190,.T.);
#11266=FACE_OUTER_BOUND('',#17191,.T.);
#11267=FACE_OUTER_BOUND('',#17192,.T.);
#11268=FACE_OUTER_BOUND('',#17193,.T.);
#11269=FACE_OUTER_BOUND('',#17194,.T.);
#11270=FACE_OUTER_BOUND('',#17195,.T.);
#11271=FACE_OUTER_BOUND('',#17196,.T.);
#11272=FACE_OUTER_BOUND('',#17197,.T.);
#11273=FACE_OUTER_BOUND('',#17198,.T.);
#11274=FACE_OUTER_BOUND('',#17199,.T.);
#11275=FACE_OUTER_BOUND('',#17200,.T.);
#11276=FACE_OUTER_BOUND('',#17201,.T.);
#11277=FACE_OUTER_BOUND('',#17202,.T.);
#11278=FACE_OUTER_BOUND('',#17203,.T.);
#11279=FACE_OUTER_BOUND('',#17204,.T.);
#11280=FACE_OUTER_BOUND('',#17205,.T.);
#11281=FACE_OUTER_BOUND('',#17206,.T.);
#11282=FACE_OUTER_BOUND('',#17207,.T.);
#11283=FACE_OUTER_BOUND('',#17208,.T.);
#11284=FACE_OUTER_BOUND('',#17209,.T.);
#11285=FACE_OUTER_BOUND('',#17210,.T.);
#11286=FACE_OUTER_BOUND('',#17211,.T.);
#11287=FACE_OUTER_BOUND('',#17212,.T.);
#11288=FACE_OUTER_BOUND('',#17213,.T.);
#11289=FACE_OUTER_BOUND('',#17214,.T.);
#11290=FACE_OUTER_BOUND('',#17215,.T.);
#11291=FACE_OUTER_BOUND('',#17216,.T.);
#11292=FACE_OUTER_BOUND('',#17217,.T.);
#11293=FACE_OUTER_BOUND('',#17218,.T.);
#11294=FACE_OUTER_BOUND('',#17219,.T.);
#11295=FACE_OUTER_BOUND('',#17220,.T.);
#11296=FACE_OUTER_BOUND('',#17221,.T.);
#11297=FACE_OUTER_BOUND('',#17222,.T.);
#11298=FACE_OUTER_BOUND('',#17223,.T.);
#11299=FACE_OUTER_BOUND('',#17224,.T.);
#11300=FACE_OUTER_BOUND('',#17225,.T.);
#11301=FACE_OUTER_BOUND('',#17226,.T.);
#11302=FACE_OUTER_BOUND('',#17227,.T.);
#11303=FACE_OUTER_BOUND('',#17228,.T.);
#11304=FACE_OUTER_BOUND('',#17229,.T.);
#11305=FACE_OUTER_BOUND('',#17230,.T.);
#11306=FACE_OUTER_BOUND('',#17231,.T.);
#11307=FACE_OUTER_BOUND('',#17232,.T.);
#11308=FACE_OUTER_BOUND('',#17233,.T.);
#11309=FACE_OUTER_BOUND('',#17234,.T.);
#11310=FACE_OUTER_BOUND('',#17235,.T.);
#11311=FACE_OUTER_BOUND('',#17236,.T.);
#11312=FACE_OUTER_BOUND('',#17237,.T.);
#11313=FACE_OUTER_BOUND('',#17238,.T.);
#11314=FACE_OUTER_BOUND('',#17239,.T.);
#11315=FACE_OUTER_BOUND('',#17240,.T.);
#11316=FACE_OUTER_BOUND('',#17241,.T.);
#11317=FACE_OUTER_BOUND('',#17242,.T.);
#11318=FACE_OUTER_BOUND('',#17243,.T.);
#11319=FACE_OUTER_BOUND('',#17244,.T.);
#11320=FACE_OUTER_BOUND('',#17245,.T.);
#11321=FACE_OUTER_BOUND('',#17246,.T.);
#11322=FACE_OUTER_BOUND('',#17247,.T.);
#11323=FACE_OUTER_BOUND('',#17248,.T.);
#11324=FACE_OUTER_BOUND('',#17249,.T.);
#11325=FACE_OUTER_BOUND('',#17250,.T.);
#11326=FACE_OUTER_BOUND('',#17251,.T.);
#11327=FACE_OUTER_BOUND('',#17252,.T.);
#11328=FACE_OUTER_BOUND('',#17253,.T.);
#11329=FACE_OUTER_BOUND('',#17254,.T.);
#11330=FACE_OUTER_BOUND('',#17255,.T.);
#11331=FACE_OUTER_BOUND('',#17256,.T.);
#11332=FACE_OUTER_BOUND('',#17257,.T.);
#11333=FACE_OUTER_BOUND('',#17258,.T.);
#11334=FACE_OUTER_BOUND('',#17259,.T.);
#11335=FACE_OUTER_BOUND('',#17260,.T.);
#11336=FACE_OUTER_BOUND('',#17261,.T.);
#11337=FACE_OUTER_BOUND('',#17262,.T.);
#11338=FACE_OUTER_BOUND('',#17263,.T.);
#11339=FACE_OUTER_BOUND('',#17264,.T.);
#11340=FACE_OUTER_BOUND('',#17265,.T.);
#11341=FACE_OUTER_BOUND('',#17266,.T.);
#11342=FACE_OUTER_BOUND('',#17267,.T.);
#11343=FACE_OUTER_BOUND('',#17268,.T.);
#11344=FACE_OUTER_BOUND('',#17269,.T.);
#11345=FACE_OUTER_BOUND('',#17270,.T.);
#11346=FACE_OUTER_BOUND('',#17271,.T.);
#11347=FACE_OUTER_BOUND('',#17272,.T.);
#11348=FACE_OUTER_BOUND('',#17273,.T.);
#11349=FACE_OUTER_BOUND('',#17274,.T.);
#11350=FACE_OUTER_BOUND('',#17275,.T.);
#11351=FACE_OUTER_BOUND('',#17276,.T.);
#11352=FACE_OUTER_BOUND('',#17277,.T.);
#11353=FACE_OUTER_BOUND('',#17278,.T.);
#11354=FACE_OUTER_BOUND('',#17279,.T.);
#11355=FACE_OUTER_BOUND('',#17280,.T.);
#11356=FACE_OUTER_BOUND('',#17281,.T.);
#11357=FACE_OUTER_BOUND('',#17282,.T.);
#11358=FACE_OUTER_BOUND('',#17283,.T.);
#11359=FACE_OUTER_BOUND('',#17284,.T.);
#11360=FACE_OUTER_BOUND('',#17285,.T.);
#11361=FACE_OUTER_BOUND('',#17286,.T.);
#11362=FACE_OUTER_BOUND('',#17287,.T.);
#11363=FACE_OUTER_BOUND('',#17288,.T.);
#11364=FACE_OUTER_BOUND('',#17289,.T.);
#11365=FACE_OUTER_BOUND('',#17290,.T.);
#11366=FACE_OUTER_BOUND('',#17291,.T.);
#11367=FACE_OUTER_BOUND('',#17292,.T.);
#11368=FACE_OUTER_BOUND('',#17293,.T.);
#11369=FACE_OUTER_BOUND('',#17294,.T.);
#11370=FACE_OUTER_BOUND('',#17295,.T.);
#11371=FACE_OUTER_BOUND('',#17296,.T.);
#11372=FACE_OUTER_BOUND('',#17297,.T.);
#11373=FACE_OUTER_BOUND('',#17298,.T.);
#11374=FACE_OUTER_BOUND('',#17299,.T.);
#11375=FACE_OUTER_BOUND('',#17300,.T.);
#11376=FACE_OUTER_BOUND('',#17301,.T.);
#11377=FACE_OUTER_BOUND('',#17302,.T.);
#11378=FACE_OUTER_BOUND('',#17303,.T.);
#11379=FACE_OUTER_BOUND('',#17304,.T.);
#11380=FACE_OUTER_BOUND('',#17305,.T.);
#11381=FACE_OUTER_BOUND('',#17306,.T.);
#11382=FACE_OUTER_BOUND('',#17307,.T.);
#11383=FACE_OUTER_BOUND('',#17308,.T.);
#11384=FACE_OUTER_BOUND('',#17309,.T.);
#11385=FACE_OUTER_BOUND('',#17310,.T.);
#11386=FACE_OUTER_BOUND('',#17311,.T.);
#11387=FACE_OUTER_BOUND('',#17312,.T.);
#11388=FACE_OUTER_BOUND('',#17313,.T.);
#11389=FACE_OUTER_BOUND('',#17314,.T.);
#11390=FACE_OUTER_BOUND('',#17315,.T.);
#11391=FACE_OUTER_BOUND('',#17316,.T.);
#11392=FACE_OUTER_BOUND('',#17317,.T.);
#11393=FACE_OUTER_BOUND('',#17318,.T.);
#11394=FACE_OUTER_BOUND('',#17319,.T.);
#11395=FACE_OUTER_BOUND('',#17320,.T.);
#11396=FACE_OUTER_BOUND('',#17321,.T.);
#11397=FACE_OUTER_BOUND('',#17322,.T.);
#11398=FACE_OUTER_BOUND('',#17323,.T.);
#11399=FACE_OUTER_BOUND('',#17324,.T.);
#11400=FACE_OUTER_BOUND('',#17325,.T.);
#11401=FACE_OUTER_BOUND('',#17326,.T.);
#11402=FACE_OUTER_BOUND('',#17327,.T.);
#11403=FACE_OUTER_BOUND('',#17328,.T.);
#11404=FACE_OUTER_BOUND('',#17329,.T.);
#11405=FACE_OUTER_BOUND('',#17330,.T.);
#11406=FACE_OUTER_BOUND('',#17331,.T.);
#11407=FACE_OUTER_BOUND('',#17332,.T.);
#11408=FACE_OUTER_BOUND('',#17333,.T.);
#11409=FACE_OUTER_BOUND('',#17334,.T.);
#11410=FACE_OUTER_BOUND('',#17335,.T.);
#11411=FACE_OUTER_BOUND('',#17336,.T.);
#11412=FACE_OUTER_BOUND('',#17337,.T.);
#11413=FACE_OUTER_BOUND('',#17338,.T.);
#11414=FACE_OUTER_BOUND('',#17339,.T.);
#11415=FACE_OUTER_BOUND('',#17340,.T.);
#11416=FACE_OUTER_BOUND('',#17341,.T.);
#11417=FACE_OUTER_BOUND('',#17342,.T.);
#11418=FACE_OUTER_BOUND('',#17343,.T.);
#11419=FACE_OUTER_BOUND('',#17344,.T.);
#11420=FACE_OUTER_BOUND('',#17345,.T.);
#11421=FACE_OUTER_BOUND('',#17346,.T.);
#11422=FACE_OUTER_BOUND('',#17347,.T.);
#11423=FACE_OUTER_BOUND('',#17348,.T.);
#11424=FACE_OUTER_BOUND('',#17349,.T.);
#11425=FACE_OUTER_BOUND('',#17350,.T.);
#11426=FACE_OUTER_BOUND('',#17351,.T.);
#11427=FACE_OUTER_BOUND('',#17352,.T.);
#11428=FACE_OUTER_BOUND('',#17353,.T.);
#11429=FACE_OUTER_BOUND('',#17354,.T.);
#11430=FACE_OUTER_BOUND('',#17355,.T.);
#11431=FACE_OUTER_BOUND('',#17356,.T.);
#11432=FACE_OUTER_BOUND('',#17357,.T.);
#11433=FACE_OUTER_BOUND('',#17358,.T.);
#11434=FACE_OUTER_BOUND('',#17359,.T.);
#11435=FACE_OUTER_BOUND('',#17360,.T.);
#11436=FACE_OUTER_BOUND('',#17361,.T.);
#11437=FACE_OUTER_BOUND('',#17362,.T.);
#11438=FACE_OUTER_BOUND('',#17363,.T.);
#11439=FACE_OUTER_BOUND('',#17364,.T.);
#11440=FACE_OUTER_BOUND('',#17365,.T.);
#11441=FACE_OUTER_BOUND('',#17366,.T.);
#11442=FACE_OUTER_BOUND('',#17367,.T.);
#11443=FACE_OUTER_BOUND('',#17368,.T.);
#11444=FACE_OUTER_BOUND('',#17369,.T.);
#11445=FACE_OUTER_BOUND('',#17370,.T.);
#11446=FACE_OUTER_BOUND('',#17371,.T.);
#11447=FACE_OUTER_BOUND('',#17372,.T.);
#11448=FACE_OUTER_BOUND('',#17373,.T.);
#11449=FACE_OUTER_BOUND('',#17374,.T.);
#11450=FACE_OUTER_BOUND('',#17375,.T.);
#11451=FACE_OUTER_BOUND('',#17376,.T.);
#11452=FACE_OUTER_BOUND('',#17377,.T.);
#11453=FACE_OUTER_BOUND('',#17378,.T.);
#11454=FACE_OUTER_BOUND('',#17379,.T.);
#11455=FACE_OUTER_BOUND('',#17380,.T.);
#11456=FACE_OUTER_BOUND('',#17381,.T.);
#11457=FACE_OUTER_BOUND('',#17382,.T.);
#11458=FACE_OUTER_BOUND('',#17383,.T.);
#11459=FACE_OUTER_BOUND('',#17384,.T.);
#11460=FACE_OUTER_BOUND('',#17385,.T.);
#11461=FACE_OUTER_BOUND('',#17386,.T.);
#11462=FACE_OUTER_BOUND('',#17387,.T.);
#11463=FACE_OUTER_BOUND('',#17388,.T.);
#11464=FACE_OUTER_BOUND('',#17389,.T.);
#11465=FACE_OUTER_BOUND('',#17390,.T.);
#11466=FACE_OUTER_BOUND('',#17391,.T.);
#11467=FACE_OUTER_BOUND('',#17392,.T.);
#11468=FACE_OUTER_BOUND('',#17393,.T.);
#11469=FACE_OUTER_BOUND('',#17394,.T.);
#11470=FACE_OUTER_BOUND('',#17395,.T.);
#11471=FACE_OUTER_BOUND('',#17396,.T.);
#11472=FACE_OUTER_BOUND('',#17397,.T.);
#11473=FACE_OUTER_BOUND('',#17398,.T.);
#11474=FACE_OUTER_BOUND('',#17399,.T.);
#11475=FACE_OUTER_BOUND('',#17400,.T.);
#11476=FACE_OUTER_BOUND('',#17401,.T.);
#11477=FACE_OUTER_BOUND('',#17402,.T.);
#11478=FACE_OUTER_BOUND('',#17403,.T.);
#11479=FACE_OUTER_BOUND('',#17404,.T.);
#11480=FACE_OUTER_BOUND('',#17405,.T.);
#11481=FACE_OUTER_BOUND('',#17406,.T.);
#11482=FACE_OUTER_BOUND('',#17407,.T.);
#11483=FACE_OUTER_BOUND('',#17408,.T.);
#11484=FACE_OUTER_BOUND('',#17409,.T.);
#11485=FACE_OUTER_BOUND('',#17410,.T.);
#11486=FACE_OUTER_BOUND('',#17411,.T.);
#11487=FACE_OUTER_BOUND('',#17412,.T.);
#11488=FACE_OUTER_BOUND('',#17413,.T.);
#11489=FACE_OUTER_BOUND('',#17414,.T.);
#11490=FACE_OUTER_BOUND('',#17415,.T.);
#11491=FACE_OUTER_BOUND('',#17416,.T.);
#11492=FACE_OUTER_BOUND('',#17417,.T.);
#11493=FACE_OUTER_BOUND('',#17418,.T.);
#11494=FACE_OUTER_BOUND('',#17419,.T.);
#11495=FACE_OUTER_BOUND('',#17420,.T.);
#11496=FACE_OUTER_BOUND('',#17421,.T.);
#11497=FACE_OUTER_BOUND('',#17422,.T.);
#11498=FACE_OUTER_BOUND('',#17423,.T.);
#11499=FACE_OUTER_BOUND('',#17424,.T.);
#11500=FACE_OUTER_BOUND('',#17425,.T.);
#11501=FACE_OUTER_BOUND('',#17426,.T.);
#11502=FACE_OUTER_BOUND('',#17427,.T.);
#11503=FACE_OUTER_BOUND('',#17428,.T.);
#11504=FACE_OUTER_BOUND('',#17429,.T.);
#11505=FACE_OUTER_BOUND('',#17430,.T.);
#11506=FACE_OUTER_BOUND('',#17431,.T.);
#11507=FACE_OUTER_BOUND('',#17432,.T.);
#11508=FACE_OUTER_BOUND('',#17433,.T.);
#11509=FACE_OUTER_BOUND('',#17434,.T.);
#11510=FACE_OUTER_BOUND('',#17435,.T.);
#11511=FACE_OUTER_BOUND('',#17436,.T.);
#11512=FACE_OUTER_BOUND('',#17437,.T.);
#11513=FACE_OUTER_BOUND('',#17438,.T.);
#11514=FACE_OUTER_BOUND('',#17439,.T.);
#11515=FACE_OUTER_BOUND('',#17440,.T.);
#11516=FACE_OUTER_BOUND('',#17441,.T.);
#11517=FACE_OUTER_BOUND('',#17442,.T.);
#11518=FACE_OUTER_BOUND('',#17443,.T.);
#11519=FACE_OUTER_BOUND('',#17444,.T.);
#11520=FACE_OUTER_BOUND('',#17445,.T.);
#11521=FACE_OUTER_BOUND('',#17446,.T.);
#11522=FACE_OUTER_BOUND('',#17447,.T.);
#11523=FACE_OUTER_BOUND('',#17448,.T.);
#11524=FACE_OUTER_BOUND('',#17449,.T.);
#11525=FACE_OUTER_BOUND('',#17450,.T.);
#11526=FACE_OUTER_BOUND('',#17451,.T.);
#11527=FACE_OUTER_BOUND('',#17452,.T.);
#11528=FACE_OUTER_BOUND('',#17453,.T.);
#11529=FACE_OUTER_BOUND('',#17454,.T.);
#11530=FACE_OUTER_BOUND('',#17455,.T.);
#11531=FACE_OUTER_BOUND('',#17456,.T.);
#11532=FACE_OUTER_BOUND('',#17457,.T.);
#11533=FACE_OUTER_BOUND('',#17458,.T.);
#11534=FACE_OUTER_BOUND('',#17459,.T.);
#11535=FACE_OUTER_BOUND('',#17460,.T.);
#11536=FACE_OUTER_BOUND('',#17461,.T.);
#11537=FACE_OUTER_BOUND('',#17462,.T.);
#11538=FACE_OUTER_BOUND('',#17463,.T.);
#11539=FACE_OUTER_BOUND('',#17464,.T.);
#11540=FACE_OUTER_BOUND('',#17465,.T.);
#11541=FACE_OUTER_BOUND('',#17466,.T.);
#11542=FACE_OUTER_BOUND('',#17467,.T.);
#11543=FACE_OUTER_BOUND('',#17468,.T.);
#11544=FACE_OUTER_BOUND('',#17469,.T.);
#11545=FACE_OUTER_BOUND('',#17470,.T.);
#11546=FACE_OUTER_BOUND('',#17471,.T.);
#11547=FACE_OUTER_BOUND('',#17472,.T.);
#11548=FACE_OUTER_BOUND('',#17473,.T.);
#11549=FACE_OUTER_BOUND('',#17474,.T.);
#11550=FACE_OUTER_BOUND('',#17475,.T.);
#11551=FACE_OUTER_BOUND('',#17476,.T.);
#11552=FACE_OUTER_BOUND('',#17477,.T.);
#11553=FACE_OUTER_BOUND('',#17478,.T.);
#11554=FACE_OUTER_BOUND('',#17479,.T.);
#11555=FACE_OUTER_BOUND('',#17480,.T.);
#11556=FACE_OUTER_BOUND('',#17481,.T.);
#11557=FACE_OUTER_BOUND('',#17482,.T.);
#11558=FACE_OUTER_BOUND('',#17483,.T.);
#11559=FACE_OUTER_BOUND('',#17484,.T.);
#11560=FACE_OUTER_BOUND('',#17485,.T.);
#11561=FACE_OUTER_BOUND('',#17486,.T.);
#11562=FACE_OUTER_BOUND('',#17487,.T.);
#11563=FACE_OUTER_BOUND('',#17488,.T.);
#11564=FACE_OUTER_BOUND('',#17489,.T.);
#11565=FACE_OUTER_BOUND('',#17490,.T.);
#11566=FACE_OUTER_BOUND('',#17491,.T.);
#11567=FACE_OUTER_BOUND('',#17492,.T.);
#11568=FACE_OUTER_BOUND('',#17493,.T.);
#11569=FACE_OUTER_BOUND('',#17494,.T.);
#11570=FACE_OUTER_BOUND('',#17495,.T.);
#11571=FACE_OUTER_BOUND('',#17496,.T.);
#11572=FACE_OUTER_BOUND('',#17497,.T.);
#11573=FACE_OUTER_BOUND('',#17498,.T.);
#11574=FACE_OUTER_BOUND('',#17499,.T.);
#11575=FACE_OUTER_BOUND('',#17500,.T.);
#11576=FACE_OUTER_BOUND('',#17501,.T.);
#11577=FACE_OUTER_BOUND('',#17502,.T.);
#11578=FACE_OUTER_BOUND('',#17503,.T.);
#11579=FACE_OUTER_BOUND('',#17504,.T.);
#11580=FACE_OUTER_BOUND('',#17505,.T.);
#11581=FACE_OUTER_BOUND('',#17506,.T.);
#11582=FACE_OUTER_BOUND('',#17507,.T.);
#11583=FACE_OUTER_BOUND('',#17508,.T.);
#11584=FACE_OUTER_BOUND('',#17509,.T.);
#11585=FACE_OUTER_BOUND('',#17510,.T.);
#11586=FACE_OUTER_BOUND('',#17511,.T.);
#11587=FACE_OUTER_BOUND('',#17512,.T.);
#11588=FACE_OUTER_BOUND('',#17513,.T.);
#11589=FACE_OUTER_BOUND('',#17514,.T.);
#11590=FACE_OUTER_BOUND('',#17515,.T.);
#11591=FACE_OUTER_BOUND('',#17516,.T.);
#11592=FACE_OUTER_BOUND('',#17517,.T.);
#11593=FACE_OUTER_BOUND('',#17518,.T.);
#11594=FACE_OUTER_BOUND('',#17519,.T.);
#11595=FACE_OUTER_BOUND('',#17520,.T.);
#11596=FACE_OUTER_BOUND('',#17521,.T.);
#11597=FACE_OUTER_BOUND('',#17522,.T.);
#11598=FACE_OUTER_BOUND('',#17523,.T.);
#11599=FACE_OUTER_BOUND('',#17524,.T.);
#11600=FACE_OUTER_BOUND('',#17525,.T.);
#11601=FACE_OUTER_BOUND('',#17526,.T.);
#11602=FACE_OUTER_BOUND('',#17527,.T.);
#11603=FACE_OUTER_BOUND('',#17528,.T.);
#11604=FACE_OUTER_BOUND('',#17529,.T.);
#11605=FACE_OUTER_BOUND('',#17530,.T.);
#11606=FACE_OUTER_BOUND('',#17531,.T.);
#11607=FACE_OUTER_BOUND('',#17532,.T.);
#11608=FACE_OUTER_BOUND('',#17533,.T.);
#11609=FACE_OUTER_BOUND('',#17534,.T.);
#11610=FACE_OUTER_BOUND('',#17535,.T.);
#11611=FACE_OUTER_BOUND('',#17536,.T.);
#11612=FACE_OUTER_BOUND('',#17537,.T.);
#11613=FACE_OUTER_BOUND('',#17538,.T.);
#11614=FACE_OUTER_BOUND('',#17539,.T.);
#11615=FACE_OUTER_BOUND('',#17540,.T.);
#11616=FACE_OUTER_BOUND('',#17541,.T.);
#11617=FACE_OUTER_BOUND('',#17542,.T.);
#11618=FACE_OUTER_BOUND('',#17543,.T.);
#11619=FACE_OUTER_BOUND('',#17544,.T.);
#11620=FACE_OUTER_BOUND('',#17545,.T.);
#11621=FACE_OUTER_BOUND('',#17546,.T.);
#11622=FACE_OUTER_BOUND('',#17547,.T.);
#11623=FACE_OUTER_BOUND('',#17548,.T.);
#11624=FACE_OUTER_BOUND('',#17549,.T.);
#11625=FACE_OUTER_BOUND('',#17550,.T.);
#11626=FACE_OUTER_BOUND('',#17551,.T.);
#11627=FACE_OUTER_BOUND('',#17552,.T.);
#11628=FACE_OUTER_BOUND('',#17553,.T.);
#11629=FACE_OUTER_BOUND('',#17554,.T.);
#11630=FACE_OUTER_BOUND('',#17555,.T.);
#11631=FACE_OUTER_BOUND('',#17556,.T.);
#11632=FACE_OUTER_BOUND('',#17557,.T.);
#11633=FACE_OUTER_BOUND('',#17558,.T.);
#11634=FACE_OUTER_BOUND('',#17559,.T.);
#11635=FACE_OUTER_BOUND('',#17560,.T.);
#11636=FACE_OUTER_BOUND('',#17561,.T.);
#11637=FACE_OUTER_BOUND('',#17562,.T.);
#11638=FACE_OUTER_BOUND('',#17563,.T.);
#11639=FACE_OUTER_BOUND('',#17564,.T.);
#11640=FACE_OUTER_BOUND('',#17565,.T.);
#11641=FACE_OUTER_BOUND('',#17566,.T.);
#11642=FACE_OUTER_BOUND('',#17567,.T.);
#11643=FACE_OUTER_BOUND('',#17568,.T.);
#11644=FACE_OUTER_BOUND('',#17569,.T.);
#11645=FACE_OUTER_BOUND('',#17570,.T.);
#11646=FACE_OUTER_BOUND('',#17571,.T.);
#11647=FACE_OUTER_BOUND('',#17572,.T.);
#11648=FACE_OUTER_BOUND('',#17573,.T.);
#11649=FACE_OUTER_BOUND('',#17574,.T.);
#11650=FACE_OUTER_BOUND('',#17575,.T.);
#11651=FACE_OUTER_BOUND('',#17576,.T.);
#11652=FACE_OUTER_BOUND('',#17577,.T.);
#11653=FACE_OUTER_BOUND('',#17578,.T.);
#11654=FACE_OUTER_BOUND('',#17579,.T.);
#11655=FACE_OUTER_BOUND('',#17580,.T.);
#11656=FACE_OUTER_BOUND('',#17581,.T.);
#11657=FACE_OUTER_BOUND('',#17582,.T.);
#11658=FACE_OUTER_BOUND('',#17583,.T.);
#11659=FACE_OUTER_BOUND('',#17584,.T.);
#11660=FACE_OUTER_BOUND('',#17585,.T.);
#11661=FACE_OUTER_BOUND('',#17586,.T.);
#11662=FACE_OUTER_BOUND('',#17587,.T.);
#11663=FACE_OUTER_BOUND('',#17588,.T.);
#11664=FACE_OUTER_BOUND('',#17589,.T.);
#11665=FACE_OUTER_BOUND('',#17590,.T.);
#11666=FACE_OUTER_BOUND('',#17591,.T.);
#11667=FACE_OUTER_BOUND('',#17592,.T.);
#11668=FACE_OUTER_BOUND('',#17593,.T.);
#11669=FACE_OUTER_BOUND('',#17594,.T.);
#11670=FACE_OUTER_BOUND('',#17595,.T.);
#11671=FACE_OUTER_BOUND('',#17596,.T.);
#11672=FACE_OUTER_BOUND('',#17597,.T.);
#11673=FACE_OUTER_BOUND('',#17598,.T.);
#11674=FACE_OUTER_BOUND('',#17599,.T.);
#11675=FACE_OUTER_BOUND('',#17600,.T.);
#11676=FACE_OUTER_BOUND('',#17601,.T.);
#11677=FACE_OUTER_BOUND('',#17602,.T.);
#11678=FACE_OUTER_BOUND('',#17603,.T.);
#11679=FACE_OUTER_BOUND('',#17604,.T.);
#11680=FACE_OUTER_BOUND('',#17605,.T.);
#11681=FACE_OUTER_BOUND('',#17606,.T.);
#11682=FACE_OUTER_BOUND('',#17607,.T.);
#11683=FACE_OUTER_BOUND('',#17608,.T.);
#11684=FACE_OUTER_BOUND('',#17609,.T.);
#11685=FACE_OUTER_BOUND('',#17610,.T.);
#11686=FACE_OUTER_BOUND('',#17611,.T.);
#11687=FACE_OUTER_BOUND('',#17612,.T.);
#11688=FACE_OUTER_BOUND('',#17613,.T.);
#11689=FACE_OUTER_BOUND('',#17614,.T.);
#11690=FACE_OUTER_BOUND('',#17615,.T.);
#11691=FACE_OUTER_BOUND('',#17616,.T.);
#11692=FACE_OUTER_BOUND('',#17617,.T.);
#11693=FACE_OUTER_BOUND('',#17618,.T.);
#11694=FACE_OUTER_BOUND('',#17619,.T.);
#11695=FACE_OUTER_BOUND('',#17620,.T.);
#11696=FACE_OUTER_BOUND('',#17621,.T.);
#11697=FACE_OUTER_BOUND('',#17622,.T.);
#11698=FACE_OUTER_BOUND('',#17623,.T.);
#11699=FACE_OUTER_BOUND('',#17624,.T.);
#11700=FACE_OUTER_BOUND('',#17625,.T.);
#11701=FACE_OUTER_BOUND('',#17626,.T.);
#11702=FACE_OUTER_BOUND('',#17627,.T.);
#11703=FACE_OUTER_BOUND('',#17628,.T.);
#11704=FACE_OUTER_BOUND('',#17629,.T.);
#11705=FACE_OUTER_BOUND('',#17630,.T.);
#11706=FACE_OUTER_BOUND('',#17631,.T.);
#11707=FACE_OUTER_BOUND('',#17632,.T.);
#11708=FACE_OUTER_BOUND('',#17633,.T.);
#11709=FACE_OUTER_BOUND('',#17634,.T.);
#11710=FACE_OUTER_BOUND('',#17635,.T.);
#11711=FACE_OUTER_BOUND('',#17636,.T.);
#11712=FACE_OUTER_BOUND('',#17637,.T.);
#11713=FACE_OUTER_BOUND('',#17638,.T.);
#11714=FACE_OUTER_BOUND('',#17639,.T.);
#11715=FACE_OUTER_BOUND('',#17640,.T.);
#11716=FACE_OUTER_BOUND('',#17641,.T.);
#11717=FACE_OUTER_BOUND('',#17642,.T.);
#11718=FACE_OUTER_BOUND('',#17643,.T.);
#11719=FACE_OUTER_BOUND('',#17644,.T.);
#11720=FACE_OUTER_BOUND('',#17645,.T.);
#11721=FACE_OUTER_BOUND('',#17646,.T.);
#11722=FACE_OUTER_BOUND('',#17647,.T.);
#11723=FACE_OUTER_BOUND('',#17648,.T.);
#11724=FACE_OUTER_BOUND('',#17649,.T.);
#11725=FACE_OUTER_BOUND('',#17650,.T.);
#11726=FACE_OUTER_BOUND('',#17651,.T.);
#11727=FACE_OUTER_BOUND('',#17652,.T.);
#11728=FACE_OUTER_BOUND('',#17653,.T.);
#11729=FACE_OUTER_BOUND('',#17654,.T.);
#11730=FACE_OUTER_BOUND('',#17655,.T.);
#11731=FACE_OUTER_BOUND('',#17656,.T.);
#11732=FACE_OUTER_BOUND('',#17657,.T.);
#11733=FACE_OUTER_BOUND('',#17658,.T.);
#11734=FACE_OUTER_BOUND('',#17659,.T.);
#11735=FACE_OUTER_BOUND('',#17660,.T.);
#11736=FACE_OUTER_BOUND('',#17661,.T.);
#11737=FACE_OUTER_BOUND('',#17662,.T.);
#11738=FACE_OUTER_BOUND('',#17663,.T.);
#11739=FACE_OUTER_BOUND('',#17664,.T.);
#11740=FACE_OUTER_BOUND('',#17665,.T.);
#11741=FACE_OUTER_BOUND('',#17666,.T.);
#11742=FACE_OUTER_BOUND('',#17667,.T.);
#11743=FACE_OUTER_BOUND('',#17668,.T.);
#11744=FACE_OUTER_BOUND('',#17669,.T.);
#11745=FACE_OUTER_BOUND('',#17670,.T.);
#11746=FACE_OUTER_BOUND('',#17671,.T.);
#11747=FACE_OUTER_BOUND('',#17672,.T.);
#11748=FACE_OUTER_BOUND('',#17673,.T.);
#11749=FACE_OUTER_BOUND('',#17674,.T.);
#11750=FACE_OUTER_BOUND('',#17675,.T.);
#11751=FACE_OUTER_BOUND('',#17676,.T.);
#11752=FACE_OUTER_BOUND('',#17677,.T.);
#11753=FACE_OUTER_BOUND('',#17678,.T.);
#11754=FACE_OUTER_BOUND('',#17679,.T.);
#11755=FACE_OUTER_BOUND('',#17680,.T.);
#11756=FACE_OUTER_BOUND('',#17681,.T.);
#11757=FACE_OUTER_BOUND('',#17682,.T.);
#11758=FACE_OUTER_BOUND('',#17683,.T.);
#11759=FACE_OUTER_BOUND('',#17684,.T.);
#11760=FACE_OUTER_BOUND('',#17685,.T.);
#11761=FACE_OUTER_BOUND('',#17686,.T.);
#11762=FACE_OUTER_BOUND('',#17687,.T.);
#11763=FACE_OUTER_BOUND('',#17688,.T.);
#11764=FACE_OUTER_BOUND('',#17689,.T.);
#11765=FACE_OUTER_BOUND('',#17690,.T.);
#11766=FACE_OUTER_BOUND('',#17691,.T.);
#11767=FACE_OUTER_BOUND('',#17692,.T.);
#11768=FACE_OUTER_BOUND('',#17693,.T.);
#11769=FACE_OUTER_BOUND('',#17694,.T.);
#11770=FACE_OUTER_BOUND('',#17695,.T.);
#11771=FACE_OUTER_BOUND('',#17696,.T.);
#11772=FACE_OUTER_BOUND('',#17697,.T.);
#11773=FACE_OUTER_BOUND('',#17698,.T.);
#11774=FACE_OUTER_BOUND('',#17699,.T.);
#11775=FACE_OUTER_BOUND('',#17700,.T.);
#11776=FACE_OUTER_BOUND('',#17701,.T.);
#11777=FACE_OUTER_BOUND('',#17702,.T.);
#11778=FACE_OUTER_BOUND('',#17703,.T.);
#11779=FACE_OUTER_BOUND('',#17704,.T.);
#11780=FACE_OUTER_BOUND('',#17705,.T.);
#11781=FACE_OUTER_BOUND('',#17706,.T.);
#11782=FACE_OUTER_BOUND('',#17707,.T.);
#11783=FACE_OUTER_BOUND('',#17708,.T.);
#11784=FACE_OUTER_BOUND('',#17709,.T.);
#11785=FACE_OUTER_BOUND('',#17710,.T.);
#11786=FACE_OUTER_BOUND('',#17711,.T.);
#11787=FACE_OUTER_BOUND('',#17712,.T.);
#11788=FACE_OUTER_BOUND('',#17713,.T.);
#11789=FACE_OUTER_BOUND('',#17714,.T.);
#11790=FACE_OUTER_BOUND('',#17715,.T.);
#11791=FACE_OUTER_BOUND('',#17716,.T.);
#11792=FACE_OUTER_BOUND('',#17717,.T.);
#11793=FACE_OUTER_BOUND('',#17718,.T.);
#11794=FACE_OUTER_BOUND('',#17719,.T.);
#11795=FACE_OUTER_BOUND('',#17720,.T.);
#11796=FACE_OUTER_BOUND('',#17721,.T.);
#11797=FACE_OUTER_BOUND('',#17722,.T.);
#11798=FACE_OUTER_BOUND('',#17723,.T.);
#11799=FACE_OUTER_BOUND('',#17724,.T.);
#11800=FACE_OUTER_BOUND('',#17725,.T.);
#11801=FACE_OUTER_BOUND('',#17726,.T.);
#11802=FACE_OUTER_BOUND('',#17727,.T.);
#11803=FACE_OUTER_BOUND('',#17728,.T.);
#11804=FACE_OUTER_BOUND('',#17729,.T.);
#11805=FACE_OUTER_BOUND('',#17730,.T.);
#11806=FACE_OUTER_BOUND('',#17731,.T.);
#11807=FACE_OUTER_BOUND('',#17732,.T.);
#11808=FACE_OUTER_BOUND('',#17733,.T.);
#11809=FACE_OUTER_BOUND('',#17734,.T.);
#11810=FACE_OUTER_BOUND('',#17735,.T.);
#11811=FACE_OUTER_BOUND('',#17736,.T.);
#11812=FACE_OUTER_BOUND('',#17737,.T.);
#11813=FACE_OUTER_BOUND('',#17738,.T.);
#11814=FACE_OUTER_BOUND('',#17739,.T.);
#11815=FACE_OUTER_BOUND('',#17740,.T.);
#11816=FACE_OUTER_BOUND('',#17741,.T.);
#11817=FACE_OUTER_BOUND('',#17742,.T.);
#11818=FACE_OUTER_BOUND('',#17743,.T.);
#11819=FACE_OUTER_BOUND('',#17744,.T.);
#11820=FACE_OUTER_BOUND('',#17745,.T.);
#11821=FACE_OUTER_BOUND('',#17746,.T.);
#11822=FACE_OUTER_BOUND('',#17747,.T.);
#11823=FACE_OUTER_BOUND('',#17748,.T.);
#11824=FACE_OUTER_BOUND('',#17749,.T.);
#11825=FACE_OUTER_BOUND('',#17750,.T.);
#11826=FACE_OUTER_BOUND('',#17751,.T.);
#11827=FACE_OUTER_BOUND('',#17752,.T.);
#11828=FACE_OUTER_BOUND('',#17753,.T.);
#11829=FACE_OUTER_BOUND('',#17754,.T.);
#11830=FACE_OUTER_BOUND('',#17755,.T.);
#11831=FACE_OUTER_BOUND('',#17756,.T.);
#11832=FACE_OUTER_BOUND('',#17757,.T.);
#11833=FACE_OUTER_BOUND('',#17758,.T.);
#11834=FACE_OUTER_BOUND('',#17759,.T.);
#11835=FACE_OUTER_BOUND('',#17760,.T.);
#11836=FACE_OUTER_BOUND('',#17761,.T.);
#11837=FACE_OUTER_BOUND('',#17762,.T.);
#11838=FACE_OUTER_BOUND('',#17763,.T.);
#11839=FACE_OUTER_BOUND('',#17764,.T.);
#11840=FACE_OUTER_BOUND('',#17765,.T.);
#11841=FACE_OUTER_BOUND('',#17766,.T.);
#11842=FACE_OUTER_BOUND('',#17767,.T.);
#11843=FACE_OUTER_BOUND('',#17768,.T.);
#11844=FACE_OUTER_BOUND('',#17769,.T.);
#11845=FACE_OUTER_BOUND('',#17770,.T.);
#11846=FACE_OUTER_BOUND('',#17771,.T.);
#11847=FACE_OUTER_BOUND('',#17772,.T.);
#11848=FACE_OUTER_BOUND('',#17773,.T.);
#11849=FACE_OUTER_BOUND('',#17774,.T.);
#11850=FACE_OUTER_BOUND('',#17775,.T.);
#11851=FACE_OUTER_BOUND('',#17776,.T.);
#11852=FACE_OUTER_BOUND('',#17777,.T.);
#11853=FACE_OUTER_BOUND('',#17778,.T.);
#11854=FACE_OUTER_BOUND('',#17779,.T.);
#11855=FACE_OUTER_BOUND('',#17780,.T.);
#11856=FACE_OUTER_BOUND('',#17781,.T.);
#11857=FACE_OUTER_BOUND('',#17782,.T.);
#11858=FACE_OUTER_BOUND('',#17783,.T.);
#11859=FACE_OUTER_BOUND('',#17784,.T.);
#11860=FACE_OUTER_BOUND('',#17785,.T.);
#11861=FACE_OUTER_BOUND('',#17786,.T.);
#11862=FACE_OUTER_BOUND('',#17787,.T.);
#11863=FACE_OUTER_BOUND('',#17788,.T.);
#11864=FACE_OUTER_BOUND('',#17789,.T.);
#11865=FACE_OUTER_BOUND('',#17790,.T.);
#11866=FACE_OUTER_BOUND('',#17791,.T.);
#11867=FACE_OUTER_BOUND('',#17792,.T.);
#11868=FACE_OUTER_BOUND('',#17793,.T.);
#11869=FACE_OUTER_BOUND('',#17794,.T.);
#11870=FACE_OUTER_BOUND('',#17795,.T.);
#11871=FACE_OUTER_BOUND('',#17796,.T.);
#11872=FACE_OUTER_BOUND('',#17797,.T.);
#11873=FACE_OUTER_BOUND('',#17798,.T.);
#11874=FACE_OUTER_BOUND('',#17799,.T.);
#11875=FACE_OUTER_BOUND('',#17800,.T.);
#11876=FACE_OUTER_BOUND('',#17801,.T.);
#11877=FACE_OUTER_BOUND('',#17802,.T.);
#11878=FACE_OUTER_BOUND('',#17803,.T.);
#11879=FACE_OUTER_BOUND('',#17804,.T.);
#11880=FACE_OUTER_BOUND('',#17805,.T.);
#11881=FACE_OUTER_BOUND('',#17806,.T.);
#11882=FACE_OUTER_BOUND('',#17807,.T.);
#11883=FACE_OUTER_BOUND('',#17808,.T.);
#11884=FACE_OUTER_BOUND('',#17809,.T.);
#11885=FACE_OUTER_BOUND('',#17810,.T.);
#11886=FACE_OUTER_BOUND('',#17811,.T.);
#11887=FACE_OUTER_BOUND('',#17812,.T.);
#11888=FACE_OUTER_BOUND('',#17813,.T.);
#11889=FACE_OUTER_BOUND('',#17814,.T.);
#11890=FACE_OUTER_BOUND('',#17815,.T.);
#11891=FACE_OUTER_BOUND('',#17816,.T.);
#11892=FACE_OUTER_BOUND('',#17817,.T.);
#11893=FACE_OUTER_BOUND('',#17818,.T.);
#11894=FACE_OUTER_BOUND('',#17819,.T.);
#11895=FACE_OUTER_BOUND('',#17820,.T.);
#11896=FACE_OUTER_BOUND('',#17821,.T.);
#11897=FACE_OUTER_BOUND('',#17822,.T.);
#11898=FACE_OUTER_BOUND('',#17823,.T.);
#11899=FACE_OUTER_BOUND('',#17824,.T.);
#11900=FACE_OUTER_BOUND('',#17825,.T.);
#11901=FACE_OUTER_BOUND('',#17826,.T.);
#11902=FACE_OUTER_BOUND('',#17827,.T.);
#11903=FACE_OUTER_BOUND('',#17828,.T.);
#11904=FACE_OUTER_BOUND('',#17829,.T.);
#11905=FACE_OUTER_BOUND('',#17830,.T.);
#11906=FACE_OUTER_BOUND('',#17831,.T.);
#11907=FACE_OUTER_BOUND('',#17832,.T.);
#11908=FACE_OUTER_BOUND('',#17833,.T.);
#11909=FACE_OUTER_BOUND('',#17834,.T.);
#11910=FACE_OUTER_BOUND('',#17835,.T.);
#11911=FACE_OUTER_BOUND('',#17836,.T.);
#11912=FACE_OUTER_BOUND('',#17837,.T.);
#11913=FACE_OUTER_BOUND('',#17838,.T.);
#11914=FACE_OUTER_BOUND('',#17839,.T.);
#11915=FACE_OUTER_BOUND('',#17840,.T.);
#11916=FACE_OUTER_BOUND('',#17841,.T.);
#11917=FACE_OUTER_BOUND('',#17842,.T.);
#11918=FACE_OUTER_BOUND('',#17843,.T.);
#11919=FACE_OUTER_BOUND('',#17844,.T.);
#11920=FACE_OUTER_BOUND('',#17845,.T.);
#11921=FACE_OUTER_BOUND('',#17846,.T.);
#11922=FACE_OUTER_BOUND('',#17847,.T.);
#11923=FACE_OUTER_BOUND('',#17848,.T.);
#11924=FACE_OUTER_BOUND('',#17849,.T.);
#11925=FACE_OUTER_BOUND('',#17850,.T.);
#11926=FACE_OUTER_BOUND('',#17851,.T.);
#11927=FACE_OUTER_BOUND('',#17852,.T.);
#11928=FACE_OUTER_BOUND('',#17853,.T.);
#11929=FACE_OUTER_BOUND('',#17854,.T.);
#11930=FACE_OUTER_BOUND('',#17855,.T.);
#11931=FACE_OUTER_BOUND('',#17856,.T.);
#11932=FACE_OUTER_BOUND('',#17857,.T.);
#11933=FACE_OUTER_BOUND('',#17858,.T.);
#11934=FACE_OUTER_BOUND('',#17859,.T.);
#11935=FACE_OUTER_BOUND('',#17860,.T.);
#11936=FACE_OUTER_BOUND('',#17861,.T.);
#11937=FACE_OUTER_BOUND('',#17862,.T.);
#11938=FACE_OUTER_BOUND('',#17863,.T.);
#11939=FACE_OUTER_BOUND('',#17864,.T.);
#11940=FACE_OUTER_BOUND('',#17865,.T.);
#11941=FACE_OUTER_BOUND('',#17866,.T.);
#11942=FACE_OUTER_BOUND('',#17867,.T.);
#11943=FACE_OUTER_BOUND('',#17868,.T.);
#11944=FACE_OUTER_BOUND('',#17869,.T.);
#11945=FACE_OUTER_BOUND('',#17870,.T.);
#11946=FACE_OUTER_BOUND('',#17871,.T.);
#11947=FACE_OUTER_BOUND('',#17872,.T.);
#11948=FACE_OUTER_BOUND('',#17873,.T.);
#11949=FACE_OUTER_BOUND('',#17874,.T.);
#11950=FACE_OUTER_BOUND('',#17875,.T.);
#11951=FACE_OUTER_BOUND('',#17876,.T.);
#11952=FACE_OUTER_BOUND('',#17877,.T.);
#11953=FACE_OUTER_BOUND('',#17878,.T.);
#11954=FACE_OUTER_BOUND('',#17879,.T.);
#11955=FACE_OUTER_BOUND('',#17880,.T.);
#11956=FACE_OUTER_BOUND('',#17881,.T.);
#11957=FACE_OUTER_BOUND('',#17882,.T.);
#11958=FACE_OUTER_BOUND('',#17883,.T.);
#11959=FACE_OUTER_BOUND('',#17884,.T.);
#11960=FACE_OUTER_BOUND('',#17885,.T.);
#11961=FACE_OUTER_BOUND('',#17886,.T.);
#11962=FACE_OUTER_BOUND('',#17887,.T.);
#11963=FACE_OUTER_BOUND('',#17888,.T.);
#11964=FACE_OUTER_BOUND('',#17889,.T.);
#11965=FACE_OUTER_BOUND('',#17890,.T.);
#11966=FACE_OUTER_BOUND('',#17891,.T.);
#11967=FACE_OUTER_BOUND('',#17892,.T.);
#11968=FACE_OUTER_BOUND('',#17893,.T.);
#11969=FACE_OUTER_BOUND('',#17894,.T.);
#11970=FACE_OUTER_BOUND('',#17900,.T.);
#11971=FACE_OUTER_BOUND('',#17901,.T.);
#11972=FACE_OUTER_BOUND('',#17902,.T.);
#11973=FACE_OUTER_BOUND('',#17903,.T.);
#11974=FACE_OUTER_BOUND('',#17909,.T.);
#11975=FACE_OUTER_BOUND('',#17910,.T.);
#11976=FACE_OUTER_BOUND('',#17911,.T.);
#11977=FACE_OUTER_BOUND('',#17912,.T.);
#11978=FACE_OUTER_BOUND('',#17913,.T.);
#11979=FACE_OUTER_BOUND('',#17914,.T.);
#11980=FACE_OUTER_BOUND('',#17915,.T.);
#11981=FACE_OUTER_BOUND('',#17916,.T.);
#11982=FACE_OUTER_BOUND('',#17917,.T.);
#11983=FACE_OUTER_BOUND('',#17918,.T.);
#11984=FACE_OUTER_BOUND('',#17919,.T.);
#11985=FACE_OUTER_BOUND('',#17920,.T.);
#11986=FACE_OUTER_BOUND('',#17921,.T.);
#11987=FACE_OUTER_BOUND('',#17922,.T.);
#11988=FACE_OUTER_BOUND('',#17923,.T.);
#11989=FACE_OUTER_BOUND('',#17924,.T.);
#11990=FACE_OUTER_BOUND('',#17925,.T.);
#11991=FACE_OUTER_BOUND('',#17926,.T.);
#11992=FACE_OUTER_BOUND('',#17927,.T.);
#11993=FACE_OUTER_BOUND('',#17928,.T.);
#11994=FACE_OUTER_BOUND('',#17929,.T.);
#11995=FACE_OUTER_BOUND('',#17930,.T.);
#11996=FACE_OUTER_BOUND('',#17931,.T.);
#11997=FACE_OUTER_BOUND('',#17932,.T.);
#11998=FACE_OUTER_BOUND('',#17933,.T.);
#11999=FACE_OUTER_BOUND('',#17935,.T.);
#12000=FACE_OUTER_BOUND('',#17937,.T.);
#12001=FACE_OUTER_BOUND('',#17939,.T.);
#12002=FACE_OUTER_BOUND('',#17941,.T.);
#12003=FACE_OUTER_BOUND('',#17943,.T.);
#12004=FACE_OUTER_BOUND('',#17945,.T.);
#12005=FACE_OUTER_BOUND('',#17947,.T.);
#12006=FACE_OUTER_BOUND('',#17949,.T.);
#12007=FACE_OUTER_BOUND('',#17951,.T.);
#12008=FACE_OUTER_BOUND('',#17953,.T.);
#12009=FACE_OUTER_BOUND('',#17955,.T.);
#12010=FACE_OUTER_BOUND('',#17957,.T.);
#12011=FACE_OUTER_BOUND('',#17959,.T.);
#12012=FACE_OUTER_BOUND('',#17961,.T.);
#12013=FACE_OUTER_BOUND('',#17963,.T.);
#12014=FACE_OUTER_BOUND('',#17965,.T.);
#12015=FACE_OUTER_BOUND('',#17967,.T.);
#12016=FACE_OUTER_BOUND('',#17969,.T.);
#12017=FACE_OUTER_BOUND('',#17971,.T.);
#12018=FACE_OUTER_BOUND('',#17973,.T.);
#12019=FACE_OUTER_BOUND('',#17974,.T.);
#12020=FACE_OUTER_BOUND('',#17975,.T.);
#12021=FACE_OUTER_BOUND('',#17976,.T.);
#12022=FACE_OUTER_BOUND('',#17977,.T.);
#12023=FACE_OUTER_BOUND('',#17978,.T.);
#12024=FACE_OUTER_BOUND('',#17979,.T.);
#12025=FACE_OUTER_BOUND('',#17980,.T.);
#12026=FACE_OUTER_BOUND('',#17981,.T.);
#12027=FACE_OUTER_BOUND('',#17982,.T.);
#12028=FACE_OUTER_BOUND('',#17983,.T.);
#12029=FACE_OUTER_BOUND('',#17984,.T.);
#12030=FACE_OUTER_BOUND('',#17985,.T.);
#12031=FACE_OUTER_BOUND('',#17986,.T.);
#12032=FACE_OUTER_BOUND('',#17987,.T.);
#12033=FACE_OUTER_BOUND('',#17988,.T.);
#12034=FACE_OUTER_BOUND('',#17989,.T.);
#12035=FACE_OUTER_BOUND('',#17990,.T.);
#12036=FACE_OUTER_BOUND('',#17991,.T.);
#12037=FACE_OUTER_BOUND('',#17992,.T.);
#12038=FACE_OUTER_BOUND('',#17993,.T.);
#12039=FACE_OUTER_BOUND('',#17994,.T.);
#12040=FACE_OUTER_BOUND('',#17995,.T.);
#12041=FACE_OUTER_BOUND('',#17996,.T.);
#12042=FACE_OUTER_BOUND('',#17997,.T.);
#12043=FACE_OUTER_BOUND('',#17998,.T.);
#12044=FACE_OUTER_BOUND('',#17999,.T.);
#12045=FACE_OUTER_BOUND('',#18000,.T.);
#12046=FACE_OUTER_BOUND('',#18001,.T.);
#12047=FACE_OUTER_BOUND('',#18002,.T.);
#12048=FACE_OUTER_BOUND('',#18003,.T.);
#12049=FACE_OUTER_BOUND('',#18004,.T.);
#12050=FACE_OUTER_BOUND('',#18005,.T.);
#12051=FACE_OUTER_BOUND('',#18006,.T.);
#12052=FACE_OUTER_BOUND('',#18007,.T.);
#12053=FACE_OUTER_BOUND('',#18008,.T.);
#12054=FACE_OUTER_BOUND('',#18009,.T.);
#12055=FACE_OUTER_BOUND('',#18010,.T.);
#12056=FACE_OUTER_BOUND('',#18011,.T.);
#12057=FACE_OUTER_BOUND('',#18012,.T.);
#12058=FACE_OUTER_BOUND('',#18013,.T.);
#12059=FACE_OUTER_BOUND('',#18014,.T.);
#12060=FACE_OUTER_BOUND('',#18015,.T.);
#12061=FACE_OUTER_BOUND('',#18016,.T.);
#12062=FACE_OUTER_BOUND('',#18017,.T.);
#12063=FACE_OUTER_BOUND('',#18018,.T.);
#12064=FACE_OUTER_BOUND('',#18020,.T.);
#12065=FACE_OUTER_BOUND('',#18021,.T.);
#12066=FACE_OUTER_BOUND('',#18022,.T.);
#12067=FACE_OUTER_BOUND('',#18023,.T.);
#12068=FACE_OUTER_BOUND('',#18024,.T.);
#12069=FACE_OUTER_BOUND('',#18025,.T.);
#12070=FACE_OUTER_BOUND('',#18026,.T.);
#12071=FACE_OUTER_BOUND('',#18027,.T.);
#12072=FACE_OUTER_BOUND('',#18028,.T.);
#12073=FACE_OUTER_BOUND('',#18029,.T.);
#12074=FACE_OUTER_BOUND('',#18030,.T.);
#12075=FACE_OUTER_BOUND('',#18031,.T.);
#12076=FACE_OUTER_BOUND('',#18032,.T.);
#12077=FACE_OUTER_BOUND('',#18034,.T.);
#12078=FACE_OUTER_BOUND('',#18035,.T.);
#12079=FACE_OUTER_BOUND('',#18037,.T.);
#12080=FACE_OUTER_BOUND('',#18039,.T.);
#12081=FACE_OUTER_BOUND('',#18041,.T.);
#12082=FACE_OUTER_BOUND('',#18042,.T.);
#12083=FACE_OUTER_BOUND('',#18043,.T.);
#12084=FACE_OUTER_BOUND('',#18045,.T.);
#12085=FACE_OUTER_BOUND('',#18046,.T.);
#12086=FACE_OUTER_BOUND('',#18047,.T.);
#12087=FACE_OUTER_BOUND('',#18048,.T.);
#12088=FACE_OUTER_BOUND('',#18049,.T.);
#12089=FACE_OUTER_BOUND('',#18050,.T.);
#12090=FACE_OUTER_BOUND('',#18051,.T.);
#12091=FACE_OUTER_BOUND('',#18052,.T.);
#12092=FACE_OUTER_BOUND('',#18053,.T.);
#12093=FACE_OUTER_BOUND('',#18054,.T.);
#12094=FACE_OUTER_BOUND('',#18055,.T.);
#12095=FACE_OUTER_BOUND('',#18056,.T.);
#12096=FACE_OUTER_BOUND('',#18057,.T.);
#12097=FACE_OUTER_BOUND('',#18058,.T.);
#12098=FACE_OUTER_BOUND('',#18059,.T.);
#12099=FACE_OUTER_BOUND('',#18060,.T.);
#12100=FACE_OUTER_BOUND('',#18061,.T.);
#12101=FACE_OUTER_BOUND('',#18062,.T.);
#12102=FACE_OUTER_BOUND('',#18064,.T.);
#12103=FACE_OUTER_BOUND('',#18065,.T.);
#12104=FACE_OUTER_BOUND('',#18066,.T.);
#12105=FACE_OUTER_BOUND('',#18067,.T.);
#12106=FACE_OUTER_BOUND('',#18068,.T.);
#12107=FACE_OUTER_BOUND('',#18069,.T.);
#12108=FACE_OUTER_BOUND('',#18070,.T.);
#12109=FACE_OUTER_BOUND('',#18071,.T.);
#12110=FACE_OUTER_BOUND('',#18072,.T.);
#12111=FACE_OUTER_BOUND('',#18073,.T.);
#12112=FACE_OUTER_BOUND('',#18075,.T.);
#12113=FACE_OUTER_BOUND('',#18077,.T.);
#12114=FACE_OUTER_BOUND('',#18078,.T.);
#12115=FACE_OUTER_BOUND('',#18079,.T.);
#12116=FACE_OUTER_BOUND('',#18080,.T.);
#12117=FACE_OUTER_BOUND('',#18081,.T.);
#12118=FACE_OUTER_BOUND('',#18082,.T.);
#12119=FACE_OUTER_BOUND('',#18083,.T.);
#12120=FACE_OUTER_BOUND('',#18085,.T.);
#12121=FACE_OUTER_BOUND('',#18086,.T.);
#12122=FACE_OUTER_BOUND('',#18087,.T.);
#12123=FACE_OUTER_BOUND('',#18088,.T.);
#12124=FACE_OUTER_BOUND('',#18089,.T.);
#12125=FACE_OUTER_BOUND('',#18090,.T.);
#12126=FACE_OUTER_BOUND('',#18091,.T.);
#12127=FACE_OUTER_BOUND('',#18092,.T.);
#12128=FACE_OUTER_BOUND('',#18093,.T.);
#12129=FACE_OUTER_BOUND('',#18096,.T.);
#12130=FACE_OUTER_BOUND('',#18097,.T.);
#12131=FACE_OUTER_BOUND('',#18098,.T.);
#12132=FACE_OUTER_BOUND('',#18101,.T.);
#12133=FACE_OUTER_BOUND('',#18104,.T.);
#12134=FACE_OUTER_BOUND('',#18106,.T.);
#12135=FACE_OUTER_BOUND('',#18108,.T.);
#12136=FACE_OUTER_BOUND('',#18109,.T.);
#12137=FACE_OUTER_BOUND('',#18110,.T.);
#12138=FACE_OUTER_BOUND('',#18111,.T.);
#12139=FACE_OUTER_BOUND('',#18112,.T.);
#12140=FACE_OUTER_BOUND('',#18113,.T.);
#12141=FACE_OUTER_BOUND('',#18114,.T.);
#12142=FACE_OUTER_BOUND('',#18115,.T.);
#12143=FACE_OUTER_BOUND('',#18116,.T.);
#12144=FACE_OUTER_BOUND('',#18117,.T.);
#12145=FACE_OUTER_BOUND('',#18118,.T.);
#12146=FACE_OUTER_BOUND('',#18119,.T.);
#12147=FACE_OUTER_BOUND('',#18120,.T.);
#12148=FACE_OUTER_BOUND('',#18121,.T.);
#12149=FACE_OUTER_BOUND('',#18122,.T.);
#12150=FACE_OUTER_BOUND('',#18123,.T.);
#12151=FACE_OUTER_BOUND('',#18124,.T.);
#12152=FACE_OUTER_BOUND('',#18125,.T.);
#12153=FACE_OUTER_BOUND('',#18126,.T.);
#12154=FACE_OUTER_BOUND('',#18127,.T.);
#12155=FACE_OUTER_BOUND('',#18128,.T.);
#12156=FACE_OUTER_BOUND('',#18129,.T.);
#12157=FACE_OUTER_BOUND('',#18130,.T.);
#12158=FACE_OUTER_BOUND('',#18131,.T.);
#12159=EDGE_LOOP('',(#58028,#58029,#58030,#58031,#58032));
#12160=EDGE_LOOP('',(#58033,#58034,#58035,#58036,#58037));
#12161=EDGE_LOOP('',(#58038,#58039,#58040,#58041,#58042));
#12162=EDGE_LOOP('',(#58043,#58044,#58045,#58046));
#12163=EDGE_LOOP('',(#58047,#58048,#58049,#58050,#58051));
#12164=EDGE_LOOP('',(#58052,#58053,#58054,#58055,#58056));
#12165=EDGE_LOOP('',(#58057,#58058,#58059,#58060,#58061));
#12166=EDGE_LOOP('',(#58062,#58063,#58064,#58065));
#12167=EDGE_LOOP('',(#58066,#58067,#58068,#58069));
#12168=EDGE_LOOP('',(#58070,#58071,#58072,#58073,#58074,#58075));
#12169=EDGE_LOOP('',(#58076,#58077,#58078,#58079,#58080,#58081));
#12170=EDGE_LOOP('',(#58082,#58083,#58084,#58085,#58086));
#12171=EDGE_LOOP('',(#58087,#58088,#58089,#58090));
#12172=EDGE_LOOP('',(#58091,#58092,#58093,#58094,#58095,#58096));
#12173=EDGE_LOOP('',(#58097,#58098,#58099,#58100,#58101,#58102));
#12174=EDGE_LOOP('',(#58103,#58104,#58105,#58106,#58107));
#12175=EDGE_LOOP('',(#58108,#58109,#58110,#58111));
#12176=EDGE_LOOP('',(#58112,#58113,#58114,#58115));
#12177=EDGE_LOOP('',(#58116,#58117,#58118,#58119,#58120));
#12178=EDGE_LOOP('',(#58121,#58122,#58123,#58124,#58125));
#12179=EDGE_LOOP('',(#58126,#58127,#58128,#58129,#58130,#58131,#58132,#58133,
#58134,#58135,#58136,#58137,#58138,#58139));
#12180=EDGE_LOOP('',(#58140,#58141,#58142,#58143,#58144,#58145,#58146,#58147,
#58148,#58149,#58150,#58151,#58152,#58153,#58154,#58155,#58156,#58157,#58158,
#58159));
#12181=EDGE_LOOP('',(#58160,#58161,#58162,#58163,#58164,#58165));
#12182=EDGE_LOOP('',(#58166,#58167,#58168,#58169));
#12183=EDGE_LOOP('',(#58170,#58171,#58172,#58173,#58174,#58175,#58176,#58177,
#58178,#58179,#58180,#58181,#58182,#58183));
#12184=EDGE_LOOP('',(#58184,#58185,#58186,#58187,#58188,#58189,#58190,#58191,
#58192,#58193,#58194,#58195,#58196,#58197,#58198,#58199,#58200,#58201,#58202,
#58203));
#12185=EDGE_LOOP('',(#58204,#58205,#58206,#58207,#58208,#58209,#58210));
#12186=EDGE_LOOP('',(#58211,#58212,#58213,#58214));
#12187=EDGE_LOOP('',(#58215,#58216,#58217,#58218));
#12188=EDGE_LOOP('',(#58219,#58220,#58221,#58222));
#12189=EDGE_LOOP('',(#58223));
#12190=EDGE_LOOP('',(#58224));
#12191=EDGE_LOOP('',(#58225,#58226,#58227,#58228,#58229));
#12192=EDGE_LOOP('',(#58230,#58231,#58232,#58233,#58234,#58235,#58236,#58237,
#58238,#58239,#58240,#58241,#58242,#58243,#58244,#58245,#58246));
#12193=EDGE_LOOP('',(#58247));
#12194=EDGE_LOOP('',(#58248));
#12195=EDGE_LOOP('',(#58249,#58250,#58251,#58252,#58253));
#12196=EDGE_LOOP('',(#58254,#58255,#58256,#58257,#58258));
#12197=EDGE_LOOP('',(#58259));
#12198=EDGE_LOOP('',(#58260));
#12199=EDGE_LOOP('',(#58261,#58262,#58263,#58264));
#12200=EDGE_LOOP('',(#58265));
#12201=EDGE_LOOP('',(#58266));
#12202=EDGE_LOOP('',(#58267,#58268,#58269,#58270));
#12203=EDGE_LOOP('',(#58271,#58272,#58273,#58274));
#12204=EDGE_LOOP('',(#58275,#58276,#58277,#58278));
#12205=EDGE_LOOP('',(#58279,#58280,#58281,#58282));
#12206=EDGE_LOOP('',(#58283,#58284,#58285,#58286));
#12207=EDGE_LOOP('',(#58287,#58288,#58289,#58290));
#12208=EDGE_LOOP('',(#58291,#58292,#58293,#58294));
#12209=EDGE_LOOP('',(#58295,#58296,#58297,#58298));
#12210=EDGE_LOOP('',(#58299,#58300,#58301,#58302));
#12211=EDGE_LOOP('',(#58303,#58304,#58305,#58306));
#12212=EDGE_LOOP('',(#58307,#58308,#58309,#58310));
#12213=EDGE_LOOP('',(#58311,#58312,#58313,#58314));
#12214=EDGE_LOOP('',(#58315,#58316,#58317,#58318));
#12215=EDGE_LOOP('',(#58319,#58320,#58321,#58322));
#12216=EDGE_LOOP('',(#58323,#58324,#58325,#58326));
#12217=EDGE_LOOP('',(#58327,#58328,#58329,#58330));
#12218=EDGE_LOOP('',(#58331,#58332,#58333,#58334));
#12219=EDGE_LOOP('',(#58335,#58336,#58337,#58338));
#12220=EDGE_LOOP('',(#58339,#58340,#58341,#58342));
#12221=EDGE_LOOP('',(#58343,#58344,#58345,#58346));
#12222=EDGE_LOOP('',(#58347,#58348,#58349,#58350));
#12223=EDGE_LOOP('',(#58351,#58352,#58353,#58354));
#12224=EDGE_LOOP('',(#58355,#58356,#58357,#58358));
#12225=EDGE_LOOP('',(#58359,#58360,#58361,#58362));
#12226=EDGE_LOOP('',(#58363,#58364,#58365,#58366));
#12227=EDGE_LOOP('',(#58367,#58368,#58369,#58370));
#12228=EDGE_LOOP('',(#58371,#58372,#58373,#58374));
#12229=EDGE_LOOP('',(#58375,#58376,#58377,#58378));
#12230=EDGE_LOOP('',(#58379,#58380,#58381,#58382));
#12231=EDGE_LOOP('',(#58383,#58384,#58385,#58386,#58387,#58388,#58389,#58390,
#58391,#58392,#58393,#58394));
#12232=EDGE_LOOP('',(#58395,#58396,#58397,#58398,#58399));
#12233=EDGE_LOOP('',(#58400,#58401,#58402,#58403,#58404));
#12234=EDGE_LOOP('',(#58405));
#12235=EDGE_LOOP('',(#58406,#58407,#58408,#58409));
#12236=EDGE_LOOP('',(#58410,#58411,#58412,#58413));
#12237=EDGE_LOOP('',(#58414,#58415,#58416,#58417));
#12238=EDGE_LOOP('',(#58418,#58419,#58420,#58421));
#12239=EDGE_LOOP('',(#58422,#58423,#58424,#58425));
#12240=EDGE_LOOP('',(#58426,#58427,#58428,#58429,#58430,#58431,#58432,#58433,
#58434,#58435,#58436,#58437,#58438,#58439,#58440,#58441,#58442,#58443,#58444,
#58445,#58446,#58447,#58448,#58449,#58450,#58451,#58452,#58453,#58454,#58455,
#58456,#58457,#58458,#58459,#58460,#58461,#58462,#58463,#58464,#58465,#58466,
#58467,#58468,#58469,#58470,#58471,#58472,#58473,#58474,#58475,#58476,#58477,
#58478,#58479,#58480,#58481,#58482,#58483,#58484,#58485));
#12241=EDGE_LOOP('',(#58486));
#12242=EDGE_LOOP('',(#58487));
#12243=EDGE_LOOP('',(#58488,#58489,#58490,#58491,#58492,#58493,#58494,#58495,
#58496,#58497,#58498,#58499,#58500,#58501,#58502,#58503,#58504,#58505,#58506,
#58507,#58508,#58509,#58510,#58511,#58512,#58513,#58514,#58515,#58516,#58517,
#58518,#58519,#58520,#58521,#58522,#58523,#58524,#58525,#58526,#58527,#58528,
#58529,#58530,#58531,#58532,#58533,#58534,#58535,#58536,#58537,#58538,#58539,
#58540,#58541,#58542,#58543,#58544,#58545,#58546,#58547));
#12244=EDGE_LOOP('',(#58548));
#12245=EDGE_LOOP('',(#58549,#58550,#58551,#58552));
#12246=EDGE_LOOP('',(#58553,#58554,#58555,#58556));
#12247=EDGE_LOOP('',(#58557,#58558,#58559,#58560));
#12248=EDGE_LOOP('',(#58561,#58562,#58563,#58564));
#12249=EDGE_LOOP('',(#58565,#58566,#58567,#58568));
#12250=EDGE_LOOP('',(#58569,#58570,#58571,#58572));
#12251=EDGE_LOOP('',(#58573,#58574,#58575,#58576));
#12252=EDGE_LOOP('',(#58577,#58578,#58579,#58580));
#12253=EDGE_LOOP('',(#58581,#58582,#58583,#58584));
#12254=EDGE_LOOP('',(#58585,#58586,#58587,#58588));
#12255=EDGE_LOOP('',(#58589,#58590,#58591,#58592));
#12256=EDGE_LOOP('',(#58593,#58594,#58595,#58596));
#12257=EDGE_LOOP('',(#58597,#58598,#58599,#58600));
#12258=EDGE_LOOP('',(#58601,#58602,#58603,#58604));
#12259=EDGE_LOOP('',(#58605,#58606,#58607,#58608));
#12260=EDGE_LOOP('',(#58609,#58610,#58611,#58612));
#12261=EDGE_LOOP('',(#58613,#58614,#58615,#58616));
#12262=EDGE_LOOP('',(#58617,#58618,#58619,#58620));
#12263=EDGE_LOOP('',(#58621,#58622,#58623,#58624));
#12264=EDGE_LOOP('',(#58625,#58626,#58627,#58628));
#12265=EDGE_LOOP('',(#58629,#58630,#58631,#58632));
#12266=EDGE_LOOP('',(#58633,#58634,#58635,#58636));
#12267=EDGE_LOOP('',(#58637,#58638,#58639,#58640));
#12268=EDGE_LOOP('',(#58641,#58642,#58643,#58644));
#12269=EDGE_LOOP('',(#58645,#58646,#58647,#58648));
#12270=EDGE_LOOP('',(#58649,#58650,#58651,#58652));
#12271=EDGE_LOOP('',(#58653,#58654,#58655,#58656));
#12272=EDGE_LOOP('',(#58657,#58658,#58659,#58660));
#12273=EDGE_LOOP('',(#58661,#58662,#58663,#58664));
#12274=EDGE_LOOP('',(#58665,#58666,#58667,#58668));
#12275=EDGE_LOOP('',(#58669,#58670,#58671,#58672));
#12276=EDGE_LOOP('',(#58673,#58674,#58675,#58676));
#12277=EDGE_LOOP('',(#58677,#58678,#58679,#58680));
#12278=EDGE_LOOP('',(#58681,#58682,#58683,#58684));
#12279=EDGE_LOOP('',(#58685,#58686,#58687,#58688));
#12280=EDGE_LOOP('',(#58689,#58690,#58691,#58692));
#12281=EDGE_LOOP('',(#58693,#58694,#58695,#58696));
#12282=EDGE_LOOP('',(#58697,#58698,#58699,#58700));
#12283=EDGE_LOOP('',(#58701,#58702,#58703,#58704));
#12284=EDGE_LOOP('',(#58705,#58706,#58707,#58708));
#12285=EDGE_LOOP('',(#58709,#58710,#58711,#58712));
#12286=EDGE_LOOP('',(#58713,#58714,#58715,#58716));
#12287=EDGE_LOOP('',(#58717,#58718,#58719,#58720));
#12288=EDGE_LOOP('',(#58721,#58722,#58723,#58724));
#12289=EDGE_LOOP('',(#58725,#58726,#58727,#58728));
#12290=EDGE_LOOP('',(#58729,#58730,#58731,#58732));
#12291=EDGE_LOOP('',(#58733,#58734,#58735,#58736));
#12292=EDGE_LOOP('',(#58737,#58738,#58739,#58740));
#12293=EDGE_LOOP('',(#58741,#58742,#58743,#58744));
#12294=EDGE_LOOP('',(#58745,#58746,#58747,#58748));
#12295=EDGE_LOOP('',(#58749,#58750,#58751,#58752));
#12296=EDGE_LOOP('',(#58753,#58754,#58755,#58756));
#12297=EDGE_LOOP('',(#58757,#58758,#58759,#58760));
#12298=EDGE_LOOP('',(#58761,#58762,#58763,#58764));
#12299=EDGE_LOOP('',(#58765,#58766,#58767,#58768));
#12300=EDGE_LOOP('',(#58769,#58770,#58771,#58772));
#12301=EDGE_LOOP('',(#58773,#58774,#58775,#58776));
#12302=EDGE_LOOP('',(#58777,#58778,#58779,#58780));
#12303=EDGE_LOOP('',(#58781,#58782,#58783,#58784));
#12304=EDGE_LOOP('',(#58785,#58786,#58787,#58788));
#12305=EDGE_LOOP('',(#58789,#58790,#58791,#58792,#58793));
#12306=EDGE_LOOP('',(#58794,#58795,#58796,#58797,#58798));
#12307=EDGE_LOOP('',(#58799,#58800,#58801,#58802,#58803,#58804));
#12308=EDGE_LOOP('',(#58805,#58806,#58807,#58808,#58809));
#12309=EDGE_LOOP('',(#58810,#58811,#58812,#58813,#58814));
#12310=EDGE_LOOP('',(#58815,#58816,#58817,#58818,#58819));
#12311=EDGE_LOOP('',(#58820,#58821,#58822,#58823,#58824,#58825));
#12312=EDGE_LOOP('',(#58826,#58827,#58828,#58829,#58830));
#12313=EDGE_LOOP('',(#58831,#58832,#58833,#58834,#58835));
#12314=EDGE_LOOP('',(#58836,#58837,#58838,#58839,#58840,#58841));
#12315=EDGE_LOOP('',(#58842,#58843,#58844,#58845,#58846));
#12316=EDGE_LOOP('',(#58847,#58848,#58849,#58850,#58851));
#12317=EDGE_LOOP('',(#58852,#58853,#58854,#58855,#58856,#58857));
#12318=EDGE_LOOP('',(#58858,#58859,#58860,#58861,#58862));
#12319=EDGE_LOOP('',(#58863,#58864,#58865,#58866,#58867));
#12320=EDGE_LOOP('',(#58868,#58869,#58870,#58871,#58872,#58873));
#12321=EDGE_LOOP('',(#58874,#58875,#58876,#58877,#58878));
#12322=EDGE_LOOP('',(#58879,#58880,#58881,#58882,#58883));
#12323=EDGE_LOOP('',(#58884,#58885,#58886,#58887,#58888,#58889));
#12324=EDGE_LOOP('',(#58890,#58891,#58892,#58893,#58894));
#12325=EDGE_LOOP('',(#58895,#58896,#58897,#58898,#58899));
#12326=EDGE_LOOP('',(#58900,#58901,#58902,#58903,#58904,#58905));
#12327=EDGE_LOOP('',(#58906,#58907,#58908,#58909,#58910));
#12328=EDGE_LOOP('',(#58911,#58912,#58913,#58914,#58915));
#12329=EDGE_LOOP('',(#58916,#58917,#58918,#58919,#58920,#58921));
#12330=EDGE_LOOP('',(#58922,#58923,#58924,#58925,#58926));
#12331=EDGE_LOOP('',(#58927,#58928,#58929,#58930,#58931));
#12332=EDGE_LOOP('',(#58932,#58933,#58934,#58935,#58936,#58937));
#12333=EDGE_LOOP('',(#58938,#58939,#58940,#58941,#58942));
#12334=EDGE_LOOP('',(#58943,#58944,#58945,#58946,#58947));
#12335=EDGE_LOOP('',(#58948,#58949,#58950,#58951,#58952,#58953));
#12336=EDGE_LOOP('',(#58954,#58955,#58956,#58957,#58958));
#12337=EDGE_LOOP('',(#58959,#58960,#58961,#58962,#58963));
#12338=EDGE_LOOP('',(#58964,#58965,#58966,#58967,#58968,#58969));
#12339=EDGE_LOOP('',(#58970,#58971,#58972,#58973,#58974));
#12340=EDGE_LOOP('',(#58975,#58976,#58977,#58978,#58979));
#12341=EDGE_LOOP('',(#58980,#58981,#58982,#58983,#58984,#58985));
#12342=EDGE_LOOP('',(#58986,#58987,#58988,#58989,#58990));
#12343=EDGE_LOOP('',(#58991,#58992,#58993,#58994,#58995));
#12344=EDGE_LOOP('',(#58996,#58997,#58998,#58999,#59000,#59001));
#12345=EDGE_LOOP('',(#59002,#59003,#59004,#59005,#59006));
#12346=EDGE_LOOP('',(#59007,#59008,#59009,#59010,#59011));
#12347=EDGE_LOOP('',(#59012,#59013,#59014,#59015));
#12348=EDGE_LOOP('',(#59016,#59017,#59018,#59019,#59020,#59021));
#12349=EDGE_LOOP('',(#59022,#59023,#59024,#59025,#59026));
#12350=EDGE_LOOP('',(#59027,#59028,#59029,#59030,#59031));
#12351=EDGE_LOOP('',(#59032,#59033,#59034,#59035,#59036));
#12352=EDGE_LOOP('',(#59037,#59038,#59039,#59040));
#12353=EDGE_LOOP('',(#59041,#59042,#59043,#59044));
#12354=EDGE_LOOP('',(#59045));
#12355=EDGE_LOOP('',(#59046,#59047,#59048,#59049));
#12356=EDGE_LOOP('',(#59050,#59051,#59052,#59053));
#12357=EDGE_LOOP('',(#59054,#59055,#59056,#59057));
#12358=EDGE_LOOP('',(#59058,#59059,#59060,#59061));
#12359=EDGE_LOOP('',(#59062,#59063,#59064,#59065));
#12360=EDGE_LOOP('',(#59066,#59067,#59068,#59069));
#12361=EDGE_LOOP('',(#59070,#59071,#59072,#59073));
#12362=EDGE_LOOP('',(#59074,#59075,#59076,#59077));
#12363=EDGE_LOOP('',(#59078,#59079,#59080,#59081));
#12364=EDGE_LOOP('',(#59082,#59083,#59084,#59085));
#12365=EDGE_LOOP('',(#59086,#59087,#59088,#59089));
#12366=EDGE_LOOP('',(#59090,#59091,#59092,#59093));
#12367=EDGE_LOOP('',(#59094,#59095,#59096,#59097,#59098,#59099,#59100,#59101,
#59102,#59103,#59104,#59105,#59106,#59107,#59108,#59109,#59110,#59111,#59112,
#59113));
#12368=EDGE_LOOP('',(#59114,#59115,#59116,#59117));
#12369=EDGE_LOOP('',(#59118,#59119,#59120,#59121));
#12370=EDGE_LOOP('',(#59122,#59123,#59124,#59125));
#12371=EDGE_LOOP('',(#59126,#59127,#59128,#59129));
#12372=EDGE_LOOP('',(#59130,#59131,#59132,#59133,#59134,#59135,#59136,#59137,
#59138,#59139,#59140,#59141,#59142,#59143,#59144,#59145,#59146,#59147,#59148,
#59149));
#12373=EDGE_LOOP('',(#59150));
#12374=EDGE_LOOP('',(#59151));
#12375=EDGE_LOOP('',(#59152,#59153,#59154,#59155));
#12376=EDGE_LOOP('',(#59156));
#12377=EDGE_LOOP('',(#59157));
#12378=EDGE_LOOP('',(#59158,#59159,#59160,#59161,#59162,#59163,#59164));
#12379=EDGE_LOOP('',(#59165,#59166,#59167,#59168,#59169,#59170,#59171));
#12380=EDGE_LOOP('',(#59172,#59173,#59174,#59175,#59176,#59177));
#12381=EDGE_LOOP('',(#59178,#59179,#59180,#59181,#59182,#59183,#59184));
#12382=EDGE_LOOP('',(#59185,#59186,#59187,#59188,#59189,#59190,#59191));
#12383=EDGE_LOOP('',(#59192,#59193,#59194,#59195));
#12384=EDGE_LOOP('',(#59196,#59197,#59198,#59199,#59200,#59201,#59202));
#12385=EDGE_LOOP('',(#59203,#59204,#59205,#59206,#59207,#59208,#59209));
#12386=EDGE_LOOP('',(#59210,#59211,#59212,#59213));
#12387=EDGE_LOOP('',(#59214,#59215,#59216,#59217,#59218,#59219,#59220));
#12388=EDGE_LOOP('',(#59221,#59222,#59223,#59224,#59225,#59226,#59227));
#12389=EDGE_LOOP('',(#59228,#59229,#59230,#59231));
#12390=EDGE_LOOP('',(#59232,#59233,#59234,#59235));
#12391=EDGE_LOOP('',(#59236,#59237,#59238,#59239));
#12392=EDGE_LOOP('',(#59240,#59241,#59242,#59243,#59244,#59245,#59246,#59247,
#59248,#59249,#59250,#59251));
#12393=EDGE_LOOP('',(#59252,#59253,#59254,#59255));
#12394=EDGE_LOOP('',(#59256,#59257,#59258,#59259));
#12395=EDGE_LOOP('',(#59260,#59261,#59262,#59263));
#12396=EDGE_LOOP('',(#59264,#59265,#59266,#59267));
#12397=EDGE_LOOP('',(#59268,#59269,#59270,#59271));
#12398=EDGE_LOOP('',(#59272,#59273,#59274,#59275));
#12399=EDGE_LOOP('',(#59276,#59277,#59278,#59279));
#12400=EDGE_LOOP('',(#59280,#59281,#59282,#59283));
#12401=EDGE_LOOP('',(#59284,#59285,#59286,#59287));
#12402=EDGE_LOOP('',(#59288,#59289,#59290,#59291,#59292,#59293));
#12403=EDGE_LOOP('',(#59294,#59295,#59296,#59297));
#12404=EDGE_LOOP('',(#59298,#59299,#59300,#59301,#59302,#59303));
#12405=EDGE_LOOP('',(#59304,#59305,#59306,#59307,#59308,#59309,#59310,#59311,
#59312,#59313,#59314,#59315));
#12406=EDGE_LOOP('',(#59316,#59317,#59318,#59319));
#12407=EDGE_LOOP('',(#59320,#59321,#59322,#59323));
#12408=EDGE_LOOP('',(#59324,#59325,#59326,#59327));
#12409=EDGE_LOOP('',(#59328,#59329,#59330,#59331));
#12410=EDGE_LOOP('',(#59332,#59333,#59334,#59335));
#12411=EDGE_LOOP('',(#59336,#59337,#59338,#59339));
#12412=EDGE_LOOP('',(#59340,#59341,#59342,#59343));
#12413=EDGE_LOOP('',(#59344,#59345,#59346,#59347));
#12414=EDGE_LOOP('',(#59348,#59349,#59350,#59351));
#12415=EDGE_LOOP('',(#59352,#59353,#59354,#59355));
#12416=EDGE_LOOP('',(#59356,#59357,#59358,#59359,#59360,#59361,#59362,#59363,
#59364,#59365));
#12417=EDGE_LOOP('',(#59366,#59367,#59368,#59369));
#12418=EDGE_LOOP('',(#59370,#59371,#59372,#59373));
#12419=EDGE_LOOP('',(#59374,#59375,#59376,#59377));
#12420=EDGE_LOOP('',(#59378,#59379,#59380,#59381));
#12421=EDGE_LOOP('',(#59382,#59383,#59384,#59385,#59386,#59387,#59388,#59389,
#59390,#59391));
#12422=EDGE_LOOP('',(#59392,#59393,#59394,#59395));
#12423=EDGE_LOOP('',(#59396,#59397,#59398,#59399));
#12424=EDGE_LOOP('',(#59400,#59401,#59402,#59403));
#12425=EDGE_LOOP('',(#59404,#59405,#59406,#59407));
#12426=EDGE_LOOP('',(#59408,#59409,#59410,#59411));
#12427=EDGE_LOOP('',(#59412,#59413,#59414,#59415));
#12428=EDGE_LOOP('',(#59416,#59417,#59418,#59419));
#12429=EDGE_LOOP('',(#59420,#59421,#59422,#59423));
#12430=EDGE_LOOP('',(#59424,#59425,#59426,#59427));
#12431=EDGE_LOOP('',(#59428,#59429,#59430,#59431));
#12432=EDGE_LOOP('',(#59432,#59433,#59434,#59435));
#12433=EDGE_LOOP('',(#59436,#59437,#59438,#59439));
#12434=EDGE_LOOP('',(#59440,#59441,#59442,#59443,#59444));
#12435=EDGE_LOOP('',(#59445,#59446,#59447,#59448));
#12436=EDGE_LOOP('',(#59449,#59450,#59451,#59452));
#12437=EDGE_LOOP('',(#59453,#59454,#59455,#59456));
#12438=EDGE_LOOP('',(#59457,#59458,#59459,#59460));
#12439=EDGE_LOOP('',(#59461,#59462,#59463,#59464));
#12440=EDGE_LOOP('',(#59465,#59466,#59467,#59468,#59469,#59470,#59471,#59472,
#59473,#59474,#59475,#59476,#59477,#59478,#59479,#59480));
#12441=EDGE_LOOP('',(#59481,#59482,#59483,#59484));
#12442=EDGE_LOOP('',(#59485,#59486,#59487,#59488));
#12443=EDGE_LOOP('',(#59489,#59490,#59491,#59492,#59493,#59494,#59495,#59496,
#59497,#59498,#59499,#59500,#59501,#59502));
#12444=EDGE_LOOP('',(#59503,#59504,#59505,#59506));
#12445=EDGE_LOOP('',(#59507,#59508,#59509,#59510));
#12446=EDGE_LOOP('',(#59511,#59512,#59513,#59514));
#12447=EDGE_LOOP('',(#59515,#59516,#59517,#59518));
#12448=EDGE_LOOP('',(#59519,#59520,#59521,#59522));
#12449=EDGE_LOOP('',(#59523,#59524,#59525,#59526));
#12450=EDGE_LOOP('',(#59527,#59528,#59529,#59530));
#12451=EDGE_LOOP('',(#59531,#59532,#59533,#59534));
#12452=EDGE_LOOP('',(#59535,#59536,#59537,#59538));
#12453=EDGE_LOOP('',(#59539,#59540,#59541,#59542));
#12454=EDGE_LOOP('',(#59543,#59544,#59545,#59546));
#12455=EDGE_LOOP('',(#59547,#59548,#59549,#59550));
#12456=EDGE_LOOP('',(#59551,#59552,#59553,#59554,#59555,#59556));
#12457=EDGE_LOOP('',(#59557,#59558,#59559,#59560));
#12458=EDGE_LOOP('',(#59561,#59562,#59563,#59564));
#12459=EDGE_LOOP('',(#59565,#59566,#59567,#59568));
#12460=EDGE_LOOP('',(#59569,#59570,#59571,#59572));
#12461=EDGE_LOOP('',(#59573,#59574,#59575,#59576,#59577,#59578,#59579,#59580,
#59581,#59582,#59583,#59584));
#12462=EDGE_LOOP('',(#59585,#59586,#59587,#59588));
#12463=EDGE_LOOP('',(#59589,#59590,#59591,#59592));
#12464=EDGE_LOOP('',(#59593,#59594,#59595,#59596));
#12465=EDGE_LOOP('',(#59597,#59598,#59599,#59600));
#12466=EDGE_LOOP('',(#59601,#59602,#59603,#59604));
#12467=EDGE_LOOP('',(#59605,#59606,#59607,#59608));
#12468=EDGE_LOOP('',(#59609,#59610,#59611,#59612));
#12469=EDGE_LOOP('',(#59613,#59614,#59615,#59616));
#12470=EDGE_LOOP('',(#59617,#59618,#59619,#59620));
#12471=EDGE_LOOP('',(#59621,#59622,#59623,#59624));
#12472=EDGE_LOOP('',(#59625,#59626,#59627,#59628));
#12473=EDGE_LOOP('',(#59629,#59630,#59631,#59632,#59633,#59634));
#12474=EDGE_LOOP('',(#59635,#59636,#59637,#59638));
#12475=EDGE_LOOP('',(#59639,#59640,#59641,#59642));
#12476=EDGE_LOOP('',(#59643,#59644,#59645,#59646));
#12477=EDGE_LOOP('',(#59647,#59648,#59649,#59650));
#12478=EDGE_LOOP('',(#59651,#59652,#59653,#59654,#59655,#59656));
#12479=EDGE_LOOP('',(#59657,#59658,#59659,#59660,#59661,#59662,#59663,#59664,
#59665,#59666,#59667));
#12480=EDGE_LOOP('',(#59668,#59669,#59670,#59671));
#12481=EDGE_LOOP('',(#59672,#59673,#59674,#59675));
#12482=EDGE_LOOP('',(#59676,#59677,#59678,#59679));
#12483=EDGE_LOOP('',(#59680,#59681,#59682,#59683));
#12484=EDGE_LOOP('',(#59684,#59685,#59686,#59687));
#12485=EDGE_LOOP('',(#59688,#59689,#59690,#59691));
#12486=EDGE_LOOP('',(#59692,#59693,#59694,#59695));
#12487=EDGE_LOOP('',(#59696,#59697,#59698,#59699));
#12488=EDGE_LOOP('',(#59700,#59701,#59702,#59703));
#12489=EDGE_LOOP('',(#59704,#59705,#59706,#59707));
#12490=EDGE_LOOP('',(#59708,#59709,#59710,#59711));
#12491=EDGE_LOOP('',(#59712,#59713,#59714,#59715));
#12492=EDGE_LOOP('',(#59716,#59717,#59718,#59719));
#12493=EDGE_LOOP('',(#59720,#59721,#59722,#59723));
#12494=EDGE_LOOP('',(#59724,#59725,#59726,#59727));
#12495=EDGE_LOOP('',(#59728,#59729,#59730,#59731));
#12496=EDGE_LOOP('',(#59732,#59733,#59734,#59735));
#12497=EDGE_LOOP('',(#59736,#59737,#59738,#59739));
#12498=EDGE_LOOP('',(#59740,#59741,#59742,#59743));
#12499=EDGE_LOOP('',(#59744,#59745,#59746,#59747));
#12500=EDGE_LOOP('',(#59748,#59749,#59750,#59751));
#12501=EDGE_LOOP('',(#59752,#59753,#59754,#59755,#59756,#59757,#59758,#59759,
#59760,#59761,#59762,#59763,#59764,#59765));
#12502=EDGE_LOOP('',(#59766,#59767,#59768,#59769));
#12503=EDGE_LOOP('',(#59770,#59771,#59772,#59773));
#12504=EDGE_LOOP('',(#59774,#59775,#59776,#59777));
#12505=EDGE_LOOP('',(#59778,#59779,#59780,#59781));
#12506=EDGE_LOOP('',(#59782,#59783,#59784,#59785));
#12507=EDGE_LOOP('',(#59786,#59787,#59788,#59789));
#12508=EDGE_LOOP('',(#59790,#59791,#59792,#59793));
#12509=EDGE_LOOP('',(#59794,#59795,#59796,#59797));
#12510=EDGE_LOOP('',(#59798,#59799,#59800,#59801));
#12511=EDGE_LOOP('',(#59802,#59803,#59804,#59805));
#12512=EDGE_LOOP('',(#59806,#59807,#59808,#59809));
#12513=EDGE_LOOP('',(#59810,#59811,#59812,#59813));
#12514=EDGE_LOOP('',(#59814,#59815,#59816,#59817));
#12515=EDGE_LOOP('',(#59818,#59819,#59820,#59821));
#12516=EDGE_LOOP('',(#59822,#59823,#59824,#59825,#59826,#59827,#59828,#59829,
#59830));
#12517=EDGE_LOOP('',(#59831,#59832,#59833,#59834));
#12518=EDGE_LOOP('',(#59835,#59836,#59837,#59838));
#12519=EDGE_LOOP('',(#59839,#59840,#59841,#59842));
#12520=EDGE_LOOP('',(#59843,#59844,#59845,#59846));
#12521=EDGE_LOOP('',(#59847,#59848,#59849,#59850));
#12522=EDGE_LOOP('',(#59851,#59852,#59853,#59854));
#12523=EDGE_LOOP('',(#59855,#59856,#59857,#59858));
#12524=EDGE_LOOP('',(#59859,#59860,#59861,#59862));
#12525=EDGE_LOOP('',(#59863,#59864,#59865,#59866));
#12526=EDGE_LOOP('',(#59867,#59868,#59869,#59870));
#12527=EDGE_LOOP('',(#59871,#59872,#59873,#59874));
#12528=EDGE_LOOP('',(#59875,#59876,#59877,#59878));
#12529=EDGE_LOOP('',(#59879,#59880,#59881,#59882));
#12530=EDGE_LOOP('',(#59883,#59884,#59885,#59886));
#12531=EDGE_LOOP('',(#59887,#59888,#59889,#59890));
#12532=EDGE_LOOP('',(#59891,#59892,#59893,#59894));
#12533=EDGE_LOOP('',(#59895,#59896,#59897,#59898));
#12534=EDGE_LOOP('',(#59899,#59900,#59901,#59902));
#12535=EDGE_LOOP('',(#59903,#59904,#59905,#59906));
#12536=EDGE_LOOP('',(#59907,#59908,#59909,#59910));
#12537=EDGE_LOOP('',(#59911,#59912,#59913,#59914));
#12538=EDGE_LOOP('',(#59915,#59916,#59917,#59918));
#12539=EDGE_LOOP('',(#59919,#59920,#59921,#59922));
#12540=EDGE_LOOP('',(#59923,#59924,#59925,#59926,#59927,#59928));
#12541=EDGE_LOOP('',(#59929,#59930,#59931,#59932,#59933,#59934,#59935,#59936,
#59937,#59938,#59939,#59940,#59941,#59942,#59943,#59944));
#12542=EDGE_LOOP('',(#59945,#59946,#59947,#59948));
#12543=EDGE_LOOP('',(#59949,#59950,#59951,#59952));
#12544=EDGE_LOOP('',(#59953,#59954,#59955,#59956));
#12545=EDGE_LOOP('',(#59957,#59958,#59959,#59960));
#12546=EDGE_LOOP('',(#59961,#59962,#59963,#59964));
#12547=EDGE_LOOP('',(#59965,#59966,#59967,#59968));
#12548=EDGE_LOOP('',(#59969,#59970,#59971,#59972));
#12549=EDGE_LOOP('',(#59973,#59974,#59975,#59976));
#12550=EDGE_LOOP('',(#59977,#59978,#59979,#59980));
#12551=EDGE_LOOP('',(#59981,#59982,#59983,#59984,#59985,#59986,#59987,#59988));
#12552=EDGE_LOOP('',(#59989,#59990,#59991,#59992));
#12553=EDGE_LOOP('',(#59993,#59994,#59995,#59996));
#12554=EDGE_LOOP('',(#59997,#59998,#59999,#60000));
#12555=EDGE_LOOP('',(#60001,#60002,#60003,#60004));
#12556=EDGE_LOOP('',(#60005,#60006,#60007,#60008,#60009,#60010,#60011,#60012,
#60013));
#12557=EDGE_LOOP('',(#60014,#60015,#60016,#60017));
#12558=EDGE_LOOP('',(#60018,#60019,#60020,#60021));
#12559=EDGE_LOOP('',(#60022,#60023,#60024,#60025));
#12560=EDGE_LOOP('',(#60026,#60027,#60028,#60029));
#12561=EDGE_LOOP('',(#60030,#60031,#60032,#60033));
#12562=EDGE_LOOP('',(#60034,#60035,#60036,#60037));
#12563=EDGE_LOOP('',(#60038,#60039,#60040,#60041));
#12564=EDGE_LOOP('',(#60042,#60043,#60044,#60045));
#12565=EDGE_LOOP('',(#60046,#60047,#60048,#60049));
#12566=EDGE_LOOP('',(#60050,#60051,#60052,#60053));
#12567=EDGE_LOOP('',(#60054,#60055,#60056,#60057));
#12568=EDGE_LOOP('',(#60058,#60059,#60060,#60061));
#12569=EDGE_LOOP('',(#60062,#60063,#60064,#60065,#60066,#60067,#60068,#60069));
#12570=EDGE_LOOP('',(#60070,#60071,#60072,#60073));
#12571=EDGE_LOOP('',(#60074,#60075,#60076,#60077));
#12572=EDGE_LOOP('',(#60078,#60079,#60080,#60081));
#12573=EDGE_LOOP('',(#60082,#60083,#60084,#60085));
#12574=EDGE_LOOP('',(#60086,#60087,#60088,#60089,#60090,#60091,#60092,#60093,
#60094,#60095,#60096,#60097,#60098,#60099,#60100,#60101,#60102,#60103));
#12575=EDGE_LOOP('',(#60104,#60105,#60106,#60107,#60108,#60109));
#12576=EDGE_LOOP('',(#60110,#60111,#60112,#60113));
#12577=EDGE_LOOP('',(#60114,#60115,#60116,#60117,#60118,#60119,#60120,#60121,
#60122,#60123,#60124,#60125,#60126,#60127));
#12578=EDGE_LOOP('',(#60128,#60129,#60130,#60131,#60132,#60133));
#12579=EDGE_LOOP('',(#60134,#60135,#60136,#60137));
#12580=EDGE_LOOP('',(#60138,#60139,#60140,#60141,#60142,#60143,#60144,#60145,
#60146,#60147,#60148,#60149,#60150,#60151,#60152,#60153,#60154,#60155,#60156,
#60157,#60158,#60159,#60160,#60161,#60162,#60163,#60164,#60165,#60166,#60167,
#60168,#60169));
#12581=EDGE_LOOP('',(#60170));
#12582=EDGE_LOOP('',(#60171,#60172,#60173,#60174));
#12583=EDGE_LOOP('',(#60175,#60176,#60177,#60178,#60179,#60180,#60181,#60182,
#60183,#60184,#60185,#60186,#60187,#60188,#60189,#60190,#60191,#60192,#60193,
#60194,#60195,#60196,#60197));
#12584=EDGE_LOOP('',(#60198,#60199,#60200,#60201,#60202,#60203,#60204,#60205,
#60206,#60207,#60208,#60209,#60210,#60211));
#12585=EDGE_LOOP('',(#60212));
#12586=EDGE_LOOP('',(#60213,#60214,#60215,#60216,#60217,#60218));
#12587=EDGE_LOOP('',(#60219,#60220,#60221,#60222));
#12588=EDGE_LOOP('',(#60223,#60224,#60225,#60226));
#12589=EDGE_LOOP('',(#60227,#60228,#60229,#60230,#60231,#60232,#60233,#60234,
#60235,#60236,#60237,#60238,#60239,#60240,#60241,#60242,#60243,#60244,#60245,
#60246,#60247,#60248,#60249,#60250,#60251,#60252));
#12590=EDGE_LOOP('',(#60253));
#12591=EDGE_LOOP('',(#60254,#60255,#60256,#60257));
#12592=EDGE_LOOP('',(#60258));
#12593=EDGE_LOOP('',(#60259));
#12594=EDGE_LOOP('',(#60260));
#12595=EDGE_LOOP('',(#60261,#60262,#60263,#60264));
#12596=EDGE_LOOP('',(#60265,#60266,#60267,#60268,#60269,#60270));
#12597=EDGE_LOOP('',(#60271,#60272,#60273,#60274));
#12598=EDGE_LOOP('',(#60275,#60276,#60277,#60278));
#12599=EDGE_LOOP('',(#60279,#60280,#60281,#60282,#60283,#60284));
#12600=EDGE_LOOP('',(#60285,#60286,#60287,#60288,#60289,#60290,#60291,#60292,
#60293,#60294,#60295,#60296,#60297,#60298,#60299,#60300,#60301,#60302,#60303,
#60304,#60305,#60306,#60307,#60308,#60309));
#12601=EDGE_LOOP('',(#60310,#60311,#60312,#60313));
#12602=EDGE_LOOP('',(#60314,#60315,#60316,#60317));
#12603=EDGE_LOOP('',(#60318,#60319,#60320,#60321));
#12604=EDGE_LOOP('',(#60322,#60323,#60324,#60325,#60326,#60327,#60328,#60329,
#60330,#60331,#60332,#60333,#60334,#60335,#60336,#60337,#60338,#60339,#60340,
#60341,#60342,#60343,#60344,#60345,#60346,#60347,#60348,#60349,#60350,#60351,
#60352,#60353));
#12605=EDGE_LOOP('',(#60354));
#12606=EDGE_LOOP('',(#60355,#60356,#60357,#60358));
#12607=EDGE_LOOP('',(#60359,#60360,#60361,#60362));
#12608=EDGE_LOOP('',(#60363,#60364,#60365,#60366,#60367,#60368));
#12609=EDGE_LOOP('',(#60369,#60370,#60371,#60372));
#12610=EDGE_LOOP('',(#60373,#60374,#60375,#60376));
#12611=EDGE_LOOP('',(#60377,#60378,#60379,#60380));
#12612=EDGE_LOOP('',(#60381,#60382,#60383,#60384));
#12613=EDGE_LOOP('',(#60385,#60386,#60387,#60388));
#12614=EDGE_LOOP('',(#60389,#60390,#60391,#60392));
#12615=EDGE_LOOP('',(#60393,#60394,#60395,#60396));
#12616=EDGE_LOOP('',(#60397,#60398,#60399,#60400));
#12617=EDGE_LOOP('',(#60401,#60402,#60403,#60404));
#12618=EDGE_LOOP('',(#60405,#60406,#60407,#60408));
#12619=EDGE_LOOP('',(#60409,#60410,#60411,#60412));
#12620=EDGE_LOOP('',(#60413,#60414,#60415,#60416));
#12621=EDGE_LOOP('',(#60417,#60418,#60419,#60420,#60421,#60422));
#12622=EDGE_LOOP('',(#60423,#60424,#60425,#60426));
#12623=EDGE_LOOP('',(#60427,#60428,#60429,#60430));
#12624=EDGE_LOOP('',(#60431,#60432,#60433,#60434));
#12625=EDGE_LOOP('',(#60435,#60436,#60437,#60438));
#12626=EDGE_LOOP('',(#60439,#60440,#60441,#60442,#60443,#60444,#60445,#60446));
#12627=EDGE_LOOP('',(#60447,#60448,#60449,#60450));
#12628=EDGE_LOOP('',(#60451,#60452,#60453,#60454));
#12629=EDGE_LOOP('',(#60455,#60456,#60457,#60458));
#12630=EDGE_LOOP('',(#60459,#60460,#60461,#60462));
#12631=EDGE_LOOP('',(#60463,#60464,#60465,#60466,#60467,#60468));
#12632=EDGE_LOOP('',(#60469,#60470,#60471,#60472));
#12633=EDGE_LOOP('',(#60473,#60474,#60475,#60476));
#12634=EDGE_LOOP('',(#60477,#60478,#60479,#60480));
#12635=EDGE_LOOP('',(#60481,#60482,#60483,#60484));
#12636=EDGE_LOOP('',(#60485,#60486,#60487,#60488));
#12637=EDGE_LOOP('',(#60489,#60490,#60491,#60492));
#12638=EDGE_LOOP('',(#60493,#60494,#60495,#60496));
#12639=EDGE_LOOP('',(#60497,#60498,#60499,#60500,#60501,#60502));
#12640=EDGE_LOOP('',(#60503,#60504,#60505,#60506));
#12641=EDGE_LOOP('',(#60507,#60508,#60509,#60510,#60511,#60512));
#12642=EDGE_LOOP('',(#60513,#60514,#60515,#60516));
#12643=EDGE_LOOP('',(#60517,#60518,#60519,#60520,#60521,#60522,#60523,#60524));
#12644=EDGE_LOOP('',(#60525,#60526,#60527,#60528));
#12645=EDGE_LOOP('',(#60529,#60530,#60531,#60532,#60533));
#12646=EDGE_LOOP('',(#60534,#60535,#60536,#60537,#60538));
#12647=EDGE_LOOP('',(#60539));
#12648=EDGE_LOOP('',(#60540));
#12649=EDGE_LOOP('',(#60541,#60542,#60543,#60544));
#12650=EDGE_LOOP('',(#60545,#60546,#60547,#60548));
#12651=EDGE_LOOP('',(#60549,#60550,#60551,#60552,#60553,#60554,#60555,#60556,
#60557));
#12652=EDGE_LOOP('',(#60558,#60559,#60560,#60561,#60562,#60563));
#12653=EDGE_LOOP('',(#60564,#60565,#60566,#60567));
#12654=EDGE_LOOP('',(#60568,#60569,#60570,#60571));
#12655=EDGE_LOOP('',(#60572,#60573,#60574,#60575));
#12656=EDGE_LOOP('',(#60576,#60577,#60578,#60579));
#12657=EDGE_LOOP('',(#60580,#60581,#60582,#60583));
#12658=EDGE_LOOP('',(#60584,#60585,#60586,#60587));
#12659=EDGE_LOOP('',(#60588,#60589,#60590,#60591));
#12660=EDGE_LOOP('',(#60592,#60593,#60594,#60595));
#12661=EDGE_LOOP('',(#60596,#60597,#60598,#60599,#60600,#60601));
#12662=EDGE_LOOP('',(#60602,#60603,#60604,#60605));
#12663=EDGE_LOOP('',(#60606,#60607,#60608,#60609));
#12664=EDGE_LOOP('',(#60610,#60611,#60612,#60613));
#12665=EDGE_LOOP('',(#60614,#60615,#60616,#60617));
#12666=EDGE_LOOP('',(#60618,#60619,#60620,#60621));
#12667=EDGE_LOOP('',(#60622,#60623,#60624,#60625));
#12668=EDGE_LOOP('',(#60626,#60627,#60628,#60629));
#12669=EDGE_LOOP('',(#60630,#60631,#60632,#60633));
#12670=EDGE_LOOP('',(#60634,#60635,#60636,#60637));
#12671=EDGE_LOOP('',(#60638,#60639,#60640,#60641));
#12672=EDGE_LOOP('',(#60642,#60643,#60644,#60645));
#12673=EDGE_LOOP('',(#60646,#60647,#60648,#60649));
#12674=EDGE_LOOP('',(#60650,#60651,#60652,#60653,#60654,#60655));
#12675=EDGE_LOOP('',(#60656,#60657,#60658,#60659,#60660,#60661,#60662,#60663,
#60664,#60665,#60666,#60667,#60668,#60669,#60670,#60671,#60672));
#12676=EDGE_LOOP('',(#60673,#60674,#60675,#60676,#60677,#60678,#60679,#60680));
#12677=EDGE_LOOP('',(#60681));
#12678=EDGE_LOOP('',(#60682,#60683,#60684,#60685,#60686));
#12679=EDGE_LOOP('',(#60687,#60688,#60689,#60690));
#12680=EDGE_LOOP('',(#60691,#60692,#60693,#60694));
#12681=EDGE_LOOP('',(#60695,#60696,#60697,#60698));
#12682=EDGE_LOOP('',(#60699,#60700,#60701,#60702));
#12683=EDGE_LOOP('',(#60703,#60704,#60705,#60706));
#12684=EDGE_LOOP('',(#60707,#60708,#60709,#60710));
#12685=EDGE_LOOP('',(#60711,#60712,#60713,#60714,#60715,#60716));
#12686=EDGE_LOOP('',(#60717));
#12687=EDGE_LOOP('',(#60718,#60719,#60720,#60721));
#12688=EDGE_LOOP('',(#60722));
#12689=EDGE_LOOP('',(#60723));
#12690=EDGE_LOOP('',(#60724,#60725,#60726,#60727));
#12691=EDGE_LOOP('',(#60728,#60729,#60730,#60731));
#12692=EDGE_LOOP('',(#60732,#60733,#60734,#60735));
#12693=EDGE_LOOP('',(#60736,#60737,#60738,#60739));
#12694=EDGE_LOOP('',(#60740,#60741,#60742,#60743));
#12695=EDGE_LOOP('',(#60744,#60745,#60746,#60747));
#12696=EDGE_LOOP('',(#60748,#60749,#60750,#60751));
#12697=EDGE_LOOP('',(#60752,#60753,#60754,#60755));
#12698=EDGE_LOOP('',(#60756));
#12699=EDGE_LOOP('',(#60757,#60758,#60759,#60760));
#12700=EDGE_LOOP('',(#60761,#60762,#60763,#60764));
#12701=EDGE_LOOP('',(#60765,#60766,#60767,#60768));
#12702=EDGE_LOOP('',(#60769,#60770,#60771,#60772));
#12703=EDGE_LOOP('',(#60773,#60774,#60775,#60776));
#12704=EDGE_LOOP('',(#60777,#60778,#60779,#60780));
#12705=EDGE_LOOP('',(#60781,#60782,#60783,#60784));
#12706=EDGE_LOOP('',(#60785,#60786,#60787,#60788));
#12707=EDGE_LOOP('',(#60789,#60790,#60791,#60792,#60793,#60794,#60795,#60796,
#60797,#60798,#60799,#60800,#60801,#60802));
#12708=EDGE_LOOP('',(#60803,#60804,#60805,#60806));
#12709=EDGE_LOOP('',(#60807,#60808,#60809,#60810,#60811));
#12710=EDGE_LOOP('',(#60812,#60813,#60814,#60815));
#12711=EDGE_LOOP('',(#60816,#60817,#60818,#60819));
#12712=EDGE_LOOP('',(#60820,#60821,#60822,#60823));
#12713=EDGE_LOOP('',(#60824,#60825,#60826,#60827));
#12714=EDGE_LOOP('',(#60828,#60829,#60830,#60831,#60832,#60833,#60834,#60835));
#12715=EDGE_LOOP('',(#60836,#60837,#60838,#60839));
#12716=EDGE_LOOP('',(#60840,#60841,#60842,#60843));
#12717=EDGE_LOOP('',(#60844,#60845,#60846,#60847));
#12718=EDGE_LOOP('',(#60848,#60849,#60850,#60851,#60852,#60853));
#12719=EDGE_LOOP('',(#60854,#60855,#60856,#60857));
#12720=EDGE_LOOP('',(#60858,#60859,#60860));
#12721=EDGE_LOOP('',(#60861,#60862,#60863,#60864));
#12722=EDGE_LOOP('',(#60865,#60866,#60867));
#12723=EDGE_LOOP('',(#60868,#60869,#60870,#60871));
#12724=EDGE_LOOP('',(#60872,#60873,#60874,#60875));
#12725=EDGE_LOOP('',(#60876,#60877,#60878,#60879));
#12726=EDGE_LOOP('',(#60880,#60881,#60882,#60883,#60884,#60885,#60886,#60887,
#60888,#60889,#60890,#60891,#60892,#60893,#60894,#60895,#60896,#60897,#60898,
#60899));
#12727=EDGE_LOOP('',(#60900,#60901,#60902,#60903));
#12728=EDGE_LOOP('',(#60904,#60905,#60906,#60907));
#12729=EDGE_LOOP('',(#60908,#60909,#60910,#60911,#60912,#60913));
#12730=EDGE_LOOP('',(#60914,#60915,#60916,#60917));
#12731=EDGE_LOOP('',(#60918,#60919,#60920,#60921));
#12732=EDGE_LOOP('',(#60922,#60923,#60924,#60925));
#12733=EDGE_LOOP('',(#60926,#60927,#60928,#60929));
#12734=EDGE_LOOP('',(#60930,#60931,#60932,#60933));
#12735=EDGE_LOOP('',(#60934,#60935,#60936,#60937));
#12736=EDGE_LOOP('',(#60938,#60939,#60940,#60941));
#12737=EDGE_LOOP('',(#60942,#60943,#60944,#60945));
#12738=EDGE_LOOP('',(#60946,#60947,#60948,#60949));
#12739=EDGE_LOOP('',(#60950,#60951,#60952,#60953));
#12740=EDGE_LOOP('',(#60954,#60955,#60956,#60957));
#12741=EDGE_LOOP('',(#60958,#60959,#60960,#60961,#60962,#60963));
#12742=EDGE_LOOP('',(#60964,#60965,#60966,#60967,#60968,#60969,#60970,#60971));
#12743=EDGE_LOOP('',(#60972,#60973,#60974,#60975));
#12744=EDGE_LOOP('',(#60976,#60977,#60978,#60979));
#12745=EDGE_LOOP('',(#60980,#60981,#60982,#60983));
#12746=EDGE_LOOP('',(#60984,#60985,#60986,#60987));
#12747=EDGE_LOOP('',(#60988,#60989,#60990,#60991));
#12748=EDGE_LOOP('',(#60992,#60993,#60994,#60995));
#12749=EDGE_LOOP('',(#60996,#60997,#60998,#60999));
#12750=EDGE_LOOP('',(#61000,#61001,#61002,#61003));
#12751=EDGE_LOOP('',(#61004,#61005,#61006,#61007));
#12752=EDGE_LOOP('',(#61008,#61009,#61010,#61011));
#12753=EDGE_LOOP('',(#61012,#61013,#61014,#61015));
#12754=EDGE_LOOP('',(#61016,#61017,#61018,#61019));
#12755=EDGE_LOOP('',(#61020,#61021,#61022,#61023,#61024,#61025,#61026,#61027));
#12756=EDGE_LOOP('',(#61028,#61029,#61030,#61031,#61032));
#12757=EDGE_LOOP('',(#61033,#61034,#61035,#61036));
#12758=EDGE_LOOP('',(#61037,#61038,#61039,#61040,#61041,#61042,#61043));
#12759=EDGE_LOOP('',(#61044,#61045,#61046,#61047,#61048,#61049,#61050,#61051,
#61052,#61053,#61054,#61055,#61056));
#12760=EDGE_LOOP('',(#61057,#61058,#61059,#61060));
#12761=EDGE_LOOP('',(#61061,#61062,#61063,#61064,#61065,#61066,#61067));
#12762=EDGE_LOOP('',(#61068,#61069,#61070,#61071));
#12763=EDGE_LOOP('',(#61072,#61073,#61074,#61075,#61076));
#12764=EDGE_LOOP('',(#61077,#61078,#61079,#61080,#61081,#61082,#61083,#61084,
#61085,#61086));
#12765=EDGE_LOOP('',(#61087,#61088,#61089,#61090));
#12766=EDGE_LOOP('',(#61091,#61092,#61093,#61094));
#12767=EDGE_LOOP('',(#61095,#61096,#61097,#61098,#61099,#61100,#61101));
#12768=EDGE_LOOP('',(#61102));
#12769=EDGE_LOOP('',(#61103,#61104,#61105,#61106));
#12770=EDGE_LOOP('',(#61107,#61108,#61109,#61110,#61111,#61112,#61113,#61114,
#61115,#61116,#61117,#61118,#61119,#61120,#61121,#61122));
#12771=EDGE_LOOP('',(#61123,#61124,#61125,#61126,#61127));
#12772=EDGE_LOOP('',(#61128,#61129,#61130,#61131,#61132));
#12773=EDGE_LOOP('',(#61133,#61134,#61135,#61136));
#12774=EDGE_LOOP('',(#61137,#61138,#61139,#61140));
#12775=EDGE_LOOP('',(#61141,#61142,#61143,#61144));
#12776=EDGE_LOOP('',(#61145,#61146,#61147,#61148));
#12777=EDGE_LOOP('',(#61149,#61150,#61151,#61152));
#12778=EDGE_LOOP('',(#61153,#61154,#61155,#61156));
#12779=EDGE_LOOP('',(#61157,#61158,#61159,#61160));
#12780=EDGE_LOOP('',(#61161,#61162,#61163,#61164));
#12781=EDGE_LOOP('',(#61165,#61166,#61167,#61168,#61169,#61170));
#12782=EDGE_LOOP('',(#61171,#61172,#61173,#61174,#61175,#61176,#61177));
#12783=EDGE_LOOP('',(#61178,#61179,#61180,#61181));
#12784=EDGE_LOOP('',(#61182,#61183,#61184,#61185,#61186,#61187));
#12785=EDGE_LOOP('',(#61188,#61189,#61190,#61191,#61192,#61193,#61194,#61195));
#12786=EDGE_LOOP('',(#61196,#61197,#61198));
#12787=EDGE_LOOP('',(#61199,#61200,#61201,#61202));
#12788=EDGE_LOOP('',(#61203,#61204,#61205,#61206,#61207));
#12789=EDGE_LOOP('',(#61208,#61209,#61210,#61211,#61212,#61213,#61214,#61215,
#61216));
#12790=EDGE_LOOP('',(#61217,#61218,#61219,#61220));
#12791=EDGE_LOOP('',(#61221,#61222,#61223,#61224));
#12792=EDGE_LOOP('',(#61225,#61226,#61227,#61228));
#12793=EDGE_LOOP('',(#61229,#61230,#61231,#61232));
#12794=EDGE_LOOP('',(#61233,#61234,#61235,#61236));
#12795=EDGE_LOOP('',(#61237,#61238,#61239,#61240));
#12796=EDGE_LOOP('',(#61241,#61242,#61243,#61244));
#12797=EDGE_LOOP('',(#61245,#61246,#61247,#61248,#61249,#61250));
#12798=EDGE_LOOP('',(#61251,#61252,#61253,#61254));
#12799=EDGE_LOOP('',(#61255,#61256,#61257,#61258));
#12800=EDGE_LOOP('',(#61259,#61260,#61261,#61262));
#12801=EDGE_LOOP('',(#61263,#61264,#61265,#61266));
#12802=EDGE_LOOP('',(#61267,#61268,#61269,#61270));
#12803=EDGE_LOOP('',(#61271,#61272,#61273,#61274));
#12804=EDGE_LOOP('',(#61275,#61276,#61277,#61278));
#12805=EDGE_LOOP('',(#61279,#61280,#61281,#61282));
#12806=EDGE_LOOP('',(#61283,#61284,#61285,#61286,#61287,#61288,#61289,#61290,
#61291,#61292,#61293,#61294,#61295,#61296,#61297));
#12807=EDGE_LOOP('',(#61298,#61299,#61300));
#12808=EDGE_LOOP('',(#61301,#61302,#61303,#61304));
#12809=EDGE_LOOP('',(#61305,#61306,#61307,#61308));
#12810=EDGE_LOOP('',(#61309,#61310,#61311,#61312));
#12811=EDGE_LOOP('',(#61313,#61314,#61315,#61316));
#12812=EDGE_LOOP('',(#61317,#61318,#61319,#61320));
#12813=EDGE_LOOP('',(#61321,#61322,#61323,#61324));
#12814=EDGE_LOOP('',(#61325,#61326,#61327,#61328));
#12815=EDGE_LOOP('',(#61329,#61330,#61331,#61332));
#12816=EDGE_LOOP('',(#61333,#61334,#61335,#61336));
#12817=EDGE_LOOP('',(#61337,#61338,#61339,#61340));
#12818=EDGE_LOOP('',(#61341,#61342,#61343,#61344));
#12819=EDGE_LOOP('',(#61345,#61346,#61347));
#12820=EDGE_LOOP('',(#61348,#61349,#61350,#61351));
#12821=EDGE_LOOP('',(#61352,#61353,#61354,#61355));
#12822=EDGE_LOOP('',(#61356,#61357,#61358,#61359));
#12823=EDGE_LOOP('',(#61360,#61361,#61362,#61363));
#12824=EDGE_LOOP('',(#61364,#61365,#61366,#61367));
#12825=EDGE_LOOP('',(#61368,#61369,#61370,#61371));
#12826=EDGE_LOOP('',(#61372,#61373,#61374,#61375,#61376,#61377,#61378,#61379,
#61380,#61381,#61382));
#12827=EDGE_LOOP('',(#61383,#61384,#61385,#61386));
#12828=EDGE_LOOP('',(#61387,#61388,#61389,#61390));
#12829=EDGE_LOOP('',(#61391,#61392,#61393,#61394));
#12830=EDGE_LOOP('',(#61395,#61396,#61397,#61398));
#12831=EDGE_LOOP('',(#61399,#61400,#61401,#61402));
#12832=EDGE_LOOP('',(#61403,#61404,#61405,#61406));
#12833=EDGE_LOOP('',(#61407,#61408,#61409,#61410));
#12834=EDGE_LOOP('',(#61411,#61412,#61413,#61414));
#12835=EDGE_LOOP('',(#61415,#61416,#61417,#61418));
#12836=EDGE_LOOP('',(#61419,#61420,#61421,#61422));
#12837=EDGE_LOOP('',(#61423,#61424,#61425,#61426));
#12838=EDGE_LOOP('',(#61427,#61428,#61429,#61430));
#12839=EDGE_LOOP('',(#61431,#61432,#61433,#61434));
#12840=EDGE_LOOP('',(#61435,#61436,#61437,#61438));
#12841=EDGE_LOOP('',(#61439,#61440,#61441,#61442));
#12842=EDGE_LOOP('',(#61443,#61444,#61445,#61446));
#12843=EDGE_LOOP('',(#61447,#61448,#61449,#61450));
#12844=EDGE_LOOP('',(#61451,#61452,#61453,#61454));
#12845=EDGE_LOOP('',(#61455,#61456,#61457,#61458,#61459,#61460,#61461,#61462,
#61463,#61464,#61465,#61466));
#12846=EDGE_LOOP('',(#61467,#61468,#61469,#61470));
#12847=EDGE_LOOP('',(#61471,#61472,#61473,#61474));
#12848=EDGE_LOOP('',(#61475,#61476,#61477,#61478));
#12849=EDGE_LOOP('',(#61479,#61480,#61481,#61482));
#12850=EDGE_LOOP('',(#61483,#61484,#61485,#61486));
#12851=EDGE_LOOP('',(#61487,#61488,#61489,#61490));
#12852=EDGE_LOOP('',(#61491,#61492,#61493,#61494));
#12853=EDGE_LOOP('',(#61495,#61496,#61497,#61498));
#12854=EDGE_LOOP('',(#61499,#61500,#61501,#61502));
#12855=EDGE_LOOP('',(#61503,#61504,#61505,#61506));
#12856=EDGE_LOOP('',(#61507,#61508,#61509,#61510));
#12857=EDGE_LOOP('',(#61511,#61512,#61513,#61514));
#12858=EDGE_LOOP('',(#61515,#61516,#61517,#61518));
#12859=EDGE_LOOP('',(#61519,#61520,#61521,#61522,#61523,#61524));
#12860=EDGE_LOOP('',(#61525,#61526,#61527,#61528,#61529,#61530,#61531,#61532,
#61533,#61534,#61535));
#12861=EDGE_LOOP('',(#61536,#61537,#61538,#61539));
#12862=EDGE_LOOP('',(#61540,#61541,#61542,#61543));
#12863=EDGE_LOOP('',(#61544,#61545,#61546,#61547,#61548,#61549,#61550,#61551,
#61552,#61553,#61554));
#12864=EDGE_LOOP('',(#61555,#61556,#61557,#61558));
#12865=EDGE_LOOP('',(#61559,#61560,#61561,#61562));
#12866=EDGE_LOOP('',(#61563,#61564,#61565,#61566));
#12867=EDGE_LOOP('',(#61567,#61568,#61569,#61570));
#12868=EDGE_LOOP('',(#61571,#61572,#61573,#61574));
#12869=EDGE_LOOP('',(#61575,#61576,#61577,#61578,#61579,#61580));
#12870=EDGE_LOOP('',(#61581,#61582,#61583,#61584));
#12871=EDGE_LOOP('',(#61585,#61586,#61587,#61588,#61589,#61590,#61591,#61592,
#61593,#61594));
#12872=EDGE_LOOP('',(#61595,#61596,#61597,#61598));
#12873=EDGE_LOOP('',(#61599,#61600,#61601,#61602,#61603,#61604));
#12874=EDGE_LOOP('',(#61605,#61606,#61607,#61608,#61609,#61610,#61611,#61612,
#61613,#61614,#61615,#61616,#61617,#61618));
#12875=EDGE_LOOP('',(#61619,#61620,#61621,#61622));
#12876=EDGE_LOOP('',(#61623,#61624,#61625,#61626));
#12877=EDGE_LOOP('',(#61627,#61628,#61629,#61630));
#12878=EDGE_LOOP('',(#61631,#61632,#61633,#61634));
#12879=EDGE_LOOP('',(#61635,#61636,#61637,#61638));
#12880=EDGE_LOOP('',(#61639,#61640,#61641,#61642));
#12881=EDGE_LOOP('',(#61643,#61644,#61645,#61646));
#12882=EDGE_LOOP('',(#61647,#61648,#61649,#61650));
#12883=EDGE_LOOP('',(#61651,#61652,#61653,#61654,#61655));
#12884=EDGE_LOOP('',(#61656,#61657,#61658,#61659));
#12885=EDGE_LOOP('',(#61660,#61661,#61662,#61663));
#12886=EDGE_LOOP('',(#61664,#61665,#61666,#61667));
#12887=EDGE_LOOP('',(#61668,#61669,#61670,#61671));
#12888=EDGE_LOOP('',(#61672,#61673,#61674,#61675,#61676,#61677,#61678,#61679,
#61680,#61681,#61682,#61683,#61684,#61685,#61686,#61687));
#12889=EDGE_LOOP('',(#61688,#61689,#61690,#61691));
#12890=EDGE_LOOP('',(#61692,#61693,#61694,#61695));
#12891=EDGE_LOOP('',(#61696,#61697,#61698,#61699));
#12892=EDGE_LOOP('',(#61700,#61701,#61702,#61703));
#12893=EDGE_LOOP('',(#61704,#61705,#61706,#61707,#61708,#61709,#61710,#61711,
#61712,#61713,#61714,#61715));
#12894=EDGE_LOOP('',(#61716,#61717,#61718,#61719));
#12895=EDGE_LOOP('',(#61720,#61721,#61722,#61723));
#12896=EDGE_LOOP('',(#61724,#61725,#61726,#61727));
#12897=EDGE_LOOP('',(#61728,#61729,#61730,#61731));
#12898=EDGE_LOOP('',(#61732,#61733,#61734,#61735));
#12899=EDGE_LOOP('',(#61736,#61737,#61738,#61739));
#12900=EDGE_LOOP('',(#61740,#61741,#61742,#61743));
#12901=EDGE_LOOP('',(#61744,#61745,#61746,#61747));
#12902=EDGE_LOOP('',(#61748,#61749,#61750,#61751));
#12903=EDGE_LOOP('',(#61752,#61753,#61754,#61755));
#12904=EDGE_LOOP('',(#61756,#61757,#61758,#61759));
#12905=EDGE_LOOP('',(#61760,#61761,#61762,#61763,#61764,#61765));
#12906=EDGE_LOOP('',(#61766,#61767,#61768,#61769));
#12907=EDGE_LOOP('',(#61770,#61771,#61772,#61773));
#12908=EDGE_LOOP('',(#61774,#61775));
#12909=EDGE_LOOP('',(#61776,#61777,#61778,#61779,#61780,#61781,#61782,#61783,
#61784,#61785,#61786,#61787,#61788,#61789,#61790,#61791,#61792,#61793,#61794,
#61795,#61796,#61797,#61798,#61799));
#12910=EDGE_LOOP('',(#61800,#61801,#61802,#61803,#61804,#61805,#61806,#61807,
#61808,#61809,#61810,#61811));
#12911=EDGE_LOOP('',(#61812,#61813,#61814,#61815));
#12912=EDGE_LOOP('',(#61816,#61817,#61818,#61819));
#12913=EDGE_LOOP('',(#61820,#61821,#61822,#61823));
#12914=EDGE_LOOP('',(#61824,#61825,#61826,#61827));
#12915=EDGE_LOOP('',(#61828,#61829,#61830,#61831));
#12916=EDGE_LOOP('',(#61832,#61833,#61834,#61835));
#12917=EDGE_LOOP('',(#61836,#61837,#61838,#61839));
#12918=EDGE_LOOP('',(#61840,#61841,#61842,#61843));
#12919=EDGE_LOOP('',(#61844,#61845,#61846,#61847));
#12920=EDGE_LOOP('',(#61848,#61849,#61850,#61851));
#12921=EDGE_LOOP('',(#61852,#61853,#61854,#61855));
#12922=EDGE_LOOP('',(#61856,#61857,#61858,#61859));
#12923=EDGE_LOOP('',(#61860,#61861,#61862,#61863));
#12924=EDGE_LOOP('',(#61864,#61865,#61866,#61867));
#12925=EDGE_LOOP('',(#61868,#61869,#61870,#61871,#61872,#61873,#61874,#61875,
#61876,#61877,#61878,#61879,#61880,#61881,#61882));
#12926=EDGE_LOOP('',(#61883,#61884,#61885,#61886,#61887,#61888,#61889,#61890,
#61891,#61892));
#12927=EDGE_LOOP('',(#61893,#61894,#61895,#61896));
#12928=EDGE_LOOP('',(#61897,#61898,#61899,#61900));
#12929=EDGE_LOOP('',(#61901,#61902,#61903,#61904));
#12930=EDGE_LOOP('',(#61905,#61906,#61907,#61908));
#12931=EDGE_LOOP('',(#61909,#61910,#61911,#61912));
#12932=EDGE_LOOP('',(#61913,#61914,#61915,#61916));
#12933=EDGE_LOOP('',(#61917,#61918,#61919,#61920,#61921,#61922,#61923,#61924));
#12934=EDGE_LOOP('',(#61925,#61926,#61927,#61928));
#12935=EDGE_LOOP('',(#61929,#61930,#61931,#61932));
#12936=EDGE_LOOP('',(#61933,#61934,#61935,#61936));
#12937=EDGE_LOOP('',(#61937,#61938,#61939,#61940));
#12938=EDGE_LOOP('',(#61941,#61942,#61943,#61944));
#12939=EDGE_LOOP('',(#61945,#61946,#61947,#61948));
#12940=EDGE_LOOP('',(#61949,#61950,#61951,#61952));
#12941=EDGE_LOOP('',(#61953,#61954,#61955,#61956));
#12942=EDGE_LOOP('',(#61957));
#12943=EDGE_LOOP('',(#61958));
#12944=EDGE_LOOP('',(#61959,#61960,#61961,#61962));
#12945=EDGE_LOOP('',(#61963,#61964,#61965,#61966));
#12946=EDGE_LOOP('',(#61967,#61968,#61969,#61970,#61971,#61972,#61973,#61974,
#61975,#61976));
#12947=EDGE_LOOP('',(#61977,#61978,#61979,#61980));
#12948=EDGE_LOOP('',(#61981,#61982,#61983,#61984));
#12949=EDGE_LOOP('',(#61985,#61986,#61987,#61988));
#12950=EDGE_LOOP('',(#61989,#61990,#61991,#61992));
#12951=EDGE_LOOP('',(#61993,#61994,#61995,#61996));
#12952=EDGE_LOOP('',(#61997,#61998,#61999,#62000));
#12953=EDGE_LOOP('',(#62001,#62002,#62003,#62004));
#12954=EDGE_LOOP('',(#62005,#62006,#62007,#62008));
#12955=EDGE_LOOP('',(#62009,#62010,#62011,#62012));
#12956=EDGE_LOOP('',(#62013,#62014,#62015,#62016));
#12957=EDGE_LOOP('',(#62017,#62018,#62019,#62020));
#12958=EDGE_LOOP('',(#62021,#62022,#62023,#62024));
#12959=EDGE_LOOP('',(#62025,#62026,#62027,#62028));
#12960=EDGE_LOOP('',(#62029,#62030,#62031,#62032));
#12961=EDGE_LOOP('',(#62033,#62034,#62035,#62036));
#12962=EDGE_LOOP('',(#62037,#62038,#62039,#62040));
#12963=EDGE_LOOP('',(#62041,#62042,#62043,#62044));
#12964=EDGE_LOOP('',(#62045,#62046));
#12965=EDGE_LOOP('',(#62047));
#12966=EDGE_LOOP('',(#62048,#62049,#62050,#62051));
#12967=EDGE_LOOP('',(#62052,#62053,#62054,#62055));
#12968=EDGE_LOOP('',(#62056,#62057));
#12969=EDGE_LOOP('',(#62058));
#12970=EDGE_LOOP('',(#62059,#62060,#62061,#62062));
#12971=EDGE_LOOP('',(#62063,#62064,#62065,#62066));
#12972=EDGE_LOOP('',(#62067,#62068,#62069,#62070,#62071,#62072));
#12973=EDGE_LOOP('',(#62073,#62074,#62075,#62076,#62077,#62078));
#12974=EDGE_LOOP('',(#62079,#62080,#62081,#62082));
#12975=EDGE_LOOP('',(#62083,#62084,#62085,#62086,#62087));
#12976=EDGE_LOOP('',(#62088,#62089,#62090,#62091));
#12977=EDGE_LOOP('',(#62092,#62093,#62094,#62095));
#12978=EDGE_LOOP('',(#62096,#62097,#62098,#62099,#62100));
#12979=EDGE_LOOP('',(#62101,#62102,#62103,#62104));
#12980=EDGE_LOOP('',(#62105,#62106,#62107,#62108,#62109));
#12981=EDGE_LOOP('',(#62110,#62111,#62112,#62113));
#12982=EDGE_LOOP('',(#62114,#62115,#62116,#62117,#62118));
#12983=EDGE_LOOP('',(#62119,#62120,#62121,#62122));
#12984=EDGE_LOOP('',(#62123,#62124,#62125,#62126));
#12985=EDGE_LOOP('',(#62127,#62128,#62129,#62130));
#12986=EDGE_LOOP('',(#62131,#62132,#62133,#62134));
#12987=EDGE_LOOP('',(#62135,#62136,#62137,#62138,#62139,#62140));
#12988=EDGE_LOOP('',(#62141,#62142,#62143,#62144));
#12989=EDGE_LOOP('',(#62145,#62146,#62147,#62148));
#12990=EDGE_LOOP('',(#62149,#62150,#62151,#62152));
#12991=EDGE_LOOP('',(#62153,#62154,#62155,#62156,#62157,#62158));
#12992=EDGE_LOOP('',(#62159,#62160,#62161,#62162));
#12993=EDGE_LOOP('',(#62163,#62164,#62165,#62166));
#12994=EDGE_LOOP('',(#62167,#62168,#62169,#62170,#62171,#62172));
#12995=EDGE_LOOP('',(#62173,#62174,#62175,#62176));
#12996=EDGE_LOOP('',(#62177,#62178,#62179,#62180));
#12997=EDGE_LOOP('',(#62181,#62182,#62183,#62184));
#12998=EDGE_LOOP('',(#62185,#62186,#62187,#62188));
#12999=EDGE_LOOP('',(#62189,#62190,#62191,#62192));
#13000=EDGE_LOOP('',(#62193,#62194,#62195,#62196,#62197,#62198));
#13001=EDGE_LOOP('',(#62199));
#13002=EDGE_LOOP('',(#62200));
#13003=EDGE_LOOP('',(#62201,#62202,#62203,#62204));
#13004=EDGE_LOOP('',(#62205,#62206,#62207,#62208,#62209));
#13005=EDGE_LOOP('',(#62210,#62211,#62212,#62213));
#13006=EDGE_LOOP('',(#62214,#62215,#62216,#62217));
#13007=EDGE_LOOP('',(#62218,#62219,#62220,#62221,#62222,#62223,#62224,#62225));
#13008=EDGE_LOOP('',(#62226,#62227,#62228,#62229,#62230,#62231));
#13009=EDGE_LOOP('',(#62232,#62233,#62234,#62235,#62236,#62237));
#13010=EDGE_LOOP('',(#62238,#62239,#62240,#62241));
#13011=EDGE_LOOP('',(#62242,#62243,#62244,#62245));
#13012=EDGE_LOOP('',(#62246,#62247,#62248,#62249));
#13013=EDGE_LOOP('',(#62250,#62251,#62252,#62253,#62254,#62255));
#13014=EDGE_LOOP('',(#62256,#62257,#62258,#62259));
#13015=EDGE_LOOP('',(#62260,#62261,#62262,#62263,#62264));
#13016=EDGE_LOOP('',(#62265,#62266,#62267,#62268));
#13017=EDGE_LOOP('',(#62269,#62270,#62271,#62272,#62273,#62274,#62275,#62276,
#62277,#62278,#62279,#62280));
#13018=EDGE_LOOP('',(#62281,#62282,#62283,#62284));
#13019=EDGE_LOOP('',(#62285,#62286,#62287,#62288));
#13020=EDGE_LOOP('',(#62289,#62290,#62291,#62292,#62293,#62294,#62295,#62296,
#62297,#62298));
#13021=EDGE_LOOP('',(#62299,#62300,#62301,#62302));
#13022=EDGE_LOOP('',(#62303,#62304,#62305,#62306,#62307,#62308,#62309,#62310,
#62311,#62312));
#13023=EDGE_LOOP('',(#62313,#62314,#62315,#62316));
#13024=EDGE_LOOP('',(#62317,#62318,#62319,#62320));
#13025=EDGE_LOOP('',(#62321,#62322,#62323,#62324));
#13026=EDGE_LOOP('',(#62325,#62326,#62327,#62328,#62329,#62330,#62331,#62332,
#62333,#62334,#62335,#62336,#62337,#62338,#62339,#62340,#62341,#62342,#62343,
#62344,#62345,#62346,#62347,#62348,#62349,#62350,#62351,#62352,#62353,#62354,
#62355,#62356,#62357,#62358,#62359,#62360,#62361,#62362,#62363,#62364,#62365,
#62366,#62367,#62368,#62369,#62370,#62371));
#13027=EDGE_LOOP('',(#62372));
#13028=EDGE_LOOP('',(#62373,#62374,#62375,#62376,#62377,#62378,#62379,#62380,
#62381,#62382,#62383,#62384,#62385,#62386));
#13029=EDGE_LOOP('',(#62387));
#13030=EDGE_LOOP('',(#62388));
#13031=EDGE_LOOP('',(#62389));
#13032=EDGE_LOOP('',(#62390,#62391,#62392,#62393));
#13033=EDGE_LOOP('',(#62394,#62395,#62396,#62397));
#13034=EDGE_LOOP('',(#62398,#62399,#62400,#62401,#62402,#62403,#62404));
#13035=EDGE_LOOP('',(#62405,#62406,#62407,#62408,#62409));
#13036=EDGE_LOOP('',(#62410,#62411,#62412,#62413));
#13037=EDGE_LOOP('',(#62414,#62415,#62416,#62417,#62418));
#13038=EDGE_LOOP('',(#62419,#62420,#62421,#62422,#62423));
#13039=EDGE_LOOP('',(#62424,#62425,#62426,#62427));
#13040=EDGE_LOOP('',(#62428,#62429,#62430,#62431,#62432,#62433,#62434));
#13041=EDGE_LOOP('',(#62435,#62436,#62437,#62438));
#13042=EDGE_LOOP('',(#62439,#62440,#62441,#62442,#62443,#62444));
#13043=EDGE_LOOP('',(#62445,#62446,#62447,#62448));
#13044=EDGE_LOOP('',(#62449));
#13045=EDGE_LOOP('',(#62450));
#13046=EDGE_LOOP('',(#62451,#62452,#62453,#62454));
#13047=EDGE_LOOP('',(#62455,#62456,#62457,#62458));
#13048=EDGE_LOOP('',(#62459,#62460,#62461,#62462));
#13049=EDGE_LOOP('',(#62463,#62464,#62465,#62466));
#13050=EDGE_LOOP('',(#62467,#62468,#62469,#62470));
#13051=EDGE_LOOP('',(#62471,#62472,#62473,#62474));
#13052=EDGE_LOOP('',(#62475,#62476,#62477,#62478));
#13053=EDGE_LOOP('',(#62479,#62480,#62481,#62482));
#13054=EDGE_LOOP('',(#62483,#62484,#62485,#62486));
#13055=EDGE_LOOP('',(#62487,#62488,#62489,#62490));
#13056=EDGE_LOOP('',(#62491,#62492,#62493,#62494));
#13057=EDGE_LOOP('',(#62495,#62496,#62497,#62498));
#13058=EDGE_LOOP('',(#62499,#62500,#62501,#62502));
#13059=EDGE_LOOP('',(#62503,#62504,#62505,#62506));
#13060=EDGE_LOOP('',(#62507,#62508,#62509,#62510,#62511,#62512,#62513));
#13061=EDGE_LOOP('',(#62514,#62515,#62516,#62517));
#13062=EDGE_LOOP('',(#62518,#62519,#62520,#62521));
#13063=EDGE_LOOP('',(#62522,#62523,#62524,#62525,#62526,#62527));
#13064=EDGE_LOOP('',(#62528,#62529,#62530,#62531));
#13065=EDGE_LOOP('',(#62532,#62533,#62534));
#13066=EDGE_LOOP('',(#62535,#62536,#62537,#62538,#62539));
#13067=EDGE_LOOP('',(#62540,#62541,#62542,#62543));
#13068=EDGE_LOOP('',(#62544));
#13069=EDGE_LOOP('',(#62545));
#13070=EDGE_LOOP('',(#62546));
#13071=EDGE_LOOP('',(#62547));
#13072=EDGE_LOOP('',(#62548,#62549,#62550,#62551));
#13073=EDGE_LOOP('',(#62552,#62553,#62554,#62555));
#13074=EDGE_LOOP('',(#62556));
#13075=EDGE_LOOP('',(#62557));
#13076=EDGE_LOOP('',(#62558,#62559,#62560,#62561,#62562));
#13077=EDGE_LOOP('',(#62563,#62564,#62565,#62566));
#13078=EDGE_LOOP('',(#62567,#62568,#62569,#62570));
#13079=EDGE_LOOP('',(#62571));
#13080=EDGE_LOOP('',(#62572));
#13081=EDGE_LOOP('',(#62573,#62574,#62575,#62576));
#13082=EDGE_LOOP('',(#62577));
#13083=EDGE_LOOP('',(#62578));
#13084=EDGE_LOOP('',(#62579,#62580,#62581,#62582,#62583));
#13085=EDGE_LOOP('',(#62584,#62585,#62586,#62587));
#13086=EDGE_LOOP('',(#62588,#62589,#62590,#62591,#62592,#62593,#62594));
#13087=EDGE_LOOP('',(#62595,#62596,#62597,#62598,#62599,#62600));
#13088=EDGE_LOOP('',(#62601));
#13089=EDGE_LOOP('',(#62602));
#13090=EDGE_LOOP('',(#62603,#62604,#62605,#62606));
#13091=EDGE_LOOP('',(#62607,#62608,#62609,#62610,#62611,#62612,#62613,#62614));
#13092=EDGE_LOOP('',(#62615,#62616,#62617,#62618,#62619,#62620,#62621,#62622));
#13093=EDGE_LOOP('',(#62623,#62624,#62625));
#13094=EDGE_LOOP('',(#62626,#62627,#62628,#62629));
#13095=EDGE_LOOP('',(#62630,#62631,#62632,#62633));
#13096=EDGE_LOOP('',(#62634,#62635,#62636,#62637));
#13097=EDGE_LOOP('',(#62638,#62639,#62640,#62641,#62642));
#13098=EDGE_LOOP('',(#62643,#62644,#62645,#62646));
#13099=EDGE_LOOP('',(#62647,#62648,#62649,#62650));
#13100=EDGE_LOOP('',(#62651,#62652,#62653,#62654));
#13101=EDGE_LOOP('',(#62655,#62656,#62657,#62658));
#13102=EDGE_LOOP('',(#62659,#62660,#62661,#62662,#62663,#62664,#62665,#62666,
#62667));
#13103=EDGE_LOOP('',(#62668,#62669,#62670,#62671));
#13104=EDGE_LOOP('',(#62672,#62673,#62674));
#13105=EDGE_LOOP('',(#62675,#62676,#62677,#62678));
#13106=EDGE_LOOP('',(#62679,#62680,#62681));
#13107=EDGE_LOOP('',(#62682,#62683,#62684,#62685));
#13108=EDGE_LOOP('',(#62686,#62687,#62688,#62689));
#13109=EDGE_LOOP('',(#62690,#62691,#62692,#62693));
#13110=EDGE_LOOP('',(#62694,#62695,#62696,#62697));
#13111=EDGE_LOOP('',(#62698,#62699,#62700,#62701,#62702,#62703,#62704,#62705,
#62706));
#13112=EDGE_LOOP('',(#62707,#62708,#62709,#62710));
#13113=EDGE_LOOP('',(#62711,#62712,#62713,#62714,#62715,#62716,#62717,#62718));
#13114=EDGE_LOOP('',(#62719,#62720,#62721,#62722,#62723,#62724,#62725,#62726,
#62727,#62728,#62729,#62730,#62731));
#13115=EDGE_LOOP('',(#62732,#62733,#62734,#62735));
#13116=EDGE_LOOP('',(#62736,#62737,#62738,#62739));
#13117=EDGE_LOOP('',(#62740,#62741,#62742,#62743));
#13118=EDGE_LOOP('',(#62744,#62745,#62746,#62747));
#13119=EDGE_LOOP('',(#62748,#62749,#62750,#62751));
#13120=EDGE_LOOP('',(#62752,#62753,#62754,#62755));
#13121=EDGE_LOOP('',(#62756,#62757,#62758,#62759));
#13122=EDGE_LOOP('',(#62760,#62761,#62762,#62763,#62764,#62765));
#13123=EDGE_LOOP('',(#62766));
#13124=EDGE_LOOP('',(#62767,#62768,#62769,#62770));
#13125=EDGE_LOOP('',(#62771,#62772,#62773,#62774));
#13126=EDGE_LOOP('',(#62775,#62776,#62777,#62778));
#13127=EDGE_LOOP('',(#62779,#62780,#62781,#62782));
#13128=EDGE_LOOP('',(#62783,#62784,#62785,#62786,#62787,#62788,#62789));
#13129=EDGE_LOOP('',(#62790,#62791,#62792,#62793,#62794,#62795,#62796,#62797,
#62798,#62799,#62800,#62801,#62802,#62803,#62804,#62805,#62806,#62807,#62808,
#62809,#62810,#62811,#62812));
#13130=EDGE_LOOP('',(#62813));
#13131=EDGE_LOOP('',(#62814,#62815,#62816,#62817));
#13132=EDGE_LOOP('',(#62818,#62819,#62820,#62821));
#13133=EDGE_LOOP('',(#62822,#62823,#62824,#62825));
#13134=EDGE_LOOP('',(#62826,#62827,#62828,#62829));
#13135=EDGE_LOOP('',(#62830,#62831,#62832,#62833));
#13136=EDGE_LOOP('',(#62834,#62835,#62836,#62837));
#13137=EDGE_LOOP('',(#62838,#62839,#62840,#62841,#62842,#62843,#62844,#62845));
#13138=EDGE_LOOP('',(#62846,#62847,#62848,#62849));
#13139=EDGE_LOOP('',(#62850,#62851,#62852,#62853));
#13140=EDGE_LOOP('',(#62854,#62855,#62856,#62857));
#13141=EDGE_LOOP('',(#62858,#62859,#62860,#62861,#62862,#62863,#62864,#62865,
#62866,#62867,#62868,#62869,#62870,#62871,#62872,#62873,#62874,#62875,#62876));
#13142=EDGE_LOOP('',(#62877,#62878,#62879,#62880));
#13143=EDGE_LOOP('',(#62881,#62882,#62883,#62884));
#13144=EDGE_LOOP('',(#62885,#62886,#62887,#62888));
#13145=EDGE_LOOP('',(#62889,#62890,#62891,#62892));
#13146=EDGE_LOOP('',(#62893,#62894,#62895,#62896,#62897,#62898,#62899,#62900,
#62901,#62902,#62903,#62904,#62905,#62906,#62907,#62908,#62909,#62910,#62911,
#62912,#62913,#62914,#62915,#62916,#62917,#62918,#62919,#62920,#62921,#62922,
#62923,#62924,#62925,#62926,#62927,#62928));
#13147=EDGE_LOOP('',(#62929));
#13148=EDGE_LOOP('',(#62930,#62931,#62932,#62933));
#13149=EDGE_LOOP('',(#62934,#62935,#62936,#62937,#62938,#62939,#62940,#62941));
#13150=EDGE_LOOP('',(#62942,#62943,#62944,#62945));
#13151=EDGE_LOOP('',(#62946,#62947,#62948,#62949,#62950));
#13152=EDGE_LOOP('',(#62951,#62952,#62953,#62954,#62955,#62956,#62957,#62958,
#62959,#62960,#62961,#62962,#62963,#62964,#62965,#62966,#62967,#62968));
#13153=EDGE_LOOP('',(#62969,#62970,#62971,#62972,#62973,#62974,#62975));
#13154=EDGE_LOOP('',(#62976,#62977,#62978,#62979));
#13155=EDGE_LOOP('',(#62980,#62981,#62982,#62983,#62984,#62985,#62986,#62987,
#62988,#62989,#62990,#62991,#62992,#62993,#62994,#62995,#62996,#62997,#62998,
#62999,#63000,#63001,#63002,#63003,#63004,#63005,#63006,#63007,#63008,#63009,
#63010,#63011,#63012,#63013,#63014,#63015,#63016,#63017,#63018,#63019,#63020,
#63021,#63022,#63023,#63024,#63025,#63026,#63027,#63028,#63029));
#13156=EDGE_LOOP('',(#63030,#63031,#63032,#63033));
#13157=EDGE_LOOP('',(#63034,#63035,#63036,#63037,#63038,#63039,#63040,#63041,
#63042));
#13158=EDGE_LOOP('',(#63043,#63044,#63045,#63046,#63047));
#13159=EDGE_LOOP('',(#63048,#63049,#63050,#63051));
#13160=EDGE_LOOP('',(#63052,#63053,#63054,#63055));
#13161=EDGE_LOOP('',(#63056,#63057,#63058,#63059,#63060,#63061));
#13162=EDGE_LOOP('',(#63062,#63063,#63064,#63065));
#13163=EDGE_LOOP('',(#63066,#63067,#63068,#63069));
#13164=EDGE_LOOP('',(#63070,#63071,#63072,#63073,#63074));
#13165=EDGE_LOOP('',(#63075,#63076,#63077,#63078));
#13166=EDGE_LOOP('',(#63079,#63080,#63081,#63082));
#13167=EDGE_LOOP('',(#63083,#63084,#63085,#63086));
#13168=EDGE_LOOP('',(#63087,#63088,#63089,#63090));
#13169=EDGE_LOOP('',(#63091,#63092,#63093,#63094));
#13170=EDGE_LOOP('',(#63095,#63096,#63097,#63098));
#13171=EDGE_LOOP('',(#63099,#63100,#63101,#63102,#63103));
#13172=EDGE_LOOP('',(#63104,#63105,#63106,#63107,#63108));
#13173=EDGE_LOOP('',(#63109,#63110,#63111,#63112,#63113));
#13174=EDGE_LOOP('',(#63114,#63115,#63116,#63117,#63118));
#13175=EDGE_LOOP('',(#63119,#63120,#63121,#63122));
#13176=EDGE_LOOP('',(#63123,#63124,#63125,#63126));
#13177=EDGE_LOOP('',(#63127,#63128,#63129,#63130,#63131,#63132));
#13178=EDGE_LOOP('',(#63133,#63134,#63135,#63136));
#13179=EDGE_LOOP('',(#63137,#63138,#63139,#63140));
#13180=EDGE_LOOP('',(#63141,#63142,#63143,#63144));
#13181=EDGE_LOOP('',(#63145,#63146,#63147,#63148));
#13182=EDGE_LOOP('',(#63149,#63150,#63151,#63152));
#13183=EDGE_LOOP('',(#63153,#63154,#63155,#63156));
#13184=EDGE_LOOP('',(#63157,#63158,#63159,#63160));
#13185=EDGE_LOOP('',(#63161,#63162,#63163,#63164));
#13186=EDGE_LOOP('',(#63165,#63166,#63167,#63168));
#13187=EDGE_LOOP('',(#63169,#63170,#63171,#63172,#63173,#63174,#63175,#63176,
#63177,#63178,#63179,#63180,#63181,#63182,#63183,#63184,#63185,#63186,#63187,
#63188,#63189,#63190,#63191,#63192));
#13188=EDGE_LOOP('',(#63193,#63194,#63195,#63196));
#13189=EDGE_LOOP('',(#63197,#63198,#63199,#63200));
#13190=EDGE_LOOP('',(#63201,#63202,#63203,#63204));
#13191=EDGE_LOOP('',(#63205,#63206,#63207,#63208));
#13192=EDGE_LOOP('',(#63209,#63210,#63211,#63212));
#13193=EDGE_LOOP('',(#63213,#63214,#63215,#63216));
#13194=EDGE_LOOP('',(#63217,#63218,#63219,#63220,#63221,#63222,#63223));
#13195=EDGE_LOOP('',(#63224,#63225,#63226,#63227));
#13196=EDGE_LOOP('',(#63228,#63229,#63230,#63231));
#13197=EDGE_LOOP('',(#63232,#63233,#63234,#63235,#63236,#63237,#63238,#63239,
#63240,#63241,#63242));
#13198=EDGE_LOOP('',(#63243,#63244,#63245,#63246,#63247,#63248,#63249,#63250));
#13199=EDGE_LOOP('',(#63251));
#13200=EDGE_LOOP('',(#63252,#63253,#63254,#63255,#63256,#63257));
#13201=EDGE_LOOP('',(#63258,#63259,#63260,#63261));
#13202=EDGE_LOOP('',(#63262,#63263,#63264,#63265,#63266,#63267,#63268,#63269));
#13203=EDGE_LOOP('',(#63270,#63271,#63272,#63273,#63274,#63275,#63276,#63277,
#63278));
#13204=EDGE_LOOP('',(#63279,#63280,#63281,#63282,#63283));
#13205=EDGE_LOOP('',(#63284,#63285,#63286,#63287,#63288));
#13206=EDGE_LOOP('',(#63289,#63290,#63291,#63292,#63293,#63294));
#13207=EDGE_LOOP('',(#63295,#63296,#63297,#63298));
#13208=EDGE_LOOP('',(#63299,#63300,#63301,#63302,#63303,#63304));
#13209=EDGE_LOOP('',(#63305,#63306,#63307,#63308));
#13210=EDGE_LOOP('',(#63309,#63310,#63311,#63312,#63313,#63314));
#13211=EDGE_LOOP('',(#63315,#63316,#63317,#63318,#63319,#63320,#63321,#63322,
#63323));
#13212=EDGE_LOOP('',(#63324,#63325,#63326,#63327,#63328,#63329,#63330,#63331,
#63332,#63333,#63334,#63335,#63336,#63337,#63338,#63339,#63340,#63341,#63342,
#63343,#63344,#63345,#63346,#63347,#63348,#63349,#63350,#63351,#63352,#63353,
#63354,#63355,#63356,#63357,#63358,#63359,#63360,#63361,#63362,#63363,#63364,
#63365,#63366,#63367,#63368,#63369));
#13213=EDGE_LOOP('',(#63370));
#13214=EDGE_LOOP('',(#63371));
#13215=EDGE_LOOP('',(#63372));
#13216=EDGE_LOOP('',(#63373,#63374,#63375,#63376));
#13217=EDGE_LOOP('',(#63377,#63378,#63379,#63380,#63381,#63382,#63383,#63384,
#63385,#63386,#63387,#63388,#63389,#63390,#63391,#63392,#63393,#63394));
#13218=EDGE_LOOP('',(#63395,#63396,#63397,#63398));
#13219=EDGE_LOOP('',(#63399,#63400,#63401,#63402,#63403,#63404,#63405,#63406));
#13220=EDGE_LOOP('',(#63407,#63408,#63409,#63410,#63411,#63412,#63413,#63414,
#63415,#63416,#63417,#63418,#63419,#63420,#63421,#63422,#63423,#63424,#63425));
#13221=EDGE_LOOP('',(#63426,#63427,#63428,#63429));
#13222=EDGE_LOOP('',(#63430,#63431,#63432,#63433));
#13223=EDGE_LOOP('',(#63434,#63435,#63436,#63437,#63438,#63439,#63440,#63441,
#63442,#63443,#63444,#63445,#63446,#63447,#63448,#63449,#63450));
#13224=EDGE_LOOP('',(#63451,#63452,#63453,#63454,#63455,#63456,#63457,#63458,
#63459,#63460,#63461,#63462,#63463,#63464,#63465,#63466,#63467));
#13225=EDGE_LOOP('',(#63468,#63469,#63470,#63471));
#13226=EDGE_LOOP('',(#63472,#63473,#63474,#63475,#63476,#63477,#63478,#63479,
#63480,#63481,#63482,#63483,#63484,#63485,#63486,#63487,#63488));
#13227=EDGE_LOOP('',(#63489,#63490,#63491,#63492));
#13228=EDGE_LOOP('',(#63493,#63494,#63495,#63496,#63497,#63498,#63499,#63500,
#63501,#63502,#63503,#63504,#63505,#63506));
#13229=EDGE_LOOP('',(#63507,#63508,#63509,#63510,#63511,#63512,#63513,#63514));
#13230=EDGE_LOOP('',(#63515,#63516,#63517,#63518));
#13231=EDGE_LOOP('',(#63519,#63520,#63521,#63522));
#13232=EDGE_LOOP('',(#63523,#63524,#63525,#63526));
#13233=EDGE_LOOP('',(#63527,#63528,#63529,#63530,#63531));
#13234=EDGE_LOOP('',(#63532,#63533,#63534,#63535));
#13235=EDGE_LOOP('',(#63536,#63537,#63538,#63539));
#13236=EDGE_LOOP('',(#63540,#63541,#63542,#63543));
#13237=EDGE_LOOP('',(#63544,#63545,#63546,#63547));
#13238=EDGE_LOOP('',(#63548,#63549,#63550,#63551));
#13239=EDGE_LOOP('',(#63552,#63553,#63554,#63555));
#13240=EDGE_LOOP('',(#63556,#63557,#63558,#63559,#63560,#63561,#63562,#63563,
#63564,#63565));
#13241=EDGE_LOOP('',(#63566,#63567,#63568,#63569));
#13242=EDGE_LOOP('',(#63570,#63571,#63572,#63573));
#13243=EDGE_LOOP('',(#63574,#63575,#63576,#63577,#63578,#63579,#63580,#63581,
#63582,#63583,#63584,#63585,#63586,#63587,#63588,#63589,#63590));
#13244=EDGE_LOOP('',(#63591,#63592,#63593,#63594));
#13245=EDGE_LOOP('',(#63595,#63596,#63597,#63598));
#13246=EDGE_LOOP('',(#63599,#63600,#63601,#63602,#63603,#63604));
#13247=EDGE_LOOP('',(#63605,#63606,#63607,#63608,#63609,#63610));
#13248=EDGE_LOOP('',(#63611,#63612,#63613,#63614));
#13249=EDGE_LOOP('',(#63615,#63616,#63617,#63618));
#13250=EDGE_LOOP('',(#63619,#63620,#63621,#63622));
#13251=EDGE_LOOP('',(#63623,#63624,#63625,#63626));
#13252=EDGE_LOOP('',(#63627,#63628,#63629,#63630));
#13253=EDGE_LOOP('',(#63631,#63632,#63633,#63634));
#13254=EDGE_LOOP('',(#63635,#63636,#63637,#63638));
#13255=EDGE_LOOP('',(#63639,#63640,#63641,#63642));
#13256=EDGE_LOOP('',(#63643,#63644,#63645,#63646));
#13257=EDGE_LOOP('',(#63647,#63648,#63649,#63650));
#13258=EDGE_LOOP('',(#63651,#63652,#63653,#63654));
#13259=EDGE_LOOP('',(#63655,#63656,#63657,#63658));
#13260=EDGE_LOOP('',(#63659,#63660,#63661,#63662));
#13261=EDGE_LOOP('',(#63663,#63664,#63665,#63666,#63667,#63668));
#13262=EDGE_LOOP('',(#63669,#63670,#63671,#63672,#63673,#63674));
#13263=EDGE_LOOP('',(#63675,#63676,#63677,#63678));
#13264=EDGE_LOOP('',(#63679));
#13265=EDGE_LOOP('',(#63680,#63681,#63682,#63683));
#13266=EDGE_LOOP('',(#63684));
#13267=EDGE_LOOP('',(#63685,#63686,#63687,#63688));
#13268=EDGE_LOOP('',(#63689,#63690,#63691,#63692));
#13269=EDGE_LOOP('',(#63693,#63694,#63695,#63696));
#13270=EDGE_LOOP('',(#63697));
#13271=EDGE_LOOP('',(#63698,#63699,#63700,#63701));
#13272=EDGE_LOOP('',(#63702));
#13273=EDGE_LOOP('',(#63703,#63704,#63705,#63706,#63707));
#13274=EDGE_LOOP('',(#63708,#63709,#63710,#63711,#63712,#63713,#63714));
#13275=EDGE_LOOP('',(#63715,#63716,#63717,#63718));
#13276=EDGE_LOOP('',(#63719,#63720,#63721,#63722,#63723,#63724,#63725));
#13277=EDGE_LOOP('',(#63726));
#13278=EDGE_LOOP('',(#63727));
#13279=EDGE_LOOP('',(#63728,#63729,#63730));
#13280=EDGE_LOOP('',(#63731));
#13281=EDGE_LOOP('',(#63732));
#13282=EDGE_LOOP('',(#63733,#63734,#63735));
#13283=EDGE_LOOP('',(#63736,#63737,#63738,#63739));
#13284=EDGE_LOOP('',(#63740,#63741,#63742,#63743));
#13285=EDGE_LOOP('',(#63744,#63745,#63746,#63747,#63748));
#13286=EDGE_LOOP('',(#63749,#63750,#63751,#63752,#63753));
#13287=EDGE_LOOP('',(#63754,#63755,#63756,#63757,#63758,#63759,#63760));
#13288=EDGE_LOOP('',(#63761,#63762,#63763,#63764));
#13289=EDGE_LOOP('',(#63765,#63766,#63767,#63768,#63769,#63770,#63771));
#13290=EDGE_LOOP('',(#63772,#63773,#63774,#63775));
#13291=EDGE_LOOP('',(#63776,#63777,#63778,#63779));
#13292=EDGE_LOOP('',(#63780,#63781,#63782,#63783));
#13293=EDGE_LOOP('',(#63784,#63785,#63786,#63787));
#13294=EDGE_LOOP('',(#63788,#63789,#63790,#63791,#63792,#63793,#63794,#63795,
#63796,#63797,#63798,#63799,#63800,#63801,#63802,#63803,#63804,#63805));
#13295=EDGE_LOOP('',(#63806,#63807,#63808,#63809));
#13296=EDGE_LOOP('',(#63810,#63811,#63812,#63813));
#13297=EDGE_LOOP('',(#63814));
#13298=EDGE_LOOP('',(#63815,#63816,#63817,#63818));
#13299=EDGE_LOOP('',(#63819));
#13300=EDGE_LOOP('',(#63820,#63821,#63822,#63823));
#13301=EDGE_LOOP('',(#63824,#63825,#63826,#63827));
#13302=EDGE_LOOP('',(#63828));
#13303=EDGE_LOOP('',(#63829,#63830,#63831,#63832));
#13304=EDGE_LOOP('',(#63833));
#13305=EDGE_LOOP('',(#63834,#63835,#63836,#63837));
#13306=EDGE_LOOP('',(#63838,#63839,#63840,#63841));
#13307=EDGE_LOOP('',(#63842,#63843,#63844,#63845));
#13308=EDGE_LOOP('',(#63846,#63847,#63848,#63849));
#13309=EDGE_LOOP('',(#63850,#63851,#63852,#63853));
#13310=EDGE_LOOP('',(#63854,#63855,#63856,#63857));
#13311=EDGE_LOOP('',(#63858,#63859,#63860,#63861));
#13312=EDGE_LOOP('',(#63862,#63863,#63864,#63865));
#13313=EDGE_LOOP('',(#63866,#63867,#63868,#63869));
#13314=EDGE_LOOP('',(#63870,#63871,#63872,#63873));
#13315=EDGE_LOOP('',(#63874,#63875,#63876,#63877));
#13316=EDGE_LOOP('',(#63878,#63879,#63880,#63881));
#13317=EDGE_LOOP('',(#63882,#63883,#63884,#63885));
#13318=EDGE_LOOP('',(#63886,#63887,#63888,#63889));
#13319=EDGE_LOOP('',(#63890,#63891,#63892,#63893));
#13320=EDGE_LOOP('',(#63894,#63895,#63896,#63897));
#13321=EDGE_LOOP('',(#63898,#63899,#63900,#63901));
#13322=EDGE_LOOP('',(#63902,#63903,#63904,#63905));
#13323=EDGE_LOOP('',(#63906,#63907,#63908,#63909));
#13324=EDGE_LOOP('',(#63910,#63911,#63912,#63913));
#13325=EDGE_LOOP('',(#63914,#63915,#63916,#63917));
#13326=EDGE_LOOP('',(#63918,#63919,#63920,#63921));
#13327=EDGE_LOOP('',(#63922,#63923,#63924,#63925));
#13328=EDGE_LOOP('',(#63926,#63927,#63928,#63929));
#13329=EDGE_LOOP('',(#63930,#63931,#63932,#63933));
#13330=EDGE_LOOP('',(#63934,#63935,#63936,#63937));
#13331=EDGE_LOOP('',(#63938,#63939,#63940,#63941));
#13332=EDGE_LOOP('',(#63942,#63943,#63944,#63945));
#13333=EDGE_LOOP('',(#63946,#63947,#63948,#63949));
#13334=EDGE_LOOP('',(#63950,#63951,#63952,#63953));
#13335=EDGE_LOOP('',(#63954,#63955,#63956,#63957));
#13336=EDGE_LOOP('',(#63958,#63959,#63960,#63961));
#13337=EDGE_LOOP('',(#63962,#63963,#63964,#63965));
#13338=EDGE_LOOP('',(#63966,#63967,#63968,#63969));
#13339=EDGE_LOOP('',(#63970,#63971,#63972,#63973));
#13340=EDGE_LOOP('',(#63974,#63975,#63976,#63977));
#13341=EDGE_LOOP('',(#63978,#63979,#63980,#63981));
#13342=EDGE_LOOP('',(#63982,#63983,#63984,#63985));
#13343=EDGE_LOOP('',(#63986,#63987,#63988,#63989));
#13344=EDGE_LOOP('',(#63990,#63991,#63992,#63993));
#13345=EDGE_LOOP('',(#63994,#63995,#63996,#63997));
#13346=EDGE_LOOP('',(#63998,#63999,#64000,#64001));
#13347=EDGE_LOOP('',(#64002,#64003,#64004,#64005));
#13348=EDGE_LOOP('',(#64006,#64007,#64008,#64009));
#13349=EDGE_LOOP('',(#64010,#64011,#64012,#64013));
#13350=EDGE_LOOP('',(#64014,#64015,#64016,#64017));
#13351=EDGE_LOOP('',(#64018,#64019,#64020,#64021));
#13352=EDGE_LOOP('',(#64022,#64023,#64024,#64025));
#13353=EDGE_LOOP('',(#64026,#64027,#64028,#64029));
#13354=EDGE_LOOP('',(#64030,#64031,#64032,#64033));
#13355=EDGE_LOOP('',(#64034,#64035,#64036,#64037));
#13356=EDGE_LOOP('',(#64038,#64039,#64040,#64041));
#13357=EDGE_LOOP('',(#64042,#64043,#64044,#64045));
#13358=EDGE_LOOP('',(#64046,#64047,#64048,#64049));
#13359=EDGE_LOOP('',(#64050,#64051,#64052,#64053));
#13360=EDGE_LOOP('',(#64054,#64055,#64056,#64057));
#13361=EDGE_LOOP('',(#64058,#64059,#64060,#64061));
#13362=EDGE_LOOP('',(#64062,#64063,#64064,#64065));
#13363=EDGE_LOOP('',(#64066,#64067,#64068,#64069));
#13364=EDGE_LOOP('',(#64070,#64071,#64072,#64073));
#13365=EDGE_LOOP('',(#64074,#64075,#64076,#64077));
#13366=EDGE_LOOP('',(#64078,#64079,#64080,#64081));
#13367=EDGE_LOOP('',(#64082,#64083,#64084,#64085));
#13368=EDGE_LOOP('',(#64086,#64087,#64088,#64089));
#13369=EDGE_LOOP('',(#64090,#64091,#64092,#64093));
#13370=EDGE_LOOP('',(#64094,#64095,#64096,#64097));
#13371=EDGE_LOOP('',(#64098,#64099,#64100,#64101));
#13372=EDGE_LOOP('',(#64102,#64103,#64104,#64105));
#13373=EDGE_LOOP('',(#64106,#64107,#64108,#64109));
#13374=EDGE_LOOP('',(#64110,#64111,#64112,#64113));
#13375=EDGE_LOOP('',(#64114,#64115,#64116,#64117,#64118));
#13376=EDGE_LOOP('',(#64119,#64120,#64121,#64122,#64123));
#13377=EDGE_LOOP('',(#64124,#64125,#64126,#64127,#64128));
#13378=EDGE_LOOP('',(#64129,#64130,#64131,#64132,#64133));
#13379=EDGE_LOOP('',(#64134,#64135,#64136,#64137));
#13380=EDGE_LOOP('',(#64138,#64139,#64140,#64141));
#13381=EDGE_LOOP('',(#64142,#64143,#64144,#64145,#64146));
#13382=EDGE_LOOP('',(#64147,#64148,#64149,#64150));
#13383=EDGE_LOOP('',(#64151,#64152,#64153,#64154,#64155));
#13384=EDGE_LOOP('',(#64156,#64157,#64158,#64159,#64160));
#13385=EDGE_LOOP('',(#64161,#64162,#64163,#64164,#64165,#64166,#64167,#64168,
#64169,#64170,#64171,#64172,#64173,#64174,#64175,#64176,#64177,#64178,#64179,
#64180,#64181,#64182,#64183,#64184,#64185,#64186,#64187,#64188,#64189,#64190,
#64191,#64192,#64193,#64194,#64195,#64196,#64197,#64198,#64199,#64200,#64201,
#64202,#64203,#64204,#64205,#64206,#64207,#64208,#64209,#64210,#64211,#64212,
#64213,#64214,#64215,#64216,#64217,#64218,#64219,#64220,#64221,#64222,#64223,
#64224,#64225,#64226,#64227,#64228,#64229,#64230,#64231,#64232,#64233,#64234,
#64235,#64236,#64237,#64238,#64239,#64240,#64241,#64242,#64243,#64244,#64245,
#64246,#64247,#64248,#64249,#64250,#64251,#64252,#64253,#64254,#64255,#64256,
#64257,#64258,#64259,#64260,#64261,#64262,#64263,#64264,#64265,#64266,#64267,
#64268,#64269,#64270,#64271,#64272,#64273,#64274,#64275,#64276,#64277,#64278,
#64279,#64280,#64281,#64282,#64283,#64284,#64285,#64286,#64287,#64288,#64289,
#64290,#64291,#64292,#64293,#64294,#64295,#64296,#64297,#64298,#64299,#64300,
#64301,#64302,#64303,#64304,#64305,#64306,#64307,#64308,#64309,#64310,#64311,
#64312,#64313,#64314,#64315,#64316,#64317,#64318,#64319,#64320,#64321,#64322,
#64323,#64324,#64325,#64326,#64327,#64328,#64329,#64330,#64331,#64332,#64333,
#64334,#64335,#64336,#64337,#64338,#64339,#64340,#64341,#64342,#64343,#64344,
#64345,#64346,#64347,#64348,#64349,#64350,#64351,#64352,#64353,#64354,#64355,
#64356,#64357,#64358,#64359,#64360,#64361,#64362,#64363,#64364,#64365,#64366,
#64367,#64368,#64369,#64370,#64371,#64372,#64373,#64374,#64375,#64376,#64377,
#64378,#64379,#64380,#64381,#64382,#64383,#64384,#64385,#64386,#64387,#64388,
#64389,#64390,#64391,#64392,#64393,#64394,#64395,#64396,#64397,#64398,#64399,
#64400,#64401,#64402,#64403,#64404,#64405,#64406,#64407,#64408,#64409,#64410,
#64411,#64412,#64413,#64414,#64415,#64416,#64417,#64418,#64419,#64420,#64421,
#64422,#64423,#64424,#64425,#64426,#64427,#64428,#64429,#64430,#64431,#64432,
#64433,#64434,#64435,#64436,#64437,#64438,#64439,#64440,#64441,#64442,#64443,
#64444));
#13386=EDGE_LOOP('',(#64445,#64446,#64447,#64448,#64449,#64450,#64451,#64452,
#64453,#64454,#64455,#64456,#64457,#64458,#64459,#64460,#64461,#64462,#64463,
#64464,#64465,#64466,#64467,#64468,#64469,#64470,#64471,#64472,#64473,#64474,
#64475,#64476,#64477,#64478,#64479,#64480,#64481,#64482,#64483,#64484,#64485,
#64486,#64487,#64488,#64489,#64490,#64491,#64492,#64493,#64494,#64495,#64496,
#64497,#64498,#64499,#64500,#64501,#64502,#64503,#64504,#64505,#64506,#64507,
#64508,#64509,#64510,#64511,#64512,#64513,#64514,#64515,#64516,#64517,#64518,
#64519,#64520,#64521,#64522,#64523,#64524,#64525,#64526,#64527,#64528,#64529,
#64530,#64531,#64532,#64533,#64534,#64535,#64536,#64537,#64538,#64539,#64540,
#64541,#64542,#64543,#64544,#64545,#64546,#64547,#64548,#64549,#64550,#64551,
#64552,#64553,#64554,#64555,#64556,#64557,#64558,#64559,#64560,#64561,#64562,
#64563,#64564,#64565,#64566,#64567,#64568,#64569,#64570,#64571,#64572,#64573,
#64574,#64575,#64576,#64577,#64578,#64579,#64580,#64581,#64582,#64583,#64584,
#64585,#64586,#64587,#64588,#64589,#64590,#64591,#64592,#64593,#64594,#64595,
#64596,#64597,#64598,#64599,#64600,#64601,#64602,#64603,#64604,#64605,#64606,
#64607,#64608,#64609,#64610,#64611,#64612,#64613,#64614,#64615,#64616,#64617,
#64618,#64619,#64620,#64621,#64622,#64623,#64624,#64625,#64626,#64627,#64628,
#64629,#64630,#64631,#64632,#64633,#64634,#64635,#64636,#64637,#64638,#64639,
#64640,#64641,#64642,#64643,#64644,#64645,#64646,#64647,#64648,#64649,#64650,
#64651,#64652,#64653,#64654,#64655,#64656,#64657,#64658,#64659,#64660,#64661,
#64662,#64663,#64664,#64665,#64666,#64667,#64668,#64669,#64670,#64671,#64672,
#64673,#64674,#64675,#64676,#64677,#64678,#64679,#64680,#64681,#64682,#64683,
#64684,#64685,#64686,#64687,#64688,#64689,#64690,#64691,#64692,#64693,#64694,
#64695,#64696,#64697,#64698,#64699,#64700,#64701,#64702,#64703,#64704,#64705,
#64706,#64707,#64708,#64709,#64710,#64711,#64712,#64713,#64714,#64715,#64716,
#64717,#64718,#64719,#64720,#64721,#64722,#64723,#64724,#64725,#64726,#64727,
#64728,#64729));
#13387=EDGE_LOOP('',(#64730,#64731,#64732,#64733,#64734));
#13388=EDGE_LOOP('',(#64735,#64736,#64737,#64738,#64739));
#13389=EDGE_LOOP('',(#64740));
#13390=EDGE_LOOP('',(#64741));
#13391=EDGE_LOOP('',(#64742));
#13392=EDGE_LOOP('',(#64743));
#13393=EDGE_LOOP('',(#64744));
#13394=EDGE_LOOP('',(#64745));
#13395=EDGE_LOOP('',(#64746));
#13396=EDGE_LOOP('',(#64747));
#13397=EDGE_LOOP('',(#64748));
#13398=EDGE_LOOP('',(#64749));
#13399=EDGE_LOOP('',(#64750,#64751,#64752,#64753));
#13400=EDGE_LOOP('',(#64754,#64755,#64756,#64757));
#13401=EDGE_LOOP('',(#64758,#64759,#64760,#64761));
#13402=EDGE_LOOP('',(#64762,#64763,#64764,#64765));
#13403=EDGE_LOOP('',(#64766,#64767,#64768,#64769));
#13404=EDGE_LOOP('',(#64770,#64771,#64772,#64773));
#13405=EDGE_LOOP('',(#64774,#64775,#64776,#64777));
#13406=EDGE_LOOP('',(#64778,#64779,#64780,#64781));
#13407=EDGE_LOOP('',(#64782,#64783,#64784,#64785));
#13408=EDGE_LOOP('',(#64786,#64787,#64788,#64789));
#13409=EDGE_LOOP('',(#64790,#64791,#64792,#64793));
#13410=EDGE_LOOP('',(#64794,#64795,#64796,#64797));
#13411=EDGE_LOOP('',(#64798,#64799,#64800,#64801));
#13412=EDGE_LOOP('',(#64802,#64803,#64804,#64805));
#13413=EDGE_LOOP('',(#64806,#64807,#64808,#64809));
#13414=EDGE_LOOP('',(#64810,#64811,#64812,#64813));
#13415=EDGE_LOOP('',(#64814,#64815,#64816,#64817));
#13416=EDGE_LOOP('',(#64818,#64819,#64820,#64821));
#13417=EDGE_LOOP('',(#64822,#64823,#64824,#64825));
#13418=EDGE_LOOP('',(#64826,#64827,#64828,#64829));
#13419=EDGE_LOOP('',(#64830,#64831,#64832,#64833));
#13420=EDGE_LOOP('',(#64834,#64835,#64836,#64837));
#13421=EDGE_LOOP('',(#64838,#64839,#64840,#64841));
#13422=EDGE_LOOP('',(#64842,#64843,#64844,#64845));
#13423=EDGE_LOOP('',(#64846,#64847,#64848,#64849));
#13424=EDGE_LOOP('',(#64850,#64851,#64852,#64853));
#13425=EDGE_LOOP('',(#64854,#64855,#64856,#64857));
#13426=EDGE_LOOP('',(#64858,#64859,#64860,#64861));
#13427=EDGE_LOOP('',(#64862,#64863,#64864,#64865));
#13428=EDGE_LOOP('',(#64866,#64867,#64868,#64869));
#13429=EDGE_LOOP('',(#64870,#64871,#64872,#64873));
#13430=EDGE_LOOP('',(#64874,#64875,#64876,#64877));
#13431=EDGE_LOOP('',(#64878,#64879,#64880,#64881));
#13432=EDGE_LOOP('',(#64882,#64883,#64884,#64885));
#13433=EDGE_LOOP('',(#64886,#64887,#64888,#64889));
#13434=EDGE_LOOP('',(#64890,#64891,#64892,#64893));
#13435=EDGE_LOOP('',(#64894,#64895,#64896,#64897));
#13436=EDGE_LOOP('',(#64898,#64899,#64900,#64901));
#13437=EDGE_LOOP('',(#64902,#64903,#64904,#64905));
#13438=EDGE_LOOP('',(#64906,#64907,#64908,#64909));
#13439=EDGE_LOOP('',(#64910,#64911,#64912,#64913));
#13440=EDGE_LOOP('',(#64914,#64915,#64916,#64917));
#13441=EDGE_LOOP('',(#64918,#64919,#64920,#64921));
#13442=EDGE_LOOP('',(#64922,#64923,#64924,#64925));
#13443=EDGE_LOOP('',(#64926,#64927,#64928,#64929));
#13444=EDGE_LOOP('',(#64930,#64931,#64932,#64933));
#13445=EDGE_LOOP('',(#64934,#64935,#64936,#64937));
#13446=EDGE_LOOP('',(#64938,#64939,#64940,#64941));
#13447=EDGE_LOOP('',(#64942,#64943,#64944,#64945));
#13448=EDGE_LOOP('',(#64946,#64947,#64948,#64949));
#13449=EDGE_LOOP('',(#64950,#64951,#64952,#64953));
#13450=EDGE_LOOP('',(#64954,#64955,#64956,#64957));
#13451=EDGE_LOOP('',(#64958,#64959,#64960,#64961));
#13452=EDGE_LOOP('',(#64962,#64963,#64964,#64965));
#13453=EDGE_LOOP('',(#64966,#64967,#64968,#64969));
#13454=EDGE_LOOP('',(#64970,#64971,#64972,#64973));
#13455=EDGE_LOOP('',(#64974,#64975,#64976,#64977));
#13456=EDGE_LOOP('',(#64978,#64979,#64980,#64981));
#13457=EDGE_LOOP('',(#64982,#64983,#64984,#64985));
#13458=EDGE_LOOP('',(#64986,#64987,#64988,#64989));
#13459=EDGE_LOOP('',(#64990,#64991,#64992,#64993));
#13460=EDGE_LOOP('',(#64994,#64995,#64996,#64997));
#13461=EDGE_LOOP('',(#64998,#64999,#65000,#65001));
#13462=EDGE_LOOP('',(#65002,#65003,#65004,#65005));
#13463=EDGE_LOOP('',(#65006,#65007,#65008,#65009));
#13464=EDGE_LOOP('',(#65010,#65011,#65012,#65013));
#13465=EDGE_LOOP('',(#65014,#65015,#65016,#65017));
#13466=EDGE_LOOP('',(#65018,#65019,#65020,#65021));
#13467=EDGE_LOOP('',(#65022,#65023,#65024,#65025));
#13468=EDGE_LOOP('',(#65026,#65027,#65028,#65029));
#13469=EDGE_LOOP('',(#65030,#65031,#65032,#65033));
#13470=EDGE_LOOP('',(#65034,#65035,#65036,#65037));
#13471=EDGE_LOOP('',(#65038,#65039,#65040,#65041));
#13472=EDGE_LOOP('',(#65042,#65043,#65044,#65045));
#13473=EDGE_LOOP('',(#65046,#65047,#65048,#65049));
#13474=EDGE_LOOP('',(#65050,#65051,#65052,#65053));
#13475=EDGE_LOOP('',(#65054,#65055,#65056,#65057));
#13476=EDGE_LOOP('',(#65058,#65059,#65060,#65061));
#13477=EDGE_LOOP('',(#65062,#65063,#65064,#65065));
#13478=EDGE_LOOP('',(#65066,#65067,#65068,#65069));
#13479=EDGE_LOOP('',(#65070,#65071,#65072,#65073));
#13480=EDGE_LOOP('',(#65074,#65075,#65076,#65077));
#13481=EDGE_LOOP('',(#65078,#65079,#65080,#65081));
#13482=EDGE_LOOP('',(#65082,#65083,#65084,#65085));
#13483=EDGE_LOOP('',(#65086,#65087,#65088,#65089));
#13484=EDGE_LOOP('',(#65090,#65091,#65092,#65093));
#13485=EDGE_LOOP('',(#65094,#65095,#65096,#65097));
#13486=EDGE_LOOP('',(#65098,#65099,#65100,#65101));
#13487=EDGE_LOOP('',(#65102,#65103,#65104,#65105));
#13488=EDGE_LOOP('',(#65106,#65107,#65108,#65109));
#13489=EDGE_LOOP('',(#65110,#65111,#65112,#65113));
#13490=EDGE_LOOP('',(#65114,#65115,#65116,#65117));
#13491=EDGE_LOOP('',(#65118,#65119,#65120,#65121));
#13492=EDGE_LOOP('',(#65122,#65123,#65124,#65125));
#13493=EDGE_LOOP('',(#65126,#65127,#65128,#65129));
#13494=EDGE_LOOP('',(#65130,#65131,#65132,#65133));
#13495=EDGE_LOOP('',(#65134,#65135,#65136,#65137));
#13496=EDGE_LOOP('',(#65138,#65139,#65140,#65141));
#13497=EDGE_LOOP('',(#65142,#65143,#65144,#65145));
#13498=EDGE_LOOP('',(#65146,#65147,#65148,#65149));
#13499=EDGE_LOOP('',(#65150,#65151,#65152,#65153));
#13500=EDGE_LOOP('',(#65154,#65155,#65156,#65157));
#13501=EDGE_LOOP('',(#65158,#65159,#65160,#65161));
#13502=EDGE_LOOP('',(#65162,#65163,#65164,#65165));
#13503=EDGE_LOOP('',(#65166,#65167,#65168,#65169));
#13504=EDGE_LOOP('',(#65170,#65171,#65172,#65173));
#13505=EDGE_LOOP('',(#65174,#65175,#65176,#65177,#65178,#65179));
#13506=EDGE_LOOP('',(#65180,#65181,#65182,#65183));
#13507=EDGE_LOOP('',(#65184,#65185,#65186,#65187));
#13508=EDGE_LOOP('',(#65188,#65189,#65190,#65191));
#13509=EDGE_LOOP('',(#65192,#65193,#65194,#65195));
#13510=EDGE_LOOP('',(#65196,#65197,#65198,#65199));
#13511=EDGE_LOOP('',(#65200,#65201,#65202,#65203));
#13512=EDGE_LOOP('',(#65204,#65205,#65206,#65207));
#13513=EDGE_LOOP('',(#65208,#65209,#65210,#65211));
#13514=EDGE_LOOP('',(#65212,#65213,#65214,#65215));
#13515=EDGE_LOOP('',(#65216,#65217,#65218,#65219));
#13516=EDGE_LOOP('',(#65220,#65221,#65222,#65223));
#13517=EDGE_LOOP('',(#65224,#65225,#65226,#65227));
#13518=EDGE_LOOP('',(#65228,#65229,#65230,#65231));
#13519=EDGE_LOOP('',(#65232,#65233,#65234,#65235));
#13520=EDGE_LOOP('',(#65236,#65237,#65238,#65239));
#13521=EDGE_LOOP('',(#65240,#65241,#65242,#65243));
#13522=EDGE_LOOP('',(#65244,#65245,#65246,#65247));
#13523=EDGE_LOOP('',(#65248,#65249,#65250,#65251));
#13524=EDGE_LOOP('',(#65252,#65253,#65254,#65255));
#13525=EDGE_LOOP('',(#65256,#65257,#65258,#65259));
#13526=EDGE_LOOP('',(#65260,#65261,#65262,#65263));
#13527=EDGE_LOOP('',(#65264,#65265,#65266,#65267));
#13528=EDGE_LOOP('',(#65268,#65269,#65270,#65271));
#13529=EDGE_LOOP('',(#65272,#65273,#65274,#65275));
#13530=EDGE_LOOP('',(#65276,#65277,#65278,#65279));
#13531=EDGE_LOOP('',(#65280,#65281,#65282,#65283));
#13532=EDGE_LOOP('',(#65284,#65285,#65286,#65287));
#13533=EDGE_LOOP('',(#65288,#65289,#65290,#65291));
#13534=EDGE_LOOP('',(#65292,#65293,#65294,#65295));
#13535=EDGE_LOOP('',(#65296,#65297,#65298,#65299));
#13536=EDGE_LOOP('',(#65300,#65301,#65302,#65303));
#13537=EDGE_LOOP('',(#65304,#65305,#65306,#65307));
#13538=EDGE_LOOP('',(#65308,#65309,#65310,#65311));
#13539=EDGE_LOOP('',(#65312,#65313,#65314,#65315));
#13540=EDGE_LOOP('',(#65316,#65317,#65318,#65319));
#13541=EDGE_LOOP('',(#65320,#65321,#65322,#65323));
#13542=EDGE_LOOP('',(#65324,#65325,#65326,#65327));
#13543=EDGE_LOOP('',(#65328,#65329,#65330,#65331));
#13544=EDGE_LOOP('',(#65332,#65333,#65334,#65335));
#13545=EDGE_LOOP('',(#65336,#65337,#65338,#65339));
#13546=EDGE_LOOP('',(#65340,#65341,#65342,#65343));
#13547=EDGE_LOOP('',(#65344,#65345,#65346,#65347));
#13548=EDGE_LOOP('',(#65348,#65349,#65350,#65351));
#13549=EDGE_LOOP('',(#65352,#65353,#65354,#65355));
#13550=EDGE_LOOP('',(#65356,#65357,#65358,#65359));
#13551=EDGE_LOOP('',(#65360,#65361,#65362,#65363));
#13552=EDGE_LOOP('',(#65364,#65365,#65366,#65367));
#13553=EDGE_LOOP('',(#65368,#65369,#65370,#65371));
#13554=EDGE_LOOP('',(#65372,#65373,#65374,#65375));
#13555=EDGE_LOOP('',(#65376,#65377,#65378,#65379));
#13556=EDGE_LOOP('',(#65380,#65381,#65382,#65383));
#13557=EDGE_LOOP('',(#65384,#65385,#65386,#65387));
#13558=EDGE_LOOP('',(#65388,#65389,#65390,#65391));
#13559=EDGE_LOOP('',(#65392,#65393,#65394,#65395));
#13560=EDGE_LOOP('',(#65396,#65397,#65398,#65399));
#13561=EDGE_LOOP('',(#65400,#65401,#65402,#65403));
#13562=EDGE_LOOP('',(#65404,#65405,#65406,#65407));
#13563=EDGE_LOOP('',(#65408,#65409,#65410,#65411));
#13564=EDGE_LOOP('',(#65412,#65413,#65414,#65415));
#13565=EDGE_LOOP('',(#65416,#65417,#65418,#65419));
#13566=EDGE_LOOP('',(#65420,#65421,#65422,#65423));
#13567=EDGE_LOOP('',(#65424,#65425,#65426,#65427));
#13568=EDGE_LOOP('',(#65428,#65429,#65430,#65431));
#13569=EDGE_LOOP('',(#65432,#65433,#65434,#65435));
#13570=EDGE_LOOP('',(#65436,#65437,#65438,#65439));
#13571=EDGE_LOOP('',(#65440,#65441,#65442,#65443));
#13572=EDGE_LOOP('',(#65444,#65445,#65446,#65447));
#13573=EDGE_LOOP('',(#65448,#65449,#65450,#65451));
#13574=EDGE_LOOP('',(#65452,#65453,#65454,#65455));
#13575=EDGE_LOOP('',(#65456,#65457,#65458,#65459));
#13576=EDGE_LOOP('',(#65460,#65461,#65462,#65463));
#13577=EDGE_LOOP('',(#65464,#65465,#65466,#65467));
#13578=EDGE_LOOP('',(#65468,#65469,#65470,#65471));
#13579=EDGE_LOOP('',(#65472,#65473,#65474,#65475));
#13580=EDGE_LOOP('',(#65476,#65477,#65478,#65479));
#13581=EDGE_LOOP('',(#65480,#65481,#65482,#65483));
#13582=EDGE_LOOP('',(#65484,#65485,#65486,#65487));
#13583=EDGE_LOOP('',(#65488,#65489,#65490,#65491));
#13584=EDGE_LOOP('',(#65492,#65493,#65494,#65495));
#13585=EDGE_LOOP('',(#65496,#65497,#65498,#65499));
#13586=EDGE_LOOP('',(#65500,#65501,#65502,#65503));
#13587=EDGE_LOOP('',(#65504,#65505,#65506,#65507));
#13588=EDGE_LOOP('',(#65508,#65509,#65510,#65511));
#13589=EDGE_LOOP('',(#65512,#65513,#65514,#65515));
#13590=EDGE_LOOP('',(#65516,#65517,#65518,#65519));
#13591=EDGE_LOOP('',(#65520,#65521,#65522,#65523));
#13592=EDGE_LOOP('',(#65524,#65525,#65526,#65527));
#13593=EDGE_LOOP('',(#65528,#65529,#65530,#65531));
#13594=EDGE_LOOP('',(#65532,#65533,#65534,#65535));
#13595=EDGE_LOOP('',(#65536,#65537,#65538,#65539));
#13596=EDGE_LOOP('',(#65540,#65541,#65542,#65543));
#13597=EDGE_LOOP('',(#65544,#65545,#65546,#65547));
#13598=EDGE_LOOP('',(#65548,#65549,#65550,#65551));
#13599=EDGE_LOOP('',(#65552,#65553,#65554,#65555));
#13600=EDGE_LOOP('',(#65556,#65557,#65558,#65559));
#13601=EDGE_LOOP('',(#65560,#65561,#65562,#65563));
#13602=EDGE_LOOP('',(#65564,#65565,#65566,#65567));
#13603=EDGE_LOOP('',(#65568,#65569,#65570,#65571));
#13604=EDGE_LOOP('',(#65572,#65573,#65574,#65575));
#13605=EDGE_LOOP('',(#65576,#65577,#65578,#65579));
#13606=EDGE_LOOP('',(#65580,#65581,#65582,#65583));
#13607=EDGE_LOOP('',(#65584,#65585,#65586,#65587));
#13608=EDGE_LOOP('',(#65588,#65589,#65590,#65591));
#13609=EDGE_LOOP('',(#65592,#65593,#65594,#65595));
#13610=EDGE_LOOP('',(#65596,#65597,#65598,#65599));
#13611=EDGE_LOOP('',(#65600,#65601,#65602,#65603));
#13612=EDGE_LOOP('',(#65604,#65605,#65606,#65607));
#13613=EDGE_LOOP('',(#65608,#65609,#65610,#65611,#65612));
#13614=EDGE_LOOP('',(#65613,#65614,#65615,#65616));
#13615=EDGE_LOOP('',(#65617,#65618,#65619,#65620,#65621));
#13616=EDGE_LOOP('',(#65622,#65623,#65624,#65625));
#13617=EDGE_LOOP('',(#65626,#65627,#65628,#65629));
#13618=EDGE_LOOP('',(#65630,#65631,#65632,#65633,#65634));
#13619=EDGE_LOOP('',(#65635,#65636,#65637,#65638,#65639));
#13620=EDGE_LOOP('',(#65640,#65641,#65642,#65643,#65644));
#13621=EDGE_LOOP('',(#65645,#65646,#65647,#65648));
#13622=EDGE_LOOP('',(#65649,#65650,#65651,#65652));
#13623=EDGE_LOOP('',(#65653,#65654,#65655,#65656,#65657));
#13624=EDGE_LOOP('',(#65658,#65659,#65660,#65661,#65662));
#13625=EDGE_LOOP('',(#65663,#65664,#65665,#65666,#65667));
#13626=EDGE_LOOP('',(#65668,#65669,#65670,#65671,#65672));
#13627=EDGE_LOOP('',(#65673,#65674,#65675,#65676));
#13628=EDGE_LOOP('',(#65677,#65678,#65679,#65680));
#13629=EDGE_LOOP('',(#65681,#65682,#65683,#65684));
#13630=EDGE_LOOP('',(#65685,#65686,#65687,#65688));
#13631=EDGE_LOOP('',(#65689,#65690,#65691,#65692,#65693));
#13632=EDGE_LOOP('',(#65694,#65695,#65696,#65697,#65698,#65699,#65700,#65701,
#65702,#65703,#65704,#65705,#65706,#65707,#65708,#65709,#65710,#65711,#65712,
#65713,#65714,#65715,#65716,#65717,#65718,#65719,#65720,#65721,#65722,#65723,
#65724,#65725,#65726,#65727,#65728,#65729,#65730,#65731,#65732,#65733,#65734,
#65735,#65736,#65737,#65738,#65739,#65740,#65741,#65742,#65743,#65744,#65745,
#65746,#65747,#65748,#65749,#65750,#65751,#65752,#65753,#65754,#65755,#65756,
#65757,#65758,#65759,#65760,#65761,#65762,#65763,#65764,#65765,#65766,#65767,
#65768,#65769,#65770,#65771,#65772,#65773,#65774,#65775,#65776,#65777,#65778,
#65779,#65780,#65781,#65782,#65783,#65784,#65785,#65786,#65787,#65788,#65789,
#65790,#65791,#65792,#65793,#65794,#65795,#65796,#65797,#65798,#65799,#65800,
#65801,#65802,#65803,#65804,#65805,#65806,#65807,#65808,#65809,#65810,#65811,
#65812,#65813,#65814,#65815,#65816,#65817,#65818,#65819,#65820,#65821,#65822,
#65823,#65824,#65825,#65826,#65827,#65828,#65829,#65830,#65831,#65832,#65833,
#65834,#65835,#65836,#65837,#65838,#65839,#65840,#65841));
#13633=EDGE_LOOP('',(#65842));
#13634=EDGE_LOOP('',(#65843));
#13635=EDGE_LOOP('',(#65844,#65845,#65846,#65847,#65848,#65849,#65850,#65851));
#13636=EDGE_LOOP('',(#65852,#65853,#65854,#65855,#65856,#65857,#65858,#65859));
#13637=EDGE_LOOP('',(#65860));
#13638=EDGE_LOOP('',(#65861,#65862,#65863,#65864));
#13639=EDGE_LOOP('',(#65865,#65866,#65867,#65868));
#13640=EDGE_LOOP('',(#65869,#65870,#65871,#65872));
#13641=EDGE_LOOP('',(#65873,#65874,#65875,#65876));
#13642=EDGE_LOOP('',(#65877,#65878,#65879,#65880));
#13643=EDGE_LOOP('',(#65881,#65882,#65883,#65884));
#13644=EDGE_LOOP('',(#65885,#65886,#65887,#65888));
#13645=EDGE_LOOP('',(#65889,#65890,#65891,#65892));
#13646=EDGE_LOOP('',(#65893,#65894,#65895,#65896));
#13647=EDGE_LOOP('',(#65897,#65898,#65899,#65900));
#13648=EDGE_LOOP('',(#65901,#65902,#65903,#65904));
#13649=EDGE_LOOP('',(#65905,#65906,#65907,#65908));
#13650=EDGE_LOOP('',(#65909,#65910,#65911,#65912));
#13651=EDGE_LOOP('',(#65913,#65914,#65915,#65916));
#13652=EDGE_LOOP('',(#65917,#65918,#65919,#65920));
#13653=EDGE_LOOP('',(#65921,#65922,#65923,#65924));
#13654=EDGE_LOOP('',(#65925,#65926,#65927,#65928));
#13655=EDGE_LOOP('',(#65929,#65930,#65931,#65932));
#13656=EDGE_LOOP('',(#65933,#65934,#65935,#65936));
#13657=EDGE_LOOP('',(#65937,#65938,#65939,#65940));
#13658=EDGE_LOOP('',(#65941,#65942,#65943,#65944));
#13659=EDGE_LOOP('',(#65945,#65946,#65947,#65948));
#13660=EDGE_LOOP('',(#65949,#65950,#65951,#65952));
#13661=EDGE_LOOP('',(#65953,#65954,#65955,#65956));
#13662=EDGE_LOOP('',(#65957,#65958,#65959,#65960));
#13663=EDGE_LOOP('',(#65961,#65962,#65963,#65964));
#13664=EDGE_LOOP('',(#65965,#65966,#65967,#65968));
#13665=EDGE_LOOP('',(#65969,#65970,#65971,#65972));
#13666=EDGE_LOOP('',(#65973,#65974,#65975,#65976));
#13667=EDGE_LOOP('',(#65977,#65978,#65979,#65980));
#13668=EDGE_LOOP('',(#65981,#65982,#65983,#65984));
#13669=EDGE_LOOP('',(#65985,#65986,#65987,#65988));
#13670=EDGE_LOOP('',(#65989,#65990,#65991,#65992));
#13671=EDGE_LOOP('',(#65993,#65994,#65995,#65996));
#13672=EDGE_LOOP('',(#65997,#65998,#65999,#66000));
#13673=EDGE_LOOP('',(#66001,#66002,#66003,#66004));
#13674=EDGE_LOOP('',(#66005,#66006,#66007,#66008,#66009,#66010,#66011,#66012,
#66013,#66014,#66015,#66016,#66017,#66018,#66019,#66020,#66021,#66022,#66023,
#66024,#66025,#66026,#66027,#66028,#66029,#66030,#66031,#66032,#66033,#66034,
#66035,#66036,#66037,#66038,#66039,#66040,#66041,#66042,#66043,#66044,#66045,
#66046,#66047,#66048,#66049,#66050,#66051,#66052,#66053,#66054,#66055,#66056,
#66057,#66058,#66059,#66060,#66061,#66062,#66063,#66064,#66065,#66066,#66067,
#66068,#66069,#66070,#66071,#66072,#66073,#66074,#66075,#66076,#66077,#66078,
#66079,#66080,#66081,#66082,#66083,#66084,#66085,#66086,#66087,#66088,#66089,
#66090,#66091,#66092,#66093,#66094,#66095,#66096,#66097,#66098,#66099,#66100,
#66101,#66102,#66103,#66104,#66105,#66106,#66107,#66108,#66109,#66110,#66111,
#66112,#66113,#66114,#66115,#66116,#66117,#66118,#66119,#66120,#66121,#66122,
#66123,#66124,#66125,#66126,#66127,#66128,#66129,#66130,#66131,#66132,#66133,
#66134,#66135,#66136,#66137,#66138,#66139,#66140,#66141,#66142,#66143,#66144,
#66145,#66146,#66147,#66148,#66149,#66150,#66151,#66152));
#13675=EDGE_LOOP('',(#66153));
#13676=EDGE_LOOP('',(#66154));
#13677=EDGE_LOOP('',(#66155));
#13678=EDGE_LOOP('',(#66156,#66157,#66158,#66159));
#13679=EDGE_LOOP('',(#66160,#66161,#66162,#66163));
#13680=EDGE_LOOP('',(#66164,#66165,#66166,#66167));
#13681=EDGE_LOOP('',(#66168,#66169,#66170,#66171));
#13682=EDGE_LOOP('',(#66172,#66173,#66174,#66175));
#13683=EDGE_LOOP('',(#66176,#66177,#66178,#66179));
#13684=EDGE_LOOP('',(#66180,#66181,#66182,#66183));
#13685=EDGE_LOOP('',(#66184,#66185,#66186,#66187));
#13686=EDGE_LOOP('',(#66188,#66189,#66190,#66191));
#13687=EDGE_LOOP('',(#66192,#66193,#66194,#66195));
#13688=EDGE_LOOP('',(#66196,#66197,#66198,#66199));
#13689=EDGE_LOOP('',(#66200,#66201,#66202,#66203));
#13690=EDGE_LOOP('',(#66204,#66205,#66206,#66207));
#13691=EDGE_LOOP('',(#66208,#66209,#66210,#66211));
#13692=EDGE_LOOP('',(#66212,#66213,#66214,#66215));
#13693=EDGE_LOOP('',(#66216,#66217,#66218,#66219));
#13694=EDGE_LOOP('',(#66220,#66221,#66222,#66223));
#13695=EDGE_LOOP('',(#66224,#66225,#66226,#66227));
#13696=EDGE_LOOP('',(#66228,#66229,#66230,#66231));
#13697=EDGE_LOOP('',(#66232,#66233,#66234,#66235));
#13698=EDGE_LOOP('',(#66236,#66237,#66238,#66239));
#13699=EDGE_LOOP('',(#66240,#66241,#66242,#66243));
#13700=EDGE_LOOP('',(#66244,#66245,#66246,#66247));
#13701=EDGE_LOOP('',(#66248,#66249,#66250,#66251));
#13702=EDGE_LOOP('',(#66252,#66253,#66254,#66255));
#13703=EDGE_LOOP('',(#66256,#66257,#66258,#66259));
#13704=EDGE_LOOP('',(#66260,#66261,#66262,#66263));
#13705=EDGE_LOOP('',(#66264,#66265,#66266,#66267));
#13706=EDGE_LOOP('',(#66268,#66269,#66270,#66271));
#13707=EDGE_LOOP('',(#66272,#66273,#66274,#66275));
#13708=EDGE_LOOP('',(#66276,#66277,#66278,#66279));
#13709=EDGE_LOOP('',(#66280,#66281,#66282,#66283));
#13710=EDGE_LOOP('',(#66284,#66285,#66286,#66287));
#13711=EDGE_LOOP('',(#66288,#66289,#66290,#66291));
#13712=EDGE_LOOP('',(#66292,#66293,#66294,#66295));
#13713=EDGE_LOOP('',(#66296,#66297,#66298,#66299));
#13714=EDGE_LOOP('',(#66300,#66301,#66302,#66303));
#13715=EDGE_LOOP('',(#66304,#66305,#66306,#66307));
#13716=EDGE_LOOP('',(#66308,#66309,#66310,#66311));
#13717=EDGE_LOOP('',(#66312,#66313,#66314,#66315));
#13718=EDGE_LOOP('',(#66316,#66317,#66318,#66319));
#13719=EDGE_LOOP('',(#66320,#66321,#66322,#66323));
#13720=EDGE_LOOP('',(#66324,#66325,#66326,#66327));
#13721=EDGE_LOOP('',(#66328,#66329,#66330,#66331));
#13722=EDGE_LOOP('',(#66332,#66333,#66334,#66335));
#13723=EDGE_LOOP('',(#66336,#66337,#66338,#66339));
#13724=EDGE_LOOP('',(#66340,#66341,#66342,#66343));
#13725=EDGE_LOOP('',(#66344,#66345,#66346,#66347));
#13726=EDGE_LOOP('',(#66348,#66349,#66350,#66351));
#13727=EDGE_LOOP('',(#66352,#66353,#66354,#66355));
#13728=EDGE_LOOP('',(#66356,#66357,#66358,#66359));
#13729=EDGE_LOOP('',(#66360,#66361,#66362,#66363));
#13730=EDGE_LOOP('',(#66364,#66365,#66366,#66367));
#13731=EDGE_LOOP('',(#66368,#66369,#66370,#66371));
#13732=EDGE_LOOP('',(#66372,#66373,#66374,#66375));
#13733=EDGE_LOOP('',(#66376,#66377,#66378,#66379));
#13734=EDGE_LOOP('',(#66380,#66381,#66382,#66383));
#13735=EDGE_LOOP('',(#66384,#66385,#66386,#66387));
#13736=EDGE_LOOP('',(#66388,#66389,#66390,#66391));
#13737=EDGE_LOOP('',(#66392,#66393,#66394,#66395));
#13738=EDGE_LOOP('',(#66396,#66397,#66398,#66399));
#13739=EDGE_LOOP('',(#66400,#66401,#66402,#66403));
#13740=EDGE_LOOP('',(#66404,#66405,#66406,#66407));
#13741=EDGE_LOOP('',(#66408,#66409,#66410,#66411));
#13742=EDGE_LOOP('',(#66412,#66413,#66414,#66415));
#13743=EDGE_LOOP('',(#66416,#66417,#66418,#66419));
#13744=EDGE_LOOP('',(#66420,#66421,#66422,#66423));
#13745=EDGE_LOOP('',(#66424,#66425,#66426,#66427));
#13746=EDGE_LOOP('',(#66428,#66429,#66430,#66431));
#13747=EDGE_LOOP('',(#66432,#66433,#66434,#66435));
#13748=EDGE_LOOP('',(#66436,#66437,#66438,#66439));
#13749=EDGE_LOOP('',(#66440,#66441,#66442,#66443));
#13750=EDGE_LOOP('',(#66444,#66445,#66446,#66447));
#13751=EDGE_LOOP('',(#66448,#66449,#66450,#66451));
#13752=EDGE_LOOP('',(#66452,#66453,#66454,#66455));
#13753=EDGE_LOOP('',(#66456,#66457,#66458,#66459));
#13754=EDGE_LOOP('',(#66460,#66461,#66462,#66463));
#13755=EDGE_LOOP('',(#66464,#66465,#66466,#66467));
#13756=EDGE_LOOP('',(#66468,#66469,#66470,#66471));
#13757=EDGE_LOOP('',(#66472,#66473,#66474,#66475));
#13758=EDGE_LOOP('',(#66476,#66477,#66478,#66479));
#13759=EDGE_LOOP('',(#66480,#66481,#66482,#66483));
#13760=EDGE_LOOP('',(#66484,#66485,#66486,#66487));
#13761=EDGE_LOOP('',(#66488,#66489,#66490,#66491));
#13762=EDGE_LOOP('',(#66492,#66493,#66494,#66495));
#13763=EDGE_LOOP('',(#66496,#66497,#66498,#66499));
#13764=EDGE_LOOP('',(#66500,#66501,#66502,#66503));
#13765=EDGE_LOOP('',(#66504,#66505,#66506,#66507));
#13766=EDGE_LOOP('',(#66508,#66509,#66510,#66511));
#13767=EDGE_LOOP('',(#66512,#66513,#66514,#66515));
#13768=EDGE_LOOP('',(#66516,#66517,#66518,#66519));
#13769=EDGE_LOOP('',(#66520,#66521,#66522,#66523));
#13770=EDGE_LOOP('',(#66524,#66525,#66526,#66527));
#13771=EDGE_LOOP('',(#66528,#66529,#66530,#66531));
#13772=EDGE_LOOP('',(#66532,#66533,#66534,#66535));
#13773=EDGE_LOOP('',(#66536,#66537,#66538,#66539));
#13774=EDGE_LOOP('',(#66540,#66541,#66542,#66543));
#13775=EDGE_LOOP('',(#66544,#66545,#66546,#66547));
#13776=EDGE_LOOP('',(#66548,#66549,#66550,#66551));
#13777=EDGE_LOOP('',(#66552,#66553,#66554,#66555));
#13778=EDGE_LOOP('',(#66556,#66557,#66558,#66559));
#13779=EDGE_LOOP('',(#66560,#66561,#66562,#66563));
#13780=EDGE_LOOP('',(#66564,#66565,#66566,#66567));
#13781=EDGE_LOOP('',(#66568,#66569,#66570,#66571));
#13782=EDGE_LOOP('',(#66572,#66573,#66574,#66575));
#13783=EDGE_LOOP('',(#66576,#66577,#66578,#66579));
#13784=EDGE_LOOP('',(#66580,#66581,#66582,#66583));
#13785=EDGE_LOOP('',(#66584,#66585,#66586,#66587));
#13786=EDGE_LOOP('',(#66588));
#13787=EDGE_LOOP('',(#66589));
#13788=EDGE_LOOP('',(#66590));
#13789=EDGE_LOOP('',(#66591));
#13790=EDGE_LOOP('',(#66592));
#13791=EDGE_LOOP('',(#66593));
#13792=EDGE_LOOP('',(#66594,#66595,#66596,#66597));
#13793=EDGE_LOOP('',(#66598,#66599,#66600,#66601));
#13794=EDGE_LOOP('',(#66602,#66603,#66604,#66605));
#13795=EDGE_LOOP('',(#66606,#66607,#66608,#66609));
#13796=EDGE_LOOP('',(#66610,#66611,#66612,#66613));
#13797=EDGE_LOOP('',(#66614,#66615,#66616,#66617));
#13798=EDGE_LOOP('',(#66618,#66619,#66620,#66621));
#13799=EDGE_LOOP('',(#66622,#66623,#66624,#66625,#66626,#66627,#66628,#66629));
#13800=EDGE_LOOP('',(#66630,#66631,#66632,#66633));
#13801=EDGE_LOOP('',(#66634,#66635,#66636,#66637));
#13802=EDGE_LOOP('',(#66638,#66639,#66640,#66641));
#13803=EDGE_LOOP('',(#66642,#66643,#66644,#66645));
#13804=EDGE_LOOP('',(#66646,#66647,#66648,#66649));
#13805=EDGE_LOOP('',(#66650,#66651,#66652,#66653));
#13806=EDGE_LOOP('',(#66654,#66655,#66656,#66657));
#13807=EDGE_LOOP('',(#66658,#66659,#66660,#66661,#66662,#66663,#66664,#66665));
#13808=EDGE_LOOP('',(#66666,#66667,#66668,#66669));
#13809=EDGE_LOOP('',(#66670,#66671,#66672,#66673));
#13810=EDGE_LOOP('',(#66674,#66675,#66676,#66677));
#13811=EDGE_LOOP('',(#66678,#66679,#66680,#66681));
#13812=EDGE_LOOP('',(#66682,#66683,#66684,#66685));
#13813=EDGE_LOOP('',(#66686,#66687,#66688,#66689));
#13814=EDGE_LOOP('',(#66690,#66691,#66692,#66693));
#13815=EDGE_LOOP('',(#66694,#66695,#66696,#66697));
#13816=EDGE_LOOP('',(#66698,#66699,#66700,#66701));
#13817=EDGE_LOOP('',(#66702,#66703,#66704,#66705));
#13818=EDGE_LOOP('',(#66706,#66707,#66708,#66709));
#13819=EDGE_LOOP('',(#66710,#66711,#66712,#66713));
#13820=EDGE_LOOP('',(#66714,#66715,#66716,#66717));
#13821=EDGE_LOOP('',(#66718,#66719,#66720,#66721));
#13822=EDGE_LOOP('',(#66722));
#13823=EDGE_LOOP('',(#66723));
#13824=EDGE_LOOP('',(#66724,#66725,#66726,#66727));
#13825=EDGE_LOOP('',(#66728,#66729,#66730,#66731));
#13826=EDGE_LOOP('',(#66732,#66733,#66734,#66735));
#13827=EDGE_LOOP('',(#66736,#66737,#66738,#66739));
#13828=EDGE_LOOP('',(#66740,#66741,#66742,#66743));
#13829=EDGE_LOOP('',(#66744,#66745,#66746,#66747));
#13830=EDGE_LOOP('',(#66748,#66749,#66750,#66751));
#13831=EDGE_LOOP('',(#66752,#66753,#66754,#66755));
#13832=EDGE_LOOP('',(#66756,#66757,#66758,#66759));
#13833=EDGE_LOOP('',(#66760,#66761,#66762,#66763));
#13834=EDGE_LOOP('',(#66764,#66765,#66766,#66767));
#13835=EDGE_LOOP('',(#66768,#66769,#66770,#66771));
#13836=EDGE_LOOP('',(#66772,#66773,#66774,#66775));
#13837=EDGE_LOOP('',(#66776,#66777,#66778,#66779));
#13838=EDGE_LOOP('',(#66780,#66781,#66782,#66783));
#13839=EDGE_LOOP('',(#66784,#66785,#66786,#66787));
#13840=EDGE_LOOP('',(#66788,#66789,#66790,#66791));
#13841=EDGE_LOOP('',(#66792,#66793,#66794,#66795));
#13842=EDGE_LOOP('',(#66796,#66797,#66798,#66799));
#13843=EDGE_LOOP('',(#66800,#66801,#66802,#66803));
#13844=EDGE_LOOP('',(#66804,#66805,#66806,#66807));
#13845=EDGE_LOOP('',(#66808,#66809,#66810,#66811));
#13846=EDGE_LOOP('',(#66812,#66813,#66814,#66815));
#13847=EDGE_LOOP('',(#66816,#66817,#66818,#66819));
#13848=EDGE_LOOP('',(#66820,#66821,#66822,#66823));
#13849=EDGE_LOOP('',(#66824,#66825,#66826,#66827));
#13850=EDGE_LOOP('',(#66828,#66829,#66830,#66831));
#13851=EDGE_LOOP('',(#66832,#66833,#66834,#66835));
#13852=EDGE_LOOP('',(#66836,#66837,#66838,#66839));
#13853=EDGE_LOOP('',(#66840,#66841,#66842,#66843));
#13854=EDGE_LOOP('',(#66844,#66845,#66846,#66847));
#13855=EDGE_LOOP('',(#66848,#66849,#66850,#66851));
#13856=EDGE_LOOP('',(#66852,#66853,#66854,#66855));
#13857=EDGE_LOOP('',(#66856,#66857,#66858,#66859));
#13858=EDGE_LOOP('',(#66860,#66861,#66862,#66863));
#13859=EDGE_LOOP('',(#66864,#66865,#66866,#66867));
#13860=EDGE_LOOP('',(#66868,#66869,#66870,#66871));
#13861=EDGE_LOOP('',(#66872,#66873,#66874,#66875));
#13862=EDGE_LOOP('',(#66876,#66877,#66878,#66879));
#13863=EDGE_LOOP('',(#66880,#66881,#66882,#66883));
#13864=EDGE_LOOP('',(#66884,#66885,#66886,#66887));
#13865=EDGE_LOOP('',(#66888,#66889,#66890,#66891));
#13866=EDGE_LOOP('',(#66892,#66893,#66894,#66895));
#13867=EDGE_LOOP('',(#66896,#66897,#66898,#66899));
#13868=EDGE_LOOP('',(#66900,#66901,#66902,#66903));
#13869=EDGE_LOOP('',(#66904,#66905,#66906,#66907));
#13870=EDGE_LOOP('',(#66908,#66909,#66910,#66911));
#13871=EDGE_LOOP('',(#66912,#66913,#66914,#66915));
#13872=EDGE_LOOP('',(#66916,#66917,#66918,#66919));
#13873=EDGE_LOOP('',(#66920,#66921,#66922,#66923));
#13874=EDGE_LOOP('',(#66924,#66925,#66926,#66927));
#13875=EDGE_LOOP('',(#66928,#66929,#66930,#66931));
#13876=EDGE_LOOP('',(#66932,#66933,#66934,#66935));
#13877=EDGE_LOOP('',(#66936,#66937,#66938,#66939));
#13878=EDGE_LOOP('',(#66940,#66941,#66942,#66943));
#13879=EDGE_LOOP('',(#66944,#66945,#66946,#66947));
#13880=EDGE_LOOP('',(#66948,#66949,#66950,#66951));
#13881=EDGE_LOOP('',(#66952,#66953,#66954,#66955));
#13882=EDGE_LOOP('',(#66956,#66957,#66958,#66959));
#13883=EDGE_LOOP('',(#66960,#66961,#66962,#66963));
#13884=EDGE_LOOP('',(#66964,#66965,#66966,#66967));
#13885=EDGE_LOOP('',(#66968,#66969,#66970,#66971));
#13886=EDGE_LOOP('',(#66972,#66973,#66974,#66975));
#13887=EDGE_LOOP('',(#66976,#66977,#66978,#66979));
#13888=EDGE_LOOP('',(#66980,#66981,#66982,#66983));
#13889=EDGE_LOOP('',(#66984,#66985,#66986,#66987));
#13890=EDGE_LOOP('',(#66988,#66989,#66990,#66991));
#13891=EDGE_LOOP('',(#66992,#66993,#66994,#66995));
#13892=EDGE_LOOP('',(#66996,#66997,#66998,#66999));
#13893=EDGE_LOOP('',(#67000,#67001,#67002,#67003));
#13894=EDGE_LOOP('',(#67004,#67005,#67006,#67007));
#13895=EDGE_LOOP('',(#67008,#67009,#67010,#67011));
#13896=EDGE_LOOP('',(#67012,#67013,#67014,#67015));
#13897=EDGE_LOOP('',(#67016,#67017,#67018,#67019));
#13898=EDGE_LOOP('',(#67020,#67021,#67022,#67023));
#13899=EDGE_LOOP('',(#67024,#67025,#67026,#67027));
#13900=EDGE_LOOP('',(#67028,#67029,#67030,#67031));
#13901=EDGE_LOOP('',(#67032,#67033,#67034,#67035));
#13902=EDGE_LOOP('',(#67036,#67037,#67038,#67039));
#13903=EDGE_LOOP('',(#67040,#67041,#67042,#67043));
#13904=EDGE_LOOP('',(#67044,#67045,#67046,#67047));
#13905=EDGE_LOOP('',(#67048,#67049,#67050,#67051));
#13906=EDGE_LOOP('',(#67052,#67053,#67054,#67055));
#13907=EDGE_LOOP('',(#67056,#67057,#67058,#67059));
#13908=EDGE_LOOP('',(#67060,#67061,#67062,#67063));
#13909=EDGE_LOOP('',(#67064,#67065,#67066,#67067));
#13910=EDGE_LOOP('',(#67068,#67069,#67070,#67071));
#13911=EDGE_LOOP('',(#67072,#67073,#67074,#67075));
#13912=EDGE_LOOP('',(#67076,#67077,#67078,#67079));
#13913=EDGE_LOOP('',(#67080,#67081,#67082,#67083));
#13914=EDGE_LOOP('',(#67084,#67085,#67086,#67087));
#13915=EDGE_LOOP('',(#67088,#67089,#67090,#67091));
#13916=EDGE_LOOP('',(#67092,#67093,#67094,#67095));
#13917=EDGE_LOOP('',(#67096,#67097,#67098,#67099));
#13918=EDGE_LOOP('',(#67100,#67101,#67102,#67103));
#13919=EDGE_LOOP('',(#67104,#67105,#67106,#67107));
#13920=EDGE_LOOP('',(#67108,#67109,#67110,#67111));
#13921=EDGE_LOOP('',(#67112,#67113,#67114,#67115));
#13922=EDGE_LOOP('',(#67116,#67117,#67118,#67119));
#13923=EDGE_LOOP('',(#67120,#67121,#67122,#67123));
#13924=EDGE_LOOP('',(#67124,#67125,#67126,#67127));
#13925=EDGE_LOOP('',(#67128,#67129,#67130,#67131));
#13926=EDGE_LOOP('',(#67132,#67133,#67134,#67135));
#13927=EDGE_LOOP('',(#67136,#67137,#67138,#67139));
#13928=EDGE_LOOP('',(#67140,#67141,#67142,#67143));
#13929=EDGE_LOOP('',(#67144,#67145,#67146,#67147));
#13930=EDGE_LOOP('',(#67148,#67149,#67150,#67151));
#13931=EDGE_LOOP('',(#67152,#67153,#67154,#67155));
#13932=EDGE_LOOP('',(#67156,#67157,#67158,#67159));
#13933=EDGE_LOOP('',(#67160,#67161,#67162,#67163));
#13934=EDGE_LOOP('',(#67164,#67165,#67166,#67167));
#13935=EDGE_LOOP('',(#67168,#67169,#67170,#67171));
#13936=EDGE_LOOP('',(#67172,#67173,#67174,#67175));
#13937=EDGE_LOOP('',(#67176,#67177,#67178,#67179));
#13938=EDGE_LOOP('',(#67180,#67181,#67182,#67183));
#13939=EDGE_LOOP('',(#67184,#67185,#67186,#67187));
#13940=EDGE_LOOP('',(#67188,#67189,#67190,#67191));
#13941=EDGE_LOOP('',(#67192,#67193,#67194,#67195));
#13942=EDGE_LOOP('',(#67196,#67197,#67198,#67199));
#13943=EDGE_LOOP('',(#67200,#67201,#67202,#67203));
#13944=EDGE_LOOP('',(#67204,#67205,#67206,#67207));
#13945=EDGE_LOOP('',(#67208,#67209,#67210,#67211));
#13946=EDGE_LOOP('',(#67212,#67213,#67214,#67215));
#13947=EDGE_LOOP('',(#67216,#67217,#67218,#67219));
#13948=EDGE_LOOP('',(#67220,#67221,#67222,#67223));
#13949=EDGE_LOOP('',(#67224,#67225,#67226,#67227));
#13950=EDGE_LOOP('',(#67228,#67229,#67230,#67231));
#13951=EDGE_LOOP('',(#67232,#67233,#67234,#67235));
#13952=EDGE_LOOP('',(#67236,#67237,#67238,#67239));
#13953=EDGE_LOOP('',(#67240,#67241,#67242,#67243));
#13954=EDGE_LOOP('',(#67244,#67245,#67246,#67247));
#13955=EDGE_LOOP('',(#67248,#67249,#67250,#67251));
#13956=EDGE_LOOP('',(#67252,#67253,#67254,#67255));
#13957=EDGE_LOOP('',(#67256,#67257,#67258,#67259));
#13958=EDGE_LOOP('',(#67260,#67261,#67262,#67263));
#13959=EDGE_LOOP('',(#67264,#67265,#67266,#67267));
#13960=EDGE_LOOP('',(#67268,#67269,#67270,#67271));
#13961=EDGE_LOOP('',(#67272,#67273,#67274,#67275));
#13962=EDGE_LOOP('',(#67276,#67277,#67278,#67279));
#13963=EDGE_LOOP('',(#67280,#67281,#67282,#67283));
#13964=EDGE_LOOP('',(#67284,#67285,#67286,#67287));
#13965=EDGE_LOOP('',(#67288,#67289,#67290,#67291));
#13966=EDGE_LOOP('',(#67292,#67293,#67294,#67295));
#13967=EDGE_LOOP('',(#67296,#67297,#67298,#67299));
#13968=EDGE_LOOP('',(#67300,#67301,#67302,#67303));
#13969=EDGE_LOOP('',(#67304,#67305,#67306,#67307));
#13970=EDGE_LOOP('',(#67308,#67309,#67310,#67311));
#13971=EDGE_LOOP('',(#67312,#67313,#67314,#67315));
#13972=EDGE_LOOP('',(#67316,#67317,#67318,#67319));
#13973=EDGE_LOOP('',(#67320,#67321,#67322,#67323));
#13974=EDGE_LOOP('',(#67324,#67325,#67326,#67327));
#13975=EDGE_LOOP('',(#67328,#67329,#67330,#67331));
#13976=EDGE_LOOP('',(#67332,#67333,#67334,#67335));
#13977=EDGE_LOOP('',(#67336,#67337,#67338,#67339));
#13978=EDGE_LOOP('',(#67340,#67341,#67342,#67343));
#13979=EDGE_LOOP('',(#67344,#67345,#67346,#67347));
#13980=EDGE_LOOP('',(#67348,#67349,#67350,#67351));
#13981=EDGE_LOOP('',(#67352,#67353,#67354,#67355));
#13982=EDGE_LOOP('',(#67356,#67357,#67358,#67359));
#13983=EDGE_LOOP('',(#67360,#67361,#67362,#67363));
#13984=EDGE_LOOP('',(#67364,#67365,#67366,#67367));
#13985=EDGE_LOOP('',(#67368,#67369,#67370,#67371));
#13986=EDGE_LOOP('',(#67372,#67373,#67374,#67375));
#13987=EDGE_LOOP('',(#67376,#67377,#67378,#67379));
#13988=EDGE_LOOP('',(#67380,#67381,#67382,#67383));
#13989=EDGE_LOOP('',(#67384,#67385,#67386,#67387));
#13990=EDGE_LOOP('',(#67388,#67389,#67390,#67391));
#13991=EDGE_LOOP('',(#67392,#67393,#67394,#67395));
#13992=EDGE_LOOP('',(#67396,#67397,#67398,#67399));
#13993=EDGE_LOOP('',(#67400,#67401,#67402,#67403));
#13994=EDGE_LOOP('',(#67404,#67405,#67406,#67407));
#13995=EDGE_LOOP('',(#67408,#67409,#67410,#67411,#67412,#67413,#67414,#67415,
#67416,#67417,#67418,#67419,#67420,#67421,#67422,#67423,#67424,#67425,#67426,
#67427,#67428,#67429,#67430,#67431,#67432,#67433,#67434,#67435,#67436,#67437,
#67438,#67439,#67440,#67441,#67442,#67443,#67444,#67445,#67446,#67447,#67448,
#67449,#67450,#67451,#67452,#67453,#67454,#67455,#67456,#67457,#67458,#67459,
#67460,#67461,#67462,#67463,#67464,#67465,#67466,#67467,#67468,#67469,#67470,
#67471,#67472,#67473,#67474,#67475,#67476,#67477,#67478,#67479,#67480,#67481,
#67482,#67483,#67484,#67485,#67486,#67487,#67488,#67489,#67490,#67491,#67492,
#67493,#67494,#67495,#67496,#67497,#67498,#67499,#67500,#67501,#67502,#67503,
#67504,#67505,#67506,#67507,#67508,#67509,#67510,#67511,#67512,#67513,#67514,
#67515,#67516,#67517,#67518,#67519,#67520,#67521,#67522,#67523,#67524,#67525,
#67526,#67527,#67528,#67529,#67530,#67531,#67532,#67533,#67534,#67535,#67536,
#67537,#67538,#67539,#67540,#67541,#67542,#67543,#67544,#67545,#67546,#67547,
#67548,#67549,#67550,#67551,#67552,#67553,#67554,#67555,#67556,#67557,#67558,
#67559,#67560,#67561,#67562,#67563,#67564,#67565,#67566,#67567,#67568,#67569,
#67570,#67571,#67572,#67573,#67574,#67575,#67576,#67577,#67578,#67579,#67580,
#67581,#67582,#67583));
#13996=EDGE_LOOP('',(#67584));
#13997=EDGE_LOOP('',(#67585,#67586,#67587,#67588));
#13998=EDGE_LOOP('',(#67589,#67590,#67591,#67592));
#13999=EDGE_LOOP('',(#67593,#67594,#67595,#67596));
#14000=EDGE_LOOP('',(#67597,#67598,#67599,#67600));
#14001=EDGE_LOOP('',(#67601,#67602,#67603,#67604));
#14002=EDGE_LOOP('',(#67605,#67606,#67607,#67608));
#14003=EDGE_LOOP('',(#67609,#67610,#67611,#67612,#67613,#67614,#67615,#67616,
#67617,#67618,#67619,#67620,#67621,#67622,#67623,#67624,#67625,#67626,#67627,
#67628,#67629,#67630,#67631,#67632,#67633,#67634,#67635,#67636,#67637,#67638,
#67639,#67640,#67641,#67642,#67643,#67644,#67645,#67646,#67647,#67648,#67649,
#67650,#67651,#67652,#67653,#67654,#67655,#67656,#67657,#67658,#67659,#67660,
#67661,#67662,#67663,#67664,#67665,#67666,#67667,#67668,#67669,#67670,#67671,
#67672,#67673,#67674,#67675,#67676,#67677,#67678,#67679,#67680,#67681,#67682,
#67683,#67684,#67685,#67686,#67687,#67688,#67689,#67690,#67691,#67692,#67693,
#67694,#67695,#67696,#67697,#67698,#67699,#67700,#67701,#67702,#67703,#67704,
#67705,#67706,#67707,#67708,#67709,#67710,#67711,#67712,#67713,#67714,#67715,
#67716,#67717,#67718,#67719,#67720,#67721,#67722,#67723,#67724,#67725,#67726,
#67727,#67728,#67729,#67730,#67731,#67732,#67733,#67734,#67735,#67736,#67737,
#67738,#67739,#67740,#67741,#67742,#67743,#67744,#67745,#67746,#67747,#67748,
#67749,#67750,#67751,#67752,#67753,#67754,#67755,#67756,#67757,#67758,#67759,
#67760,#67761,#67762,#67763,#67764,#67765,#67766,#67767,#67768,#67769,#67770,
#67771,#67772,#67773,#67774,#67775,#67776,#67777,#67778,#67779,#67780,#67781,
#67782,#67783,#67784));
#14004=EDGE_LOOP('',(#67785));
#14005=EDGE_LOOP('',(#67786,#67787,#67788,#67789));
#14006=EDGE_LOOP('',(#67790,#67791,#67792,#67793));
#14007=EDGE_LOOP('',(#67794));
#14008=EDGE_LOOP('',(#67795));
#14009=EDGE_LOOP('',(#67796,#67797,#67798,#67799,#67800,#67801,#67802,#67803,
#67804,#67805,#67806,#67807,#67808,#67809,#67810,#67811,#67812,#67813,#67814,
#67815,#67816,#67817,#67818,#67819,#67820,#67821,#67822,#67823,#67824,#67825,
#67826,#67827,#67828,#67829,#67830,#67831,#67832,#67833,#67834,#67835,#67836,
#67837,#67838,#67839,#67840,#67841,#67842,#67843,#67844,#67845,#67846,#67847,
#67848,#67849,#67850,#67851,#67852,#67853,#67854,#67855,#67856,#67857,#67858,
#67859,#67860,#67861,#67862,#67863,#67864,#67865,#67866,#67867,#67868,#67869,
#67870,#67871,#67872,#67873,#67874,#67875,#67876,#67877,#67878,#67879,#67880,
#67881,#67882,#67883,#67884,#67885,#67886,#67887,#67888,#67889,#67890,#67891,
#67892,#67893,#67894,#67895,#67896,#67897));
#14010=EDGE_LOOP('',(#67898));
#14011=EDGE_LOOP('',(#67899,#67900,#67901,#67902));
#14012=EDGE_LOOP('',(#67903));
#14013=EDGE_LOOP('',(#67904));
#14014=EDGE_LOOP('',(#67905,#67906,#67907,#67908));
#14015=EDGE_LOOP('',(#67909,#67910,#67911,#67912));
#14016=EDGE_LOOP('',(#67913,#67914,#67915,#67916));
#14017=EDGE_LOOP('',(#67917,#67918,#67919,#67920));
#14018=EDGE_LOOP('',(#67921,#67922,#67923,#67924));
#14019=EDGE_LOOP('',(#67925,#67926,#67927,#67928));
#14020=EDGE_LOOP('',(#67929,#67930,#67931,#67932));
#14021=EDGE_LOOP('',(#67933,#67934,#67935,#67936));
#14022=EDGE_LOOP('',(#67937,#67938,#67939,#67940));
#14023=EDGE_LOOP('',(#67941,#67942,#67943,#67944));
#14024=EDGE_LOOP('',(#67945,#67946,#67947,#67948));
#14025=EDGE_LOOP('',(#67949,#67950,#67951,#67952));
#14026=EDGE_LOOP('',(#67953,#67954,#67955,#67956));
#14027=EDGE_LOOP('',(#67957,#67958,#67959,#67960));
#14028=EDGE_LOOP('',(#67961,#67962,#67963,#67964));
#14029=EDGE_LOOP('',(#67965,#67966,#67967,#67968));
#14030=EDGE_LOOP('',(#67969,#67970,#67971,#67972));
#14031=EDGE_LOOP('',(#67973,#67974,#67975,#67976));
#14032=EDGE_LOOP('',(#67977,#67978,#67979,#67980));
#14033=EDGE_LOOP('',(#67981,#67982,#67983,#67984));
#14034=EDGE_LOOP('',(#67985,#67986,#67987,#67988));
#14035=EDGE_LOOP('',(#67989,#67990,#67991,#67992));
#14036=EDGE_LOOP('',(#67993,#67994,#67995,#67996));
#14037=EDGE_LOOP('',(#67997,#67998,#67999,#68000));
#14038=EDGE_LOOP('',(#68001,#68002,#68003,#68004));
#14039=EDGE_LOOP('',(#68005,#68006,#68007,#68008));
#14040=EDGE_LOOP('',(#68009,#68010,#68011,#68012));
#14041=EDGE_LOOP('',(#68013,#68014,#68015,#68016));
#14042=EDGE_LOOP('',(#68017,#68018,#68019,#68020));
#14043=EDGE_LOOP('',(#68021,#68022,#68023,#68024));
#14044=EDGE_LOOP('',(#68025,#68026,#68027,#68028));
#14045=EDGE_LOOP('',(#68029,#68030,#68031,#68032));
#14046=EDGE_LOOP('',(#68033,#68034,#68035,#68036));
#14047=EDGE_LOOP('',(#68037,#68038,#68039,#68040));
#14048=EDGE_LOOP('',(#68041,#68042,#68043,#68044));
#14049=EDGE_LOOP('',(#68045,#68046,#68047,#68048));
#14050=EDGE_LOOP('',(#68049,#68050,#68051,#68052));
#14051=EDGE_LOOP('',(#68053,#68054,#68055,#68056));
#14052=EDGE_LOOP('',(#68057,#68058,#68059,#68060));
#14053=EDGE_LOOP('',(#68061,#68062,#68063,#68064));
#14054=EDGE_LOOP('',(#68065,#68066,#68067,#68068));
#14055=EDGE_LOOP('',(#68069,#68070,#68071,#68072));
#14056=EDGE_LOOP('',(#68073,#68074,#68075,#68076));
#14057=EDGE_LOOP('',(#68077,#68078,#68079,#68080));
#14058=EDGE_LOOP('',(#68081,#68082,#68083,#68084));
#14059=EDGE_LOOP('',(#68085,#68086,#68087,#68088));
#14060=EDGE_LOOP('',(#68089,#68090,#68091,#68092));
#14061=EDGE_LOOP('',(#68093,#68094,#68095,#68096));
#14062=EDGE_LOOP('',(#68097,#68098,#68099,#68100));
#14063=EDGE_LOOP('',(#68101,#68102,#68103,#68104));
#14064=EDGE_LOOP('',(#68105,#68106,#68107,#68108));
#14065=EDGE_LOOP('',(#68109,#68110,#68111,#68112,#68113,#68114,#68115,#68116,
#68117,#68118,#68119,#68120,#68121,#68122,#68123,#68124,#68125,#68126,#68127,
#68128,#68129,#68130,#68131,#68132,#68133,#68134,#68135,#68136,#68137,#68138,
#68139,#68140,#68141,#68142,#68143,#68144,#68145,#68146,#68147,#68148,#68149,
#68150,#68151,#68152,#68153,#68154,#68155,#68156,#68157,#68158,#68159,#68160,
#68161,#68162,#68163,#68164,#68165,#68166,#68167,#68168,#68169,#68170,#68171,
#68172,#68173,#68174,#68175,#68176,#68177,#68178,#68179,#68180,#68181,#68182,
#68183,#68184,#68185,#68186,#68187,#68188,#68189,#68190,#68191,#68192,#68193,
#68194,#68195,#68196,#68197,#68198,#68199,#68200,#68201,#68202,#68203,#68204,
#68205,#68206,#68207,#68208,#68209,#68210));
#14066=EDGE_LOOP('',(#68211));
#14067=EDGE_LOOP('',(#68212,#68213,#68214,#68215));
#14068=EDGE_LOOP('',(#68216,#68217,#68218,#68219));
#14069=EDGE_LOOP('',(#68220,#68221,#68222,#68223));
#14070=EDGE_LOOP('',(#68224,#68225,#68226,#68227));
#14071=EDGE_LOOP('',(#68228,#68229,#68230,#68231));
#14072=EDGE_LOOP('',(#68232,#68233,#68234,#68235));
#14073=EDGE_LOOP('',(#68236,#68237,#68238,#68239));
#14074=EDGE_LOOP('',(#68240,#68241,#68242,#68243));
#14075=EDGE_LOOP('',(#68244,#68245,#68246,#68247));
#14076=EDGE_LOOP('',(#68248,#68249,#68250,#68251));
#14077=EDGE_LOOP('',(#68252,#68253,#68254,#68255));
#14078=EDGE_LOOP('',(#68256,#68257,#68258,#68259));
#14079=EDGE_LOOP('',(#68260,#68261,#68262,#68263));
#14080=EDGE_LOOP('',(#68264,#68265,#68266,#68267));
#14081=EDGE_LOOP('',(#68268,#68269,#68270,#68271));
#14082=EDGE_LOOP('',(#68272,#68273,#68274,#68275));
#14083=EDGE_LOOP('',(#68276,#68277,#68278,#68279));
#14084=EDGE_LOOP('',(#68280,#68281,#68282,#68283));
#14085=EDGE_LOOP('',(#68284,#68285,#68286,#68287));
#14086=EDGE_LOOP('',(#68288,#68289,#68290,#68291));
#14087=EDGE_LOOP('',(#68292,#68293,#68294,#68295));
#14088=EDGE_LOOP('',(#68296,#68297,#68298,#68299));
#14089=EDGE_LOOP('',(#68300,#68301,#68302,#68303));
#14090=EDGE_LOOP('',(#68304,#68305,#68306,#68307));
#14091=EDGE_LOOP('',(#68308,#68309,#68310,#68311));
#14092=EDGE_LOOP('',(#68312,#68313,#68314,#68315));
#14093=EDGE_LOOP('',(#68316,#68317,#68318,#68319));
#14094=EDGE_LOOP('',(#68320,#68321,#68322,#68323));
#14095=EDGE_LOOP('',(#68324,#68325,#68326,#68327));
#14096=EDGE_LOOP('',(#68328,#68329,#68330,#68331));
#14097=EDGE_LOOP('',(#68332,#68333,#68334,#68335));
#14098=EDGE_LOOP('',(#68336,#68337,#68338,#68339));
#14099=EDGE_LOOP('',(#68340,#68341,#68342,#68343));
#14100=EDGE_LOOP('',(#68344,#68345,#68346,#68347));
#14101=EDGE_LOOP('',(#68348,#68349,#68350,#68351));
#14102=EDGE_LOOP('',(#68352,#68353,#68354,#68355));
#14103=EDGE_LOOP('',(#68356,#68357,#68358,#68359));
#14104=EDGE_LOOP('',(#68360,#68361,#68362,#68363));
#14105=EDGE_LOOP('',(#68364,#68365,#68366,#68367));
#14106=EDGE_LOOP('',(#68368,#68369,#68370,#68371));
#14107=EDGE_LOOP('',(#68372,#68373,#68374,#68375));
#14108=EDGE_LOOP('',(#68376,#68377,#68378,#68379));
#14109=EDGE_LOOP('',(#68380,#68381,#68382,#68383));
#14110=EDGE_LOOP('',(#68384,#68385,#68386,#68387));
#14111=EDGE_LOOP('',(#68388,#68389,#68390,#68391));
#14112=EDGE_LOOP('',(#68392,#68393,#68394,#68395));
#14113=EDGE_LOOP('',(#68396,#68397,#68398,#68399));
#14114=EDGE_LOOP('',(#68400,#68401,#68402,#68403));
#14115=EDGE_LOOP('',(#68404,#68405,#68406,#68407));
#14116=EDGE_LOOP('',(#68408,#68409,#68410,#68411));
#14117=EDGE_LOOP('',(#68412,#68413,#68414,#68415));
#14118=EDGE_LOOP('',(#68416,#68417,#68418,#68419));
#14119=EDGE_LOOP('',(#68420));
#14120=EDGE_LOOP('',(#68421));
#14121=EDGE_LOOP('',(#68422,#68423,#68424,#68425));
#14122=EDGE_LOOP('',(#68426));
#14123=EDGE_LOOP('',(#68427));
#14124=EDGE_LOOP('',(#68428,#68429,#68430,#68431,#68432,#68433,#68434,#68435,
#68436,#68437,#68438,#68439,#68440));
#14125=EDGE_LOOP('',(#68441,#68442,#68443,#68444));
#14126=EDGE_LOOP('',(#68445,#68446,#68447,#68448));
#14127=EDGE_LOOP('',(#68449,#68450,#68451,#68452));
#14128=EDGE_LOOP('',(#68453,#68454,#68455,#68456));
#14129=EDGE_LOOP('',(#68457,#68458,#68459,#68460));
#14130=EDGE_LOOP('',(#68461,#68462,#68463,#68464));
#14131=EDGE_LOOP('',(#68465,#68466,#68467,#68468));
#14132=EDGE_LOOP('',(#68469,#68470,#68471,#68472,#68473));
#14133=EDGE_LOOP('',(#68474,#68475,#68476,#68477,#68478,#68479,#68480,#68481,
#68482,#68483,#68484,#68485,#68486));
#14134=EDGE_LOOP('',(#68487,#68488,#68489,#68490));
#14135=EDGE_LOOP('',(#68491,#68492,#68493,#68494));
#14136=EDGE_LOOP('',(#68495,#68496,#68497,#68498));
#14137=EDGE_LOOP('',(#68499,#68500,#68501,#68502));
#14138=EDGE_LOOP('',(#68503,#68504,#68505,#68506));
#14139=EDGE_LOOP('',(#68507,#68508,#68509,#68510));
#14140=EDGE_LOOP('',(#68511,#68512,#68513,#68514));
#14141=EDGE_LOOP('',(#68515,#68516,#68517,#68518));
#14142=EDGE_LOOP('',(#68519));
#14143=EDGE_LOOP('',(#68520));
#14144=EDGE_LOOP('',(#68521,#68522,#68523,#68524,#68525));
#14145=EDGE_LOOP('',(#68526,#68527,#68528,#68529));
#14146=EDGE_LOOP('',(#68530,#68531,#68532,#68533));
#14147=EDGE_LOOP('',(#68534,#68535,#68536,#68537));
#14148=EDGE_LOOP('',(#68538,#68539,#68540,#68541));
#14149=EDGE_LOOP('',(#68542,#68543,#68544,#68545));
#14150=EDGE_LOOP('',(#68546,#68547,#68548,#68549));
#14151=EDGE_LOOP('',(#68550,#68551,#68552,#68553));
#14152=EDGE_LOOP('',(#68554,#68555,#68556,#68557));
#14153=EDGE_LOOP('',(#68558,#68559,#68560,#68561));
#14154=EDGE_LOOP('',(#68562,#68563,#68564,#68565));
#14155=EDGE_LOOP('',(#68566,#68567,#68568,#68569));
#14156=EDGE_LOOP('',(#68570,#68571,#68572,#68573));
#14157=EDGE_LOOP('',(#68574,#68575,#68576,#68577,#68578,#68579));
#14158=EDGE_LOOP('',(#68580,#68581,#68582,#68583));
#14159=EDGE_LOOP('',(#68584,#68585,#68586,#68587,#68588,#68589));
#14160=EDGE_LOOP('',(#68590,#68591,#68592,#68593));
#14161=EDGE_LOOP('',(#68594,#68595,#68596,#68597));
#14162=EDGE_LOOP('',(#68598,#68599,#68600,#68601));
#14163=EDGE_LOOP('',(#68602,#68603,#68604,#68605));
#14164=EDGE_LOOP('',(#68606,#68607,#68608,#68609));
#14165=EDGE_LOOP('',(#68610,#68611,#68612,#68613));
#14166=EDGE_LOOP('',(#68614,#68615,#68616,#68617));
#14167=EDGE_LOOP('',(#68618,#68619,#68620,#68621));
#14168=EDGE_LOOP('',(#68622,#68623,#68624,#68625));
#14169=EDGE_LOOP('',(#68626,#68627,#68628,#68629));
#14170=EDGE_LOOP('',(#68630,#68631,#68632,#68633));
#14171=EDGE_LOOP('',(#68634,#68635,#68636,#68637));
#14172=EDGE_LOOP('',(#68638,#68639,#68640,#68641));
#14173=EDGE_LOOP('',(#68642,#68643,#68644,#68645));
#14174=EDGE_LOOP('',(#68646,#68647,#68648,#68649));
#14175=EDGE_LOOP('',(#68650,#68651,#68652,#68653));
#14176=EDGE_LOOP('',(#68654,#68655,#68656,#68657));
#14177=EDGE_LOOP('',(#68658,#68659,#68660,#68661));
#14178=EDGE_LOOP('',(#68662,#68663,#68664,#68665));
#14179=EDGE_LOOP('',(#68666));
#14180=EDGE_LOOP('',(#68667,#68668,#68669,#68670));
#14181=EDGE_LOOP('',(#68671));
#14182=EDGE_LOOP('',(#68672,#68673,#68674,#68675));
#14183=EDGE_LOOP('',(#68676,#68677,#68678,#68679));
#14184=EDGE_LOOP('',(#68680));
#14185=EDGE_LOOP('',(#68681,#68682,#68683,#68684));
#14186=EDGE_LOOP('',(#68685));
#14187=EDGE_LOOP('',(#68686,#68687,#68688,#68689));
#14188=EDGE_LOOP('',(#68690,#68691,#68692,#68693));
#14189=EDGE_LOOP('',(#68694));
#14190=EDGE_LOOP('',(#68695,#68696,#68697,#68698));
#14191=EDGE_LOOP('',(#68699));
#14192=EDGE_LOOP('',(#68700,#68701,#68702,#68703));
#14193=EDGE_LOOP('',(#68704,#68705,#68706,#68707));
#14194=EDGE_LOOP('',(#68708));
#14195=EDGE_LOOP('',(#68709,#68710,#68711,#68712));
#14196=EDGE_LOOP('',(#68713));
#14197=EDGE_LOOP('',(#68714,#68715,#68716,#68717));
#14198=EDGE_LOOP('',(#68718,#68719,#68720,#68721));
#14199=EDGE_LOOP('',(#68722));
#14200=EDGE_LOOP('',(#68723,#68724,#68725,#68726));
#14201=EDGE_LOOP('',(#68727));
#14202=EDGE_LOOP('',(#68728,#68729,#68730,#68731));
#14203=EDGE_LOOP('',(#68732,#68733,#68734,#68735));
#14204=EDGE_LOOP('',(#68736));
#14205=EDGE_LOOP('',(#68737,#68738,#68739,#68740));
#14206=EDGE_LOOP('',(#68741));
#14207=EDGE_LOOP('',(#68742,#68743,#68744,#68745));
#14208=EDGE_LOOP('',(#68746,#68747,#68748,#68749));
#14209=EDGE_LOOP('',(#68750));
#14210=EDGE_LOOP('',(#68751,#68752,#68753,#68754));
#14211=EDGE_LOOP('',(#68755));
#14212=EDGE_LOOP('',(#68756,#68757,#68758,#68759));
#14213=EDGE_LOOP('',(#68760,#68761,#68762,#68763));
#14214=EDGE_LOOP('',(#68764));
#14215=EDGE_LOOP('',(#68765,#68766,#68767,#68768));
#14216=EDGE_LOOP('',(#68769));
#14217=EDGE_LOOP('',(#68770,#68771,#68772,#68773));
#14218=EDGE_LOOP('',(#68774,#68775,#68776,#68777));
#14219=EDGE_LOOP('',(#68778,#68779,#68780,#68781));
#14220=EDGE_LOOP('',(#68782,#68783,#68784,#68785));
#14221=EDGE_LOOP('',(#68786,#68787,#68788,#68789));
#14222=EDGE_LOOP('',(#68790,#68791,#68792,#68793));
#14223=EDGE_LOOP('',(#68794,#68795,#68796,#68797));
#14224=EDGE_LOOP('',(#68798,#68799,#68800,#68801));
#14225=EDGE_LOOP('',(#68802,#68803,#68804,#68805));
#14226=EDGE_LOOP('',(#68806,#68807,#68808,#68809));
#14227=EDGE_LOOP('',(#68810,#68811,#68812,#68813));
#14228=EDGE_LOOP('',(#68814,#68815,#68816,#68817));
#14229=EDGE_LOOP('',(#68818,#68819,#68820,#68821));
#14230=EDGE_LOOP('',(#68822,#68823,#68824,#68825));
#14231=EDGE_LOOP('',(#68826,#68827,#68828,#68829));
#14232=EDGE_LOOP('',(#68830,#68831,#68832,#68833));
#14233=EDGE_LOOP('',(#68834,#68835,#68836,#68837));
#14234=EDGE_LOOP('',(#68838,#68839,#68840,#68841));
#14235=EDGE_LOOP('',(#68842,#68843,#68844,#68845));
#14236=EDGE_LOOP('',(#68846,#68847,#68848,#68849));
#14237=EDGE_LOOP('',(#68850,#68851,#68852,#68853));
#14238=EDGE_LOOP('',(#68854,#68855,#68856,#68857));
#14239=EDGE_LOOP('',(#68858,#68859,#68860,#68861));
#14240=EDGE_LOOP('',(#68862,#68863,#68864,#68865));
#14241=EDGE_LOOP('',(#68866,#68867,#68868,#68869));
#14242=EDGE_LOOP('',(#68870,#68871,#68872,#68873));
#14243=EDGE_LOOP('',(#68874,#68875,#68876,#68877));
#14244=EDGE_LOOP('',(#68878,#68879,#68880,#68881));
#14245=EDGE_LOOP('',(#68882,#68883,#68884,#68885));
#14246=EDGE_LOOP('',(#68886,#68887,#68888,#68889));
#14247=EDGE_LOOP('',(#68890,#68891,#68892,#68893));
#14248=EDGE_LOOP('',(#68894,#68895,#68896,#68897,#68898));
#14249=EDGE_LOOP('',(#68899,#68900,#68901,#68902));
#14250=EDGE_LOOP('',(#68903,#68904,#68905,#68906));
#14251=EDGE_LOOP('',(#68907,#68908,#68909,#68910));
#14252=EDGE_LOOP('',(#68911,#68912,#68913,#68914));
#14253=EDGE_LOOP('',(#68915,#68916,#68917,#68918));
#14254=EDGE_LOOP('',(#68919,#68920,#68921,#68922));
#14255=EDGE_LOOP('',(#68923,#68924,#68925,#68926));
#14256=EDGE_LOOP('',(#68927,#68928,#68929,#68930));
#14257=EDGE_LOOP('',(#68931,#68932,#68933,#68934));
#14258=EDGE_LOOP('',(#68935,#68936,#68937,#68938));
#14259=EDGE_LOOP('',(#68939,#68940,#68941,#68942));
#14260=EDGE_LOOP('',(#68943,#68944,#68945,#68946));
#14261=EDGE_LOOP('',(#68947,#68948,#68949,#68950));
#14262=EDGE_LOOP('',(#68951,#68952,#68953,#68954));
#14263=EDGE_LOOP('',(#68955,#68956,#68957,#68958));
#14264=EDGE_LOOP('',(#68959,#68960,#68961,#68962));
#14265=EDGE_LOOP('',(#68963,#68964,#68965,#68966));
#14266=EDGE_LOOP('',(#68967,#68968,#68969,#68970));
#14267=EDGE_LOOP('',(#68971,#68972,#68973,#68974));
#14268=EDGE_LOOP('',(#68975,#68976,#68977,#68978));
#14269=EDGE_LOOP('',(#68979,#68980,#68981,#68982));
#14270=EDGE_LOOP('',(#68983,#68984,#68985,#68986));
#14271=EDGE_LOOP('',(#68987,#68988,#68989,#68990));
#14272=EDGE_LOOP('',(#68991,#68992,#68993,#68994));
#14273=EDGE_LOOP('',(#68995,#68996,#68997,#68998));
#14274=EDGE_LOOP('',(#68999,#69000,#69001,#69002));
#14275=EDGE_LOOP('',(#69003,#69004,#69005,#69006));
#14276=EDGE_LOOP('',(#69007,#69008,#69009,#69010));
#14277=EDGE_LOOP('',(#69011,#69012,#69013,#69014));
#14278=EDGE_LOOP('',(#69015,#69016,#69017,#69018));
#14279=EDGE_LOOP('',(#69019,#69020,#69021,#69022));
#14280=EDGE_LOOP('',(#69023,#69024));
#14281=EDGE_LOOP('',(#69025));
#14282=EDGE_LOOP('',(#69026));
#14283=EDGE_LOOP('',(#69027,#69028,#69029,#69030));
#14284=EDGE_LOOP('',(#69031,#69032,#69033,#69034,#69035,#69036,#69037,#69038,
#69039));
#14285=EDGE_LOOP('',(#69040,#69041,#69042,#69043,#69044));
#14286=EDGE_LOOP('',(#69045));
#14287=EDGE_LOOP('',(#69046));
#14288=EDGE_LOOP('',(#69047,#69048,#69049,#69050));
#14289=EDGE_LOOP('',(#69051));
#14290=EDGE_LOOP('',(#69052));
#14291=EDGE_LOOP('',(#69053));
#14292=EDGE_LOOP('',(#69054,#69055,#69056,#69057,#69058,#69059));
#14293=EDGE_LOOP('',(#69060,#69061));
#14294=EDGE_LOOP('',(#69062,#69063));
#14295=EDGE_LOOP('',(#69064,#69065));
#14296=EDGE_LOOP('',(#69066,#69067));
#14297=EDGE_LOOP('',(#69068,#69069));
#14298=EDGE_LOOP('',(#69070,#69071,#69072,#69073,#69074,#69075));
#14299=EDGE_LOOP('',(#69076,#69077,#69078,#69079));
#14300=EDGE_LOOP('',(#69080,#69081,#69082,#69083));
#14301=EDGE_LOOP('',(#69084,#69085,#69086,#69087));
#14302=EDGE_LOOP('',(#69088,#69089,#69090,#69091));
#14303=EDGE_LOOP('',(#69092,#69093,#69094,#69095));
#14304=EDGE_LOOP('',(#69096,#69097,#69098,#69099));
#14305=EDGE_LOOP('',(#69100,#69101,#69102,#69103,#69104,#69105,#69106,#69107,
#69108,#69109,#69110,#69111,#69112,#69113,#69114,#69115,#69116,#69117,#69118,
#69119,#69120,#69121,#69122,#69123,#69124,#69125,#69126,#69127,#69128,#69129,
#69130,#69131,#69132,#69133,#69134,#69135,#69136,#69137,#69138,#69139,#69140,
#69141,#69142,#69143,#69144,#69145,#69146,#69147,#69148,#69149,#69150,#69151,
#69152,#69153,#69154,#69155,#69156,#69157,#69158,#69159,#69160,#69161,#69162,
#69163,#69164,#69165,#69166,#69167));
#14306=EDGE_LOOP('',(#69168,#69169,#69170));
#14307=EDGE_LOOP('',(#69171,#69172,#69173,#69174,#69175,#69176,#69177,#69178,
#69179,#69180,#69181,#69182,#69183,#69184,#69185,#69186,#69187,#69188,#69189,
#69190,#69191,#69192,#69193,#69194,#69195,#69196,#69197,#69198,#69199,#69200,
#69201,#69202,#69203,#69204,#69205,#69206,#69207,#69208,#69209,#69210,#69211,
#69212,#69213,#69214,#69215,#69216,#69217,#69218,#69219,#69220,#69221,#69222,
#69223,#69224,#69225,#69226,#69227,#69228,#69229,#69230,#69231,#69232,#69233,
#69234,#69235,#69236,#69237));
#14308=EDGE_LOOP('',(#69238,#69239,#69240,#69241,#69242));
#14309=EDGE_LOOP('',(#69243,#69244,#69245,#69246,#69247,#69248));
#14310=EDGE_LOOP('',(#69249,#69250,#69251,#69252,#69253));
#14311=EDGE_LOOP('',(#69254,#69255,#69256,#69257,#69258));
#14312=EDGE_LOOP('',(#69259,#69260));
#14313=EDGE_LOOP('',(#69261,#69262,#69263,#69264,#69265,#69266));
#14314=EDGE_LOOP('',(#69267,#69268));
#14315=EDGE_LOOP('',(#69269,#69270,#69271,#69272,#69273));
#14316=EDGE_LOOP('',(#69274,#69275,#69276,#69277));
#14317=EDGE_LOOP('',(#69278,#69279,#69280,#69281));
#14318=EDGE_LOOP('',(#69282,#69283,#69284,#69285));
#14319=EDGE_LOOP('',(#69286,#69287,#69288,#69289));
#14320=EDGE_LOOP('',(#69290,#69291,#69292,#69293,#69294));
#14321=EDGE_LOOP('',(#69295,#69296,#69297,#69298,#69299));
#14322=EDGE_LOOP('',(#69300));
#14323=EDGE_LOOP('',(#69301));
#14324=EDGE_LOOP('',(#69302));
#14325=EDGE_LOOP('',(#69303));
#14326=EDGE_LOOP('',(#69304,#69305,#69306,#69307));
#14327=EDGE_LOOP('',(#69308,#69309,#69310,#69311));
#14328=EDGE_LOOP('',(#69312,#69313,#69314,#69315,#69316));
#14329=EDGE_LOOP('',(#69317,#69318,#69319,#69320,#69321));
#14330=EDGE_LOOP('',(#69322,#69323,#69324,#69325));
#14331=EDGE_LOOP('',(#69326,#69327,#69328,#69329));
#14332=EDGE_LOOP('',(#69330));
#14333=EDGE_LOOP('',(#69331));
#14334=EDGE_LOOP('',(#69332));
#14335=EDGE_LOOP('',(#69333));
#14336=EDGE_LOOP('',(#69334,#69335));
#14337=EDGE_LOOP('',(#69336,#69337));
#14338=EDGE_LOOP('',(#69338,#69339));
#14339=EDGE_LOOP('',(#69340,#69341));
#14340=EDGE_LOOP('',(#69342,#69343));
#14341=EDGE_LOOP('',(#69344,#69345));
#14342=EDGE_LOOP('',(#69346,#69347));
#14343=EDGE_LOOP('',(#69348,#69349));
#14344=EDGE_LOOP('',(#69350,#69351));
#14345=EDGE_LOOP('',(#69352,#69353));
#14346=EDGE_LOOP('',(#69354,#69355));
#14347=EDGE_LOOP('',(#69356,#69357));
#14348=EDGE_LOOP('',(#69358,#69359,#69360,#69361));
#14349=EDGE_LOOP('',(#69362,#69363,#69364,#69365));
#14350=EDGE_LOOP('',(#69366));
#14351=EDGE_LOOP('',(#69367));
#14352=EDGE_LOOP('',(#69368));
#14353=EDGE_LOOP('',(#69369));
#14354=EDGE_LOOP('',(#69370,#69371,#69372,#69373));
#14355=EDGE_LOOP('',(#69374,#69375,#69376,#69377));
#14356=EDGE_LOOP('',(#69378));
#14357=EDGE_LOOP('',(#69379));
#14358=EDGE_LOOP('',(#69380));
#14359=EDGE_LOOP('',(#69381));
#14360=EDGE_LOOP('',(#69382,#69383,#69384));
#14361=EDGE_LOOP('',(#69385,#69386,#69387,#69388,#69389));
#14362=EDGE_LOOP('',(#69390,#69391,#69392,#69393));
#14363=EDGE_LOOP('',(#69394,#69395,#69396,#69397));
#14364=EDGE_LOOP('',(#69398,#69399,#69400,#69401));
#14365=EDGE_LOOP('',(#69402,#69403,#69404,#69405));
#14366=EDGE_LOOP('',(#69406,#69407,#69408,#69409));
#14367=EDGE_LOOP('',(#69410,#69411,#69412,#69413));
#14368=EDGE_LOOP('',(#69414,#69415,#69416,#69417));
#14369=EDGE_LOOP('',(#69418,#69419,#69420,#69421));
#14370=EDGE_LOOP('',(#69422,#69423,#69424,#69425));
#14371=EDGE_LOOP('',(#69426,#69427,#69428,#69429));
#14372=EDGE_LOOP('',(#69430,#69431,#69432,#69433));
#14373=EDGE_LOOP('',(#69434,#69435,#69436,#69437));
#14374=EDGE_LOOP('',(#69438,#69439,#69440,#69441));
#14375=EDGE_LOOP('',(#69442,#69443,#69444,#69445));
#14376=EDGE_LOOP('',(#69446,#69447,#69448,#69449));
#14377=EDGE_LOOP('',(#69450,#69451,#69452,#69453));
#14378=EDGE_LOOP('',(#69454,#69455,#69456,#69457));
#14379=EDGE_LOOP('',(#69458,#69459,#69460,#69461));
#14380=EDGE_LOOP('',(#69462,#69463,#69464,#69465));
#14381=EDGE_LOOP('',(#69466,#69467,#69468,#69469));
#14382=EDGE_LOOP('',(#69470,#69471,#69472,#69473));
#14383=EDGE_LOOP('',(#69474,#69475,#69476,#69477));
#14384=EDGE_LOOP('',(#69478,#69479,#69480,#69481));
#14385=EDGE_LOOP('',(#69482,#69483,#69484,#69485));
#14386=EDGE_LOOP('',(#69486,#69487,#69488,#69489));
#14387=EDGE_LOOP('',(#69490,#69491,#69492,#69493));
#14388=EDGE_LOOP('',(#69494,#69495,#69496,#69497));
#14389=EDGE_LOOP('',(#69498,#69499,#69500,#69501));
#14390=EDGE_LOOP('',(#69502,#69503,#69504,#69505));
#14391=EDGE_LOOP('',(#69506,#69507));
#14392=EDGE_LOOP('',(#69508));
#14393=EDGE_LOOP('',(#69509));
#14394=EDGE_LOOP('',(#69510,#69511,#69512,#69513));
#14395=EDGE_LOOP('',(#69514,#69515,#69516,#69517,#69518,#69519,#69520,#69521,
#69522));
#14396=EDGE_LOOP('',(#69523,#69524,#69525,#69526));
#14397=EDGE_LOOP('',(#69527));
#14398=EDGE_LOOP('',(#69528));
#14399=EDGE_LOOP('',(#69529,#69530,#69531,#69532));
#14400=EDGE_LOOP('',(#69533));
#14401=EDGE_LOOP('',(#69534));
#14402=EDGE_LOOP('',(#69535));
#14403=EDGE_LOOP('',(#69536,#69537,#69538,#69539,#69540,#69541));
#14404=EDGE_LOOP('',(#69542,#69543));
#14405=EDGE_LOOP('',(#69544,#69545));
#14406=EDGE_LOOP('',(#69546,#69547));
#14407=EDGE_LOOP('',(#69548,#69549));
#14408=EDGE_LOOP('',(#69550,#69551));
#14409=EDGE_LOOP('',(#69552,#69553,#69554,#69555,#69556,#69557));
#14410=EDGE_LOOP('',(#69558,#69559,#69560,#69561));
#14411=EDGE_LOOP('',(#69562,#69563,#69564,#69565));
#14412=EDGE_LOOP('',(#69566,#69567,#69568,#69569));
#14413=EDGE_LOOP('',(#69570,#69571,#69572,#69573));
#14414=EDGE_LOOP('',(#69574,#69575,#69576,#69577));
#14415=EDGE_LOOP('',(#69578,#69579,#69580,#69581));
#14416=EDGE_LOOP('',(#69582,#69583,#69584,#69585,#69586,#69587,#69588,#69589,
#69590,#69591,#69592,#69593,#69594,#69595,#69596,#69597,#69598,#69599,#69600,
#69601,#69602,#69603,#69604,#69605,#69606,#69607,#69608,#69609,#69610,#69611,
#69612,#69613,#69614,#69615,#69616));
#14417=EDGE_LOOP('',(#69617,#69618,#69619,#69620));
#14418=EDGE_LOOP('',(#69621,#69622,#69623,#69624,#69625,#69626,#69627,#69628,
#69629,#69630,#69631,#69632,#69633,#69634,#69635,#69636,#69637,#69638,#69639,
#69640,#69641,#69642,#69643,#69644,#69645,#69646,#69647,#69648,#69649,#69650,
#69651,#69652,#69653,#69654,#69655));
#14419=EDGE_LOOP('',(#69656,#69657,#69658,#69659));
#14420=EDGE_LOOP('',(#69660,#69661,#69662,#69663));
#14421=EDGE_LOOP('',(#69664,#69665,#69666,#69667));
#14422=EDGE_LOOP('',(#69668,#69669,#69670,#69671));
#14423=EDGE_LOOP('',(#69672,#69673,#69674,#69675));
#14424=EDGE_LOOP('',(#69676,#69677,#69678,#69679));
#14425=EDGE_LOOP('',(#69680,#69681,#69682,#69683));
#14426=EDGE_LOOP('',(#69684,#69685,#69686,#69687));
#14427=EDGE_LOOP('',(#69688,#69689,#69690,#69691));
#14428=EDGE_LOOP('',(#69692,#69693,#69694,#69695));
#14429=EDGE_LOOP('',(#69696,#69697,#69698,#69699));
#14430=EDGE_LOOP('',(#69700,#69701,#69702,#69703));
#14431=EDGE_LOOP('',(#69704,#69705,#69706,#69707));
#14432=EDGE_LOOP('',(#69708,#69709,#69710,#69711));
#14433=EDGE_LOOP('',(#69712,#69713,#69714,#69715,#69716));
#14434=EDGE_LOOP('',(#69717,#69718,#69719,#69720));
#14435=EDGE_LOOP('',(#69721,#69722,#69723,#69724));
#14436=EDGE_LOOP('',(#69725,#69726,#69727,#69728));
#14437=EDGE_LOOP('',(#69729,#69730,#69731,#69732));
#14438=EDGE_LOOP('',(#69733,#69734,#69735,#69736));
#14439=EDGE_LOOP('',(#69737,#69738,#69739,#69740));
#14440=EDGE_LOOP('',(#69741,#69742,#69743,#69744));
#14441=EDGE_LOOP('',(#69745,#69746,#69747,#69748));
#14442=EDGE_LOOP('',(#69749,#69750,#69751,#69752));
#14443=EDGE_LOOP('',(#69753,#69754,#69755,#69756));
#14444=EDGE_LOOP('',(#69757,#69758,#69759,#69760));
#14445=EDGE_LOOP('',(#69761,#69762,#69763,#69764));
#14446=EDGE_LOOP('',(#69765,#69766,#69767,#69768));
#14447=EDGE_LOOP('',(#69769,#69770,#69771,#69772));
#14448=EDGE_LOOP('',(#69773,#69774,#69775,#69776,#69777,#69778,#69779,#69780,
#69781));
#14449=EDGE_LOOP('',(#69782,#69783,#69784,#69785));
#14450=EDGE_LOOP('',(#69786,#69787));
#14451=EDGE_LOOP('',(#69788,#69789,#69790,#69791));
#14452=EDGE_LOOP('',(#69792,#69793,#69794,#69795,#69796,#69797,#69798,#69799));
#14453=EDGE_LOOP('',(#69800));
#14454=EDGE_LOOP('',(#69801,#69802,#69803,#69804,#69805,#69806));
#14455=EDGE_LOOP('',(#69807,#69808,#69809,#69810,#69811));
#14456=EDGE_LOOP('',(#69812,#69813));
#14457=EDGE_LOOP('',(#69814,#69815));
#14458=EDGE_LOOP('',(#69816,#69817));
#14459=EDGE_LOOP('',(#69818,#69819));
#14460=EDGE_LOOP('',(#69820,#69821));
#14461=EDGE_LOOP('',(#69822,#69823,#69824,#69825,#69826,#69827));
#14462=EDGE_LOOP('',(#69828,#69829,#69830,#69831));
#14463=EDGE_LOOP('',(#69832,#69833,#69834,#69835));
#14464=EDGE_LOOP('',(#69836,#69837,#69838,#69839));
#14465=EDGE_LOOP('',(#69840,#69841,#69842,#69843));
#14466=EDGE_LOOP('',(#69844,#69845,#69846,#69847));
#14467=EDGE_LOOP('',(#69848,#69849,#69850,#69851));
#14468=EDGE_LOOP('',(#69852));
#14469=EDGE_LOOP('',(#69853,#69854,#69855,#69856,#69857,#69858,#69859,#69860,
#69861,#69862,#69863,#69864,#69865,#69866,#69867,#69868,#69869,#69870,#69871,
#69872,#69873,#69874,#69875,#69876,#69877,#69878,#69879,#69880,#69881,#69882,
#69883,#69884,#69885,#69886));
#14470=EDGE_LOOP('',(#69887,#69888,#69889));
#14471=EDGE_LOOP('',(#69890,#69891,#69892,#69893,#69894,#69895,#69896,#69897,
#69898,#69899,#69900,#69901,#69902,#69903,#69904,#69905,#69906,#69907,#69908,
#69909,#69910,#69911,#69912,#69913,#69914,#69915,#69916,#69917,#69918,#69919,
#69920,#69921,#69922,#69923));
#14472=EDGE_LOOP('',(#69924,#69925,#69926));
#14473=EDGE_LOOP('',(#69927,#69928,#69929,#69930));
#14474=EDGE_LOOP('',(#69931,#69932,#69933,#69934));
#14475=EDGE_LOOP('',(#69935,#69936,#69937,#69938));
#14476=EDGE_LOOP('',(#69939,#69940,#69941,#69942));
#14477=EDGE_LOOP('',(#69943,#69944,#69945,#69946));
#14478=EDGE_LOOP('',(#69947,#69948,#69949,#69950));
#14479=EDGE_LOOP('',(#69951,#69952,#69953,#69954));
#14480=EDGE_LOOP('',(#69955,#69956,#69957,#69958));
#14481=EDGE_LOOP('',(#69959,#69960,#69961,#69962));
#14482=EDGE_LOOP('',(#69963,#69964,#69965,#69966));
#14483=EDGE_LOOP('',(#69967,#69968,#69969,#69970));
#14484=EDGE_LOOP('',(#69971,#69972,#69973,#69974));
#14485=EDGE_LOOP('',(#69975,#69976,#69977,#69978));
#14486=EDGE_LOOP('',(#69979,#69980,#69981,#69982));
#14487=EDGE_LOOP('',(#69983,#69984,#69985,#69986));
#14488=EDGE_LOOP('',(#69987,#69988,#69989,#69990));
#14489=EDGE_LOOP('',(#69991,#69992,#69993,#69994));
#14490=EDGE_LOOP('',(#69995,#69996,#69997,#69998));
#14491=EDGE_LOOP('',(#69999,#70000,#70001,#70002));
#14492=EDGE_LOOP('',(#70003,#70004,#70005,#70006));
#14493=EDGE_LOOP('',(#70007,#70008,#70009,#70010));
#14494=EDGE_LOOP('',(#70011,#70012,#70013,#70014));
#14495=EDGE_LOOP('',(#70015,#70016,#70017,#70018));
#14496=EDGE_LOOP('',(#70019,#70020,#70021,#70022));
#14497=EDGE_LOOP('',(#70023,#70024,#70025,#70026));
#14498=EDGE_LOOP('',(#70027,#70028,#70029,#70030));
#14499=EDGE_LOOP('',(#70031,#70032,#70033,#70034));
#14500=EDGE_LOOP('',(#70035,#70036,#70037,#70038));
#14501=EDGE_LOOP('',(#70039,#70040,#70041,#70042,#70043,#70044,#70045,#70046));
#14502=EDGE_LOOP('',(#70047,#70048,#70049,#70050));
#14503=EDGE_LOOP('',(#70051,#70052,#70053,#70054));
#14504=EDGE_LOOP('',(#70055,#70056,#70057,#70058));
#14505=EDGE_LOOP('',(#70059,#70060,#70061,#70062));
#14506=EDGE_LOOP('',(#70063,#70064,#70065,#70066));
#14507=EDGE_LOOP('',(#70067,#70068,#70069,#70070));
#14508=EDGE_LOOP('',(#70071,#70072,#70073,#70074));
#14509=EDGE_LOOP('',(#70075,#70076,#70077,#70078));
#14510=EDGE_LOOP('',(#70079,#70080,#70081,#70082));
#14511=EDGE_LOOP('',(#70083,#70084,#70085,#70086));
#14512=EDGE_LOOP('',(#70087,#70088,#70089,#70090));
#14513=EDGE_LOOP('',(#70091,#70092,#70093,#70094));
#14514=EDGE_LOOP('',(#70095,#70096,#70097,#70098));
#14515=EDGE_LOOP('',(#70099,#70100,#70101,#70102));
#14516=EDGE_LOOP('',(#70103,#70104,#70105,#70106));
#14517=EDGE_LOOP('',(#70107,#70108,#70109,#70110));
#14518=EDGE_LOOP('',(#70111,#70112,#70113,#70114));
#14519=EDGE_LOOP('',(#70115,#70116,#70117,#70118));
#14520=EDGE_LOOP('',(#70119,#70120,#70121,#70122));
#14521=EDGE_LOOP('',(#70123,#70124,#70125,#70126));
#14522=EDGE_LOOP('',(#70127,#70128,#70129,#70130));
#14523=EDGE_LOOP('',(#70131,#70132,#70133,#70134));
#14524=EDGE_LOOP('',(#70135,#70136,#70137,#70138));
#14525=EDGE_LOOP('',(#70139,#70140,#70141,#70142));
#14526=EDGE_LOOP('',(#70143,#70144,#70145,#70146));
#14527=EDGE_LOOP('',(#70147,#70148,#70149,#70150));
#14528=EDGE_LOOP('',(#70151,#70152,#70153,#70154));
#14529=EDGE_LOOP('',(#70155,#70156,#70157,#70158));
#14530=EDGE_LOOP('',(#70159,#70160,#70161));
#14531=EDGE_LOOP('',(#70162,#70163,#70164,#70165,#70166));
#14532=EDGE_LOOP('',(#70167,#70168,#70169,#70170));
#14533=EDGE_LOOP('',(#70171,#70172,#70173,#70174));
#14534=EDGE_LOOP('',(#70175,#70176,#70177,#70178));
#14535=EDGE_LOOP('',(#70179,#70180,#70181,#70182,#70183,#70184,#70185,#70186));
#14536=EDGE_LOOP('',(#70187,#70188));
#14537=EDGE_LOOP('',(#70189,#70190,#70191,#70192));
#14538=EDGE_LOOP('',(#70193,#70194,#70195,#70196));
#14539=EDGE_LOOP('',(#70197,#70198,#70199,#70200));
#14540=EDGE_LOOP('',(#70201,#70202,#70203,#70204,#70205,#70206,#70207,#70208,
#70209,#70210,#70211,#70212,#70213,#70214,#70215,#70216,#70217,#70218,#70219,
#70220,#70221,#70222,#70223,#70224,#70225,#70226,#70227,#70228,#70229,#70230,
#70231,#70232,#70233,#70234,#70235,#70236,#70237,#70238,#70239,#70240,#70241,
#70242,#70243,#70244,#70245,#70246,#70247,#70248,#70249,#70250,#70251,#70252,
#70253,#70254,#70255,#70256,#70257,#70258,#70259,#70260,#70261,#70262,#70263,
#70264,#70265,#70266,#70267,#70268,#70269,#70270,#70271,#70272,#70273,#70274,
#70275,#70276,#70277,#70278,#70279,#70280,#70281,#70282,#70283,#70284,#70285,
#70286,#70287,#70288,#70289,#70290,#70291,#70292,#70293,#70294,#70295,#70296,
#70297,#70298,#70299,#70300,#70301,#70302,#70303,#70304,#70305,#70306,#70307,
#70308,#70309,#70310,#70311,#70312,#70313,#70314,#70315,#70316,#70317,#70318,
#70319,#70320,#70321,#70322,#70323,#70324,#70325,#70326,#70327,#70328,#70329,
#70330,#70331,#70332,#70333,#70334,#70335,#70336,#70337,#70338,#70339,#70340,
#70341,#70342,#70343,#70344,#70345,#70346,#70347,#70348,#70349,#70350,#70351,
#70352,#70353,#70354,#70355,#70356,#70357,#70358,#70359,#70360,#70361,#70362,
#70363,#70364,#70365,#70366,#70367,#70368,#70369,#70370,#70371,#70372,#70373,
#70374,#70375,#70376,#70377,#70378,#70379,#70380,#70381,#70382,#70383,#70384,
#70385,#70386,#70387,#70388,#70389,#70390,#70391,#70392,#70393,#70394,#70395,
#70396,#70397,#70398,#70399,#70400,#70401,#70402,#70403,#70404,#70405,#70406,
#70407,#70408,#70409,#70410,#70411,#70412,#70413,#70414,#70415,#70416,#70417,
#70418,#70419,#70420,#70421,#70422,#70423,#70424,#70425,#70426,#70427,#70428,
#70429,#70430,#70431,#70432,#70433,#70434,#70435,#70436,#70437,#70438,#70439,
#70440,#70441,#70442,#70443,#70444,#70445,#70446,#70447,#70448,#70449,#70450,
#70451,#70452,#70453,#70454,#70455,#70456,#70457,#70458,#70459,#70460,#70461,
#70462,#70463,#70464,#70465,#70466,#70467,#70468,#70469,#70470,#70471,#70472,
#70473,#70474,#70475,#70476,#70477,#70478,#70479,#70480,#70481,#70482,#70483,
#70484,#70485,#70486,#70487,#70488,#70489,#70490,#70491,#70492,#70493,#70494,
#70495,#70496,#70497,#70498,#70499,#70500,#70501,#70502,#70503,#70504,#70505,
#70506,#70507,#70508,#70509,#70510,#70511,#70512,#70513,#70514,#70515,#70516,
#70517,#70518,#70519,#70520,#70521,#70522,#70523,#70524,#70525,#70526,#70527,
#70528,#70529,#70530,#70531,#70532,#70533,#70534,#70535,#70536,#70537,#70538,
#70539,#70540,#70541,#70542,#70543,#70544,#70545,#70546,#70547,#70548,#70549,
#70550,#70551,#70552,#70553,#70554,#70555,#70556,#70557,#70558,#70559,#70560,
#70561,#70562,#70563,#70564,#70565,#70566,#70567,#70568,#70569,#70570,#70571,
#70572,#70573,#70574,#70575,#70576,#70577,#70578,#70579,#70580,#70581,#70582,
#70583,#70584,#70585,#70586,#70587,#70588,#70589,#70590,#70591,#70592,#70593,
#70594,#70595,#70596,#70597));
#14541=EDGE_LOOP('',(#70598,#70599,#70600,#70601,#70602));
#14542=EDGE_LOOP('',(#70603,#70604,#70605,#70606,#70607,#70608,#70609,#70610,
#70611,#70612,#70613,#70614,#70615,#70616,#70617,#70618,#70619,#70620,#70621,
#70622,#70623,#70624,#70625,#70626,#70627,#70628,#70629,#70630,#70631,#70632,
#70633,#70634,#70635,#70636,#70637,#70638,#70639,#70640,#70641,#70642,#70643,
#70644,#70645,#70646,#70647,#70648,#70649,#70650,#70651,#70652,#70653,#70654,
#70655,#70656,#70657,#70658,#70659,#70660,#70661,#70662,#70663,#70664,#70665,
#70666,#70667,#70668,#70669,#70670,#70671,#70672,#70673,#70674,#70675,#70676,
#70677,#70678,#70679,#70680,#70681,#70682,#70683,#70684,#70685,#70686,#70687,
#70688,#70689,#70690,#70691,#70692,#70693,#70694,#70695,#70696,#70697,#70698,
#70699,#70700,#70701,#70702,#70703,#70704,#70705,#70706,#70707,#70708,#70709,
#70710,#70711,#70712,#70713,#70714,#70715,#70716,#70717,#70718,#70719,#70720,
#70721,#70722,#70723,#70724,#70725,#70726,#70727,#70728,#70729,#70730,#70731,
#70732,#70733,#70734,#70735,#70736,#70737,#70738,#70739,#70740,#70741,#70742,
#70743,#70744,#70745,#70746,#70747,#70748,#70749,#70750,#70751,#70752,#70753,
#70754,#70755,#70756,#70757,#70758,#70759,#70760,#70761,#70762,#70763,#70764,
#70765,#70766,#70767,#70768,#70769,#70770,#70771,#70772,#70773,#70774,#70775,
#70776,#70777,#70778,#70779,#70780,#70781,#70782,#70783,#70784,#70785,#70786,
#70787,#70788,#70789,#70790,#70791,#70792,#70793,#70794,#70795,#70796,#70797,
#70798,#70799,#70800,#70801,#70802,#70803,#70804,#70805,#70806,#70807,#70808,
#70809,#70810,#70811,#70812,#70813,#70814,#70815,#70816,#70817,#70818,#70819,
#70820,#70821,#70822,#70823,#70824,#70825,#70826,#70827,#70828,#70829,#70830,
#70831,#70832,#70833,#70834,#70835,#70836,#70837,#70838,#70839,#70840,#70841,
#70842,#70843,#70844,#70845,#70846,#70847,#70848,#70849,#70850,#70851,#70852,
#70853,#70854,#70855,#70856,#70857,#70858,#70859,#70860,#70861,#70862,#70863,
#70864,#70865,#70866,#70867,#70868,#70869,#70870,#70871,#70872,#70873,#70874,
#70875,#70876,#70877,#70878,#70879,#70880,#70881,#70882,#70883,#70884,#70885,
#70886,#70887,#70888,#70889,#70890,#70891,#70892,#70893,#70894,#70895,#70896,
#70897,#70898,#70899,#70900,#70901,#70902,#70903,#70904,#70905,#70906,#70907,
#70908,#70909,#70910,#70911,#70912,#70913,#70914,#70915,#70916,#70917,#70918,
#70919,#70920,#70921,#70922,#70923,#70924,#70925,#70926,#70927,#70928,#70929,
#70930,#70931,#70932,#70933,#70934,#70935,#70936,#70937,#70938,#70939,#70940,
#70941,#70942,#70943,#70944,#70945,#70946,#70947,#70948,#70949,#70950,#70951,
#70952,#70953,#70954,#70955,#70956,#70957,#70958,#70959,#70960,#70961,#70962,
#70963,#70964,#70965,#70966,#70967,#70968,#70969,#70970,#70971,#70972,#70973,
#70974,#70975,#70976,#70977,#70978,#70979,#70980,#70981,#70982,#70983,#70984,
#70985,#70986,#70987,#70988,#70989,#70990,#70991,#70992,#70993,#70994,#70995,
#70996,#70997,#70998,#70999,#71000,#71001,#71002,#71003,#71004,#71005,#71006,
#71007,#71008,#71009,#71010,#71011,#71012,#71013,#71014,#71015,#71016,#71017,
#71018,#71019,#71020,#71021,#71022,#71023,#71024,#71025,#71026,#71027,#71028,
#71029,#71030,#71031,#71032,#71033,#71034,#71035,#71036,#71037,#71038,#71039,
#71040,#71041,#71042,#71043,#71044,#71045,#71046,#71047,#71048,#71049,#71050,
#71051,#71052,#71053,#71054,#71055,#71056,#71057,#71058,#71059,#71060,#71061,
#71062,#71063,#71064,#71065,#71066,#71067,#71068,#71069,#71070,#71071,#71072,
#71073,#71074,#71075,#71076,#71077,#71078,#71079,#71080,#71081,#71082,#71083,
#71084,#71085,#71086,#71087,#71088,#71089,#71090,#71091,#71092,#71093,#71094,
#71095,#71096,#71097,#71098,#71099,#71100,#71101,#71102,#71103,#71104,#71105,
#71106,#71107,#71108,#71109,#71110,#71111,#71112,#71113,#71114,#71115,#71116,
#71117,#71118,#71119,#71120,#71121,#71122,#71123,#71124,#71125,#71126,#71127,
#71128,#71129,#71130,#71131,#71132,#71133,#71134,#71135,#71136,#71137,#71138,
#71139,#71140,#71141,#71142,#71143,#71144,#71145,#71146,#71147,#71148,#71149,
#71150,#71151,#71152,#71153,#71154,#71155,#71156,#71157,#71158,#71159,#71160,
#71161,#71162,#71163,#71164,#71165,#71166,#71167,#71168,#71169,#71170,#71171,
#71172,#71173,#71174,#71175,#71176,#71177,#71178,#71179,#71180,#71181,#71182,
#71183,#71184,#71185,#71186,#71187,#71188,#71189,#71190,#71191,#71192,#71193,
#71194));
#14543=EDGE_LOOP('',(#71195,#71196,#71197,#71198,#71199));
#14544=EDGE_LOOP('',(#71200,#71201,#71202,#71203));
#14545=EDGE_LOOP('',(#71204,#71205,#71206,#71207));
#14546=EDGE_LOOP('',(#71208,#71209,#71210,#71211));
#14547=EDGE_LOOP('',(#71212,#71213,#71214,#71215));
#14548=EDGE_LOOP('',(#71216,#71217,#71218,#71219));
#14549=EDGE_LOOP('',(#71220,#71221,#71222,#71223));
#14550=EDGE_LOOP('',(#71224,#71225,#71226,#71227));
#14551=EDGE_LOOP('',(#71228,#71229,#71230,#71231));
#14552=EDGE_LOOP('',(#71232,#71233,#71234,#71235));
#14553=EDGE_LOOP('',(#71236,#71237,#71238,#71239));
#14554=EDGE_LOOP('',(#71240,#71241,#71242,#71243));
#14555=EDGE_LOOP('',(#71244,#71245,#71246,#71247));
#14556=EDGE_LOOP('',(#71248,#71249,#71250,#71251));
#14557=EDGE_LOOP('',(#71252,#71253,#71254,#71255));
#14558=EDGE_LOOP('',(#71256,#71257,#71258,#71259));
#14559=EDGE_LOOP('',(#71260,#71261,#71262,#71263));
#14560=EDGE_LOOP('',(#71264,#71265,#71266,#71267));
#14561=EDGE_LOOP('',(#71268,#71269,#71270,#71271));
#14562=EDGE_LOOP('',(#71272,#71273,#71274,#71275));
#14563=EDGE_LOOP('',(#71276,#71277,#71278,#71279));
#14564=EDGE_LOOP('',(#71280,#71281,#71282,#71283));
#14565=EDGE_LOOP('',(#71284,#71285,#71286,#71287));
#14566=EDGE_LOOP('',(#71288,#71289,#71290,#71291));
#14567=EDGE_LOOP('',(#71292,#71293,#71294,#71295));
#14568=EDGE_LOOP('',(#71296,#71297,#71298,#71299));
#14569=EDGE_LOOP('',(#71300,#71301,#71302,#71303));
#14570=EDGE_LOOP('',(#71304,#71305,#71306,#71307));
#14571=EDGE_LOOP('',(#71308,#71309,#71310,#71311));
#14572=EDGE_LOOP('',(#71312,#71313,#71314,#71315));
#14573=EDGE_LOOP('',(#71316,#71317,#71318,#71319));
#14574=EDGE_LOOP('',(#71320,#71321,#71322,#71323));
#14575=EDGE_LOOP('',(#71324,#71325,#71326,#71327));
#14576=EDGE_LOOP('',(#71328,#71329,#71330,#71331));
#14577=EDGE_LOOP('',(#71332,#71333,#71334,#71335));
#14578=EDGE_LOOP('',(#71336,#71337,#71338,#71339));
#14579=EDGE_LOOP('',(#71340,#71341,#71342,#71343));
#14580=EDGE_LOOP('',(#71344,#71345,#71346,#71347));
#14581=EDGE_LOOP('',(#71348,#71349,#71350,#71351));
#14582=EDGE_LOOP('',(#71352,#71353,#71354,#71355));
#14583=EDGE_LOOP('',(#71356,#71357,#71358,#71359));
#14584=EDGE_LOOP('',(#71360,#71361,#71362,#71363));
#14585=EDGE_LOOP('',(#71364,#71365,#71366,#71367,#71368));
#14586=EDGE_LOOP('',(#71369,#71370,#71371,#71372));
#14587=EDGE_LOOP('',(#71373,#71374,#71375,#71376));
#14588=EDGE_LOOP('',(#71377,#71378,#71379,#71380));
#14589=EDGE_LOOP('',(#71381,#71382,#71383,#71384));
#14590=EDGE_LOOP('',(#71385,#71386,#71387,#71388));
#14591=EDGE_LOOP('',(#71389,#71390,#71391,#71392));
#14592=EDGE_LOOP('',(#71393,#71394,#71395,#71396));
#14593=EDGE_LOOP('',(#71397,#71398,#71399,#71400));
#14594=EDGE_LOOP('',(#71401,#71402,#71403,#71404));
#14595=EDGE_LOOP('',(#71405,#71406,#71407,#71408));
#14596=EDGE_LOOP('',(#71409,#71410,#71411,#71412));
#14597=EDGE_LOOP('',(#71413,#71414,#71415,#71416));
#14598=EDGE_LOOP('',(#71417,#71418,#71419,#71420));
#14599=EDGE_LOOP('',(#71421,#71422,#71423,#71424));
#14600=EDGE_LOOP('',(#71425,#71426,#71427,#71428));
#14601=EDGE_LOOP('',(#71429,#71430,#71431,#71432));
#14602=EDGE_LOOP('',(#71433,#71434,#71435,#71436));
#14603=EDGE_LOOP('',(#71437,#71438,#71439,#71440));
#14604=EDGE_LOOP('',(#71441,#71442,#71443,#71444));
#14605=EDGE_LOOP('',(#71445,#71446,#71447,#71448));
#14606=EDGE_LOOP('',(#71449,#71450,#71451,#71452));
#14607=EDGE_LOOP('',(#71453,#71454,#71455,#71456));
#14608=EDGE_LOOP('',(#71457,#71458,#71459,#71460));
#14609=EDGE_LOOP('',(#71461,#71462,#71463,#71464));
#14610=EDGE_LOOP('',(#71465,#71466,#71467,#71468));
#14611=EDGE_LOOP('',(#71469,#71470,#71471,#71472));
#14612=EDGE_LOOP('',(#71473,#71474,#71475,#71476));
#14613=EDGE_LOOP('',(#71477,#71478,#71479,#71480));
#14614=EDGE_LOOP('',(#71481,#71482,#71483,#71484));
#14615=EDGE_LOOP('',(#71485,#71486,#71487,#71488));
#14616=EDGE_LOOP('',(#71489,#71490,#71491,#71492));
#14617=EDGE_LOOP('',(#71493,#71494,#71495,#71496));
#14618=EDGE_LOOP('',(#71497,#71498,#71499,#71500));
#14619=EDGE_LOOP('',(#71501,#71502,#71503,#71504));
#14620=EDGE_LOOP('',(#71505,#71506,#71507,#71508));
#14621=EDGE_LOOP('',(#71509,#71510,#71511,#71512));
#14622=EDGE_LOOP('',(#71513,#71514,#71515,#71516));
#14623=EDGE_LOOP('',(#71517,#71518,#71519,#71520));
#14624=EDGE_LOOP('',(#71521,#71522,#71523,#71524));
#14625=EDGE_LOOP('',(#71525,#71526,#71527,#71528));
#14626=EDGE_LOOP('',(#71529,#71530,#71531,#71532));
#14627=EDGE_LOOP('',(#71533,#71534,#71535,#71536));
#14628=EDGE_LOOP('',(#71537,#71538,#71539,#71540));
#14629=EDGE_LOOP('',(#71541,#71542,#71543,#71544));
#14630=EDGE_LOOP('',(#71545,#71546,#71547,#71548));
#14631=EDGE_LOOP('',(#71549,#71550,#71551,#71552));
#14632=EDGE_LOOP('',(#71553,#71554,#71555,#71556));
#14633=EDGE_LOOP('',(#71557,#71558,#71559,#71560));
#14634=EDGE_LOOP('',(#71561,#71562,#71563,#71564));
#14635=EDGE_LOOP('',(#71565,#71566,#71567,#71568));
#14636=EDGE_LOOP('',(#71569,#71570,#71571,#71572));
#14637=EDGE_LOOP('',(#71573,#71574,#71575,#71576));
#14638=EDGE_LOOP('',(#71577,#71578,#71579,#71580));
#14639=EDGE_LOOP('',(#71581,#71582,#71583,#71584));
#14640=EDGE_LOOP('',(#71585,#71586,#71587,#71588));
#14641=EDGE_LOOP('',(#71589,#71590,#71591,#71592,#71593));
#14642=EDGE_LOOP('',(#71594,#71595,#71596,#71597,#71598));
#14643=EDGE_LOOP('',(#71599,#71600,#71601));
#14644=EDGE_LOOP('',(#71602,#71603,#71604));
#14645=EDGE_LOOP('',(#71605,#71606,#71607));
#14646=EDGE_LOOP('',(#71608,#71609,#71610));
#14647=EDGE_LOOP('',(#71611,#71612,#71613));
#14648=EDGE_LOOP('',(#71614));
#14649=EDGE_LOOP('',(#71615,#71616,#71617,#71618,#71619,#71620));
#14650=EDGE_LOOP('',(#71621,#71622,#71623,#71624));
#14651=EDGE_LOOP('',(#71625,#71626,#71627,#71628,#71629));
#14652=EDGE_LOOP('',(#71630,#71631,#71632,#71633,#71634));
#14653=EDGE_LOOP('',(#71635,#71636,#71637,#71638,#71639));
#14654=EDGE_LOOP('',(#71640,#71641,#71642,#71643,#71644));
#14655=EDGE_LOOP('',(#71645,#71646,#71647,#71648,#71649));
#14656=EDGE_LOOP('',(#71650,#71651,#71652,#71653,#71654));
#14657=EDGE_LOOP('',(#71655,#71656,#71657));
#14658=EDGE_LOOP('',(#71658,#71659));
#14659=EDGE_LOOP('',(#71660,#71661));
#14660=EDGE_LOOP('',(#71662,#71663));
#14661=EDGE_LOOP('',(#71664,#71665));
#14662=EDGE_LOOP('',(#71666,#71667));
#14663=EDGE_LOOP('',(#71668));
#14664=EDGE_LOOP('',(#71669));
#14665=EDGE_LOOP('',(#71670,#71671,#71672));
#14666=EDGE_LOOP('',(#71673,#71674,#71675,#71676));
#14667=EDGE_LOOP('',(#71677,#71678,#71679,#71680,#71681,#71682,#71683,#71684,
#71685,#71686,#71687,#71688,#71689,#71690,#71691,#71692,#71693,#71694,#71695,
#71696,#71697,#71698,#71699,#71700,#71701,#71702,#71703,#71704,#71705,#71706,
#71707,#71708,#71709,#71710,#71711,#71712,#71713,#71714,#71715,#71716,#71717,
#71718,#71719,#71720,#71721,#71722,#71723,#71724,#71725,#71726,#71727,#71728,
#71729,#71730,#71731,#71732,#71733,#71734,#71735,#71736,#71737,#71738));
#14668=EDGE_LOOP('',(#71739,#71740,#71741,#71742,#71743,#71744,#71745,#71746,
#71747,#71748,#71749,#71750,#71751,#71752,#71753,#71754,#71755,#71756,#71757,
#71758,#71759,#71760,#71761,#71762,#71763,#71764,#71765,#71766,#71767,#71768,
#71769,#71770,#71771,#71772,#71773,#71774,#71775,#71776,#71777,#71778,#71779,
#71780,#71781,#71782,#71783,#71784,#71785,#71786,#71787,#71788,#71789,#71790,
#71791,#71792,#71793,#71794,#71795,#71796,#71797,#71798,#71799));
#14669=EDGE_LOOP('',(#71800,#71801,#71802));
#14670=EDGE_LOOP('',(#71803,#71804,#71805,#71806));
#14671=EDGE_LOOP('',(#71807,#71808,#71809,#71810));
#14672=EDGE_LOOP('',(#71811,#71812,#71813));
#14673=EDGE_LOOP('',(#71814,#71815,#71816,#71817));
#14674=EDGE_LOOP('',(#71818,#71819,#71820,#71821));
#14675=EDGE_LOOP('',(#71822,#71823,#71824,#71825));
#14676=EDGE_LOOP('',(#71826,#71827,#71828,#71829));
#14677=EDGE_LOOP('',(#71830,#71831,#71832,#71833));
#14678=EDGE_LOOP('',(#71834,#71835,#71836,#71837));
#14679=EDGE_LOOP('',(#71838,#71839,#71840,#71841));
#14680=EDGE_LOOP('',(#71842,#71843,#71844,#71845));
#14681=EDGE_LOOP('',(#71846,#71847,#71848,#71849));
#14682=EDGE_LOOP('',(#71850,#71851,#71852,#71853));
#14683=EDGE_LOOP('',(#71854,#71855,#71856,#71857,#71858));
#14684=EDGE_LOOP('',(#71859,#71860,#71861,#71862,#71863));
#14685=EDGE_LOOP('',(#71864,#71865,#71866,#71867));
#14686=EDGE_LOOP('',(#71868,#71869,#71870,#71871));
#14687=EDGE_LOOP('',(#71872,#71873,#71874));
#14688=EDGE_LOOP('',(#71875,#71876,#71877,#71878));
#14689=EDGE_LOOP('',(#71879,#71880,#71881,#71882));
#14690=EDGE_LOOP('',(#71883,#71884,#71885,#71886));
#14691=EDGE_LOOP('',(#71887,#71888,#71889,#71890));
#14692=EDGE_LOOP('',(#71891,#71892,#71893,#71894));
#14693=EDGE_LOOP('',(#71895,#71896,#71897,#71898));
#14694=EDGE_LOOP('',(#71899,#71900,#71901,#71902));
#14695=EDGE_LOOP('',(#71903,#71904,#71905,#71906));
#14696=EDGE_LOOP('',(#71907,#71908,#71909,#71910));
#14697=EDGE_LOOP('',(#71911,#71912,#71913,#71914));
#14698=EDGE_LOOP('',(#71915,#71916,#71917,#71918));
#14699=EDGE_LOOP('',(#71919,#71920,#71921));
#14700=EDGE_LOOP('',(#71922,#71923,#71924,#71925,#71926));
#14701=EDGE_LOOP('',(#71927,#71928,#71929,#71930,#71931));
#14702=EDGE_LOOP('',(#71932,#71933,#71934,#71935));
#14703=EDGE_LOOP('',(#71936,#71937,#71938,#71939));
#14704=EDGE_LOOP('',(#71940,#71941,#71942));
#14705=EDGE_LOOP('',(#71943,#71944,#71945,#71946));
#14706=EDGE_LOOP('',(#71947,#71948,#71949,#71950));
#14707=EDGE_LOOP('',(#71951,#71952,#71953,#71954));
#14708=EDGE_LOOP('',(#71955,#71956,#71957,#71958));
#14709=EDGE_LOOP('',(#71959,#71960,#71961,#71962));
#14710=EDGE_LOOP('',(#71963,#71964,#71965,#71966));
#14711=EDGE_LOOP('',(#71967,#71968,#71969,#71970));
#14712=EDGE_LOOP('',(#71971,#71972,#71973,#71974));
#14713=EDGE_LOOP('',(#71975,#71976,#71977,#71978));
#14714=EDGE_LOOP('',(#71979,#71980,#71981,#71982));
#14715=EDGE_LOOP('',(#71983,#71984,#71985,#71986));
#14716=EDGE_LOOP('',(#71987,#71988,#71989));
#14717=EDGE_LOOP('',(#71990,#71991,#71992,#71993,#71994));
#14718=EDGE_LOOP('',(#71995,#71996,#71997,#71998,#71999));
#14719=EDGE_LOOP('',(#72000,#72001,#72002,#72003));
#14720=EDGE_LOOP('',(#72004,#72005,#72006,#72007));
#14721=EDGE_LOOP('',(#72008,#72009,#72010));
#14722=EDGE_LOOP('',(#72011,#72012,#72013,#72014));
#14723=EDGE_LOOP('',(#72015,#72016,#72017,#72018));
#14724=EDGE_LOOP('',(#72019,#72020,#72021,#72022));
#14725=EDGE_LOOP('',(#72023,#72024,#72025,#72026));
#14726=EDGE_LOOP('',(#72027,#72028,#72029,#72030));
#14727=EDGE_LOOP('',(#72031,#72032,#72033,#72034));
#14728=EDGE_LOOP('',(#72035,#72036,#72037,#72038));
#14729=EDGE_LOOP('',(#72039,#72040,#72041,#72042));
#14730=EDGE_LOOP('',(#72043,#72044,#72045,#72046));
#14731=EDGE_LOOP('',(#72047,#72048,#72049,#72050));
#14732=EDGE_LOOP('',(#72051,#72052,#72053,#72054));
#14733=EDGE_LOOP('',(#72055,#72056,#72057));
#14734=EDGE_LOOP('',(#72058,#72059,#72060,#72061,#72062));
#14735=EDGE_LOOP('',(#72063,#72064,#72065,#72066,#72067));
#14736=EDGE_LOOP('',(#72068,#72069,#72070,#72071));
#14737=EDGE_LOOP('',(#72072,#72073,#72074,#72075));
#14738=EDGE_LOOP('',(#72076,#72077,#72078));
#14739=EDGE_LOOP('',(#72079,#72080,#72081,#72082));
#14740=EDGE_LOOP('',(#72083,#72084,#72085,#72086));
#14741=EDGE_LOOP('',(#72087,#72088,#72089,#72090));
#14742=EDGE_LOOP('',(#72091,#72092,#72093,#72094));
#14743=EDGE_LOOP('',(#72095,#72096,#72097,#72098));
#14744=EDGE_LOOP('',(#72099,#72100,#72101,#72102));
#14745=EDGE_LOOP('',(#72103,#72104,#72105,#72106));
#14746=EDGE_LOOP('',(#72107,#72108,#72109,#72110));
#14747=EDGE_LOOP('',(#72111,#72112,#72113,#72114));
#14748=EDGE_LOOP('',(#72115,#72116,#72117,#72118));
#14749=EDGE_LOOP('',(#72119,#72120,#72121,#72122));
#14750=EDGE_LOOP('',(#72123,#72124,#72125));
#14751=EDGE_LOOP('',(#72126,#72127,#72128,#72129,#72130));
#14752=EDGE_LOOP('',(#72131,#72132,#72133,#72134,#72135));
#14753=EDGE_LOOP('',(#72136,#72137,#72138,#72139));
#14754=EDGE_LOOP('',(#72140,#72141,#72142,#72143));
#14755=EDGE_LOOP('',(#72144,#72145,#72146));
#14756=EDGE_LOOP('',(#72147,#72148,#72149,#72150));
#14757=EDGE_LOOP('',(#72151,#72152,#72153,#72154));
#14758=EDGE_LOOP('',(#72155,#72156,#72157,#72158));
#14759=EDGE_LOOP('',(#72159,#72160,#72161,#72162));
#14760=EDGE_LOOP('',(#72163,#72164,#72165,#72166));
#14761=EDGE_LOOP('',(#72167,#72168,#72169,#72170));
#14762=EDGE_LOOP('',(#72171,#72172,#72173,#72174));
#14763=EDGE_LOOP('',(#72175,#72176,#72177,#72178));
#14764=EDGE_LOOP('',(#72179,#72180,#72181,#72182));
#14765=EDGE_LOOP('',(#72183,#72184,#72185,#72186));
#14766=EDGE_LOOP('',(#72187,#72188,#72189,#72190));
#14767=EDGE_LOOP('',(#72191,#72192,#72193));
#14768=EDGE_LOOP('',(#72194,#72195,#72196,#72197,#72198));
#14769=EDGE_LOOP('',(#72199,#72200,#72201,#72202,#72203));
#14770=EDGE_LOOP('',(#72204,#72205,#72206,#72207));
#14771=EDGE_LOOP('',(#72208,#72209,#72210,#72211));
#14772=EDGE_LOOP('',(#72212,#72213,#72214));
#14773=EDGE_LOOP('',(#72215,#72216,#72217,#72218));
#14774=EDGE_LOOP('',(#72219,#72220,#72221,#72222));
#14775=EDGE_LOOP('',(#72223,#72224,#72225,#72226));
#14776=EDGE_LOOP('',(#72227,#72228,#72229,#72230));
#14777=EDGE_LOOP('',(#72231,#72232,#72233,#72234));
#14778=EDGE_LOOP('',(#72235,#72236,#72237,#72238));
#14779=EDGE_LOOP('',(#72239,#72240,#72241,#72242));
#14780=EDGE_LOOP('',(#72243,#72244,#72245,#72246));
#14781=EDGE_LOOP('',(#72247,#72248,#72249,#72250));
#14782=EDGE_LOOP('',(#72251,#72252,#72253,#72254));
#14783=EDGE_LOOP('',(#72255,#72256,#72257,#72258));
#14784=EDGE_LOOP('',(#72259,#72260,#72261));
#14785=EDGE_LOOP('',(#72262,#72263,#72264,#72265,#72266));
#14786=EDGE_LOOP('',(#72267,#72268,#72269,#72270,#72271));
#14787=EDGE_LOOP('',(#72272,#72273,#72274,#72275));
#14788=EDGE_LOOP('',(#72276,#72277,#72278,#72279));
#14789=EDGE_LOOP('',(#72280,#72281,#72282));
#14790=EDGE_LOOP('',(#72283,#72284,#72285,#72286));
#14791=EDGE_LOOP('',(#72287,#72288,#72289,#72290));
#14792=EDGE_LOOP('',(#72291,#72292,#72293,#72294));
#14793=EDGE_LOOP('',(#72295,#72296,#72297,#72298));
#14794=EDGE_LOOP('',(#72299,#72300,#72301,#72302));
#14795=EDGE_LOOP('',(#72303,#72304,#72305,#72306));
#14796=EDGE_LOOP('',(#72307,#72308,#72309,#72310));
#14797=EDGE_LOOP('',(#72311,#72312,#72313,#72314));
#14798=EDGE_LOOP('',(#72315,#72316,#72317,#72318));
#14799=EDGE_LOOP('',(#72319,#72320,#72321,#72322));
#14800=EDGE_LOOP('',(#72323,#72324,#72325,#72326));
#14801=EDGE_LOOP('',(#72327,#72328,#72329));
#14802=EDGE_LOOP('',(#72330,#72331,#72332,#72333,#72334));
#14803=EDGE_LOOP('',(#72335,#72336,#72337,#72338,#72339));
#14804=EDGE_LOOP('',(#72340,#72341,#72342,#72343));
#14805=EDGE_LOOP('',(#72344,#72345,#72346,#72347));
#14806=EDGE_LOOP('',(#72348,#72349,#72350));
#14807=EDGE_LOOP('',(#72351,#72352,#72353,#72354));
#14808=EDGE_LOOP('',(#72355,#72356,#72357,#72358));
#14809=EDGE_LOOP('',(#72359,#72360,#72361,#72362));
#14810=EDGE_LOOP('',(#72363,#72364,#72365,#72366));
#14811=EDGE_LOOP('',(#72367,#72368,#72369,#72370));
#14812=EDGE_LOOP('',(#72371,#72372,#72373,#72374));
#14813=EDGE_LOOP('',(#72375,#72376,#72377,#72378));
#14814=EDGE_LOOP('',(#72379,#72380,#72381,#72382));
#14815=EDGE_LOOP('',(#72383,#72384,#72385,#72386));
#14816=EDGE_LOOP('',(#72387,#72388,#72389,#72390));
#14817=EDGE_LOOP('',(#72391,#72392,#72393,#72394));
#14818=EDGE_LOOP('',(#72395,#72396,#72397));
#14819=EDGE_LOOP('',(#72398,#72399,#72400,#72401,#72402));
#14820=EDGE_LOOP('',(#72403,#72404,#72405,#72406,#72407));
#14821=EDGE_LOOP('',(#72408,#72409,#72410,#72411));
#14822=EDGE_LOOP('',(#72412,#72413,#72414,#72415));
#14823=EDGE_LOOP('',(#72416,#72417,#72418));
#14824=EDGE_LOOP('',(#72419,#72420,#72421,#72422));
#14825=EDGE_LOOP('',(#72423,#72424,#72425,#72426));
#14826=EDGE_LOOP('',(#72427,#72428,#72429,#72430));
#14827=EDGE_LOOP('',(#72431,#72432,#72433,#72434));
#14828=EDGE_LOOP('',(#72435,#72436,#72437,#72438));
#14829=EDGE_LOOP('',(#72439,#72440,#72441,#72442));
#14830=EDGE_LOOP('',(#72443,#72444,#72445,#72446));
#14831=EDGE_LOOP('',(#72447,#72448,#72449,#72450));
#14832=EDGE_LOOP('',(#72451,#72452,#72453,#72454));
#14833=EDGE_LOOP('',(#72455,#72456,#72457,#72458));
#14834=EDGE_LOOP('',(#72459,#72460,#72461,#72462));
#14835=EDGE_LOOP('',(#72463,#72464,#72465));
#14836=EDGE_LOOP('',(#72466,#72467,#72468,#72469,#72470));
#14837=EDGE_LOOP('',(#72471,#72472,#72473,#72474,#72475));
#14838=EDGE_LOOP('',(#72476,#72477,#72478,#72479));
#14839=EDGE_LOOP('',(#72480,#72481,#72482,#72483));
#14840=EDGE_LOOP('',(#72484,#72485,#72486));
#14841=EDGE_LOOP('',(#72487,#72488,#72489,#72490));
#14842=EDGE_LOOP('',(#72491,#72492,#72493,#72494));
#14843=EDGE_LOOP('',(#72495,#72496,#72497,#72498));
#14844=EDGE_LOOP('',(#72499,#72500,#72501,#72502));
#14845=EDGE_LOOP('',(#72503,#72504,#72505,#72506));
#14846=EDGE_LOOP('',(#72507,#72508,#72509,#72510));
#14847=EDGE_LOOP('',(#72511,#72512,#72513,#72514));
#14848=EDGE_LOOP('',(#72515,#72516,#72517,#72518));
#14849=EDGE_LOOP('',(#72519,#72520,#72521,#72522));
#14850=EDGE_LOOP('',(#72523,#72524,#72525,#72526));
#14851=EDGE_LOOP('',(#72527,#72528,#72529,#72530));
#14852=EDGE_LOOP('',(#72531,#72532,#72533));
#14853=EDGE_LOOP('',(#72534,#72535,#72536,#72537,#72538));
#14854=EDGE_LOOP('',(#72539,#72540,#72541,#72542,#72543));
#14855=EDGE_LOOP('',(#72544,#72545,#72546,#72547));
#14856=EDGE_LOOP('',(#72548,#72549,#72550,#72551));
#14857=EDGE_LOOP('',(#72552,#72553,#72554));
#14858=EDGE_LOOP('',(#72555,#72556,#72557,#72558));
#14859=EDGE_LOOP('',(#72559,#72560,#72561,#72562));
#14860=EDGE_LOOP('',(#72563,#72564,#72565,#72566));
#14861=EDGE_LOOP('',(#72567,#72568,#72569,#72570));
#14862=EDGE_LOOP('',(#72571,#72572,#72573,#72574));
#14863=EDGE_LOOP('',(#72575,#72576,#72577,#72578));
#14864=EDGE_LOOP('',(#72579,#72580,#72581,#72582));
#14865=EDGE_LOOP('',(#72583,#72584,#72585,#72586));
#14866=EDGE_LOOP('',(#72587,#72588,#72589,#72590));
#14867=EDGE_LOOP('',(#72591,#72592,#72593,#72594));
#14868=EDGE_LOOP('',(#72595,#72596,#72597,#72598));
#14869=EDGE_LOOP('',(#72599,#72600,#72601));
#14870=EDGE_LOOP('',(#72602,#72603,#72604,#72605,#72606));
#14871=EDGE_LOOP('',(#72607,#72608,#72609,#72610,#72611));
#14872=EDGE_LOOP('',(#72612,#72613,#72614,#72615));
#14873=EDGE_LOOP('',(#72616,#72617,#72618,#72619));
#14874=EDGE_LOOP('',(#72620,#72621,#72622));
#14875=EDGE_LOOP('',(#72623,#72624,#72625,#72626));
#14876=EDGE_LOOP('',(#72627,#72628,#72629,#72630));
#14877=EDGE_LOOP('',(#72631,#72632,#72633,#72634));
#14878=EDGE_LOOP('',(#72635,#72636,#72637,#72638));
#14879=EDGE_LOOP('',(#72639,#72640,#72641,#72642));
#14880=EDGE_LOOP('',(#72643,#72644,#72645,#72646));
#14881=EDGE_LOOP('',(#72647,#72648,#72649,#72650));
#14882=EDGE_LOOP('',(#72651,#72652,#72653,#72654));
#14883=EDGE_LOOP('',(#72655,#72656,#72657,#72658));
#14884=EDGE_LOOP('',(#72659,#72660,#72661,#72662));
#14885=EDGE_LOOP('',(#72663,#72664,#72665,#72666));
#14886=EDGE_LOOP('',(#72667,#72668,#72669));
#14887=EDGE_LOOP('',(#72670,#72671,#72672,#72673,#72674));
#14888=EDGE_LOOP('',(#72675,#72676,#72677,#72678,#72679));
#14889=EDGE_LOOP('',(#72680,#72681,#72682,#72683));
#14890=EDGE_LOOP('',(#72684,#72685,#72686,#72687));
#14891=EDGE_LOOP('',(#72688,#72689,#72690));
#14892=EDGE_LOOP('',(#72691,#72692,#72693,#72694));
#14893=EDGE_LOOP('',(#72695,#72696,#72697,#72698));
#14894=EDGE_LOOP('',(#72699,#72700,#72701,#72702));
#14895=EDGE_LOOP('',(#72703,#72704,#72705,#72706));
#14896=EDGE_LOOP('',(#72707,#72708,#72709,#72710));
#14897=EDGE_LOOP('',(#72711,#72712,#72713,#72714));
#14898=EDGE_LOOP('',(#72715,#72716,#72717,#72718));
#14899=EDGE_LOOP('',(#72719,#72720,#72721,#72722));
#14900=EDGE_LOOP('',(#72723,#72724,#72725,#72726));
#14901=EDGE_LOOP('',(#72727,#72728,#72729,#72730));
#14902=EDGE_LOOP('',(#72731,#72732,#72733,#72734));
#14903=EDGE_LOOP('',(#72735,#72736,#72737));
#14904=EDGE_LOOP('',(#72738,#72739,#72740,#72741,#72742));
#14905=EDGE_LOOP('',(#72743,#72744,#72745,#72746,#72747));
#14906=EDGE_LOOP('',(#72748,#72749,#72750,#72751));
#14907=EDGE_LOOP('',(#72752,#72753,#72754,#72755));
#14908=EDGE_LOOP('',(#72756,#72757,#72758));
#14909=EDGE_LOOP('',(#72759,#72760,#72761,#72762));
#14910=EDGE_LOOP('',(#72763,#72764,#72765,#72766));
#14911=EDGE_LOOP('',(#72767,#72768,#72769,#72770));
#14912=EDGE_LOOP('',(#72771,#72772,#72773,#72774));
#14913=EDGE_LOOP('',(#72775,#72776,#72777,#72778));
#14914=EDGE_LOOP('',(#72779,#72780,#72781,#72782));
#14915=EDGE_LOOP('',(#72783,#72784,#72785,#72786));
#14916=EDGE_LOOP('',(#72787,#72788,#72789,#72790));
#14917=EDGE_LOOP('',(#72791,#72792,#72793,#72794));
#14918=EDGE_LOOP('',(#72795,#72796,#72797,#72798));
#14919=EDGE_LOOP('',(#72799,#72800,#72801,#72802));
#14920=EDGE_LOOP('',(#72803,#72804,#72805));
#14921=EDGE_LOOP('',(#72806,#72807,#72808,#72809,#72810));
#14922=EDGE_LOOP('',(#72811,#72812,#72813,#72814,#72815));
#14923=EDGE_LOOP('',(#72816,#72817,#72818,#72819));
#14924=EDGE_LOOP('',(#72820,#72821,#72822,#72823));
#14925=EDGE_LOOP('',(#72824,#72825,#72826));
#14926=EDGE_LOOP('',(#72827,#72828,#72829,#72830));
#14927=EDGE_LOOP('',(#72831,#72832,#72833,#72834));
#14928=EDGE_LOOP('',(#72835,#72836,#72837,#72838));
#14929=EDGE_LOOP('',(#72839,#72840,#72841,#72842));
#14930=EDGE_LOOP('',(#72843,#72844,#72845,#72846));
#14931=EDGE_LOOP('',(#72847,#72848,#72849,#72850));
#14932=EDGE_LOOP('',(#72851,#72852,#72853,#72854));
#14933=EDGE_LOOP('',(#72855,#72856,#72857,#72858));
#14934=EDGE_LOOP('',(#72859,#72860,#72861,#72862));
#14935=EDGE_LOOP('',(#72863,#72864,#72865,#72866));
#14936=EDGE_LOOP('',(#72867,#72868,#72869,#72870));
#14937=EDGE_LOOP('',(#72871,#72872,#72873));
#14938=EDGE_LOOP('',(#72874,#72875,#72876,#72877,#72878));
#14939=EDGE_LOOP('',(#72879,#72880,#72881,#72882,#72883));
#14940=EDGE_LOOP('',(#72884,#72885,#72886,#72887));
#14941=EDGE_LOOP('',(#72888,#72889,#72890,#72891));
#14942=EDGE_LOOP('',(#72892,#72893,#72894));
#14943=EDGE_LOOP('',(#72895,#72896,#72897,#72898));
#14944=EDGE_LOOP('',(#72899,#72900,#72901,#72902));
#14945=EDGE_LOOP('',(#72903,#72904,#72905,#72906));
#14946=EDGE_LOOP('',(#72907,#72908,#72909,#72910));
#14947=EDGE_LOOP('',(#72911,#72912,#72913,#72914));
#14948=EDGE_LOOP('',(#72915,#72916,#72917,#72918));
#14949=EDGE_LOOP('',(#72919,#72920,#72921,#72922));
#14950=EDGE_LOOP('',(#72923,#72924,#72925,#72926));
#14951=EDGE_LOOP('',(#72927,#72928,#72929,#72930));
#14952=EDGE_LOOP('',(#72931,#72932,#72933,#72934));
#14953=EDGE_LOOP('',(#72935,#72936,#72937,#72938));
#14954=EDGE_LOOP('',(#72939,#72940,#72941));
#14955=EDGE_LOOP('',(#72942,#72943,#72944,#72945,#72946));
#14956=EDGE_LOOP('',(#72947,#72948,#72949,#72950,#72951));
#14957=EDGE_LOOP('',(#72952,#72953,#72954,#72955));
#14958=EDGE_LOOP('',(#72956,#72957,#72958,#72959));
#14959=EDGE_LOOP('',(#72960,#72961,#72962));
#14960=EDGE_LOOP('',(#72963,#72964,#72965,#72966));
#14961=EDGE_LOOP('',(#72967,#72968,#72969,#72970));
#14962=EDGE_LOOP('',(#72971,#72972,#72973,#72974));
#14963=EDGE_LOOP('',(#72975,#72976,#72977,#72978));
#14964=EDGE_LOOP('',(#72979,#72980,#72981,#72982));
#14965=EDGE_LOOP('',(#72983,#72984,#72985,#72986));
#14966=EDGE_LOOP('',(#72987,#72988,#72989,#72990));
#14967=EDGE_LOOP('',(#72991,#72992,#72993,#72994));
#14968=EDGE_LOOP('',(#72995,#72996,#72997,#72998));
#14969=EDGE_LOOP('',(#72999,#73000,#73001,#73002));
#14970=EDGE_LOOP('',(#73003,#73004,#73005,#73006));
#14971=EDGE_LOOP('',(#73007,#73008,#73009));
#14972=EDGE_LOOP('',(#73010,#73011,#73012,#73013,#73014));
#14973=EDGE_LOOP('',(#73015,#73016,#73017,#73018,#73019));
#14974=EDGE_LOOP('',(#73020,#73021,#73022,#73023));
#14975=EDGE_LOOP('',(#73024,#73025,#73026,#73027));
#14976=EDGE_LOOP('',(#73028,#73029,#73030));
#14977=EDGE_LOOP('',(#73031,#73032,#73033,#73034));
#14978=EDGE_LOOP('',(#73035,#73036,#73037,#73038));
#14979=EDGE_LOOP('',(#73039,#73040,#73041,#73042));
#14980=EDGE_LOOP('',(#73043,#73044,#73045,#73046));
#14981=EDGE_LOOP('',(#73047,#73048,#73049,#73050));
#14982=EDGE_LOOP('',(#73051,#73052,#73053,#73054));
#14983=EDGE_LOOP('',(#73055,#73056,#73057,#73058));
#14984=EDGE_LOOP('',(#73059,#73060,#73061,#73062));
#14985=EDGE_LOOP('',(#73063,#73064,#73065,#73066));
#14986=EDGE_LOOP('',(#73067,#73068,#73069,#73070));
#14987=EDGE_LOOP('',(#73071,#73072,#73073,#73074));
#14988=EDGE_LOOP('',(#73075,#73076,#73077));
#14989=EDGE_LOOP('',(#73078,#73079,#73080,#73081,#73082));
#14990=EDGE_LOOP('',(#73083,#73084,#73085,#73086,#73087));
#14991=EDGE_LOOP('',(#73088,#73089,#73090,#73091));
#14992=EDGE_LOOP('',(#73092,#73093,#73094,#73095));
#14993=EDGE_LOOP('',(#73096,#73097,#73098));
#14994=EDGE_LOOP('',(#73099,#73100,#73101,#73102));
#14995=EDGE_LOOP('',(#73103,#73104,#73105,#73106));
#14996=EDGE_LOOP('',(#73107,#73108,#73109,#73110));
#14997=EDGE_LOOP('',(#73111,#73112,#73113,#73114));
#14998=EDGE_LOOP('',(#73115,#73116,#73117,#73118));
#14999=EDGE_LOOP('',(#73119,#73120,#73121,#73122));
#15000=EDGE_LOOP('',(#73123,#73124,#73125,#73126));
#15001=EDGE_LOOP('',(#73127,#73128,#73129,#73130));
#15002=EDGE_LOOP('',(#73131,#73132,#73133,#73134));
#15003=EDGE_LOOP('',(#73135,#73136,#73137,#73138));
#15004=EDGE_LOOP('',(#73139,#73140,#73141,#73142));
#15005=EDGE_LOOP('',(#73143,#73144,#73145));
#15006=EDGE_LOOP('',(#73146,#73147,#73148,#73149,#73150));
#15007=EDGE_LOOP('',(#73151,#73152,#73153,#73154,#73155));
#15008=EDGE_LOOP('',(#73156,#73157,#73158,#73159));
#15009=EDGE_LOOP('',(#73160,#73161,#73162,#73163));
#15010=EDGE_LOOP('',(#73164,#73165,#73166));
#15011=EDGE_LOOP('',(#73167,#73168,#73169,#73170));
#15012=EDGE_LOOP('',(#73171,#73172,#73173,#73174));
#15013=EDGE_LOOP('',(#73175,#73176,#73177,#73178));
#15014=EDGE_LOOP('',(#73179,#73180,#73181,#73182));
#15015=EDGE_LOOP('',(#73183,#73184,#73185,#73186));
#15016=EDGE_LOOP('',(#73187,#73188,#73189,#73190));
#15017=EDGE_LOOP('',(#73191,#73192,#73193,#73194));
#15018=EDGE_LOOP('',(#73195,#73196,#73197,#73198));
#15019=EDGE_LOOP('',(#73199,#73200,#73201,#73202));
#15020=EDGE_LOOP('',(#73203,#73204,#73205,#73206));
#15021=EDGE_LOOP('',(#73207,#73208,#73209,#73210));
#15022=EDGE_LOOP('',(#73211,#73212,#73213));
#15023=EDGE_LOOP('',(#73214,#73215,#73216,#73217,#73218));
#15024=EDGE_LOOP('',(#73219,#73220,#73221,#73222,#73223));
#15025=EDGE_LOOP('',(#73224,#73225,#73226,#73227));
#15026=EDGE_LOOP('',(#73228,#73229,#73230,#73231));
#15027=EDGE_LOOP('',(#73232,#73233,#73234));
#15028=EDGE_LOOP('',(#73235,#73236,#73237,#73238));
#15029=EDGE_LOOP('',(#73239,#73240,#73241,#73242));
#15030=EDGE_LOOP('',(#73243,#73244,#73245,#73246));
#15031=EDGE_LOOP('',(#73247,#73248,#73249,#73250));
#15032=EDGE_LOOP('',(#73251,#73252,#73253,#73254));
#15033=EDGE_LOOP('',(#73255,#73256,#73257,#73258));
#15034=EDGE_LOOP('',(#73259,#73260,#73261,#73262));
#15035=EDGE_LOOP('',(#73263,#73264,#73265,#73266));
#15036=EDGE_LOOP('',(#73267,#73268,#73269,#73270));
#15037=EDGE_LOOP('',(#73271,#73272,#73273,#73274));
#15038=EDGE_LOOP('',(#73275,#73276,#73277,#73278));
#15039=EDGE_LOOP('',(#73279,#73280,#73281));
#15040=EDGE_LOOP('',(#73282,#73283,#73284,#73285,#73286));
#15041=EDGE_LOOP('',(#73287,#73288,#73289,#73290,#73291));
#15042=EDGE_LOOP('',(#73292,#73293,#73294,#73295));
#15043=EDGE_LOOP('',(#73296,#73297,#73298,#73299));
#15044=EDGE_LOOP('',(#73300,#73301,#73302));
#15045=EDGE_LOOP('',(#73303,#73304,#73305,#73306));
#15046=EDGE_LOOP('',(#73307,#73308,#73309,#73310));
#15047=EDGE_LOOP('',(#73311,#73312,#73313,#73314));
#15048=EDGE_LOOP('',(#73315,#73316,#73317,#73318));
#15049=EDGE_LOOP('',(#73319,#73320,#73321,#73322));
#15050=EDGE_LOOP('',(#73323,#73324,#73325,#73326));
#15051=EDGE_LOOP('',(#73327,#73328,#73329,#73330));
#15052=EDGE_LOOP('',(#73331,#73332,#73333,#73334));
#15053=EDGE_LOOP('',(#73335,#73336,#73337,#73338));
#15054=EDGE_LOOP('',(#73339,#73340,#73341,#73342));
#15055=EDGE_LOOP('',(#73343,#73344,#73345,#73346));
#15056=EDGE_LOOP('',(#73347,#73348,#73349));
#15057=EDGE_LOOP('',(#73350,#73351,#73352,#73353,#73354));
#15058=EDGE_LOOP('',(#73355,#73356,#73357,#73358,#73359));
#15059=EDGE_LOOP('',(#73360,#73361,#73362,#73363));
#15060=EDGE_LOOP('',(#73364,#73365,#73366,#73367));
#15061=EDGE_LOOP('',(#73368,#73369,#73370));
#15062=EDGE_LOOP('',(#73371,#73372,#73373,#73374));
#15063=EDGE_LOOP('',(#73375,#73376,#73377,#73378));
#15064=EDGE_LOOP('',(#73379,#73380,#73381,#73382));
#15065=EDGE_LOOP('',(#73383,#73384,#73385,#73386));
#15066=EDGE_LOOP('',(#73387,#73388,#73389,#73390));
#15067=EDGE_LOOP('',(#73391,#73392,#73393,#73394));
#15068=EDGE_LOOP('',(#73395,#73396,#73397,#73398));
#15069=EDGE_LOOP('',(#73399,#73400,#73401,#73402));
#15070=EDGE_LOOP('',(#73403,#73404,#73405,#73406));
#15071=EDGE_LOOP('',(#73407,#73408,#73409,#73410));
#15072=EDGE_LOOP('',(#73411,#73412,#73413,#73414));
#15073=EDGE_LOOP('',(#73415,#73416,#73417));
#15074=EDGE_LOOP('',(#73418,#73419,#73420,#73421,#73422));
#15075=EDGE_LOOP('',(#73423,#73424,#73425,#73426,#73427));
#15076=EDGE_LOOP('',(#73428,#73429,#73430,#73431));
#15077=EDGE_LOOP('',(#73432,#73433,#73434,#73435));
#15078=EDGE_LOOP('',(#73436,#73437,#73438));
#15079=EDGE_LOOP('',(#73439,#73440,#73441,#73442));
#15080=EDGE_LOOP('',(#73443,#73444,#73445,#73446));
#15081=EDGE_LOOP('',(#73447,#73448,#73449,#73450));
#15082=EDGE_LOOP('',(#73451,#73452,#73453,#73454));
#15083=EDGE_LOOP('',(#73455,#73456,#73457,#73458));
#15084=EDGE_LOOP('',(#73459,#73460,#73461,#73462));
#15085=EDGE_LOOP('',(#73463,#73464,#73465,#73466));
#15086=EDGE_LOOP('',(#73467,#73468,#73469,#73470));
#15087=EDGE_LOOP('',(#73471,#73472,#73473,#73474));
#15088=EDGE_LOOP('',(#73475,#73476,#73477,#73478));
#15089=EDGE_LOOP('',(#73479,#73480,#73481,#73482));
#15090=EDGE_LOOP('',(#73483,#73484,#73485));
#15091=EDGE_LOOP('',(#73486,#73487,#73488,#73489,#73490));
#15092=EDGE_LOOP('',(#73491,#73492,#73493,#73494,#73495));
#15093=EDGE_LOOP('',(#73496,#73497,#73498,#73499));
#15094=EDGE_LOOP('',(#73500,#73501,#73502,#73503));
#15095=EDGE_LOOP('',(#73504,#73505,#73506));
#15096=EDGE_LOOP('',(#73507,#73508,#73509,#73510));
#15097=EDGE_LOOP('',(#73511,#73512,#73513,#73514));
#15098=EDGE_LOOP('',(#73515,#73516,#73517,#73518));
#15099=EDGE_LOOP('',(#73519,#73520,#73521,#73522));
#15100=EDGE_LOOP('',(#73523,#73524,#73525,#73526));
#15101=EDGE_LOOP('',(#73527,#73528,#73529,#73530));
#15102=EDGE_LOOP('',(#73531,#73532,#73533,#73534));
#15103=EDGE_LOOP('',(#73535,#73536,#73537,#73538));
#15104=EDGE_LOOP('',(#73539,#73540,#73541,#73542));
#15105=EDGE_LOOP('',(#73543,#73544,#73545,#73546));
#15106=EDGE_LOOP('',(#73547,#73548,#73549,#73550));
#15107=EDGE_LOOP('',(#73551,#73552,#73553));
#15108=EDGE_LOOP('',(#73554,#73555,#73556,#73557,#73558));
#15109=EDGE_LOOP('',(#73559,#73560,#73561,#73562,#73563));
#15110=EDGE_LOOP('',(#73564,#73565,#73566,#73567));
#15111=EDGE_LOOP('',(#73568,#73569,#73570,#73571));
#15112=EDGE_LOOP('',(#73572,#73573,#73574));
#15113=EDGE_LOOP('',(#73575,#73576,#73577,#73578));
#15114=EDGE_LOOP('',(#73579,#73580,#73581,#73582));
#15115=EDGE_LOOP('',(#73583,#73584,#73585,#73586));
#15116=EDGE_LOOP('',(#73587,#73588,#73589,#73590));
#15117=EDGE_LOOP('',(#73591,#73592,#73593,#73594));
#15118=EDGE_LOOP('',(#73595,#73596,#73597,#73598));
#15119=EDGE_LOOP('',(#73599,#73600,#73601,#73602));
#15120=EDGE_LOOP('',(#73603,#73604,#73605,#73606));
#15121=EDGE_LOOP('',(#73607,#73608,#73609,#73610));
#15122=EDGE_LOOP('',(#73611,#73612,#73613,#73614));
#15123=EDGE_LOOP('',(#73615,#73616,#73617,#73618));
#15124=EDGE_LOOP('',(#73619,#73620,#73621));
#15125=EDGE_LOOP('',(#73622,#73623,#73624,#73625,#73626));
#15126=EDGE_LOOP('',(#73627,#73628,#73629,#73630,#73631));
#15127=EDGE_LOOP('',(#73632,#73633,#73634,#73635));
#15128=EDGE_LOOP('',(#73636,#73637,#73638,#73639));
#15129=EDGE_LOOP('',(#73640,#73641,#73642));
#15130=EDGE_LOOP('',(#73643,#73644,#73645,#73646));
#15131=EDGE_LOOP('',(#73647,#73648,#73649,#73650));
#15132=EDGE_LOOP('',(#73651,#73652,#73653,#73654));
#15133=EDGE_LOOP('',(#73655,#73656,#73657,#73658));
#15134=EDGE_LOOP('',(#73659,#73660,#73661,#73662));
#15135=EDGE_LOOP('',(#73663,#73664,#73665,#73666));
#15136=EDGE_LOOP('',(#73667,#73668,#73669,#73670));
#15137=EDGE_LOOP('',(#73671,#73672,#73673,#73674));
#15138=EDGE_LOOP('',(#73675,#73676,#73677,#73678));
#15139=EDGE_LOOP('',(#73679,#73680,#73681,#73682));
#15140=EDGE_LOOP('',(#73683,#73684,#73685,#73686));
#15141=EDGE_LOOP('',(#73687,#73688,#73689));
#15142=EDGE_LOOP('',(#73690,#73691,#73692,#73693,#73694));
#15143=EDGE_LOOP('',(#73695,#73696,#73697,#73698,#73699));
#15144=EDGE_LOOP('',(#73700,#73701,#73702,#73703));
#15145=EDGE_LOOP('',(#73704,#73705,#73706,#73707));
#15146=EDGE_LOOP('',(#73708,#73709,#73710));
#15147=EDGE_LOOP('',(#73711,#73712,#73713,#73714));
#15148=EDGE_LOOP('',(#73715,#73716,#73717,#73718));
#15149=EDGE_LOOP('',(#73719,#73720,#73721,#73722));
#15150=EDGE_LOOP('',(#73723,#73724,#73725,#73726));
#15151=EDGE_LOOP('',(#73727,#73728,#73729,#73730));
#15152=EDGE_LOOP('',(#73731,#73732,#73733,#73734));
#15153=EDGE_LOOP('',(#73735,#73736,#73737,#73738));
#15154=EDGE_LOOP('',(#73739,#73740,#73741,#73742));
#15155=EDGE_LOOP('',(#73743,#73744,#73745,#73746));
#15156=EDGE_LOOP('',(#73747,#73748,#73749,#73750));
#15157=EDGE_LOOP('',(#73751,#73752,#73753,#73754));
#15158=EDGE_LOOP('',(#73755,#73756,#73757));
#15159=EDGE_LOOP('',(#73758,#73759,#73760,#73761,#73762));
#15160=EDGE_LOOP('',(#73763,#73764,#73765,#73766,#73767));
#15161=EDGE_LOOP('',(#73768,#73769,#73770,#73771));
#15162=EDGE_LOOP('',(#73772,#73773,#73774,#73775));
#15163=EDGE_LOOP('',(#73776,#73777,#73778));
#15164=EDGE_LOOP('',(#73779,#73780,#73781,#73782));
#15165=EDGE_LOOP('',(#73783,#73784,#73785,#73786));
#15166=EDGE_LOOP('',(#73787,#73788,#73789,#73790));
#15167=EDGE_LOOP('',(#73791,#73792,#73793,#73794));
#15168=EDGE_LOOP('',(#73795,#73796,#73797,#73798));
#15169=EDGE_LOOP('',(#73799,#73800,#73801,#73802));
#15170=EDGE_LOOP('',(#73803,#73804,#73805,#73806));
#15171=EDGE_LOOP('',(#73807,#73808,#73809,#73810));
#15172=EDGE_LOOP('',(#73811,#73812,#73813,#73814));
#15173=EDGE_LOOP('',(#73815,#73816,#73817,#73818));
#15174=EDGE_LOOP('',(#73819,#73820,#73821,#73822));
#15175=EDGE_LOOP('',(#73823,#73824,#73825));
#15176=EDGE_LOOP('',(#73826,#73827,#73828,#73829,#73830));
#15177=EDGE_LOOP('',(#73831,#73832,#73833,#73834,#73835));
#15178=EDGE_LOOP('',(#73836,#73837,#73838,#73839));
#15179=EDGE_LOOP('',(#73840,#73841,#73842,#73843));
#15180=EDGE_LOOP('',(#73844,#73845,#73846));
#15181=EDGE_LOOP('',(#73847,#73848,#73849,#73850));
#15182=EDGE_LOOP('',(#73851,#73852,#73853,#73854));
#15183=EDGE_LOOP('',(#73855,#73856,#73857,#73858));
#15184=EDGE_LOOP('',(#73859,#73860,#73861,#73862));
#15185=EDGE_LOOP('',(#73863,#73864,#73865,#73866));
#15186=EDGE_LOOP('',(#73867,#73868,#73869,#73870));
#15187=EDGE_LOOP('',(#73871,#73872,#73873,#73874));
#15188=EDGE_LOOP('',(#73875,#73876,#73877,#73878));
#15189=EDGE_LOOP('',(#73879,#73880,#73881,#73882));
#15190=EDGE_LOOP('',(#73883,#73884,#73885,#73886));
#15191=EDGE_LOOP('',(#73887,#73888,#73889,#73890));
#15192=EDGE_LOOP('',(#73891,#73892,#73893));
#15193=EDGE_LOOP('',(#73894,#73895,#73896,#73897,#73898));
#15194=EDGE_LOOP('',(#73899,#73900,#73901,#73902,#73903));
#15195=EDGE_LOOP('',(#73904,#73905,#73906,#73907));
#15196=EDGE_LOOP('',(#73908,#73909,#73910,#73911));
#15197=EDGE_LOOP('',(#73912,#73913,#73914));
#15198=EDGE_LOOP('',(#73915,#73916,#73917,#73918));
#15199=EDGE_LOOP('',(#73919,#73920,#73921,#73922));
#15200=EDGE_LOOP('',(#73923,#73924,#73925,#73926));
#15201=EDGE_LOOP('',(#73927,#73928,#73929,#73930));
#15202=EDGE_LOOP('',(#73931,#73932,#73933,#73934));
#15203=EDGE_LOOP('',(#73935,#73936,#73937,#73938));
#15204=EDGE_LOOP('',(#73939,#73940,#73941,#73942));
#15205=EDGE_LOOP('',(#73943,#73944,#73945,#73946));
#15206=EDGE_LOOP('',(#73947,#73948,#73949,#73950));
#15207=EDGE_LOOP('',(#73951,#73952,#73953,#73954));
#15208=EDGE_LOOP('',(#73955,#73956,#73957,#73958));
#15209=EDGE_LOOP('',(#73959,#73960,#73961));
#15210=EDGE_LOOP('',(#73962,#73963,#73964,#73965,#73966));
#15211=EDGE_LOOP('',(#73967,#73968,#73969,#73970,#73971));
#15212=EDGE_LOOP('',(#73972,#73973,#73974,#73975));
#15213=EDGE_LOOP('',(#73976,#73977,#73978,#73979));
#15214=EDGE_LOOP('',(#73980,#73981,#73982));
#15215=EDGE_LOOP('',(#73983,#73984,#73985,#73986));
#15216=EDGE_LOOP('',(#73987,#73988,#73989,#73990));
#15217=EDGE_LOOP('',(#73991,#73992,#73993,#73994));
#15218=EDGE_LOOP('',(#73995,#73996,#73997,#73998));
#15219=EDGE_LOOP('',(#73999,#74000,#74001,#74002));
#15220=EDGE_LOOP('',(#74003,#74004,#74005,#74006));
#15221=EDGE_LOOP('',(#74007,#74008,#74009,#74010));
#15222=EDGE_LOOP('',(#74011,#74012,#74013,#74014));
#15223=EDGE_LOOP('',(#74015,#74016,#74017,#74018));
#15224=EDGE_LOOP('',(#74019,#74020,#74021,#74022));
#15225=EDGE_LOOP('',(#74023,#74024,#74025,#74026));
#15226=EDGE_LOOP('',(#74027,#74028,#74029));
#15227=EDGE_LOOP('',(#74030,#74031,#74032,#74033,#74034));
#15228=EDGE_LOOP('',(#74035,#74036,#74037,#74038,#74039));
#15229=EDGE_LOOP('',(#74040,#74041,#74042,#74043));
#15230=EDGE_LOOP('',(#74044,#74045,#74046,#74047));
#15231=EDGE_LOOP('',(#74048,#74049,#74050));
#15232=EDGE_LOOP('',(#74051,#74052,#74053,#74054));
#15233=EDGE_LOOP('',(#74055,#74056,#74057,#74058));
#15234=EDGE_LOOP('',(#74059,#74060,#74061,#74062));
#15235=EDGE_LOOP('',(#74063,#74064,#74065,#74066));
#15236=EDGE_LOOP('',(#74067,#74068,#74069,#74070));
#15237=EDGE_LOOP('',(#74071,#74072,#74073,#74074));
#15238=EDGE_LOOP('',(#74075,#74076,#74077,#74078));
#15239=EDGE_LOOP('',(#74079,#74080,#74081,#74082));
#15240=EDGE_LOOP('',(#74083,#74084,#74085,#74086));
#15241=EDGE_LOOP('',(#74087,#74088,#74089,#74090));
#15242=EDGE_LOOP('',(#74091,#74092,#74093,#74094));
#15243=EDGE_LOOP('',(#74095,#74096,#74097));
#15244=EDGE_LOOP('',(#74098,#74099,#74100,#74101,#74102));
#15245=EDGE_LOOP('',(#74103,#74104,#74105,#74106,#74107));
#15246=EDGE_LOOP('',(#74108,#74109,#74110,#74111));
#15247=EDGE_LOOP('',(#74112,#74113,#74114,#74115));
#15248=EDGE_LOOP('',(#74116,#74117,#74118));
#15249=EDGE_LOOP('',(#74119,#74120,#74121,#74122));
#15250=EDGE_LOOP('',(#74123,#74124,#74125,#74126));
#15251=EDGE_LOOP('',(#74127,#74128,#74129,#74130));
#15252=EDGE_LOOP('',(#74131,#74132,#74133,#74134));
#15253=EDGE_LOOP('',(#74135,#74136,#74137,#74138));
#15254=EDGE_LOOP('',(#74139,#74140,#74141,#74142));
#15255=EDGE_LOOP('',(#74143,#74144,#74145,#74146));
#15256=EDGE_LOOP('',(#74147,#74148,#74149,#74150));
#15257=EDGE_LOOP('',(#74151,#74152,#74153,#74154));
#15258=EDGE_LOOP('',(#74155,#74156,#74157,#74158));
#15259=EDGE_LOOP('',(#74159,#74160,#74161,#74162));
#15260=EDGE_LOOP('',(#74163,#74164,#74165));
#15261=EDGE_LOOP('',(#74166,#74167,#74168,#74169,#74170));
#15262=EDGE_LOOP('',(#74171,#74172,#74173,#74174,#74175));
#15263=EDGE_LOOP('',(#74176,#74177,#74178,#74179));
#15264=EDGE_LOOP('',(#74180,#74181,#74182,#74183));
#15265=EDGE_LOOP('',(#74184,#74185,#74186));
#15266=EDGE_LOOP('',(#74187,#74188,#74189,#74190));
#15267=EDGE_LOOP('',(#74191,#74192,#74193,#74194));
#15268=EDGE_LOOP('',(#74195,#74196,#74197,#74198));
#15269=EDGE_LOOP('',(#74199,#74200,#74201,#74202));
#15270=EDGE_LOOP('',(#74203,#74204,#74205,#74206));
#15271=EDGE_LOOP('',(#74207,#74208,#74209,#74210));
#15272=EDGE_LOOP('',(#74211,#74212,#74213,#74214));
#15273=EDGE_LOOP('',(#74215,#74216,#74217,#74218));
#15274=EDGE_LOOP('',(#74219,#74220,#74221,#74222));
#15275=EDGE_LOOP('',(#74223,#74224,#74225,#74226));
#15276=EDGE_LOOP('',(#74227,#74228,#74229,#74230));
#15277=EDGE_LOOP('',(#74231,#74232,#74233));
#15278=EDGE_LOOP('',(#74234,#74235,#74236,#74237,#74238));
#15279=EDGE_LOOP('',(#74239,#74240,#74241,#74242,#74243));
#15280=EDGE_LOOP('',(#74244,#74245,#74246,#74247));
#15281=EDGE_LOOP('',(#74248,#74249,#74250,#74251));
#15282=EDGE_LOOP('',(#74252,#74253,#74254));
#15283=EDGE_LOOP('',(#74255,#74256,#74257,#74258));
#15284=EDGE_LOOP('',(#74259,#74260,#74261,#74262));
#15285=EDGE_LOOP('',(#74263,#74264,#74265,#74266));
#15286=EDGE_LOOP('',(#74267,#74268,#74269,#74270));
#15287=EDGE_LOOP('',(#74271,#74272,#74273,#74274));
#15288=EDGE_LOOP('',(#74275,#74276,#74277,#74278));
#15289=EDGE_LOOP('',(#74279,#74280,#74281,#74282));
#15290=EDGE_LOOP('',(#74283,#74284,#74285,#74286));
#15291=EDGE_LOOP('',(#74287,#74288,#74289,#74290));
#15292=EDGE_LOOP('',(#74291,#74292,#74293,#74294));
#15293=EDGE_LOOP('',(#74295,#74296,#74297,#74298));
#15294=EDGE_LOOP('',(#74299,#74300,#74301));
#15295=EDGE_LOOP('',(#74302,#74303,#74304,#74305,#74306));
#15296=EDGE_LOOP('',(#74307,#74308,#74309,#74310,#74311));
#15297=EDGE_LOOP('',(#74312,#74313,#74314,#74315));
#15298=EDGE_LOOP('',(#74316,#74317,#74318,#74319));
#15299=EDGE_LOOP('',(#74320,#74321,#74322));
#15300=EDGE_LOOP('',(#74323,#74324,#74325,#74326));
#15301=EDGE_LOOP('',(#74327,#74328,#74329,#74330));
#15302=EDGE_LOOP('',(#74331,#74332,#74333,#74334));
#15303=EDGE_LOOP('',(#74335,#74336,#74337,#74338));
#15304=EDGE_LOOP('',(#74339,#74340,#74341,#74342));
#15305=EDGE_LOOP('',(#74343,#74344,#74345,#74346));
#15306=EDGE_LOOP('',(#74347,#74348,#74349,#74350));
#15307=EDGE_LOOP('',(#74351,#74352,#74353,#74354));
#15308=EDGE_LOOP('',(#74355,#74356,#74357,#74358));
#15309=EDGE_LOOP('',(#74359,#74360,#74361,#74362));
#15310=EDGE_LOOP('',(#74363,#74364,#74365,#74366));
#15311=EDGE_LOOP('',(#74367,#74368,#74369));
#15312=EDGE_LOOP('',(#74370,#74371,#74372,#74373,#74374));
#15313=EDGE_LOOP('',(#74375,#74376,#74377,#74378,#74379));
#15314=EDGE_LOOP('',(#74380,#74381,#74382,#74383));
#15315=EDGE_LOOP('',(#74384,#74385,#74386,#74387));
#15316=EDGE_LOOP('',(#74388,#74389,#74390));
#15317=EDGE_LOOP('',(#74391,#74392,#74393,#74394));
#15318=EDGE_LOOP('',(#74395,#74396,#74397,#74398));
#15319=EDGE_LOOP('',(#74399,#74400,#74401,#74402));
#15320=EDGE_LOOP('',(#74403,#74404,#74405,#74406));
#15321=EDGE_LOOP('',(#74407,#74408,#74409,#74410));
#15322=EDGE_LOOP('',(#74411,#74412,#74413,#74414));
#15323=EDGE_LOOP('',(#74415,#74416,#74417,#74418));
#15324=EDGE_LOOP('',(#74419,#74420,#74421,#74422));
#15325=EDGE_LOOP('',(#74423,#74424,#74425,#74426));
#15326=EDGE_LOOP('',(#74427,#74428,#74429,#74430));
#15327=EDGE_LOOP('',(#74431,#74432,#74433,#74434));
#15328=EDGE_LOOP('',(#74435,#74436,#74437));
#15329=EDGE_LOOP('',(#74438,#74439,#74440,#74441,#74442));
#15330=EDGE_LOOP('',(#74443,#74444,#74445,#74446,#74447));
#15331=EDGE_LOOP('',(#74448,#74449,#74450,#74451));
#15332=EDGE_LOOP('',(#74452,#74453,#74454,#74455));
#15333=EDGE_LOOP('',(#74456,#74457,#74458));
#15334=EDGE_LOOP('',(#74459,#74460,#74461,#74462));
#15335=EDGE_LOOP('',(#74463,#74464,#74465,#74466));
#15336=EDGE_LOOP('',(#74467,#74468,#74469,#74470));
#15337=EDGE_LOOP('',(#74471,#74472,#74473,#74474));
#15338=EDGE_LOOP('',(#74475,#74476,#74477,#74478));
#15339=EDGE_LOOP('',(#74479,#74480,#74481,#74482));
#15340=EDGE_LOOP('',(#74483,#74484,#74485,#74486));
#15341=EDGE_LOOP('',(#74487,#74488,#74489,#74490));
#15342=EDGE_LOOP('',(#74491,#74492,#74493,#74494));
#15343=EDGE_LOOP('',(#74495,#74496,#74497,#74498));
#15344=EDGE_LOOP('',(#74499,#74500,#74501,#74502));
#15345=EDGE_LOOP('',(#74503,#74504,#74505));
#15346=EDGE_LOOP('',(#74506,#74507,#74508,#74509,#74510));
#15347=EDGE_LOOP('',(#74511,#74512,#74513,#74514,#74515));
#15348=EDGE_LOOP('',(#74516,#74517,#74518,#74519));
#15349=EDGE_LOOP('',(#74520,#74521,#74522,#74523));
#15350=EDGE_LOOP('',(#74524,#74525,#74526));
#15351=EDGE_LOOP('',(#74527,#74528,#74529,#74530));
#15352=EDGE_LOOP('',(#74531,#74532,#74533,#74534));
#15353=EDGE_LOOP('',(#74535,#74536,#74537,#74538));
#15354=EDGE_LOOP('',(#74539,#74540,#74541,#74542));
#15355=EDGE_LOOP('',(#74543,#74544,#74545,#74546));
#15356=EDGE_LOOP('',(#74547,#74548,#74549,#74550));
#15357=EDGE_LOOP('',(#74551,#74552,#74553,#74554));
#15358=EDGE_LOOP('',(#74555,#74556,#74557,#74558));
#15359=EDGE_LOOP('',(#74559,#74560,#74561,#74562));
#15360=EDGE_LOOP('',(#74563,#74564,#74565,#74566));
#15361=EDGE_LOOP('',(#74567,#74568,#74569,#74570));
#15362=EDGE_LOOP('',(#74571,#74572,#74573));
#15363=EDGE_LOOP('',(#74574,#74575,#74576,#74577,#74578));
#15364=EDGE_LOOP('',(#74579,#74580,#74581,#74582,#74583));
#15365=EDGE_LOOP('',(#74584,#74585,#74586,#74587));
#15366=EDGE_LOOP('',(#74588,#74589,#74590,#74591));
#15367=EDGE_LOOP('',(#74592,#74593,#74594));
#15368=EDGE_LOOP('',(#74595,#74596,#74597,#74598));
#15369=EDGE_LOOP('',(#74599,#74600,#74601,#74602));
#15370=EDGE_LOOP('',(#74603,#74604,#74605,#74606));
#15371=EDGE_LOOP('',(#74607,#74608,#74609,#74610));
#15372=EDGE_LOOP('',(#74611,#74612,#74613,#74614));
#15373=EDGE_LOOP('',(#74615,#74616,#74617,#74618));
#15374=EDGE_LOOP('',(#74619,#74620,#74621,#74622));
#15375=EDGE_LOOP('',(#74623,#74624,#74625,#74626));
#15376=EDGE_LOOP('',(#74627,#74628,#74629,#74630));
#15377=EDGE_LOOP('',(#74631,#74632,#74633,#74634));
#15378=EDGE_LOOP('',(#74635,#74636,#74637,#74638));
#15379=EDGE_LOOP('',(#74639,#74640,#74641));
#15380=EDGE_LOOP('',(#74642,#74643,#74644,#74645,#74646));
#15381=EDGE_LOOP('',(#74647,#74648,#74649,#74650,#74651));
#15382=EDGE_LOOP('',(#74652,#74653,#74654,#74655));
#15383=EDGE_LOOP('',(#74656,#74657,#74658,#74659));
#15384=EDGE_LOOP('',(#74660,#74661,#74662));
#15385=EDGE_LOOP('',(#74663,#74664,#74665,#74666));
#15386=EDGE_LOOP('',(#74667,#74668,#74669,#74670));
#15387=EDGE_LOOP('',(#74671,#74672,#74673,#74674));
#15388=EDGE_LOOP('',(#74675,#74676,#74677,#74678));
#15389=EDGE_LOOP('',(#74679,#74680,#74681,#74682));
#15390=EDGE_LOOP('',(#74683,#74684,#74685,#74686));
#15391=EDGE_LOOP('',(#74687,#74688,#74689,#74690));
#15392=EDGE_LOOP('',(#74691,#74692,#74693,#74694));
#15393=EDGE_LOOP('',(#74695,#74696,#74697,#74698));
#15394=EDGE_LOOP('',(#74699,#74700,#74701,#74702));
#15395=EDGE_LOOP('',(#74703,#74704,#74705,#74706));
#15396=EDGE_LOOP('',(#74707,#74708,#74709));
#15397=EDGE_LOOP('',(#74710,#74711,#74712,#74713,#74714));
#15398=EDGE_LOOP('',(#74715,#74716,#74717,#74718,#74719));
#15399=EDGE_LOOP('',(#74720,#74721,#74722,#74723));
#15400=EDGE_LOOP('',(#74724,#74725,#74726,#74727));
#15401=EDGE_LOOP('',(#74728,#74729,#74730));
#15402=EDGE_LOOP('',(#74731,#74732,#74733,#74734));
#15403=EDGE_LOOP('',(#74735,#74736,#74737,#74738));
#15404=EDGE_LOOP('',(#74739,#74740,#74741,#74742));
#15405=EDGE_LOOP('',(#74743,#74744,#74745,#74746));
#15406=EDGE_LOOP('',(#74747,#74748,#74749,#74750));
#15407=EDGE_LOOP('',(#74751,#74752,#74753,#74754));
#15408=EDGE_LOOP('',(#74755,#74756,#74757,#74758));
#15409=EDGE_LOOP('',(#74759,#74760,#74761,#74762));
#15410=EDGE_LOOP('',(#74763,#74764,#74765,#74766));
#15411=EDGE_LOOP('',(#74767,#74768,#74769,#74770));
#15412=EDGE_LOOP('',(#74771,#74772,#74773,#74774));
#15413=EDGE_LOOP('',(#74775,#74776,#74777));
#15414=EDGE_LOOP('',(#74778,#74779,#74780,#74781,#74782));
#15415=EDGE_LOOP('',(#74783,#74784,#74785,#74786,#74787));
#15416=EDGE_LOOP('',(#74788,#74789,#74790,#74791));
#15417=EDGE_LOOP('',(#74792,#74793,#74794,#74795));
#15418=EDGE_LOOP('',(#74796,#74797,#74798));
#15419=EDGE_LOOP('',(#74799,#74800,#74801,#74802));
#15420=EDGE_LOOP('',(#74803,#74804,#74805,#74806));
#15421=EDGE_LOOP('',(#74807,#74808,#74809,#74810));
#15422=EDGE_LOOP('',(#74811,#74812,#74813,#74814));
#15423=EDGE_LOOP('',(#74815,#74816,#74817,#74818));
#15424=EDGE_LOOP('',(#74819,#74820,#74821,#74822));
#15425=EDGE_LOOP('',(#74823,#74824,#74825,#74826));
#15426=EDGE_LOOP('',(#74827,#74828,#74829,#74830));
#15427=EDGE_LOOP('',(#74831,#74832,#74833,#74834));
#15428=EDGE_LOOP('',(#74835,#74836,#74837,#74838));
#15429=EDGE_LOOP('',(#74839,#74840,#74841,#74842));
#15430=EDGE_LOOP('',(#74843,#74844,#74845));
#15431=EDGE_LOOP('',(#74846,#74847,#74848,#74849,#74850));
#15432=EDGE_LOOP('',(#74851,#74852,#74853,#74854,#74855));
#15433=EDGE_LOOP('',(#74856,#74857,#74858,#74859));
#15434=EDGE_LOOP('',(#74860,#74861,#74862,#74863));
#15435=EDGE_LOOP('',(#74864,#74865,#74866));
#15436=EDGE_LOOP('',(#74867,#74868,#74869,#74870));
#15437=EDGE_LOOP('',(#74871,#74872,#74873,#74874));
#15438=EDGE_LOOP('',(#74875,#74876,#74877,#74878));
#15439=EDGE_LOOP('',(#74879,#74880,#74881,#74882));
#15440=EDGE_LOOP('',(#74883,#74884,#74885,#74886));
#15441=EDGE_LOOP('',(#74887,#74888,#74889,#74890));
#15442=EDGE_LOOP('',(#74891,#74892,#74893,#74894));
#15443=EDGE_LOOP('',(#74895,#74896,#74897,#74898));
#15444=EDGE_LOOP('',(#74899,#74900,#74901,#74902));
#15445=EDGE_LOOP('',(#74903,#74904,#74905,#74906));
#15446=EDGE_LOOP('',(#74907,#74908,#74909,#74910));
#15447=EDGE_LOOP('',(#74911,#74912,#74913));
#15448=EDGE_LOOP('',(#74914,#74915,#74916,#74917,#74918));
#15449=EDGE_LOOP('',(#74919,#74920,#74921,#74922,#74923));
#15450=EDGE_LOOP('',(#74924,#74925,#74926,#74927));
#15451=EDGE_LOOP('',(#74928,#74929,#74930,#74931));
#15452=EDGE_LOOP('',(#74932,#74933,#74934));
#15453=EDGE_LOOP('',(#74935,#74936,#74937,#74938));
#15454=EDGE_LOOP('',(#74939,#74940,#74941,#74942));
#15455=EDGE_LOOP('',(#74943,#74944,#74945,#74946));
#15456=EDGE_LOOP('',(#74947,#74948,#74949,#74950));
#15457=EDGE_LOOP('',(#74951,#74952,#74953,#74954));
#15458=EDGE_LOOP('',(#74955,#74956,#74957,#74958));
#15459=EDGE_LOOP('',(#74959,#74960,#74961,#74962));
#15460=EDGE_LOOP('',(#74963,#74964,#74965,#74966));
#15461=EDGE_LOOP('',(#74967,#74968,#74969,#74970));
#15462=EDGE_LOOP('',(#74971,#74972,#74973,#74974));
#15463=EDGE_LOOP('',(#74975,#74976,#74977,#74978));
#15464=EDGE_LOOP('',(#74979,#74980,#74981));
#15465=EDGE_LOOP('',(#74982,#74983,#74984,#74985,#74986));
#15466=EDGE_LOOP('',(#74987,#74988,#74989,#74990,#74991));
#15467=EDGE_LOOP('',(#74992,#74993,#74994,#74995));
#15468=EDGE_LOOP('',(#74996,#74997,#74998,#74999));
#15469=EDGE_LOOP('',(#75000,#75001,#75002));
#15470=EDGE_LOOP('',(#75003,#75004,#75005,#75006));
#15471=EDGE_LOOP('',(#75007,#75008,#75009,#75010));
#15472=EDGE_LOOP('',(#75011,#75012,#75013,#75014));
#15473=EDGE_LOOP('',(#75015,#75016,#75017,#75018));
#15474=EDGE_LOOP('',(#75019,#75020,#75021,#75022));
#15475=EDGE_LOOP('',(#75023,#75024,#75025,#75026));
#15476=EDGE_LOOP('',(#75027,#75028,#75029,#75030));
#15477=EDGE_LOOP('',(#75031,#75032,#75033,#75034));
#15478=EDGE_LOOP('',(#75035,#75036,#75037,#75038));
#15479=EDGE_LOOP('',(#75039,#75040,#75041,#75042));
#15480=EDGE_LOOP('',(#75043,#75044,#75045,#75046));
#15481=EDGE_LOOP('',(#75047,#75048,#75049));
#15482=EDGE_LOOP('',(#75050,#75051,#75052,#75053,#75054));
#15483=EDGE_LOOP('',(#75055,#75056,#75057,#75058,#75059));
#15484=EDGE_LOOP('',(#75060,#75061,#75062,#75063));
#15485=EDGE_LOOP('',(#75064,#75065,#75066,#75067));
#15486=EDGE_LOOP('',(#75068,#75069,#75070));
#15487=EDGE_LOOP('',(#75071,#75072,#75073,#75074));
#15488=EDGE_LOOP('',(#75075,#75076,#75077,#75078));
#15489=EDGE_LOOP('',(#75079,#75080,#75081,#75082));
#15490=EDGE_LOOP('',(#75083,#75084,#75085,#75086));
#15491=EDGE_LOOP('',(#75087,#75088,#75089,#75090));
#15492=EDGE_LOOP('',(#75091,#75092,#75093,#75094));
#15493=EDGE_LOOP('',(#75095,#75096,#75097,#75098));
#15494=EDGE_LOOP('',(#75099,#75100,#75101,#75102));
#15495=EDGE_LOOP('',(#75103,#75104,#75105,#75106));
#15496=EDGE_LOOP('',(#75107,#75108,#75109,#75110));
#15497=EDGE_LOOP('',(#75111,#75112,#75113,#75114));
#15498=EDGE_LOOP('',(#75115,#75116,#75117));
#15499=EDGE_LOOP('',(#75118,#75119,#75120,#75121,#75122));
#15500=EDGE_LOOP('',(#75123,#75124,#75125,#75126,#75127));
#15501=EDGE_LOOP('',(#75128,#75129,#75130,#75131));
#15502=EDGE_LOOP('',(#75132,#75133,#75134,#75135));
#15503=EDGE_LOOP('',(#75136,#75137,#75138));
#15504=EDGE_LOOP('',(#75139,#75140,#75141,#75142));
#15505=EDGE_LOOP('',(#75143,#75144,#75145,#75146));
#15506=EDGE_LOOP('',(#75147,#75148,#75149,#75150));
#15507=EDGE_LOOP('',(#75151,#75152,#75153,#75154));
#15508=EDGE_LOOP('',(#75155,#75156,#75157,#75158));
#15509=EDGE_LOOP('',(#75159,#75160,#75161,#75162));
#15510=EDGE_LOOP('',(#75163,#75164,#75165,#75166));
#15511=EDGE_LOOP('',(#75167,#75168,#75169,#75170));
#15512=EDGE_LOOP('',(#75171,#75172,#75173,#75174));
#15513=EDGE_LOOP('',(#75175,#75176,#75177,#75178));
#15514=EDGE_LOOP('',(#75179,#75180,#75181,#75182));
#15515=EDGE_LOOP('',(#75183,#75184,#75185));
#15516=EDGE_LOOP('',(#75186,#75187,#75188,#75189,#75190));
#15517=EDGE_LOOP('',(#75191,#75192,#75193,#75194,#75195));
#15518=EDGE_LOOP('',(#75196,#75197,#75198,#75199));
#15519=EDGE_LOOP('',(#75200,#75201,#75202,#75203));
#15520=EDGE_LOOP('',(#75204,#75205,#75206));
#15521=EDGE_LOOP('',(#75207,#75208,#75209,#75210));
#15522=EDGE_LOOP('',(#75211,#75212,#75213,#75214));
#15523=EDGE_LOOP('',(#75215,#75216,#75217,#75218));
#15524=EDGE_LOOP('',(#75219,#75220,#75221,#75222));
#15525=EDGE_LOOP('',(#75223,#75224,#75225,#75226));
#15526=EDGE_LOOP('',(#75227,#75228,#75229,#75230));
#15527=EDGE_LOOP('',(#75231,#75232,#75233,#75234));
#15528=EDGE_LOOP('',(#75235,#75236,#75237,#75238));
#15529=EDGE_LOOP('',(#75239,#75240,#75241,#75242));
#15530=EDGE_LOOP('',(#75243,#75244,#75245,#75246));
#15531=EDGE_LOOP('',(#75247,#75248,#75249,#75250));
#15532=EDGE_LOOP('',(#75251,#75252,#75253));
#15533=EDGE_LOOP('',(#75254,#75255,#75256,#75257,#75258));
#15534=EDGE_LOOP('',(#75259,#75260,#75261,#75262,#75263));
#15535=EDGE_LOOP('',(#75264,#75265,#75266,#75267));
#15536=EDGE_LOOP('',(#75268,#75269,#75270,#75271));
#15537=EDGE_LOOP('',(#75272,#75273,#75274));
#15538=EDGE_LOOP('',(#75275,#75276,#75277,#75278));
#15539=EDGE_LOOP('',(#75279,#75280,#75281,#75282));
#15540=EDGE_LOOP('',(#75283,#75284,#75285,#75286));
#15541=EDGE_LOOP('',(#75287,#75288,#75289,#75290));
#15542=EDGE_LOOP('',(#75291,#75292,#75293,#75294));
#15543=EDGE_LOOP('',(#75295,#75296,#75297,#75298));
#15544=EDGE_LOOP('',(#75299,#75300,#75301,#75302));
#15545=EDGE_LOOP('',(#75303,#75304,#75305,#75306));
#15546=EDGE_LOOP('',(#75307,#75308,#75309,#75310));
#15547=EDGE_LOOP('',(#75311,#75312,#75313,#75314));
#15548=EDGE_LOOP('',(#75315,#75316,#75317,#75318));
#15549=EDGE_LOOP('',(#75319,#75320,#75321));
#15550=EDGE_LOOP('',(#75322,#75323,#75324,#75325,#75326));
#15551=EDGE_LOOP('',(#75327,#75328,#75329,#75330,#75331));
#15552=EDGE_LOOP('',(#75332,#75333,#75334,#75335));
#15553=EDGE_LOOP('',(#75336,#75337,#75338,#75339));
#15554=EDGE_LOOP('',(#75340,#75341,#75342));
#15555=EDGE_LOOP('',(#75343,#75344,#75345,#75346));
#15556=EDGE_LOOP('',(#75347,#75348,#75349,#75350));
#15557=EDGE_LOOP('',(#75351,#75352,#75353,#75354));
#15558=EDGE_LOOP('',(#75355,#75356,#75357,#75358));
#15559=EDGE_LOOP('',(#75359,#75360,#75361,#75362));
#15560=EDGE_LOOP('',(#75363,#75364,#75365,#75366));
#15561=EDGE_LOOP('',(#75367,#75368,#75369,#75370));
#15562=EDGE_LOOP('',(#75371,#75372,#75373,#75374));
#15563=EDGE_LOOP('',(#75375,#75376,#75377,#75378));
#15564=EDGE_LOOP('',(#75379,#75380,#75381,#75382));
#15565=EDGE_LOOP('',(#75383,#75384,#75385,#75386));
#15566=EDGE_LOOP('',(#75387,#75388,#75389));
#15567=EDGE_LOOP('',(#75390,#75391,#75392,#75393,#75394));
#15568=EDGE_LOOP('',(#75395,#75396,#75397,#75398,#75399));
#15569=EDGE_LOOP('',(#75400,#75401,#75402,#75403));
#15570=EDGE_LOOP('',(#75404,#75405,#75406,#75407));
#15571=EDGE_LOOP('',(#75408,#75409,#75410));
#15572=EDGE_LOOP('',(#75411,#75412,#75413,#75414));
#15573=EDGE_LOOP('',(#75415,#75416,#75417,#75418));
#15574=EDGE_LOOP('',(#75419,#75420,#75421,#75422));
#15575=EDGE_LOOP('',(#75423,#75424,#75425,#75426));
#15576=EDGE_LOOP('',(#75427,#75428,#75429,#75430));
#15577=EDGE_LOOP('',(#75431,#75432,#75433,#75434));
#15578=EDGE_LOOP('',(#75435,#75436,#75437,#75438));
#15579=EDGE_LOOP('',(#75439,#75440,#75441,#75442));
#15580=EDGE_LOOP('',(#75443,#75444,#75445,#75446));
#15581=EDGE_LOOP('',(#75447,#75448,#75449,#75450));
#15582=EDGE_LOOP('',(#75451,#75452,#75453,#75454));
#15583=EDGE_LOOP('',(#75455,#75456,#75457));
#15584=EDGE_LOOP('',(#75458,#75459,#75460,#75461,#75462));
#15585=EDGE_LOOP('',(#75463,#75464,#75465,#75466,#75467));
#15586=EDGE_LOOP('',(#75468,#75469,#75470,#75471));
#15587=EDGE_LOOP('',(#75472,#75473,#75474,#75475));
#15588=EDGE_LOOP('',(#75476,#75477,#75478));
#15589=EDGE_LOOP('',(#75479,#75480,#75481,#75482));
#15590=EDGE_LOOP('',(#75483,#75484,#75485,#75486));
#15591=EDGE_LOOP('',(#75487,#75488,#75489,#75490));
#15592=EDGE_LOOP('',(#75491,#75492,#75493,#75494));
#15593=EDGE_LOOP('',(#75495,#75496,#75497,#75498));
#15594=EDGE_LOOP('',(#75499,#75500,#75501,#75502));
#15595=EDGE_LOOP('',(#75503,#75504,#75505,#75506));
#15596=EDGE_LOOP('',(#75507,#75508,#75509,#75510));
#15597=EDGE_LOOP('',(#75511,#75512,#75513,#75514));
#15598=EDGE_LOOP('',(#75515,#75516,#75517,#75518));
#15599=EDGE_LOOP('',(#75519,#75520,#75521,#75522));
#15600=EDGE_LOOP('',(#75523,#75524,#75525));
#15601=EDGE_LOOP('',(#75526,#75527,#75528,#75529,#75530));
#15602=EDGE_LOOP('',(#75531,#75532,#75533,#75534,#75535));
#15603=EDGE_LOOP('',(#75536,#75537,#75538,#75539));
#15604=EDGE_LOOP('',(#75540,#75541,#75542,#75543));
#15605=EDGE_LOOP('',(#75544,#75545,#75546));
#15606=EDGE_LOOP('',(#75547,#75548,#75549,#75550));
#15607=EDGE_LOOP('',(#75551,#75552,#75553,#75554));
#15608=EDGE_LOOP('',(#75555,#75556,#75557,#75558));
#15609=EDGE_LOOP('',(#75559,#75560,#75561,#75562));
#15610=EDGE_LOOP('',(#75563,#75564,#75565,#75566));
#15611=EDGE_LOOP('',(#75567,#75568,#75569,#75570));
#15612=EDGE_LOOP('',(#75571,#75572,#75573,#75574));
#15613=EDGE_LOOP('',(#75575,#75576,#75577,#75578));
#15614=EDGE_LOOP('',(#75579,#75580,#75581,#75582));
#15615=EDGE_LOOP('',(#75583,#75584,#75585,#75586));
#15616=EDGE_LOOP('',(#75587,#75588,#75589,#75590));
#15617=EDGE_LOOP('',(#75591,#75592,#75593));
#15618=EDGE_LOOP('',(#75594,#75595,#75596,#75597,#75598));
#15619=EDGE_LOOP('',(#75599,#75600,#75601,#75602,#75603));
#15620=EDGE_LOOP('',(#75604,#75605,#75606,#75607));
#15621=EDGE_LOOP('',(#75608,#75609,#75610,#75611));
#15622=EDGE_LOOP('',(#75612,#75613,#75614));
#15623=EDGE_LOOP('',(#75615,#75616,#75617,#75618));
#15624=EDGE_LOOP('',(#75619,#75620,#75621,#75622));
#15625=EDGE_LOOP('',(#75623,#75624,#75625,#75626));
#15626=EDGE_LOOP('',(#75627,#75628,#75629,#75630));
#15627=EDGE_LOOP('',(#75631,#75632,#75633,#75634));
#15628=EDGE_LOOP('',(#75635,#75636,#75637,#75638));
#15629=EDGE_LOOP('',(#75639,#75640,#75641,#75642));
#15630=EDGE_LOOP('',(#75643,#75644,#75645,#75646));
#15631=EDGE_LOOP('',(#75647,#75648,#75649,#75650));
#15632=EDGE_LOOP('',(#75651,#75652,#75653,#75654));
#15633=EDGE_LOOP('',(#75655,#75656,#75657,#75658));
#15634=EDGE_LOOP('',(#75659,#75660,#75661));
#15635=EDGE_LOOP('',(#75662,#75663,#75664,#75665,#75666));
#15636=EDGE_LOOP('',(#75667,#75668,#75669,#75670,#75671));
#15637=EDGE_LOOP('',(#75672,#75673,#75674,#75675));
#15638=EDGE_LOOP('',(#75676,#75677,#75678,#75679));
#15639=EDGE_LOOP('',(#75680,#75681,#75682));
#15640=EDGE_LOOP('',(#75683,#75684,#75685,#75686));
#15641=EDGE_LOOP('',(#75687,#75688,#75689,#75690));
#15642=EDGE_LOOP('',(#75691,#75692,#75693,#75694));
#15643=EDGE_LOOP('',(#75695,#75696,#75697,#75698));
#15644=EDGE_LOOP('',(#75699,#75700,#75701,#75702));
#15645=EDGE_LOOP('',(#75703,#75704,#75705,#75706));
#15646=EDGE_LOOP('',(#75707,#75708,#75709,#75710));
#15647=EDGE_LOOP('',(#75711,#75712,#75713,#75714));
#15648=EDGE_LOOP('',(#75715,#75716,#75717,#75718));
#15649=EDGE_LOOP('',(#75719,#75720,#75721,#75722));
#15650=EDGE_LOOP('',(#75723,#75724,#75725,#75726));
#15651=EDGE_LOOP('',(#75727,#75728,#75729));
#15652=EDGE_LOOP('',(#75730,#75731,#75732,#75733,#75734));
#15653=EDGE_LOOP('',(#75735,#75736,#75737,#75738,#75739));
#15654=EDGE_LOOP('',(#75740,#75741,#75742,#75743));
#15655=EDGE_LOOP('',(#75744,#75745,#75746,#75747));
#15656=EDGE_LOOP('',(#75748,#75749,#75750));
#15657=EDGE_LOOP('',(#75751,#75752,#75753,#75754));
#15658=EDGE_LOOP('',(#75755,#75756,#75757,#75758));
#15659=EDGE_LOOP('',(#75759,#75760,#75761,#75762));
#15660=EDGE_LOOP('',(#75763,#75764,#75765,#75766));
#15661=EDGE_LOOP('',(#75767,#75768,#75769,#75770));
#15662=EDGE_LOOP('',(#75771,#75772,#75773,#75774));
#15663=EDGE_LOOP('',(#75775,#75776,#75777,#75778));
#15664=EDGE_LOOP('',(#75779,#75780,#75781,#75782));
#15665=EDGE_LOOP('',(#75783,#75784,#75785,#75786));
#15666=EDGE_LOOP('',(#75787,#75788,#75789,#75790));
#15667=EDGE_LOOP('',(#75791,#75792,#75793,#75794));
#15668=EDGE_LOOP('',(#75795,#75796,#75797));
#15669=EDGE_LOOP('',(#75798,#75799,#75800,#75801,#75802));
#15670=EDGE_LOOP('',(#75803,#75804,#75805,#75806,#75807));
#15671=EDGE_LOOP('',(#75808,#75809,#75810,#75811));
#15672=EDGE_LOOP('',(#75812,#75813,#75814,#75815));
#15673=EDGE_LOOP('',(#75816,#75817,#75818));
#15674=EDGE_LOOP('',(#75819,#75820,#75821,#75822));
#15675=EDGE_LOOP('',(#75823,#75824,#75825,#75826));
#15676=EDGE_LOOP('',(#75827,#75828,#75829,#75830));
#15677=EDGE_LOOP('',(#75831,#75832,#75833,#75834));
#15678=EDGE_LOOP('',(#75835,#75836,#75837,#75838));
#15679=EDGE_LOOP('',(#75839,#75840,#75841,#75842));
#15680=EDGE_LOOP('',(#75843,#75844,#75845,#75846));
#15681=EDGE_LOOP('',(#75847,#75848,#75849,#75850));
#15682=EDGE_LOOP('',(#75851,#75852,#75853,#75854));
#15683=EDGE_LOOP('',(#75855,#75856,#75857,#75858));
#15684=EDGE_LOOP('',(#75859,#75860,#75861,#75862));
#15685=EDGE_LOOP('',(#75863,#75864,#75865));
#15686=EDGE_LOOP('',(#75866,#75867,#75868,#75869,#75870));
#15687=EDGE_LOOP('',(#75871,#75872,#75873,#75874,#75875));
#15688=EDGE_LOOP('',(#75876,#75877,#75878,#75879));
#15689=EDGE_LOOP('',(#75880,#75881,#75882,#75883));
#15690=EDGE_LOOP('',(#75884,#75885,#75886));
#15691=EDGE_LOOP('',(#75887,#75888,#75889,#75890));
#15692=EDGE_LOOP('',(#75891,#75892,#75893,#75894));
#15693=EDGE_LOOP('',(#75895,#75896,#75897,#75898));
#15694=EDGE_LOOP('',(#75899,#75900,#75901,#75902));
#15695=EDGE_LOOP('',(#75903,#75904,#75905,#75906));
#15696=EDGE_LOOP('',(#75907,#75908,#75909,#75910));
#15697=EDGE_LOOP('',(#75911,#75912,#75913,#75914));
#15698=EDGE_LOOP('',(#75915,#75916,#75917,#75918));
#15699=EDGE_LOOP('',(#75919,#75920,#75921,#75922));
#15700=EDGE_LOOP('',(#75923,#75924,#75925,#75926));
#15701=EDGE_LOOP('',(#75927,#75928,#75929,#75930));
#15702=EDGE_LOOP('',(#75931,#75932,#75933));
#15703=EDGE_LOOP('',(#75934,#75935,#75936,#75937,#75938));
#15704=EDGE_LOOP('',(#75939,#75940,#75941,#75942,#75943));
#15705=EDGE_LOOP('',(#75944,#75945,#75946,#75947));
#15706=EDGE_LOOP('',(#75948,#75949,#75950,#75951));
#15707=EDGE_LOOP('',(#75952,#75953,#75954));
#15708=EDGE_LOOP('',(#75955,#75956,#75957,#75958));
#15709=EDGE_LOOP('',(#75959,#75960,#75961,#75962));
#15710=EDGE_LOOP('',(#75963,#75964,#75965,#75966));
#15711=EDGE_LOOP('',(#75967,#75968,#75969,#75970));
#15712=EDGE_LOOP('',(#75971,#75972,#75973,#75974));
#15713=EDGE_LOOP('',(#75975,#75976,#75977,#75978));
#15714=EDGE_LOOP('',(#75979,#75980,#75981,#75982));
#15715=EDGE_LOOP('',(#75983,#75984,#75985,#75986));
#15716=EDGE_LOOP('',(#75987,#75988,#75989,#75990));
#15717=EDGE_LOOP('',(#75991,#75992,#75993,#75994));
#15718=EDGE_LOOP('',(#75995,#75996,#75997,#75998));
#15719=EDGE_LOOP('',(#75999,#76000,#76001));
#15720=EDGE_LOOP('',(#76002,#76003,#76004,#76005,#76006));
#15721=EDGE_LOOP('',(#76007,#76008,#76009,#76010,#76011));
#15722=EDGE_LOOP('',(#76012,#76013,#76014,#76015));
#15723=EDGE_LOOP('',(#76016,#76017,#76018,#76019));
#15724=EDGE_LOOP('',(#76020,#76021,#76022));
#15725=EDGE_LOOP('',(#76023,#76024,#76025,#76026));
#15726=EDGE_LOOP('',(#76027,#76028,#76029,#76030));
#15727=EDGE_LOOP('',(#76031,#76032,#76033,#76034));
#15728=EDGE_LOOP('',(#76035,#76036,#76037,#76038));
#15729=EDGE_LOOP('',(#76039,#76040,#76041,#76042));
#15730=EDGE_LOOP('',(#76043,#76044,#76045,#76046));
#15731=EDGE_LOOP('',(#76047,#76048,#76049,#76050));
#15732=EDGE_LOOP('',(#76051,#76052,#76053,#76054));
#15733=EDGE_LOOP('',(#76055,#76056,#76057,#76058));
#15734=EDGE_LOOP('',(#76059,#76060,#76061,#76062));
#15735=EDGE_LOOP('',(#76063,#76064,#76065,#76066));
#15736=EDGE_LOOP('',(#76067,#76068,#76069));
#15737=EDGE_LOOP('',(#76070,#76071,#76072,#76073,#76074));
#15738=EDGE_LOOP('',(#76075,#76076,#76077,#76078,#76079));
#15739=EDGE_LOOP('',(#76080,#76081,#76082,#76083));
#15740=EDGE_LOOP('',(#76084,#76085,#76086,#76087));
#15741=EDGE_LOOP('',(#76088,#76089,#76090));
#15742=EDGE_LOOP('',(#76091,#76092,#76093,#76094));
#15743=EDGE_LOOP('',(#76095,#76096,#76097,#76098));
#15744=EDGE_LOOP('',(#76099,#76100,#76101,#76102));
#15745=EDGE_LOOP('',(#76103,#76104,#76105,#76106));
#15746=EDGE_LOOP('',(#76107,#76108,#76109,#76110));
#15747=EDGE_LOOP('',(#76111,#76112,#76113,#76114));
#15748=EDGE_LOOP('',(#76115,#76116,#76117,#76118));
#15749=EDGE_LOOP('',(#76119,#76120,#76121,#76122));
#15750=EDGE_LOOP('',(#76123,#76124,#76125,#76126));
#15751=EDGE_LOOP('',(#76127,#76128,#76129,#76130));
#15752=EDGE_LOOP('',(#76131,#76132,#76133,#76134));
#15753=EDGE_LOOP('',(#76135,#76136,#76137));
#15754=EDGE_LOOP('',(#76138,#76139,#76140,#76141,#76142));
#15755=EDGE_LOOP('',(#76143,#76144,#76145,#76146,#76147));
#15756=EDGE_LOOP('',(#76148,#76149,#76150,#76151));
#15757=EDGE_LOOP('',(#76152,#76153,#76154,#76155));
#15758=EDGE_LOOP('',(#76156,#76157,#76158));
#15759=EDGE_LOOP('',(#76159,#76160,#76161,#76162));
#15760=EDGE_LOOP('',(#76163,#76164,#76165,#76166));
#15761=EDGE_LOOP('',(#76167,#76168,#76169,#76170));
#15762=EDGE_LOOP('',(#76171,#76172,#76173,#76174));
#15763=EDGE_LOOP('',(#76175,#76176,#76177,#76178));
#15764=EDGE_LOOP('',(#76179,#76180,#76181,#76182));
#15765=EDGE_LOOP('',(#76183,#76184,#76185,#76186));
#15766=EDGE_LOOP('',(#76187,#76188,#76189,#76190));
#15767=EDGE_LOOP('',(#76191,#76192,#76193,#76194));
#15768=EDGE_LOOP('',(#76195,#76196,#76197,#76198));
#15769=EDGE_LOOP('',(#76199,#76200,#76201,#76202));
#15770=EDGE_LOOP('',(#76203,#76204,#76205));
#15771=EDGE_LOOP('',(#76206,#76207,#76208,#76209,#76210));
#15772=EDGE_LOOP('',(#76211,#76212,#76213,#76214,#76215));
#15773=EDGE_LOOP('',(#76216,#76217,#76218,#76219));
#15774=EDGE_LOOP('',(#76220,#76221,#76222,#76223));
#15775=EDGE_LOOP('',(#76224,#76225,#76226));
#15776=EDGE_LOOP('',(#76227,#76228,#76229,#76230));
#15777=EDGE_LOOP('',(#76231,#76232,#76233,#76234));
#15778=EDGE_LOOP('',(#76235,#76236,#76237,#76238));
#15779=EDGE_LOOP('',(#76239,#76240,#76241,#76242));
#15780=EDGE_LOOP('',(#76243,#76244,#76245,#76246));
#15781=EDGE_LOOP('',(#76247,#76248,#76249,#76250));
#15782=EDGE_LOOP('',(#76251,#76252,#76253,#76254));
#15783=EDGE_LOOP('',(#76255,#76256,#76257,#76258));
#15784=EDGE_LOOP('',(#76259,#76260,#76261,#76262));
#15785=EDGE_LOOP('',(#76263,#76264,#76265,#76266));
#15786=EDGE_LOOP('',(#76267,#76268,#76269,#76270));
#15787=EDGE_LOOP('',(#76271,#76272,#76273));
#15788=EDGE_LOOP('',(#76274,#76275,#76276,#76277,#76278));
#15789=EDGE_LOOP('',(#76279,#76280,#76281,#76282,#76283));
#15790=EDGE_LOOP('',(#76284,#76285,#76286,#76287));
#15791=EDGE_LOOP('',(#76288,#76289,#76290,#76291));
#15792=EDGE_LOOP('',(#76292,#76293,#76294));
#15793=EDGE_LOOP('',(#76295,#76296,#76297,#76298));
#15794=EDGE_LOOP('',(#76299,#76300,#76301,#76302));
#15795=EDGE_LOOP('',(#76303,#76304,#76305,#76306));
#15796=EDGE_LOOP('',(#76307,#76308,#76309,#76310));
#15797=EDGE_LOOP('',(#76311,#76312,#76313,#76314));
#15798=EDGE_LOOP('',(#76315,#76316,#76317,#76318));
#15799=EDGE_LOOP('',(#76319,#76320,#76321,#76322));
#15800=EDGE_LOOP('',(#76323,#76324,#76325,#76326));
#15801=EDGE_LOOP('',(#76327,#76328,#76329,#76330));
#15802=EDGE_LOOP('',(#76331,#76332,#76333,#76334));
#15803=EDGE_LOOP('',(#76335,#76336,#76337,#76338));
#15804=EDGE_LOOP('',(#76339,#76340,#76341));
#15805=EDGE_LOOP('',(#76342,#76343,#76344,#76345,#76346));
#15806=EDGE_LOOP('',(#76347,#76348,#76349,#76350,#76351));
#15807=EDGE_LOOP('',(#76352,#76353,#76354,#76355));
#15808=EDGE_LOOP('',(#76356,#76357,#76358,#76359));
#15809=EDGE_LOOP('',(#76360,#76361,#76362));
#15810=EDGE_LOOP('',(#76363,#76364,#76365,#76366));
#15811=EDGE_LOOP('',(#76367,#76368,#76369,#76370));
#15812=EDGE_LOOP('',(#76371,#76372,#76373,#76374));
#15813=EDGE_LOOP('',(#76375,#76376,#76377,#76378));
#15814=EDGE_LOOP('',(#76379,#76380,#76381,#76382));
#15815=EDGE_LOOP('',(#76383,#76384,#76385,#76386));
#15816=EDGE_LOOP('',(#76387,#76388,#76389,#76390));
#15817=EDGE_LOOP('',(#76391,#76392,#76393,#76394));
#15818=EDGE_LOOP('',(#76395,#76396,#76397,#76398));
#15819=EDGE_LOOP('',(#76399,#76400,#76401,#76402));
#15820=EDGE_LOOP('',(#76403,#76404,#76405,#76406));
#15821=EDGE_LOOP('',(#76407,#76408,#76409));
#15822=EDGE_LOOP('',(#76410,#76411,#76412,#76413,#76414));
#15823=EDGE_LOOP('',(#76415,#76416,#76417,#76418,#76419));
#15824=EDGE_LOOP('',(#76420,#76421,#76422,#76423));
#15825=EDGE_LOOP('',(#76424,#76425,#76426,#76427));
#15826=EDGE_LOOP('',(#76428,#76429,#76430));
#15827=EDGE_LOOP('',(#76431,#76432,#76433,#76434));
#15828=EDGE_LOOP('',(#76435,#76436,#76437,#76438));
#15829=EDGE_LOOP('',(#76439,#76440,#76441,#76442));
#15830=EDGE_LOOP('',(#76443,#76444,#76445,#76446));
#15831=EDGE_LOOP('',(#76447,#76448,#76449,#76450));
#15832=EDGE_LOOP('',(#76451,#76452,#76453,#76454));
#15833=EDGE_LOOP('',(#76455,#76456,#76457,#76458));
#15834=EDGE_LOOP('',(#76459,#76460,#76461,#76462));
#15835=EDGE_LOOP('',(#76463,#76464,#76465,#76466));
#15836=EDGE_LOOP('',(#76467,#76468,#76469,#76470));
#15837=EDGE_LOOP('',(#76471,#76472,#76473,#76474));
#15838=EDGE_LOOP('',(#76475,#76476,#76477));
#15839=EDGE_LOOP('',(#76478,#76479,#76480,#76481,#76482));
#15840=EDGE_LOOP('',(#76483,#76484,#76485,#76486,#76487));
#15841=EDGE_LOOP('',(#76488,#76489,#76490,#76491));
#15842=EDGE_LOOP('',(#76492,#76493,#76494,#76495));
#15843=EDGE_LOOP('',(#76496,#76497,#76498));
#15844=EDGE_LOOP('',(#76499,#76500,#76501,#76502));
#15845=EDGE_LOOP('',(#76503,#76504,#76505,#76506));
#15846=EDGE_LOOP('',(#76507,#76508,#76509,#76510));
#15847=EDGE_LOOP('',(#76511,#76512,#76513,#76514));
#15848=EDGE_LOOP('',(#76515,#76516,#76517,#76518));
#15849=EDGE_LOOP('',(#76519,#76520,#76521,#76522));
#15850=EDGE_LOOP('',(#76523,#76524,#76525,#76526));
#15851=EDGE_LOOP('',(#76527,#76528,#76529,#76530));
#15852=EDGE_LOOP('',(#76531,#76532,#76533,#76534));
#15853=EDGE_LOOP('',(#76535,#76536,#76537,#76538));
#15854=EDGE_LOOP('',(#76539,#76540,#76541,#76542));
#15855=EDGE_LOOP('',(#76543,#76544,#76545));
#15856=EDGE_LOOP('',(#76546,#76547,#76548,#76549,#76550));
#15857=EDGE_LOOP('',(#76551,#76552,#76553,#76554,#76555));
#15858=EDGE_LOOP('',(#76556,#76557,#76558,#76559));
#15859=EDGE_LOOP('',(#76560,#76561,#76562,#76563));
#15860=EDGE_LOOP('',(#76564,#76565,#76566));
#15861=EDGE_LOOP('',(#76567,#76568,#76569,#76570));
#15862=EDGE_LOOP('',(#76571,#76572,#76573,#76574));
#15863=EDGE_LOOP('',(#76575,#76576,#76577,#76578));
#15864=EDGE_LOOP('',(#76579,#76580,#76581,#76582));
#15865=EDGE_LOOP('',(#76583,#76584,#76585,#76586));
#15866=EDGE_LOOP('',(#76587,#76588,#76589,#76590));
#15867=EDGE_LOOP('',(#76591,#76592,#76593,#76594));
#15868=EDGE_LOOP('',(#76595,#76596,#76597,#76598));
#15869=EDGE_LOOP('',(#76599,#76600,#76601,#76602));
#15870=EDGE_LOOP('',(#76603,#76604,#76605,#76606));
#15871=EDGE_LOOP('',(#76607,#76608,#76609,#76610));
#15872=EDGE_LOOP('',(#76611,#76612,#76613));
#15873=EDGE_LOOP('',(#76614,#76615,#76616,#76617,#76618));
#15874=EDGE_LOOP('',(#76619,#76620,#76621,#76622,#76623));
#15875=EDGE_LOOP('',(#76624,#76625,#76626,#76627));
#15876=EDGE_LOOP('',(#76628,#76629,#76630,#76631));
#15877=EDGE_LOOP('',(#76632,#76633,#76634));
#15878=EDGE_LOOP('',(#76635,#76636,#76637,#76638));
#15879=EDGE_LOOP('',(#76639,#76640,#76641,#76642));
#15880=EDGE_LOOP('',(#76643,#76644,#76645,#76646));
#15881=EDGE_LOOP('',(#76647,#76648,#76649,#76650));
#15882=EDGE_LOOP('',(#76651,#76652,#76653,#76654));
#15883=EDGE_LOOP('',(#76655,#76656,#76657,#76658));
#15884=EDGE_LOOP('',(#76659,#76660,#76661,#76662));
#15885=EDGE_LOOP('',(#76663,#76664,#76665,#76666));
#15886=EDGE_LOOP('',(#76667,#76668,#76669,#76670));
#15887=EDGE_LOOP('',(#76671,#76672,#76673,#76674));
#15888=EDGE_LOOP('',(#76675,#76676,#76677,#76678));
#15889=EDGE_LOOP('',(#76679,#76680,#76681));
#15890=EDGE_LOOP('',(#76682,#76683,#76684,#76685,#76686));
#15891=EDGE_LOOP('',(#76687,#76688,#76689,#76690,#76691));
#15892=EDGE_LOOP('',(#76692,#76693,#76694,#76695));
#15893=EDGE_LOOP('',(#76696,#76697,#76698,#76699));
#15894=EDGE_LOOP('',(#76700,#76701,#76702));
#15895=EDGE_LOOP('',(#76703,#76704,#76705,#76706));
#15896=EDGE_LOOP('',(#76707,#76708,#76709,#76710));
#15897=EDGE_LOOP('',(#76711,#76712,#76713,#76714));
#15898=EDGE_LOOP('',(#76715,#76716,#76717,#76718));
#15899=EDGE_LOOP('',(#76719,#76720,#76721,#76722));
#15900=EDGE_LOOP('',(#76723,#76724,#76725,#76726));
#15901=EDGE_LOOP('',(#76727,#76728,#76729,#76730));
#15902=EDGE_LOOP('',(#76731,#76732,#76733,#76734));
#15903=EDGE_LOOP('',(#76735,#76736,#76737,#76738));
#15904=EDGE_LOOP('',(#76739,#76740,#76741,#76742));
#15905=EDGE_LOOP('',(#76743,#76744,#76745,#76746));
#15906=EDGE_LOOP('',(#76747,#76748,#76749));
#15907=EDGE_LOOP('',(#76750,#76751,#76752,#76753,#76754));
#15908=EDGE_LOOP('',(#76755,#76756,#76757,#76758,#76759));
#15909=EDGE_LOOP('',(#76760,#76761,#76762,#76763));
#15910=EDGE_LOOP('',(#76764,#76765,#76766,#76767));
#15911=EDGE_LOOP('',(#76768,#76769,#76770));
#15912=EDGE_LOOP('',(#76771,#76772,#76773,#76774));
#15913=EDGE_LOOP('',(#76775,#76776,#76777,#76778));
#15914=EDGE_LOOP('',(#76779,#76780,#76781,#76782));
#15915=EDGE_LOOP('',(#76783,#76784,#76785,#76786));
#15916=EDGE_LOOP('',(#76787,#76788,#76789,#76790));
#15917=EDGE_LOOP('',(#76791,#76792,#76793,#76794));
#15918=EDGE_LOOP('',(#76795,#76796,#76797,#76798));
#15919=EDGE_LOOP('',(#76799,#76800,#76801,#76802));
#15920=EDGE_LOOP('',(#76803,#76804,#76805,#76806));
#15921=EDGE_LOOP('',(#76807,#76808,#76809,#76810));
#15922=EDGE_LOOP('',(#76811,#76812,#76813,#76814));
#15923=EDGE_LOOP('',(#76815,#76816,#76817));
#15924=EDGE_LOOP('',(#76818,#76819,#76820,#76821,#76822));
#15925=EDGE_LOOP('',(#76823,#76824,#76825,#76826,#76827));
#15926=EDGE_LOOP('',(#76828,#76829,#76830,#76831));
#15927=EDGE_LOOP('',(#76832,#76833,#76834,#76835));
#15928=EDGE_LOOP('',(#76836,#76837,#76838));
#15929=EDGE_LOOP('',(#76839,#76840,#76841,#76842));
#15930=EDGE_LOOP('',(#76843,#76844,#76845,#76846));
#15931=EDGE_LOOP('',(#76847,#76848,#76849,#76850));
#15932=EDGE_LOOP('',(#76851,#76852,#76853,#76854));
#15933=EDGE_LOOP('',(#76855,#76856,#76857,#76858));
#15934=EDGE_LOOP('',(#76859,#76860,#76861,#76862));
#15935=EDGE_LOOP('',(#76863,#76864,#76865,#76866));
#15936=EDGE_LOOP('',(#76867,#76868,#76869,#76870));
#15937=EDGE_LOOP('',(#76871,#76872,#76873,#76874));
#15938=EDGE_LOOP('',(#76875,#76876,#76877,#76878));
#15939=EDGE_LOOP('',(#76879,#76880,#76881,#76882));
#15940=EDGE_LOOP('',(#76883,#76884,#76885));
#15941=EDGE_LOOP('',(#76886,#76887,#76888,#76889,#76890));
#15942=EDGE_LOOP('',(#76891,#76892,#76893,#76894,#76895));
#15943=EDGE_LOOP('',(#76896,#76897,#76898,#76899));
#15944=EDGE_LOOP('',(#76900,#76901,#76902,#76903));
#15945=EDGE_LOOP('',(#76904,#76905,#76906));
#15946=EDGE_LOOP('',(#76907,#76908,#76909,#76910));
#15947=EDGE_LOOP('',(#76911,#76912,#76913,#76914));
#15948=EDGE_LOOP('',(#76915,#76916,#76917,#76918));
#15949=EDGE_LOOP('',(#76919,#76920,#76921,#76922));
#15950=EDGE_LOOP('',(#76923,#76924,#76925,#76926));
#15951=EDGE_LOOP('',(#76927,#76928,#76929,#76930));
#15952=EDGE_LOOP('',(#76931,#76932,#76933,#76934));
#15953=EDGE_LOOP('',(#76935,#76936,#76937,#76938));
#15954=EDGE_LOOP('',(#76939,#76940,#76941,#76942));
#15955=EDGE_LOOP('',(#76943,#76944,#76945,#76946));
#15956=EDGE_LOOP('',(#76947,#76948,#76949,#76950));
#15957=EDGE_LOOP('',(#76951,#76952,#76953));
#15958=EDGE_LOOP('',(#76954,#76955,#76956,#76957,#76958));
#15959=EDGE_LOOP('',(#76959,#76960,#76961,#76962,#76963));
#15960=EDGE_LOOP('',(#76964,#76965,#76966,#76967));
#15961=EDGE_LOOP('',(#76968,#76969,#76970,#76971));
#15962=EDGE_LOOP('',(#76972,#76973,#76974));
#15963=EDGE_LOOP('',(#76975,#76976,#76977,#76978));
#15964=EDGE_LOOP('',(#76979,#76980,#76981,#76982));
#15965=EDGE_LOOP('',(#76983,#76984,#76985,#76986));
#15966=EDGE_LOOP('',(#76987,#76988,#76989,#76990));
#15967=EDGE_LOOP('',(#76991,#76992,#76993,#76994));
#15968=EDGE_LOOP('',(#76995,#76996,#76997,#76998));
#15969=EDGE_LOOP('',(#76999,#77000,#77001,#77002));
#15970=EDGE_LOOP('',(#77003,#77004,#77005,#77006));
#15971=EDGE_LOOP('',(#77007,#77008,#77009,#77010));
#15972=EDGE_LOOP('',(#77011,#77012,#77013,#77014));
#15973=EDGE_LOOP('',(#77015,#77016,#77017,#77018));
#15974=EDGE_LOOP('',(#77019,#77020,#77021));
#15975=EDGE_LOOP('',(#77022,#77023,#77024,#77025,#77026));
#15976=EDGE_LOOP('',(#77027,#77028,#77029,#77030,#77031));
#15977=EDGE_LOOP('',(#77032,#77033,#77034,#77035));
#15978=EDGE_LOOP('',(#77036,#77037,#77038,#77039));
#15979=EDGE_LOOP('',(#77040,#77041,#77042));
#15980=EDGE_LOOP('',(#77043,#77044,#77045,#77046));
#15981=EDGE_LOOP('',(#77047,#77048,#77049,#77050));
#15982=EDGE_LOOP('',(#77051,#77052,#77053,#77054));
#15983=EDGE_LOOP('',(#77055,#77056,#77057,#77058));
#15984=EDGE_LOOP('',(#77059,#77060,#77061,#77062));
#15985=EDGE_LOOP('',(#77063,#77064,#77065,#77066));
#15986=EDGE_LOOP('',(#77067,#77068,#77069,#77070));
#15987=EDGE_LOOP('',(#77071,#77072,#77073,#77074));
#15988=EDGE_LOOP('',(#77075,#77076,#77077,#77078));
#15989=EDGE_LOOP('',(#77079,#77080,#77081,#77082));
#15990=EDGE_LOOP('',(#77083,#77084,#77085,#77086));
#15991=EDGE_LOOP('',(#77087,#77088,#77089));
#15992=EDGE_LOOP('',(#77090,#77091,#77092,#77093,#77094));
#15993=EDGE_LOOP('',(#77095,#77096,#77097,#77098,#77099));
#15994=EDGE_LOOP('',(#77100,#77101,#77102,#77103));
#15995=EDGE_LOOP('',(#77104,#77105,#77106,#77107));
#15996=EDGE_LOOP('',(#77108,#77109,#77110));
#15997=EDGE_LOOP('',(#77111,#77112,#77113,#77114));
#15998=EDGE_LOOP('',(#77115,#77116,#77117,#77118));
#15999=EDGE_LOOP('',(#77119,#77120,#77121,#77122));
#16000=EDGE_LOOP('',(#77123,#77124,#77125,#77126));
#16001=EDGE_LOOP('',(#77127,#77128,#77129,#77130));
#16002=EDGE_LOOP('',(#77131,#77132,#77133,#77134));
#16003=EDGE_LOOP('',(#77135,#77136,#77137,#77138));
#16004=EDGE_LOOP('',(#77139,#77140,#77141,#77142));
#16005=EDGE_LOOP('',(#77143,#77144,#77145,#77146));
#16006=EDGE_LOOP('',(#77147,#77148,#77149,#77150));
#16007=EDGE_LOOP('',(#77151,#77152,#77153,#77154));
#16008=EDGE_LOOP('',(#77155,#77156,#77157));
#16009=EDGE_LOOP('',(#77158,#77159,#77160,#77161,#77162));
#16010=EDGE_LOOP('',(#77163,#77164,#77165,#77166,#77167));
#16011=EDGE_LOOP('',(#77168,#77169,#77170,#77171));
#16012=EDGE_LOOP('',(#77172,#77173,#77174,#77175));
#16013=EDGE_LOOP('',(#77176,#77177,#77178));
#16014=EDGE_LOOP('',(#77179,#77180,#77181,#77182));
#16015=EDGE_LOOP('',(#77183,#77184,#77185,#77186));
#16016=EDGE_LOOP('',(#77187,#77188,#77189,#77190));
#16017=EDGE_LOOP('',(#77191,#77192,#77193,#77194));
#16018=EDGE_LOOP('',(#77195,#77196,#77197,#77198));
#16019=EDGE_LOOP('',(#77199,#77200,#77201,#77202));
#16020=EDGE_LOOP('',(#77203,#77204,#77205,#77206));
#16021=EDGE_LOOP('',(#77207,#77208,#77209,#77210));
#16022=EDGE_LOOP('',(#77211,#77212,#77213,#77214));
#16023=EDGE_LOOP('',(#77215,#77216,#77217,#77218));
#16024=EDGE_LOOP('',(#77219,#77220,#77221,#77222));
#16025=EDGE_LOOP('',(#77223,#77224,#77225));
#16026=EDGE_LOOP('',(#77226,#77227,#77228,#77229,#77230));
#16027=EDGE_LOOP('',(#77231,#77232,#77233,#77234,#77235));
#16028=EDGE_LOOP('',(#77236,#77237,#77238,#77239));
#16029=EDGE_LOOP('',(#77240,#77241,#77242,#77243));
#16030=EDGE_LOOP('',(#77244,#77245,#77246));
#16031=EDGE_LOOP('',(#77247,#77248,#77249,#77250));
#16032=EDGE_LOOP('',(#77251,#77252,#77253,#77254));
#16033=EDGE_LOOP('',(#77255,#77256,#77257,#77258));
#16034=EDGE_LOOP('',(#77259,#77260,#77261,#77262));
#16035=EDGE_LOOP('',(#77263,#77264,#77265,#77266));
#16036=EDGE_LOOP('',(#77267,#77268,#77269,#77270));
#16037=EDGE_LOOP('',(#77271,#77272,#77273,#77274));
#16038=EDGE_LOOP('',(#77275,#77276,#77277,#77278));
#16039=EDGE_LOOP('',(#77279,#77280,#77281,#77282));
#16040=EDGE_LOOP('',(#77283,#77284,#77285,#77286));
#16041=EDGE_LOOP('',(#77287,#77288,#77289,#77290));
#16042=EDGE_LOOP('',(#77291,#77292,#77293));
#16043=EDGE_LOOP('',(#77294,#77295,#77296,#77297,#77298));
#16044=EDGE_LOOP('',(#77299,#77300,#77301,#77302,#77303));
#16045=EDGE_LOOP('',(#77304,#77305,#77306,#77307));
#16046=EDGE_LOOP('',(#77308,#77309,#77310,#77311));
#16047=EDGE_LOOP('',(#77312,#77313,#77314));
#16048=EDGE_LOOP('',(#77315,#77316,#77317,#77318));
#16049=EDGE_LOOP('',(#77319,#77320,#77321,#77322));
#16050=EDGE_LOOP('',(#77323,#77324,#77325,#77326));
#16051=EDGE_LOOP('',(#77327,#77328,#77329,#77330));
#16052=EDGE_LOOP('',(#77331,#77332,#77333,#77334));
#16053=EDGE_LOOP('',(#77335,#77336,#77337,#77338));
#16054=EDGE_LOOP('',(#77339,#77340,#77341,#77342));
#16055=EDGE_LOOP('',(#77343,#77344,#77345,#77346));
#16056=EDGE_LOOP('',(#77347,#77348,#77349,#77350));
#16057=EDGE_LOOP('',(#77351,#77352,#77353,#77354));
#16058=EDGE_LOOP('',(#77355,#77356,#77357,#77358));
#16059=EDGE_LOOP('',(#77359,#77360,#77361));
#16060=EDGE_LOOP('',(#77362,#77363,#77364,#77365,#77366));
#16061=EDGE_LOOP('',(#77367,#77368,#77369,#77370,#77371));
#16062=EDGE_LOOP('',(#77372,#77373,#77374,#77375));
#16063=EDGE_LOOP('',(#77376,#77377,#77378,#77379));
#16064=EDGE_LOOP('',(#77380,#77381,#77382));
#16065=EDGE_LOOP('',(#77383,#77384,#77385,#77386));
#16066=EDGE_LOOP('',(#77387,#77388,#77389,#77390));
#16067=EDGE_LOOP('',(#77391,#77392,#77393,#77394));
#16068=EDGE_LOOP('',(#77395,#77396,#77397,#77398));
#16069=EDGE_LOOP('',(#77399,#77400,#77401,#77402));
#16070=EDGE_LOOP('',(#77403,#77404,#77405,#77406));
#16071=EDGE_LOOP('',(#77407,#77408,#77409,#77410));
#16072=EDGE_LOOP('',(#77411,#77412,#77413,#77414));
#16073=EDGE_LOOP('',(#77415,#77416,#77417,#77418));
#16074=EDGE_LOOP('',(#77419,#77420,#77421,#77422));
#16075=EDGE_LOOP('',(#77423,#77424,#77425,#77426));
#16076=EDGE_LOOP('',(#77427,#77428,#77429));
#16077=EDGE_LOOP('',(#77430,#77431,#77432,#77433,#77434));
#16078=EDGE_LOOP('',(#77435,#77436,#77437,#77438,#77439));
#16079=EDGE_LOOP('',(#77440,#77441,#77442,#77443));
#16080=EDGE_LOOP('',(#77444,#77445,#77446,#77447));
#16081=EDGE_LOOP('',(#77448,#77449,#77450));
#16082=EDGE_LOOP('',(#77451,#77452,#77453,#77454));
#16083=EDGE_LOOP('',(#77455,#77456,#77457,#77458));
#16084=EDGE_LOOP('',(#77459,#77460,#77461,#77462));
#16085=EDGE_LOOP('',(#77463,#77464,#77465,#77466));
#16086=EDGE_LOOP('',(#77467,#77468,#77469,#77470));
#16087=EDGE_LOOP('',(#77471,#77472,#77473,#77474));
#16088=EDGE_LOOP('',(#77475,#77476,#77477,#77478));
#16089=EDGE_LOOP('',(#77479,#77480,#77481,#77482));
#16090=EDGE_LOOP('',(#77483,#77484,#77485,#77486));
#16091=EDGE_LOOP('',(#77487,#77488,#77489,#77490));
#16092=EDGE_LOOP('',(#77491,#77492,#77493,#77494));
#16093=EDGE_LOOP('',(#77495,#77496,#77497));
#16094=EDGE_LOOP('',(#77498,#77499,#77500,#77501,#77502));
#16095=EDGE_LOOP('',(#77503,#77504,#77505,#77506,#77507));
#16096=EDGE_LOOP('',(#77508,#77509,#77510,#77511));
#16097=EDGE_LOOP('',(#77512,#77513,#77514,#77515));
#16098=EDGE_LOOP('',(#77516,#77517,#77518));
#16099=EDGE_LOOP('',(#77519,#77520,#77521,#77522));
#16100=EDGE_LOOP('',(#77523,#77524,#77525,#77526));
#16101=EDGE_LOOP('',(#77527,#77528,#77529,#77530));
#16102=EDGE_LOOP('',(#77531,#77532,#77533,#77534));
#16103=EDGE_LOOP('',(#77535,#77536,#77537,#77538));
#16104=EDGE_LOOP('',(#77539,#77540,#77541,#77542));
#16105=EDGE_LOOP('',(#77543,#77544,#77545,#77546));
#16106=EDGE_LOOP('',(#77547,#77548,#77549,#77550));
#16107=EDGE_LOOP('',(#77551,#77552,#77553,#77554));
#16108=EDGE_LOOP('',(#77555,#77556,#77557,#77558));
#16109=EDGE_LOOP('',(#77559,#77560,#77561,#77562));
#16110=EDGE_LOOP('',(#77563,#77564,#77565));
#16111=EDGE_LOOP('',(#77566,#77567,#77568,#77569,#77570));
#16112=EDGE_LOOP('',(#77571,#77572,#77573,#77574,#77575));
#16113=EDGE_LOOP('',(#77576,#77577,#77578,#77579));
#16114=EDGE_LOOP('',(#77580,#77581,#77582,#77583));
#16115=EDGE_LOOP('',(#77584,#77585,#77586));
#16116=EDGE_LOOP('',(#77587,#77588,#77589,#77590));
#16117=EDGE_LOOP('',(#77591,#77592,#77593,#77594));
#16118=EDGE_LOOP('',(#77595,#77596,#77597,#77598));
#16119=EDGE_LOOP('',(#77599,#77600,#77601,#77602));
#16120=EDGE_LOOP('',(#77603,#77604,#77605,#77606));
#16121=EDGE_LOOP('',(#77607,#77608,#77609,#77610));
#16122=EDGE_LOOP('',(#77611,#77612,#77613,#77614));
#16123=EDGE_LOOP('',(#77615,#77616,#77617,#77618));
#16124=EDGE_LOOP('',(#77619,#77620,#77621,#77622));
#16125=EDGE_LOOP('',(#77623,#77624,#77625,#77626));
#16126=EDGE_LOOP('',(#77627,#77628,#77629,#77630));
#16127=EDGE_LOOP('',(#77631,#77632,#77633));
#16128=EDGE_LOOP('',(#77634,#77635,#77636,#77637,#77638));
#16129=EDGE_LOOP('',(#77639,#77640,#77641,#77642,#77643));
#16130=EDGE_LOOP('',(#77644,#77645,#77646,#77647));
#16131=EDGE_LOOP('',(#77648,#77649,#77650,#77651));
#16132=EDGE_LOOP('',(#77652,#77653,#77654));
#16133=EDGE_LOOP('',(#77655,#77656,#77657,#77658));
#16134=EDGE_LOOP('',(#77659,#77660,#77661,#77662));
#16135=EDGE_LOOP('',(#77663,#77664,#77665,#77666));
#16136=EDGE_LOOP('',(#77667,#77668,#77669,#77670));
#16137=EDGE_LOOP('',(#77671,#77672,#77673,#77674));
#16138=EDGE_LOOP('',(#77675,#77676,#77677,#77678));
#16139=EDGE_LOOP('',(#77679,#77680,#77681,#77682));
#16140=EDGE_LOOP('',(#77683,#77684,#77685,#77686));
#16141=EDGE_LOOP('',(#77687,#77688,#77689,#77690));
#16142=EDGE_LOOP('',(#77691,#77692,#77693,#77694));
#16143=EDGE_LOOP('',(#77695,#77696,#77697,#77698));
#16144=EDGE_LOOP('',(#77699,#77700,#77701));
#16145=EDGE_LOOP('',(#77702,#77703,#77704,#77705,#77706));
#16146=EDGE_LOOP('',(#77707,#77708,#77709,#77710,#77711));
#16147=EDGE_LOOP('',(#77712,#77713,#77714,#77715));
#16148=EDGE_LOOP('',(#77716,#77717,#77718,#77719));
#16149=EDGE_LOOP('',(#77720,#77721,#77722));
#16150=EDGE_LOOP('',(#77723,#77724,#77725,#77726));
#16151=EDGE_LOOP('',(#77727,#77728,#77729,#77730));
#16152=EDGE_LOOP('',(#77731,#77732,#77733,#77734));
#16153=EDGE_LOOP('',(#77735,#77736,#77737,#77738));
#16154=EDGE_LOOP('',(#77739,#77740,#77741,#77742));
#16155=EDGE_LOOP('',(#77743,#77744,#77745,#77746));
#16156=EDGE_LOOP('',(#77747,#77748,#77749,#77750));
#16157=EDGE_LOOP('',(#77751,#77752,#77753,#77754));
#16158=EDGE_LOOP('',(#77755,#77756,#77757,#77758));
#16159=EDGE_LOOP('',(#77759,#77760,#77761,#77762));
#16160=EDGE_LOOP('',(#77763,#77764,#77765,#77766));
#16161=EDGE_LOOP('',(#77767,#77768,#77769));
#16162=EDGE_LOOP('',(#77770,#77771,#77772,#77773,#77774));
#16163=EDGE_LOOP('',(#77775,#77776,#77777,#77778,#77779));
#16164=EDGE_LOOP('',(#77780,#77781,#77782,#77783));
#16165=EDGE_LOOP('',(#77784,#77785,#77786,#77787));
#16166=EDGE_LOOP('',(#77788,#77789,#77790));
#16167=EDGE_LOOP('',(#77791,#77792,#77793,#77794));
#16168=EDGE_LOOP('',(#77795,#77796,#77797,#77798));
#16169=EDGE_LOOP('',(#77799,#77800,#77801,#77802));
#16170=EDGE_LOOP('',(#77803,#77804,#77805,#77806));
#16171=EDGE_LOOP('',(#77807,#77808,#77809,#77810));
#16172=EDGE_LOOP('',(#77811,#77812,#77813,#77814));
#16173=EDGE_LOOP('',(#77815,#77816,#77817,#77818));
#16174=EDGE_LOOP('',(#77819,#77820,#77821,#77822));
#16175=EDGE_LOOP('',(#77823,#77824,#77825,#77826));
#16176=EDGE_LOOP('',(#77827,#77828,#77829,#77830));
#16177=EDGE_LOOP('',(#77831,#77832,#77833,#77834));
#16178=EDGE_LOOP('',(#77835,#77836,#77837));
#16179=EDGE_LOOP('',(#77838,#77839,#77840,#77841,#77842));
#16180=EDGE_LOOP('',(#77843,#77844,#77845,#77846,#77847));
#16181=EDGE_LOOP('',(#77848,#77849,#77850,#77851));
#16182=EDGE_LOOP('',(#77852,#77853,#77854,#77855));
#16183=EDGE_LOOP('',(#77856,#77857,#77858));
#16184=EDGE_LOOP('',(#77859,#77860,#77861,#77862));
#16185=EDGE_LOOP('',(#77863,#77864,#77865,#77866));
#16186=EDGE_LOOP('',(#77867,#77868,#77869,#77870));
#16187=EDGE_LOOP('',(#77871,#77872,#77873,#77874));
#16188=EDGE_LOOP('',(#77875,#77876,#77877,#77878));
#16189=EDGE_LOOP('',(#77879,#77880,#77881,#77882));
#16190=EDGE_LOOP('',(#77883,#77884,#77885,#77886));
#16191=EDGE_LOOP('',(#77887,#77888,#77889,#77890));
#16192=EDGE_LOOP('',(#77891,#77892,#77893,#77894));
#16193=EDGE_LOOP('',(#77895,#77896,#77897,#77898));
#16194=EDGE_LOOP('',(#77899,#77900,#77901,#77902));
#16195=EDGE_LOOP('',(#77903,#77904,#77905));
#16196=EDGE_LOOP('',(#77906,#77907,#77908,#77909,#77910));
#16197=EDGE_LOOP('',(#77911,#77912,#77913,#77914,#77915));
#16198=EDGE_LOOP('',(#77916,#77917,#77918,#77919));
#16199=EDGE_LOOP('',(#77920,#77921,#77922,#77923));
#16200=EDGE_LOOP('',(#77924,#77925,#77926));
#16201=EDGE_LOOP('',(#77927,#77928,#77929,#77930));
#16202=EDGE_LOOP('',(#77931,#77932,#77933,#77934));
#16203=EDGE_LOOP('',(#77935,#77936,#77937,#77938));
#16204=EDGE_LOOP('',(#77939,#77940,#77941,#77942));
#16205=EDGE_LOOP('',(#77943,#77944,#77945,#77946));
#16206=EDGE_LOOP('',(#77947,#77948,#77949,#77950));
#16207=EDGE_LOOP('',(#77951,#77952,#77953,#77954));
#16208=EDGE_LOOP('',(#77955,#77956,#77957,#77958));
#16209=EDGE_LOOP('',(#77959,#77960,#77961,#77962));
#16210=EDGE_LOOP('',(#77963,#77964,#77965,#77966));
#16211=EDGE_LOOP('',(#77967,#77968,#77969,#77970));
#16212=EDGE_LOOP('',(#77971,#77972,#77973));
#16213=EDGE_LOOP('',(#77974,#77975,#77976,#77977,#77978));
#16214=EDGE_LOOP('',(#77979,#77980,#77981,#77982,#77983));
#16215=EDGE_LOOP('',(#77984,#77985,#77986,#77987));
#16216=EDGE_LOOP('',(#77988,#77989,#77990,#77991));
#16217=EDGE_LOOP('',(#77992,#77993,#77994));
#16218=EDGE_LOOP('',(#77995,#77996,#77997,#77998));
#16219=EDGE_LOOP('',(#77999,#78000,#78001,#78002));
#16220=EDGE_LOOP('',(#78003,#78004,#78005,#78006));
#16221=EDGE_LOOP('',(#78007,#78008,#78009,#78010));
#16222=EDGE_LOOP('',(#78011,#78012,#78013,#78014));
#16223=EDGE_LOOP('',(#78015,#78016,#78017,#78018));
#16224=EDGE_LOOP('',(#78019,#78020,#78021,#78022));
#16225=EDGE_LOOP('',(#78023,#78024,#78025,#78026));
#16226=EDGE_LOOP('',(#78027,#78028,#78029,#78030));
#16227=EDGE_LOOP('',(#78031,#78032,#78033,#78034));
#16228=EDGE_LOOP('',(#78035,#78036,#78037,#78038));
#16229=EDGE_LOOP('',(#78039,#78040,#78041));
#16230=EDGE_LOOP('',(#78042,#78043,#78044,#78045,#78046));
#16231=EDGE_LOOP('',(#78047,#78048,#78049,#78050,#78051));
#16232=EDGE_LOOP('',(#78052,#78053,#78054,#78055));
#16233=EDGE_LOOP('',(#78056,#78057,#78058,#78059));
#16234=EDGE_LOOP('',(#78060,#78061,#78062));
#16235=EDGE_LOOP('',(#78063,#78064,#78065,#78066));
#16236=EDGE_LOOP('',(#78067,#78068,#78069,#78070));
#16237=EDGE_LOOP('',(#78071,#78072,#78073,#78074));
#16238=EDGE_LOOP('',(#78075,#78076,#78077,#78078));
#16239=EDGE_LOOP('',(#78079,#78080,#78081,#78082));
#16240=EDGE_LOOP('',(#78083,#78084,#78085,#78086));
#16241=EDGE_LOOP('',(#78087,#78088,#78089,#78090));
#16242=EDGE_LOOP('',(#78091,#78092,#78093,#78094));
#16243=EDGE_LOOP('',(#78095,#78096,#78097,#78098));
#16244=EDGE_LOOP('',(#78099,#78100,#78101,#78102));
#16245=EDGE_LOOP('',(#78103,#78104,#78105,#78106));
#16246=EDGE_LOOP('',(#78107,#78108,#78109));
#16247=EDGE_LOOP('',(#78110,#78111,#78112,#78113,#78114));
#16248=EDGE_LOOP('',(#78115,#78116,#78117,#78118,#78119));
#16249=EDGE_LOOP('',(#78120,#78121,#78122,#78123));
#16250=EDGE_LOOP('',(#78124,#78125,#78126,#78127));
#16251=EDGE_LOOP('',(#78128,#78129,#78130));
#16252=EDGE_LOOP('',(#78131,#78132,#78133,#78134));
#16253=EDGE_LOOP('',(#78135,#78136,#78137,#78138));
#16254=EDGE_LOOP('',(#78139,#78140,#78141,#78142));
#16255=EDGE_LOOP('',(#78143,#78144,#78145,#78146));
#16256=EDGE_LOOP('',(#78147,#78148,#78149,#78150));
#16257=EDGE_LOOP('',(#78151,#78152,#78153,#78154));
#16258=EDGE_LOOP('',(#78155,#78156,#78157,#78158));
#16259=EDGE_LOOP('',(#78159,#78160,#78161,#78162));
#16260=EDGE_LOOP('',(#78163,#78164,#78165,#78166));
#16261=EDGE_LOOP('',(#78167,#78168,#78169,#78170));
#16262=EDGE_LOOP('',(#78171,#78172,#78173,#78174));
#16263=EDGE_LOOP('',(#78175,#78176,#78177));
#16264=EDGE_LOOP('',(#78178,#78179,#78180,#78181,#78182));
#16265=EDGE_LOOP('',(#78183,#78184,#78185,#78186,#78187));
#16266=EDGE_LOOP('',(#78188,#78189,#78190,#78191));
#16267=EDGE_LOOP('',(#78192,#78193,#78194,#78195));
#16268=EDGE_LOOP('',(#78196,#78197,#78198));
#16269=EDGE_LOOP('',(#78199,#78200,#78201,#78202));
#16270=EDGE_LOOP('',(#78203,#78204,#78205,#78206));
#16271=EDGE_LOOP('',(#78207,#78208,#78209,#78210));
#16272=EDGE_LOOP('',(#78211,#78212,#78213,#78214));
#16273=EDGE_LOOP('',(#78215,#78216,#78217,#78218));
#16274=EDGE_LOOP('',(#78219,#78220,#78221,#78222));
#16275=EDGE_LOOP('',(#78223,#78224,#78225,#78226));
#16276=EDGE_LOOP('',(#78227,#78228,#78229,#78230));
#16277=EDGE_LOOP('',(#78231,#78232,#78233,#78234));
#16278=EDGE_LOOP('',(#78235,#78236,#78237,#78238));
#16279=EDGE_LOOP('',(#78239,#78240,#78241,#78242));
#16280=EDGE_LOOP('',(#78243,#78244,#78245));
#16281=EDGE_LOOP('',(#78246,#78247,#78248,#78249,#78250));
#16282=EDGE_LOOP('',(#78251,#78252,#78253,#78254,#78255));
#16283=EDGE_LOOP('',(#78256,#78257,#78258,#78259));
#16284=EDGE_LOOP('',(#78260,#78261,#78262,#78263));
#16285=EDGE_LOOP('',(#78264,#78265,#78266));
#16286=EDGE_LOOP('',(#78267,#78268,#78269,#78270));
#16287=EDGE_LOOP('',(#78271,#78272,#78273,#78274));
#16288=EDGE_LOOP('',(#78275,#78276,#78277,#78278));
#16289=EDGE_LOOP('',(#78279,#78280,#78281,#78282));
#16290=EDGE_LOOP('',(#78283,#78284,#78285,#78286));
#16291=EDGE_LOOP('',(#78287,#78288,#78289,#78290));
#16292=EDGE_LOOP('',(#78291,#78292,#78293,#78294));
#16293=EDGE_LOOP('',(#78295,#78296,#78297,#78298));
#16294=EDGE_LOOP('',(#78299,#78300,#78301,#78302));
#16295=EDGE_LOOP('',(#78303,#78304,#78305,#78306));
#16296=EDGE_LOOP('',(#78307,#78308,#78309,#78310));
#16297=EDGE_LOOP('',(#78311,#78312,#78313));
#16298=EDGE_LOOP('',(#78314,#78315,#78316,#78317,#78318));
#16299=EDGE_LOOP('',(#78319,#78320,#78321,#78322,#78323));
#16300=EDGE_LOOP('',(#78324,#78325,#78326,#78327));
#16301=EDGE_LOOP('',(#78328,#78329,#78330,#78331));
#16302=EDGE_LOOP('',(#78332,#78333,#78334));
#16303=EDGE_LOOP('',(#78335,#78336,#78337,#78338));
#16304=EDGE_LOOP('',(#78339,#78340,#78341,#78342));
#16305=EDGE_LOOP('',(#78343,#78344,#78345,#78346));
#16306=EDGE_LOOP('',(#78347,#78348,#78349,#78350));
#16307=EDGE_LOOP('',(#78351,#78352,#78353,#78354));
#16308=EDGE_LOOP('',(#78355,#78356,#78357,#78358));
#16309=EDGE_LOOP('',(#78359,#78360,#78361,#78362));
#16310=EDGE_LOOP('',(#78363,#78364,#78365,#78366));
#16311=EDGE_LOOP('',(#78367,#78368,#78369,#78370));
#16312=EDGE_LOOP('',(#78371,#78372,#78373,#78374));
#16313=EDGE_LOOP('',(#78375,#78376,#78377,#78378));
#16314=EDGE_LOOP('',(#78379,#78380,#78381));
#16315=EDGE_LOOP('',(#78382,#78383,#78384,#78385,#78386));
#16316=EDGE_LOOP('',(#78387,#78388,#78389,#78390,#78391));
#16317=EDGE_LOOP('',(#78392,#78393,#78394,#78395));
#16318=EDGE_LOOP('',(#78396,#78397,#78398,#78399));
#16319=EDGE_LOOP('',(#78400,#78401,#78402));
#16320=EDGE_LOOP('',(#78403,#78404,#78405,#78406));
#16321=EDGE_LOOP('',(#78407,#78408,#78409,#78410));
#16322=EDGE_LOOP('',(#78411,#78412,#78413,#78414));
#16323=EDGE_LOOP('',(#78415,#78416,#78417,#78418));
#16324=EDGE_LOOP('',(#78419,#78420,#78421,#78422));
#16325=EDGE_LOOP('',(#78423,#78424,#78425,#78426));
#16326=EDGE_LOOP('',(#78427,#78428,#78429,#78430));
#16327=EDGE_LOOP('',(#78431,#78432,#78433,#78434));
#16328=EDGE_LOOP('',(#78435,#78436,#78437,#78438));
#16329=EDGE_LOOP('',(#78439,#78440,#78441,#78442));
#16330=EDGE_LOOP('',(#78443,#78444,#78445,#78446));
#16331=EDGE_LOOP('',(#78447,#78448,#78449));
#16332=EDGE_LOOP('',(#78450,#78451,#78452));
#16333=EDGE_LOOP('',(#78453,#78454,#78455,#78456));
#16334=EDGE_LOOP('',(#78457,#78458,#78459,#78460));
#16335=EDGE_LOOP('',(#78461,#78462,#78463,#78464));
#16336=EDGE_LOOP('',(#78465,#78466,#78467,#78468));
#16337=EDGE_LOOP('',(#78469,#78470,#78471,#78472));
#16338=EDGE_LOOP('',(#78473,#78474,#78475,#78476));
#16339=EDGE_LOOP('',(#78477,#78478,#78479,#78480));
#16340=EDGE_LOOP('',(#78481,#78482,#78483,#78484));
#16341=EDGE_LOOP('',(#78485,#78486,#78487,#78488));
#16342=EDGE_LOOP('',(#78489,#78490,#78491,#78492));
#16343=EDGE_LOOP('',(#78493,#78494,#78495,#78496));
#16344=EDGE_LOOP('',(#78497,#78498,#78499,#78500));
#16345=EDGE_LOOP('',(#78501,#78502,#78503,#78504));
#16346=EDGE_LOOP('',(#78505,#78506,#78507,#78508));
#16347=EDGE_LOOP('',(#78509,#78510,#78511,#78512));
#16348=EDGE_LOOP('',(#78513,#78514,#78515,#78516));
#16349=EDGE_LOOP('',(#78517,#78518,#78519,#78520));
#16350=EDGE_LOOP('',(#78521,#78522,#78523,#78524));
#16351=EDGE_LOOP('',(#78525,#78526,#78527,#78528));
#16352=EDGE_LOOP('',(#78529,#78530,#78531,#78532));
#16353=EDGE_LOOP('',(#78533,#78534,#78535,#78536));
#16354=EDGE_LOOP('',(#78537,#78538,#78539,#78540));
#16355=EDGE_LOOP('',(#78541,#78542,#78543,#78544));
#16356=EDGE_LOOP('',(#78545,#78546,#78547,#78548));
#16357=EDGE_LOOP('',(#78549,#78550,#78551,#78552));
#16358=EDGE_LOOP('',(#78553,#78554,#78555,#78556));
#16359=EDGE_LOOP('',(#78557,#78558,#78559,#78560));
#16360=EDGE_LOOP('',(#78561,#78562,#78563,#78564));
#16361=EDGE_LOOP('',(#78565,#78566,#78567,#78568));
#16362=EDGE_LOOP('',(#78569,#78570,#78571,#78572));
#16363=EDGE_LOOP('',(#78573,#78574,#78575,#78576));
#16364=EDGE_LOOP('',(#78577,#78578,#78579,#78580));
#16365=EDGE_LOOP('',(#78581,#78582,#78583,#78584));
#16366=EDGE_LOOP('',(#78585,#78586,#78587,#78588));
#16367=EDGE_LOOP('',(#78589,#78590,#78591,#78592));
#16368=EDGE_LOOP('',(#78593,#78594,#78595,#78596));
#16369=EDGE_LOOP('',(#78597,#78598,#78599));
#16370=EDGE_LOOP('',(#78600,#78601,#78602,#78603));
#16371=EDGE_LOOP('',(#78604,#78605,#78606,#78607));
#16372=EDGE_LOOP('',(#78608,#78609,#78610,#78611));
#16373=EDGE_LOOP('',(#78612,#78613,#78614,#78615));
#16374=EDGE_LOOP('',(#78616,#78617,#78618,#78619));
#16375=EDGE_LOOP('',(#78620,#78621,#78622,#78623));
#16376=EDGE_LOOP('',(#78624,#78625,#78626,#78627));
#16377=EDGE_LOOP('',(#78628,#78629,#78630,#78631));
#16378=EDGE_LOOP('',(#78632,#78633,#78634,#78635));
#16379=EDGE_LOOP('',(#78636,#78637,#78638,#78639));
#16380=EDGE_LOOP('',(#78640,#78641,#78642,#78643));
#16381=EDGE_LOOP('',(#78644,#78645,#78646,#78647));
#16382=EDGE_LOOP('',(#78648,#78649,#78650,#78651));
#16383=EDGE_LOOP('',(#78652,#78653,#78654,#78655));
#16384=EDGE_LOOP('',(#78656,#78657,#78658,#78659));
#16385=EDGE_LOOP('',(#78660,#78661,#78662,#78663));
#16386=EDGE_LOOP('',(#78664,#78665,#78666,#78667));
#16387=EDGE_LOOP('',(#78668,#78669,#78670,#78671));
#16388=EDGE_LOOP('',(#78672,#78673,#78674,#78675));
#16389=EDGE_LOOP('',(#78676,#78677,#78678,#78679));
#16390=EDGE_LOOP('',(#78680,#78681,#78682,#78683));
#16391=EDGE_LOOP('',(#78684,#78685,#78686,#78687));
#16392=EDGE_LOOP('',(#78688,#78689,#78690,#78691));
#16393=EDGE_LOOP('',(#78692,#78693,#78694,#78695));
#16394=EDGE_LOOP('',(#78696,#78697,#78698,#78699));
#16395=EDGE_LOOP('',(#78700,#78701,#78702,#78703));
#16396=EDGE_LOOP('',(#78704,#78705,#78706,#78707));
#16397=EDGE_LOOP('',(#78708,#78709,#78710,#78711));
#16398=EDGE_LOOP('',(#78712,#78713,#78714,#78715));
#16399=EDGE_LOOP('',(#78716,#78717,#78718,#78719));
#16400=EDGE_LOOP('',(#78720,#78721,#78722,#78723));
#16401=EDGE_LOOP('',(#78724,#78725,#78726,#78727,#78728));
#16402=EDGE_LOOP('',(#78729,#78730,#78731,#78732));
#16403=EDGE_LOOP('',(#78733,#78734,#78735,#78736));
#16404=EDGE_LOOP('',(#78737,#78738,#78739,#78740,#78741,#78742,#78743));
#16405=EDGE_LOOP('',(#78744,#78745,#78746,#78747));
#16406=EDGE_LOOP('',(#78748,#78749,#78750,#78751));
#16407=EDGE_LOOP('',(#78752,#78753,#78754,#78755));
#16408=EDGE_LOOP('',(#78756,#78757,#78758,#78759));
#16409=EDGE_LOOP('',(#78760,#78761,#78762,#78763));
#16410=EDGE_LOOP('',(#78764,#78765,#78766,#78767));
#16411=EDGE_LOOP('',(#78768,#78769,#78770,#78771));
#16412=EDGE_LOOP('',(#78772,#78773,#78774,#78775));
#16413=EDGE_LOOP('',(#78776,#78777,#78778,#78779));
#16414=EDGE_LOOP('',(#78780,#78781,#78782,#78783));
#16415=EDGE_LOOP('',(#78784,#78785,#78786,#78787));
#16416=EDGE_LOOP('',(#78788,#78789,#78790,#78791));
#16417=EDGE_LOOP('',(#78792,#78793,#78794,#78795));
#16418=EDGE_LOOP('',(#78796,#78797,#78798,#78799));
#16419=EDGE_LOOP('',(#78800,#78801,#78802,#78803));
#16420=EDGE_LOOP('',(#78804,#78805,#78806,#78807));
#16421=EDGE_LOOP('',(#78808,#78809,#78810,#78811));
#16422=EDGE_LOOP('',(#78812,#78813,#78814,#78815));
#16423=EDGE_LOOP('',(#78816,#78817,#78818,#78819));
#16424=EDGE_LOOP('',(#78820,#78821,#78822,#78823));
#16425=EDGE_LOOP('',(#78824,#78825,#78826,#78827));
#16426=EDGE_LOOP('',(#78828,#78829,#78830,#78831));
#16427=EDGE_LOOP('',(#78832,#78833,#78834,#78835));
#16428=EDGE_LOOP('',(#78836,#78837,#78838,#78839));
#16429=EDGE_LOOP('',(#78840,#78841,#78842,#78843));
#16430=EDGE_LOOP('',(#78844,#78845,#78846,#78847));
#16431=EDGE_LOOP('',(#78848,#78849,#78850,#78851));
#16432=EDGE_LOOP('',(#78852,#78853,#78854,#78855));
#16433=EDGE_LOOP('',(#78856,#78857,#78858,#78859));
#16434=EDGE_LOOP('',(#78860,#78861,#78862,#78863));
#16435=EDGE_LOOP('',(#78864,#78865,#78866,#78867));
#16436=EDGE_LOOP('',(#78868,#78869,#78870,#78871));
#16437=EDGE_LOOP('',(#78872,#78873,#78874,#78875));
#16438=EDGE_LOOP('',(#78876,#78877,#78878,#78879));
#16439=EDGE_LOOP('',(#78880,#78881,#78882,#78883));
#16440=EDGE_LOOP('',(#78884,#78885,#78886,#78887));
#16441=EDGE_LOOP('',(#78888,#78889,#78890,#78891));
#16442=EDGE_LOOP('',(#78892,#78893,#78894,#78895));
#16443=EDGE_LOOP('',(#78896,#78897,#78898,#78899));
#16444=EDGE_LOOP('',(#78900,#78901,#78902,#78903));
#16445=EDGE_LOOP('',(#78904,#78905,#78906,#78907));
#16446=EDGE_LOOP('',(#78908,#78909,#78910,#78911));
#16447=EDGE_LOOP('',(#78912,#78913,#78914,#78915));
#16448=EDGE_LOOP('',(#78916,#78917,#78918,#78919));
#16449=EDGE_LOOP('',(#78920,#78921,#78922,#78923));
#16450=EDGE_LOOP('',(#78924,#78925,#78926,#78927));
#16451=EDGE_LOOP('',(#78928,#78929,#78930,#78931));
#16452=EDGE_LOOP('',(#78932,#78933,#78934,#78935));
#16453=EDGE_LOOP('',(#78936,#78937,#78938,#78939));
#16454=EDGE_LOOP('',(#78940,#78941,#78942,#78943));
#16455=EDGE_LOOP('',(#78944,#78945,#78946,#78947));
#16456=EDGE_LOOP('',(#78948,#78949,#78950,#78951));
#16457=EDGE_LOOP('',(#78952,#78953,#78954,#78955));
#16458=EDGE_LOOP('',(#78956,#78957,#78958,#78959));
#16459=EDGE_LOOP('',(#78960,#78961,#78962,#78963));
#16460=EDGE_LOOP('',(#78964,#78965,#78966,#78967));
#16461=EDGE_LOOP('',(#78968,#78969,#78970,#78971));
#16462=EDGE_LOOP('',(#78972,#78973,#78974,#78975));
#16463=EDGE_LOOP('',(#78976,#78977,#78978,#78979));
#16464=EDGE_LOOP('',(#78980,#78981,#78982,#78983));
#16465=EDGE_LOOP('',(#78984,#78985,#78986,#78987));
#16466=EDGE_LOOP('',(#78988,#78989,#78990,#78991));
#16467=EDGE_LOOP('',(#78992,#78993,#78994,#78995));
#16468=EDGE_LOOP('',(#78996,#78997,#78998,#78999));
#16469=EDGE_LOOP('',(#79000,#79001,#79002,#79003));
#16470=EDGE_LOOP('',(#79004,#79005,#79006,#79007));
#16471=EDGE_LOOP('',(#79008,#79009,#79010,#79011));
#16472=EDGE_LOOP('',(#79012,#79013,#79014,#79015));
#16473=EDGE_LOOP('',(#79016,#79017,#79018,#79019));
#16474=EDGE_LOOP('',(#79020,#79021,#79022,#79023));
#16475=EDGE_LOOP('',(#79024,#79025,#79026,#79027));
#16476=EDGE_LOOP('',(#79028,#79029,#79030,#79031));
#16477=EDGE_LOOP('',(#79032,#79033,#79034,#79035));
#16478=EDGE_LOOP('',(#79036,#79037,#79038,#79039));
#16479=EDGE_LOOP('',(#79040,#79041,#79042,#79043));
#16480=EDGE_LOOP('',(#79044,#79045,#79046,#79047));
#16481=EDGE_LOOP('',(#79048,#79049,#79050,#79051,#79052));
#16482=EDGE_LOOP('',(#79053,#79054,#79055,#79056));
#16483=EDGE_LOOP('',(#79057,#79058,#79059,#79060,#79061));
#16484=EDGE_LOOP('',(#79062,#79063,#79064,#79065));
#16485=EDGE_LOOP('',(#79066,#79067,#79068));
#16486=EDGE_LOOP('',(#79069,#79070,#79071,#79072,#79073,#79074,#79075,#79076));
#16487=EDGE_LOOP('',(#79077,#79078));
#16488=EDGE_LOOP('',(#79079,#79080,#79081,#79082));
#16489=EDGE_LOOP('',(#79083,#79084,#79085,#79086));
#16490=EDGE_LOOP('',(#79087,#79088,#79089,#79090));
#16491=EDGE_LOOP('',(#79091,#79092,#79093,#79094,#79095,#79096,#79097,#79098,
#79099,#79100,#79101,#79102,#79103,#79104,#79105,#79106,#79107,#79108,#79109,
#79110,#79111,#79112,#79113,#79114,#79115,#79116,#79117,#79118,#79119,#79120,
#79121,#79122,#79123,#79124,#79125,#79126,#79127,#79128,#79129,#79130,#79131,
#79132,#79133,#79134,#79135,#79136,#79137,#79138,#79139,#79140,#79141,#79142,
#79143,#79144,#79145,#79146,#79147,#79148,#79149,#79150,#79151,#79152,#79153,
#79154,#79155,#79156,#79157,#79158,#79159,#79160,#79161,#79162,#79163,#79164,
#79165,#79166,#79167,#79168,#79169,#79170,#79171,#79172,#79173,#79174,#79175,
#79176,#79177,#79178,#79179,#79180,#79181,#79182,#79183,#79184,#79185,#79186,
#79187,#79188,#79189,#79190,#79191,#79192,#79193,#79194,#79195,#79196,#79197,
#79198,#79199,#79200,#79201,#79202,#79203,#79204,#79205,#79206,#79207,#79208,
#79209,#79210,#79211,#79212,#79213,#79214,#79215,#79216,#79217,#79218,#79219,
#79220,#79221,#79222,#79223,#79224,#79225,#79226,#79227,#79228,#79229,#79230,
#79231,#79232,#79233,#79234,#79235,#79236,#79237,#79238,#79239,#79240,#79241,
#79242,#79243,#79244,#79245,#79246,#79247,#79248,#79249,#79250,#79251,#79252,
#79253,#79254,#79255,#79256,#79257,#79258,#79259,#79260,#79261,#79262,#79263,
#79264,#79265,#79266,#79267,#79268,#79269,#79270,#79271,#79272,#79273,#79274,
#79275,#79276,#79277,#79278,#79279,#79280,#79281,#79282,#79283,#79284,#79285,
#79286,#79287,#79288,#79289,#79290,#79291,#79292,#79293,#79294,#79295,#79296,
#79297,#79298,#79299,#79300,#79301,#79302,#79303,#79304,#79305,#79306,#79307,
#79308,#79309,#79310,#79311,#79312,#79313,#79314,#79315,#79316,#79317,#79318,
#79319,#79320,#79321,#79322,#79323,#79324,#79325,#79326,#79327,#79328,#79329,
#79330,#79331,#79332,#79333,#79334,#79335,#79336,#79337,#79338,#79339,#79340,
#79341,#79342,#79343,#79344,#79345,#79346,#79347,#79348,#79349,#79350,#79351,
#79352,#79353,#79354,#79355,#79356,#79357,#79358,#79359,#79360,#79361,#79362,
#79363,#79364,#79365,#79366,#79367,#79368,#79369,#79370,#79371,#79372,#79373,
#79374,#79375,#79376,#79377,#79378,#79379,#79380,#79381,#79382,#79383,#79384,
#79385,#79386,#79387,#79388,#79389,#79390,#79391,#79392,#79393,#79394,#79395,
#79396,#79397,#79398,#79399,#79400,#79401,#79402,#79403,#79404));
#16492=EDGE_LOOP('',(#79405,#79406,#79407,#79408,#79409));
#16493=EDGE_LOOP('',(#79410,#79411,#79412,#79413,#79414,#79415,#79416,#79417,
#79418,#79419,#79420,#79421,#79422,#79423,#79424,#79425,#79426,#79427,#79428,
#79429,#79430,#79431,#79432,#79433,#79434,#79435,#79436,#79437,#79438,#79439,
#79440,#79441,#79442,#79443,#79444,#79445,#79446,#79447,#79448,#79449,#79450,
#79451,#79452,#79453,#79454,#79455,#79456,#79457,#79458,#79459,#79460,#79461,
#79462,#79463,#79464,#79465,#79466,#79467,#79468,#79469,#79470,#79471,#79472,
#79473,#79474,#79475,#79476,#79477,#79478,#79479,#79480,#79481,#79482,#79483,
#79484,#79485,#79486,#79487,#79488,#79489,#79490,#79491,#79492,#79493,#79494,
#79495,#79496,#79497,#79498,#79499,#79500,#79501,#79502,#79503,#79504,#79505,
#79506,#79507,#79508,#79509,#79510,#79511,#79512,#79513,#79514,#79515,#79516,
#79517,#79518,#79519,#79520,#79521,#79522,#79523,#79524,#79525,#79526,#79527,
#79528,#79529,#79530,#79531,#79532,#79533,#79534,#79535,#79536,#79537,#79538,
#79539,#79540,#79541,#79542,#79543,#79544,#79545,#79546,#79547,#79548,#79549,
#79550,#79551,#79552,#79553,#79554,#79555,#79556,#79557,#79558,#79559,#79560,
#79561,#79562,#79563,#79564,#79565,#79566,#79567,#79568,#79569,#79570,#79571,
#79572,#79573,#79574,#79575,#79576,#79577,#79578,#79579,#79580,#79581,#79582,
#79583,#79584,#79585,#79586,#79587,#79588,#79589,#79590,#79591,#79592,#79593,
#79594,#79595,#79596,#79597,#79598,#79599,#79600,#79601,#79602,#79603,#79604,
#79605,#79606,#79607,#79608,#79609,#79610,#79611,#79612,#79613,#79614,#79615,
#79616,#79617,#79618,#79619,#79620,#79621,#79622,#79623,#79624,#79625,#79626,
#79627,#79628,#79629,#79630,#79631,#79632,#79633,#79634,#79635,#79636,#79637,
#79638,#79639,#79640,#79641,#79642,#79643,#79644,#79645,#79646,#79647,#79648,
#79649,#79650,#79651,#79652,#79653,#79654,#79655,#79656,#79657,#79658,#79659,
#79660,#79661,#79662,#79663,#79664,#79665,#79666,#79667,#79668,#79669,#79670,
#79671,#79672,#79673,#79674,#79675,#79676,#79677,#79678,#79679,#79680,#79681,
#79682,#79683,#79684,#79685,#79686,#79687,#79688,#79689,#79690,#79691,#79692,
#79693,#79694,#79695,#79696,#79697,#79698,#79699,#79700,#79701,#79702,#79703,
#79704,#79705,#79706,#79707,#79708,#79709,#79710,#79711,#79712,#79713,#79714,
#79715,#79716,#79717,#79718,#79719,#79720,#79721,#79722,#79723,#79724,#79725,
#79726,#79727,#79728,#79729,#79730,#79731,#79732,#79733,#79734,#79735,#79736,
#79737,#79738,#79739,#79740,#79741,#79742,#79743,#79744,#79745,#79746,#79747,
#79748,#79749,#79750,#79751,#79752,#79753,#79754,#79755,#79756,#79757,#79758,
#79759,#79760,#79761,#79762,#79763,#79764,#79765,#79766,#79767,#79768,#79769,
#79770,#79771,#79772,#79773,#79774,#79775,#79776,#79777,#79778,#79779,#79780,
#79781,#79782,#79783,#79784,#79785,#79786,#79787,#79788,#79789,#79790,#79791,
#79792,#79793,#79794,#79795,#79796,#79797,#79798,#79799,#79800,#79801,#79802,
#79803,#79804,#79805,#79806,#79807,#79808,#79809,#79810,#79811,#79812,#79813,
#79814,#79815,#79816,#79817,#79818,#79819,#79820,#79821,#79822,#79823,#79824,
#79825,#79826,#79827,#79828,#79829,#79830,#79831,#79832,#79833,#79834,#79835,
#79836,#79837,#79838,#79839,#79840,#79841,#79842,#79843,#79844,#79845,#79846,
#79847,#79848,#79849,#79850,#79851,#79852,#79853,#79854,#79855,#79856,#79857,
#79858,#79859,#79860,#79861,#79862,#79863,#79864,#79865,#79866,#79867,#79868,
#79869,#79870,#79871,#79872,#79873,#79874,#79875));
#16494=EDGE_LOOP('',(#79876,#79877,#79878,#79879,#79880));
#16495=EDGE_LOOP('',(#79881,#79882,#79883,#79884));
#16496=EDGE_LOOP('',(#79885,#79886,#79887,#79888));
#16497=EDGE_LOOP('',(#79889,#79890,#79891,#79892));
#16498=EDGE_LOOP('',(#79893,#79894,#79895,#79896));
#16499=EDGE_LOOP('',(#79897,#79898,#79899,#79900));
#16500=EDGE_LOOP('',(#79901,#79902,#79903,#79904));
#16501=EDGE_LOOP('',(#79905,#79906,#79907,#79908));
#16502=EDGE_LOOP('',(#79909,#79910,#79911,#79912));
#16503=EDGE_LOOP('',(#79913,#79914,#79915,#79916));
#16504=EDGE_LOOP('',(#79917,#79918,#79919,#79920));
#16505=EDGE_LOOP('',(#79921,#79922,#79923,#79924));
#16506=EDGE_LOOP('',(#79925,#79926,#79927,#79928));
#16507=EDGE_LOOP('',(#79929,#79930,#79931,#79932));
#16508=EDGE_LOOP('',(#79933,#79934,#79935,#79936));
#16509=EDGE_LOOP('',(#79937,#79938,#79939,#79940));
#16510=EDGE_LOOP('',(#79941,#79942,#79943,#79944));
#16511=EDGE_LOOP('',(#79945,#79946,#79947,#79948));
#16512=EDGE_LOOP('',(#79949,#79950,#79951,#79952));
#16513=EDGE_LOOP('',(#79953,#79954,#79955,#79956));
#16514=EDGE_LOOP('',(#79957,#79958,#79959,#79960));
#16515=EDGE_LOOP('',(#79961,#79962,#79963,#79964));
#16516=EDGE_LOOP('',(#79965,#79966,#79967,#79968));
#16517=EDGE_LOOP('',(#79969,#79970,#79971,#79972));
#16518=EDGE_LOOP('',(#79973,#79974,#79975,#79976));
#16519=EDGE_LOOP('',(#79977,#79978,#79979,#79980));
#16520=EDGE_LOOP('',(#79981,#79982,#79983,#79984));
#16521=EDGE_LOOP('',(#79985,#79986,#79987,#79988));
#16522=EDGE_LOOP('',(#79989,#79990,#79991,#79992));
#16523=EDGE_LOOP('',(#79993,#79994,#79995,#79996));
#16524=EDGE_LOOP('',(#79997,#79998,#79999,#80000));
#16525=EDGE_LOOP('',(#80001,#80002,#80003,#80004));
#16526=EDGE_LOOP('',(#80005,#80006,#80007,#80008));
#16527=EDGE_LOOP('',(#80009,#80010,#80011,#80012));
#16528=EDGE_LOOP('',(#80013,#80014,#80015,#80016));
#16529=EDGE_LOOP('',(#80017,#80018,#80019,#80020));
#16530=EDGE_LOOP('',(#80021,#80022,#80023,#80024));
#16531=EDGE_LOOP('',(#80025,#80026,#80027,#80028));
#16532=EDGE_LOOP('',(#80029,#80030,#80031,#80032));
#16533=EDGE_LOOP('',(#80033,#80034,#80035,#80036));
#16534=EDGE_LOOP('',(#80037,#80038,#80039,#80040));
#16535=EDGE_LOOP('',(#80041,#80042,#80043,#80044));
#16536=EDGE_LOOP('',(#80045,#80046,#80047,#80048));
#16537=EDGE_LOOP('',(#80049,#80050,#80051,#80052));
#16538=EDGE_LOOP('',(#80053,#80054,#80055,#80056));
#16539=EDGE_LOOP('',(#80057,#80058,#80059,#80060));
#16540=EDGE_LOOP('',(#80061,#80062,#80063,#80064));
#16541=EDGE_LOOP('',(#80065,#80066,#80067,#80068));
#16542=EDGE_LOOP('',(#80069,#80070,#80071,#80072));
#16543=EDGE_LOOP('',(#80073,#80074,#80075,#80076));
#16544=EDGE_LOOP('',(#80077,#80078,#80079,#80080));
#16545=EDGE_LOOP('',(#80081,#80082,#80083,#80084));
#16546=EDGE_LOOP('',(#80085,#80086,#80087,#80088));
#16547=EDGE_LOOP('',(#80089,#80090,#80091,#80092));
#16548=EDGE_LOOP('',(#80093,#80094,#80095,#80096));
#16549=EDGE_LOOP('',(#80097,#80098,#80099,#80100));
#16550=EDGE_LOOP('',(#80101,#80102,#80103,#80104));
#16551=EDGE_LOOP('',(#80105,#80106,#80107,#80108));
#16552=EDGE_LOOP('',(#80109,#80110,#80111,#80112));
#16553=EDGE_LOOP('',(#80113,#80114,#80115,#80116));
#16554=EDGE_LOOP('',(#80117,#80118,#80119,#80120));
#16555=EDGE_LOOP('',(#80121,#80122,#80123,#80124));
#16556=EDGE_LOOP('',(#80125,#80126,#80127,#80128));
#16557=EDGE_LOOP('',(#80129,#80130,#80131,#80132));
#16558=EDGE_LOOP('',(#80133,#80134,#80135,#80136));
#16559=EDGE_LOOP('',(#80137,#80138,#80139,#80140));
#16560=EDGE_LOOP('',(#80141,#80142,#80143,#80144));
#16561=EDGE_LOOP('',(#80145,#80146,#80147,#80148));
#16562=EDGE_LOOP('',(#80149,#80150,#80151,#80152));
#16563=EDGE_LOOP('',(#80153,#80154,#80155,#80156));
#16564=EDGE_LOOP('',(#80157,#80158,#80159,#80160));
#16565=EDGE_LOOP('',(#80161,#80162,#80163,#80164));
#16566=EDGE_LOOP('',(#80165,#80166,#80167,#80168));
#16567=EDGE_LOOP('',(#80169,#80170,#80171,#80172));
#16568=EDGE_LOOP('',(#80173,#80174,#80175,#80176));
#16569=EDGE_LOOP('',(#80177,#80178,#80179,#80180));
#16570=EDGE_LOOP('',(#80181,#80182,#80183,#80184,#80185,#80186));
#16571=EDGE_LOOP('',(#80187,#80188,#80189,#80190,#80191));
#16572=EDGE_LOOP('',(#80192,#80193,#80194,#80195,#80196));
#16573=EDGE_LOOP('',(#80197));
#16574=EDGE_LOOP('',(#80198));
#16575=EDGE_LOOP('',(#80199,#80200,#80201));
#16576=EDGE_LOOP('',(#80202,#80203,#80204));
#16577=EDGE_LOOP('',(#80205,#80206,#80207));
#16578=EDGE_LOOP('',(#80208,#80209,#80210));
#16579=EDGE_LOOP('',(#80211,#80212,#80213));
#16580=EDGE_LOOP('',(#80214));
#16581=EDGE_LOOP('',(#80215,#80216,#80217,#80218,#80219,#80220));
#16582=EDGE_LOOP('',(#80221,#80222,#80223,#80224));
#16583=EDGE_LOOP('',(#80225,#80226,#80227,#80228,#80229));
#16584=EDGE_LOOP('',(#80230,#80231,#80232,#80233,#80234));
#16585=EDGE_LOOP('',(#80235,#80236,#80237,#80238,#80239));
#16586=EDGE_LOOP('',(#80240,#80241,#80242,#80243,#80244));
#16587=EDGE_LOOP('',(#80245,#80246,#80247,#80248,#80249));
#16588=EDGE_LOOP('',(#80250,#80251,#80252,#80253,#80254));
#16589=EDGE_LOOP('',(#80255,#80256,#80257));
#16590=EDGE_LOOP('',(#80258,#80259));
#16591=EDGE_LOOP('',(#80260,#80261));
#16592=EDGE_LOOP('',(#80262,#80263));
#16593=EDGE_LOOP('',(#80264,#80265));
#16594=EDGE_LOOP('',(#80266,#80267));
#16595=EDGE_LOOP('',(#80268,#80269,#80270));
#16596=EDGE_LOOP('',(#80271,#80272,#80273,#80274,#80275,#80276,#80277,#80278,
#80279,#80280,#80281,#80282,#80283,#80284,#80285,#80286,#80287,#80288,#80289,
#80290,#80291,#80292,#80293,#80294,#80295,#80296,#80297,#80298,#80299,#80300,
#80301,#80302,#80303,#80304,#80305,#80306,#80307,#80308,#80309,#80310,#80311,
#80312,#80313,#80314,#80315,#80316,#80317,#80318,#80319,#80320,#80321,#80322,
#80323,#80324,#80325,#80326,#80327,#80328,#80329,#80330,#80331,#80332,#80333,
#80334,#80335,#80336,#80337,#80338,#80339,#80340,#80341,#80342,#80343,#80344,
#80345,#80346));
#16597=EDGE_LOOP('',(#80347,#80348,#80349,#80350));
#16598=EDGE_LOOP('',(#80351,#80352,#80353,#80354,#80355,#80356,#80357,#80358,
#80359,#80360,#80361,#80362,#80363,#80364,#80365,#80366,#80367,#80368,#80369,
#80370,#80371,#80372,#80373,#80374,#80375,#80376,#80377,#80378,#80379,#80380,
#80381,#80382,#80383,#80384,#80385,#80386,#80387,#80388,#80389,#80390,#80391,
#80392,#80393,#80394,#80395,#80396,#80397,#80398,#80399,#80400,#80401,#80402,
#80403,#80404,#80405,#80406,#80407,#80408,#80409,#80410,#80411,#80412,#80413,
#80414,#80415,#80416,#80417,#80418,#80419,#80420,#80421,#80422,#80423,#80424,
#80425,#80426));
#16599=EDGE_LOOP('',(#80427,#80428,#80429,#80430));
#16600=EDGE_LOOP('',(#80431,#80432,#80433,#80434));
#16601=EDGE_LOOP('',(#80435,#80436,#80437,#80438));
#16602=EDGE_LOOP('',(#80439,#80440,#80441,#80442,#80443));
#16603=EDGE_LOOP('',(#80444,#80445,#80446,#80447));
#16604=EDGE_LOOP('',(#80448,#80449,#80450,#80451));
#16605=EDGE_LOOP('',(#80452,#80453,#80454,#80455));
#16606=EDGE_LOOP('',(#80456,#80457,#80458,#80459));
#16607=EDGE_LOOP('',(#80460,#80461,#80462,#80463));
#16608=EDGE_LOOP('',(#80464,#80465,#80466,#80467,#80468,#80469));
#16609=EDGE_LOOP('',(#80470,#80471,#80472,#80473));
#16610=EDGE_LOOP('',(#80474,#80475,#80476,#80477));
#16611=EDGE_LOOP('',(#80478,#80479,#80480,#80481));
#16612=EDGE_LOOP('',(#80482,#80483,#80484,#80485,#80486));
#16613=EDGE_LOOP('',(#80487,#80488,#80489,#80490,#80491));
#16614=EDGE_LOOP('',(#80492,#80493,#80494,#80495,#80496,#80497));
#16615=EDGE_LOOP('',(#80498,#80499,#80500,#80501));
#16616=EDGE_LOOP('',(#80502,#80503,#80504,#80505,#80506));
#16617=EDGE_LOOP('',(#80507,#80508,#80509,#80510));
#16618=EDGE_LOOP('',(#80511,#80512,#80513,#80514));
#16619=EDGE_LOOP('',(#80515,#80516,#80517,#80518));
#16620=EDGE_LOOP('',(#80519,#80520,#80521,#80522));
#16621=EDGE_LOOP('',(#80523,#80524,#80525,#80526));
#16622=EDGE_LOOP('',(#80527,#80528,#80529,#80530,#80531));
#16623=EDGE_LOOP('',(#80532,#80533,#80534,#80535));
#16624=EDGE_LOOP('',(#80536,#80537,#80538,#80539));
#16625=EDGE_LOOP('',(#80540,#80541,#80542,#80543));
#16626=EDGE_LOOP('',(#80544,#80545,#80546,#80547));
#16627=EDGE_LOOP('',(#80548,#80549,#80550,#80551));
#16628=EDGE_LOOP('',(#80552,#80553,#80554,#80555,#80556));
#16629=EDGE_LOOP('',(#80557,#80558,#80559,#80560,#80561));
#16630=EDGE_LOOP('',(#80562,#80563,#80564,#80565,#80566,#80567));
#16631=EDGE_LOOP('',(#80568,#80569,#80570,#80571));
#16632=EDGE_LOOP('',(#80572,#80573,#80574,#80575,#80576));
#16633=EDGE_LOOP('',(#80577,#80578,#80579,#80580));
#16634=EDGE_LOOP('',(#80581,#80582,#80583,#80584));
#16635=EDGE_LOOP('',(#80585,#80586,#80587,#80588));
#16636=EDGE_LOOP('',(#80589,#80590,#80591,#80592));
#16637=EDGE_LOOP('',(#80593,#80594,#80595,#80596));
#16638=EDGE_LOOP('',(#80597,#80598,#80599,#80600,#80601));
#16639=EDGE_LOOP('',(#80602,#80603,#80604,#80605));
#16640=EDGE_LOOP('',(#80606,#80607,#80608,#80609));
#16641=EDGE_LOOP('',(#80610,#80611,#80612,#80613));
#16642=EDGE_LOOP('',(#80614,#80615,#80616,#80617));
#16643=EDGE_LOOP('',(#80618,#80619,#80620,#80621));
#16644=EDGE_LOOP('',(#80622,#80623,#80624,#80625,#80626));
#16645=EDGE_LOOP('',(#80627,#80628,#80629,#80630,#80631));
#16646=EDGE_LOOP('',(#80632,#80633,#80634,#80635,#80636,#80637));
#16647=EDGE_LOOP('',(#80638,#80639,#80640,#80641));
#16648=EDGE_LOOP('',(#80642,#80643,#80644,#80645,#80646));
#16649=EDGE_LOOP('',(#80647,#80648,#80649,#80650));
#16650=EDGE_LOOP('',(#80651,#80652,#80653,#80654));
#16651=EDGE_LOOP('',(#80655,#80656,#80657,#80658));
#16652=EDGE_LOOP('',(#80659,#80660,#80661,#80662));
#16653=EDGE_LOOP('',(#80663,#80664,#80665,#80666));
#16654=EDGE_LOOP('',(#80667,#80668,#80669,#80670,#80671));
#16655=EDGE_LOOP('',(#80672,#80673,#80674,#80675));
#16656=EDGE_LOOP('',(#80676,#80677,#80678,#80679));
#16657=EDGE_LOOP('',(#80680,#80681,#80682,#80683));
#16658=EDGE_LOOP('',(#80684,#80685,#80686,#80687));
#16659=EDGE_LOOP('',(#80688,#80689,#80690,#80691));
#16660=EDGE_LOOP('',(#80692,#80693,#80694,#80695,#80696));
#16661=EDGE_LOOP('',(#80697,#80698,#80699,#80700,#80701));
#16662=EDGE_LOOP('',(#80702,#80703,#80704,#80705,#80706,#80707));
#16663=EDGE_LOOP('',(#80708,#80709,#80710,#80711));
#16664=EDGE_LOOP('',(#80712,#80713,#80714,#80715,#80716));
#16665=EDGE_LOOP('',(#80717,#80718,#80719,#80720));
#16666=EDGE_LOOP('',(#80721,#80722,#80723,#80724));
#16667=EDGE_LOOP('',(#80725,#80726,#80727,#80728));
#16668=EDGE_LOOP('',(#80729,#80730,#80731,#80732));
#16669=EDGE_LOOP('',(#80733,#80734,#80735,#80736));
#16670=EDGE_LOOP('',(#80737,#80738,#80739,#80740,#80741));
#16671=EDGE_LOOP('',(#80742,#80743,#80744,#80745));
#16672=EDGE_LOOP('',(#80746,#80747,#80748,#80749));
#16673=EDGE_LOOP('',(#80750,#80751,#80752,#80753));
#16674=EDGE_LOOP('',(#80754,#80755,#80756,#80757));
#16675=EDGE_LOOP('',(#80758,#80759,#80760,#80761));
#16676=EDGE_LOOP('',(#80762,#80763,#80764,#80765,#80766));
#16677=EDGE_LOOP('',(#80767,#80768,#80769,#80770,#80771));
#16678=EDGE_LOOP('',(#80772,#80773,#80774,#80775,#80776,#80777));
#16679=EDGE_LOOP('',(#80778,#80779,#80780,#80781));
#16680=EDGE_LOOP('',(#80782,#80783,#80784,#80785,#80786));
#16681=EDGE_LOOP('',(#80787,#80788,#80789,#80790));
#16682=EDGE_LOOP('',(#80791,#80792,#80793,#80794));
#16683=EDGE_LOOP('',(#80795,#80796,#80797,#80798));
#16684=EDGE_LOOP('',(#80799,#80800,#80801,#80802));
#16685=EDGE_LOOP('',(#80803,#80804,#80805,#80806));
#16686=EDGE_LOOP('',(#80807,#80808,#80809,#80810,#80811));
#16687=EDGE_LOOP('',(#80812,#80813,#80814,#80815));
#16688=EDGE_LOOP('',(#80816,#80817,#80818,#80819));
#16689=EDGE_LOOP('',(#80820,#80821,#80822,#80823));
#16690=EDGE_LOOP('',(#80824,#80825,#80826,#80827));
#16691=EDGE_LOOP('',(#80828,#80829,#80830,#80831));
#16692=EDGE_LOOP('',(#80832,#80833,#80834,#80835,#80836));
#16693=EDGE_LOOP('',(#80837,#80838,#80839,#80840,#80841));
#16694=EDGE_LOOP('',(#80842,#80843,#80844,#80845,#80846,#80847));
#16695=EDGE_LOOP('',(#80848,#80849,#80850,#80851));
#16696=EDGE_LOOP('',(#80852,#80853,#80854,#80855,#80856));
#16697=EDGE_LOOP('',(#80857,#80858,#80859,#80860));
#16698=EDGE_LOOP('',(#80861,#80862,#80863,#80864));
#16699=EDGE_LOOP('',(#80865,#80866,#80867,#80868));
#16700=EDGE_LOOP('',(#80869,#80870,#80871,#80872));
#16701=EDGE_LOOP('',(#80873,#80874,#80875,#80876));
#16702=EDGE_LOOP('',(#80877,#80878,#80879,#80880,#80881));
#16703=EDGE_LOOP('',(#80882,#80883,#80884,#80885));
#16704=EDGE_LOOP('',(#80886,#80887,#80888,#80889));
#16705=EDGE_LOOP('',(#80890,#80891,#80892,#80893));
#16706=EDGE_LOOP('',(#80894,#80895,#80896,#80897));
#16707=EDGE_LOOP('',(#80898,#80899,#80900,#80901));
#16708=EDGE_LOOP('',(#80902,#80903,#80904,#80905,#80906));
#16709=EDGE_LOOP('',(#80907,#80908,#80909,#80910,#80911));
#16710=EDGE_LOOP('',(#80912,#80913,#80914,#80915,#80916,#80917));
#16711=EDGE_LOOP('',(#80918,#80919,#80920,#80921));
#16712=EDGE_LOOP('',(#80922,#80923,#80924,#80925,#80926));
#16713=EDGE_LOOP('',(#80927,#80928,#80929,#80930));
#16714=EDGE_LOOP('',(#80931,#80932,#80933,#80934));
#16715=EDGE_LOOP('',(#80935,#80936,#80937,#80938));
#16716=EDGE_LOOP('',(#80939,#80940,#80941,#80942));
#16717=EDGE_LOOP('',(#80943,#80944,#80945,#80946));
#16718=EDGE_LOOP('',(#80947,#80948,#80949,#80950,#80951));
#16719=EDGE_LOOP('',(#80952,#80953,#80954,#80955));
#16720=EDGE_LOOP('',(#80956,#80957,#80958,#80959));
#16721=EDGE_LOOP('',(#80960,#80961,#80962,#80963));
#16722=EDGE_LOOP('',(#80964,#80965,#80966,#80967));
#16723=EDGE_LOOP('',(#80968,#80969,#80970,#80971));
#16724=EDGE_LOOP('',(#80972,#80973,#80974,#80975,#80976));
#16725=EDGE_LOOP('',(#80977,#80978,#80979,#80980,#80981));
#16726=EDGE_LOOP('',(#80982,#80983,#80984,#80985,#80986,#80987));
#16727=EDGE_LOOP('',(#80988,#80989,#80990,#80991));
#16728=EDGE_LOOP('',(#80992,#80993,#80994,#80995,#80996));
#16729=EDGE_LOOP('',(#80997,#80998,#80999,#81000));
#16730=EDGE_LOOP('',(#81001,#81002,#81003,#81004));
#16731=EDGE_LOOP('',(#81005,#81006,#81007,#81008));
#16732=EDGE_LOOP('',(#81009,#81010,#81011,#81012));
#16733=EDGE_LOOP('',(#81013,#81014,#81015,#81016));
#16734=EDGE_LOOP('',(#81017,#81018,#81019,#81020,#81021));
#16735=EDGE_LOOP('',(#81022,#81023,#81024,#81025));
#16736=EDGE_LOOP('',(#81026,#81027,#81028,#81029));
#16737=EDGE_LOOP('',(#81030,#81031,#81032,#81033));
#16738=EDGE_LOOP('',(#81034,#81035,#81036,#81037));
#16739=EDGE_LOOP('',(#81038,#81039,#81040,#81041));
#16740=EDGE_LOOP('',(#81042,#81043,#81044,#81045,#81046));
#16741=EDGE_LOOP('',(#81047,#81048,#81049,#81050,#81051));
#16742=EDGE_LOOP('',(#81052,#81053,#81054,#81055,#81056,#81057));
#16743=EDGE_LOOP('',(#81058,#81059,#81060,#81061));
#16744=EDGE_LOOP('',(#81062,#81063,#81064,#81065,#81066));
#16745=EDGE_LOOP('',(#81067,#81068,#81069,#81070));
#16746=EDGE_LOOP('',(#81071,#81072,#81073,#81074));
#16747=EDGE_LOOP('',(#81075,#81076,#81077,#81078));
#16748=EDGE_LOOP('',(#81079,#81080,#81081,#81082));
#16749=EDGE_LOOP('',(#81083,#81084,#81085,#81086));
#16750=EDGE_LOOP('',(#81087,#81088,#81089,#81090,#81091));
#16751=EDGE_LOOP('',(#81092,#81093,#81094,#81095));
#16752=EDGE_LOOP('',(#81096,#81097,#81098,#81099));
#16753=EDGE_LOOP('',(#81100,#81101,#81102,#81103));
#16754=EDGE_LOOP('',(#81104,#81105,#81106,#81107));
#16755=EDGE_LOOP('',(#81108,#81109,#81110,#81111));
#16756=EDGE_LOOP('',(#81112,#81113,#81114,#81115,#81116));
#16757=EDGE_LOOP('',(#81117,#81118,#81119,#81120,#81121));
#16758=EDGE_LOOP('',(#81122,#81123,#81124,#81125,#81126,#81127));
#16759=EDGE_LOOP('',(#81128,#81129,#81130,#81131));
#16760=EDGE_LOOP('',(#81132,#81133,#81134,#81135,#81136));
#16761=EDGE_LOOP('',(#81137,#81138,#81139,#81140));
#16762=EDGE_LOOP('',(#81141,#81142,#81143,#81144));
#16763=EDGE_LOOP('',(#81145,#81146,#81147,#81148));
#16764=EDGE_LOOP('',(#81149,#81150,#81151,#81152));
#16765=EDGE_LOOP('',(#81153,#81154,#81155,#81156));
#16766=EDGE_LOOP('',(#81157,#81158,#81159,#81160,#81161));
#16767=EDGE_LOOP('',(#81162,#81163,#81164,#81165));
#16768=EDGE_LOOP('',(#81166,#81167,#81168,#81169));
#16769=EDGE_LOOP('',(#81170,#81171,#81172,#81173));
#16770=EDGE_LOOP('',(#81174,#81175,#81176,#81177));
#16771=EDGE_LOOP('',(#81178,#81179,#81180,#81181));
#16772=EDGE_LOOP('',(#81182,#81183,#81184,#81185,#81186));
#16773=EDGE_LOOP('',(#81187,#81188,#81189,#81190,#81191));
#16774=EDGE_LOOP('',(#81192,#81193,#81194,#81195,#81196,#81197));
#16775=EDGE_LOOP('',(#81198,#81199,#81200,#81201));
#16776=EDGE_LOOP('',(#81202,#81203,#81204,#81205,#81206));
#16777=EDGE_LOOP('',(#81207,#81208,#81209,#81210));
#16778=EDGE_LOOP('',(#81211,#81212,#81213,#81214));
#16779=EDGE_LOOP('',(#81215,#81216,#81217,#81218));
#16780=EDGE_LOOP('',(#81219,#81220,#81221,#81222));
#16781=EDGE_LOOP('',(#81223,#81224,#81225,#81226));
#16782=EDGE_LOOP('',(#81227,#81228,#81229,#81230,#81231));
#16783=EDGE_LOOP('',(#81232,#81233,#81234,#81235));
#16784=EDGE_LOOP('',(#81236,#81237,#81238,#81239));
#16785=EDGE_LOOP('',(#81240,#81241,#81242,#81243));
#16786=EDGE_LOOP('',(#81244,#81245,#81246,#81247));
#16787=EDGE_LOOP('',(#81248,#81249,#81250,#81251));
#16788=EDGE_LOOP('',(#81252,#81253,#81254,#81255,#81256));
#16789=EDGE_LOOP('',(#81257,#81258,#81259,#81260,#81261));
#16790=EDGE_LOOP('',(#81262,#81263,#81264,#81265,#81266,#81267));
#16791=EDGE_LOOP('',(#81268,#81269,#81270,#81271));
#16792=EDGE_LOOP('',(#81272,#81273,#81274,#81275,#81276));
#16793=EDGE_LOOP('',(#81277,#81278,#81279,#81280));
#16794=EDGE_LOOP('',(#81281,#81282,#81283,#81284));
#16795=EDGE_LOOP('',(#81285,#81286,#81287,#81288));
#16796=EDGE_LOOP('',(#81289,#81290,#81291,#81292));
#16797=EDGE_LOOP('',(#81293,#81294,#81295,#81296));
#16798=EDGE_LOOP('',(#81297,#81298,#81299,#81300,#81301));
#16799=EDGE_LOOP('',(#81302,#81303,#81304,#81305));
#16800=EDGE_LOOP('',(#81306,#81307,#81308,#81309));
#16801=EDGE_LOOP('',(#81310,#81311,#81312,#81313));
#16802=EDGE_LOOP('',(#81314,#81315,#81316,#81317));
#16803=EDGE_LOOP('',(#81318,#81319,#81320,#81321));
#16804=EDGE_LOOP('',(#81322,#81323,#81324,#81325,#81326));
#16805=EDGE_LOOP('',(#81327,#81328,#81329,#81330,#81331));
#16806=EDGE_LOOP('',(#81332,#81333,#81334,#81335,#81336,#81337));
#16807=EDGE_LOOP('',(#81338,#81339,#81340,#81341));
#16808=EDGE_LOOP('',(#81342,#81343,#81344,#81345,#81346));
#16809=EDGE_LOOP('',(#81347,#81348,#81349,#81350));
#16810=EDGE_LOOP('',(#81351,#81352,#81353,#81354));
#16811=EDGE_LOOP('',(#81355,#81356,#81357,#81358));
#16812=EDGE_LOOP('',(#81359,#81360,#81361,#81362));
#16813=EDGE_LOOP('',(#81363,#81364,#81365,#81366));
#16814=EDGE_LOOP('',(#81367,#81368,#81369,#81370,#81371));
#16815=EDGE_LOOP('',(#81372,#81373,#81374,#81375));
#16816=EDGE_LOOP('',(#81376,#81377,#81378,#81379));
#16817=EDGE_LOOP('',(#81380,#81381,#81382,#81383));
#16818=EDGE_LOOP('',(#81384,#81385,#81386,#81387));
#16819=EDGE_LOOP('',(#81388,#81389,#81390,#81391));
#16820=EDGE_LOOP('',(#81392,#81393,#81394,#81395,#81396));
#16821=EDGE_LOOP('',(#81397,#81398,#81399,#81400,#81401));
#16822=EDGE_LOOP('',(#81402,#81403,#81404,#81405,#81406,#81407));
#16823=EDGE_LOOP('',(#81408,#81409,#81410,#81411));
#16824=EDGE_LOOP('',(#81412,#81413,#81414,#81415,#81416));
#16825=EDGE_LOOP('',(#81417,#81418,#81419,#81420));
#16826=EDGE_LOOP('',(#81421,#81422,#81423,#81424));
#16827=EDGE_LOOP('',(#81425,#81426,#81427,#81428));
#16828=EDGE_LOOP('',(#81429,#81430,#81431,#81432));
#16829=EDGE_LOOP('',(#81433,#81434,#81435,#81436));
#16830=EDGE_LOOP('',(#81437,#81438,#81439,#81440,#81441));
#16831=EDGE_LOOP('',(#81442,#81443,#81444,#81445));
#16832=EDGE_LOOP('',(#81446,#81447,#81448,#81449));
#16833=EDGE_LOOP('',(#81450,#81451,#81452,#81453));
#16834=EDGE_LOOP('',(#81454,#81455,#81456,#81457));
#16835=EDGE_LOOP('',(#81458,#81459,#81460,#81461));
#16836=EDGE_LOOP('',(#81462,#81463,#81464,#81465,#81466));
#16837=EDGE_LOOP('',(#81467,#81468,#81469,#81470,#81471));
#16838=EDGE_LOOP('',(#81472,#81473,#81474,#81475,#81476,#81477));
#16839=EDGE_LOOP('',(#81478,#81479,#81480,#81481));
#16840=EDGE_LOOP('',(#81482,#81483,#81484,#81485,#81486));
#16841=EDGE_LOOP('',(#81487,#81488,#81489,#81490));
#16842=EDGE_LOOP('',(#81491,#81492,#81493,#81494));
#16843=EDGE_LOOP('',(#81495,#81496,#81497,#81498));
#16844=EDGE_LOOP('',(#81499,#81500,#81501,#81502));
#16845=EDGE_LOOP('',(#81503,#81504,#81505,#81506));
#16846=EDGE_LOOP('',(#81507,#81508,#81509,#81510,#81511));
#16847=EDGE_LOOP('',(#81512,#81513,#81514,#81515));
#16848=EDGE_LOOP('',(#81516,#81517,#81518,#81519));
#16849=EDGE_LOOP('',(#81520,#81521,#81522,#81523));
#16850=EDGE_LOOP('',(#81524,#81525,#81526,#81527));
#16851=EDGE_LOOP('',(#81528,#81529,#81530,#81531));
#16852=EDGE_LOOP('',(#81532,#81533,#81534,#81535,#81536));
#16853=EDGE_LOOP('',(#81537,#81538,#81539,#81540,#81541));
#16854=EDGE_LOOP('',(#81542,#81543,#81544,#81545,#81546,#81547));
#16855=EDGE_LOOP('',(#81548,#81549,#81550,#81551));
#16856=EDGE_LOOP('',(#81552,#81553,#81554,#81555,#81556));
#16857=EDGE_LOOP('',(#81557,#81558,#81559,#81560));
#16858=EDGE_LOOP('',(#81561,#81562,#81563,#81564));
#16859=EDGE_LOOP('',(#81565,#81566,#81567,#81568));
#16860=EDGE_LOOP('',(#81569,#81570,#81571,#81572));
#16861=EDGE_LOOP('',(#81573,#81574,#81575,#81576));
#16862=EDGE_LOOP('',(#81577,#81578,#81579,#81580,#81581));
#16863=EDGE_LOOP('',(#81582,#81583,#81584,#81585));
#16864=EDGE_LOOP('',(#81586,#81587,#81588,#81589));
#16865=EDGE_LOOP('',(#81590,#81591,#81592,#81593));
#16866=EDGE_LOOP('',(#81594,#81595,#81596,#81597));
#16867=EDGE_LOOP('',(#81598,#81599,#81600,#81601));
#16868=EDGE_LOOP('',(#81602,#81603,#81604,#81605,#81606));
#16869=EDGE_LOOP('',(#81607,#81608,#81609,#81610,#81611));
#16870=EDGE_LOOP('',(#81612,#81613,#81614,#81615,#81616,#81617));
#16871=EDGE_LOOP('',(#81618,#81619,#81620,#81621));
#16872=EDGE_LOOP('',(#81622,#81623,#81624,#81625,#81626));
#16873=EDGE_LOOP('',(#81627,#81628,#81629,#81630));
#16874=EDGE_LOOP('',(#81631,#81632,#81633,#81634));
#16875=EDGE_LOOP('',(#81635,#81636,#81637,#81638));
#16876=EDGE_LOOP('',(#81639,#81640,#81641,#81642));
#16877=EDGE_LOOP('',(#81643,#81644,#81645,#81646));
#16878=EDGE_LOOP('',(#81647,#81648,#81649,#81650,#81651));
#16879=EDGE_LOOP('',(#81652,#81653,#81654,#81655));
#16880=EDGE_LOOP('',(#81656,#81657,#81658,#81659));
#16881=EDGE_LOOP('',(#81660,#81661,#81662,#81663));
#16882=EDGE_LOOP('',(#81664,#81665,#81666,#81667));
#16883=EDGE_LOOP('',(#81668,#81669,#81670,#81671));
#16884=EDGE_LOOP('',(#81672,#81673,#81674,#81675,#81676));
#16885=EDGE_LOOP('',(#81677,#81678,#81679,#81680,#81681));
#16886=EDGE_LOOP('',(#81682,#81683,#81684,#81685,#81686,#81687));
#16887=EDGE_LOOP('',(#81688,#81689,#81690,#81691));
#16888=EDGE_LOOP('',(#81692,#81693,#81694,#81695,#81696));
#16889=EDGE_LOOP('',(#81697,#81698,#81699,#81700));
#16890=EDGE_LOOP('',(#81701,#81702,#81703,#81704));
#16891=EDGE_LOOP('',(#81705,#81706,#81707,#81708));
#16892=EDGE_LOOP('',(#81709,#81710,#81711,#81712));
#16893=EDGE_LOOP('',(#81713,#81714,#81715,#81716));
#16894=EDGE_LOOP('',(#81717,#81718,#81719,#81720,#81721));
#16895=EDGE_LOOP('',(#81722,#81723,#81724,#81725));
#16896=EDGE_LOOP('',(#81726,#81727,#81728,#81729));
#16897=EDGE_LOOP('',(#81730,#81731,#81732,#81733));
#16898=EDGE_LOOP('',(#81734,#81735,#81736,#81737));
#16899=EDGE_LOOP('',(#81738,#81739,#81740,#81741));
#16900=EDGE_LOOP('',(#81742,#81743,#81744,#81745,#81746));
#16901=EDGE_LOOP('',(#81747,#81748,#81749,#81750,#81751));
#16902=EDGE_LOOP('',(#81752,#81753,#81754,#81755,#81756,#81757));
#16903=EDGE_LOOP('',(#81758,#81759,#81760,#81761));
#16904=EDGE_LOOP('',(#81762,#81763,#81764,#81765,#81766));
#16905=EDGE_LOOP('',(#81767,#81768,#81769,#81770));
#16906=EDGE_LOOP('',(#81771,#81772,#81773,#81774));
#16907=EDGE_LOOP('',(#81775,#81776,#81777,#81778));
#16908=EDGE_LOOP('',(#81779,#81780,#81781,#81782));
#16909=EDGE_LOOP('',(#81783,#81784,#81785,#81786));
#16910=EDGE_LOOP('',(#81787,#81788,#81789,#81790,#81791));
#16911=EDGE_LOOP('',(#81792,#81793,#81794,#81795));
#16912=EDGE_LOOP('',(#81796,#81797,#81798,#81799));
#16913=EDGE_LOOP('',(#81800,#81801,#81802,#81803));
#16914=EDGE_LOOP('',(#81804,#81805,#81806,#81807));
#16915=EDGE_LOOP('',(#81808,#81809,#81810,#81811));
#16916=EDGE_LOOP('',(#81812,#81813,#81814,#81815,#81816));
#16917=EDGE_LOOP('',(#81817,#81818,#81819,#81820,#81821));
#16918=EDGE_LOOP('',(#81822,#81823,#81824,#81825,#81826,#81827));
#16919=EDGE_LOOP('',(#81828,#81829,#81830,#81831));
#16920=EDGE_LOOP('',(#81832,#81833,#81834,#81835,#81836));
#16921=EDGE_LOOP('',(#81837,#81838,#81839,#81840));
#16922=EDGE_LOOP('',(#81841,#81842,#81843,#81844));
#16923=EDGE_LOOP('',(#81845,#81846,#81847,#81848));
#16924=EDGE_LOOP('',(#81849,#81850,#81851,#81852));
#16925=EDGE_LOOP('',(#81853,#81854,#81855,#81856));
#16926=EDGE_LOOP('',(#81857,#81858,#81859,#81860,#81861));
#16927=EDGE_LOOP('',(#81862,#81863,#81864,#81865));
#16928=EDGE_LOOP('',(#81866,#81867,#81868,#81869));
#16929=EDGE_LOOP('',(#81870,#81871,#81872,#81873));
#16930=EDGE_LOOP('',(#81874,#81875,#81876,#81877));
#16931=EDGE_LOOP('',(#81878,#81879,#81880,#81881));
#16932=EDGE_LOOP('',(#81882,#81883,#81884,#81885,#81886));
#16933=EDGE_LOOP('',(#81887,#81888,#81889,#81890,#81891));
#16934=EDGE_LOOP('',(#81892,#81893,#81894,#81895,#81896,#81897));
#16935=EDGE_LOOP('',(#81898,#81899,#81900,#81901));
#16936=EDGE_LOOP('',(#81902,#81903,#81904,#81905,#81906));
#16937=EDGE_LOOP('',(#81907,#81908,#81909,#81910));
#16938=EDGE_LOOP('',(#81911,#81912,#81913,#81914));
#16939=EDGE_LOOP('',(#81915,#81916,#81917,#81918));
#16940=EDGE_LOOP('',(#81919,#81920,#81921,#81922));
#16941=EDGE_LOOP('',(#81923,#81924,#81925,#81926));
#16942=EDGE_LOOP('',(#81927,#81928,#81929,#81930,#81931));
#16943=EDGE_LOOP('',(#81932,#81933,#81934,#81935));
#16944=EDGE_LOOP('',(#81936,#81937,#81938,#81939));
#16945=EDGE_LOOP('',(#81940,#81941,#81942,#81943));
#16946=EDGE_LOOP('',(#81944,#81945,#81946,#81947));
#16947=EDGE_LOOP('',(#81948,#81949,#81950,#81951));
#16948=EDGE_LOOP('',(#81952,#81953,#81954,#81955,#81956));
#16949=EDGE_LOOP('',(#81957,#81958,#81959,#81960,#81961));
#16950=EDGE_LOOP('',(#81962,#81963,#81964,#81965,#81966,#81967));
#16951=EDGE_LOOP('',(#81968,#81969,#81970,#81971));
#16952=EDGE_LOOP('',(#81972,#81973,#81974,#81975,#81976));
#16953=EDGE_LOOP('',(#81977,#81978,#81979,#81980));
#16954=EDGE_LOOP('',(#81981,#81982,#81983,#81984));
#16955=EDGE_LOOP('',(#81985,#81986,#81987,#81988));
#16956=EDGE_LOOP('',(#81989,#81990,#81991,#81992));
#16957=EDGE_LOOP('',(#81993,#81994,#81995,#81996));
#16958=EDGE_LOOP('',(#81997,#81998,#81999,#82000,#82001));
#16959=EDGE_LOOP('',(#82002,#82003,#82004,#82005));
#16960=EDGE_LOOP('',(#82006,#82007,#82008,#82009));
#16961=EDGE_LOOP('',(#82010,#82011,#82012,#82013));
#16962=EDGE_LOOP('',(#82014,#82015,#82016,#82017));
#16963=EDGE_LOOP('',(#82018,#82019,#82020,#82021));
#16964=EDGE_LOOP('',(#82022,#82023,#82024,#82025,#82026));
#16965=EDGE_LOOP('',(#82027,#82028,#82029,#82030,#82031));
#16966=EDGE_LOOP('',(#82032,#82033,#82034,#82035,#82036,#82037));
#16967=EDGE_LOOP('',(#82038,#82039,#82040,#82041));
#16968=EDGE_LOOP('',(#82042,#82043,#82044,#82045,#82046));
#16969=EDGE_LOOP('',(#82047,#82048,#82049,#82050));
#16970=EDGE_LOOP('',(#82051,#82052,#82053,#82054));
#16971=EDGE_LOOP('',(#82055,#82056,#82057,#82058));
#16972=EDGE_LOOP('',(#82059,#82060,#82061,#82062));
#16973=EDGE_LOOP('',(#82063,#82064,#82065,#82066));
#16974=EDGE_LOOP('',(#82067,#82068,#82069,#82070,#82071));
#16975=EDGE_LOOP('',(#82072,#82073,#82074,#82075));
#16976=EDGE_LOOP('',(#82076,#82077,#82078,#82079));
#16977=EDGE_LOOP('',(#82080,#82081,#82082,#82083));
#16978=EDGE_LOOP('',(#82084,#82085,#82086,#82087));
#16979=EDGE_LOOP('',(#82088,#82089,#82090,#82091));
#16980=EDGE_LOOP('',(#82092,#82093,#82094,#82095,#82096));
#16981=EDGE_LOOP('',(#82097,#82098,#82099,#82100,#82101));
#16982=EDGE_LOOP('',(#82102,#82103,#82104,#82105,#82106,#82107));
#16983=EDGE_LOOP('',(#82108,#82109,#82110,#82111));
#16984=EDGE_LOOP('',(#82112,#82113,#82114,#82115,#82116));
#16985=EDGE_LOOP('',(#82117,#82118,#82119,#82120));
#16986=EDGE_LOOP('',(#82121,#82122,#82123,#82124));
#16987=EDGE_LOOP('',(#82125,#82126,#82127,#82128));
#16988=EDGE_LOOP('',(#82129,#82130,#82131,#82132));
#16989=EDGE_LOOP('',(#82133,#82134,#82135,#82136));
#16990=EDGE_LOOP('',(#82137,#82138,#82139,#82140,#82141));
#16991=EDGE_LOOP('',(#82142,#82143,#82144,#82145));
#16992=EDGE_LOOP('',(#82146,#82147,#82148,#82149));
#16993=EDGE_LOOP('',(#82150,#82151,#82152,#82153));
#16994=EDGE_LOOP('',(#82154,#82155,#82156,#82157));
#16995=EDGE_LOOP('',(#82158,#82159,#82160,#82161));
#16996=EDGE_LOOP('',(#82162,#82163,#82164,#82165,#82166));
#16997=EDGE_LOOP('',(#82167,#82168,#82169,#82170,#82171));
#16998=EDGE_LOOP('',(#82172,#82173,#82174,#82175,#82176,#82177));
#16999=EDGE_LOOP('',(#82178,#82179,#82180,#82181));
#17000=EDGE_LOOP('',(#82182,#82183,#82184,#82185,#82186));
#17001=EDGE_LOOP('',(#82187,#82188,#82189,#82190));
#17002=EDGE_LOOP('',(#82191,#82192,#82193,#82194));
#17003=EDGE_LOOP('',(#82195,#82196,#82197,#82198));
#17004=EDGE_LOOP('',(#82199,#82200,#82201,#82202));
#17005=EDGE_LOOP('',(#82203,#82204,#82205,#82206));
#17006=EDGE_LOOP('',(#82207,#82208,#82209,#82210,#82211));
#17007=EDGE_LOOP('',(#82212,#82213,#82214,#82215));
#17008=EDGE_LOOP('',(#82216,#82217,#82218,#82219));
#17009=EDGE_LOOP('',(#82220,#82221,#82222,#82223));
#17010=EDGE_LOOP('',(#82224,#82225,#82226,#82227));
#17011=EDGE_LOOP('',(#82228,#82229,#82230,#82231));
#17012=EDGE_LOOP('',(#82232,#82233,#82234,#82235,#82236));
#17013=EDGE_LOOP('',(#82237,#82238,#82239,#82240,#82241));
#17014=EDGE_LOOP('',(#82242,#82243,#82244,#82245,#82246,#82247));
#17015=EDGE_LOOP('',(#82248,#82249,#82250,#82251));
#17016=EDGE_LOOP('',(#82252,#82253,#82254,#82255,#82256));
#17017=EDGE_LOOP('',(#82257,#82258,#82259,#82260));
#17018=EDGE_LOOP('',(#82261,#82262,#82263,#82264));
#17019=EDGE_LOOP('',(#82265,#82266,#82267,#82268));
#17020=EDGE_LOOP('',(#82269,#82270,#82271,#82272));
#17021=EDGE_LOOP('',(#82273,#82274,#82275,#82276));
#17022=EDGE_LOOP('',(#82277,#82278,#82279,#82280,#82281));
#17023=EDGE_LOOP('',(#82282,#82283,#82284,#82285));
#17024=EDGE_LOOP('',(#82286,#82287,#82288,#82289));
#17025=EDGE_LOOP('',(#82290,#82291,#82292,#82293));
#17026=EDGE_LOOP('',(#82294,#82295,#82296,#82297));
#17027=EDGE_LOOP('',(#82298,#82299,#82300,#82301));
#17028=EDGE_LOOP('',(#82302,#82303,#82304,#82305,#82306));
#17029=EDGE_LOOP('',(#82307,#82308,#82309,#82310,#82311));
#17030=EDGE_LOOP('',(#82312,#82313,#82314,#82315,#82316,#82317));
#17031=EDGE_LOOP('',(#82318,#82319,#82320,#82321));
#17032=EDGE_LOOP('',(#82322,#82323,#82324,#82325,#82326));
#17033=EDGE_LOOP('',(#82327,#82328,#82329,#82330));
#17034=EDGE_LOOP('',(#82331,#82332,#82333,#82334));
#17035=EDGE_LOOP('',(#82335,#82336,#82337,#82338));
#17036=EDGE_LOOP('',(#82339,#82340,#82341,#82342));
#17037=EDGE_LOOP('',(#82343,#82344,#82345,#82346));
#17038=EDGE_LOOP('',(#82347,#82348,#82349,#82350,#82351));
#17039=EDGE_LOOP('',(#82352,#82353,#82354,#82355));
#17040=EDGE_LOOP('',(#82356,#82357,#82358,#82359));
#17041=EDGE_LOOP('',(#82360,#82361,#82362,#82363));
#17042=EDGE_LOOP('',(#82364,#82365,#82366,#82367));
#17043=EDGE_LOOP('',(#82368,#82369,#82370,#82371));
#17044=EDGE_LOOP('',(#82372,#82373,#82374,#82375,#82376));
#17045=EDGE_LOOP('',(#82377,#82378,#82379,#82380,#82381));
#17046=EDGE_LOOP('',(#82382,#82383,#82384,#82385,#82386,#82387));
#17047=EDGE_LOOP('',(#82388,#82389,#82390,#82391));
#17048=EDGE_LOOP('',(#82392,#82393,#82394,#82395,#82396));
#17049=EDGE_LOOP('',(#82397,#82398,#82399,#82400));
#17050=EDGE_LOOP('',(#82401,#82402,#82403,#82404));
#17051=EDGE_LOOP('',(#82405,#82406,#82407,#82408));
#17052=EDGE_LOOP('',(#82409,#82410,#82411,#82412));
#17053=EDGE_LOOP('',(#82413,#82414,#82415,#82416));
#17054=EDGE_LOOP('',(#82417,#82418,#82419,#82420,#82421));
#17055=EDGE_LOOP('',(#82422,#82423,#82424,#82425));
#17056=EDGE_LOOP('',(#82426,#82427,#82428,#82429));
#17057=EDGE_LOOP('',(#82430,#82431,#82432,#82433));
#17058=EDGE_LOOP('',(#82434,#82435,#82436,#82437));
#17059=EDGE_LOOP('',(#82438,#82439,#82440,#82441));
#17060=EDGE_LOOP('',(#82442,#82443,#82444,#82445,#82446));
#17061=EDGE_LOOP('',(#82447,#82448,#82449,#82450,#82451));
#17062=EDGE_LOOP('',(#82452,#82453,#82454,#82455,#82456,#82457));
#17063=EDGE_LOOP('',(#82458,#82459,#82460,#82461));
#17064=EDGE_LOOP('',(#82462,#82463,#82464,#82465,#82466));
#17065=EDGE_LOOP('',(#82467,#82468,#82469,#82470));
#17066=EDGE_LOOP('',(#82471,#82472,#82473,#82474));
#17067=EDGE_LOOP('',(#82475,#82476,#82477,#82478));
#17068=EDGE_LOOP('',(#82479,#82480,#82481,#82482));
#17069=EDGE_LOOP('',(#82483,#82484,#82485,#82486));
#17070=EDGE_LOOP('',(#82487,#82488,#82489,#82490,#82491));
#17071=EDGE_LOOP('',(#82492,#82493,#82494,#82495));
#17072=EDGE_LOOP('',(#82496,#82497,#82498,#82499));
#17073=EDGE_LOOP('',(#82500,#82501,#82502,#82503));
#17074=EDGE_LOOP('',(#82504,#82505,#82506,#82507));
#17075=EDGE_LOOP('',(#82508,#82509,#82510,#82511));
#17076=EDGE_LOOP('',(#82512,#82513,#82514,#82515,#82516));
#17077=EDGE_LOOP('',(#82517,#82518,#82519,#82520,#82521));
#17078=EDGE_LOOP('',(#82522,#82523,#82524,#82525,#82526,#82527));
#17079=EDGE_LOOP('',(#82528,#82529,#82530,#82531));
#17080=EDGE_LOOP('',(#82532,#82533,#82534,#82535,#82536));
#17081=EDGE_LOOP('',(#82537,#82538,#82539,#82540));
#17082=EDGE_LOOP('',(#82541,#82542,#82543,#82544));
#17083=EDGE_LOOP('',(#82545,#82546,#82547,#82548));
#17084=EDGE_LOOP('',(#82549,#82550,#82551,#82552));
#17085=EDGE_LOOP('',(#82553,#82554,#82555,#82556));
#17086=EDGE_LOOP('',(#82557,#82558,#82559,#82560,#82561));
#17087=EDGE_LOOP('',(#82562,#82563,#82564,#82565));
#17088=EDGE_LOOP('',(#82566,#82567,#82568,#82569));
#17089=EDGE_LOOP('',(#82570,#82571,#82572,#82573));
#17090=EDGE_LOOP('',(#82574,#82575,#82576,#82577));
#17091=EDGE_LOOP('',(#82578,#82579,#82580,#82581));
#17092=EDGE_LOOP('',(#82582,#82583,#82584,#82585,#82586));
#17093=EDGE_LOOP('',(#82587,#82588,#82589,#82590,#82591));
#17094=EDGE_LOOP('',(#82592,#82593,#82594,#82595,#82596,#82597));
#17095=EDGE_LOOP('',(#82598,#82599,#82600,#82601));
#17096=EDGE_LOOP('',(#82602,#82603,#82604,#82605,#82606));
#17097=EDGE_LOOP('',(#82607,#82608,#82609,#82610));
#17098=EDGE_LOOP('',(#82611,#82612,#82613,#82614));
#17099=EDGE_LOOP('',(#82615,#82616,#82617,#82618));
#17100=EDGE_LOOP('',(#82619,#82620,#82621,#82622));
#17101=EDGE_LOOP('',(#82623,#82624,#82625,#82626));
#17102=EDGE_LOOP('',(#82627,#82628,#82629,#82630,#82631));
#17103=EDGE_LOOP('',(#82632,#82633,#82634,#82635));
#17104=EDGE_LOOP('',(#82636,#82637,#82638,#82639));
#17105=EDGE_LOOP('',(#82640,#82641,#82642,#82643));
#17106=EDGE_LOOP('',(#82644,#82645,#82646,#82647));
#17107=EDGE_LOOP('',(#82648,#82649,#82650,#82651));
#17108=EDGE_LOOP('',(#82652,#82653,#82654,#82655,#82656));
#17109=EDGE_LOOP('',(#82657,#82658,#82659,#82660,#82661));
#17110=EDGE_LOOP('',(#82662,#82663,#82664,#82665,#82666,#82667));
#17111=EDGE_LOOP('',(#82668,#82669,#82670,#82671));
#17112=EDGE_LOOP('',(#82672,#82673,#82674,#82675,#82676));
#17113=EDGE_LOOP('',(#82677,#82678,#82679,#82680));
#17114=EDGE_LOOP('',(#82681,#82682,#82683,#82684));
#17115=EDGE_LOOP('',(#82685,#82686,#82687,#82688));
#17116=EDGE_LOOP('',(#82689,#82690,#82691,#82692));
#17117=EDGE_LOOP('',(#82693,#82694,#82695,#82696));
#17118=EDGE_LOOP('',(#82697,#82698,#82699,#82700,#82701));
#17119=EDGE_LOOP('',(#82702,#82703,#82704,#82705));
#17120=EDGE_LOOP('',(#82706,#82707,#82708,#82709));
#17121=EDGE_LOOP('',(#82710,#82711,#82712,#82713));
#17122=EDGE_LOOP('',(#82714,#82715,#82716,#82717));
#17123=EDGE_LOOP('',(#82718,#82719,#82720,#82721));
#17124=EDGE_LOOP('',(#82722,#82723,#82724,#82725,#82726));
#17125=EDGE_LOOP('',(#82727,#82728,#82729,#82730,#82731));
#17126=EDGE_LOOP('',(#82732,#82733,#82734,#82735,#82736,#82737));
#17127=EDGE_LOOP('',(#82738,#82739,#82740,#82741));
#17128=EDGE_LOOP('',(#82742,#82743,#82744,#82745,#82746));
#17129=EDGE_LOOP('',(#82747,#82748,#82749,#82750));
#17130=EDGE_LOOP('',(#82751,#82752,#82753,#82754));
#17131=EDGE_LOOP('',(#82755,#82756,#82757,#82758));
#17132=EDGE_LOOP('',(#82759,#82760,#82761,#82762));
#17133=EDGE_LOOP('',(#82763,#82764,#82765,#82766));
#17134=EDGE_LOOP('',(#82767,#82768,#82769,#82770,#82771));
#17135=EDGE_LOOP('',(#82772,#82773,#82774,#82775));
#17136=EDGE_LOOP('',(#82776,#82777,#82778,#82779));
#17137=EDGE_LOOP('',(#82780,#82781,#82782,#82783));
#17138=EDGE_LOOP('',(#82784,#82785,#82786,#82787));
#17139=EDGE_LOOP('',(#82788,#82789,#82790,#82791));
#17140=EDGE_LOOP('',(#82792,#82793,#82794,#82795,#82796));
#17141=EDGE_LOOP('',(#82797,#82798,#82799,#82800,#82801));
#17142=EDGE_LOOP('',(#82802,#82803,#82804,#82805,#82806,#82807));
#17143=EDGE_LOOP('',(#82808,#82809,#82810,#82811));
#17144=EDGE_LOOP('',(#82812,#82813,#82814,#82815,#82816));
#17145=EDGE_LOOP('',(#82817,#82818,#82819,#82820));
#17146=EDGE_LOOP('',(#82821,#82822,#82823,#82824));
#17147=EDGE_LOOP('',(#82825,#82826,#82827,#82828));
#17148=EDGE_LOOP('',(#82829,#82830,#82831,#82832));
#17149=EDGE_LOOP('',(#82833,#82834,#82835,#82836));
#17150=EDGE_LOOP('',(#82837,#82838,#82839,#82840,#82841));
#17151=EDGE_LOOP('',(#82842,#82843,#82844,#82845));
#17152=EDGE_LOOP('',(#82846,#82847,#82848,#82849));
#17153=EDGE_LOOP('',(#82850,#82851,#82852,#82853));
#17154=EDGE_LOOP('',(#82854,#82855,#82856,#82857));
#17155=EDGE_LOOP('',(#82858,#82859,#82860,#82861));
#17156=EDGE_LOOP('',(#82862,#82863,#82864,#82865,#82866));
#17157=EDGE_LOOP('',(#82867,#82868,#82869,#82870,#82871));
#17158=EDGE_LOOP('',(#82872,#82873,#82874,#82875,#82876,#82877));
#17159=EDGE_LOOP('',(#82878,#82879,#82880,#82881));
#17160=EDGE_LOOP('',(#82882,#82883,#82884,#82885,#82886));
#17161=EDGE_LOOP('',(#82887,#82888,#82889,#82890));
#17162=EDGE_LOOP('',(#82891,#82892,#82893,#82894));
#17163=EDGE_LOOP('',(#82895,#82896,#82897,#82898));
#17164=EDGE_LOOP('',(#82899,#82900,#82901,#82902));
#17165=EDGE_LOOP('',(#82903,#82904,#82905,#82906));
#17166=EDGE_LOOP('',(#82907,#82908,#82909,#82910,#82911));
#17167=EDGE_LOOP('',(#82912,#82913,#82914,#82915));
#17168=EDGE_LOOP('',(#82916,#82917,#82918,#82919));
#17169=EDGE_LOOP('',(#82920,#82921,#82922,#82923));
#17170=EDGE_LOOP('',(#82924,#82925,#82926,#82927));
#17171=EDGE_LOOP('',(#82928,#82929,#82930,#82931));
#17172=EDGE_LOOP('',(#82932,#82933,#82934,#82935,#82936));
#17173=EDGE_LOOP('',(#82937,#82938,#82939,#82940,#82941));
#17174=EDGE_LOOP('',(#82942,#82943,#82944,#82945,#82946,#82947));
#17175=EDGE_LOOP('',(#82948,#82949,#82950,#82951));
#17176=EDGE_LOOP('',(#82952,#82953,#82954,#82955,#82956));
#17177=EDGE_LOOP('',(#82957,#82958,#82959,#82960));
#17178=EDGE_LOOP('',(#82961,#82962,#82963,#82964));
#17179=EDGE_LOOP('',(#82965,#82966,#82967,#82968));
#17180=EDGE_LOOP('',(#82969,#82970,#82971,#82972));
#17181=EDGE_LOOP('',(#82973,#82974,#82975,#82976));
#17182=EDGE_LOOP('',(#82977,#82978,#82979,#82980,#82981));
#17183=EDGE_LOOP('',(#82982,#82983,#82984,#82985));
#17184=EDGE_LOOP('',(#82986,#82987,#82988,#82989));
#17185=EDGE_LOOP('',(#82990,#82991,#82992,#82993));
#17186=EDGE_LOOP('',(#82994,#82995,#82996,#82997));
#17187=EDGE_LOOP('',(#82998,#82999,#83000,#83001));
#17188=EDGE_LOOP('',(#83002,#83003,#83004,#83005,#83006));
#17189=EDGE_LOOP('',(#83007,#83008,#83009,#83010,#83011));
#17190=EDGE_LOOP('',(#83012,#83013,#83014,#83015,#83016,#83017));
#17191=EDGE_LOOP('',(#83018,#83019,#83020,#83021));
#17192=EDGE_LOOP('',(#83022,#83023,#83024,#83025,#83026));
#17193=EDGE_LOOP('',(#83027,#83028,#83029,#83030));
#17194=EDGE_LOOP('',(#83031,#83032,#83033,#83034));
#17195=EDGE_LOOP('',(#83035,#83036,#83037,#83038));
#17196=EDGE_LOOP('',(#83039,#83040,#83041,#83042));
#17197=EDGE_LOOP('',(#83043,#83044,#83045,#83046));
#17198=EDGE_LOOP('',(#83047,#83048,#83049,#83050,#83051));
#17199=EDGE_LOOP('',(#83052,#83053,#83054,#83055));
#17200=EDGE_LOOP('',(#83056,#83057,#83058,#83059));
#17201=EDGE_LOOP('',(#83060,#83061,#83062,#83063));
#17202=EDGE_LOOP('',(#83064,#83065,#83066,#83067));
#17203=EDGE_LOOP('',(#83068,#83069,#83070,#83071));
#17204=EDGE_LOOP('',(#83072,#83073,#83074,#83075,#83076));
#17205=EDGE_LOOP('',(#83077,#83078,#83079,#83080,#83081));
#17206=EDGE_LOOP('',(#83082,#83083,#83084,#83085,#83086,#83087));
#17207=EDGE_LOOP('',(#83088,#83089,#83090,#83091));
#17208=EDGE_LOOP('',(#83092,#83093,#83094,#83095,#83096));
#17209=EDGE_LOOP('',(#83097,#83098,#83099,#83100));
#17210=EDGE_LOOP('',(#83101,#83102,#83103,#83104));
#17211=EDGE_LOOP('',(#83105,#83106,#83107,#83108));
#17212=EDGE_LOOP('',(#83109,#83110,#83111,#83112));
#17213=EDGE_LOOP('',(#83113,#83114,#83115,#83116));
#17214=EDGE_LOOP('',(#83117,#83118,#83119,#83120,#83121));
#17215=EDGE_LOOP('',(#83122,#83123,#83124,#83125));
#17216=EDGE_LOOP('',(#83126,#83127,#83128,#83129));
#17217=EDGE_LOOP('',(#83130,#83131,#83132,#83133));
#17218=EDGE_LOOP('',(#83134,#83135,#83136,#83137));
#17219=EDGE_LOOP('',(#83138,#83139,#83140,#83141));
#17220=EDGE_LOOP('',(#83142,#83143,#83144,#83145,#83146));
#17221=EDGE_LOOP('',(#83147,#83148,#83149,#83150,#83151));
#17222=EDGE_LOOP('',(#83152,#83153,#83154,#83155,#83156,#83157));
#17223=EDGE_LOOP('',(#83158,#83159,#83160,#83161));
#17224=EDGE_LOOP('',(#83162,#83163,#83164,#83165,#83166));
#17225=EDGE_LOOP('',(#83167,#83168,#83169,#83170));
#17226=EDGE_LOOP('',(#83171,#83172,#83173,#83174));
#17227=EDGE_LOOP('',(#83175,#83176,#83177,#83178));
#17228=EDGE_LOOP('',(#83179,#83180,#83181,#83182));
#17229=EDGE_LOOP('',(#83183,#83184,#83185,#83186));
#17230=EDGE_LOOP('',(#83187,#83188,#83189,#83190,#83191));
#17231=EDGE_LOOP('',(#83192,#83193,#83194,#83195));
#17232=EDGE_LOOP('',(#83196,#83197,#83198,#83199));
#17233=EDGE_LOOP('',(#83200,#83201,#83202,#83203));
#17234=EDGE_LOOP('',(#83204,#83205,#83206,#83207));
#17235=EDGE_LOOP('',(#83208,#83209,#83210,#83211));
#17236=EDGE_LOOP('',(#83212,#83213,#83214,#83215,#83216));
#17237=EDGE_LOOP('',(#83217,#83218,#83219,#83220,#83221));
#17238=EDGE_LOOP('',(#83222,#83223,#83224,#83225,#83226,#83227));
#17239=EDGE_LOOP('',(#83228,#83229,#83230,#83231));
#17240=EDGE_LOOP('',(#83232,#83233,#83234,#83235,#83236));
#17241=EDGE_LOOP('',(#83237,#83238,#83239,#83240));
#17242=EDGE_LOOP('',(#83241,#83242,#83243,#83244));
#17243=EDGE_LOOP('',(#83245,#83246,#83247,#83248));
#17244=EDGE_LOOP('',(#83249,#83250,#83251,#83252));
#17245=EDGE_LOOP('',(#83253,#83254,#83255,#83256));
#17246=EDGE_LOOP('',(#83257,#83258,#83259,#83260,#83261));
#17247=EDGE_LOOP('',(#83262,#83263,#83264,#83265));
#17248=EDGE_LOOP('',(#83266,#83267,#83268,#83269));
#17249=EDGE_LOOP('',(#83270,#83271,#83272,#83273));
#17250=EDGE_LOOP('',(#83274,#83275,#83276,#83277));
#17251=EDGE_LOOP('',(#83278,#83279,#83280,#83281));
#17252=EDGE_LOOP('',(#83282,#83283,#83284,#83285,#83286));
#17253=EDGE_LOOP('',(#83287,#83288,#83289,#83290,#83291));
#17254=EDGE_LOOP('',(#83292,#83293,#83294,#83295,#83296,#83297));
#17255=EDGE_LOOP('',(#83298,#83299,#83300,#83301));
#17256=EDGE_LOOP('',(#83302,#83303,#83304,#83305,#83306));
#17257=EDGE_LOOP('',(#83307,#83308,#83309,#83310));
#17258=EDGE_LOOP('',(#83311,#83312,#83313,#83314));
#17259=EDGE_LOOP('',(#83315,#83316,#83317,#83318));
#17260=EDGE_LOOP('',(#83319,#83320,#83321,#83322));
#17261=EDGE_LOOP('',(#83323,#83324,#83325,#83326));
#17262=EDGE_LOOP('',(#83327,#83328,#83329,#83330,#83331));
#17263=EDGE_LOOP('',(#83332,#83333,#83334,#83335));
#17264=EDGE_LOOP('',(#83336,#83337,#83338,#83339));
#17265=EDGE_LOOP('',(#83340,#83341,#83342,#83343));
#17266=EDGE_LOOP('',(#83344,#83345,#83346,#83347));
#17267=EDGE_LOOP('',(#83348,#83349,#83350,#83351));
#17268=EDGE_LOOP('',(#83352,#83353,#83354,#83355,#83356));
#17269=EDGE_LOOP('',(#83357,#83358,#83359,#83360,#83361));
#17270=EDGE_LOOP('',(#83362,#83363,#83364,#83365,#83366,#83367));
#17271=EDGE_LOOP('',(#83368,#83369,#83370,#83371));
#17272=EDGE_LOOP('',(#83372,#83373,#83374,#83375,#83376));
#17273=EDGE_LOOP('',(#83377,#83378,#83379,#83380));
#17274=EDGE_LOOP('',(#83381,#83382,#83383,#83384));
#17275=EDGE_LOOP('',(#83385,#83386,#83387,#83388));
#17276=EDGE_LOOP('',(#83389,#83390,#83391,#83392));
#17277=EDGE_LOOP('',(#83393,#83394,#83395,#83396));
#17278=EDGE_LOOP('',(#83397,#83398,#83399,#83400,#83401));
#17279=EDGE_LOOP('',(#83402,#83403,#83404,#83405));
#17280=EDGE_LOOP('',(#83406,#83407,#83408,#83409));
#17281=EDGE_LOOP('',(#83410,#83411,#83412,#83413));
#17282=EDGE_LOOP('',(#83414,#83415,#83416,#83417));
#17283=EDGE_LOOP('',(#83418,#83419,#83420,#83421));
#17284=EDGE_LOOP('',(#83422,#83423,#83424,#83425,#83426));
#17285=EDGE_LOOP('',(#83427,#83428,#83429,#83430,#83431));
#17286=EDGE_LOOP('',(#83432,#83433,#83434,#83435,#83436,#83437));
#17287=EDGE_LOOP('',(#83438,#83439,#83440,#83441));
#17288=EDGE_LOOP('',(#83442,#83443,#83444,#83445,#83446));
#17289=EDGE_LOOP('',(#83447,#83448,#83449,#83450));
#17290=EDGE_LOOP('',(#83451,#83452,#83453,#83454));
#17291=EDGE_LOOP('',(#83455,#83456,#83457,#83458));
#17292=EDGE_LOOP('',(#83459,#83460,#83461,#83462));
#17293=EDGE_LOOP('',(#83463,#83464,#83465,#83466));
#17294=EDGE_LOOP('',(#83467,#83468,#83469,#83470,#83471));
#17295=EDGE_LOOP('',(#83472,#83473,#83474,#83475));
#17296=EDGE_LOOP('',(#83476,#83477,#83478,#83479));
#17297=EDGE_LOOP('',(#83480,#83481,#83482,#83483));
#17298=EDGE_LOOP('',(#83484,#83485,#83486,#83487));
#17299=EDGE_LOOP('',(#83488,#83489,#83490,#83491));
#17300=EDGE_LOOP('',(#83492,#83493,#83494,#83495,#83496));
#17301=EDGE_LOOP('',(#83497,#83498,#83499,#83500,#83501));
#17302=EDGE_LOOP('',(#83502,#83503,#83504,#83505,#83506,#83507));
#17303=EDGE_LOOP('',(#83508,#83509,#83510,#83511));
#17304=EDGE_LOOP('',(#83512,#83513,#83514,#83515,#83516));
#17305=EDGE_LOOP('',(#83517,#83518,#83519,#83520));
#17306=EDGE_LOOP('',(#83521,#83522,#83523,#83524));
#17307=EDGE_LOOP('',(#83525,#83526,#83527,#83528));
#17308=EDGE_LOOP('',(#83529,#83530,#83531,#83532));
#17309=EDGE_LOOP('',(#83533,#83534,#83535,#83536));
#17310=EDGE_LOOP('',(#83537,#83538,#83539,#83540,#83541));
#17311=EDGE_LOOP('',(#83542,#83543,#83544,#83545));
#17312=EDGE_LOOP('',(#83546,#83547,#83548,#83549));
#17313=EDGE_LOOP('',(#83550,#83551,#83552,#83553));
#17314=EDGE_LOOP('',(#83554,#83555,#83556,#83557));
#17315=EDGE_LOOP('',(#83558,#83559,#83560,#83561));
#17316=EDGE_LOOP('',(#83562,#83563,#83564,#83565,#83566));
#17317=EDGE_LOOP('',(#83567,#83568,#83569,#83570,#83571));
#17318=EDGE_LOOP('',(#83572,#83573,#83574,#83575,#83576,#83577));
#17319=EDGE_LOOP('',(#83578,#83579,#83580,#83581));
#17320=EDGE_LOOP('',(#83582,#83583,#83584,#83585,#83586));
#17321=EDGE_LOOP('',(#83587,#83588,#83589,#83590));
#17322=EDGE_LOOP('',(#83591,#83592,#83593,#83594));
#17323=EDGE_LOOP('',(#83595,#83596,#83597,#83598));
#17324=EDGE_LOOP('',(#83599,#83600,#83601,#83602));
#17325=EDGE_LOOP('',(#83603,#83604,#83605,#83606));
#17326=EDGE_LOOP('',(#83607,#83608,#83609,#83610,#83611));
#17327=EDGE_LOOP('',(#83612,#83613,#83614,#83615));
#17328=EDGE_LOOP('',(#83616,#83617,#83618,#83619));
#17329=EDGE_LOOP('',(#83620,#83621,#83622,#83623));
#17330=EDGE_LOOP('',(#83624,#83625,#83626,#83627));
#17331=EDGE_LOOP('',(#83628,#83629,#83630,#83631));
#17332=EDGE_LOOP('',(#83632,#83633,#83634,#83635,#83636));
#17333=EDGE_LOOP('',(#83637,#83638,#83639,#83640,#83641));
#17334=EDGE_LOOP('',(#83642,#83643,#83644,#83645,#83646,#83647));
#17335=EDGE_LOOP('',(#83648,#83649,#83650,#83651));
#17336=EDGE_LOOP('',(#83652,#83653,#83654,#83655,#83656));
#17337=EDGE_LOOP('',(#83657,#83658,#83659,#83660));
#17338=EDGE_LOOP('',(#83661,#83662,#83663,#83664));
#17339=EDGE_LOOP('',(#83665,#83666,#83667,#83668));
#17340=EDGE_LOOP('',(#83669,#83670,#83671,#83672));
#17341=EDGE_LOOP('',(#83673,#83674,#83675,#83676));
#17342=EDGE_LOOP('',(#83677,#83678,#83679,#83680,#83681));
#17343=EDGE_LOOP('',(#83682,#83683,#83684,#83685));
#17344=EDGE_LOOP('',(#83686,#83687,#83688,#83689));
#17345=EDGE_LOOP('',(#83690,#83691,#83692,#83693));
#17346=EDGE_LOOP('',(#83694,#83695,#83696,#83697));
#17347=EDGE_LOOP('',(#83698,#83699,#83700,#83701));
#17348=EDGE_LOOP('',(#83702,#83703,#83704,#83705,#83706));
#17349=EDGE_LOOP('',(#83707,#83708,#83709,#83710,#83711));
#17350=EDGE_LOOP('',(#83712,#83713,#83714,#83715,#83716,#83717));
#17351=EDGE_LOOP('',(#83718,#83719,#83720,#83721));
#17352=EDGE_LOOP('',(#83722,#83723,#83724,#83725,#83726));
#17353=EDGE_LOOP('',(#83727,#83728,#83729,#83730));
#17354=EDGE_LOOP('',(#83731,#83732,#83733,#83734));
#17355=EDGE_LOOP('',(#83735,#83736,#83737,#83738));
#17356=EDGE_LOOP('',(#83739,#83740,#83741,#83742));
#17357=EDGE_LOOP('',(#83743,#83744,#83745,#83746));
#17358=EDGE_LOOP('',(#83747,#83748,#83749,#83750,#83751));
#17359=EDGE_LOOP('',(#83752,#83753,#83754,#83755));
#17360=EDGE_LOOP('',(#83756,#83757,#83758,#83759));
#17361=EDGE_LOOP('',(#83760,#83761,#83762,#83763));
#17362=EDGE_LOOP('',(#83764,#83765,#83766,#83767));
#17363=EDGE_LOOP('',(#83768,#83769,#83770,#83771));
#17364=EDGE_LOOP('',(#83772,#83773,#83774,#83775,#83776));
#17365=EDGE_LOOP('',(#83777,#83778,#83779,#83780,#83781));
#17366=EDGE_LOOP('',(#83782,#83783,#83784,#83785,#83786,#83787));
#17367=EDGE_LOOP('',(#83788,#83789,#83790,#83791));
#17368=EDGE_LOOP('',(#83792,#83793,#83794,#83795,#83796));
#17369=EDGE_LOOP('',(#83797,#83798,#83799,#83800));
#17370=EDGE_LOOP('',(#83801,#83802,#83803,#83804));
#17371=EDGE_LOOP('',(#83805,#83806,#83807,#83808));
#17372=EDGE_LOOP('',(#83809,#83810,#83811,#83812));
#17373=EDGE_LOOP('',(#83813,#83814,#83815,#83816));
#17374=EDGE_LOOP('',(#83817,#83818,#83819,#83820,#83821));
#17375=EDGE_LOOP('',(#83822,#83823,#83824,#83825));
#17376=EDGE_LOOP('',(#83826,#83827,#83828,#83829));
#17377=EDGE_LOOP('',(#83830,#83831,#83832,#83833));
#17378=EDGE_LOOP('',(#83834,#83835,#83836,#83837));
#17379=EDGE_LOOP('',(#83838,#83839,#83840,#83841));
#17380=EDGE_LOOP('',(#83842,#83843,#83844,#83845,#83846));
#17381=EDGE_LOOP('',(#83847,#83848,#83849,#83850,#83851));
#17382=EDGE_LOOP('',(#83852,#83853,#83854,#83855,#83856,#83857));
#17383=EDGE_LOOP('',(#83858,#83859,#83860,#83861));
#17384=EDGE_LOOP('',(#83862,#83863,#83864,#83865,#83866));
#17385=EDGE_LOOP('',(#83867,#83868,#83869,#83870));
#17386=EDGE_LOOP('',(#83871,#83872,#83873,#83874));
#17387=EDGE_LOOP('',(#83875,#83876,#83877,#83878));
#17388=EDGE_LOOP('',(#83879,#83880,#83881,#83882));
#17389=EDGE_LOOP('',(#83883,#83884,#83885,#83886));
#17390=EDGE_LOOP('',(#83887,#83888,#83889,#83890,#83891));
#17391=EDGE_LOOP('',(#83892,#83893,#83894,#83895));
#17392=EDGE_LOOP('',(#83896,#83897,#83898,#83899));
#17393=EDGE_LOOP('',(#83900,#83901,#83902,#83903));
#17394=EDGE_LOOP('',(#83904,#83905,#83906,#83907));
#17395=EDGE_LOOP('',(#83908,#83909,#83910,#83911));
#17396=EDGE_LOOP('',(#83912,#83913,#83914,#83915,#83916));
#17397=EDGE_LOOP('',(#83917,#83918,#83919,#83920,#83921));
#17398=EDGE_LOOP('',(#83922,#83923,#83924,#83925,#83926,#83927));
#17399=EDGE_LOOP('',(#83928,#83929,#83930,#83931));
#17400=EDGE_LOOP('',(#83932,#83933,#83934,#83935,#83936));
#17401=EDGE_LOOP('',(#83937,#83938,#83939,#83940));
#17402=EDGE_LOOP('',(#83941,#83942,#83943,#83944));
#17403=EDGE_LOOP('',(#83945,#83946,#83947,#83948));
#17404=EDGE_LOOP('',(#83949,#83950,#83951,#83952));
#17405=EDGE_LOOP('',(#83953,#83954,#83955,#83956));
#17406=EDGE_LOOP('',(#83957,#83958,#83959,#83960,#83961));
#17407=EDGE_LOOP('',(#83962,#83963,#83964,#83965));
#17408=EDGE_LOOP('',(#83966,#83967,#83968,#83969));
#17409=EDGE_LOOP('',(#83970,#83971,#83972,#83973));
#17410=EDGE_LOOP('',(#83974,#83975,#83976,#83977));
#17411=EDGE_LOOP('',(#83978,#83979,#83980,#83981));
#17412=EDGE_LOOP('',(#83982,#83983,#83984,#83985,#83986));
#17413=EDGE_LOOP('',(#83987,#83988,#83989,#83990,#83991));
#17414=EDGE_LOOP('',(#83992,#83993,#83994,#83995,#83996,#83997));
#17415=EDGE_LOOP('',(#83998,#83999,#84000,#84001));
#17416=EDGE_LOOP('',(#84002,#84003,#84004,#84005,#84006));
#17417=EDGE_LOOP('',(#84007,#84008,#84009,#84010));
#17418=EDGE_LOOP('',(#84011,#84012,#84013,#84014));
#17419=EDGE_LOOP('',(#84015,#84016,#84017,#84018));
#17420=EDGE_LOOP('',(#84019,#84020,#84021,#84022));
#17421=EDGE_LOOP('',(#84023,#84024,#84025,#84026));
#17422=EDGE_LOOP('',(#84027,#84028,#84029,#84030,#84031));
#17423=EDGE_LOOP('',(#84032,#84033,#84034,#84035));
#17424=EDGE_LOOP('',(#84036,#84037,#84038,#84039));
#17425=EDGE_LOOP('',(#84040,#84041,#84042,#84043));
#17426=EDGE_LOOP('',(#84044,#84045,#84046,#84047));
#17427=EDGE_LOOP('',(#84048,#84049,#84050,#84051));
#17428=EDGE_LOOP('',(#84052,#84053,#84054,#84055,#84056));
#17429=EDGE_LOOP('',(#84057,#84058,#84059,#84060,#84061));
#17430=EDGE_LOOP('',(#84062,#84063,#84064,#84065,#84066,#84067));
#17431=EDGE_LOOP('',(#84068,#84069,#84070,#84071));
#17432=EDGE_LOOP('',(#84072,#84073,#84074,#84075,#84076));
#17433=EDGE_LOOP('',(#84077,#84078,#84079,#84080));
#17434=EDGE_LOOP('',(#84081,#84082,#84083,#84084));
#17435=EDGE_LOOP('',(#84085,#84086,#84087,#84088));
#17436=EDGE_LOOP('',(#84089,#84090,#84091,#84092));
#17437=EDGE_LOOP('',(#84093,#84094,#84095,#84096));
#17438=EDGE_LOOP('',(#84097,#84098,#84099,#84100,#84101));
#17439=EDGE_LOOP('',(#84102,#84103,#84104,#84105));
#17440=EDGE_LOOP('',(#84106,#84107,#84108,#84109));
#17441=EDGE_LOOP('',(#84110,#84111,#84112,#84113));
#17442=EDGE_LOOP('',(#84114,#84115,#84116,#84117));
#17443=EDGE_LOOP('',(#84118,#84119,#84120,#84121));
#17444=EDGE_LOOP('',(#84122,#84123,#84124,#84125,#84126));
#17445=EDGE_LOOP('',(#84127,#84128,#84129,#84130,#84131));
#17446=EDGE_LOOP('',(#84132,#84133,#84134,#84135,#84136,#84137));
#17447=EDGE_LOOP('',(#84138,#84139,#84140,#84141));
#17448=EDGE_LOOP('',(#84142,#84143,#84144,#84145,#84146));
#17449=EDGE_LOOP('',(#84147,#84148,#84149,#84150));
#17450=EDGE_LOOP('',(#84151,#84152,#84153,#84154));
#17451=EDGE_LOOP('',(#84155,#84156,#84157,#84158));
#17452=EDGE_LOOP('',(#84159,#84160,#84161,#84162));
#17453=EDGE_LOOP('',(#84163,#84164,#84165,#84166));
#17454=EDGE_LOOP('',(#84167,#84168,#84169,#84170,#84171));
#17455=EDGE_LOOP('',(#84172,#84173,#84174,#84175));
#17456=EDGE_LOOP('',(#84176,#84177,#84178,#84179));
#17457=EDGE_LOOP('',(#84180,#84181,#84182,#84183));
#17458=EDGE_LOOP('',(#84184,#84185,#84186,#84187));
#17459=EDGE_LOOP('',(#84188,#84189,#84190,#84191));
#17460=EDGE_LOOP('',(#84192,#84193,#84194,#84195,#84196));
#17461=EDGE_LOOP('',(#84197,#84198,#84199,#84200,#84201));
#17462=EDGE_LOOP('',(#84202,#84203,#84204,#84205,#84206,#84207));
#17463=EDGE_LOOP('',(#84208,#84209,#84210,#84211));
#17464=EDGE_LOOP('',(#84212,#84213,#84214,#84215,#84216));
#17465=EDGE_LOOP('',(#84217,#84218,#84219,#84220));
#17466=EDGE_LOOP('',(#84221,#84222,#84223,#84224));
#17467=EDGE_LOOP('',(#84225,#84226,#84227,#84228));
#17468=EDGE_LOOP('',(#84229,#84230,#84231,#84232));
#17469=EDGE_LOOP('',(#84233,#84234,#84235,#84236));
#17470=EDGE_LOOP('',(#84237,#84238,#84239,#84240,#84241));
#17471=EDGE_LOOP('',(#84242,#84243,#84244,#84245));
#17472=EDGE_LOOP('',(#84246,#84247,#84248,#84249));
#17473=EDGE_LOOP('',(#84250,#84251,#84252,#84253));
#17474=EDGE_LOOP('',(#84254,#84255,#84256,#84257));
#17475=EDGE_LOOP('',(#84258,#84259,#84260,#84261));
#17476=EDGE_LOOP('',(#84262,#84263,#84264,#84265,#84266));
#17477=EDGE_LOOP('',(#84267,#84268,#84269,#84270,#84271));
#17478=EDGE_LOOP('',(#84272,#84273,#84274,#84275,#84276,#84277));
#17479=EDGE_LOOP('',(#84278,#84279,#84280,#84281));
#17480=EDGE_LOOP('',(#84282,#84283,#84284,#84285,#84286));
#17481=EDGE_LOOP('',(#84287,#84288,#84289,#84290));
#17482=EDGE_LOOP('',(#84291,#84292,#84293,#84294));
#17483=EDGE_LOOP('',(#84295,#84296,#84297,#84298));
#17484=EDGE_LOOP('',(#84299,#84300,#84301,#84302));
#17485=EDGE_LOOP('',(#84303,#84304,#84305,#84306));
#17486=EDGE_LOOP('',(#84307,#84308,#84309,#84310,#84311));
#17487=EDGE_LOOP('',(#84312,#84313,#84314,#84315));
#17488=EDGE_LOOP('',(#84316,#84317,#84318,#84319));
#17489=EDGE_LOOP('',(#84320,#84321,#84322,#84323));
#17490=EDGE_LOOP('',(#84324,#84325,#84326,#84327));
#17491=EDGE_LOOP('',(#84328,#84329,#84330,#84331));
#17492=EDGE_LOOP('',(#84332,#84333,#84334,#84335,#84336));
#17493=EDGE_LOOP('',(#84337,#84338,#84339,#84340,#84341));
#17494=EDGE_LOOP('',(#84342,#84343,#84344,#84345,#84346,#84347));
#17495=EDGE_LOOP('',(#84348,#84349,#84350,#84351));
#17496=EDGE_LOOP('',(#84352,#84353,#84354,#84355,#84356));
#17497=EDGE_LOOP('',(#84357,#84358,#84359,#84360));
#17498=EDGE_LOOP('',(#84361,#84362,#84363,#84364));
#17499=EDGE_LOOP('',(#84365,#84366,#84367,#84368));
#17500=EDGE_LOOP('',(#84369,#84370,#84371,#84372));
#17501=EDGE_LOOP('',(#84373,#84374,#84375,#84376));
#17502=EDGE_LOOP('',(#84377,#84378,#84379,#84380,#84381));
#17503=EDGE_LOOP('',(#84382,#84383,#84384,#84385));
#17504=EDGE_LOOP('',(#84386,#84387,#84388,#84389));
#17505=EDGE_LOOP('',(#84390,#84391,#84392,#84393));
#17506=EDGE_LOOP('',(#84394,#84395,#84396,#84397));
#17507=EDGE_LOOP('',(#84398,#84399,#84400,#84401));
#17508=EDGE_LOOP('',(#84402,#84403,#84404,#84405,#84406));
#17509=EDGE_LOOP('',(#84407,#84408,#84409,#84410,#84411));
#17510=EDGE_LOOP('',(#84412,#84413,#84414,#84415,#84416,#84417));
#17511=EDGE_LOOP('',(#84418,#84419,#84420,#84421));
#17512=EDGE_LOOP('',(#84422,#84423,#84424,#84425,#84426));
#17513=EDGE_LOOP('',(#84427,#84428,#84429,#84430));
#17514=EDGE_LOOP('',(#84431,#84432,#84433,#84434));
#17515=EDGE_LOOP('',(#84435,#84436,#84437,#84438));
#17516=EDGE_LOOP('',(#84439,#84440,#84441,#84442));
#17517=EDGE_LOOP('',(#84443,#84444,#84445,#84446));
#17518=EDGE_LOOP('',(#84447,#84448,#84449,#84450,#84451));
#17519=EDGE_LOOP('',(#84452,#84453,#84454,#84455));
#17520=EDGE_LOOP('',(#84456,#84457,#84458,#84459));
#17521=EDGE_LOOP('',(#84460,#84461,#84462,#84463));
#17522=EDGE_LOOP('',(#84464,#84465,#84466,#84467));
#17523=EDGE_LOOP('',(#84468,#84469,#84470,#84471));
#17524=EDGE_LOOP('',(#84472,#84473,#84474,#84475,#84476));
#17525=EDGE_LOOP('',(#84477,#84478,#84479,#84480,#84481));
#17526=EDGE_LOOP('',(#84482,#84483,#84484,#84485,#84486,#84487));
#17527=EDGE_LOOP('',(#84488,#84489,#84490,#84491));
#17528=EDGE_LOOP('',(#84492,#84493,#84494,#84495,#84496));
#17529=EDGE_LOOP('',(#84497,#84498,#84499,#84500));
#17530=EDGE_LOOP('',(#84501,#84502,#84503,#84504));
#17531=EDGE_LOOP('',(#84505,#84506,#84507,#84508));
#17532=EDGE_LOOP('',(#84509,#84510,#84511,#84512));
#17533=EDGE_LOOP('',(#84513,#84514,#84515,#84516));
#17534=EDGE_LOOP('',(#84517,#84518,#84519,#84520,#84521));
#17535=EDGE_LOOP('',(#84522,#84523,#84524,#84525));
#17536=EDGE_LOOP('',(#84526,#84527,#84528,#84529));
#17537=EDGE_LOOP('',(#84530,#84531,#84532,#84533));
#17538=EDGE_LOOP('',(#84534,#84535,#84536,#84537));
#17539=EDGE_LOOP('',(#84538,#84539,#84540,#84541));
#17540=EDGE_LOOP('',(#84542,#84543,#84544,#84545,#84546));
#17541=EDGE_LOOP('',(#84547,#84548,#84549,#84550,#84551));
#17542=EDGE_LOOP('',(#84552,#84553,#84554,#84555,#84556,#84557));
#17543=EDGE_LOOP('',(#84558,#84559,#84560,#84561));
#17544=EDGE_LOOP('',(#84562,#84563,#84564,#84565,#84566));
#17545=EDGE_LOOP('',(#84567,#84568,#84569,#84570));
#17546=EDGE_LOOP('',(#84571,#84572,#84573,#84574));
#17547=EDGE_LOOP('',(#84575,#84576,#84577,#84578));
#17548=EDGE_LOOP('',(#84579,#84580,#84581,#84582));
#17549=EDGE_LOOP('',(#84583,#84584,#84585,#84586));
#17550=EDGE_LOOP('',(#84587,#84588,#84589,#84590,#84591));
#17551=EDGE_LOOP('',(#84592,#84593,#84594,#84595));
#17552=EDGE_LOOP('',(#84596,#84597,#84598,#84599));
#17553=EDGE_LOOP('',(#84600,#84601,#84602,#84603));
#17554=EDGE_LOOP('',(#84604,#84605,#84606,#84607));
#17555=EDGE_LOOP('',(#84608,#84609,#84610,#84611));
#17556=EDGE_LOOP('',(#84612,#84613,#84614,#84615,#84616));
#17557=EDGE_LOOP('',(#84617,#84618,#84619,#84620,#84621));
#17558=EDGE_LOOP('',(#84622,#84623,#84624,#84625,#84626,#84627));
#17559=EDGE_LOOP('',(#84628,#84629,#84630,#84631));
#17560=EDGE_LOOP('',(#84632,#84633,#84634,#84635,#84636));
#17561=EDGE_LOOP('',(#84637,#84638,#84639,#84640));
#17562=EDGE_LOOP('',(#84641,#84642,#84643,#84644));
#17563=EDGE_LOOP('',(#84645,#84646,#84647,#84648));
#17564=EDGE_LOOP('',(#84649,#84650,#84651,#84652));
#17565=EDGE_LOOP('',(#84653,#84654,#84655,#84656));
#17566=EDGE_LOOP('',(#84657,#84658,#84659,#84660,#84661));
#17567=EDGE_LOOP('',(#84662,#84663,#84664,#84665));
#17568=EDGE_LOOP('',(#84666,#84667,#84668,#84669));
#17569=EDGE_LOOP('',(#84670,#84671,#84672,#84673));
#17570=EDGE_LOOP('',(#84674,#84675,#84676,#84677));
#17571=EDGE_LOOP('',(#84678,#84679,#84680,#84681));
#17572=EDGE_LOOP('',(#84682,#84683,#84684,#84685,#84686));
#17573=EDGE_LOOP('',(#84687,#84688,#84689,#84690,#84691));
#17574=EDGE_LOOP('',(#84692,#84693,#84694,#84695,#84696,#84697));
#17575=EDGE_LOOP('',(#84698,#84699,#84700,#84701));
#17576=EDGE_LOOP('',(#84702,#84703,#84704,#84705,#84706));
#17577=EDGE_LOOP('',(#84707,#84708,#84709,#84710));
#17578=EDGE_LOOP('',(#84711,#84712,#84713,#84714));
#17579=EDGE_LOOP('',(#84715,#84716,#84717,#84718));
#17580=EDGE_LOOP('',(#84719,#84720,#84721,#84722));
#17581=EDGE_LOOP('',(#84723,#84724,#84725,#84726));
#17582=EDGE_LOOP('',(#84727,#84728,#84729,#84730,#84731));
#17583=EDGE_LOOP('',(#84732,#84733,#84734,#84735));
#17584=EDGE_LOOP('',(#84736,#84737,#84738,#84739));
#17585=EDGE_LOOP('',(#84740,#84741,#84742,#84743));
#17586=EDGE_LOOP('',(#84744,#84745,#84746,#84747));
#17587=EDGE_LOOP('',(#84748,#84749,#84750,#84751));
#17588=EDGE_LOOP('',(#84752,#84753,#84754,#84755,#84756));
#17589=EDGE_LOOP('',(#84757,#84758,#84759,#84760,#84761));
#17590=EDGE_LOOP('',(#84762,#84763,#84764,#84765,#84766,#84767));
#17591=EDGE_LOOP('',(#84768,#84769,#84770,#84771));
#17592=EDGE_LOOP('',(#84772,#84773,#84774,#84775,#84776));
#17593=EDGE_LOOP('',(#84777,#84778,#84779,#84780));
#17594=EDGE_LOOP('',(#84781,#84782,#84783,#84784));
#17595=EDGE_LOOP('',(#84785,#84786,#84787,#84788));
#17596=EDGE_LOOP('',(#84789,#84790,#84791,#84792));
#17597=EDGE_LOOP('',(#84793,#84794,#84795,#84796));
#17598=EDGE_LOOP('',(#84797,#84798,#84799,#84800,#84801));
#17599=EDGE_LOOP('',(#84802,#84803,#84804,#84805));
#17600=EDGE_LOOP('',(#84806,#84807,#84808,#84809));
#17601=EDGE_LOOP('',(#84810,#84811,#84812,#84813));
#17602=EDGE_LOOP('',(#84814,#84815,#84816,#84817));
#17603=EDGE_LOOP('',(#84818,#84819,#84820,#84821));
#17604=EDGE_LOOP('',(#84822,#84823,#84824,#84825,#84826));
#17605=EDGE_LOOP('',(#84827,#84828,#84829,#84830,#84831));
#17606=EDGE_LOOP('',(#84832,#84833,#84834,#84835,#84836,#84837));
#17607=EDGE_LOOP('',(#84838,#84839,#84840,#84841));
#17608=EDGE_LOOP('',(#84842,#84843,#84844,#84845,#84846));
#17609=EDGE_LOOP('',(#84847,#84848,#84849,#84850));
#17610=EDGE_LOOP('',(#84851,#84852,#84853,#84854));
#17611=EDGE_LOOP('',(#84855,#84856,#84857,#84858));
#17612=EDGE_LOOP('',(#84859,#84860,#84861,#84862));
#17613=EDGE_LOOP('',(#84863,#84864,#84865,#84866));
#17614=EDGE_LOOP('',(#84867,#84868,#84869,#84870,#84871));
#17615=EDGE_LOOP('',(#84872,#84873,#84874,#84875));
#17616=EDGE_LOOP('',(#84876,#84877,#84878,#84879));
#17617=EDGE_LOOP('',(#84880,#84881,#84882,#84883));
#17618=EDGE_LOOP('',(#84884,#84885,#84886,#84887));
#17619=EDGE_LOOP('',(#84888,#84889,#84890,#84891));
#17620=EDGE_LOOP('',(#84892,#84893,#84894,#84895,#84896));
#17621=EDGE_LOOP('',(#84897,#84898,#84899,#84900,#84901));
#17622=EDGE_LOOP('',(#84902,#84903,#84904,#84905,#84906,#84907));
#17623=EDGE_LOOP('',(#84908,#84909,#84910,#84911));
#17624=EDGE_LOOP('',(#84912,#84913,#84914,#84915,#84916));
#17625=EDGE_LOOP('',(#84917,#84918,#84919,#84920));
#17626=EDGE_LOOP('',(#84921,#84922,#84923,#84924));
#17627=EDGE_LOOP('',(#84925,#84926,#84927,#84928));
#17628=EDGE_LOOP('',(#84929,#84930,#84931,#84932));
#17629=EDGE_LOOP('',(#84933,#84934,#84935,#84936));
#17630=EDGE_LOOP('',(#84937,#84938,#84939,#84940,#84941));
#17631=EDGE_LOOP('',(#84942,#84943,#84944,#84945));
#17632=EDGE_LOOP('',(#84946,#84947,#84948,#84949));
#17633=EDGE_LOOP('',(#84950,#84951,#84952,#84953));
#17634=EDGE_LOOP('',(#84954,#84955,#84956,#84957));
#17635=EDGE_LOOP('',(#84958,#84959,#84960,#84961));
#17636=EDGE_LOOP('',(#84962,#84963,#84964,#84965,#84966));
#17637=EDGE_LOOP('',(#84967,#84968,#84969,#84970,#84971));
#17638=EDGE_LOOP('',(#84972,#84973,#84974,#84975,#84976,#84977));
#17639=EDGE_LOOP('',(#84978,#84979,#84980,#84981));
#17640=EDGE_LOOP('',(#84982,#84983,#84984,#84985,#84986));
#17641=EDGE_LOOP('',(#84987,#84988,#84989,#84990));
#17642=EDGE_LOOP('',(#84991,#84992,#84993,#84994));
#17643=EDGE_LOOP('',(#84995,#84996,#84997,#84998));
#17644=EDGE_LOOP('',(#84999,#85000,#85001,#85002));
#17645=EDGE_LOOP('',(#85003,#85004,#85005,#85006));
#17646=EDGE_LOOP('',(#85007,#85008,#85009,#85010,#85011));
#17647=EDGE_LOOP('',(#85012,#85013,#85014,#85015));
#17648=EDGE_LOOP('',(#85016,#85017,#85018,#85019));
#17649=EDGE_LOOP('',(#85020,#85021,#85022,#85023));
#17650=EDGE_LOOP('',(#85024,#85025,#85026,#85027));
#17651=EDGE_LOOP('',(#85028,#85029,#85030,#85031));
#17652=EDGE_LOOP('',(#85032,#85033,#85034,#85035,#85036));
#17653=EDGE_LOOP('',(#85037,#85038,#85039,#85040,#85041));
#17654=EDGE_LOOP('',(#85042,#85043,#85044,#85045,#85046,#85047));
#17655=EDGE_LOOP('',(#85048,#85049,#85050,#85051));
#17656=EDGE_LOOP('',(#85052,#85053,#85054,#85055,#85056));
#17657=EDGE_LOOP('',(#85057,#85058,#85059,#85060));
#17658=EDGE_LOOP('',(#85061,#85062,#85063,#85064));
#17659=EDGE_LOOP('',(#85065,#85066,#85067,#85068));
#17660=EDGE_LOOP('',(#85069,#85070,#85071,#85072));
#17661=EDGE_LOOP('',(#85073,#85074,#85075,#85076));
#17662=EDGE_LOOP('',(#85077,#85078,#85079,#85080,#85081));
#17663=EDGE_LOOP('',(#85082,#85083,#85084,#85085));
#17664=EDGE_LOOP('',(#85086,#85087,#85088,#85089));
#17665=EDGE_LOOP('',(#85090,#85091,#85092,#85093));
#17666=EDGE_LOOP('',(#85094,#85095,#85096,#85097));
#17667=EDGE_LOOP('',(#85098,#85099,#85100,#85101));
#17668=EDGE_LOOP('',(#85102,#85103,#85104,#85105,#85106));
#17669=EDGE_LOOP('',(#85107,#85108,#85109,#85110,#85111));
#17670=EDGE_LOOP('',(#85112,#85113,#85114,#85115,#85116,#85117));
#17671=EDGE_LOOP('',(#85118,#85119,#85120,#85121));
#17672=EDGE_LOOP('',(#85122,#85123,#85124,#85125,#85126));
#17673=EDGE_LOOP('',(#85127,#85128,#85129,#85130));
#17674=EDGE_LOOP('',(#85131,#85132,#85133,#85134));
#17675=EDGE_LOOP('',(#85135,#85136,#85137,#85138));
#17676=EDGE_LOOP('',(#85139,#85140,#85141,#85142));
#17677=EDGE_LOOP('',(#85143,#85144,#85145,#85146));
#17678=EDGE_LOOP('',(#85147,#85148,#85149,#85150,#85151));
#17679=EDGE_LOOP('',(#85152,#85153,#85154,#85155));
#17680=EDGE_LOOP('',(#85156,#85157,#85158,#85159));
#17681=EDGE_LOOP('',(#85160,#85161,#85162,#85163));
#17682=EDGE_LOOP('',(#85164,#85165,#85166,#85167));
#17683=EDGE_LOOP('',(#85168,#85169,#85170,#85171));
#17684=EDGE_LOOP('',(#85172,#85173,#85174,#85175,#85176));
#17685=EDGE_LOOP('',(#85177,#85178,#85179,#85180,#85181));
#17686=EDGE_LOOP('',(#85182,#85183,#85184,#85185,#85186,#85187));
#17687=EDGE_LOOP('',(#85188,#85189,#85190,#85191));
#17688=EDGE_LOOP('',(#85192,#85193,#85194,#85195,#85196));
#17689=EDGE_LOOP('',(#85197,#85198,#85199,#85200));
#17690=EDGE_LOOP('',(#85201,#85202,#85203,#85204));
#17691=EDGE_LOOP('',(#85205,#85206,#85207,#85208));
#17692=EDGE_LOOP('',(#85209,#85210,#85211,#85212));
#17693=EDGE_LOOP('',(#85213,#85214,#85215,#85216));
#17694=EDGE_LOOP('',(#85217,#85218,#85219,#85220,#85221));
#17695=EDGE_LOOP('',(#85222,#85223,#85224,#85225));
#17696=EDGE_LOOP('',(#85226,#85227,#85228,#85229));
#17697=EDGE_LOOP('',(#85230,#85231,#85232,#85233));
#17698=EDGE_LOOP('',(#85234,#85235,#85236,#85237));
#17699=EDGE_LOOP('',(#85238,#85239,#85240,#85241));
#17700=EDGE_LOOP('',(#85242,#85243,#85244,#85245,#85246));
#17701=EDGE_LOOP('',(#85247,#85248,#85249,#85250,#85251));
#17702=EDGE_LOOP('',(#85252,#85253,#85254,#85255,#85256,#85257));
#17703=EDGE_LOOP('',(#85258,#85259,#85260,#85261));
#17704=EDGE_LOOP('',(#85262,#85263,#85264,#85265,#85266));
#17705=EDGE_LOOP('',(#85267,#85268,#85269,#85270));
#17706=EDGE_LOOP('',(#85271,#85272,#85273,#85274));
#17707=EDGE_LOOP('',(#85275,#85276,#85277,#85278));
#17708=EDGE_LOOP('',(#85279,#85280,#85281,#85282));
#17709=EDGE_LOOP('',(#85283,#85284,#85285,#85286));
#17710=EDGE_LOOP('',(#85287,#85288,#85289,#85290,#85291));
#17711=EDGE_LOOP('',(#85292,#85293,#85294,#85295));
#17712=EDGE_LOOP('',(#85296,#85297,#85298,#85299));
#17713=EDGE_LOOP('',(#85300,#85301,#85302,#85303));
#17714=EDGE_LOOP('',(#85304,#85305,#85306,#85307));
#17715=EDGE_LOOP('',(#85308,#85309,#85310,#85311));
#17716=EDGE_LOOP('',(#85312,#85313,#85314,#85315,#85316));
#17717=EDGE_LOOP('',(#85317,#85318,#85319,#85320,#85321));
#17718=EDGE_LOOP('',(#85322,#85323,#85324,#85325,#85326,#85327));
#17719=EDGE_LOOP('',(#85328,#85329,#85330,#85331));
#17720=EDGE_LOOP('',(#85332,#85333,#85334,#85335,#85336));
#17721=EDGE_LOOP('',(#85337,#85338,#85339,#85340));
#17722=EDGE_LOOP('',(#85341,#85342,#85343,#85344));
#17723=EDGE_LOOP('',(#85345,#85346,#85347,#85348));
#17724=EDGE_LOOP('',(#85349,#85350,#85351,#85352));
#17725=EDGE_LOOP('',(#85353,#85354,#85355,#85356));
#17726=EDGE_LOOP('',(#85357,#85358,#85359,#85360,#85361));
#17727=EDGE_LOOP('',(#85362,#85363,#85364,#85365));
#17728=EDGE_LOOP('',(#85366,#85367,#85368,#85369));
#17729=EDGE_LOOP('',(#85370,#85371,#85372,#85373));
#17730=EDGE_LOOP('',(#85374,#85375,#85376,#85377));
#17731=EDGE_LOOP('',(#85378,#85379,#85380,#85381));
#17732=EDGE_LOOP('',(#85382,#85383,#85384,#85385,#85386));
#17733=EDGE_LOOP('',(#85387,#85388,#85389,#85390,#85391));
#17734=EDGE_LOOP('',(#85392,#85393,#85394,#85395,#85396,#85397));
#17735=EDGE_LOOP('',(#85398,#85399,#85400,#85401));
#17736=EDGE_LOOP('',(#85402,#85403,#85404,#85405,#85406));
#17737=EDGE_LOOP('',(#85407,#85408,#85409,#85410));
#17738=EDGE_LOOP('',(#85411,#85412,#85413,#85414));
#17739=EDGE_LOOP('',(#85415,#85416,#85417,#85418));
#17740=EDGE_LOOP('',(#85419,#85420,#85421,#85422));
#17741=EDGE_LOOP('',(#85423,#85424,#85425,#85426));
#17742=EDGE_LOOP('',(#85427,#85428,#85429,#85430,#85431));
#17743=EDGE_LOOP('',(#85432,#85433,#85434,#85435));
#17744=EDGE_LOOP('',(#85436,#85437,#85438,#85439));
#17745=EDGE_LOOP('',(#85440,#85441,#85442,#85443));
#17746=EDGE_LOOP('',(#85444,#85445,#85446,#85447));
#17747=EDGE_LOOP('',(#85448,#85449,#85450,#85451));
#17748=EDGE_LOOP('',(#85452,#85453,#85454,#85455,#85456));
#17749=EDGE_LOOP('',(#85457,#85458,#85459,#85460,#85461));
#17750=EDGE_LOOP('',(#85462,#85463,#85464,#85465,#85466,#85467));
#17751=EDGE_LOOP('',(#85468,#85469,#85470,#85471));
#17752=EDGE_LOOP('',(#85472,#85473,#85474,#85475,#85476));
#17753=EDGE_LOOP('',(#85477,#85478,#85479,#85480));
#17754=EDGE_LOOP('',(#85481,#85482,#85483,#85484));
#17755=EDGE_LOOP('',(#85485,#85486,#85487,#85488));
#17756=EDGE_LOOP('',(#85489,#85490,#85491,#85492));
#17757=EDGE_LOOP('',(#85493,#85494,#85495,#85496));
#17758=EDGE_LOOP('',(#85497,#85498,#85499,#85500,#85501));
#17759=EDGE_LOOP('',(#85502,#85503,#85504,#85505));
#17760=EDGE_LOOP('',(#85506,#85507,#85508,#85509));
#17761=EDGE_LOOP('',(#85510,#85511,#85512,#85513));
#17762=EDGE_LOOP('',(#85514,#85515,#85516,#85517));
#17763=EDGE_LOOP('',(#85518,#85519,#85520,#85521));
#17764=EDGE_LOOP('',(#85522,#85523,#85524,#85525,#85526));
#17765=EDGE_LOOP('',(#85527,#85528,#85529,#85530,#85531));
#17766=EDGE_LOOP('',(#85532,#85533,#85534,#85535,#85536,#85537));
#17767=EDGE_LOOP('',(#85538,#85539,#85540,#85541));
#17768=EDGE_LOOP('',(#85542,#85543,#85544,#85545,#85546));
#17769=EDGE_LOOP('',(#85547,#85548,#85549,#85550));
#17770=EDGE_LOOP('',(#85551,#85552,#85553,#85554));
#17771=EDGE_LOOP('',(#85555,#85556,#85557,#85558));
#17772=EDGE_LOOP('',(#85559,#85560,#85561,#85562));
#17773=EDGE_LOOP('',(#85563,#85564,#85565,#85566));
#17774=EDGE_LOOP('',(#85567,#85568,#85569,#85570,#85571));
#17775=EDGE_LOOP('',(#85572,#85573,#85574,#85575));
#17776=EDGE_LOOP('',(#85576,#85577,#85578,#85579));
#17777=EDGE_LOOP('',(#85580,#85581,#85582,#85583));
#17778=EDGE_LOOP('',(#85584,#85585,#85586,#85587));
#17779=EDGE_LOOP('',(#85588,#85589,#85590,#85591));
#17780=EDGE_LOOP('',(#85592,#85593,#85594,#85595,#85596));
#17781=EDGE_LOOP('',(#85597,#85598,#85599,#85600,#85601));
#17782=EDGE_LOOP('',(#85602,#85603,#85604,#85605,#85606,#85607));
#17783=EDGE_LOOP('',(#85608,#85609,#85610,#85611));
#17784=EDGE_LOOP('',(#85612,#85613,#85614,#85615,#85616));
#17785=EDGE_LOOP('',(#85617,#85618,#85619,#85620));
#17786=EDGE_LOOP('',(#85621,#85622,#85623,#85624));
#17787=EDGE_LOOP('',(#85625,#85626,#85627,#85628));
#17788=EDGE_LOOP('',(#85629,#85630,#85631,#85632));
#17789=EDGE_LOOP('',(#85633,#85634,#85635,#85636));
#17790=EDGE_LOOP('',(#85637,#85638,#85639,#85640,#85641));
#17791=EDGE_LOOP('',(#85642,#85643,#85644,#85645));
#17792=EDGE_LOOP('',(#85646,#85647,#85648,#85649));
#17793=EDGE_LOOP('',(#85650,#85651,#85652,#85653));
#17794=EDGE_LOOP('',(#85654,#85655,#85656,#85657));
#17795=EDGE_LOOP('',(#85658,#85659,#85660,#85661));
#17796=EDGE_LOOP('',(#85662,#85663,#85664,#85665,#85666));
#17797=EDGE_LOOP('',(#85667,#85668,#85669,#85670,#85671));
#17798=EDGE_LOOP('',(#85672,#85673,#85674,#85675,#85676,#85677));
#17799=EDGE_LOOP('',(#85678,#85679,#85680,#85681));
#17800=EDGE_LOOP('',(#85682,#85683,#85684,#85685,#85686));
#17801=EDGE_LOOP('',(#85687,#85688,#85689,#85690));
#17802=EDGE_LOOP('',(#85691,#85692,#85693,#85694));
#17803=EDGE_LOOP('',(#85695,#85696,#85697,#85698));
#17804=EDGE_LOOP('',(#85699,#85700,#85701,#85702));
#17805=EDGE_LOOP('',(#85703,#85704,#85705,#85706));
#17806=EDGE_LOOP('',(#85707,#85708,#85709,#85710,#85711));
#17807=EDGE_LOOP('',(#85712,#85713,#85714,#85715));
#17808=EDGE_LOOP('',(#85716,#85717,#85718,#85719));
#17809=EDGE_LOOP('',(#85720,#85721,#85722,#85723));
#17810=EDGE_LOOP('',(#85724,#85725,#85726,#85727));
#17811=EDGE_LOOP('',(#85728,#85729,#85730,#85731));
#17812=EDGE_LOOP('',(#85732,#85733,#85734,#85735,#85736));
#17813=EDGE_LOOP('',(#85737,#85738,#85739,#85740,#85741));
#17814=EDGE_LOOP('',(#85742,#85743,#85744,#85745,#85746,#85747));
#17815=EDGE_LOOP('',(#85748,#85749,#85750,#85751));
#17816=EDGE_LOOP('',(#85752,#85753,#85754,#85755,#85756));
#17817=EDGE_LOOP('',(#85757,#85758,#85759,#85760));
#17818=EDGE_LOOP('',(#85761,#85762,#85763,#85764));
#17819=EDGE_LOOP('',(#85765,#85766,#85767,#85768));
#17820=EDGE_LOOP('',(#85769,#85770,#85771,#85772));
#17821=EDGE_LOOP('',(#85773,#85774,#85775,#85776));
#17822=EDGE_LOOP('',(#85777,#85778,#85779,#85780,#85781));
#17823=EDGE_LOOP('',(#85782,#85783,#85784,#85785));
#17824=EDGE_LOOP('',(#85786,#85787,#85788,#85789));
#17825=EDGE_LOOP('',(#85790,#85791,#85792,#85793));
#17826=EDGE_LOOP('',(#85794,#85795,#85796,#85797));
#17827=EDGE_LOOP('',(#85798,#85799,#85800,#85801));
#17828=EDGE_LOOP('',(#85802,#85803,#85804));
#17829=EDGE_LOOP('',(#85805,#85806,#85807,#85808,#85809));
#17830=EDGE_LOOP('',(#85810,#85811,#85812,#85813));
#17831=EDGE_LOOP('',(#85814,#85815,#85816,#85817));
#17832=EDGE_LOOP('',(#85818,#85819,#85820,#85821));
#17833=EDGE_LOOP('',(#85822,#85823,#85824,#85825));
#17834=EDGE_LOOP('',(#85826,#85827,#85828,#85829));
#17835=EDGE_LOOP('',(#85830,#85831,#85832,#85833));
#17836=EDGE_LOOP('',(#85834,#85835,#85836,#85837));
#17837=EDGE_LOOP('',(#85838,#85839,#85840,#85841));
#17838=EDGE_LOOP('',(#85842,#85843,#85844,#85845));
#17839=EDGE_LOOP('',(#85846,#85847,#85848,#85849));
#17840=EDGE_LOOP('',(#85850,#85851,#85852,#85853));
#17841=EDGE_LOOP('',(#85854,#85855,#85856,#85857));
#17842=EDGE_LOOP('',(#85858,#85859,#85860,#85861));
#17843=EDGE_LOOP('',(#85862,#85863,#85864,#85865));
#17844=EDGE_LOOP('',(#85866,#85867,#85868));
#17845=EDGE_LOOP('',(#85869,#85870,#85871,#85872,#85873));
#17846=EDGE_LOOP('',(#85874,#85875,#85876,#85877));
#17847=EDGE_LOOP('',(#85878,#85879,#85880,#85881));
#17848=EDGE_LOOP('',(#85882,#85883,#85884,#85885));
#17849=EDGE_LOOP('',(#85886,#85887,#85888,#85889));
#17850=EDGE_LOOP('',(#85890,#85891,#85892,#85893));
#17851=EDGE_LOOP('',(#85894,#85895,#85896,#85897));
#17852=EDGE_LOOP('',(#85898,#85899,#85900,#85901));
#17853=EDGE_LOOP('',(#85902,#85903,#85904,#85905));
#17854=EDGE_LOOP('',(#85906,#85907,#85908,#85909));
#17855=EDGE_LOOP('',(#85910,#85911,#85912,#85913));
#17856=EDGE_LOOP('',(#85914,#85915,#85916,#85917));
#17857=EDGE_LOOP('',(#85918,#85919,#85920,#85921));
#17858=EDGE_LOOP('',(#85922,#85923,#85924,#85925));
#17859=EDGE_LOOP('',(#85926,#85927,#85928,#85929));
#17860=EDGE_LOOP('',(#85930,#85931,#85932));
#17861=EDGE_LOOP('',(#85933,#85934,#85935,#85936,#85937));
#17862=EDGE_LOOP('',(#85938,#85939,#85940,#85941));
#17863=EDGE_LOOP('',(#85942,#85943,#85944,#85945));
#17864=EDGE_LOOP('',(#85946,#85947,#85948,#85949));
#17865=EDGE_LOOP('',(#85950,#85951,#85952,#85953));
#17866=EDGE_LOOP('',(#85954,#85955,#85956,#85957));
#17867=EDGE_LOOP('',(#85958,#85959,#85960,#85961));
#17868=EDGE_LOOP('',(#85962,#85963,#85964,#85965));
#17869=EDGE_LOOP('',(#85966,#85967,#85968,#85969));
#17870=EDGE_LOOP('',(#85970,#85971,#85972,#85973));
#17871=EDGE_LOOP('',(#85974,#85975,#85976,#85977));
#17872=EDGE_LOOP('',(#85978,#85979,#85980,#85981));
#17873=EDGE_LOOP('',(#85982,#85983,#85984,#85985));
#17874=EDGE_LOOP('',(#85986,#85987,#85988,#85989));
#17875=EDGE_LOOP('',(#85990,#85991,#85992,#85993));
#17876=EDGE_LOOP('',(#85994,#85995,#85996));
#17877=EDGE_LOOP('',(#85997,#85998,#85999,#86000,#86001));
#17878=EDGE_LOOP('',(#86002,#86003,#86004,#86005));
#17879=EDGE_LOOP('',(#86006,#86007,#86008,#86009));
#17880=EDGE_LOOP('',(#86010,#86011,#86012,#86013));
#17881=EDGE_LOOP('',(#86014,#86015,#86016,#86017));
#17882=EDGE_LOOP('',(#86018,#86019,#86020,#86021));
#17883=EDGE_LOOP('',(#86022,#86023,#86024,#86025));
#17884=EDGE_LOOP('',(#86026,#86027,#86028,#86029));
#17885=EDGE_LOOP('',(#86030,#86031,#86032,#86033));
#17886=EDGE_LOOP('',(#86034,#86035,#86036,#86037));
#17887=EDGE_LOOP('',(#86038,#86039,#86040,#86041));
#17888=EDGE_LOOP('',(#86042,#86043,#86044,#86045));
#17889=EDGE_LOOP('',(#86046,#86047,#86048,#86049));
#17890=EDGE_LOOP('',(#86050,#86051,#86052,#86053));
#17891=EDGE_LOOP('',(#86054,#86055,#86056,#86057));
#17892=EDGE_LOOP('',(#86058,#86059,#86060,#86061));
#17893=EDGE_LOOP('',(#86062,#86063,#86064,#86065,#86066));
#17894=EDGE_LOOP('',(#86067));
#17895=EDGE_LOOP('',(#86068,#86069,#86070,#86071));
#17896=EDGE_LOOP('',(#86072,#86073,#86074,#86075));
#17897=EDGE_LOOP('',(#86076,#86077,#86078,#86079));
#17898=EDGE_LOOP('',(#86080,#86081,#86082,#86083));
#17899=EDGE_LOOP('',(#86084));
#17900=EDGE_LOOP('',(#86085,#86086,#86087,#86088));
#17901=EDGE_LOOP('',(#86089,#86090,#86091,#86092,#86093,#86094,#86095,#86096,
#86097,#86098,#86099,#86100,#86101,#86102,#86103,#86104,#86105,#86106,#86107,
#86108));
#17902=EDGE_LOOP('',(#86109,#86110,#86111,#86112,#86113,#86114,#86115,#86116,
#86117,#86118,#86119,#86120,#86121,#86122,#86123,#86124,#86125,#86126,#86127));
#17903=EDGE_LOOP('',(#86128));
#17904=EDGE_LOOP('',(#86129,#86130,#86131,#86132,#86133));
#17905=EDGE_LOOP('',(#86134,#86135,#86136,#86137,#86138));
#17906=EDGE_LOOP('',(#86139,#86140,#86141,#86142,#86143));
#17907=EDGE_LOOP('',(#86144));
#17908=EDGE_LOOP('',(#86145,#86146,#86147,#86148,#86149));
#17909=EDGE_LOOP('',(#86150,#86151,#86152,#86153));
#17910=EDGE_LOOP('',(#86154,#86155,#86156,#86157));
#17911=EDGE_LOOP('',(#86158,#86159,#86160,#86161,#86162));
#17912=EDGE_LOOP('',(#86163,#86164,#86165,#86166));
#17913=EDGE_LOOP('',(#86167,#86168,#86169,#86170));
#17914=EDGE_LOOP('',(#86171,#86172,#86173,#86174));
#17915=EDGE_LOOP('',(#86175,#86176,#86177,#86178));
#17916=EDGE_LOOP('',(#86179,#86180,#86181,#86182));
#17917=EDGE_LOOP('',(#86183,#86184,#86185,#86186));
#17918=EDGE_LOOP('',(#86187,#86188,#86189,#86190));
#17919=EDGE_LOOP('',(#86191,#86192,#86193,#86194));
#17920=EDGE_LOOP('',(#86195,#86196,#86197,#86198));
#17921=EDGE_LOOP('',(#86199,#86200,#86201,#86202));
#17922=EDGE_LOOP('',(#86203,#86204,#86205,#86206));
#17923=EDGE_LOOP('',(#86207,#86208,#86209,#86210));
#17924=EDGE_LOOP('',(#86211,#86212,#86213,#86214));
#17925=EDGE_LOOP('',(#86215,#86216,#86217,#86218));
#17926=EDGE_LOOP('',(#86219,#86220,#86221,#86222));
#17927=EDGE_LOOP('',(#86223,#86224,#86225,#86226));
#17928=EDGE_LOOP('',(#86227,#86228,#86229,#86230));
#17929=EDGE_LOOP('',(#86231,#86232,#86233,#86234));
#17930=EDGE_LOOP('',(#86235,#86236,#86237,#86238));
#17931=EDGE_LOOP('',(#86239,#86240,#86241,#86242));
#17932=EDGE_LOOP('',(#86243,#86244,#86245,#86246));
#17933=EDGE_LOOP('',(#86247));
#17934=EDGE_LOOP('',(#86248));
#17935=EDGE_LOOP('',(#86249));
#17936=EDGE_LOOP('',(#86250));
#17937=EDGE_LOOP('',(#86251));
#17938=EDGE_LOOP('',(#86252));
#17939=EDGE_LOOP('',(#86253));
#17940=EDGE_LOOP('',(#86254));
#17941=EDGE_LOOP('',(#86255));
#17942=EDGE_LOOP('',(#86256));
#17943=EDGE_LOOP('',(#86257));
#17944=EDGE_LOOP('',(#86258));
#17945=EDGE_LOOP('',(#86259));
#17946=EDGE_LOOP('',(#86260));
#17947=EDGE_LOOP('',(#86261));
#17948=EDGE_LOOP('',(#86262));
#17949=EDGE_LOOP('',(#86263));
#17950=EDGE_LOOP('',(#86264));
#17951=EDGE_LOOP('',(#86265));
#17952=EDGE_LOOP('',(#86266));
#17953=EDGE_LOOP('',(#86267));
#17954=EDGE_LOOP('',(#86268));
#17955=EDGE_LOOP('',(#86269));
#17956=EDGE_LOOP('',(#86270));
#17957=EDGE_LOOP('',(#86271));
#17958=EDGE_LOOP('',(#86272));
#17959=EDGE_LOOP('',(#86273));
#17960=EDGE_LOOP('',(#86274));
#17961=EDGE_LOOP('',(#86275));
#17962=EDGE_LOOP('',(#86276));
#17963=EDGE_LOOP('',(#86277));
#17964=EDGE_LOOP('',(#86278));
#17965=EDGE_LOOP('',(#86279));
#17966=EDGE_LOOP('',(#86280));
#17967=EDGE_LOOP('',(#86281));
#17968=EDGE_LOOP('',(#86282));
#17969=EDGE_LOOP('',(#86283));
#17970=EDGE_LOOP('',(#86284));
#17971=EDGE_LOOP('',(#86285));
#17972=EDGE_LOOP('',(#86286));
#17973=EDGE_LOOP('',(#86287,#86288,#86289,#86290));
#17974=EDGE_LOOP('',(#86291,#86292,#86293,#86294,#86295,#86296,#86297,#86298,
#86299,#86300,#86301,#86302,#86303,#86304,#86305,#86306,#86307,#86308,#86309,
#86310));
#17975=EDGE_LOOP('',(#86311,#86312,#86313,#86314,#86315,#86316,#86317,#86318,
#86319,#86320,#86321,#86322,#86323,#86324,#86325,#86326,#86327,#86328,#86329));
#17976=EDGE_LOOP('',(#86330,#86331,#86332,#86333));
#17977=EDGE_LOOP('',(#86334,#86335,#86336,#86337));
#17978=EDGE_LOOP('',(#86338,#86339,#86340,#86341,#86342,#86343,#86344,#86345,
#86346,#86347,#86348,#86349,#86350,#86351,#86352,#86353,#86354,#86355,#86356,
#86357));
#17979=EDGE_LOOP('',(#86358,#86359,#86360,#86361,#86362,#86363,#86364,#86365,
#86366,#86367,#86368,#86369,#86370,#86371,#86372,#86373,#86374,#86375,#86376));
#17980=EDGE_LOOP('',(#86377,#86378,#86379,#86380));
#17981=EDGE_LOOP('',(#86381,#86382,#86383,#86384));
#17982=EDGE_LOOP('',(#86385,#86386,#86387,#86388,#86389,#86390,#86391,#86392,
#86393,#86394,#86395,#86396,#86397,#86398,#86399,#86400,#86401,#86402,#86403,
#86404));
#17983=EDGE_LOOP('',(#86405,#86406,#86407,#86408,#86409,#86410,#86411,#86412,
#86413,#86414,#86415,#86416,#86417,#86418,#86419,#86420,#86421,#86422,#86423));
#17984=EDGE_LOOP('',(#86424,#86425,#86426,#86427));
#17985=EDGE_LOOP('',(#86428,#86429,#86430,#86431));
#17986=EDGE_LOOP('',(#86432,#86433,#86434,#86435));
#17987=EDGE_LOOP('',(#86436,#86437,#86438,#86439));
#17988=EDGE_LOOP('',(#86440,#86441,#86442,#86443));
#17989=EDGE_LOOP('',(#86444,#86445,#86446,#86447));
#17990=EDGE_LOOP('',(#86448,#86449,#86450,#86451));
#17991=EDGE_LOOP('',(#86452,#86453,#86454,#86455));
#17992=EDGE_LOOP('',(#86456,#86457,#86458,#86459));
#17993=EDGE_LOOP('',(#86460,#86461,#86462,#86463));
#17994=EDGE_LOOP('',(#86464,#86465,#86466,#86467));
#17995=EDGE_LOOP('',(#86468,#86469,#86470));
#17996=EDGE_LOOP('',(#86471,#86472,#86473,#86474,#86475));
#17997=EDGE_LOOP('',(#86476,#86477,#86478,#86479));
#17998=EDGE_LOOP('',(#86480,#86481,#86482,#86483));
#17999=EDGE_LOOP('',(#86484,#86485,#86486,#86487));
#18000=EDGE_LOOP('',(#86488,#86489,#86490,#86491));
#18001=EDGE_LOOP('',(#86492,#86493,#86494,#86495));
#18002=EDGE_LOOP('',(#86496,#86497,#86498,#86499));
#18003=EDGE_LOOP('',(#86500,#86501,#86502,#86503));
#18004=EDGE_LOOP('',(#86504,#86505,#86506,#86507));
#18005=EDGE_LOOP('',(#86508,#86509,#86510,#86511));
#18006=EDGE_LOOP('',(#86512,#86513,#86514,#86515));
#18007=EDGE_LOOP('',(#86516,#86517,#86518,#86519));
#18008=EDGE_LOOP('',(#86520,#86521,#86522,#86523));
#18009=EDGE_LOOP('',(#86524,#86525,#86526,#86527));
#18010=EDGE_LOOP('',(#86528,#86529,#86530,#86531));
#18011=EDGE_LOOP('',(#86532,#86533,#86534,#86535));
#18012=EDGE_LOOP('',(#86536,#86537,#86538,#86539));
#18013=EDGE_LOOP('',(#86540,#86541,#86542,#86543));
#18014=EDGE_LOOP('',(#86544,#86545,#86546,#86547));
#18015=EDGE_LOOP('',(#86548,#86549,#86550,#86551,#86552,#86553,#86554,#86555,
#86556,#86557,#86558,#86559,#86560,#86561));
#18016=EDGE_LOOP('',(#86562,#86563,#86564,#86565));
#18017=EDGE_LOOP('',(#86566,#86567,#86568,#86569,#86570,#86571,#86572,#86573,
#86574,#86575,#86576,#86577,#86578,#86579));
#18018=EDGE_LOOP('',(#86580,#86581,#86582,#86583));
#18019=EDGE_LOOP('',(#86584));
#18020=EDGE_LOOP('',(#86585,#86586,#86587,#86588));
#18021=EDGE_LOOP('',(#86589,#86590,#86591,#86592,#86593,#86594));
#18022=EDGE_LOOP('',(#86595,#86596,#86597,#86598,#86599,#86600,#86601,#86602,
#86603,#86604,#86605,#86606,#86607,#86608,#86609,#86610,#86611,#86612,#86613,
#86614,#86615,#86616,#86617,#86618));
#18023=EDGE_LOOP('',(#86619,#86620,#86621,#86622));
#18024=EDGE_LOOP('',(#86623,#86624,#86625,#86626,#86627,#86628,#86629,#86630,
#86631,#86632,#86633,#86634,#86635,#86636,#86637,#86638,#86639,#86640,#86641,
#86642,#86643,#86644,#86645,#86646,#86647));
#18025=EDGE_LOOP('',(#86648,#86649,#86650,#86651,#86652));
#18026=EDGE_LOOP('',(#86653,#86654,#86655,#86656));
#18027=EDGE_LOOP('',(#86657,#86658,#86659,#86660));
#18028=EDGE_LOOP('',(#86661,#86662,#86663,#86664,#86665,#86666,#86667));
#18029=EDGE_LOOP('',(#86668,#86669,#86670,#86671));
#18030=EDGE_LOOP('',(#86672,#86673,#86674,#86675));
#18031=EDGE_LOOP('',(#86676,#86677,#86678,#86679));
#18032=EDGE_LOOP('',(#86680));
#18033=EDGE_LOOP('',(#86681));
#18034=EDGE_LOOP('',(#86682,#86683,#86684,#86685));
#18035=EDGE_LOOP('',(#86686,#86687,#86688,#86689));
#18036=EDGE_LOOP('',(#86690));
#18037=EDGE_LOOP('',(#86691,#86692,#86693,#86694));
#18038=EDGE_LOOP('',(#86695));
#18039=EDGE_LOOP('',(#86696));
#18040=EDGE_LOOP('',(#86697));
#18041=EDGE_LOOP('',(#86698,#86699,#86700,#86701));
#18042=EDGE_LOOP('',(#86702,#86703,#86704,#86705));
#18043=EDGE_LOOP('',(#86706));
#18044=EDGE_LOOP('',(#86707));
#18045=EDGE_LOOP('',(#86708,#86709,#86710,#86711));
#18046=EDGE_LOOP('',(#86712,#86713,#86714,#86715));
#18047=EDGE_LOOP('',(#86716,#86717,#86718,#86719));
#18048=EDGE_LOOP('',(#86720,#86721,#86722,#86723));
#18049=EDGE_LOOP('',(#86724,#86725,#86726,#86727));
#18050=EDGE_LOOP('',(#86728,#86729,#86730,#86731));
#18051=EDGE_LOOP('',(#86732,#86733,#86734,#86735));
#18052=EDGE_LOOP('',(#86736,#86737,#86738,#86739));
#18053=EDGE_LOOP('',(#86740,#86741,#86742,#86743));
#18054=EDGE_LOOP('',(#86744,#86745,#86746,#86747));
#18055=EDGE_LOOP('',(#86748,#86749,#86750,#86751));
#18056=EDGE_LOOP('',(#86752,#86753,#86754,#86755));
#18057=EDGE_LOOP('',(#86756,#86757,#86758,#86759,#86760,#86761,#86762,#86763,
#86764,#86765,#86766,#86767,#86768,#86769,#86770,#86771,#86772));
#18058=EDGE_LOOP('',(#86773,#86774,#86775,#86776));
#18059=EDGE_LOOP('',(#86777,#86778,#86779,#86780));
#18060=EDGE_LOOP('',(#86781,#86782,#86783,#86784,#86785,#86786,#86787,#86788,
#86789,#86790,#86791,#86792,#86793,#86794,#86795,#86796,#86797));
#18061=EDGE_LOOP('',(#86798,#86799,#86800,#86801,#86802));
#18062=EDGE_LOOP('',(#86803,#86804,#86805,#86806));
#18063=EDGE_LOOP('',(#86807));
#18064=EDGE_LOOP('',(#86808,#86809,#86810,#86811));
#18065=EDGE_LOOP('',(#86812,#86813,#86814,#86815,#86816));
#18066=EDGE_LOOP('',(#86817,#86818,#86819,#86820));
#18067=EDGE_LOOP('',(#86821,#86822,#86823,#86824));
#18068=EDGE_LOOP('',(#86825,#86826,#86827,#86828));
#18069=EDGE_LOOP('',(#86829,#86830,#86831,#86832,#86833,#86834));
#18070=EDGE_LOOP('',(#86835,#86836,#86837,#86838,#86839));
#18071=EDGE_LOOP('',(#86840,#86841,#86842,#86843,#86844,#86845));
#18072=EDGE_LOOP('',(#86846,#86847,#86848,#86849));
#18073=EDGE_LOOP('',(#86850,#86851,#86852,#86853,#86854,#86855));
#18074=EDGE_LOOP('',(#86856));
#18075=EDGE_LOOP('',(#86857,#86858,#86859,#86860,#86861,#86862));
#18076=EDGE_LOOP('',(#86863));
#18077=EDGE_LOOP('',(#86864,#86865,#86866,#86867));
#18078=EDGE_LOOP('',(#86868,#86869,#86870,#86871));
#18079=EDGE_LOOP('',(#86872,#86873,#86874,#86875));
#18080=EDGE_LOOP('',(#86876,#86877,#86878,#86879));
#18081=EDGE_LOOP('',(#86880,#86881,#86882,#86883));
#18082=EDGE_LOOP('',(#86884,#86885,#86886,#86887));
#18083=EDGE_LOOP('',(#86888));
#18084=EDGE_LOOP('',(#86889));
#18085=EDGE_LOOP('',(#86890,#86891,#86892,#86893));
#18086=EDGE_LOOP('',(#86894,#86895,#86896,#86897));
#18087=EDGE_LOOP('',(#86898,#86899,#86900,#86901));
#18088=EDGE_LOOP('',(#86902,#86903,#86904,#86905));
#18089=EDGE_LOOP('',(#86906,#86907,#86908,#86909));
#18090=EDGE_LOOP('',(#86910,#86911,#86912,#86913));
#18091=EDGE_LOOP('',(#86914,#86915,#86916,#86917));
#18092=EDGE_LOOP('',(#86918,#86919,#86920,#86921));
#18093=EDGE_LOOP('',(#86922,#86923,#86924,#86925,#86926,#86927,#86928,#86929));
#18094=EDGE_LOOP('',(#86930));
#18095=EDGE_LOOP('',(#86931));
#18096=EDGE_LOOP('',(#86932,#86933,#86934,#86935));
#18097=EDGE_LOOP('',(#86936,#86937,#86938,#86939,#86940,#86941,#86942,#86943));
#18098=EDGE_LOOP('',(#86944,#86945,#86946,#86947));
#18099=EDGE_LOOP('',(#86948));
#18100=EDGE_LOOP('',(#86949));
#18101=EDGE_LOOP('',(#86950,#86951,#86952,#86953));
#18102=EDGE_LOOP('',(#86954));
#18103=EDGE_LOOP('',(#86955));
#18104=EDGE_LOOP('',(#86956,#86957,#86958,#86959,#86960,#86961));
#18105=EDGE_LOOP('',(#86962));
#18106=EDGE_LOOP('',(#86963,#86964,#86965,#86966,#86967,#86968));
#18107=EDGE_LOOP('',(#86969));
#18108=EDGE_LOOP('',(#86970));
#18109=EDGE_LOOP('',(#86971));
#18110=EDGE_LOOP('',(#86972,#86973,#86974,#86975));
#18111=EDGE_LOOP('',(#86976,#86977,#86978,#86979));
#18112=EDGE_LOOP('',(#86980,#86981,#86982));
#18113=EDGE_LOOP('',(#86983,#86984,#86985));
#18114=EDGE_LOOP('',(#86986,#86987,#86988,#86989));
#18115=EDGE_LOOP('',(#86990,#86991,#86992,#86993));
#18116=EDGE_LOOP('',(#86994,#86995,#86996,#86997));
#18117=EDGE_LOOP('',(#86998,#86999,#87000,#87001));
#18118=EDGE_LOOP('',(#87002,#87003,#87004,#87005));
#18119=EDGE_LOOP('',(#87006,#87007,#87008,#87009));
#18120=EDGE_LOOP('',(#87010,#87011,#87012,#87013));
#18121=EDGE_LOOP('',(#87014,#87015,#87016));
#18122=EDGE_LOOP('',(#87017,#87018,#87019));
#18123=EDGE_LOOP('',(#87020,#87021,#87022));
#18124=EDGE_LOOP('',(#87023,#87024,#87025));
#18125=EDGE_LOOP('',(#87026,#87027,#87028,#87029));
#18126=EDGE_LOOP('',(#87030,#87031,#87032,#87033));
#18127=EDGE_LOOP('',(#87034,#87035,#87036,#87037));
#18128=EDGE_LOOP('',(#87038,#87039,#87040,#87041));
#18129=EDGE_LOOP('',(#87042,#87043,#87044));
#18130=EDGE_LOOP('',(#87045,#87046,#87047));
#18131=EDGE_LOOP('',(#87048,#87049,#87050,#87051));
#18132=CIRCLE('',#94908,1.2645);
#18133=CIRCLE('',#94912,1.2645);
#18134=CIRCLE('',#94914,1.2645);
#18135=CIRCLE('',#94918,1.2645);
#18136=CIRCLE('',#94920,1.543);
#18137=CIRCLE('',#94924,1.543);
#18138=CIRCLE('',#94926,1.543);
#18139=CIRCLE('',#94930,1.543);
#18140=CIRCLE('',#94936,1.1);
#18141=CIRCLE('',#94937,3.40000000056584);
#18142=CIRCLE('',#94938,1.1);
#18143=CIRCLE('',#94939,18.25);
#18144=CIRCLE('',#94941,1.1);
#18145=CIRCLE('',#94942,3.39999999943896);
#18146=CIRCLE('',#94943,1.1);
#18147=CIRCLE('',#94944,18.25);
#18148=CIRCLE('',#94945,18.25);
#18149=CIRCLE('',#94947,8.);
#18150=CIRCLE('',#94948,7.9);
#18151=CIRCLE('',#94950,8.);
#18152=CIRCLE('',#94952,1.5);
#18153=CIRCLE('',#94954,18.25);
#18154=CIRCLE('',#94955,18.15);
#18155=CIRCLE('',#94956,18.25);
#18156=CIRCLE('',#94958,18.25);
#18157=CIRCLE('',#94959,18.25);
#18158=CIRCLE('',#94961,17.5);
#18159=CIRCLE('',#94963,18.25);
#18160=CIRCLE('',#94964,18.15);
#18161=CIRCLE('',#94965,18.25);
#18162=CIRCLE('',#94967,18.25);
#18163=CIRCLE('',#94969,17.5);
#18164=CIRCLE('',#94971,2.5);
#18165=CIRCLE('',#94972,2.6);
#18166=CIRCLE('',#94974,18.15);
#18167=CIRCLE('',#94976,2.5);
#18168=CIRCLE('',#94979,1.);
#18169=CIRCLE('',#94982,3.50000000056584);
#18170=CIRCLE('',#94985,1.);
#18171=CIRCLE('',#94987,1.);
#18172=CIRCLE('',#94990,3.49999999943895);
#18173=CIRCLE('',#94993,1.);
#18174=CIRCLE('',#94996,3.49999999943895);
#18175=CIRCLE('',#94997,3.39999999943896);
#18176=CIRCLE('',#95000,1.);
#18177=CIRCLE('',#95001,1.1);
#18178=CIRCLE('',#95003,18.15);
#18179=CIRCLE('',#95005,1.);
#18180=CIRCLE('',#95006,1.1);
#18181=CIRCLE('',#95009,3.50000000056584);
#18182=CIRCLE('',#95010,3.40000000056584);
#18183=CIRCLE('',#95013,1.);
#18184=CIRCLE('',#95014,1.1);
#18185=CIRCLE('',#95016,18.15);
#18186=CIRCLE('',#95018,1.);
#18187=CIRCLE('',#95019,1.1);
#18188=CIRCLE('',#95030,1.);
#18189=CIRCLE('',#95031,1.3);
#18190=CIRCLE('',#95033,1.);
#18191=CIRCLE('',#95035,1.875);
#18192=CIRCLE('',#95036,3.);
#18193=CIRCLE('',#95037,1.875);
#18194=CIRCLE('',#95038,3.);
#18195=CIRCLE('',#95039,1.875);
#18196=CIRCLE('',#95040,3.);
#18197=CIRCLE('',#95041,1.875);
#18198=CIRCLE('',#95042,3.);
#18199=CIRCLE('',#95043,1.875);
#18200=CIRCLE('',#95044,3.);
#18201=CIRCLE('',#95045,1.875);
#18202=CIRCLE('',#95046,3.);
#18203=CIRCLE('',#95047,1.875);
#18204=CIRCLE('',#95048,3.);
#18205=CIRCLE('',#95049,1.875);
#18206=CIRCLE('',#95050,3.);
#18207=CIRCLE('',#95051,1.875);
#18208=CIRCLE('',#95052,3.);
#18209=CIRCLE('',#95053,1.875);
#18210=CIRCLE('',#95054,3.);
#18211=CIRCLE('',#95057,1.875);
#18212=CIRCLE('',#95058,3.);
#18213=CIRCLE('',#95059,1.875);
#18214=CIRCLE('',#95060,3.);
#18215=CIRCLE('',#95061,1.875);
#18216=CIRCLE('',#95062,3.);
#18217=CIRCLE('',#95063,1.875);
#18218=CIRCLE('',#95064,3.);
#18219=CIRCLE('',#95065,1.875);
#18220=CIRCLE('',#95066,3.);
#18221=CIRCLE('',#95067,1.875);
#18222=CIRCLE('',#95068,3.);
#18223=CIRCLE('',#95069,1.875);
#18224=CIRCLE('',#95070,3.);
#18225=CIRCLE('',#95071,1.875);
#18226=CIRCLE('',#95072,3.);
#18227=CIRCLE('',#95073,1.875);
#18228=CIRCLE('',#95074,3.);
#18229=CIRCLE('',#95075,1.875);
#18230=CIRCLE('',#95076,3.);
#18231=CIRCLE('',#95077,1.5);
#18232=CIRCLE('',#95119,17.5);
#18233=CIRCLE('',#95120,17.4);
#18234=CIRCLE('',#95121,17.5);
#18235=CIRCLE('',#95123,17.5);
#18236=CIRCLE('',#95124,17.5);
#18237=CIRCLE('',#95126,17.5);
#18238=CIRCLE('',#95127,17.5);
#18239=CIRCLE('',#95130,17.5);
#18240=CIRCLE('',#95131,17.4);
#18241=CIRCLE('',#95132,17.5);
#18242=CIRCLE('',#95135,17.5);
#18243=CIRCLE('',#95136,17.5);
#18244=CIRCLE('',#95138,17.5);
#18245=CIRCLE('',#95139,17.4);
#18246=CIRCLE('',#95140,17.5);
#18247=CIRCLE('',#95143,17.5);
#18248=CIRCLE('',#95144,17.5);
#18249=CIRCLE('',#95146,17.5);
#18250=CIRCLE('',#95147,17.4);
#18251=CIRCLE('',#95148,17.5);
#18252=CIRCLE('',#95151,17.5);
#18253=CIRCLE('',#95152,17.5);
#18254=CIRCLE('',#95154,17.5);
#18255=CIRCLE('',#95155,17.4);
#18256=CIRCLE('',#95156,17.5);
#18257=CIRCLE('',#95159,17.5);
#18258=CIRCLE('',#95160,17.5);
#18259=CIRCLE('',#95162,17.5);
#18260=CIRCLE('',#95163,17.4);
#18261=CIRCLE('',#95164,17.5);
#18262=CIRCLE('',#95167,17.5);
#18263=CIRCLE('',#95168,17.5);
#18264=CIRCLE('',#95170,17.5);
#18265=CIRCLE('',#95171,17.4);
#18266=CIRCLE('',#95172,17.5);
#18267=CIRCLE('',#95175,17.5);
#18268=CIRCLE('',#95176,17.5);
#18269=CIRCLE('',#95178,17.5);
#18270=CIRCLE('',#95179,17.4);
#18271=CIRCLE('',#95180,17.5);
#18272=CIRCLE('',#95183,17.5);
#18273=CIRCLE('',#95184,17.5);
#18274=CIRCLE('',#95186,17.5);
#18275=CIRCLE('',#95187,17.4);
#18276=CIRCLE('',#95188,17.5);
#18277=CIRCLE('',#95191,17.5);
#18278=CIRCLE('',#95192,17.5);
#18279=CIRCLE('',#95194,17.5);
#18280=CIRCLE('',#95195,17.4);
#18281=CIRCLE('',#95196,17.5);
#18282=CIRCLE('',#95199,17.5);
#18283=CIRCLE('',#95200,17.5);
#18284=CIRCLE('',#95202,17.5);
#18285=CIRCLE('',#95203,17.4);
#18286=CIRCLE('',#95204,17.5);
#18287=CIRCLE('',#95207,17.5);
#18288=CIRCLE('',#95208,17.5);
#18289=CIRCLE('',#95210,17.5);
#18290=CIRCLE('',#95211,17.4);
#18291=CIRCLE('',#95212,17.5);
#18292=CIRCLE('',#95215,17.5);
#18293=CIRCLE('',#95216,17.5);
#18294=CIRCLE('',#95218,17.5);
#18295=CIRCLE('',#95219,17.4);
#18296=CIRCLE('',#95220,17.5);
#18297=CIRCLE('',#95223,17.5);
#18298=CIRCLE('',#95224,17.5);
#18299=CIRCLE('',#95226,17.5);
#18300=CIRCLE('',#95227,17.4);
#18301=CIRCLE('',#95228,17.5);
#18302=CIRCLE('',#95232,17.5);
#18303=CIRCLE('',#95233,17.5);
#18304=CIRCLE('',#95235,17.5);
#18305=CIRCLE('',#95236,17.5);
#18306=CIRCLE('',#95237,17.4);
#18307=CIRCLE('',#95245,3.5);
#18308=CIRCLE('',#95246,2.);
#18309=CIRCLE('',#95248,2.);
#18310=CIRCLE('',#95249,3.5);
#18311=CIRCLE('',#95251,2.);
#18312=CIRCLE('',#95252,3.5);
#18313=CIRCLE('',#95254,4.);
#18314=CIRCLE('',#95256,4.);
#18315=CIRCLE('',#95258,4.);
#18316=CIRCLE('',#95260,3.49999999999999);
#18317=CIRCLE('',#95262,3.49999999999999);
#18318=CIRCLE('',#95264,3.49999999999999);
#18319=CIRCLE('',#95266,3.);
#18320=CIRCLE('',#95268,3.);
#18321=CIRCLE('',#95270,3.);
#18322=CIRCLE('',#95272,2.);
#18323=CIRCLE('',#95273,2.);
#18324=CIRCLE('',#95274,2.);
#18325=CIRCLE('',#95275,2.);
#18326=CIRCLE('',#95276,2.);
#18327=CIRCLE('',#95277,2.);
#18328=CIRCLE('',#95278,2.);
#18329=CIRCLE('',#95280,3.5);
#18330=CIRCLE('',#95282,4.);
#18331=CIRCLE('',#95284,3.49999999999999);
#18332=CIRCLE('',#95286,3.);
#18333=CIRCLE('',#95288,3.);
#18334=CIRCLE('',#95289,3.);
#18335=CIRCLE('',#95290,3.);
#18336=CIRCLE('',#95291,3.);
#18337=CIRCLE('',#95292,3.);
#18338=CIRCLE('',#95293,3.);
#18339=CIRCLE('',#95295,5.);
#18340=CIRCLE('',#95297,5.);
#18341=CIRCLE('',#95312,0.4);
#18342=CIRCLE('',#95313,0.4);
#18343=CIRCLE('',#95316,2.9);
#18344=CIRCLE('',#95317,0.4);
#18345=CIRCLE('',#95318,0.4);
#18346=CIRCLE('',#95319,4.75);
#18347=CIRCLE('',#95320,4.75);
#18348=CIRCLE('',#95321,0.4);
#18349=CIRCLE('',#95323,0.4);
#18350=CIRCLE('',#95325,4.75);
#18351=CIRCLE('',#95327,0.4);
#18352=CIRCLE('',#95329,2.9);
#18353=CIRCLE('',#95331,0.4);
#18354=CIRCLE('',#95333,4.75);
#18355=CIRCLE('',#95343,0.4);
#18356=CIRCLE('',#95344,0.4);
#18357=CIRCLE('',#95345,0.4);
#18358=CIRCLE('',#95346,0.8);
#18359=CIRCLE('',#95347,0.4);
#18360=CIRCLE('',#95349,0.4);
#18361=CIRCLE('',#95350,4.65);
#18362=CIRCLE('',#95351,5.05);
#18363=CIRCLE('',#95352,0.400000000000001);
#18364=CIRCLE('',#95353,0.8);
#18365=CIRCLE('',#95354,0.4);
#18366=CIRCLE('',#95356,0.400000000000002);
#18367=CIRCLE('',#95357,10.0999999997296);
#18368=CIRCLE('',#95358,10.4999999997296);
#18369=CIRCLE('',#95359,0.4);
#18370=CIRCLE('',#95360,0.8);
#18371=CIRCLE('',#95361,0.4);
#18372=CIRCLE('',#95363,0.4);
#18373=CIRCLE('',#95364,12.);
#18374=CIRCLE('',#95365,11.6);
#18375=CIRCLE('',#95366,0.4);
#18376=CIRCLE('',#95367,0.8);
#18377=CIRCLE('',#95368,0.4);
#18378=CIRCLE('',#95370,0.4);
#18379=CIRCLE('',#95371,0.8);
#18380=CIRCLE('',#95372,0.4);
#18381=CIRCLE('',#95374,12.);
#18382=CIRCLE('',#95375,12.);
#18383=CIRCLE('',#95376,12.);
#18384=CIRCLE('',#95378,0.8);
#18385=CIRCLE('',#95381,0.8);
#18386=CIRCLE('',#95385,0.399999999999998);
#18387=CIRCLE('',#95386,0.400000000000001);
#18388=CIRCLE('',#95387,0.4);
#18389=CIRCLE('',#95388,0.6);
#18390=CIRCLE('',#95389,0.2);
#18391=CIRCLE('',#95391,0.4);
#18392=CIRCLE('',#95392,3.2);
#18393=CIRCLE('',#95393,3.6);
#18394=CIRCLE('',#95394,0.4);
#18395=CIRCLE('',#95395,0.8);
#18396=CIRCLE('',#95396,0.4);
#18397=CIRCLE('',#95398,0.4);
#18398=CIRCLE('',#95399,0.399999999999999);
#18399=CIRCLE('',#95400,0.8);
#18400=CIRCLE('',#95401,0.4);
#18401=CIRCLE('',#95403,0.4);
#18402=CIRCLE('',#95405,0.4);
#18403=CIRCLE('',#95406,0.8);
#18404=CIRCLE('',#95407,1.2);
#18405=CIRCLE('',#95409,0.4);
#18406=CIRCLE('',#95410,0.399999999999999);
#18407=CIRCLE('',#95411,0.8);
#18408=CIRCLE('',#95412,0.4);
#18409=CIRCLE('',#95414,0.399999999999999);
#18410=CIRCLE('',#95415,13.2);
#18411=CIRCLE('',#95416,13.6);
#18412=CIRCLE('',#95417,0.4);
#18413=CIRCLE('',#95418,0.6);
#18414=CIRCLE('',#95419,0.2);
#18415=CIRCLE('',#95421,0.4);
#18416=CIRCLE('',#95422,3.15);
#18417=CIRCLE('',#95423,3.15);
#18418=CIRCLE('',#95424,3.55);
#18419=CIRCLE('',#95425,0.8);
#18420=CIRCLE('',#95426,0.4);
#18421=CIRCLE('',#95429,0.8);
#18422=CIRCLE('',#95431,13.2);
#18423=CIRCLE('',#95433,0.6);
#18424=CIRCLE('',#95435,3.15);
#18425=CIRCLE('',#95436,3.15);
#18426=CIRCLE('',#95437,3.15);
#18427=CIRCLE('',#95438,3.15);
#18428=CIRCLE('',#95439,3.15);
#18429=CIRCLE('',#95440,3.15);
#18430=CIRCLE('',#95442,0.8);
#18431=CIRCLE('',#95446,0.4);
#18432=CIRCLE('',#95447,10.1000000149012);
#18433=CIRCLE('',#95448,0.4);
#18434=CIRCLE('',#95449,9.70000001490116);
#18435=CIRCLE('',#95450,0.4);
#18436=CIRCLE('',#95451,0.6);
#18437=CIRCLE('',#95452,0.2);
#18438=CIRCLE('',#95454,0.399999999999999);
#18439=CIRCLE('',#95455,0.399999999999999);
#18440=CIRCLE('',#95456,0.6);
#18441=CIRCLE('',#95457,0.2);
#18442=CIRCLE('',#95459,0.4);
#18443=CIRCLE('',#95460,0.4);
#18444=CIRCLE('',#95461,0.6);
#18445=CIRCLE('',#95462,0.2);
#18446=CIRCLE('',#95464,0.4);
#18447=CIRCLE('',#95465,3.2);
#18448=CIRCLE('',#95466,3.6);
#18449=CIRCLE('',#95467,0.400000000000001);
#18450=CIRCLE('',#95468,0.6);
#18451=CIRCLE('',#95469,0.2);
#18452=CIRCLE('',#95471,0.4);
#18453=CIRCLE('',#95472,0.4);
#18454=CIRCLE('',#95473,0.6);
#18455=CIRCLE('',#95474,0.2);
#18456=CIRCLE('',#95476,0.399999999999999);
#18457=CIRCLE('',#95477,3.55);
#18458=CIRCLE('',#95478,0.6);
#18459=CIRCLE('',#95479,0.2);
#18460=CIRCLE('',#95481,0.6);
#18461=CIRCLE('',#95482,0.6);
#18462=CIRCLE('',#95485,0.6);
#18463=CIRCLE('',#95487,0.6);
#18464=CIRCLE('',#95489,9.70000001490116);
#18465=CIRCLE('',#95492,0.400000000000001);
#18466=CIRCLE('',#95493,0.399999999999999);
#18467=CIRCLE('',#95494,0.399999999999999);
#18468=CIRCLE('',#95495,0.6);
#18469=CIRCLE('',#95496,0.2);
#18470=CIRCLE('',#95498,0.4);
#18471=CIRCLE('',#95499,9.70000001490116);
#18472=CIRCLE('',#95500,10.1000000149012);
#18473=CIRCLE('',#95501,0.4);
#18474=CIRCLE('',#95502,0.6);
#18475=CIRCLE('',#95503,0.2);
#18476=CIRCLE('',#95505,0.4);
#18477=CIRCLE('',#95506,3.7);
#18478=CIRCLE('',#95507,4.1);
#18479=CIRCLE('',#95509,0.399999999999999);
#18480=CIRCLE('',#95510,3.6);
#18481=CIRCLE('',#95511,3.2);
#18482=CIRCLE('',#95513,0.4);
#18483=CIRCLE('',#95515,0.399999999999999);
#18484=CIRCLE('',#95516,5.40000000000001);
#18485=CIRCLE('',#95517,5.80000000000001);
#18486=CIRCLE('',#95518,0.4);
#18487=CIRCLE('',#95519,0.6);
#18488=CIRCLE('',#95520,0.2);
#18489=CIRCLE('',#95522,0.4);
#18490=CIRCLE('',#95523,0.6);
#18491=CIRCLE('',#95524,0.2);
#18492=CIRCLE('',#95527,5.40000000000001);
#18493=CIRCLE('',#95529,0.6);
#18494=CIRCLE('',#95532,0.6);
#18495=CIRCLE('',#95536,0.4);
#18496=CIRCLE('',#95537,5.2);
#18497=CIRCLE('',#95538,0.4);
#18498=CIRCLE('',#95539,4.8);
#18499=CIRCLE('',#95540,0.4);
#18500=CIRCLE('',#95541,0.6);
#18501=CIRCLE('',#95542,0.2);
#18502=CIRCLE('',#95544,0.399999999999999);
#18503=CIRCLE('',#95545,5.4);
#18504=CIRCLE('',#95546,5.8);
#18505=CIRCLE('',#95548,0.4);
#18506=CIRCLE('',#95549,7.99496173936711);
#18507=CIRCLE('',#95550,7.59496173936711);
#18508=CIRCLE('',#95551,0.4);
#18509=CIRCLE('',#95552,0.8);
#18510=CIRCLE('',#95553,0.4);
#18511=CIRCLE('',#95555,0.4);
#18512=CIRCLE('',#95557,0.4);
#18513=CIRCLE('',#95558,0.8);
#18514=CIRCLE('',#95559,1.2);
#18515=CIRCLE('',#95561,0.4);
#18516=CIRCLE('',#95562,0.4);
#18517=CIRCLE('',#95563,0.8);
#18518=CIRCLE('',#95564,0.4);
#18519=CIRCLE('',#95566,0.4);
#18520=CIRCLE('',#95567,0.4);
#18521=CIRCLE('',#95568,0.6);
#18522=CIRCLE('',#95569,0.2);
#18523=CIRCLE('',#95571,0.4);
#18524=CIRCLE('',#95572,3.1);
#18525=CIRCLE('',#95573,3.5);
#18526=CIRCLE('',#95574,0.400000000000001);
#18527=CIRCLE('',#95575,0.800000000000001);
#18528=CIRCLE('',#95576,0.400000000000001);
#18529=CIRCLE('',#95579,0.8);
#18530=CIRCLE('',#95582,0.6);
#18531=CIRCLE('',#95584,3.1);
#18532=CIRCLE('',#95586,0.800000000000001);
#18533=CIRCLE('',#95589,4.8);
#18534=CIRCLE('',#95592,0.400000000000002);
#18535=CIRCLE('',#95593,9.79496173936711);
#18536=CIRCLE('',#95594,0.400000000000001);
#18537=CIRCLE('',#95595,9.3949617393671);
#18538=CIRCLE('',#95597,0.4);
#18539=CIRCLE('',#95598,4.);
#18540=CIRCLE('',#95599,3.6);
#18541=CIRCLE('',#95600,0.4);
#18542=CIRCLE('',#95601,0.6);
#18543=CIRCLE('',#95602,0.2);
#18544=CIRCLE('',#95604,0.4);
#18545=CIRCLE('',#95605,9.7);
#18546=CIRCLE('',#95606,10.1);
#18547=CIRCLE('',#95607,0.400000000000001);
#18548=CIRCLE('',#95608,0.6);
#18549=CIRCLE('',#95609,0.2);
#18550=CIRCLE('',#95611,0.400000000000001);
#18551=CIRCLE('',#95612,17.3949617393671);
#18552=CIRCLE('',#95613,16.9949617393671);
#18553=CIRCLE('',#95614,0.4);
#18554=CIRCLE('',#95615,0.8);
#18555=CIRCLE('',#95616,0.4);
#18556=CIRCLE('',#95618,0.4);
#18557=CIRCLE('',#95619,0.8);
#18558=CIRCLE('',#95620,0.4);
#18559=CIRCLE('',#95622,17.3949617393671);
#18560=CIRCLE('',#95624,0.8);
#18561=CIRCLE('',#95627,0.8);
#18562=CIRCLE('',#95629,9.3949617393671);
#18563=CIRCLE('',#95632,0.400000000000001);
#18564=CIRCLE('',#95633,4.);
#18565=CIRCLE('',#95634,0.4);
#18566=CIRCLE('',#95635,3.6);
#18567=CIRCLE('',#95636,0.400000000000003);
#18568=CIRCLE('',#95637,0.8);
#18569=CIRCLE('',#95638,0.4);
#18570=CIRCLE('',#95640,0.399999999999998);
#18571=CIRCLE('',#95641,23.7449617393671);
#18572=CIRCLE('',#95642,23.3449617393671);
#18573=CIRCLE('',#95644,0.400000000000003);
#18574=CIRCLE('',#95645,0.4);
#18575=CIRCLE('',#95646,0.8);
#18576=CIRCLE('',#95648,0.4);
#18577=CIRCLE('',#95649,7.8);
#18578=CIRCLE('',#95650,8.2);
#18579=CIRCLE('',#95651,0.399999999999998);
#18580=CIRCLE('',#95652,0.8);
#18581=CIRCLE('',#95653,0.4);
#18582=CIRCLE('',#95655,0.4);
#18583=CIRCLE('',#95656,0.4);
#18584=CIRCLE('',#95657,0.6);
#18585=CIRCLE('',#95658,0.2);
#18586=CIRCLE('',#95660,0.4);
#18587=CIRCLE('',#95661,0.4);
#18588=CIRCLE('',#95662,0.8);
#18589=CIRCLE('',#95663,0.4);
#18590=CIRCLE('',#95665,0.4);
#18591=CIRCLE('',#95666,0.4);
#18592=CIRCLE('',#95667,0.8);
#18593=CIRCLE('',#95668,0.4);
#18594=CIRCLE('',#95670,0.4);
#18595=CIRCLE('',#95671,18.9949617393671);
#18596=CIRCLE('',#95672,19.3949617393671);
#18597=CIRCLE('',#95673,0.399999999999999);
#18598=CIRCLE('',#95674,0.6);
#18599=CIRCLE('',#95675,0.2);
#18600=CIRCLE('',#95677,0.4);
#18601=CIRCLE('',#95678,9.7);
#18602=CIRCLE('',#95679,10.1);
#18603=CIRCLE('',#95680,0.6);
#18604=CIRCLE('',#95681,0.2);
#18605=CIRCLE('',#95683,0.8);
#18606=CIRCLE('',#95686,0.8);
#18607=CIRCLE('',#95688,18.9949617393671);
#18608=CIRCLE('',#95690,0.6);
#18609=CIRCLE('',#95692,9.7);
#18610=CIRCLE('',#95694,0.6);
#18611=CIRCLE('',#95696,3.6);
#18612=CIRCLE('',#95697,3.6);
#18613=CIRCLE('',#95700,0.4);
#18614=CIRCLE('',#95701,5.05);
#18615=CIRCLE('',#95702,0.4);
#18616=CIRCLE('',#95703,4.65);
#18617=CIRCLE('',#95704,0.399999999999998);
#18618=CIRCLE('',#95705,0.8);
#18619=CIRCLE('',#95706,0.4);
#18620=CIRCLE('',#95708,0.400000000000001);
#18621=CIRCLE('',#95709,13.4);
#18622=CIRCLE('',#95710,13.);
#18623=CIRCLE('',#95712,0.4);
#18624=CIRCLE('',#95713,0.4);
#18625=CIRCLE('',#95714,0.8);
#18626=CIRCLE('',#95715,0.4);
#18627=CIRCLE('',#95717,0.4);
#18628=CIRCLE('',#95718,12.);
#18629=CIRCLE('',#95719,11.6);
#18630=CIRCLE('',#95720,0.4);
#18631=CIRCLE('',#95721,0.8);
#18632=CIRCLE('',#95722,0.4);
#18633=CIRCLE('',#95724,0.400000000000002);
#18634=CIRCLE('',#95725,10.0999999997296);
#18635=CIRCLE('',#95726,10.4999999997296);
#18636=CIRCLE('',#95727,0.8);
#18637=CIRCLE('',#95728,0.4);
#18638=CIRCLE('',#95730,12.);
#18639=CIRCLE('',#95731,12.);
#18640=CIRCLE('',#95732,12.);
#18641=CIRCLE('',#95734,0.8);
#18642=CIRCLE('',#95736,10.0999999997296);
#18643=CIRCLE('',#95738,0.8);
#18644=CIRCLE('',#95740,4.65);
#18645=CIRCLE('',#95743,0.4);
#18646=CIRCLE('',#95744,0.4);
#18647=CIRCLE('',#95745,0.399999999999999);
#18648=CIRCLE('',#95746,0.6);
#18649=CIRCLE('',#95747,0.2);
#18650=CIRCLE('',#95749,0.4);
#18651=CIRCLE('',#95750,0.4);
#18652=CIRCLE('',#95751,0.6);
#18653=CIRCLE('',#95752,0.2);
#18654=CIRCLE('',#95754,0.399999999999999);
#18655=CIRCLE('',#95755,3.6);
#18656=CIRCLE('',#95756,4.);
#18657=CIRCLE('',#95757,0.4);
#18658=CIRCLE('',#95758,0.6);
#18659=CIRCLE('',#95759,0.2);
#18660=CIRCLE('',#95761,0.4);
#18661=CIRCLE('',#95762,13.2);
#18662=CIRCLE('',#95763,13.6);
#18663=CIRCLE('',#95764,0.6);
#18664=CIRCLE('',#95765,0.2);
#18665=CIRCLE('',#95767,0.6);
#18666=CIRCLE('',#95769,13.2);
#18667=CIRCLE('',#95771,0.6);
#18668=CIRCLE('',#95774,0.200000000000001);
#18669=CIRCLE('',#95775,0.2);
#18670=CIRCLE('',#95777,0.4);
#18671=CIRCLE('',#95779,8.5);
#18672=CIRCLE('',#95780,8.5);
#18673=CIRCLE('',#95781,8.5);
#18674=CIRCLE('',#95782,8.5);
#18675=CIRCLE('',#95783,8.5);
#18676=CIRCLE('',#95784,8.5);
#18677=CIRCLE('',#95785,8.5);
#18678=CIRCLE('',#95786,8.5);
#18679=CIRCLE('',#95789,0.4);
#18680=CIRCLE('',#95790,0.4);
#18681=CIRCLE('',#95792,0.8);
#18682=CIRCLE('',#95793,0.8);
#18683=CIRCLE('',#95794,0.6);
#18684=CIRCLE('',#95797,0.8);
#18685=CIRCLE('',#95798,0.8);
#18686=CIRCLE('',#95800,4.2);
#18687=CIRCLE('',#95801,0.4);
#18688=CIRCLE('',#95802,0.79999999999745);
#18689=CIRCLE('',#95803,0.6);
#18690=CIRCLE('',#95804,0.6);
#18691=CIRCLE('',#95805,3.2);
#18692=CIRCLE('',#95806,10.45);
#18693=CIRCLE('',#95807,3.43614417320658);
#18694=CIRCLE('',#95808,0.6);
#18695=CIRCLE('',#95809,3.2);
#18696=CIRCLE('',#95810,0.8);
#18697=CIRCLE('',#95811,0.8);
#18698=CIRCLE('',#95812,0.8);
#18699=CIRCLE('',#95813,3.60000000004514);
#18700=CIRCLE('',#95814,1.6);
#18701=CIRCLE('',#95816,4.2);
#18702=CIRCLE('',#95818,4.);
#18703=CIRCLE('',#95819,0.8);
#18704=CIRCLE('',#95820,0.8);
#18705=CIRCLE('',#95821,8.4949617393671);
#18706=CIRCLE('',#95822,4.9);
#18707=CIRCLE('',#95823,0.8);
#18708=CIRCLE('',#95824,0.6);
#18709=CIRCLE('',#95825,9.70000001490116);
#18710=CIRCLE('',#95826,0.6);
#18711=CIRCLE('',#95827,3.7);
#18712=CIRCLE('',#95828,3.6);
#18713=CIRCLE('',#95829,0.4);
#18714=CIRCLE('',#95830,0.8);
#18715=CIRCLE('',#95831,0.6);
#18716=CIRCLE('',#95832,5.4);
#18717=CIRCLE('',#95833,7.99496173936711);
#18718=CIRCLE('',#95834,0.8);
#18719=CIRCLE('',#95835,1.55);
#18720=CIRCLE('',#95838,0.8);
#18721=CIRCLE('',#95841,4.);
#18722=CIRCLE('',#95842,3.60000000004514);
#18723=CIRCLE('',#95843,0.8);
#18724=CIRCLE('',#95844,0.8);
#18725=CIRCLE('',#95845,0.8);
#18726=CIRCLE('',#95846,0.8);
#18727=CIRCLE('',#95847,1.58);
#18728=CIRCLE('',#95848,3.25);
#18729=CIRCLE('',#95849,3.25);
#18730=CIRCLE('',#95850,10.9);
#18731=CIRCLE('',#95851,0.8);
#18732=CIRCLE('',#95852,0.8);
#18733=CIRCLE('',#95853,0.8);
#18734=CIRCLE('',#95854,1.6);
#18735=CIRCLE('',#95855,1.6);
#18736=CIRCLE('',#95856,1.6);
#18737=CIRCLE('',#95857,1.55);
#18738=CIRCLE('',#95858,3.05);
#18739=CIRCLE('',#95862,0.8);
#18740=CIRCLE('',#95864,0.8);
#18741=CIRCLE('',#95867,1.);
#18742=CIRCLE('',#95868,2.);
#18743=CIRCLE('',#95869,7.8);
#18744=CIRCLE('',#95870,0.8);
#18745=CIRCLE('',#95871,0.6);
#18746=CIRCLE('',#95872,100.);
#18747=CIRCLE('',#95873,0.8);
#18748=CIRCLE('',#95874,18.2949617393671);
#18749=CIRCLE('',#95876,0.8);
#18750=CIRCLE('',#95879,0.8);
#18751=CIRCLE('',#95881,0.8);
#18752=CIRCLE('',#95882,4.65);
#18753=CIRCLE('',#95883,0.8);
#18754=CIRCLE('',#95884,10.0999999997296);
#18755=CIRCLE('',#95885,0.8);
#18756=CIRCLE('',#95886,3.75);
#18757=CIRCLE('',#95887,0.8);
#18758=CIRCLE('',#95888,13.4);
#18759=CIRCLE('',#95889,0.8);
#18760=CIRCLE('',#95890,0.4);
#18761=CIRCLE('',#95891,3.05);
#18762=CIRCLE('',#95903,0.6);
#18763=CIRCLE('',#95905,9.7);
#18764=CIRCLE('',#95907,0.6);
#18765=CIRCLE('',#95909,23.7449617393671);
#18766=CIRCLE('',#95911,0.4);
#18767=CIRCLE('',#95913,7.8);
#18768=CIRCLE('',#95919,17.3949617393671);
#18769=CIRCLE('',#95920,9.3949617393671);
#18770=CIRCLE('',#95934,17.3949617393671);
#18771=CIRCLE('',#95939,0.79999999999745);
#18772=CIRCLE('',#95940,0.6);
#18773=CIRCLE('',#95941,0.6);
#18774=CIRCLE('',#95946,1.55);
#18775=CIRCLE('',#95948,3.43614417320658);
#18776=CIRCLE('',#95950,10.45);
#18777=CIRCLE('',#95952,0.6);
#18778=CIRCLE('',#95955,100.);
#18779=CIRCLE('',#95957,0.8);
#18780=CIRCLE('',#95960,0.6);
#18781=CIRCLE('',#95962,3.6);
#18782=CIRCLE('',#95976,0.6);
#18783=CIRCLE('',#95982,0.8);
#18784=CIRCLE('',#95983,2.);
#18785=CIRCLE('',#95984,1.);
#18786=CIRCLE('',#95985,0.4);
#18787=CIRCLE('',#95986,3.75);
#18788=CIRCLE('',#95987,2.3);
#18789=CIRCLE('',#95989,4.);
#18790=CIRCLE('',#95990,4.);
#18791=CIRCLE('',#95999,1.6);
#18792=CIRCLE('',#96001,1.6);
#18793=CIRCLE('',#96003,2.);
#18794=CIRCLE('',#96006,3.25);
#18795=CIRCLE('',#96009,3.25);
#18796=CIRCLE('',#96011,1.6);
#18797=CIRCLE('',#96014,1.6);
#18798=CIRCLE('',#96017,1.55);
#18799=CIRCLE('',#96020,2.);
#18800=CIRCLE('',#96022,1.58);
#18801=CIRCLE('',#96024,2.);
#18802=CIRCLE('',#96027,10.9);
#18803=CIRCLE('',#96030,1.);
#18804=CIRCLE('',#96032,2.);
#18805=CIRCLE('',#96033,1.);
#18806=CIRCLE('',#96048,11.65);
#18807=CIRCLE('',#96049,6.4499999999938);
#18808=CIRCLE('',#96053,0.8);
#18809=CIRCLE('',#96054,0.8);
#18810=CIRCLE('',#96056,5.);
#18811=CIRCLE('',#96057,0.8);
#18812=CIRCLE('',#96058,0.8);
#18813=CIRCLE('',#96059,0.4);
#18814=CIRCLE('',#96060,10.6);
#18815=CIRCLE('',#96061,0.4);
#18816=CIRCLE('',#96062,0.8);
#18817=CIRCLE('',#96063,0.8);
#18818=CIRCLE('',#96064,0.4);
#18819=CIRCLE('',#96065,10.);
#18820=CIRCLE('',#96066,0.8);
#18821=CIRCLE('',#96068,5.);
#18822=CIRCLE('',#96070,0.8);
#18823=CIRCLE('',#96073,0.4);
#18824=CIRCLE('',#96074,5.05);
#18825=CIRCLE('',#96075,0.4);
#18826=CIRCLE('',#96076,4.65);
#18827=CIRCLE('',#96077,0.4);
#18828=CIRCLE('',#96078,0.8);
#18829=CIRCLE('',#96079,0.4);
#18830=CIRCLE('',#96081,0.4);
#18831=CIRCLE('',#96082,0.4);
#18832=CIRCLE('',#96083,0.8);
#18833=CIRCLE('',#96084,0.4);
#18834=CIRCLE('',#96086,0.4);
#18835=CIRCLE('',#96087,0.4);
#18836=CIRCLE('',#96088,0.8);
#18837=CIRCLE('',#96089,0.4);
#18838=CIRCLE('',#96091,0.399999999999996);
#18839=CIRCLE('',#96092,10.6);
#18840=CIRCLE('',#96093,11.);
#18841=CIRCLE('',#96094,0.6);
#18842=CIRCLE('',#96095,0.2);
#18843=CIRCLE('',#96097,0.8);
#18844=CIRCLE('',#96099,10.6);
#18845=CIRCLE('',#96101,0.6);
#18846=CIRCLE('',#96103,4.64999999999989);
#18847=CIRCLE('',#96104,4.64999999999989);
#18848=CIRCLE('',#96107,3.6);
#18849=CIRCLE('',#96108,0.4);
#18850=CIRCLE('',#96109,4.);
#18851=CIRCLE('',#96111,2.1);
#18852=CIRCLE('',#96112,0.4);
#18853=CIRCLE('',#96113,2.5);
#18854=CIRCLE('',#96115,0.4);
#18855=CIRCLE('',#96117,2.5);
#18856=CIRCLE('',#96118,2.1);
#18857=CIRCLE('',#96120,16.9949617393671);
#18858=CIRCLE('',#96121,0.4);
#18859=CIRCLE('',#96122,17.3949617393671);
#18860=CIRCLE('',#96124,4.);
#18861=CIRCLE('',#96125,3.6);
#18862=CIRCLE('',#96127,9.3949617393671);
#18863=CIRCLE('',#96128,9.79496173936711);
#18864=CIRCLE('',#96131,4.);
#18865=CIRCLE('',#96133,9.3949617393671);
#18866=CIRCLE('',#96136,17.3949617393671);
#18867=CIRCLE('',#96139,11.95);
#18868=CIRCLE('',#96140,0.399999999999996);
#18869=CIRCLE('',#96141,11.55);
#18870=CIRCLE('',#96142,0.4);
#18871=CIRCLE('',#96143,0.599999999999999);
#18872=CIRCLE('',#96144,0.199999999999999);
#18873=CIRCLE('',#96146,4.2);
#18874=CIRCLE('',#96147,3.8);
#18875=CIRCLE('',#96148,4.2);
#18876=CIRCLE('',#96150,11.55);
#18877=CIRCLE('',#96153,3.8);
#18878=CIRCLE('',#96154,3.8);
#18879=CIRCLE('',#96156,0.4);
#18880=CIRCLE('',#96158,0.2);
#18881=CIRCLE('',#96161,0.4);
#18882=CIRCLE('',#96162,0.4);
#18883=CIRCLE('',#96163,0.6);
#18884=CIRCLE('',#96166,0.4);
#18885=CIRCLE('',#96167,2.85);
#18886=CIRCLE('',#96168,1.65);
#18887=CIRCLE('',#96171,4.64877154610377);
#18888=CIRCLE('',#96179,4.2);
#18889=CIRCLE('',#96180,0.4);
#18890=CIRCLE('',#96181,3.8);
#18891=CIRCLE('',#96182,0.4);
#18892=CIRCLE('',#96183,0.6);
#18893=CIRCLE('',#96184,0.2);
#18894=CIRCLE('',#96186,0.400000000000005);
#18895=CIRCLE('',#96187,24.9449617393673);
#18896=CIRCLE('',#96188,25.3449617393673);
#18897=CIRCLE('',#96189,0.4);
#18898=CIRCLE('',#96190,0.6);
#18899=CIRCLE('',#96191,0.2);
#18900=CIRCLE('',#96196,3.6);
#18901=CIRCLE('',#96199,3.8);
#18902=CIRCLE('',#96202,3.69774423765867);
#18903=CIRCLE('',#96203,4.09750037145961);
#18904=CIRCLE('',#96204,0.4);
#18905=CIRCLE('',#96205,0.600000000000001);
#18906=CIRCLE('',#96207,0.4);
#18907=CIRCLE('',#96208,3.6);
#18908=CIRCLE('',#96210,4.1);
#18909=CIRCLE('',#96211,0.4);
#18910=CIRCLE('',#96212,3.7);
#18911=CIRCLE('',#96214,8.8);
#18912=CIRCLE('',#96215,0.2);
#18913=CIRCLE('',#96216,0.2);
#18914=CIRCLE('',#96217,0.2);
#18915=CIRCLE('',#96219,0.4);
#18916=CIRCLE('',#96220,0.4);
#18917=CIRCLE('',#96221,0.6);
#18918=CIRCLE('',#96223,0.4);
#18919=CIRCLE('',#96224,0.4);
#18920=CIRCLE('',#96225,0.6);
#18921=CIRCLE('',#96227,0.4);
#18922=CIRCLE('',#96228,0.4);
#18923=CIRCLE('',#96229,0.6);
#18924=CIRCLE('',#96231,9.2);
#18925=CIRCLE('',#96233,0.600000000000001);
#18926=CIRCLE('',#96235,3.6);
#18927=CIRCLE('',#96237,3.7);
#18928=CIRCLE('',#96240,0.6);
#18929=CIRCLE('',#96243,0.6);
#18930=CIRCLE('',#96246,0.6);
#18931=CIRCLE('',#96248,9.2);
#18932=CIRCLE('',#96249,9.2);
#18933=CIRCLE('',#96251,9.2);
#18934=CIRCLE('',#96254,0.399999999999999);
#18935=CIRCLE('',#96255,4.6);
#18936=CIRCLE('',#96256,0.399999999999996);
#18937=CIRCLE('',#96257,4.2);
#18938=CIRCLE('',#96258,0.4);
#18939=CIRCLE('',#96259,0.800000000000001);
#18940=CIRCLE('',#96260,0.400000000000001);
#18941=CIRCLE('',#96262,0.4);
#18942=CIRCLE('',#96264,0.4);
#18943=CIRCLE('',#96265,0.8);
#18944=CIRCLE('',#96266,1.2);
#18945=CIRCLE('',#96268,0.4);
#18946=CIRCLE('',#96269,0.4);
#18947=CIRCLE('',#96270,0.8);
#18948=CIRCLE('',#96271,0.4);
#18949=CIRCLE('',#96273,0.400000000000001);
#18950=CIRCLE('',#96274,6.1);
#18951=CIRCLE('',#96275,0.4);
#18952=CIRCLE('',#96276,5.7);
#18953=CIRCLE('',#96277,0.4);
#18954=CIRCLE('',#96278,0.6);
#18955=CIRCLE('',#96279,0.2);
#18956=CIRCLE('',#96281,0.4);
#18957=CIRCLE('',#96282,4.8);
#18958=CIRCLE('',#96283,5.2);
#18959=CIRCLE('',#96285,0.4);
#18960=CIRCLE('',#96287,7.69496173936711);
#18961=CIRCLE('',#96288,7.2949617393671);
#18962=CIRCLE('',#96290,0.399999999999999);
#18963=CIRCLE('',#96293,0.8);
#18964=CIRCLE('',#96296,0.8);
#18965=CIRCLE('',#96298,7.69496173936711);
#18966=CIRCLE('',#96300,5.7);
#18967=CIRCLE('',#96303,0.400000000000003);
#18968=CIRCLE('',#96304,0.4);
#18969=CIRCLE('',#96305,0.400000000000005);
#18970=CIRCLE('',#96306,0.6);
#18971=CIRCLE('',#96307,0.2);
#18972=CIRCLE('',#96309,0.4);
#18973=CIRCLE('',#96311,0.400000000000005);
#18974=CIRCLE('',#96312,4.1);
#18975=CIRCLE('',#96313,4.5);
#18976=CIRCLE('',#96314,0.400000000000005);
#18977=CIRCLE('',#96315,0.6);
#18978=CIRCLE('',#96316,0.2);
#18979=CIRCLE('',#96318,0.4);
#18980=CIRCLE('',#96320,0.4);
#18981=CIRCLE('',#96321,7.8);
#18982=CIRCLE('',#96322,8.2);
#18983=CIRCLE('',#96323,0.4);
#18984=CIRCLE('',#96324,0.6);
#18985=CIRCLE('',#96325,0.2);
#18986=CIRCLE('',#96327,0.399999999999996);
#18987=CIRCLE('',#96328,19.0949617393671);
#18988=CIRCLE('',#96329,19.4949617393671);
#18989=CIRCLE('',#96330,0.4);
#18990=CIRCLE('',#96331,0.8);
#18991=CIRCLE('',#96332,0.4);
#18992=CIRCLE('',#96334,0.4);
#18993=CIRCLE('',#96335,0.8);
#18994=CIRCLE('',#96336,0.4);
#18995=CIRCLE('',#96338,0.6);
#18996=CIRCLE('',#96340,19.0949617393671);
#18997=CIRCLE('',#96342,0.8);
#18998=CIRCLE('',#96345,0.8);
#18999=CIRCLE('',#96349,0.4);
#19000=CIRCLE('',#96350,0.4);
#19001=CIRCLE('',#96351,0.4);
#19002=CIRCLE('',#96352,0.6);
#19003=CIRCLE('',#96353,0.2);
#19004=CIRCLE('',#96355,0.4);
#19005=CIRCLE('',#96356,0.4);
#19006=CIRCLE('',#96357,0.6);
#19007=CIRCLE('',#96358,0.2);
#19008=CIRCLE('',#96360,0.4);
#19009=CIRCLE('',#96362,0.4);
#19010=CIRCLE('',#96363,3.7);
#19011=CIRCLE('',#96364,4.1);
#19012=CIRCLE('',#96366,0.4);
#19013=CIRCLE('',#96367,6.6);
#19014=CIRCLE('',#96368,6.2);
#19015=CIRCLE('',#96369,0.4);
#19016=CIRCLE('',#96370,0.6);
#19017=CIRCLE('',#96371,0.2);
#19018=CIRCLE('',#96373,0.4);
#19019=CIRCLE('',#96374,22.5949617393671);
#19020=CIRCLE('',#96375,22.1949617393671);
#19021=CIRCLE('',#96377,0.4);
#19022=CIRCLE('',#96378,9.2);
#19023=CIRCLE('',#96379,8.8);
#19024=CIRCLE('',#96380,0.6);
#19025=CIRCLE('',#96381,0.2);
#19026=CIRCLE('',#96383,6.6);
#19027=CIRCLE('',#96385,0.6);
#19028=CIRCLE('',#96387,22.5949617393671);
#19029=CIRCLE('',#96388,22.5949617393671);
#19030=CIRCLE('',#96390,9.2);
#19031=CIRCLE('',#96392,9.2);
#19032=CIRCLE('',#96394,0.6);
#19033=CIRCLE('',#96398,12.05);
#19034=CIRCLE('',#96399,0.400000000000005);
#19035=CIRCLE('',#96400,11.65);
#19036=CIRCLE('',#96401,0.4);
#19037=CIRCLE('',#96402,0.6);
#19038=CIRCLE('',#96403,0.2);
#19039=CIRCLE('',#96405,0.4);
#19040=CIRCLE('',#96406,3.2);
#19041=CIRCLE('',#96407,3.6);
#19042=CIRCLE('',#96408,0.4);
#19043=CIRCLE('',#96409,0.6);
#19044=CIRCLE('',#96410,0.2);
#19045=CIRCLE('',#96414,0.4);
#19046=CIRCLE('',#96416,0.6);
#19047=CIRCLE('',#96418,3.7);
#19048=CIRCLE('',#96419,3.6);
#19049=CIRCLE('',#96420,4.1);
#19050=CIRCLE('',#96424,11.65);
#19051=CIRCLE('',#96425,11.65);
#19052=CIRCLE('',#96427,0.399999999999998);
#19053=CIRCLE('',#96428,0.4);
#19054=CIRCLE('',#96430,0.4);
#19055=CIRCLE('',#96431,0.8);
#19056=CIRCLE('',#96432,1.2);
#19057=CIRCLE('',#96434,0.4);
#19058=CIRCLE('',#96435,0.4);
#19059=CIRCLE('',#96436,0.6);
#19060=CIRCLE('',#96437,0.2);
#19061=CIRCLE('',#96439,0.4);
#19062=CIRCLE('',#96440,9.2);
#19063=CIRCLE('',#96441,8.8);
#19064=CIRCLE('',#96442,0.4);
#19065=CIRCLE('',#96443,0.6);
#19066=CIRCLE('',#96444,0.2);
#19067=CIRCLE('',#96446,0.4);
#19068=CIRCLE('',#96447,0.4);
#19069=CIRCLE('',#96448,0.6);
#19070=CIRCLE('',#96449,0.2);
#19071=CIRCLE('',#96451,0.4);
#19072=CIRCLE('',#96452,3.5);
#19073=CIRCLE('',#96453,3.5);
#19074=CIRCLE('',#96454,3.9);
#19075=CIRCLE('',#96455,0.4);
#19076=CIRCLE('',#96456,0.6);
#19077=CIRCLE('',#96457,0.2);
#19078=CIRCLE('',#96459,0.4);
#19079=CIRCLE('',#96460,0.800000000000001);
#19080=CIRCLE('',#96461,0.400000000000001);
#19081=CIRCLE('',#96463,0.6);
#19082=CIRCLE('',#96465,3.5);
#19083=CIRCLE('',#96466,3.5);
#19084=CIRCLE('',#96467,3.5);
#19085=CIRCLE('',#96468,3.5);
#19086=CIRCLE('',#96469,3.5);
#19087=CIRCLE('',#96470,3.5);
#19088=CIRCLE('',#96472,0.6);
#19089=CIRCLE('',#96475,0.800000000000001);
#19090=CIRCLE('',#96479,8.8);
#19091=CIRCLE('',#96480,0.4);
#19092=CIRCLE('',#96481,9.2);
#19093=CIRCLE('',#96482,0.4);
#19094=CIRCLE('',#96483,0.6);
#19095=CIRCLE('',#96484,0.2);
#19096=CIRCLE('',#96486,0.4);
#19097=CIRCLE('',#96487,0.4);
#19098=CIRCLE('',#96488,0.6);
#19099=CIRCLE('',#96489,0.2);
#19100=CIRCLE('',#96491,0.4);
#19101=CIRCLE('',#96492,0.4);
#19102=CIRCLE('',#96493,0.6);
#19103=CIRCLE('',#96494,0.2);
#19104=CIRCLE('',#96496,0.4);
#19105=CIRCLE('',#96497,3.9);
#19106=CIRCLE('',#96498,0.4);
#19107=CIRCLE('',#96499,0.6);
#19108=CIRCLE('',#96500,0.2);
#19109=CIRCLE('',#96502,0.4);
#19110=CIRCLE('',#96503,0.4);
#19111=CIRCLE('',#96504,0.6);
#19112=CIRCLE('',#96505,0.2);
#19113=CIRCLE('',#96507,9.2);
#19114=CIRCLE('',#96508,8.8);
#19115=CIRCLE('',#96510,3.69774423765867);
#19116=CIRCLE('',#96511,4.0975003714596);
#19117=CIRCLE('',#96514,0.6);
#19118=CIRCLE('',#96517,9.2);
#19119=CIRCLE('',#96518,9.2);
#19120=CIRCLE('',#96522,9.2);
#19121=CIRCLE('',#96523,9.2);
#19122=CIRCLE('',#96526,0.4);
#19123=CIRCLE('',#96527,8.8);
#19124=CIRCLE('',#96528,0.4);
#19125=CIRCLE('',#96529,9.2);
#19126=CIRCLE('',#96530,0.4);
#19127=CIRCLE('',#96531,0.6);
#19128=CIRCLE('',#96532,0.2);
#19129=CIRCLE('',#96534,0.4);
#19130=CIRCLE('',#96535,0.4);
#19131=CIRCLE('',#96536,0.6);
#19132=CIRCLE('',#96537,0.2);
#19133=CIRCLE('',#96539,0.4);
#19134=CIRCLE('',#96540,3.9);
#19135=CIRCLE('',#96541,0.4);
#19136=CIRCLE('',#96542,0.6);
#19137=CIRCLE('',#96543,0.2);
#19138=CIRCLE('',#96545,0.4);
#19139=CIRCLE('',#96546,0.4);
#19140=CIRCLE('',#96547,0.6);
#19141=CIRCLE('',#96548,0.2);
#19142=CIRCLE('',#96550,0.4);
#19143=CIRCLE('',#96551,0.6);
#19144=CIRCLE('',#96552,0.2);
#19145=CIRCLE('',#96555,0.6);
#19146=CIRCLE('',#96558,0.6);
#19147=CIRCLE('',#96560,9.2);
#19148=CIRCLE('',#96561,9.2);
#19149=CIRCLE('',#96564,9.2);
#19150=CIRCLE('',#96567,0.8);
#19151=CIRCLE('',#96570,0.6);
#19152=CIRCLE('',#96572,0.6);
#19153=CIRCLE('',#96574,3.2);
#19154=CIRCLE('',#96576,0.399999999999999);
#19155=CIRCLE('',#96577,0.399999999999999);
#19156=CIRCLE('',#96581,0.4);
#19157=CIRCLE('',#96582,0.4);
#19158=CIRCLE('',#96584,0.6);
#19159=CIRCLE('',#96586,0.8);
#19160=CIRCLE('',#96587,0.8);
#19161=CIRCLE('',#96589,0.8);
#19162=CIRCLE('',#96590,0.8);
#19163=CIRCLE('',#96592,3.43614417320659);
#19164=CIRCLE('',#96593,3.43614417320659);
#19165=CIRCLE('',#96596,3.60000000004514);
#19166=CIRCLE('',#96597,3.60000000004514);
#19167=CIRCLE('',#96599,2.8);
#19168=CIRCLE('',#96600,1.6);
#19169=CIRCLE('',#96602,1.6);
#19170=CIRCLE('',#96604,2.8);
#19171=CIRCLE('',#96607,0.4);
#19172=CIRCLE('',#96609,4.2);
#19173=CIRCLE('',#96611,0.800000000000001);
#19174=CIRCLE('',#96613,0.4);
#19175=CIRCLE('',#96614,0.4);
#19176=CIRCLE('',#96616,0.8);
#19177=CIRCLE('',#96617,0.8);
#19178=CIRCLE('',#96620,0.6);
#19179=CIRCLE('',#96623,4.);
#19180=CIRCLE('',#96624,4.);
#19181=CIRCLE('',#96626,0.8);
#19182=CIRCLE('',#96627,0.8);
#19183=CIRCLE('',#96629,4.2);
#19184=CIRCLE('',#96630,4.2);
#19185=CIRCLE('',#96632,1.55);
#19186=CIRCLE('',#96633,1.55);
#19187=CIRCLE('',#96635,0.4);
#19188=CIRCLE('',#96636,0.4);
#19189=CIRCLE('',#96638,0.75);
#19190=CIRCLE('',#96639,0.75);
#19191=CIRCLE('',#96643,1.3);
#19192=CIRCLE('',#96644,1.3);
#19193=CIRCLE('',#96646,2.5);
#19194=CIRCLE('',#96647,2.10000000000135);
#19195=CIRCLE('',#96650,1.3);
#19196=CIRCLE('',#96651,1.3);
#19197=CIRCLE('',#96653,2.5);
#19198=CIRCLE('',#96654,2.10000000000135);
#19199=CIRCLE('',#96658,2.09999999998101);
#19200=CIRCLE('',#96659,2.5);
#19201=CIRCLE('',#96661,2.09999999998101);
#19202=CIRCLE('',#96662,2.5);
#19203=CIRCLE('',#96665,2.5);
#19204=CIRCLE('',#96666,2.5);
#19205=CIRCLE('',#96670,2.5);
#19206=CIRCLE('',#96671,2.5);
#19207=CIRCLE('',#96674,2.5);
#19208=CIRCLE('',#96675,2.5);
#19209=CIRCLE('',#96677,2.5);
#19210=CIRCLE('',#96679,2.5);
#19211=CIRCLE('',#96680,2.5);
#19212=CIRCLE('',#96682,2.5);
#19213=CIRCLE('',#96685,1.3);
#19214=CIRCLE('',#96686,1.3);
#19215=CIRCLE('',#96691,1.3);
#19216=CIRCLE('',#96692,1.3);
#19217=CIRCLE('',#96701,0.6);
#19218=CIRCLE('',#96703,11.55);
#19219=CIRCLE('',#96706,3.6);
#19220=CIRCLE('',#96708,2.);
#19221=CIRCLE('',#96709,1.);
#19222=CIRCLE('',#96711,2.);
#19223=CIRCLE('',#96713,4.1);
#19224=CIRCLE('',#96716,0.6);
#19225=CIRCLE('',#96718,3.7);
#19226=CIRCLE('',#96721,0.6);
#19227=CIRCLE('',#96722,0.6);
#19228=CIRCLE('',#96724,0.6);
#19229=CIRCLE('',#96725,5.79999999999998);
#19230=CIRCLE('',#96727,0.6);
#19231=CIRCLE('',#96729,5.79999999999998);
#19232=CIRCLE('',#96731,0.6);
#19233=CIRCLE('',#96736,11.55);
#19234=CIRCLE('',#96738,0.6);
#19235=CIRCLE('',#96741,10.45);
#19236=CIRCLE('',#96742,10.45);
#19237=CIRCLE('',#96743,10.45);
#19238=CIRCLE('',#96746,10.35);
#19239=CIRCLE('',#96747,10.35);
#19240=CIRCLE('',#96748,10.35);
#19241=CIRCLE('',#96755,0.6);
#19242=CIRCLE('',#96757,0.599999999999999);
#19243=CIRCLE('',#96759,2.85);
#19244=CIRCLE('',#96760,3.2);
#19245=CIRCLE('',#96762,2.8);
#19246=CIRCLE('',#96763,2.8);
#19247=CIRCLE('',#96765,3.6);
#19248=CIRCLE('',#96766,3.6);
#19249=CIRCLE('',#96770,0.6);
#19250=CIRCLE('',#96772,6.4499999999938);
#19251=CIRCLE('',#96774,1.);
#19252=CIRCLE('',#96776,11.65);
#19253=CIRCLE('',#96778,4.15);
#19254=CIRCLE('',#96779,3.75);
#19255=CIRCLE('',#96781,2.4);
#19256=CIRCLE('',#96783,4.15);
#19257=CIRCLE('',#96785,2.1);
#19258=CIRCLE('',#96787,2.8);
#19259=CIRCLE('',#96788,2.8);
#19260=CIRCLE('',#96791,1.6);
#19261=CIRCLE('',#96792,1.6);
#19262=CIRCLE('',#96795,2.30000000000004);
#19263=CIRCLE('',#96796,2.);
#19264=CIRCLE('',#96798,2.);
#19265=CIRCLE('',#96800,0.4);
#19266=CIRCLE('',#96801,0.4);
#19267=CIRCLE('',#96803,10.35);
#19268=CIRCLE('',#96804,10.35);
#19269=CIRCLE('',#96806,0.75);
#19270=CIRCLE('',#96807,0.75);
#19271=CIRCLE('',#96809,10.);
#19272=CIRCLE('',#96812,0.4);
#19273=CIRCLE('',#96814,2.5);
#19274=CIRCLE('',#96816,3.1);
#19275=CIRCLE('',#96817,3.1);
#19276=CIRCLE('',#96820,2.5);
#19277=CIRCLE('',#96822,0.6);
#19278=CIRCLE('',#96824,4.);
#19279=CIRCLE('',#96826,4.9);
#19280=CIRCLE('',#96828,0.6);
#19281=CIRCLE('',#96830,1.55);
#19282=CIRCLE('',#96832,3.05);
#19283=CIRCLE('',#96833,2.);
#19284=CIRCLE('',#96835,1.55);
#19285=CIRCLE('',#96837,2.);
#19286=CIRCLE('',#96841,8.4949617393671);
#19287=CIRCLE('',#96842,9.3949617393671);
#19288=CIRCLE('',#96844,23.7449617393671);
#19289=CIRCLE('',#96845,23.7449617393671);
#19290=CIRCLE('',#96847,1.65);
#19291=CIRCLE('',#96851,2.1);
#19292=CIRCLE('',#96852,1.2);
#19293=CIRCLE('',#96854,1.);
#19294=CIRCLE('',#96855,1.);
#19295=CIRCLE('',#96857,2.8);
#19296=CIRCLE('',#96859,2.8);
#19297=CIRCLE('',#96864,5.35);
#19298=CIRCLE('',#96865,5.35);
#19299=CIRCLE('',#96866,5.35);
#19300=CIRCLE('',#96868,3.3);
#19301=CIRCLE('',#96869,3.3);
#19302=CIRCLE('',#96870,3.3);
#19303=CIRCLE('',#96873,2.2);
#19304=CIRCLE('',#96878,0.75);
#19305=CIRCLE('',#96881,3.6);
#19306=CIRCLE('',#96883,0.5);
#19307=CIRCLE('',#96885,0.4);
#19308=CIRCLE('',#96886,3.2);
#19309=CIRCLE('',#96888,3.2);
#19310=CIRCLE('',#96890,0.4);
#19311=CIRCLE('',#96892,0.400000000000005);
#19312=CIRCLE('',#96893,0.399999999999949);
#19313=CIRCLE('',#96895,0.4);
#19314=CIRCLE('',#96897,0.400000000000001);
#19315=CIRCLE('',#96898,0.4);
#19316=CIRCLE('',#96900,0.4);
#19317=CIRCLE('',#96901,0.400000000000003);
#19318=CIRCLE('',#96904,0.4);
#19319=CIRCLE('',#96906,2.8);
#19320=CIRCLE('',#96909,24.9449617393673);
#19321=CIRCLE('',#96912,0.399999999999997);
#19322=CIRCLE('',#96913,4.3);
#19323=CIRCLE('',#96915,4.3);
#19324=CIRCLE('',#96918,0.6);
#19325=CIRCLE('',#96920,4.1);
#19326=CIRCLE('',#96922,0.6);
#19327=CIRCLE('',#96925,1.);
#19328=CIRCLE('',#96926,1.);
#19329=CIRCLE('',#96928,2.5);
#19330=CIRCLE('',#96929,2.5);
#19331=CIRCLE('',#96932,1.);
#19332=CIRCLE('',#96933,1.);
#19333=CIRCLE('',#96935,17.3949617393671);
#19334=CIRCLE('',#96936,18.2949617393671);
#19335=CIRCLE('',#96938,4.8);
#19336=CIRCLE('',#96939,0.8);
#19337=CIRCLE('',#96941,0.6);
#19338=CIRCLE('',#96943,0.8);
#19339=CIRCLE('',#96946,0.800000000000001);
#19340=CIRCLE('',#96949,0.800000000000003);
#19341=CIRCLE('',#96950,0.8);
#19342=CIRCLE('',#96953,0.8);
#19343=CIRCLE('',#96956,0.8);
#19344=CIRCLE('',#96958,0.8);
#19345=CIRCLE('',#96959,7.8);
#19346=CIRCLE('',#96962,0.8);
#19347=CIRCLE('',#96964,0.8);
#19348=CIRCLE('',#96966,5.25);
#19349=CIRCLE('',#96967,5.25);
#19350=CIRCLE('',#96969,0.4);
#19351=CIRCLE('',#96970,7.8);
#19352=CIRCLE('',#96971,10.45);
#19353=CIRCLE('',#96973,0.4);
#19354=CIRCLE('',#96975,10.45);
#19355=CIRCLE('',#96976,10.45);
#19356=CIRCLE('',#96977,10.45);
#19357=CIRCLE('',#96979,0.4);
#19358=CIRCLE('',#96980,0.4);
#19359=CIRCLE('',#96982,3.05);
#19360=CIRCLE('',#96983,3.05);
#19361=CIRCLE('',#96985,3.25);
#19362=CIRCLE('',#96986,3.25);
#19363=CIRCLE('',#96990,0.2);
#19364=CIRCLE('',#96991,0.2);
#19365=CIRCLE('',#96992,0.6);
#19366=CIRCLE('',#96993,0.6);
#19367=CIRCLE('',#96994,0.6);
#19368=CIRCLE('',#96995,0.2);
#19369=CIRCLE('',#96996,0.2);
#19370=CIRCLE('',#96997,0.6);
#19371=CIRCLE('',#96998,0.6);
#19372=CIRCLE('',#96999,3.7);
#19373=CIRCLE('',#97000,0.4);
#19374=CIRCLE('',#97001,7.8);
#19375=CIRCLE('',#97002,4.8);
#19376=CIRCLE('',#97004,0.6);
#19377=CIRCLE('',#97022,0.2);
#19378=CIRCLE('',#97024,0.2);
#19379=CIRCLE('',#97026,0.2);
#19380=CIRCLE('',#97029,0.2);
#19381=CIRCLE('',#97039,0.299999999999997);
#19382=CIRCLE('',#97044,0.4);
#19383=CIRCLE('',#97049,0.6);
#19384=CIRCLE('',#97051,0.4);
#19385=CIRCLE('',#97053,10.6);
#19386=CIRCLE('',#97055,0.4);
#19387=CIRCLE('',#97057,0.4);
#19388=CIRCLE('',#97058,7.8);
#19389=CIRCLE('',#97060,0.4);
#19390=CIRCLE('',#97079,0.8);
#19391=CIRCLE('',#97080,0.800000000000001);
#19392=CIRCLE('',#97086,0.8);
#19393=CIRCLE('',#97088,0.8);
#19394=CIRCLE('',#97097,4.);
#19395=CIRCLE('',#97098,5.);
#19396=CIRCLE('',#97099,4.9);
#19397=CIRCLE('',#97100,8.);
#19398=CIRCLE('',#97101,1.);
#19399=CIRCLE('',#97102,1.);
#19400=CIRCLE('',#97104,4.);
#19401=CIRCLE('',#97105,10.25);
#19402=CIRCLE('',#97106,4.);
#19403=CIRCLE('',#97107,5.);
#19404=CIRCLE('',#97108,3.);
#19405=CIRCLE('',#97109,4.2);
#19406=CIRCLE('',#97110,3.);
#19407=CIRCLE('',#97111,8.);
#19408=CIRCLE('',#97114,8.);
#19409=CIRCLE('',#97115,3.);
#19410=CIRCLE('',#97116,4.2);
#19411=CIRCLE('',#97117,3.);
#19412=CIRCLE('',#97118,5.);
#19413=CIRCLE('',#97119,4.);
#19414=CIRCLE('',#97120,10.25);
#19415=CIRCLE('',#97121,4.);
#19416=CIRCLE('',#97124,1.7);
#19417=CIRCLE('',#97125,1.7);
#19418=CIRCLE('',#97126,1.7);
#19419=CIRCLE('',#97128,3.4);
#19420=CIRCLE('',#97129,3.4);
#19421=CIRCLE('',#97140,4.);
#19422=CIRCLE('',#97142,1.);
#19423=CIRCLE('',#97145,1.);
#19424=CIRCLE('',#97146,8.);
#19425=CIRCLE('',#97147,4.9);
#19426=CIRCLE('',#97148,5.);
#19427=CIRCLE('',#97149,4.);
#19428=CIRCLE('',#97155,1.7);
#19429=CIRCLE('',#97157,3.2);
#19430=CIRCLE('',#97160,3.2);
#19431=CIRCLE('',#97164,3.2);
#19432=CIRCLE('',#97167,3.2);
#19433=CIRCLE('',#97169,1.7);
#19434=CIRCLE('',#97174,4.);
#19435=CIRCLE('',#97176,4.);
#19436=CIRCLE('',#97178,3.);
#19437=CIRCLE('',#97179,2.99999999999999);
#19438=CIRCLE('',#97180,1.5);
#19439=CIRCLE('',#97182,3.);
#19440=CIRCLE('',#97183,2.99999999999999);
#19441=CIRCLE('',#97184,1.5);
#19442=CIRCLE('',#97186,4.);
#19443=CIRCLE('',#97188,4.);
#19444=CIRCLE('',#97190,2.99999999999999);
#19445=CIRCLE('',#97191,3.);
#19446=CIRCLE('',#97192,1.5);
#19447=CIRCLE('',#97194,3.);
#19448=CIRCLE('',#97195,2.99999999999999);
#19449=CIRCLE('',#97196,1.5);
#19450=CIRCLE('',#97202,4.);
#19451=CIRCLE('',#97203,1.6);
#19452=CIRCLE('',#97205,4.);
#19453=CIRCLE('',#97207,4.);
#19454=CIRCLE('',#97208,1.6);
#19455=CIRCLE('',#97210,4.);
#19456=CIRCLE('',#97225,1.3);
#19457=CIRCLE('',#97226,1.5);
#19458=CIRCLE('',#97228,1.5);
#19459=CIRCLE('',#97231,1.3);
#19460=CIRCLE('',#97235,1.4);
#19461=CIRCLE('',#97236,1.5);
#19462=CIRCLE('',#97238,1.5);
#19463=CIRCLE('',#97241,1.4);
#19464=CIRCLE('',#97245,9.);
#19465=CIRCLE('',#97246,9.);
#19466=CIRCLE('',#97248,9.);
#19467=CIRCLE('',#97249,9.);
#19468=CIRCLE('',#97251,9.);
#19469=CIRCLE('',#97252,9.);
#19470=CIRCLE('',#97254,9.);
#19471=CIRCLE('',#97255,9.);
#19472=CIRCLE('',#97257,9.);
#19473=CIRCLE('',#97258,9.);
#19474=CIRCLE('',#97260,9.);
#19475=CIRCLE('',#97261,9.);
#19476=CIRCLE('',#97263,9.);
#19477=CIRCLE('',#97264,9.);
#19478=CIRCLE('',#97266,9.);
#19479=CIRCLE('',#97267,9.);
#19480=CIRCLE('',#97269,9.);
#19481=CIRCLE('',#97270,9.);
#19482=CIRCLE('',#97272,9.);
#19483=CIRCLE('',#97273,9.);
#19484=CIRCLE('',#97275,9.);
#19485=CIRCLE('',#97276,9.);
#19486=CIRCLE('',#97278,9.);
#19487=CIRCLE('',#97279,9.);
#19488=CIRCLE('',#97281,9.);
#19489=CIRCLE('',#97282,9.);
#19490=CIRCLE('',#97284,9.);
#19491=CIRCLE('',#97285,9.);
#19492=CIRCLE('',#97287,9.);
#19493=CIRCLE('',#97288,9.);
#19494=CIRCLE('',#97290,9.);
#19495=CIRCLE('',#97291,9.);
#19496=CIRCLE('',#97293,9.);
#19497=CIRCLE('',#97294,9.);
#19498=CIRCLE('',#97296,9.);
#19499=CIRCLE('',#97297,9.);
#19500=CIRCLE('',#97299,9.);
#19501=CIRCLE('',#97300,9.);
#19502=CIRCLE('',#97302,9.);
#19503=CIRCLE('',#97303,9.);
#19504=CIRCLE('',#97305,9.);
#19505=CIRCLE('',#97306,9.);
#19506=CIRCLE('',#97308,9.);
#19507=CIRCLE('',#97309,9.);
#19508=CIRCLE('',#97311,9.);
#19509=CIRCLE('',#97312,9.);
#19510=CIRCLE('',#97314,9.);
#19511=CIRCLE('',#97315,9.);
#19512=CIRCLE('',#97317,9.);
#19513=CIRCLE('',#97318,9.);
#19514=CIRCLE('',#97320,9.);
#19515=CIRCLE('',#97321,9.);
#19516=CIRCLE('',#97323,9.);
#19517=CIRCLE('',#97324,9.);
#19518=CIRCLE('',#97326,9.);
#19519=CIRCLE('',#97327,9.);
#19520=CIRCLE('',#97329,9.);
#19521=CIRCLE('',#97330,9.);
#19522=CIRCLE('',#97332,9.);
#19523=CIRCLE('',#97333,9.);
#19524=CIRCLE('',#97335,9.);
#19525=CIRCLE('',#97336,9.);
#19526=CIRCLE('',#97338,9.);
#19527=CIRCLE('',#97339,9.);
#19528=CIRCLE('',#97341,9.);
#19529=CIRCLE('',#97342,9.);
#19530=CIRCLE('',#97344,9.);
#19531=CIRCLE('',#97345,9.);
#19532=CIRCLE('',#97347,9.);
#19533=CIRCLE('',#97348,9.);
#19534=CIRCLE('',#97350,9.);
#19535=CIRCLE('',#97351,9.);
#19536=CIRCLE('',#97353,9.);
#19537=CIRCLE('',#97354,9.);
#19538=CIRCLE('',#97356,9.);
#19539=CIRCLE('',#97357,9.);
#19540=CIRCLE('',#97359,9.);
#19541=CIRCLE('',#97360,9.);
#19542=CIRCLE('',#97362,9.);
#19543=CIRCLE('',#97363,9.);
#19544=CIRCLE('',#97365,9.);
#19545=CIRCLE('',#97366,9.);
#19546=CIRCLE('',#97368,9.);
#19547=CIRCLE('',#97369,9.);
#19548=CIRCLE('',#97371,9.);
#19549=CIRCLE('',#97372,9.);
#19550=CIRCLE('',#97374,9.);
#19551=CIRCLE('',#97375,9.);
#19552=CIRCLE('',#97377,9.);
#19553=CIRCLE('',#97378,9.);
#19554=CIRCLE('',#97380,9.);
#19555=CIRCLE('',#97381,9.);
#19556=CIRCLE('',#97383,9.);
#19557=CIRCLE('',#97384,9.);
#19558=CIRCLE('',#97386,9.);
#19559=CIRCLE('',#97387,9.);
#19560=CIRCLE('',#97389,9.);
#19561=CIRCLE('',#97390,9.);
#19562=CIRCLE('',#97392,9.);
#19563=CIRCLE('',#97393,9.);
#19564=CIRCLE('',#97395,9.);
#19565=CIRCLE('',#97396,9.);
#19566=CIRCLE('',#97398,9.);
#19567=CIRCLE('',#97399,9.);
#19568=CIRCLE('',#97401,9.);
#19569=CIRCLE('',#97402,9.);
#19570=CIRCLE('',#97404,9.);
#19571=CIRCLE('',#97405,9.);
#19572=CIRCLE('',#97407,9.);
#19573=CIRCLE('',#97408,9.);
#19574=CIRCLE('',#97410,9.);
#19575=CIRCLE('',#97411,9.);
#19576=CIRCLE('',#97413,9.);
#19577=CIRCLE('',#97414,9.);
#19578=CIRCLE('',#97416,9.);
#19579=CIRCLE('',#97417,9.);
#19580=CIRCLE('',#97419,9.);
#19581=CIRCLE('',#97420,9.);
#19582=CIRCLE('',#97422,9.);
#19583=CIRCLE('',#97423,9.);
#19584=CIRCLE('',#97425,9.);
#19585=CIRCLE('',#97426,9.);
#19586=CIRCLE('',#97428,9.);
#19587=CIRCLE('',#97429,9.);
#19588=CIRCLE('',#97431,9.);
#19589=CIRCLE('',#97432,9.);
#19590=CIRCLE('',#97434,9.);
#19591=CIRCLE('',#97435,9.);
#19592=CIRCLE('',#97437,9.);
#19593=CIRCLE('',#97438,9.);
#19594=CIRCLE('',#97440,9.);
#19595=CIRCLE('',#97441,9.);
#19596=CIRCLE('',#97443,9.);
#19597=CIRCLE('',#97444,9.);
#19598=CIRCLE('',#97446,9.);
#19599=CIRCLE('',#97447,9.);
#19600=CIRCLE('',#97449,9.);
#19601=CIRCLE('',#97450,9.);
#19602=CIRCLE('',#97452,9.);
#19603=CIRCLE('',#97453,9.);
#19604=CIRCLE('',#97455,2.5);
#19605=CIRCLE('',#97456,2.9);
#19606=CIRCLE('',#97457,2.5);
#19607=CIRCLE('',#97459,1.5);
#19608=CIRCLE('',#97460,1.7);
#19609=CIRCLE('',#97461,1.5);
#19610=CIRCLE('',#97463,1.5);
#19611=CIRCLE('',#97464,1.7);
#19612=CIRCLE('',#97465,1.5);
#19613=CIRCLE('',#97467,9.);
#19614=CIRCLE('',#97468,8.8);
#19615=CIRCLE('',#97469,9.);
#19616=CIRCLE('',#97471,1.5);
#19617=CIRCLE('',#97472,1.7);
#19618=CIRCLE('',#97474,1.5);
#19619=CIRCLE('',#97475,1.7);
#19620=CIRCLE('',#97477,3.5);
#19621=CIRCLE('',#97478,3.3);
#19622=CIRCLE('',#97479,3.5);
#19623=CIRCLE('',#97481,2.5);
#19624=CIRCLE('',#97482,2.7);
#19625=CIRCLE('',#97486,8.5);
#19626=CIRCLE('',#97489,3.5);
#19627=CIRCLE('',#97495,2.272884449);
#19628=CIRCLE('',#97497,2.272884449);
#19629=CIRCLE('',#97500,2.272884449);
#19630=CIRCLE('',#97502,2.272884449);
#19631=CIRCLE('',#97505,2.272884449);
#19632=CIRCLE('',#97507,2.272884449);
#19633=CIRCLE('',#97510,2.272884449);
#19634=CIRCLE('',#97512,2.272884449);
#19635=CIRCLE('',#97515,2.272884449);
#19636=CIRCLE('',#97517,2.272884449);
#19637=CIRCLE('',#97520,2.272884449);
#19638=CIRCLE('',#97522,2.272884449);
#19639=CIRCLE('',#97525,2.272884449);
#19640=CIRCLE('',#97527,2.27288445);
#19641=CIRCLE('',#97530,2.272884449);
#19642=CIRCLE('',#97532,2.272884449);
#19643=CIRCLE('',#97535,2.272884449);
#19644=CIRCLE('',#97537,2.272884449);
#19645=CIRCLE('',#97540,2.272884449);
#19646=CIRCLE('',#97542,2.272884449);
#19647=CIRCLE('',#97545,2.272884449);
#19648=CIRCLE('',#97547,2.27288445);
#19649=CIRCLE('',#97550,2.27288445);
#19650=CIRCLE('',#97552,2.272884449);
#19651=CIRCLE('',#97555,2.272884449);
#19652=CIRCLE('',#97557,2.272884449);
#19653=CIRCLE('',#97560,2.272884449);
#19654=CIRCLE('',#97562,2.272884449);
#19655=CIRCLE('',#97565,2.272884449);
#19656=CIRCLE('',#97567,2.272884449);
#19657=CIRCLE('',#97570,2.272884449);
#19658=CIRCLE('',#97572,2.272884449);
#19659=CIRCLE('',#97575,2.272884449);
#19660=CIRCLE('',#97577,2.272884449);
#19661=CIRCLE('',#97580,2.272884449);
#19662=CIRCLE('',#97582,2.272884449);
#19663=CIRCLE('',#97585,2.272884449);
#19664=CIRCLE('',#97587,2.272884449);
#19665=CIRCLE('',#97590,2.27288445);
#19666=CIRCLE('',#97592,2.272884449);
#19667=CIRCLE('',#97595,2.272884449);
#19668=CIRCLE('',#97597,2.272884449);
#19669=CIRCLE('',#97600,2.272884449);
#19670=CIRCLE('',#97602,2.272884449);
#19671=CIRCLE('',#97605,2.272884449);
#19672=CIRCLE('',#97607,2.272884449);
#19673=CIRCLE('',#97610,2.272884449);
#19674=CIRCLE('',#97612,2.272884449);
#19675=CIRCLE('',#97615,2.272884449);
#19676=CIRCLE('',#97617,2.272884449);
#19677=CIRCLE('',#97620,2.272884449);
#19678=CIRCLE('',#97622,2.272884449);
#19679=CIRCLE('',#97625,2.272884449);
#19680=CIRCLE('',#97627,2.272884449);
#19681=CIRCLE('',#97630,2.272884449);
#19682=CIRCLE('',#97632,2.272884449);
#19683=CIRCLE('',#97635,2.272884449);
#19684=CIRCLE('',#97637,2.272884449);
#19685=CIRCLE('',#97640,2.272884449);
#19686=CIRCLE('',#97642,2.272884449);
#19687=CIRCLE('',#97645,2.272884449);
#19688=CIRCLE('',#97647,2.272884449);
#19689=CIRCLE('',#97650,2.272884449);
#19690=CIRCLE('',#97652,2.272884449);
#19691=CIRCLE('',#97655,2.272884449);
#19692=CIRCLE('',#97657,2.272884449);
#19693=CIRCLE('',#97660,2.272884449);
#19694=CIRCLE('',#97662,2.272884449);
#19695=CIRCLE('',#97665,2.272884449);
#19696=CIRCLE('',#97667,2.27288445);
#19697=CIRCLE('',#97670,2.272884449);
#19698=CIRCLE('',#97672,2.272884449);
#19699=CIRCLE('',#97675,2.272884449);
#19700=CIRCLE('',#97677,2.272884449);
#19701=CIRCLE('',#97680,2.272884449);
#19702=CIRCLE('',#97682,2.272884449);
#19703=CIRCLE('',#97685,2.272884449);
#19704=CIRCLE('',#97687,2.272884449);
#19705=CIRCLE('',#97690,2.272884449);
#19706=CIRCLE('',#97692,2.272884449);
#19707=CIRCLE('',#97695,2.272884449);
#19708=CIRCLE('',#97697,2.272884449);
#19709=CIRCLE('',#97700,2.272884449);
#19710=CIRCLE('',#97702,2.27288445);
#19711=CIRCLE('',#97705,2.272884449);
#19712=CIRCLE('',#97707,2.272884449);
#19713=CIRCLE('',#97710,2.272884449);
#19714=CIRCLE('',#97712,2.272884449);
#19715=CIRCLE('',#97715,2.272884449);
#19716=CIRCLE('',#97717,2.272884449);
#19717=CIRCLE('',#97720,2.272884449);
#19718=CIRCLE('',#97722,2.27288445);
#19719=CIRCLE('',#97725,2.27288445);
#19720=CIRCLE('',#97727,2.272884449);
#19721=CIRCLE('',#97730,2.272884449);
#19722=CIRCLE('',#97732,2.272884449);
#19723=CIRCLE('',#97735,2.272884449);
#19724=CIRCLE('',#97737,2.272884449);
#19725=CIRCLE('',#97740,2.272884449);
#19726=CIRCLE('',#97742,2.272884449);
#19727=CIRCLE('',#97745,2.272884449);
#19728=CIRCLE('',#97747,2.272884449);
#19729=CIRCLE('',#97750,2.272884449);
#19730=CIRCLE('',#97752,2.272884449);
#19731=CIRCLE('',#97755,2.272884449);
#19732=CIRCLE('',#97757,2.272884449);
#19733=CIRCLE('',#97760,2.272884449);
#19734=CIRCLE('',#97762,2.272884449);
#19735=CIRCLE('',#97765,2.27288445);
#19736=CIRCLE('',#97767,2.272884449);
#19737=CIRCLE('',#97770,2.272884449);
#19738=CIRCLE('',#97772,2.272884449);
#19739=CIRCLE('',#97775,2.272884449);
#19740=CIRCLE('',#97777,2.272884449);
#19741=CIRCLE('',#97780,2.272884449);
#19742=CIRCLE('',#97782,2.272884449);
#19743=CIRCLE('',#97785,2.272884449);
#19744=CIRCLE('',#97787,2.272884449);
#19745=CIRCLE('',#97790,2.272884449);
#19746=CIRCLE('',#97792,2.272884449);
#19747=CIRCLE('',#97795,2.272884449);
#19748=CIRCLE('',#97797,2.272884449);
#19749=CIRCLE('',#97800,2.272884449);
#19750=CIRCLE('',#97802,2.272884449);
#19751=CIRCLE('',#97805,2.272884449);
#19752=CIRCLE('',#97807,2.272884449);
#19753=CIRCLE('',#97810,2.272884449);
#19754=CIRCLE('',#97812,2.272884449);
#19755=CIRCLE('',#97815,2.272884449);
#19756=CIRCLE('',#97817,2.272884449);
#19757=CIRCLE('',#97820,2.272884449);
#19758=CIRCLE('',#97822,2.272884449);
#19759=CIRCLE('',#97825,2.272884449);
#19760=CIRCLE('',#97827,2.272884449);
#19761=CIRCLE('',#97830,2.272884449);
#19762=CIRCLE('',#97832,2.272884449);
#19763=CIRCLE('',#97835,2.272884449);
#19764=CIRCLE('',#97837,2.272884449);
#19765=CIRCLE('',#97840,2.272884449);
#19766=CIRCLE('',#97842,2.27288445);
#19767=CIRCLE('',#97845,1.);
#19768=CIRCLE('',#97846,1.);
#19769=CIRCLE('',#97848,1.);
#19770=CIRCLE('',#97849,1.);
#19771=CIRCLE('',#97851,1.6);
#19772=CIRCLE('',#97852,0.1);
#19773=CIRCLE('',#97853,1.5);
#19774=CIRCLE('',#97855,1.6);
#19775=CIRCLE('',#97856,0.1);
#19776=CIRCLE('',#97857,1.5);
#19777=CIRCLE('',#97859,1.5);
#19778=CIRCLE('',#97860,0.2);
#19779=CIRCLE('',#97861,1.7);
#19780=CIRCLE('',#97862,1.5);
#19781=CIRCLE('',#97864,1.5);
#19782=CIRCLE('',#97865,0.2);
#19783=CIRCLE('',#97866,1.7);
#19784=CIRCLE('',#97868,2.8);
#19785=CIRCLE('',#97869,0.2);
#19786=CIRCLE('',#97870,3.);
#19787=CIRCLE('',#97871,3.);
#19788=CIRCLE('',#97873,0.4);
#19789=CIRCLE('',#97874,0.2);
#19790=CIRCLE('',#97875,0.6);
#19791=CIRCLE('',#97876,0.2);
#19792=CIRCLE('',#97878,0.4);
#19793=CIRCLE('',#97879,0.2);
#19794=CIRCLE('',#97880,0.6);
#19795=CIRCLE('',#97881,0.2);
#19796=CIRCLE('',#97883,3.9);
#19797=CIRCLE('',#97884,0.4);
#19798=CIRCLE('',#97885,3.5);
#19799=CIRCLE('',#97886,3.5);
#19800=CIRCLE('',#97888,1.1);
#19801=CIRCLE('',#97889,0.4);
#19802=CIRCLE('',#97890,1.5);
#19803=CIRCLE('',#97891,1.5);
#19804=CIRCLE('',#97893,1.1);
#19805=CIRCLE('',#97894,0.4);
#19806=CIRCLE('',#97895,1.5);
#19807=CIRCLE('',#97896,1.5);
#19808=CIRCLE('',#97898,0.4);
#19809=CIRCLE('',#97899,0.4);
#19810=CIRCLE('',#97901,0.4);
#19811=CIRCLE('',#97902,0.4);
#19812=CIRCLE('',#97904,3.5);
#19813=CIRCLE('',#97908,3.);
#19814=CIRCLE('',#97910,3.7);
#19815=CIRCLE('',#97911,3.7);
#19816=CIRCLE('',#97913,3.7);
#19817=CIRCLE('',#97914,3.7);
#19818=CIRCLE('',#97916,3.7);
#19819=CIRCLE('',#97917,3.7);
#19820=CIRCLE('',#97919,3.7);
#19821=CIRCLE('',#97920,3.7);
#19822=CIRCLE('',#97923,3.7);
#19823=CIRCLE('',#97924,8.624);
#19824=CIRCLE('',#97925,3.7);
#19825=CIRCLE('',#97926,9.75);
#19826=CIRCLE('',#97927,3.7);
#19827=CIRCLE('',#97928,8.624);
#19828=CIRCLE('',#97929,3.7);
#19829=CIRCLE('',#97930,9.75);
#19830=CIRCLE('',#97931,3.7);
#19831=CIRCLE('',#97932,8.624);
#19832=CIRCLE('',#97933,3.7);
#19833=CIRCLE('',#97934,9.75);
#19834=CIRCLE('',#97935,3.7);
#19835=CIRCLE('',#97936,8.624);
#19836=CIRCLE('',#97937,3.7);
#19837=CIRCLE('',#97938,9.75);
#19838=CIRCLE('',#97939,3.7);
#19839=CIRCLE('',#97940,8.624);
#19840=CIRCLE('',#97941,3.7);
#19841=CIRCLE('',#97942,9.75);
#19842=CIRCLE('',#97943,3.7);
#19843=CIRCLE('',#97944,8.624);
#19844=CIRCLE('',#97945,3.7);
#19845=CIRCLE('',#97946,9.75);
#19846=CIRCLE('',#97947,3.7);
#19847=CIRCLE('',#97948,8.624);
#19848=CIRCLE('',#97949,3.7);
#19849=CIRCLE('',#97950,9.75);
#19850=CIRCLE('',#97951,3.7);
#19851=CIRCLE('',#97952,8.624);
#19852=CIRCLE('',#97953,9.75);
#19853=CIRCLE('',#97954,3.7);
#19854=CIRCLE('',#97955,8.624);
#19855=CIRCLE('',#97956,9.75);
#19856=CIRCLE('',#97957,3.7);
#19857=CIRCLE('',#97958,8.624);
#19858=CIRCLE('',#97959,3.7);
#19859=CIRCLE('',#97960,9.75);
#19860=CIRCLE('',#97961,3.7);
#19861=CIRCLE('',#97962,8.624);
#19862=CIRCLE('',#97963,3.7);
#19863=CIRCLE('',#97964,9.75);
#19864=CIRCLE('',#97965,3.7);
#19865=CIRCLE('',#97966,8.624);
#19866=CIRCLE('',#97967,3.7);
#19867=CIRCLE('',#97968,9.75);
#19868=CIRCLE('',#97969,3.7);
#19869=CIRCLE('',#97970,8.624);
#19870=CIRCLE('',#97971,3.7);
#19871=CIRCLE('',#97972,9.75);
#19872=CIRCLE('',#97973,3.7);
#19873=CIRCLE('',#97974,8.624);
#19874=CIRCLE('',#97975,3.7);
#19875=CIRCLE('',#97976,9.75);
#19876=CIRCLE('',#97977,3.7);
#19877=CIRCLE('',#97978,8.624);
#19878=CIRCLE('',#97979,3.7);
#19879=CIRCLE('',#97980,9.75);
#19880=CIRCLE('',#97981,3.7);
#19881=CIRCLE('',#97982,8.624);
#19882=CIRCLE('',#97983,3.7);
#19883=CIRCLE('',#97984,9.75);
#19884=CIRCLE('',#97985,3.7);
#19885=CIRCLE('',#97986,8.624);
#19886=CIRCLE('',#97987,3.7);
#19887=CIRCLE('',#97988,9.75);
#19888=CIRCLE('',#97989,3.7);
#19889=CIRCLE('',#97990,8.624);
#19890=CIRCLE('',#97991,3.7);
#19891=CIRCLE('',#97992,9.75);
#19892=CIRCLE('',#97993,3.7);
#19893=CIRCLE('',#97994,8.624);
#19894=CIRCLE('',#97995,3.7);
#19895=CIRCLE('',#97996,9.75);
#19896=CIRCLE('',#97997,3.7);
#19897=CIRCLE('',#97998,8.624);
#19898=CIRCLE('',#97999,3.7);
#19899=CIRCLE('',#98000,9.75);
#19900=CIRCLE('',#98001,3.7);
#19901=CIRCLE('',#98002,8.624);
#19902=CIRCLE('',#98003,3.7);
#19903=CIRCLE('',#98004,9.75);
#19904=CIRCLE('',#98005,3.7);
#19905=CIRCLE('',#98006,8.624);
#19906=CIRCLE('',#98007,3.7);
#19907=CIRCLE('',#98008,9.75);
#19908=CIRCLE('',#98009,3.7);
#19909=CIRCLE('',#98010,8.624);
#19910=CIRCLE('',#98011,3.7);
#19911=CIRCLE('',#98012,9.75);
#19912=CIRCLE('',#98013,3.7);
#19913=CIRCLE('',#98014,8.624);
#19914=CIRCLE('',#98015,3.7);
#19915=CIRCLE('',#98016,9.75);
#19916=CIRCLE('',#98017,3.7);
#19917=CIRCLE('',#98018,8.624);
#19918=CIRCLE('',#98019,3.7);
#19919=CIRCLE('',#98020,9.75);
#19920=CIRCLE('',#98021,3.7);
#19921=CIRCLE('',#98022,8.624);
#19922=CIRCLE('',#98023,3.7);
#19923=CIRCLE('',#98024,9.75);
#19924=CIRCLE('',#98025,3.7);
#19925=CIRCLE('',#98026,8.624);
#19926=CIRCLE('',#98027,3.7);
#19927=CIRCLE('',#98028,9.75);
#19928=CIRCLE('',#98029,3.7);
#19929=CIRCLE('',#98030,8.624);
#19930=CIRCLE('',#98031,3.7);
#19931=CIRCLE('',#98032,9.75);
#19932=CIRCLE('',#98033,3.7);
#19933=CIRCLE('',#98034,8.624);
#19934=CIRCLE('',#98035,3.7);
#19935=CIRCLE('',#98036,9.75);
#19936=CIRCLE('',#98037,3.7);
#19937=CIRCLE('',#98038,8.624);
#19938=CIRCLE('',#98039,3.7);
#19939=CIRCLE('',#98040,9.75);
#19940=CIRCLE('',#98041,8.624);
#19941=CIRCLE('',#98042,3.7);
#19942=CIRCLE('',#98043,9.75);
#19943=CIRCLE('',#98044,8.624);
#19944=CIRCLE('',#98045,3.7);
#19945=CIRCLE('',#98046,9.75);
#19946=CIRCLE('',#98047,3.7);
#19947=CIRCLE('',#98048,8.624);
#19948=CIRCLE('',#98049,3.7);
#19949=CIRCLE('',#98050,9.75);
#19950=CIRCLE('',#98051,3.7);
#19951=CIRCLE('',#98052,8.624);
#19952=CIRCLE('',#98053,3.7);
#19953=CIRCLE('',#98054,9.75);
#19954=CIRCLE('',#98055,3.7);
#19955=CIRCLE('',#98056,8.624);
#19956=CIRCLE('',#98057,3.7);
#19957=CIRCLE('',#98058,9.75);
#19958=CIRCLE('',#98059,3.7);
#19959=CIRCLE('',#98060,8.624);
#19960=CIRCLE('',#98061,3.7);
#19961=CIRCLE('',#98062,9.75);
#19962=CIRCLE('',#98063,3.7);
#19963=CIRCLE('',#98064,8.624);
#19964=CIRCLE('',#98065,3.7);
#19965=CIRCLE('',#98066,9.75);
#19966=CIRCLE('',#98067,4.8);
#19967=CIRCLE('',#98068,0.6);
#19968=CIRCLE('',#98069,7.4);
#19969=CIRCLE('',#98070,0.6);
#19970=CIRCLE('',#98071,0.6);
#19971=CIRCLE('',#98072,0.6);
#19972=CIRCLE('',#98073,7.4);
#19973=CIRCLE('',#98074,0.6);
#19974=CIRCLE('',#98075,4.8);
#19975=CIRCLE('',#98076,0.6);
#19976=CIRCLE('',#98078,9.75);
#19977=CIRCLE('',#98080,9.75);
#19978=CIRCLE('',#98082,9.75);
#19979=CIRCLE('',#98084,9.75);
#19980=CIRCLE('',#98086,9.75);
#19981=CIRCLE('',#98088,9.75);
#19982=CIRCLE('',#98090,9.75);
#19983=CIRCLE('',#98092,9.75);
#19984=CIRCLE('',#98094,9.75);
#19985=CIRCLE('',#98096,9.75);
#19986=CIRCLE('',#98098,9.75);
#19987=CIRCLE('',#98100,9.75);
#19988=CIRCLE('',#98102,9.75);
#19989=CIRCLE('',#98104,9.75);
#19990=CIRCLE('',#98106,9.75);
#19991=CIRCLE('',#98108,9.75);
#19992=CIRCLE('',#98110,9.75);
#19993=CIRCLE('',#98112,9.75);
#19994=CIRCLE('',#98114,9.75);
#19995=CIRCLE('',#98116,9.75);
#19996=CIRCLE('',#98118,9.75);
#19997=CIRCLE('',#98120,9.75);
#19998=CIRCLE('',#98122,9.75);
#19999=CIRCLE('',#98124,9.75);
#20000=CIRCLE('',#98126,9.75);
#20001=CIRCLE('',#98128,9.75);
#20002=CIRCLE('',#98130,9.75);
#20003=CIRCLE('',#98132,9.75);
#20004=CIRCLE('',#98134,9.75);
#20005=CIRCLE('',#98136,9.75);
#20006=CIRCLE('',#98138,9.75);
#20007=CIRCLE('',#98140,9.75);
#20008=CIRCLE('',#98142,9.75);
#20009=CIRCLE('',#98144,9.75);
#20010=CIRCLE('',#98146,9.75);
#20011=CIRCLE('',#98148,9.75);
#20012=CIRCLE('',#98150,3.7);
#20013=CIRCLE('',#98151,3.7);
#20014=CIRCLE('',#98152,8.624);
#20015=CIRCLE('',#98153,3.7);
#20016=CIRCLE('',#98154,3.7);
#20017=CIRCLE('',#98155,8.624);
#20018=CIRCLE('',#98156,3.7);
#20019=CIRCLE('',#98157,3.7);
#20020=CIRCLE('',#98158,8.624);
#20021=CIRCLE('',#98159,3.7);
#20022=CIRCLE('',#98160,3.7);
#20023=CIRCLE('',#98161,8.624);
#20024=CIRCLE('',#98162,3.7);
#20025=CIRCLE('',#98163,3.7);
#20026=CIRCLE('',#98164,8.624);
#20027=CIRCLE('',#98165,3.7);
#20028=CIRCLE('',#98166,3.7);
#20029=CIRCLE('',#98167,8.624);
#20030=CIRCLE('',#98168,3.7);
#20031=CIRCLE('',#98169,8.624);
#20032=CIRCLE('',#98170,3.7);
#20033=CIRCLE('',#98171,8.624);
#20034=CIRCLE('',#98172,3.7);
#20035=CIRCLE('',#98173,9.75);
#20036=CIRCLE('',#98174,3.7);
#20037=CIRCLE('',#98175,8.624);
#20038=CIRCLE('',#98176,3.7);
#20039=CIRCLE('',#98177,3.7);
#20040=CIRCLE('',#98178,8.624);
#20041=CIRCLE('',#98179,3.7);
#20042=CIRCLE('',#98180,3.7);
#20043=CIRCLE('',#98181,8.624);
#20044=CIRCLE('',#98182,3.7);
#20045=CIRCLE('',#98183,3.7);
#20046=CIRCLE('',#98184,8.624);
#20047=CIRCLE('',#98185,3.7);
#20048=CIRCLE('',#98186,3.7);
#20049=CIRCLE('',#98187,8.624);
#20050=CIRCLE('',#98188,3.7);
#20051=CIRCLE('',#98189,3.7);
#20052=CIRCLE('',#98190,8.624);
#20053=CIRCLE('',#98191,3.7);
#20054=CIRCLE('',#98192,3.7);
#20055=CIRCLE('',#98193,8.624);
#20056=CIRCLE('',#98194,3.7);
#20057=CIRCLE('',#98195,3.7);
#20058=CIRCLE('',#98196,8.624);
#20059=CIRCLE('',#98197,3.7);
#20060=CIRCLE('',#98198,3.7);
#20061=CIRCLE('',#98199,8.624);
#20062=CIRCLE('',#98200,3.7);
#20063=CIRCLE('',#98201,3.7);
#20064=CIRCLE('',#98202,8.624);
#20065=CIRCLE('',#98203,3.7);
#20066=CIRCLE('',#98204,3.7);
#20067=CIRCLE('',#98205,8.624);
#20068=CIRCLE('',#98206,3.7);
#20069=CIRCLE('',#98207,3.7);
#20070=CIRCLE('',#98208,8.624);
#20071=CIRCLE('',#98209,3.7);
#20072=CIRCLE('',#98210,3.7);
#20073=CIRCLE('',#98211,8.624);
#20074=CIRCLE('',#98212,3.7);
#20075=CIRCLE('',#98213,3.7);
#20076=CIRCLE('',#98214,8.624);
#20077=CIRCLE('',#98215,3.7);
#20078=CIRCLE('',#98216,3.7);
#20079=CIRCLE('',#98217,8.624);
#20080=CIRCLE('',#98218,3.7);
#20081=CIRCLE('',#98219,3.7);
#20082=CIRCLE('',#98220,8.624);
#20083=CIRCLE('',#98221,3.7);
#20084=CIRCLE('',#98222,3.7);
#20085=CIRCLE('',#98223,8.624);
#20086=CIRCLE('',#98224,3.7);
#20087=CIRCLE('',#98225,3.7);
#20088=CIRCLE('',#98226,8.624);
#20089=CIRCLE('',#98227,3.7);
#20090=CIRCLE('',#98228,3.7);
#20091=CIRCLE('',#98229,8.624);
#20092=CIRCLE('',#98230,3.7);
#20093=CIRCLE('',#98231,3.7);
#20094=CIRCLE('',#98232,8.624);
#20095=CIRCLE('',#98233,3.7);
#20096=CIRCLE('',#98234,8.624);
#20097=CIRCLE('',#98235,3.7);
#20098=CIRCLE('',#98236,8.624);
#20099=CIRCLE('',#98237,3.7);
#20100=CIRCLE('',#98238,3.7);
#20101=CIRCLE('',#98239,8.624);
#20102=CIRCLE('',#98240,3.7);
#20103=CIRCLE('',#98241,3.7);
#20104=CIRCLE('',#98242,8.624);
#20105=CIRCLE('',#98243,3.7);
#20106=CIRCLE('',#98244,3.7);
#20107=CIRCLE('',#98245,8.624);
#20108=CIRCLE('',#98246,3.7);
#20109=CIRCLE('',#98247,3.7);
#20110=CIRCLE('',#98248,8.624);
#20111=CIRCLE('',#98249,3.7);
#20112=CIRCLE('',#98250,3.7);
#20113=CIRCLE('',#98251,8.624);
#20114=CIRCLE('',#98252,3.7);
#20115=CIRCLE('',#98253,3.7);
#20116=CIRCLE('',#98254,8.624);
#20117=CIRCLE('',#98255,3.7);
#20118=CIRCLE('',#98256,3.7);
#20119=CIRCLE('',#98257,8.624);
#20120=CIRCLE('',#98372,0.4);
#20121=CIRCLE('',#98373,0.4);
#20122=CIRCLE('',#98375,5.);
#20123=CIRCLE('',#98376,5.);
#20124=CIRCLE('',#98378,0.4);
#20125=CIRCLE('',#98379,0.4);
#20126=CIRCLE('',#98382,0.4);
#20127=CIRCLE('',#98384,7.2);
#20128=CIRCLE('',#98385,7.2);
#20129=CIRCLE('',#98388,0.4);
#20130=CIRCLE('',#98389,0.4);
#20131=CIRCLE('',#98392,7.2);
#20132=CIRCLE('',#98393,7.2);
#20133=CIRCLE('',#98395,0.4);
#20134=CIRCLE('',#98398,0.4);
#20135=CIRCLE('',#98399,0.4);
#20136=CIRCLE('',#98401,5.);
#20137=CIRCLE('',#98402,5.);
#20138=CIRCLE('',#98405,0.2);
#20139=CIRCLE('',#98406,0.2);
#20140=CIRCLE('',#98408,0.2);
#20141=CIRCLE('',#98411,0.2);
#20142=CIRCLE('',#98413,0.2);
#20143=CIRCLE('',#98415,0.2);
#20144=CIRCLE('',#98418,0.2);
#20145=CIRCLE('',#98419,0.2);
#20146=CIRCLE('',#98421,0.2);
#20147=CIRCLE('',#98424,0.2);
#20148=CIRCLE('',#98426,0.2);
#20149=CIRCLE('',#98428,0.2);
#20150=CIRCLE('',#98434,11.5);
#20151=CIRCLE('',#98435,11.5);
#20152=CIRCLE('',#98437,10.375);
#20153=CIRCLE('',#98438,10.375);
#20154=CIRCLE('',#98440,11.5);
#20155=CIRCLE('',#98441,11.5);
#20156=CIRCLE('',#98443,10.375);
#20157=CIRCLE('',#98444,10.375);
#20158=CIRCLE('',#98446,11.5);
#20159=CIRCLE('',#98447,11.5);
#20160=CIRCLE('',#98449,10.375);
#20161=CIRCLE('',#98450,10.375);
#20162=CIRCLE('',#98452,11.5);
#20163=CIRCLE('',#98453,11.5);
#20164=CIRCLE('',#98455,10.375);
#20165=CIRCLE('',#98456,10.375);
#20166=CIRCLE('',#98458,11.5);
#20167=CIRCLE('',#98459,11.5);
#20168=CIRCLE('',#98461,10.375);
#20169=CIRCLE('',#98462,10.375);
#20170=CIRCLE('',#98464,11.5);
#20171=CIRCLE('',#98465,11.5);
#20172=CIRCLE('',#98467,10.375);
#20173=CIRCLE('',#98468,10.375);
#20174=CIRCLE('',#98470,11.5);
#20175=CIRCLE('',#98471,11.5);
#20176=CIRCLE('',#98473,10.375);
#20177=CIRCLE('',#98474,10.375);
#20178=CIRCLE('',#98476,11.5);
#20179=CIRCLE('',#98477,11.5);
#20180=CIRCLE('',#98479,10.375);
#20181=CIRCLE('',#98480,10.375);
#20182=CIRCLE('',#98482,11.5);
#20183=CIRCLE('',#98483,11.5);
#20184=CIRCLE('',#98485,10.375);
#20185=CIRCLE('',#98486,10.375);
#20186=CIRCLE('',#98488,11.5);
#20187=CIRCLE('',#98489,11.5);
#20188=CIRCLE('',#98491,10.375);
#20189=CIRCLE('',#98492,10.375);
#20190=CIRCLE('',#98494,11.5);
#20191=CIRCLE('',#98495,11.5);
#20192=CIRCLE('',#98497,10.375);
#20193=CIRCLE('',#98498,10.375);
#20194=CIRCLE('',#98500,11.5);
#20195=CIRCLE('',#98501,11.5);
#20196=CIRCLE('',#98503,10.375);
#20197=CIRCLE('',#98504,10.375);
#20198=CIRCLE('',#98506,11.5);
#20199=CIRCLE('',#98507,11.5);
#20200=CIRCLE('',#98509,10.375);
#20201=CIRCLE('',#98510,10.375);
#20202=CIRCLE('',#98512,11.5);
#20203=CIRCLE('',#98513,11.5);
#20204=CIRCLE('',#98515,10.375);
#20205=CIRCLE('',#98516,10.375);
#20206=CIRCLE('',#98518,11.5);
#20207=CIRCLE('',#98519,11.5);
#20208=CIRCLE('',#98521,10.375);
#20209=CIRCLE('',#98522,10.375);
#20210=CIRCLE('',#98524,11.5);
#20211=CIRCLE('',#98525,11.5);
#20212=CIRCLE('',#98527,10.375);
#20213=CIRCLE('',#98528,10.375);
#20214=CIRCLE('',#98530,11.5);
#20215=CIRCLE('',#98531,11.5);
#20216=CIRCLE('',#98533,10.375);
#20217=CIRCLE('',#98534,10.375);
#20218=CIRCLE('',#98536,11.5);
#20219=CIRCLE('',#98537,11.5);
#20220=CIRCLE('',#98539,10.375);
#20221=CIRCLE('',#98540,10.375);
#20222=CIRCLE('',#98542,11.5);
#20223=CIRCLE('',#98543,11.5);
#20224=CIRCLE('',#98545,10.375);
#20225=CIRCLE('',#98546,10.375);
#20226=CIRCLE('',#98548,11.5);
#20227=CIRCLE('',#98549,11.5);
#20228=CIRCLE('',#98551,10.375);
#20229=CIRCLE('',#98552,10.375);
#20230=CIRCLE('',#98554,11.5);
#20231=CIRCLE('',#98555,11.5);
#20232=CIRCLE('',#98557,10.375);
#20233=CIRCLE('',#98558,10.375);
#20234=CIRCLE('',#98560,11.5);
#20235=CIRCLE('',#98561,11.5);
#20236=CIRCLE('',#98563,10.375);
#20237=CIRCLE('',#98564,10.375);
#20238=CIRCLE('',#98566,11.5);
#20239=CIRCLE('',#98567,11.5);
#20240=CIRCLE('',#98569,10.375);
#20241=CIRCLE('',#98570,10.375);
#20242=CIRCLE('',#98572,11.5);
#20243=CIRCLE('',#98573,11.5);
#20244=CIRCLE('',#98575,10.375);
#20245=CIRCLE('',#98576,10.375);
#20246=CIRCLE('',#98578,11.5);
#20247=CIRCLE('',#98579,11.5);
#20248=CIRCLE('',#98581,10.375);
#20249=CIRCLE('',#98582,10.375);
#20250=CIRCLE('',#98584,11.5);
#20251=CIRCLE('',#98585,11.5);
#20252=CIRCLE('',#98587,10.375);
#20253=CIRCLE('',#98588,10.375);
#20254=CIRCLE('',#98590,11.5);
#20255=CIRCLE('',#98591,11.5);
#20256=CIRCLE('',#98593,10.375);
#20257=CIRCLE('',#98594,10.375);
#20258=CIRCLE('',#98596,11.5);
#20259=CIRCLE('',#98597,11.5);
#20260=CIRCLE('',#98599,10.375);
#20261=CIRCLE('',#98600,10.375);
#20262=CIRCLE('',#98602,11.5);
#20263=CIRCLE('',#98603,11.5);
#20264=CIRCLE('',#98605,10.375);
#20265=CIRCLE('',#98606,10.375);
#20266=CIRCLE('',#98608,11.5);
#20267=CIRCLE('',#98609,11.5);
#20268=CIRCLE('',#98611,10.375);
#20269=CIRCLE('',#98612,10.375);
#20270=CIRCLE('',#98614,11.5);
#20271=CIRCLE('',#98615,11.5);
#20272=CIRCLE('',#98617,10.375);
#20273=CIRCLE('',#98618,10.375);
#20274=CIRCLE('',#98620,11.5);
#20275=CIRCLE('',#98621,11.5);
#20276=CIRCLE('',#98623,10.375);
#20277=CIRCLE('',#98624,10.375);
#20278=CIRCLE('',#98626,11.5);
#20279=CIRCLE('',#98627,11.5);
#20280=CIRCLE('',#98629,10.375);
#20281=CIRCLE('',#98630,10.375);
#20282=CIRCLE('',#98632,11.5);
#20283=CIRCLE('',#98633,11.5);
#20284=CIRCLE('',#98635,10.375);
#20285=CIRCLE('',#98636,10.375);
#20286=CIRCLE('',#98638,11.5);
#20287=CIRCLE('',#98639,11.5);
#20288=CIRCLE('',#98641,10.375);
#20289=CIRCLE('',#98642,10.375);
#20290=CIRCLE('',#98644,11.5);
#20291=CIRCLE('',#98645,11.5);
#20292=CIRCLE('',#98647,10.375);
#20293=CIRCLE('',#98648,10.375);
#20294=CIRCLE('',#98650,11.5);
#20295=CIRCLE('',#98651,11.5);
#20296=CIRCLE('',#98653,10.375);
#20297=CIRCLE('',#98654,10.375);
#20298=CIRCLE('',#98656,11.5);
#20299=CIRCLE('',#98657,11.5);
#20300=CIRCLE('',#98659,10.375);
#20301=CIRCLE('',#98660,10.375);
#20302=CIRCLE('',#98662,11.5);
#20303=CIRCLE('',#98663,11.5);
#20304=CIRCLE('',#98665,10.375);
#20305=CIRCLE('',#98666,10.375);
#20306=CIRCLE('',#98668,11.5);
#20307=CIRCLE('',#98669,11.5);
#20308=CIRCLE('',#98671,10.375);
#20309=CIRCLE('',#98672,10.375);
#20310=CIRCLE('',#98674,11.5);
#20311=CIRCLE('',#98675,11.5);
#20312=CIRCLE('',#98677,10.375);
#20313=CIRCLE('',#98678,10.375);
#20314=CIRCLE('',#98680,11.5);
#20315=CIRCLE('',#98681,11.5);
#20316=CIRCLE('',#98683,10.375);
#20317=CIRCLE('',#98684,10.375);
#20318=CIRCLE('',#98686,11.5);
#20319=CIRCLE('',#98687,11.5);
#20320=CIRCLE('',#98689,10.375);
#20321=CIRCLE('',#98690,10.375);
#20322=CIRCLE('',#98691,11.5);
#20323=CIRCLE('',#98692,3.5);
#20324=CIRCLE('',#98694,10.375);
#20325=CIRCLE('',#98696,10.375);
#20326=CIRCLE('',#98698,11.5);
#20327=CIRCLE('',#98700,3.5);
#20328=CIRCLE('',#98703,1.5);
#20329=CIRCLE('',#98704,1.5);
#20330=CIRCLE('',#98706,1.5);
#20331=CIRCLE('',#98707,1.5);
#20332=CIRCLE('',#98711,3.625);
#20333=CIRCLE('',#98712,4.75);
#20334=CIRCLE('',#98713,3.625);
#20335=CIRCLE('',#98714,4.75);
#20336=CIRCLE('',#98715,3.625);
#20337=CIRCLE('',#98716,4.75);
#20338=CIRCLE('',#98717,3.625);
#20339=CIRCLE('',#98718,4.75);
#20340=CIRCLE('',#98719,3.625);
#20341=CIRCLE('',#98720,4.75);
#20342=CIRCLE('',#98721,3.625);
#20343=CIRCLE('',#98722,4.75);
#20344=CIRCLE('',#98723,3.625);
#20345=CIRCLE('',#98724,4.75);
#20346=CIRCLE('',#98725,3.625);
#20347=CIRCLE('',#98726,4.75);
#20348=CIRCLE('',#98727,3.625);
#20349=CIRCLE('',#98728,4.75);
#20350=CIRCLE('',#98729,3.625);
#20351=CIRCLE('',#98730,4.75);
#20352=CIRCLE('',#98731,3.625);
#20353=CIRCLE('',#98732,4.75);
#20354=CIRCLE('',#98733,3.625);
#20355=CIRCLE('',#98734,4.75);
#20356=CIRCLE('',#98735,3.625);
#20357=CIRCLE('',#98736,4.75);
#20358=CIRCLE('',#98737,3.625);
#20359=CIRCLE('',#98738,4.75);
#20360=CIRCLE('',#98739,3.625);
#20361=CIRCLE('',#98740,4.75);
#20362=CIRCLE('',#98741,3.625);
#20363=CIRCLE('',#98742,4.75);
#20364=CIRCLE('',#98743,3.625);
#20365=CIRCLE('',#98744,4.75);
#20366=CIRCLE('',#98745,3.5);
#20367=CIRCLE('',#98747,3.);
#20368=CIRCLE('',#98748,3.);
#20369=CIRCLE('',#98751,4.75);
#20370=CIRCLE('',#98754,3.625);
#20371=CIRCLE('',#98757,4.75);
#20372=CIRCLE('',#98760,3.625);
#20373=CIRCLE('',#98763,4.75);
#20374=CIRCLE('',#98766,3.625);
#20375=CIRCLE('',#98769,4.75);
#20376=CIRCLE('',#98772,3.625);
#20377=CIRCLE('',#98775,4.75);
#20378=CIRCLE('',#98778,3.625);
#20379=CIRCLE('',#98781,4.75);
#20380=CIRCLE('',#98784,3.625);
#20381=CIRCLE('',#98787,4.75);
#20382=CIRCLE('',#98790,3.625);
#20383=CIRCLE('',#98793,4.75);
#20384=CIRCLE('',#98796,3.625);
#20385=CIRCLE('',#98799,4.75);
#20386=CIRCLE('',#98802,3.625);
#20387=CIRCLE('',#98803,4.75);
#20388=CIRCLE('',#98804,3.625);
#20389=CIRCLE('',#98805,4.75);
#20390=CIRCLE('',#98806,3.625);
#20391=CIRCLE('',#98807,4.75);
#20392=CIRCLE('',#98808,3.625);
#20393=CIRCLE('',#98809,4.75);
#20394=CIRCLE('',#98810,3.625);
#20395=CIRCLE('',#98811,4.75);
#20396=CIRCLE('',#98812,3.625);
#20397=CIRCLE('',#98813,4.75);
#20398=CIRCLE('',#98814,3.625);
#20399=CIRCLE('',#98815,4.75);
#20400=CIRCLE('',#98816,3.625);
#20401=CIRCLE('',#98817,4.75);
#20402=CIRCLE('',#98818,3.625);
#20403=CIRCLE('',#98854,3.5);
#20404=CIRCLE('',#98858,1.76666666666667);
#20405=CIRCLE('',#98859,0.166666666666667);
#20406=CIRCLE('',#98860,1.6);
#20407=CIRCLE('',#98862,2.23333333333333);
#20408=CIRCLE('',#98864,1.6);
#20409=CIRCLE('',#98865,1.6);
#20410=CIRCLE('',#98866,1.6);
#20411=CIRCLE('',#98867,1.6);
#20412=CIRCLE('',#98868,1.6);
#20413=CIRCLE('',#98869,1.6);
#20414=CIRCLE('',#98870,1.6);
#20415=CIRCLE('',#98871,1.6);
#20416=CIRCLE('',#98872,1.6);
#20417=CIRCLE('',#98873,1.6);
#20418=CIRCLE('',#98874,1.6);
#20419=CIRCLE('',#98875,1.6);
#20420=CIRCLE('',#98876,1.6);
#20421=CIRCLE('',#98877,1.6);
#20422=CIRCLE('',#98878,1.6);
#20423=CIRCLE('',#98879,1.6);
#20424=CIRCLE('',#98880,1.6);
#20425=CIRCLE('',#98881,1.6);
#20426=CIRCLE('',#98882,1.6);
#20427=CIRCLE('',#98883,1.6);
#20428=CIRCLE('',#98885,0.166666666666667);
#20429=CIRCLE('',#98886,2.4);
#20430=CIRCLE('',#98887,2.4);
#20431=CIRCLE('',#98889,2.4);
#20432=CIRCLE('',#98890,2.4);
#20433=CIRCLE('',#98891,2.4);
#20434=CIRCLE('',#98892,2.4);
#20435=CIRCLE('',#98893,2.4);
#20436=CIRCLE('',#98894,2.4);
#20437=CIRCLE('',#98895,2.4);
#20438=CIRCLE('',#98896,2.4);
#20439=CIRCLE('',#98897,2.4);
#20440=CIRCLE('',#98898,2.4);
#20441=CIRCLE('',#98899,2.4);
#20442=CIRCLE('',#98900,2.4);
#20443=CIRCLE('',#98901,2.4);
#20444=CIRCLE('',#98902,2.4);
#20445=CIRCLE('',#98903,2.4);
#20446=CIRCLE('',#98904,2.4);
#20447=CIRCLE('',#98905,2.4);
#20448=CIRCLE('',#98906,2.4);
#20449=CIRCLE('',#98907,2.4);
#20450=CIRCLE('',#98909,2.23333333333333);
#20451=CIRCLE('',#98910,0.166666666666667);
#20452=CIRCLE('',#98912,1.76666666666667);
#20453=CIRCLE('',#98914,0.166666666666667);
#20454=CIRCLE('',#98916,0.525);
#20455=CIRCLE('',#98917,0.525);
#20456=CIRCLE('',#98919,0.525);
#20457=CIRCLE('',#98921,0.525);
#20458=CIRCLE('',#98924,0.525);
#20459=CIRCLE('',#98925,0.525);
#20460=CIRCLE('',#98927,0.525);
#20461=CIRCLE('',#98929,0.525);
#20462=CIRCLE('',#98932,0.525);
#20463=CIRCLE('',#98933,0.525);
#20464=CIRCLE('',#98935,0.525);
#20465=CIRCLE('',#98937,0.525);
#20466=CIRCLE('',#98940,0.525);
#20467=CIRCLE('',#98941,0.525);
#20468=CIRCLE('',#98943,0.525);
#20469=CIRCLE('',#98945,0.525);
#20470=CIRCLE('',#98948,0.525);
#20471=CIRCLE('',#98949,0.525);
#20472=CIRCLE('',#98951,0.525);
#20473=CIRCLE('',#98953,0.525);
#20474=CIRCLE('',#98956,0.525);
#20475=CIRCLE('',#98957,0.525);
#20476=CIRCLE('',#98959,0.525);
#20477=CIRCLE('',#98961,0.525);
#20478=CIRCLE('',#98964,0.525);
#20479=CIRCLE('',#98965,0.525);
#20480=CIRCLE('',#98967,0.525);
#20481=CIRCLE('',#98969,0.525);
#20482=CIRCLE('',#98972,0.525);
#20483=CIRCLE('',#98973,0.525);
#20484=CIRCLE('',#98975,0.525);
#20485=CIRCLE('',#98977,0.525);
#20486=CIRCLE('',#98980,0.5);
#20487=CIRCLE('',#98981,0.475);
#20488=CIRCLE('',#98983,0.5);
#20489=CIRCLE('',#98986,0.475);
#20490=CIRCLE('',#98989,0.5);
#20491=CIRCLE('',#98990,0.475);
#20492=CIRCLE('',#98992,0.5);
#20493=CIRCLE('',#98995,0.475);
#20494=CIRCLE('',#98998,0.5);
#20495=CIRCLE('',#98999,0.475);
#20496=CIRCLE('',#99001,0.5);
#20497=CIRCLE('',#99004,0.475);
#20498=CIRCLE('',#99007,0.5);
#20499=CIRCLE('',#99008,0.475);
#20500=CIRCLE('',#99010,0.5);
#20501=CIRCLE('',#99013,0.475);
#20502=CIRCLE('',#99016,0.5);
#20503=CIRCLE('',#99017,0.475);
#20504=CIRCLE('',#99019,0.5);
#20505=CIRCLE('',#99022,0.475);
#20506=CIRCLE('',#99025,0.5);
#20507=CIRCLE('',#99026,0.475);
#20508=CIRCLE('',#99028,0.5);
#20509=CIRCLE('',#99031,0.475);
#20510=CIRCLE('',#99034,0.5);
#20511=CIRCLE('',#99035,0.475);
#20512=CIRCLE('',#99037,0.5);
#20513=CIRCLE('',#99040,0.475);
#20514=CIRCLE('',#99043,0.5);
#20515=CIRCLE('',#99044,0.475);
#20516=CIRCLE('',#99046,0.5);
#20517=CIRCLE('',#99049,0.475);
#20518=CIRCLE('',#99054,1.17524047358083);
#20519=CIRCLE('',#99086,1.17524047357586);
#20520=CIRCLE('',#99088,1.5);
#20521=CIRCLE('',#99120,1.15470053837925);
#20522=CIRCLE('',#99122,2.75);
#20523=CIRCLE('',#99123,1.5);
#20524=CIRCLE('',#99125,3.5);
#20525=CIRCLE('',#99126,3.5);
#20526=CIRCLE('',#99128,1.17524047357586);
#20527=CIRCLE('',#99129,1.5);
#20528=CIRCLE('',#99130,1.125);
#20529=CIRCLE('',#99136,1.15470053837925);
#20530=CIRCLE('',#99137,1.15470053837925);
#20531=CIRCLE('',#99138,1.15470053837925);
#20532=CIRCLE('',#99139,1.15470053837925);
#20533=CIRCLE('',#99140,1.15470053837925);
#20534=CIRCLE('',#99173,2.40384615384615);
#20535=CIRCLE('',#99174,2.40384615384615);
#20536=CIRCLE('',#99176,2.40384615384615);
#20537=CIRCLE('',#99177,0.576463888168111);
#20538=CIRCLE('',#99179,2.40384615384615);
#20539=CIRCLE('',#99181,3.);
#20540=CIRCLE('',#99182,2.875);
#20541=CIRCLE('',#99184,3.);
#20542=CIRCLE('',#99185,3.);
#20543=CIRCLE('',#99187,2.875);
#20544=CIRCLE('',#99191,2.09615384615385);
#20545=CIRCLE('',#99192,0.57646388816811);
#20546=CIRCLE('',#99193,2.09615384615385);
#20547=CIRCLE('',#99195,1.5);
#20548=CIRCLE('',#99196,1.625);
#20549=CIRCLE('',#99198,1.5);
#20550=CIRCLE('',#99199,1.5);
#20551=CIRCLE('',#99201,1.625);
#20552=CIRCLE('',#99203,2.09615384615385);
#20553=CIRCLE('',#99205,2.09615384615385);
#20554=CIRCLE('',#99209,0.576463888168111);
#20555=CIRCLE('',#99211,0.576463888168111);
#20556=CIRCLE('',#99213,0.576463888168111);
#20557=CIRCLE('',#99215,0.576463888168111);
#20558=CIRCLE('',#99217,0.576463888168111);
#20559=CIRCLE('',#99219,0.576463888168111);
#20560=CIRCLE('',#99221,0.576463888168111);
#20561=CIRCLE('',#99223,0.576463888168111);
#20562=CIRCLE('',#99225,0.576463888168111);
#20563=CIRCLE('',#99227,0.576463888168111);
#20564=CIRCLE('',#99229,0.576463888168111);
#20565=CIRCLE('',#99231,0.576463888168111);
#20566=CIRCLE('',#99233,2.40384615384615);
#20567=CIRCLE('',#99234,2.40384615384615);
#20568=CIRCLE('',#99236,2.09615384615385);
#20569=CIRCLE('',#99237,2.09615384615385);
#20570=CIRCLE('',#99241,2.40384615384615);
#20571=CIRCLE('',#99242,2.40384615384615);
#20572=CIRCLE('',#99244,2.09615384615385);
#20573=CIRCLE('',#99245,2.09615384615385);
#20574=CIRCLE('',#99250,1.17524047358089);
#20575=CIRCLE('',#99252,1.17524047358089);
#20576=CIRCLE('',#99268,1.5);
#20577=CIRCLE('',#99284,1.15470053837925);
#20578=CIRCLE('',#99286,2.75);
#20579=CIRCLE('',#99287,1.5);
#20580=CIRCLE('',#99289,3.5);
#20581=CIRCLE('',#99290,3.5);
#20582=CIRCLE('',#99292,1.5);
#20583=CIRCLE('',#99293,1.125);
#20584=CIRCLE('',#99297,1.17524047358083);
#20585=CIRCLE('',#99300,1.15470053837925);
#20586=CIRCLE('',#99301,1.15470053837925);
#20587=CIRCLE('',#99302,1.15470053837925);
#20588=CIRCLE('',#99303,1.15470053837925);
#20589=CIRCLE('',#99304,1.15470053837925);
#20590=CIRCLE('',#99320,0.957716426222737);
#20591=CIRCLE('',#99335,0.957716426224497);
#20592=CIRCLE('',#99337,1.25000000000001);
#20593=CIRCLE('',#99352,0.957716426224497);
#20594=CIRCLE('',#99353,0.912499999999999);
#20595=CIRCLE('',#99355,1.25000000000001);
#20596=CIRCLE('',#99357,0.866025403784441);
#20597=CIRCLE('',#99359,2.5);
#20598=CIRCLE('',#99360,2.5);
#20599=CIRCLE('',#99362,1.075);
#20600=CIRCLE('',#99363,1.075);
#20601=CIRCLE('',#99365,0.866025403784441);
#20602=CIRCLE('',#99366,0.866025403784441);
#20603=CIRCLE('',#99367,0.866025403784441);
#20604=CIRCLE('',#99368,0.866025403784441);
#20605=CIRCLE('',#99369,0.866025403784441);
#20606=CIRCLE('',#99387,1.17524047358083);
#20607=CIRCLE('',#99417,1.5);
#20608=CIRCLE('',#99418,1.5);
#20609=CIRCLE('',#99419,1.5);
#20610=CIRCLE('',#99448,1.17524047358085);
#20611=CIRCLE('',#99450,1.17524047358083);
#20612=CIRCLE('',#99452,1.17524047358083);
#20613=CIRCLE('',#99453,1.5);
#20614=CIRCLE('',#99457,0.125);
#20615=CIRCLE('',#99458,1.625);
#20616=CIRCLE('',#99460,1.25);
#20617=CIRCLE('',#99461,1.25);
#20618=CIRCLE('',#99462,1.25);
#20619=CIRCLE('',#99463,1.25);
#20620=CIRCLE('',#99464,1.25);
#20621=CIRCLE('',#99465,1.25);
#20622=CIRCLE('',#99467,1.44337567297406);
#20623=CIRCLE('',#99469,2.54610912703474);
#20624=CIRCLE('',#99470,0.0550000000000003);
#20625=CIRCLE('',#99471,2.50721825406948);
#20626=CIRCLE('',#99473,2.73389087296526);
#20627=CIRCLE('',#99475,2.75);
#20628=CIRCLE('',#99476,0.0550000000000007);
#20629=CIRCLE('',#99478,2.73389087296526);
#20630=CIRCLE('',#99480,2.73389087296526);
#20631=CIRCLE('',#99482,2.73389087296526);
#20632=CIRCLE('',#99484,2.73389087296526);
#20633=CIRCLE('',#99486,2.73389087296526);
#20634=CIRCLE('',#99488,2.73389087296526);
#20635=CIRCLE('',#99490,2.73389087296526);
#20636=CIRCLE('',#99492,2.73389087296526);
#20637=CIRCLE('',#99494,2.73389087296526);
#20638=CIRCLE('',#99496,2.73389087296526);
#20639=CIRCLE('',#99498,2.73389087296526);
#20640=CIRCLE('',#99500,2.73389087296526);
#20641=CIRCLE('',#99502,2.73389087296526);
#20642=CIRCLE('',#99504,2.73389087296526);
#20643=CIRCLE('',#99506,2.73389087296526);
#20644=CIRCLE('',#99508,2.73389087296526);
#20645=CIRCLE('',#99510,2.73389087296526);
#20646=CIRCLE('',#99512,2.73389087296526);
#20647=CIRCLE('',#99514,2.73389087296526);
#20648=CIRCLE('',#99516,2.73389087296526);
#20649=CIRCLE('',#99518,2.73389087296526);
#20650=CIRCLE('',#99520,2.73389087296526);
#20651=CIRCLE('',#99522,2.73389087296526);
#20652=CIRCLE('',#99524,2.73389087296526);
#20653=CIRCLE('',#99526,2.73389087296526);
#20654=CIRCLE('',#99528,2.73389087296526);
#20655=CIRCLE('',#99530,2.73389087296526);
#20656=CIRCLE('',#99532,2.73389087296526);
#20657=CIRCLE('',#99534,2.73389087296526);
#20658=CIRCLE('',#99536,2.73389087296526);
#20659=CIRCLE('',#99538,2.73389087296526);
#20660=CIRCLE('',#99540,2.73389087296526);
#20661=CIRCLE('',#99542,2.73389087296526);
#20662=CIRCLE('',#99544,2.73389087296526);
#20663=CIRCLE('',#99546,2.73389087296526);
#20664=CIRCLE('',#99548,2.73389087296526);
#20665=CIRCLE('',#99550,2.73389087296526);
#20666=CIRCLE('',#99552,2.73389087296526);
#20667=CIRCLE('',#99554,2.73389087296526);
#20668=CIRCLE('',#99556,2.73389087296526);
#20669=CIRCLE('',#99558,2.73389087296526);
#20670=CIRCLE('',#99560,2.73389087296526);
#20671=CIRCLE('',#99562,2.73389087296526);
#20672=CIRCLE('',#99564,2.73389087296526);
#20673=CIRCLE('',#99566,2.73389087296526);
#20674=CIRCLE('',#99568,2.73389087296526);
#20675=CIRCLE('',#99570,2.73389087296526);
#20676=CIRCLE('',#99572,2.73389087296526);
#20677=CIRCLE('',#99574,2.73389087296526);
#20678=CIRCLE('',#99576,2.73389087296526);
#20679=CIRCLE('',#99577,2.54610912703474);
#20680=CIRCLE('',#99578,2.54610912703474);
#20681=CIRCLE('',#99579,2.73389087296526);
#20682=CIRCLE('',#99581,2.73389087296526);
#20683=CIRCLE('',#99583,2.73389087296526);
#20684=CIRCLE('',#99585,2.73389087296526);
#20685=CIRCLE('',#99587,2.73389087296526);
#20686=CIRCLE('',#99589,2.73389087296526);
#20687=CIRCLE('',#99591,2.73389087296526);
#20688=CIRCLE('',#99593,2.73389087296526);
#20689=CIRCLE('',#99595,2.73389087296526);
#20690=CIRCLE('',#99597,2.73389087296526);
#20691=CIRCLE('',#99599,2.73389087296526);
#20692=CIRCLE('',#99601,2.73389087296526);
#20693=CIRCLE('',#99603,2.73389087296526);
#20694=CIRCLE('',#99605,2.73389087296526);
#20695=CIRCLE('',#99607,2.73389087296526);
#20696=CIRCLE('',#99609,2.73389087296526);
#20697=CIRCLE('',#99611,2.73389087296526);
#20698=CIRCLE('',#99613,2.73389087296526);
#20699=CIRCLE('',#99615,2.73389087296526);
#20700=CIRCLE('',#99617,2.73389087296526);
#20701=CIRCLE('',#99619,2.73389087296526);
#20702=CIRCLE('',#99621,2.73389087296526);
#20703=CIRCLE('',#99623,2.73389087296526);
#20704=CIRCLE('',#99625,2.73389087296526);
#20705=CIRCLE('',#99627,2.73389087296526);
#20706=CIRCLE('',#99629,2.73389087296526);
#20707=CIRCLE('',#99631,2.73389087296526);
#20708=CIRCLE('',#99633,2.73389087296526);
#20709=CIRCLE('',#99635,2.73389087296526);
#20710=CIRCLE('',#99637,2.73389087296526);
#20711=CIRCLE('',#99639,2.73389087296526);
#20712=CIRCLE('',#99641,2.73389087296526);
#20713=CIRCLE('',#99643,2.73389087296526);
#20714=CIRCLE('',#99645,2.73389087296526);
#20715=CIRCLE('',#99647,2.73389087296526);
#20716=CIRCLE('',#99649,2.73389087296526);
#20717=CIRCLE('',#99651,2.73389087296526);
#20718=CIRCLE('',#99653,2.73389087296526);
#20719=CIRCLE('',#99655,2.73389087296526);
#20720=CIRCLE('',#99657,2.73389087296526);
#20721=CIRCLE('',#99659,2.73389087296526);
#20722=CIRCLE('',#99661,2.73389087296526);
#20723=CIRCLE('',#99663,2.73389087296526);
#20724=CIRCLE('',#99665,2.73389087296526);
#20725=CIRCLE('',#99667,2.73389087296526);
#20726=CIRCLE('',#99669,2.73389087296526);
#20727=CIRCLE('',#99671,2.73389087296526);
#20728=CIRCLE('',#99673,2.73389087296526);
#20729=CIRCLE('',#99675,2.73389087296526);
#20730=CIRCLE('',#99678,2.50721825406948);
#20731=CIRCLE('',#99679,0.0549999999999999);
#20732=CIRCLE('',#99681,2.75);
#20733=CIRCLE('',#99683,2.75);
#20734=CIRCLE('',#99685,2.75);
#20735=CIRCLE('',#99687,2.75);
#20736=CIRCLE('',#99689,2.75);
#20737=CIRCLE('',#99691,2.75);
#20738=CIRCLE('',#99693,2.75);
#20739=CIRCLE('',#99695,2.75);
#20740=CIRCLE('',#99697,2.75);
#20741=CIRCLE('',#99699,2.75);
#20742=CIRCLE('',#99701,2.75);
#20743=CIRCLE('',#99703,2.75);
#20744=CIRCLE('',#99705,2.75);
#20745=CIRCLE('',#99707,2.75);
#20746=CIRCLE('',#99709,2.75);
#20747=CIRCLE('',#99711,2.75);
#20748=CIRCLE('',#99713,2.75);
#20749=CIRCLE('',#99715,2.75);
#20750=CIRCLE('',#99717,2.75);
#20751=CIRCLE('',#99719,2.75);
#20752=CIRCLE('',#99721,2.75);
#20753=CIRCLE('',#99723,2.75);
#20754=CIRCLE('',#99725,2.75);
#20755=CIRCLE('',#99727,2.75);
#20756=CIRCLE('',#99729,2.75);
#20757=CIRCLE('',#99731,2.75);
#20758=CIRCLE('',#99733,2.75);
#20759=CIRCLE('',#99735,2.75);
#20760=CIRCLE('',#99737,2.75);
#20761=CIRCLE('',#99739,2.75);
#20762=CIRCLE('',#99741,2.75);
#20763=CIRCLE('',#99743,2.75);
#20764=CIRCLE('',#99745,2.75);
#20765=CIRCLE('',#99747,2.75);
#20766=CIRCLE('',#99749,2.75);
#20767=CIRCLE('',#99751,2.75);
#20768=CIRCLE('',#99753,2.75);
#20769=CIRCLE('',#99755,2.75);
#20770=CIRCLE('',#99757,2.75);
#20771=CIRCLE('',#99759,2.75);
#20772=CIRCLE('',#99761,2.75);
#20773=CIRCLE('',#99763,2.75);
#20774=CIRCLE('',#99765,2.75);
#20775=CIRCLE('',#99767,2.75);
#20776=CIRCLE('',#99769,2.75);
#20777=CIRCLE('',#99771,2.75);
#20778=CIRCLE('',#99773,2.75);
#20779=CIRCLE('',#99775,2.75);
#20780=CIRCLE('',#99777,2.75);
#20781=CIRCLE('',#99779,2.75);
#20782=CIRCLE('',#99781,2.75);
#20783=CIRCLE('',#99783,2.75);
#20784=CIRCLE('',#99785,2.75);
#20785=CIRCLE('',#99787,2.75);
#20786=CIRCLE('',#99789,2.75);
#20787=CIRCLE('',#99791,2.75);
#20788=CIRCLE('',#99793,2.75);
#20789=CIRCLE('',#99795,2.75);
#20790=CIRCLE('',#99797,2.75);
#20791=CIRCLE('',#99799,2.75);
#20792=CIRCLE('',#99801,2.75);
#20793=CIRCLE('',#99803,2.75);
#20794=CIRCLE('',#99805,2.75);
#20795=CIRCLE('',#99807,2.75);
#20796=CIRCLE('',#99809,2.75);
#20797=CIRCLE('',#99811,2.75);
#20798=CIRCLE('',#99813,2.75);
#20799=CIRCLE('',#99815,2.75);
#20800=CIRCLE('',#99817,2.75);
#20801=CIRCLE('',#99819,2.75);
#20802=CIRCLE('',#99821,2.75);
#20803=CIRCLE('',#99823,2.75);
#20804=CIRCLE('',#99825,2.75);
#20805=CIRCLE('',#99827,2.75);
#20806=CIRCLE('',#99829,2.75);
#20807=CIRCLE('',#99831,2.75);
#20808=CIRCLE('',#99833,2.75);
#20809=CIRCLE('',#99835,2.75);
#20810=CIRCLE('',#99837,2.75);
#20811=CIRCLE('',#99839,2.75);
#20812=CIRCLE('',#99841,2.75);
#20813=CIRCLE('',#99843,2.75);
#20814=CIRCLE('',#99845,2.75);
#20815=CIRCLE('',#99847,2.75);
#20816=CIRCLE('',#99849,2.75);
#20817=CIRCLE('',#99851,2.75);
#20818=CIRCLE('',#99853,2.75);
#20819=CIRCLE('',#99855,2.75);
#20820=CIRCLE('',#99857,2.75);
#20821=CIRCLE('',#99859,2.75);
#20822=CIRCLE('',#99861,2.75);
#20823=CIRCLE('',#99863,2.75);
#20824=CIRCLE('',#99865,2.75);
#20825=CIRCLE('',#99867,2.75);
#20826=CIRCLE('',#99869,2.75);
#20827=CIRCLE('',#99871,2.75);
#20828=CIRCLE('',#99873,2.75);
#20829=CIRCLE('',#99875,2.75);
#20830=CIRCLE('',#99877,2.75);
#20831=CIRCLE('',#99878,2.75);
#20832=CIRCLE('',#99880,2.75);
#20833=CIRCLE('',#99882,2.75);
#20834=CIRCLE('',#99884,2.75);
#20835=CIRCLE('',#99886,2.75);
#20836=CIRCLE('',#99888,2.75);
#20837=CIRCLE('',#99890,2.75);
#20838=CIRCLE('',#99892,2.75);
#20839=CIRCLE('',#99894,2.75);
#20840=CIRCLE('',#99896,2.75);
#20841=CIRCLE('',#99898,2.75);
#20842=CIRCLE('',#99900,2.75);
#20843=CIRCLE('',#99902,2.75);
#20844=CIRCLE('',#99904,2.75);
#20845=CIRCLE('',#99906,2.75);
#20846=CIRCLE('',#99908,2.75);
#20847=CIRCLE('',#99910,2.75);
#20848=CIRCLE('',#99912,2.75);
#20849=CIRCLE('',#99914,2.75);
#20850=CIRCLE('',#99916,2.75);
#20851=CIRCLE('',#99918,2.75);
#20852=CIRCLE('',#99920,2.75);
#20853=CIRCLE('',#99922,2.75);
#20854=CIRCLE('',#99924,2.75);
#20855=CIRCLE('',#99926,2.75);
#20856=CIRCLE('',#99928,2.75);
#20857=CIRCLE('',#99930,2.75);
#20858=CIRCLE('',#99932,2.75);
#20859=CIRCLE('',#99934,2.75);
#20860=CIRCLE('',#99936,2.75);
#20861=CIRCLE('',#99938,2.75);
#20862=CIRCLE('',#99940,2.75);
#20863=CIRCLE('',#99942,2.75);
#20864=CIRCLE('',#99944,2.75);
#20865=CIRCLE('',#99946,2.75);
#20866=CIRCLE('',#99948,2.75);
#20867=CIRCLE('',#99950,2.75);
#20868=CIRCLE('',#99952,2.75);
#20869=CIRCLE('',#99954,2.75);
#20870=CIRCLE('',#99956,2.75);
#20871=CIRCLE('',#99958,2.75);
#20872=CIRCLE('',#99960,2.75);
#20873=CIRCLE('',#99962,2.75);
#20874=CIRCLE('',#99964,2.75);
#20875=CIRCLE('',#99966,2.75);
#20876=CIRCLE('',#99968,2.75);
#20877=CIRCLE('',#99970,2.75);
#20878=CIRCLE('',#99972,2.75);
#20879=CIRCLE('',#99974,2.75);
#20880=CIRCLE('',#99976,2.75);
#20881=CIRCLE('',#99978,2.75);
#20882=CIRCLE('',#99980,2.75);
#20883=CIRCLE('',#99982,2.75);
#20884=CIRCLE('',#99984,2.75);
#20885=CIRCLE('',#99986,2.75);
#20886=CIRCLE('',#99988,2.75);
#20887=CIRCLE('',#99990,2.75);
#20888=CIRCLE('',#99992,2.75);
#20889=CIRCLE('',#99994,2.75);
#20890=CIRCLE('',#99996,2.75);
#20891=CIRCLE('',#99998,2.75);
#20892=CIRCLE('',#100000,2.75);
#20893=CIRCLE('',#100002,2.75);
#20894=CIRCLE('',#100004,2.75);
#20895=CIRCLE('',#100006,2.75);
#20896=CIRCLE('',#100008,2.75);
#20897=CIRCLE('',#100010,2.75);
#20898=CIRCLE('',#100012,2.75);
#20899=CIRCLE('',#100014,2.75);
#20900=CIRCLE('',#100016,2.75);
#20901=CIRCLE('',#100018,2.75);
#20902=CIRCLE('',#100020,2.75);
#20903=CIRCLE('',#100022,2.75);
#20904=CIRCLE('',#100024,2.75);
#20905=CIRCLE('',#100026,2.75);
#20906=CIRCLE('',#100028,2.75);
#20907=CIRCLE('',#100030,2.75);
#20908=CIRCLE('',#100032,2.75);
#20909=CIRCLE('',#100034,2.75);
#20910=CIRCLE('',#100036,2.75);
#20911=CIRCLE('',#100038,2.75);
#20912=CIRCLE('',#100040,2.75);
#20913=CIRCLE('',#100042,2.75);
#20914=CIRCLE('',#100044,2.75);
#20915=CIRCLE('',#100046,2.75);
#20916=CIRCLE('',#100048,2.75);
#20917=CIRCLE('',#100050,2.75);
#20918=CIRCLE('',#100052,2.75);
#20919=CIRCLE('',#100054,2.75);
#20920=CIRCLE('',#100056,2.75);
#20921=CIRCLE('',#100058,2.75);
#20922=CIRCLE('',#100060,2.75);
#20923=CIRCLE('',#100062,2.75);
#20924=CIRCLE('',#100064,2.75);
#20925=CIRCLE('',#100066,2.75);
#20926=CIRCLE('',#100068,2.75);
#20927=CIRCLE('',#100070,2.75);
#20928=CIRCLE('',#100072,2.75);
#20929=CIRCLE('',#100366,0.00687499999999997);
#20930=CIRCLE('',#100377,1.44337567297406);
#20931=CIRCLE('',#100378,1.44337567297406);
#20932=CIRCLE('',#100379,1.44337567297406);
#20933=CIRCLE('',#100380,1.44337567297406);
#20934=CIRCLE('',#100381,1.44337567297406);
#20935=CIRCLE('',#100401,2.74633883476483);
#20936=CIRCLE('',#100404,0.0125);
#20937=CIRCLE('',#100405,0.0125);
#20938=CIRCLE('',#100407,0.0125000000000001);
#20939=CIRCLE('',#100408,0.0125000000000001);
#20940=CIRCLE('',#100410,0.0125000000000001);
#20941=CIRCLE('',#100411,0.0125000000000004);
#20942=CIRCLE('',#100412,0.0125);
#20943=CIRCLE('',#100413,0.0125000000000004);
#20944=CIRCLE('',#100415,0.0125);
#20945=CIRCLE('',#100416,0.0124999999999998);
#20946=CIRCLE('',#100422,0.00687499999999996);
#20947=CIRCLE('',#100426,0.0125000000000002);
#20948=CIRCLE('',#100427,2.74633883476483);
#20949=CIRCLE('',#100428,0.0124999999999998);
#20950=CIRCLE('',#100429,0.0125);
#20951=CIRCLE('',#100431,0.0125);
#20952=CIRCLE('',#100432,0.0125000000000001);
#20953=CIRCLE('',#100433,0.0125000000000003);
#20954=CIRCLE('',#100434,0.0125000000000003);
#20955=CIRCLE('',#100435,0.0124999999999998);
#20956=CIRCLE('',#100436,0.0125);
#20957=CIRCLE('',#100438,0.0125);
#20958=CIRCLE('',#100445,0.00687499999999999);
#20959=CIRCLE('',#100449,0.0124999999999998);
#20960=CIRCLE('',#100450,2.74633883476483);
#20961=CIRCLE('',#100451,0.0125000000000002);
#20962=CIRCLE('',#100452,0.0125);
#20963=CIRCLE('',#100454,0.0125);
#20964=CIRCLE('',#100455,0.0125000000000001);
#20965=CIRCLE('',#100456,0.0125000000000003);
#20966=CIRCLE('',#100457,0.0125000000000003);
#20967=CIRCLE('',#100458,0.0124999999999997);
#20968=CIRCLE('',#100459,0.0125);
#20969=CIRCLE('',#100461,0.0125);
#20970=CIRCLE('',#100468,0.00687499999999993);
#20971=CIRCLE('',#100472,0.0124999999999999);
#20972=CIRCLE('',#100473,2.74633883476483);
#20973=CIRCLE('',#100474,0.0124999999999999);
#20974=CIRCLE('',#100475,0.0125);
#20975=CIRCLE('',#100477,0.0125);
#20976=CIRCLE('',#100478,0.0124999999999999);
#20977=CIRCLE('',#100479,0.0125000000000004);
#20978=CIRCLE('',#100480,0.0125000000000004);
#20979=CIRCLE('',#100481,0.0124999999999999);
#20980=CIRCLE('',#100482,0.0125);
#20981=CIRCLE('',#100484,0.0125);
#20982=CIRCLE('',#100491,0.00687499999999995);
#20983=CIRCLE('',#100495,0.0124999999999999);
#20984=CIRCLE('',#100496,2.74633883476483);
#20985=CIRCLE('',#100497,0.0124999999999999);
#20986=CIRCLE('',#100498,0.0125);
#20987=CIRCLE('',#100500,0.0125);
#20988=CIRCLE('',#100501,0.0125);
#20989=CIRCLE('',#100502,0.0125000000000005);
#20990=CIRCLE('',#100503,0.0125000000000005);
#20991=CIRCLE('',#100504,0.0124999999999997);
#20992=CIRCLE('',#100505,0.0125);
#20993=CIRCLE('',#100507,0.0125000000000001);
#20994=CIRCLE('',#100514,0.00687499999999998);
#20995=CIRCLE('',#100518,0.0125);
#20996=CIRCLE('',#100519,2.74633883476483);
#20997=CIRCLE('',#100520,0.0125000000000002);
#20998=CIRCLE('',#100521,0.0125000000000001);
#20999=CIRCLE('',#100523,0.0125000000000001);
#21000=CIRCLE('',#100524,0.0125000000000001);
#21001=CIRCLE('',#100525,0.0125000000000004);
#21002=CIRCLE('',#100526,0.0125000000000004);
#21003=CIRCLE('',#100527,0.0124999999999998);
#21004=CIRCLE('',#100528,0.0125000000000001);
#21005=CIRCLE('',#100530,0.0125);
#21006=CIRCLE('',#100537,0.00687499999999991);
#21007=CIRCLE('',#100541,0.0125000000000002);
#21008=CIRCLE('',#100542,2.74633883476483);
#21009=CIRCLE('',#100543,0.0124999999999999);
#21010=CIRCLE('',#100544,0.0125);
#21011=CIRCLE('',#100546,0.0125);
#21012=CIRCLE('',#100547,0.0125);
#21013=CIRCLE('',#100548,0.0125000000000005);
#21014=CIRCLE('',#100549,0.0125000000000005);
#21015=CIRCLE('',#100550,0.0124999999999997);
#21016=CIRCLE('',#100551,0.0125);
#21017=CIRCLE('',#100553,0.0125);
#21018=CIRCLE('',#100560,0.00687500000000009);
#21019=CIRCLE('',#100564,0.0125000000000001);
#21020=CIRCLE('',#100565,2.74633883476483);
#21021=CIRCLE('',#100566,0.0125);
#21022=CIRCLE('',#100567,0.0124999999999999);
#21023=CIRCLE('',#100569,0.0124999999999999);
#21024=CIRCLE('',#100570,0.0125000000000001);
#21025=CIRCLE('',#100571,0.0125000000000004);
#21026=CIRCLE('',#100572,0.0125000000000004);
#21027=CIRCLE('',#100573,0.0124999999999998);
#21028=CIRCLE('',#100574,0.0124999999999999);
#21029=CIRCLE('',#100576,0.0125000000000001);
#21030=CIRCLE('',#100583,0.00687500000000007);
#21031=CIRCLE('',#100587,0.0124999999999999);
#21032=CIRCLE('',#100588,2.74633883476483);
#21033=CIRCLE('',#100589,0.0125);
#21034=CIRCLE('',#100590,0.0125000000000001);
#21035=CIRCLE('',#100592,0.0125000000000001);
#21036=CIRCLE('',#100593,0.0125);
#21037=CIRCLE('',#100594,0.0125000000000003);
#21038=CIRCLE('',#100595,0.0125000000000003);
#21039=CIRCLE('',#100596,0.0124999999999999);
#21040=CIRCLE('',#100597,0.0125000000000001);
#21041=CIRCLE('',#100599,0.0124999999999998);
#21042=CIRCLE('',#100606,0.00687500000000009);
#21043=CIRCLE('',#100610,0.0124999999999999);
#21044=CIRCLE('',#100611,2.74633883476483);
#21045=CIRCLE('',#100612,0.0125000000000001);
#21046=CIRCLE('',#100613,0.0125000000000001);
#21047=CIRCLE('',#100615,0.0125000000000001);
#21048=CIRCLE('',#100616,0.0125000000000001);
#21049=CIRCLE('',#100617,0.0125000000000004);
#21050=CIRCLE('',#100618,0.0125000000000004);
#21051=CIRCLE('',#100619,0.0124999999999998);
#21052=CIRCLE('',#100620,0.0125000000000001);
#21053=CIRCLE('',#100622,0.0125000000000001);
#21054=CIRCLE('',#100629,0.00687500000000004);
#21055=CIRCLE('',#100633,0.0124999999999999);
#21056=CIRCLE('',#100634,2.74633883476483);
#21057=CIRCLE('',#100635,0.0124999999999999);
#21058=CIRCLE('',#100636,0.0125000000000001);
#21059=CIRCLE('',#100638,0.0125000000000001);
#21060=CIRCLE('',#100639,0.0125000000000001);
#21061=CIRCLE('',#100640,0.0125000000000004);
#21062=CIRCLE('',#100641,0.0125000000000004);
#21063=CIRCLE('',#100642,0.0124999999999998);
#21064=CIRCLE('',#100643,0.0125000000000001);
#21065=CIRCLE('',#100645,0.0124999999999998);
#21066=CIRCLE('',#100652,0.00687500000000003);
#21067=CIRCLE('',#100656,0.0124999999999998);
#21068=CIRCLE('',#100657,2.74633883476483);
#21069=CIRCLE('',#100658,0.0125);
#21070=CIRCLE('',#100659,0.0125);
#21071=CIRCLE('',#100661,0.0125);
#21072=CIRCLE('',#100662,0.0124999999999999);
#21073=CIRCLE('',#100663,0.0125000000000003);
#21074=CIRCLE('',#100664,0.0125000000000003);
#21075=CIRCLE('',#100665,0.0124999999999998);
#21076=CIRCLE('',#100666,0.0125);
#21077=CIRCLE('',#100668,0.0125000000000001);
#21078=CIRCLE('',#100675,0.00687499999999996);
#21079=CIRCLE('',#100679,0.0124999999999999);
#21080=CIRCLE('',#100680,2.74633883476483);
#21081=CIRCLE('',#100681,0.0124999999999999);
#21082=CIRCLE('',#100682,0.0125);
#21083=CIRCLE('',#100684,0.0125);
#21084=CIRCLE('',#100685,0.0125);
#21085=CIRCLE('',#100686,0.0125000000000003);
#21086=CIRCLE('',#100687,0.0125000000000003);
#21087=CIRCLE('',#100688,0.0124999999999997);
#21088=CIRCLE('',#100689,0.0125);
#21089=CIRCLE('',#100691,0.0125000000000001);
#21090=CIRCLE('',#100698,0.00687499999999994);
#21091=CIRCLE('',#100702,0.0125000000000001);
#21092=CIRCLE('',#100703,2.74633883476483);
#21093=CIRCLE('',#100704,0.0124999999999999);
#21094=CIRCLE('',#100705,0.0125);
#21095=CIRCLE('',#100707,0.0125);
#21096=CIRCLE('',#100708,0.0125);
#21097=CIRCLE('',#100709,0.0125000000000004);
#21098=CIRCLE('',#100710,0.0125000000000004);
#21099=CIRCLE('',#100711,0.0124999999999998);
#21100=CIRCLE('',#100712,0.0125000000000001);
#21101=CIRCLE('',#100714,0.0125);
#21102=CIRCLE('',#100721,0.00687499999999994);
#21103=CIRCLE('',#100725,0.0125);
#21104=CIRCLE('',#100726,2.74633883476483);
#21105=CIRCLE('',#100727,0.0124999999999998);
#21106=CIRCLE('',#100728,0.0124999999999999);
#21107=CIRCLE('',#100730,0.0124999999999999);
#21108=CIRCLE('',#100731,0.0125);
#21109=CIRCLE('',#100732,0.0125000000000004);
#21110=CIRCLE('',#100733,0.0125000000000003);
#21111=CIRCLE('',#100734,0.0124999999999999);
#21112=CIRCLE('',#100735,0.0124999999999999);
#21113=CIRCLE('',#100737,0.0124999999999999);
#21114=CIRCLE('',#100744,0.00687500000000012);
#21115=CIRCLE('',#100748,0.0124999999999999);
#21116=CIRCLE('',#100749,2.74633883476483);
#21117=CIRCLE('',#100750,0.0125000000000002);
#21118=CIRCLE('',#100751,0.0125);
#21119=CIRCLE('',#100753,0.0125);
#21120=CIRCLE('',#100754,0.0125000000000001);
#21121=CIRCLE('',#100755,0.0125000000000005);
#21122=CIRCLE('',#100756,0.0125000000000005);
#21123=CIRCLE('',#100757,0.0124999999999998);
#21124=CIRCLE('',#100758,0.0125);
#21125=CIRCLE('',#100760,0.0125);
#21126=CIRCLE('',#100767,0.00687499999999988);
#21127=CIRCLE('',#100771,0.0125);
#21128=CIRCLE('',#100772,2.74633883476483);
#21129=CIRCLE('',#100773,0.0125000000000001);
#21130=CIRCLE('',#100774,0.0125);
#21131=CIRCLE('',#100776,0.0125);
#21132=CIRCLE('',#100777,0.0124999999999999);
#21133=CIRCLE('',#100778,0.0125000000000004);
#21134=CIRCLE('',#100779,0.0125000000000004);
#21135=CIRCLE('',#100780,0.0124999999999998);
#21136=CIRCLE('',#100781,0.0125);
#21137=CIRCLE('',#100783,0.0124999999999999);
#21138=CIRCLE('',#100790,0.00687500000000008);
#21139=CIRCLE('',#100794,0.0125);
#21140=CIRCLE('',#100795,2.74633883476483);
#21141=CIRCLE('',#100796,0.0124999999999999);
#21142=CIRCLE('',#100797,0.0125000000000001);
#21143=CIRCLE('',#100799,0.0125000000000001);
#21144=CIRCLE('',#100800,0.0124999999999998);
#21145=CIRCLE('',#100801,0.0125000000000005);
#21146=CIRCLE('',#100802,0.0125000000000005);
#21147=CIRCLE('',#100803,0.0124999999999998);
#21148=CIRCLE('',#100804,0.0125000000000001);
#21149=CIRCLE('',#100806,0.0124999999999999);
#21150=CIRCLE('',#100813,0.00687500000000005);
#21151=CIRCLE('',#100817,0.0125000000000001);
#21152=CIRCLE('',#100818,2.74633883476483);
#21153=CIRCLE('',#100819,0.0124999999999999);
#21154=CIRCLE('',#100820,0.0125);
#21155=CIRCLE('',#100822,0.0125);
#21156=CIRCLE('',#100823,0.0125000000000001);
#21157=CIRCLE('',#100824,0.0125000000000005);
#21158=CIRCLE('',#100825,0.0125000000000005);
#21159=CIRCLE('',#100826,0.0124999999999998);
#21160=CIRCLE('',#100827,0.0125);
#21161=CIRCLE('',#100829,0.0125);
#21162=CIRCLE('',#100836,0.00687499999999988);
#21163=CIRCLE('',#100840,0.0125000000000001);
#21164=CIRCLE('',#100841,2.74633883476483);
#21165=CIRCLE('',#100842,0.0124999999999998);
#21166=CIRCLE('',#100843,0.0125);
#21167=CIRCLE('',#100845,0.0125);
#21168=CIRCLE('',#100846,0.0124999999999998);
#21169=CIRCLE('',#100847,0.0125000000000005);
#21170=CIRCLE('',#100848,0.0125000000000005);
#21171=CIRCLE('',#100849,0.0124999999999999);
#21172=CIRCLE('',#100850,0.0125);
#21173=CIRCLE('',#100852,0.0125);
#21174=CIRCLE('',#100859,0.00687499999999997);
#21175=CIRCLE('',#100863,0.0125);
#21176=CIRCLE('',#100864,2.74633883476483);
#21177=CIRCLE('',#100865,0.0125);
#21178=CIRCLE('',#100866,0.0125);
#21179=CIRCLE('',#100868,0.0125);
#21180=CIRCLE('',#100869,0.0125000000000001);
#21181=CIRCLE('',#100870,0.0125000000000005);
#21182=CIRCLE('',#100871,0.0125000000000002);
#21183=CIRCLE('',#100872,0.0124999999999998);
#21184=CIRCLE('',#100873,0.0125);
#21185=CIRCLE('',#100875,0.0125);
#21186=CIRCLE('',#100882,0.00687499999999996);
#21187=CIRCLE('',#100886,0.0125);
#21188=CIRCLE('',#100887,2.74633883476483);
#21189=CIRCLE('',#100888,0.0125);
#21190=CIRCLE('',#100889,0.0125);
#21191=CIRCLE('',#100891,0.0125);
#21192=CIRCLE('',#100892,0.0125);
#21193=CIRCLE('',#100893,0.0125000000000004);
#21194=CIRCLE('',#100894,0.0125000000000004);
#21195=CIRCLE('',#100895,0.0124999999999997);
#21196=CIRCLE('',#100896,0.0125);
#21197=CIRCLE('',#100898,0.0125);
#21198=CIRCLE('',#100905,0.00687499999999993);
#21199=CIRCLE('',#100909,0.0125);
#21200=CIRCLE('',#100910,2.74633883476483);
#21201=CIRCLE('',#100911,0.0125);
#21202=CIRCLE('',#100912,0.0125);
#21203=CIRCLE('',#100914,0.0125);
#21204=CIRCLE('',#100915,0.0124999999999998);
#21205=CIRCLE('',#100916,0.0125000000000004);
#21206=CIRCLE('',#100917,0.0125000000000004);
#21207=CIRCLE('',#100918,0.0124999999999998);
#21208=CIRCLE('',#100919,0.0125);
#21209=CIRCLE('',#100921,0.0125);
#21210=CIRCLE('',#100928,0.00687500000000001);
#21211=CIRCLE('',#100932,0.0125);
#21212=CIRCLE('',#100933,2.74633883476484);
#21213=CIRCLE('',#100934,0.0125000000000002);
#21214=CIRCLE('',#100935,0.0125000000000001);
#21215=CIRCLE('',#100937,0.0125);
#21216=CIRCLE('',#100938,0.0125);
#21217=CIRCLE('',#100939,0.0125000000000003);
#21218=CIRCLE('',#100940,0.0125000000000003);
#21219=CIRCLE('',#100941,0.0124999999999997);
#21220=CIRCLE('',#100942,0.0125);
#21221=CIRCLE('',#100944,0.0125);
#21222=CIRCLE('',#100951,0.00687499999999995);
#21223=CIRCLE('',#100955,0.0125000000000001);
#21224=CIRCLE('',#100956,2.74633883476483);
#21225=CIRCLE('',#100957,0.0125000000000001);
#21226=CIRCLE('',#100958,0.0125);
#21227=CIRCLE('',#100960,0.0125);
#21228=CIRCLE('',#100961,0.0125);
#21229=CIRCLE('',#100962,0.0125000000000003);
#21230=CIRCLE('',#100963,0.0125000000000003);
#21231=CIRCLE('',#100964,0.0124999999999997);
#21232=CIRCLE('',#100965,0.0125);
#21233=CIRCLE('',#100967,0.0125);
#21234=CIRCLE('',#100974,0.00687499999999997);
#21235=CIRCLE('',#100978,0.0125);
#21236=CIRCLE('',#100979,2.74633883476483);
#21237=CIRCLE('',#100980,0.0125);
#21238=CIRCLE('',#100981,0.0125);
#21239=CIRCLE('',#100983,0.0125);
#21240=CIRCLE('',#100984,0.0125);
#21241=CIRCLE('',#100985,0.0125000000000004);
#21242=CIRCLE('',#100986,0.0125000000000004);
#21243=CIRCLE('',#100987,0.0124999999999997);
#21244=CIRCLE('',#100988,0.0125);
#21245=CIRCLE('',#100990,0.0125);
#21246=CIRCLE('',#100997,0.00687499999999996);
#21247=CIRCLE('',#101001,0.0125);
#21248=CIRCLE('',#101002,2.74633883476483);
#21249=CIRCLE('',#101003,0.0125);
#21250=CIRCLE('',#101004,0.0125);
#21251=CIRCLE('',#101006,0.0125);
#21252=CIRCLE('',#101007,0.0125);
#21253=CIRCLE('',#101008,0.0125000000000004);
#21254=CIRCLE('',#101009,0.0125000000000004);
#21255=CIRCLE('',#101010,0.0124999999999997);
#21256=CIRCLE('',#101011,0.0125);
#21257=CIRCLE('',#101013,0.0125);
#21258=CIRCLE('',#101020,0.00687500000000001);
#21259=CIRCLE('',#101024,0.0125);
#21260=CIRCLE('',#101025,2.74633883476483);
#21261=CIRCLE('',#101026,0.0125);
#21262=CIRCLE('',#101027,0.0125);
#21263=CIRCLE('',#101029,0.0125);
#21264=CIRCLE('',#101030,0.0125);
#21265=CIRCLE('',#101031,0.0125000000000003);
#21266=CIRCLE('',#101032,0.0125000000000003);
#21267=CIRCLE('',#101033,0.0124999999999997);
#21268=CIRCLE('',#101034,0.0125);
#21269=CIRCLE('',#101036,0.0125);
#21270=CIRCLE('',#101043,0.00687499999999995);
#21271=CIRCLE('',#101047,0.0125000000000001);
#21272=CIRCLE('',#101048,2.74633883476483);
#21273=CIRCLE('',#101049,0.0125);
#21274=CIRCLE('',#101050,0.0125);
#21275=CIRCLE('',#101052,0.0125);
#21276=CIRCLE('',#101053,0.0125);
#21277=CIRCLE('',#101054,0.0125000000000003);
#21278=CIRCLE('',#101055,0.0125000000000003);
#21279=CIRCLE('',#101056,0.0124999999999997);
#21280=CIRCLE('',#101057,0.0125);
#21281=CIRCLE('',#101059,0.0125);
#21282=CIRCLE('',#101066,0.00687499999999993);
#21283=CIRCLE('',#101070,0.0125);
#21284=CIRCLE('',#101071,2.74633883476483);
#21285=CIRCLE('',#101072,0.0124999999999999);
#21286=CIRCLE('',#101073,0.0125);
#21287=CIRCLE('',#101075,0.0125);
#21288=CIRCLE('',#101076,0.0125000000000001);
#21289=CIRCLE('',#101077,0.0125000000000004);
#21290=CIRCLE('',#101078,0.0125000000000004);
#21291=CIRCLE('',#101079,0.0124999999999998);
#21292=CIRCLE('',#101080,0.0125);
#21293=CIRCLE('',#101082,0.0125);
#21294=CIRCLE('',#101089,0.00687499999999996);
#21295=CIRCLE('',#101093,0.0124999999999999);
#21296=CIRCLE('',#101094,2.74633883476483);
#21297=CIRCLE('',#101095,0.0124999999999999);
#21298=CIRCLE('',#101096,0.0125000000000001);
#21299=CIRCLE('',#101098,0.0125000000000001);
#21300=CIRCLE('',#101099,0.0124999999999999);
#21301=CIRCLE('',#101100,0.0125000000000004);
#21302=CIRCLE('',#101101,0.0125000000000004);
#21303=CIRCLE('',#101102,0.0124999999999999);
#21304=CIRCLE('',#101103,0.0125000000000001);
#21305=CIRCLE('',#101105,0.0125000000000001);
#21306=CIRCLE('',#101112,0.00687499999999997);
#21307=CIRCLE('',#101116,0.0124999999999999);
#21308=CIRCLE('',#101117,2.74633883476483);
#21309=CIRCLE('',#101118,0.0124999999999999);
#21310=CIRCLE('',#101119,0.0125000000000001);
#21311=CIRCLE('',#101121,0.0125000000000001);
#21312=CIRCLE('',#101122,0.0125000000000001);
#21313=CIRCLE('',#101123,0.0125000000000005);
#21314=CIRCLE('',#101124,0.0125000000000005);
#21315=CIRCLE('',#101125,0.0124999999999998);
#21316=CIRCLE('',#101126,0.0125);
#21317=CIRCLE('',#101128,0.0124999999999999);
#21318=CIRCLE('',#101135,0.00687499999999988);
#21319=CIRCLE('',#101139,0.0125000000000001);
#21320=CIRCLE('',#101140,2.74633883476484);
#21321=CIRCLE('',#101141,0.0125);
#21322=CIRCLE('',#101142,0.0124999999999999);
#21323=CIRCLE('',#101144,0.0124999999999999);
#21324=CIRCLE('',#101145,0.0125000000000001);
#21325=CIRCLE('',#101146,0.0125000000000004);
#21326=CIRCLE('',#101147,0.0125000000000004);
#21327=CIRCLE('',#101148,0.0124999999999998);
#21328=CIRCLE('',#101149,0.0124999999999999);
#21329=CIRCLE('',#101151,0.0124999999999999);
#21330=CIRCLE('',#101158,0.00687500000000005);
#21331=CIRCLE('',#101162,0.0124999999999998);
#21332=CIRCLE('',#101163,2.74633883476483);
#21333=CIRCLE('',#101164,0.0125);
#21334=CIRCLE('',#101165,0.0125);
#21335=CIRCLE('',#101167,0.0125);
#21336=CIRCLE('',#101168,0.0125000000000001);
#21337=CIRCLE('',#101169,0.0125000000000005);
#21338=CIRCLE('',#101170,0.0125000000000005);
#21339=CIRCLE('',#101171,0.0124999999999997);
#21340=CIRCLE('',#101172,0.0125);
#21341=CIRCLE('',#101174,0.0125);
#21342=CIRCLE('',#101181,0.00687499999999999);
#21343=CIRCLE('',#101185,0.0124999999999999);
#21344=CIRCLE('',#101186,2.74633883476483);
#21345=CIRCLE('',#101187,0.0124999999999999);
#21346=CIRCLE('',#101188,0.0125);
#21347=CIRCLE('',#101190,0.0125);
#21348=CIRCLE('',#101191,0.0124999999999999);
#21349=CIRCLE('',#101192,0.0125000000000004);
#21350=CIRCLE('',#101193,0.0125000000000004);
#21351=CIRCLE('',#101194,0.0124999999999999);
#21352=CIRCLE('',#101195,0.0125);
#21353=CIRCLE('',#101197,0.0125);
#21354=CIRCLE('',#101204,0.00687499999999995);
#21355=CIRCLE('',#101208,0.0125);
#21356=CIRCLE('',#101209,2.74633883476483);
#21357=CIRCLE('',#101210,0.0124999999999999);
#21358=CIRCLE('',#101211,0.0125);
#21359=CIRCLE('',#101213,0.0125);
#21360=CIRCLE('',#101214,0.0125);
#21361=CIRCLE('',#101215,0.0125000000000006);
#21362=CIRCLE('',#101216,0.0125000000000002);
#21363=CIRCLE('',#101217,0.0124999999999997);
#21364=CIRCLE('',#101218,0.0125);
#21365=CIRCLE('',#101220,0.0125);
#21366=CIRCLE('',#101227,0.00687499999999988);
#21367=CIRCLE('',#101231,0.0124999999999998);
#21368=CIRCLE('',#101232,2.74633883476484);
#21369=CIRCLE('',#101233,0.0125000000000001);
#21370=CIRCLE('',#101234,0.0124999999999999);
#21371=CIRCLE('',#101236,0.0124999999999999);
#21372=CIRCLE('',#101237,0.0125000000000001);
#21373=CIRCLE('',#101238,0.0125000000000004);
#21374=CIRCLE('',#101239,0.0125000000000004);
#21375=CIRCLE('',#101240,0.0124999999999998);
#21376=CIRCLE('',#101241,0.0124999999999999);
#21377=CIRCLE('',#101243,0.0125000000000001);
#21378=CIRCLE('',#101250,0.00687499999999991);
#21379=CIRCLE('',#101254,0.0125);
#21380=CIRCLE('',#101255,2.74633883476483);
#21381=CIRCLE('',#101256,0.0124999999999998);
#21382=CIRCLE('',#101257,0.0125);
#21383=CIRCLE('',#101259,0.0124999999999999);
#21384=CIRCLE('',#101260,0.0125);
#21385=CIRCLE('',#101261,0.0125000000000005);
#21386=CIRCLE('',#101262,0.0125000000000005);
#21387=CIRCLE('',#101263,0.0124999999999997);
#21388=CIRCLE('',#101264,0.0125);
#21389=CIRCLE('',#101266,0.0124999999999999);
#21390=CIRCLE('',#101273,0.0068749999999999);
#21391=CIRCLE('',#101277,0.0125000000000001);
#21392=CIRCLE('',#101278,2.74633883476483);
#21393=CIRCLE('',#101279,0.0125000000000002);
#21394=CIRCLE('',#101280,0.0125000000000001);
#21395=CIRCLE('',#101282,0.0125000000000001);
#21396=CIRCLE('',#101283,0.0124999999999999);
#21397=CIRCLE('',#101284,0.0125000000000004);
#21398=CIRCLE('',#101285,0.0125000000000004);
#21399=CIRCLE('',#101286,0.0124999999999999);
#21400=CIRCLE('',#101287,0.0125);
#21401=CIRCLE('',#101289,0.0124999999999999);
#21402=CIRCLE('',#101296,0.00687499999999987);
#21403=CIRCLE('',#101300,0.0125);
#21404=CIRCLE('',#101301,2.74633883476483);
#21405=CIRCLE('',#101302,0.0125);
#21406=CIRCLE('',#101303,0.0125);
#21407=CIRCLE('',#101305,0.0125);
#21408=CIRCLE('',#101306,0.0125);
#21409=CIRCLE('',#101307,0.0125000000000003);
#21410=CIRCLE('',#101308,0.0125000000000003);
#21411=CIRCLE('',#101309,0.0124999999999997);
#21412=CIRCLE('',#101310,0.0125);
#21413=CIRCLE('',#101312,0.0125000000000001);
#21414=CIRCLE('',#101319,0.00687500000000009);
#21415=CIRCLE('',#101323,0.0125000000000002);
#21416=CIRCLE('',#101324,2.74633883476483);
#21417=CIRCLE('',#101325,0.0125);
#21418=CIRCLE('',#101326,0.0124999999999999);
#21419=CIRCLE('',#101328,0.0124999999999999);
#21420=CIRCLE('',#101329,0.0125000000000002);
#21421=CIRCLE('',#101330,0.0125000000000005);
#21422=CIRCLE('',#101331,0.0125000000000005);
#21423=CIRCLE('',#101332,0.0124999999999998);
#21424=CIRCLE('',#101333,0.0124999999999999);
#21425=CIRCLE('',#101335,0.0124999999999999);
#21426=CIRCLE('',#101342,0.00687499999999986);
#21427=CIRCLE('',#101346,0.0124999999999999);
#21428=CIRCLE('',#101347,2.74633883476483);
#21429=CIRCLE('',#101348,0.0125);
#21430=CIRCLE('',#101349,0.0124999999999999);
#21431=CIRCLE('',#101351,0.0124999999999999);
#21432=CIRCLE('',#101352,0.0124999999999999);
#21433=CIRCLE('',#101353,0.0125000000000005);
#21434=CIRCLE('',#101354,0.0125000000000005);
#21435=CIRCLE('',#101355,0.0124999999999998);
#21436=CIRCLE('',#101356,0.0124999999999999);
#21437=CIRCLE('',#101358,0.0125);
#21438=CIRCLE('',#101365,0.00687500000000003);
#21439=CIRCLE('',#101369,0.0125000000000002);
#21440=CIRCLE('',#101370,2.74633883476483);
#21441=CIRCLE('',#101371,0.0124999999999999);
#21442=CIRCLE('',#101372,0.0124999999999999);
#21443=CIRCLE('',#101374,0.0124999999999999);
#21444=CIRCLE('',#101375,0.0124999999999999);
#21445=CIRCLE('',#101376,0.0125000000000004);
#21446=CIRCLE('',#101377,0.0125000000000004);
#21447=CIRCLE('',#101378,0.0124999999999999);
#21448=CIRCLE('',#101379,0.0124999999999999);
#21449=CIRCLE('',#101381,0.0125);
#21450=CIRCLE('',#101388,0.00687499999999996);
#21451=CIRCLE('',#101392,0.0125);
#21452=CIRCLE('',#101393,2.74633883476483);
#21453=CIRCLE('',#101394,0.0124999999999999);
#21454=CIRCLE('',#101395,0.0124999999999998);
#21455=CIRCLE('',#101397,0.0124999999999998);
#21456=CIRCLE('',#101398,0.0125000000000001);
#21457=CIRCLE('',#101399,0.0125000000000003);
#21458=CIRCLE('',#101400,0.0125000000000003);
#21459=CIRCLE('',#101401,0.0124999999999998);
#21460=CIRCLE('',#101402,0.0124999999999998);
#21461=CIRCLE('',#101404,0.0125);
#21462=CIRCLE('',#101411,0.00687499999999994);
#21463=CIRCLE('',#101415,0.0125000000000001);
#21464=CIRCLE('',#101416,2.74633883476483);
#21465=CIRCLE('',#101417,0.0124999999999999);
#21466=CIRCLE('',#101418,0.0125);
#21467=CIRCLE('',#101420,0.0125);
#21468=CIRCLE('',#101421,0.0125);
#21469=CIRCLE('',#101422,0.0125000000000004);
#21470=CIRCLE('',#101423,0.0125000000000004);
#21471=CIRCLE('',#101424,0.0125);
#21472=CIRCLE('',#101425,0.0125000000000001);
#21473=CIRCLE('',#101427,0.0125);
#21474=CIRCLE('',#101434,0.00687499999999994);
#21475=CIRCLE('',#101438,0.0125000000000002);
#21476=CIRCLE('',#101439,2.74633883476483);
#21477=CIRCLE('',#101440,0.0125);
#21478=CIRCLE('',#101441,0.0125);
#21479=CIRCLE('',#101443,0.0125);
#21480=CIRCLE('',#101444,0.0124999999999999);
#21481=CIRCLE('',#101445,0.0125000000000005);
#21482=CIRCLE('',#101446,0.0125000000000005);
#21483=CIRCLE('',#101447,0.0124999999999998);
#21484=CIRCLE('',#101448,0.0125);
#21485=CIRCLE('',#101450,0.0125);
#21486=CIRCLE('',#101457,0.00687499999999985);
#21487=CIRCLE('',#101461,0.0125000000000001);
#21488=CIRCLE('',#101462,2.74633883476483);
#21489=CIRCLE('',#101463,0.0125000000000001);
#21490=CIRCLE('',#101464,0.0125);
#21491=CIRCLE('',#101466,0.0125);
#21492=CIRCLE('',#101467,0.0125);
#21493=CIRCLE('',#101468,0.0125000000000004);
#21494=CIRCLE('',#101469,0.0125000000000004);
#21495=CIRCLE('',#101470,0.0124999999999997);
#21496=CIRCLE('',#101471,0.0125);
#21497=CIRCLE('',#101473,0.0124999999999998);
#21498=CIRCLE('',#101480,0.00687500000000006);
#21499=CIRCLE('',#101484,0.0125);
#21500=CIRCLE('',#101485,2.74633883476483);
#21501=CIRCLE('',#101486,0.0125);
#21502=CIRCLE('',#101487,0.0125);
#21503=CIRCLE('',#101489,0.0125);
#21504=CIRCLE('',#101490,0.0125000000000001);
#21505=CIRCLE('',#101491,0.0125000000000004);
#21506=CIRCLE('',#101492,0.0125000000000004);
#21507=CIRCLE('',#101493,0.0124999999999998);
#21508=CIRCLE('',#101494,0.0125);
#21509=CIRCLE('',#101496,0.0125000000000001);
#21510=CIRCLE('',#101503,0.00687500000000008);
#21511=CIRCLE('',#101507,0.0124999999999999);
#21512=CIRCLE('',#101508,2.74633883476483);
#21513=CIRCLE('',#101509,0.0125);
#21514=CIRCLE('',#101510,0.0124999999999999);
#21515=CIRCLE('',#101512,0.0124999999999999);
#21516=CIRCLE('',#101513,0.0125000000000001);
#21517=CIRCLE('',#101514,0.0125000000000004);
#21518=CIRCLE('',#101515,0.0125000000000004);
#21519=CIRCLE('',#101516,0.0124999999999998);
#21520=CIRCLE('',#101517,0.0124999999999999);
#21521=CIRCLE('',#101519,0.0124999999999999);
#21522=CIRCLE('',#101526,0.00687500000000005);
#21523=CIRCLE('',#101530,0.0124999999999998);
#21524=CIRCLE('',#101531,2.74633883476483);
#21525=CIRCLE('',#101532,0.0125);
#21526=CIRCLE('',#101533,0.0124999999999998);
#21527=CIRCLE('',#101535,0.0124999999999998);
#21528=CIRCLE('',#101536,0.0125000000000001);
#21529=CIRCLE('',#101537,0.0125000000000005);
#21530=CIRCLE('',#101538,0.0125000000000005);
#21531=CIRCLE('',#101539,0.0124999999999997);
#21532=CIRCLE('',#101540,0.0124999999999998);
#21533=CIRCLE('',#101542,0.0125);
#21534=CIRCLE('',#101549,0.00687499999999988);
#21535=CIRCLE('',#101553,0.0124999999999998);
#21536=CIRCLE('',#101554,2.74633883476483);
#21537=CIRCLE('',#101555,0.0125000000000001);
#21538=CIRCLE('',#101556,0.0124999999999999);
#21539=CIRCLE('',#101558,0.0124999999999999);
#21540=CIRCLE('',#101559,0.0125000000000001);
#21541=CIRCLE('',#101560,0.0125000000000004);
#21542=CIRCLE('',#101561,0.0125000000000004);
#21543=CIRCLE('',#101562,0.0124999999999998);
#21544=CIRCLE('',#101563,0.0124999999999999);
#21545=CIRCLE('',#101565,0.0125);
#21546=CIRCLE('',#101572,0.00687499999999997);
#21547=CIRCLE('',#101576,0.0125);
#21548=CIRCLE('',#101577,2.74633883476483);
#21549=CIRCLE('',#101578,0.0124999999999999);
#21550=CIRCLE('',#101579,0.0125);
#21551=CIRCLE('',#101581,0.0125);
#21552=CIRCLE('',#101582,0.0125000000000001);
#21553=CIRCLE('',#101583,0.0125000000000005);
#21554=CIRCLE('',#101584,0.0125000000000005);
#21555=CIRCLE('',#101585,0.0124999999999998);
#21556=CIRCLE('',#101586,0.0125);
#21557=CIRCLE('',#101588,0.0125);
#21558=CIRCLE('',#101595,0.00687499999999996);
#21559=CIRCLE('',#101599,0.0125);
#21560=CIRCLE('',#101600,2.74633883476483);
#21561=CIRCLE('',#101601,0.0124999999999999);
#21562=CIRCLE('',#101602,0.0125);
#21563=CIRCLE('',#101604,0.0125);
#21564=CIRCLE('',#101605,0.0124999999999999);
#21565=CIRCLE('',#101606,0.0125000000000004);
#21566=CIRCLE('',#101607,0.0125000000000004);
#21567=CIRCLE('',#101608,0.0125);
#21568=CIRCLE('',#101609,0.0125);
#21569=CIRCLE('',#101611,0.0125);
#21570=CIRCLE('',#101618,0.00687499999999993);
#21571=CIRCLE('',#101622,0.0125);
#21572=CIRCLE('',#101623,2.74633883476483);
#21573=CIRCLE('',#101624,0.0125);
#21574=CIRCLE('',#101625,0.0125);
#21575=CIRCLE('',#101627,0.0125);
#21576=CIRCLE('',#101628,0.0125000000000001);
#21577=CIRCLE('',#101629,0.0125000000000004);
#21578=CIRCLE('',#101630,0.0125000000000004);
#21579=CIRCLE('',#101631,0.0124999999999998);
#21580=CIRCLE('',#101632,0.0125);
#21581=CIRCLE('',#101634,0.0125);
#21582=CIRCLE('',#101641,0.00687499999999995);
#21583=CIRCLE('',#101645,0.0125000000000001);
#21584=CIRCLE('',#101646,2.74633883476483);
#21585=CIRCLE('',#101647,0.0125);
#21586=CIRCLE('',#101648,0.0125);
#21587=CIRCLE('',#101650,0.0125);
#21588=CIRCLE('',#101651,0.0125);
#21589=CIRCLE('',#101652,0.0125000000000003);
#21590=CIRCLE('',#101653,0.0125000000000003);
#21591=CIRCLE('',#101654,0.0124999999999997);
#21592=CIRCLE('',#101655,0.0125);
#21593=CIRCLE('',#101657,0.0125);
#21594=CIRCLE('',#101664,0.00687499999999995);
#21595=CIRCLE('',#101668,0.0125);
#21596=CIRCLE('',#101669,2.74633883476483);
#21597=CIRCLE('',#101670,0.0125000000000001);
#21598=CIRCLE('',#101671,0.0125);
#21599=CIRCLE('',#101673,0.0125);
#21600=CIRCLE('',#101674,0.0125);
#21601=CIRCLE('',#101675,0.0125000000000003);
#21602=CIRCLE('',#101676,0.0125000000000003);
#21603=CIRCLE('',#101677,0.0124999999999997);
#21604=CIRCLE('',#101678,0.0125);
#21605=CIRCLE('',#101680,0.0125);
#21606=CIRCLE('',#101687,0.00687499999999996);
#21607=CIRCLE('',#101691,0.0125);
#21608=CIRCLE('',#101692,2.74633883476483);
#21609=CIRCLE('',#101693,0.0125);
#21610=CIRCLE('',#101694,0.0125);
#21611=CIRCLE('',#101696,0.0125);
#21612=CIRCLE('',#101697,0.0125);
#21613=CIRCLE('',#101698,0.0125000000000004);
#21614=CIRCLE('',#101699,0.0125000000000004);
#21615=CIRCLE('',#101700,0.0124999999999997);
#21616=CIRCLE('',#101701,0.0125);
#21617=CIRCLE('',#101703,0.0125);
#21618=CIRCLE('',#101710,0.00687499999999996);
#21619=CIRCLE('',#101714,0.0125);
#21620=CIRCLE('',#101715,2.74633883476483);
#21621=CIRCLE('',#101716,0.0125);
#21622=CIRCLE('',#101717,0.0125);
#21623=CIRCLE('',#101719,0.0125);
#21624=CIRCLE('',#101720,0.0125);
#21625=CIRCLE('',#101721,0.0125000000000004);
#21626=CIRCLE('',#101722,0.0125000000000004);
#21627=CIRCLE('',#101723,0.0124999999999997);
#21628=CIRCLE('',#101724,0.0125);
#21629=CIRCLE('',#101726,0.0125);
#21630=CIRCLE('',#101733,0.00687499999999995);
#21631=CIRCLE('',#101737,0.0125000000000001);
#21632=CIRCLE('',#101738,2.74633883476483);
#21633=CIRCLE('',#101739,0.0125);
#21634=CIRCLE('',#101740,0.0125);
#21635=CIRCLE('',#101742,0.0125);
#21636=CIRCLE('',#101743,0.0125);
#21637=CIRCLE('',#101744,0.0125000000000003);
#21638=CIRCLE('',#101745,0.0125000000000003);
#21639=CIRCLE('',#101746,0.0124999999999997);
#21640=CIRCLE('',#101747,0.0125);
#21641=CIRCLE('',#101749,0.0125);
#21642=CIRCLE('',#101756,0.00687500000000001);
#21643=CIRCLE('',#101760,0.0125);
#21644=CIRCLE('',#101761,2.74633883476483);
#21645=CIRCLE('',#101762,0.0125000000000002);
#21646=CIRCLE('',#101763,0.0125000000000001);
#21647=CIRCLE('',#101765,0.0125000000000001);
#21648=CIRCLE('',#101766,0.0125);
#21649=CIRCLE('',#101767,0.0125000000000003);
#21650=CIRCLE('',#101768,0.0125000000000003);
#21651=CIRCLE('',#101769,0.0124999999999997);
#21652=CIRCLE('',#101770,0.0125000000000001);
#21653=CIRCLE('',#101772,0.0125);
#21654=CIRCLE('',#101779,0.00687499999999993);
#21655=CIRCLE('',#101783,0.0125);
#21656=CIRCLE('',#101784,2.74633883476483);
#21657=CIRCLE('',#101785,0.0125);
#21658=CIRCLE('',#101786,0.0125);
#21659=CIRCLE('',#101788,0.0125);
#21660=CIRCLE('',#101789,0.0125000000000001);
#21661=CIRCLE('',#101790,0.0125000000000004);
#21662=CIRCLE('',#101791,0.0125000000000004);
#21663=CIRCLE('',#101792,0.0124999999999998);
#21664=CIRCLE('',#101793,0.0125);
#21665=CIRCLE('',#101795,0.0124999999999999);
#21666=CIRCLE('',#101802,0.00687499999999996);
#21667=CIRCLE('',#101806,0.0125);
#21668=CIRCLE('',#101807,2.74633883476483);
#21669=CIRCLE('',#101808,0.0125);
#21670=CIRCLE('',#101809,0.0125);
#21671=CIRCLE('',#101811,0.0125);
#21672=CIRCLE('',#101812,0.0125);
#21673=CIRCLE('',#101813,0.0125000000000004);
#21674=CIRCLE('',#101814,0.0125000000000004);
#21675=CIRCLE('',#101815,0.0125);
#21676=CIRCLE('',#101816,0.0125);
#21677=CIRCLE('',#101818,0.0125);
#21678=CIRCLE('',#101825,0.00687499999999997);
#21679=CIRCLE('',#101829,0.0124999999999999);
#21680=CIRCLE('',#101830,2.74633883476483);
#21681=CIRCLE('',#101831,0.0125);
#21682=CIRCLE('',#101832,0.0125);
#21683=CIRCLE('',#101834,0.0125);
#21684=CIRCLE('',#101835,0.0125000000000001);
#21685=CIRCLE('',#101836,0.0125000000000005);
#21686=CIRCLE('',#101837,0.0125000000000005);
#21687=CIRCLE('',#101838,0.0124999999999998);
#21688=CIRCLE('',#101839,0.0125);
#21689=CIRCLE('',#101841,0.0125);
#21690=CIRCLE('',#101848,0.00687499999999988);
#21691=CIRCLE('',#101852,0.0125000000000001);
#21692=CIRCLE('',#101853,2.74633883476483);
#21693=CIRCLE('',#101854,0.0124999999999998);
#21694=CIRCLE('',#101855,0.0125);
#21695=CIRCLE('',#101857,0.0125);
#21696=CIRCLE('',#101858,0.0125000000000001);
#21697=CIRCLE('',#101859,0.0125000000000005);
#21698=CIRCLE('',#101860,0.0125000000000005);
#21699=CIRCLE('',#101861,0.0124999999999998);
#21700=CIRCLE('',#101862,0.0125);
#21701=CIRCLE('',#101864,0.0125);
#21702=CIRCLE('',#101871,0.00687500000000005);
#21703=CIRCLE('',#101875,0.0125000000000001);
#21704=CIRCLE('',#101876,2.74633883476483);
#21705=CIRCLE('',#101877,0.0124999999999999);
#21706=CIRCLE('',#101878,0.0125);
#21707=CIRCLE('',#101880,0.0125);
#21708=CIRCLE('',#101881,0.0125000000000001);
#21709=CIRCLE('',#101882,0.0125000000000005);
#21710=CIRCLE('',#101883,0.0125000000000005);
#21711=CIRCLE('',#101884,0.0124999999999998);
#21712=CIRCLE('',#101885,0.0125);
#21713=CIRCLE('',#101887,0.0125);
#21714=CIRCLE('',#101894,0.00687500000000008);
#21715=CIRCLE('',#101898,0.0125);
#21716=CIRCLE('',#101899,2.74633883476483);
#21717=CIRCLE('',#101900,0.0124999999999999);
#21718=CIRCLE('',#101901,0.0125000000000001);
#21719=CIRCLE('',#101903,0.0125000000000001);
#21720=CIRCLE('',#101904,0.0125000000000001);
#21721=CIRCLE('',#101905,0.0125000000000005);
#21722=CIRCLE('',#101906,0.0125000000000005);
#21723=CIRCLE('',#101907,0.0124999999999998);
#21724=CIRCLE('',#101908,0.0125000000000001);
#21725=CIRCLE('',#101910,0.0125);
#21726=CIRCLE('',#101917,0.00687499999999988);
#21727=CIRCLE('',#101921,0.0125);
#21728=CIRCLE('',#101922,2.74633883476483);
#21729=CIRCLE('',#101923,0.0125000000000001);
#21730=CIRCLE('',#101924,0.0125);
#21731=CIRCLE('',#101926,0.0125);
#21732=CIRCLE('',#101927,0.0125000000000001);
#21733=CIRCLE('',#101928,0.0125000000000004);
#21734=CIRCLE('',#101929,0.0125000000000004);
#21735=CIRCLE('',#101930,0.0124999999999998);
#21736=CIRCLE('',#101931,0.0125);
#21737=CIRCLE('',#101933,0.0124999999999999);
#21738=CIRCLE('',#101940,0.00687499999999985);
#21739=CIRCLE('',#101944,0.0124999999999998);
#21740=CIRCLE('',#101945,2.74633883476483);
#21741=CIRCLE('',#101946,0.0125000000000001);
#21742=CIRCLE('',#101947,0.0125);
#21743=CIRCLE('',#101949,0.0125);
#21744=CIRCLE('',#101950,0.0125);
#21745=CIRCLE('',#101951,0.0125000000000004);
#21746=CIRCLE('',#101952,0.0125000000000004);
#21747=CIRCLE('',#101953,0.0124999999999998);
#21748=CIRCLE('',#101954,0.0125);
#21749=CIRCLE('',#101956,0.0125000000000002);
#21750=CIRCLE('',#101963,0.00687499999999994);
#21751=CIRCLE('',#101967,0.0125);
#21752=CIRCLE('',#101968,2.74633883476483);
#21753=CIRCLE('',#101969,0.0125000000000002);
#21754=CIRCLE('',#101970,0.0125);
#21755=CIRCLE('',#101972,0.0125);
#21756=CIRCLE('',#101973,0.0124999999999999);
#21757=CIRCLE('',#101974,0.0125000000000004);
#21758=CIRCLE('',#101975,0.0125000000000003);
#21759=CIRCLE('',#101976,0.0124999999999999);
#21760=CIRCLE('',#101977,0.0125);
#21761=CIRCLE('',#101979,0.0125);
#21762=CIRCLE('',#101986,0.00687500000000009);
#21763=CIRCLE('',#101990,0.0125000000000001);
#21764=CIRCLE('',#101991,2.74633883476483);
#21765=CIRCLE('',#101992,0.0124999999999999);
#21766=CIRCLE('',#101993,0.0124999999999998);
#21767=CIRCLE('',#101995,0.0124999999999998);
#21768=CIRCLE('',#101996,0.0125);
#21769=CIRCLE('',#101997,0.0125000000000004);
#21770=CIRCLE('',#101998,0.0125000000000004);
#21771=CIRCLE('',#101999,0.0124999999999998);
#21772=CIRCLE('',#102000,0.0125);
#21773=CIRCLE('',#102002,0.0125);
#21774=CIRCLE('',#102009,0.00687499999999996);
#21775=CIRCLE('',#102013,0.0124999999999999);
#21776=CIRCLE('',#102014,2.74633883476483);
#21777=CIRCLE('',#102015,0.0125);
#21778=CIRCLE('',#102016,0.0124999999999998);
#21779=CIRCLE('',#102018,0.0124999999999998);
#21780=CIRCLE('',#102019,0.0125);
#21781=CIRCLE('',#102020,0.0125000000000003);
#21782=CIRCLE('',#102021,0.0125000000000003);
#21783=CIRCLE('',#102022,0.0124999999999998);
#21784=CIRCLE('',#102023,0.0124999999999998);
#21785=CIRCLE('',#102025,0.0125000000000001);
#21786=CIRCLE('',#102032,0.00687500000000003);
#21787=CIRCLE('',#102036,0.0124999999999999);
#21788=CIRCLE('',#102037,2.74633883476483);
#21789=CIRCLE('',#102038,0.0125000000000002);
#21790=CIRCLE('',#102039,0.0125);
#21791=CIRCLE('',#102041,0.0125);
#21792=CIRCLE('',#102042,0.0124999999999999);
#21793=CIRCLE('',#102043,0.0125000000000004);
#21794=CIRCLE('',#102044,0.0125000000000004);
#21795=CIRCLE('',#102045,0.0124999999999998);
#21796=CIRCLE('',#102046,0.0125);
#21797=CIRCLE('',#102048,0.0124999999999999);
#21798=CIRCLE('',#102055,0.00687500000000004);
#21799=CIRCLE('',#102059,0.0125);
#21800=CIRCLE('',#102060,2.74633883476483);
#21801=CIRCLE('',#102061,0.0124999999999999);
#21802=CIRCLE('',#102062,0.0124999999999999);
#21803=CIRCLE('',#102064,0.0124999999999999);
#21804=CIRCLE('',#102065,0.0125000000000001);
#21805=CIRCLE('',#102066,0.0125000000000005);
#21806=CIRCLE('',#102067,0.0125000000000005);
#21807=CIRCLE('',#102068,0.0124999999999998);
#21808=CIRCLE('',#102069,0.0124999999999999);
#21809=CIRCLE('',#102071,0.0125000000000001);
#21810=CIRCLE('',#102078,0.00687500000000009);
#21811=CIRCLE('',#102082,0.0125);
#21812=CIRCLE('',#102083,2.74633883476483);
#21813=CIRCLE('',#102084,0.0125000000000001);
#21814=CIRCLE('',#102085,0.0124999999999999);
#21815=CIRCLE('',#102087,0.0124999999999999);
#21816=CIRCLE('',#102088,0.0125000000000001);
#21817=CIRCLE('',#102089,0.0125000000000004);
#21818=CIRCLE('',#102090,0.0125000000000004);
#21819=CIRCLE('',#102091,0.0124999999999998);
#21820=CIRCLE('',#102092,0.0124999999999999);
#21821=CIRCLE('',#102094,0.0124999999999999);
#21822=CIRCLE('',#102101,0.00687500000000007);
#21823=CIRCLE('',#102105,0.0124999999999999);
#21824=CIRCLE('',#102106,2.74633883476483);
#21825=CIRCLE('',#102107,0.0125);
#21826=CIRCLE('',#102108,0.0124999999999999);
#21827=CIRCLE('',#102110,0.0124999999999999);
#21828=CIRCLE('',#102111,0.0125);
#21829=CIRCLE('',#102112,0.0125000000000003);
#21830=CIRCLE('',#102113,0.0125000000000003);
#21831=CIRCLE('',#102114,0.0124999999999997);
#21832=CIRCLE('',#102115,0.0124999999999999);
#21833=CIRCLE('',#102117,0.0125);
#21834=CIRCLE('',#102124,0.00687500000000009);
#21835=CIRCLE('',#102128,0.0125000000000001);
#21836=CIRCLE('',#102129,2.74633883476483);
#21837=CIRCLE('',#102130,0.0125000000000001);
#21838=CIRCLE('',#102131,0.0125000000000001);
#21839=CIRCLE('',#102133,0.0125);
#21840=CIRCLE('',#102134,0.0125000000000001);
#21841=CIRCLE('',#102135,0.0125000000000004);
#21842=CIRCLE('',#102136,0.0125000000000004);
#21843=CIRCLE('',#102137,0.0124999999999998);
#21844=CIRCLE('',#102138,0.0125000000000001);
#21845=CIRCLE('',#102140,0.0124999999999999);
#21846=CIRCLE('',#102147,0.00687499999999991);
#21847=CIRCLE('',#102151,0.0125000000000002);
#21848=CIRCLE('',#102152,2.74633883476483);
#21849=CIRCLE('',#102153,0.0124999999999999);
#21850=CIRCLE('',#102154,0.0125);
#21851=CIRCLE('',#102156,0.0125);
#21852=CIRCLE('',#102157,0.0125);
#21853=CIRCLE('',#102158,0.0125000000000005);
#21854=CIRCLE('',#102159,0.0125000000000005);
#21855=CIRCLE('',#102160,0.0124999999999997);
#21856=CIRCLE('',#102161,0.0125);
#21857=CIRCLE('',#102163,0.0125);
#21858=CIRCLE('',#102170,0.00687499999999998);
#21859=CIRCLE('',#102174,0.0125);
#21860=CIRCLE('',#102175,2.74633883476483);
#21861=CIRCLE('',#102176,0.0124999999999998);
#21862=CIRCLE('',#102177,0.0124999999999999);
#21863=CIRCLE('',#102179,0.0124999999999999);
#21864=CIRCLE('',#102180,0.0125000000000001);
#21865=CIRCLE('',#102181,0.0125000000000004);
#21866=CIRCLE('',#102182,0.0125000000000004);
#21867=CIRCLE('',#102183,0.0124999999999998);
#21868=CIRCLE('',#102184,0.0124999999999999);
#21869=CIRCLE('',#102186,0.0125);
#21870=CIRCLE('',#102193,0.00687499999999995);
#21871=CIRCLE('',#102197,0.0124999999999999);
#21872=CIRCLE('',#102198,2.74633883476483);
#21873=CIRCLE('',#102199,0.0125);
#21874=CIRCLE('',#102200,0.0125);
#21875=CIRCLE('',#102202,0.0125);
#21876=CIRCLE('',#102203,0.0125);
#21877=CIRCLE('',#102204,0.0125000000000005);
#21878=CIRCLE('',#102205,0.0125000000000005);
#21879=CIRCLE('',#102206,0.0124999999999997);
#21880=CIRCLE('',#102207,0.0125);
#21881=CIRCLE('',#102209,0.0125000000000001);
#21882=CIRCLE('',#102216,0.00687499999999993);
#21883=CIRCLE('',#102220,0.0124999999999999);
#21884=CIRCLE('',#102221,2.74633883476483);
#21885=CIRCLE('',#102222,0.0124999999999999);
#21886=CIRCLE('',#102223,0.0125);
#21887=CIRCLE('',#102225,0.0125);
#21888=CIRCLE('',#102226,0.0124999999999999);
#21889=CIRCLE('',#102227,0.0125000000000004);
#21890=CIRCLE('',#102228,0.0125000000000004);
#21891=CIRCLE('',#102229,0.0124999999999999);
#21892=CIRCLE('',#102230,0.0125);
#21893=CIRCLE('',#102232,0.0125);
#21894=CIRCLE('',#102239,0.00687499999999999);
#21895=CIRCLE('',#102243,0.0124999999999998);
#21896=CIRCLE('',#102244,2.74633883476483);
#21897=CIRCLE('',#102245,0.0125000000000002);
#21898=CIRCLE('',#102246,0.0125);
#21899=CIRCLE('',#102248,0.0125);
#21900=CIRCLE('',#102249,0.0125000000000001);
#21901=CIRCLE('',#102250,0.0125000000000003);
#21902=CIRCLE('',#102251,0.0125000000000003);
#21903=CIRCLE('',#102252,0.0124999999999997);
#21904=CIRCLE('',#102253,0.0125);
#21905=CIRCLE('',#102255,0.0125);
#21906=CIRCLE('',#102262,0.00687499999999997);
#21907=CIRCLE('',#102266,0.0125000000000001);
#21908=CIRCLE('',#102267,2.74633883476483);
#21909=CIRCLE('',#102268,0.0125000000000001);
#21910=CIRCLE('',#102269,0.0125);
#21911=CIRCLE('',#102271,0.0125);
#21912=CIRCLE('',#102272,0.0125000000000001);
#21913=CIRCLE('',#102273,0.0125000000000004);
#21914=CIRCLE('',#102274,0.0125000000000004);
#21915=CIRCLE('',#102275,0.0124999999999998);
#21916=CIRCLE('',#102276,0.0125);
#21917=CIRCLE('',#102278,0.0125);
#21918=CIRCLE('',#102285,0.00687499999999996);
#21919=CIRCLE('',#102289,0.0124999999999998);
#21920=CIRCLE('',#102290,2.74633883476483);
#21921=CIRCLE('',#102291,0.0124999999999998);
#21922=CIRCLE('',#102292,0.0125);
#21923=CIRCLE('',#102294,0.0125);
#21924=CIRCLE('',#102295,0.0125000000000001);
#21925=CIRCLE('',#102296,0.0125000000000003);
#21926=CIRCLE('',#102297,0.0125000000000003);
#21927=CIRCLE('',#102298,0.0124999999999998);
#21928=CIRCLE('',#102299,0.0125);
#21929=CIRCLE('',#102301,0.0125);
#21930=CIRCLE('',#102308,0.00687499999999999);
#21931=CIRCLE('',#102312,0.0124999999999999);
#21932=CIRCLE('',#102313,2.74633883476483);
#21933=CIRCLE('',#102314,0.0124999999999999);
#21934=CIRCLE('',#102315,0.0125);
#21935=CIRCLE('',#102317,0.0125);
#21936=CIRCLE('',#102318,0.0124999999999999);
#21937=CIRCLE('',#102319,0.0125000000000004);
#21938=CIRCLE('',#102320,0.0125000000000004);
#21939=CIRCLE('',#102321,0.0124999999999999);
#21940=CIRCLE('',#102322,0.0125);
#21941=CIRCLE('',#102324,0.0125);
#21942=CIRCLE('',#102331,0.00687499999999995);
#21943=CIRCLE('',#102335,0.0125);
#21944=CIRCLE('',#102336,2.74633883476483);
#21945=CIRCLE('',#102337,0.0124999999999999);
#21946=CIRCLE('',#102338,0.0125);
#21947=CIRCLE('',#102340,0.0125);
#21948=CIRCLE('',#102341,0.0125);
#21949=CIRCLE('',#102342,0.0125000000000002);
#21950=CIRCLE('',#102343,0.0125000000000002);
#21951=CIRCLE('',#102344,0.0124999999999997);
#21952=CIRCLE('',#102345,0.0125);
#21953=CIRCLE('',#102347,0.0125);
#21954=CIRCLE('',#102354,0.00687499999999988);
#21955=CIRCLE('',#102358,0.0124999999999999);
#21956=CIRCLE('',#102359,2.74633883476483);
#21957=CIRCLE('',#102360,0.0125000000000001);
#21958=CIRCLE('',#102361,0.0125000000000001);
#21959=CIRCLE('',#102363,0.0125000000000001);
#21960=CIRCLE('',#102364,0.0125000000000001);
#21961=CIRCLE('',#102365,0.0125000000000004);
#21962=CIRCLE('',#102366,0.0125000000000004);
#21963=CIRCLE('',#102367,0.0124999999999998);
#21964=CIRCLE('',#102368,0.0125000000000001);
#21965=CIRCLE('',#102370,0.0125000000000001);
#21966=CIRCLE('',#102377,0.00687500000000005);
#21967=CIRCLE('',#102381,0.0125);
#21968=CIRCLE('',#102382,2.74633883476483);
#21969=CIRCLE('',#102383,0.0124999999999998);
#21970=CIRCLE('',#102384,0.0125);
#21971=CIRCLE('',#102386,0.0125);
#21972=CIRCLE('',#102387,0.0125000000000001);
#21973=CIRCLE('',#102388,0.0125000000000005);
#21974=CIRCLE('',#102389,0.0125000000000005);
#21975=CIRCLE('',#102390,0.0124999999999997);
#21976=CIRCLE('',#102391,0.0125);
#21977=CIRCLE('',#102393,0.0125);
#21978=CIRCLE('',#102400,0.0068749999999999);
#21979=CIRCLE('',#102404,0.0125000000000001);
#21980=CIRCLE('',#102405,2.74633883476483);
#21981=CIRCLE('',#102406,0.0124999999999998);
#21982=CIRCLE('',#102407,0.0125000000000001);
#21983=CIRCLE('',#102409,0.0125000000000001);
#21984=CIRCLE('',#102410,0.0124999999999999);
#21985=CIRCLE('',#102411,0.0125000000000004);
#21986=CIRCLE('',#102412,0.0125000000000004);
#21987=CIRCLE('',#102413,0.0124999999999998);
#21988=CIRCLE('',#102414,0.0125);
#21989=CIRCLE('',#102416,0.0125000000000001);
#21990=CIRCLE('',#102423,0.00687499999999987);
#21991=CIRCLE('',#102427,0.0125000000000001);
#21992=CIRCLE('',#102428,2.74633883476483);
#21993=CIRCLE('',#102429,0.0125);
#21994=CIRCLE('',#102430,0.0125);
#21995=CIRCLE('',#102432,0.0125);
#21996=CIRCLE('',#102433,0.0125);
#21997=CIRCLE('',#102434,0.0125000000000003);
#21998=CIRCLE('',#102435,0.0125000000000003);
#21999=CIRCLE('',#102436,0.0124999999999997);
#22000=CIRCLE('',#102437,0.0125);
#22001=CIRCLE('',#102439,0.0125000000000001);
#22002=CIRCLE('',#102446,0.0068749999999999);
#22003=CIRCLE('',#102450,0.0125000000000002);
#22004=CIRCLE('',#102451,2.74633883476483);
#22005=CIRCLE('',#102452,0.0125);
#22006=CIRCLE('',#102453,0.0124999999999999);
#22007=CIRCLE('',#102455,0.0124999999999999);
#22008=CIRCLE('',#102456,0.0124999999999999);
#22009=CIRCLE('',#102457,0.0125000000000005);
#22010=CIRCLE('',#102458,0.0125000000000005);
#22011=CIRCLE('',#102459,0.0124999999999998);
#22012=CIRCLE('',#102460,0.0124999999999999);
#22013=CIRCLE('',#102462,0.0125000000000001);
#22014=CIRCLE('',#102469,0.00687499999999986);
#22015=CIRCLE('',#102473,0.0125);
#22016=CIRCLE('',#102474,2.74633883476483);
#22017=CIRCLE('',#102475,0.0125);
#22018=CIRCLE('',#102476,0.0125000000000001);
#22019=CIRCLE('',#102478,0.0125000000000001);
#22020=CIRCLE('',#102479,0.0124999999999999);
#22021=CIRCLE('',#102480,0.0125000000000005);
#22022=CIRCLE('',#102481,0.0125000000000005);
#22023=CIRCLE('',#102482,0.0124999999999998);
#22024=CIRCLE('',#102483,0.0125000000000001);
#22025=CIRCLE('',#102485,0.0125);
#22026=CIRCLE('',#102492,0.00687499999999985);
#22027=CIRCLE('',#102496,0.0124999999999998);
#22028=CIRCLE('',#102497,2.74633883476483);
#22029=CIRCLE('',#102498,0.0124999999999999);
#22030=CIRCLE('',#102499,0.0125000000000001);
#22031=CIRCLE('',#102501,0.0125000000000001);
#22032=CIRCLE('',#102502,0.0125);
#22033=CIRCLE('',#102503,0.0125000000000004);
#22034=CIRCLE('',#102504,0.0125000000000004);
#22035=CIRCLE('',#102505,0.0124999999999999);
#22036=CIRCLE('',#102506,0.0125000000000001);
#22037=CIRCLE('',#102508,0.0124999999999999);
#22038=CIRCLE('',#102515,0.00687499999999996);
#22039=CIRCLE('',#102519,0.0125);
#22040=CIRCLE('',#102520,2.74633883476483);
#22041=CIRCLE('',#102521,0.0125000000000001);
#22042=CIRCLE('',#102522,0.0125000000000001);
#22043=CIRCLE('',#102524,0.0125000000000001);
#22044=CIRCLE('',#102525,0.0125000000000001);
#22045=CIRCLE('',#102526,0.0125000000000004);
#22046=CIRCLE('',#102527,0.0125000000000004);
#22047=CIRCLE('',#102528,0.0124999999999998);
#22048=CIRCLE('',#102529,0.0125000000000001);
#22049=CIRCLE('',#102531,0.0125);
#22050=CIRCLE('',#102538,0.00687499999999994);
#22051=CIRCLE('',#102542,0.0124999999999999);
#22052=CIRCLE('',#102543,2.74633883476483);
#22053=CIRCLE('',#102544,0.0124999999999999);
#22054=CIRCLE('',#102545,0.0125);
#22055=CIRCLE('',#102547,0.0125);
#22056=CIRCLE('',#102548,0.0125000000000001);
#22057=CIRCLE('',#102549,0.0125000000000003);
#22058=CIRCLE('',#102550,0.0125000000000003);
#22059=CIRCLE('',#102551,0.0124999999999998);
#22060=CIRCLE('',#102552,0.0125000000000001);
#22061=CIRCLE('',#102554,0.0125000000000001);
#22062=CIRCLE('',#102561,0.00687499999999994);
#22063=CIRCLE('',#102565,0.0125);
#22064=CIRCLE('',#102566,2.74633883476483);
#22065=CIRCLE('',#102567,0.0124999999999999);
#22066=CIRCLE('',#102568,0.0125);
#22067=CIRCLE('',#102570,0.0125);
#22068=CIRCLE('',#102571,0.0124999999999999);
#22069=CIRCLE('',#102572,0.0125000000000005);
#22070=CIRCLE('',#102573,0.0125000000000005);
#22071=CIRCLE('',#102574,0.0124999999999998);
#22072=CIRCLE('',#102575,0.0125);
#22073=CIRCLE('',#102577,0.0124999999999998);
#22074=CIRCLE('',#102584,0.00687499999999985);
#22075=CIRCLE('',#102588,0.0125000000000001);
#22076=CIRCLE('',#102589,2.74633883476483);
#22077=CIRCLE('',#102590,0.0125000000000001);
#22078=CIRCLE('',#102591,0.0125);
#22079=CIRCLE('',#102593,0.0125);
#22080=CIRCLE('',#102594,0.0125000000000001);
#22081=CIRCLE('',#102595,0.0125000000000004);
#22082=CIRCLE('',#102596,0.0125000000000004);
#22083=CIRCLE('',#102597,0.0124999999999997);
#22084=CIRCLE('',#102598,0.0125);
#22085=CIRCLE('',#102600,0.0125);
#22086=CIRCLE('',#102607,0.00687500000000006);
#22087=CIRCLE('',#102611,0.0125);
#22088=CIRCLE('',#102612,2.74633883476483);
#22089=CIRCLE('',#102613,0.0124999999999998);
#22090=CIRCLE('',#102614,0.0125);
#22091=CIRCLE('',#102616,0.0125);
#22092=CIRCLE('',#102617,0.0125000000000001);
#22093=CIRCLE('',#102618,0.0125000000000004);
#22094=CIRCLE('',#102619,0.0125000000000004);
#22095=CIRCLE('',#102620,0.0124999999999997);
#22096=CIRCLE('',#102621,0.0125);
#22097=CIRCLE('',#102623,0.0125);
#22098=CIRCLE('',#102630,0.00687500000000008);
#22099=CIRCLE('',#102634,0.0125000000000001);
#22100=CIRCLE('',#102635,2.74633883476483);
#22101=CIRCLE('',#102636,0.0124999999999999);
#22102=CIRCLE('',#102637,0.0124999999999999);
#22103=CIRCLE('',#102639,0.0124999999999999);
#22104=CIRCLE('',#102640,0.0125000000000001);
#22105=CIRCLE('',#102641,0.0125000000000004);
#22106=CIRCLE('',#102642,0.0125000000000004);
#22107=CIRCLE('',#102643,0.0124999999999998);
#22108=CIRCLE('',#102644,0.0124999999999999);
#22109=CIRCLE('',#102646,0.0124999999999998);
#22110=CIRCLE('',#102650,1.17524047358087);
#22111=CIRCLE('',#102687,1.17524047358085);
#22112=CIRCLE('',#102689,1.17524047358087);
#22113=CIRCLE('',#102691,1.50000000000006);
#22114=CIRCLE('',#102726,1.50000000000006);
#22115=CIRCLE('',#102727,1.50000000000005);
#22116=CIRCLE('',#102729,2.7435563491861);
#22117=CIRCLE('',#102730,0.0220000000000001);
#22118=CIRCLE('',#102731,2.75);
#22119=CIRCLE('',#102732,0.0219999999999999);
#22120=CIRCLE('',#102734,2.7435563491861);
#22121=CIRCLE('',#102735,0.0219999999999998);
#22122=CIRCLE('',#102736,2.75);
#22123=CIRCLE('',#102737,0.0219999999999999);
#22124=CIRCLE('',#102739,2.7435563491861);
#22125=CIRCLE('',#102740,0.022);
#22126=CIRCLE('',#102741,2.75);
#22127=CIRCLE('',#102742,0.0220000000000001);
#22128=CIRCLE('',#102744,2.7435563491861);
#22129=CIRCLE('',#102745,0.0219999999999999);
#22130=CIRCLE('',#102746,2.75);
#22131=CIRCLE('',#102747,0.0220000000000001);
#22132=CIRCLE('',#102749,2.7435563491861);
#22133=CIRCLE('',#102750,0.0219999999999999);
#22134=CIRCLE('',#102751,2.75);
#22135=CIRCLE('',#102752,0.0219999999999998);
#22136=CIRCLE('',#102754,2.7435563491861);
#22137=CIRCLE('',#102755,0.0220000000000001);
#22138=CIRCLE('',#102756,2.75);
#22139=CIRCLE('',#102757,0.0220000000000001);
#22140=CIRCLE('',#102759,2.7435563491861);
#22141=CIRCLE('',#102760,0.0220000000000001);
#22142=CIRCLE('',#102761,2.75);
#22143=CIRCLE('',#102762,0.022);
#22144=CIRCLE('',#102764,2.7435563491861);
#22145=CIRCLE('',#102765,0.022);
#22146=CIRCLE('',#102766,2.75);
#22147=CIRCLE('',#102767,0.0219999999999998);
#22148=CIRCLE('',#102769,2.74355634918611);
#22149=CIRCLE('',#102770,0.0220000000000002);
#22150=CIRCLE('',#102771,2.75);
#22151=CIRCLE('',#102772,0.022);
#22152=CIRCLE('',#102774,2.7435563491861);
#22153=CIRCLE('',#102775,0.0220000000000002);
#22154=CIRCLE('',#102776,2.75);
#22155=CIRCLE('',#102777,0.0220000000000002);
#22156=CIRCLE('',#102779,2.74355634918611);
#22157=CIRCLE('',#102780,0.0219999999999998);
#22158=CIRCLE('',#102781,2.75);
#22159=CIRCLE('',#102782,0.0219999999999998);
#22160=CIRCLE('',#102784,2.7435563491861);
#22161=CIRCLE('',#102785,0.022);
#22162=CIRCLE('',#102786,2.75);
#22163=CIRCLE('',#102787,0.0219999999999998);
#22164=CIRCLE('',#102789,2.7435563491861);
#22165=CIRCLE('',#102790,0.0220000000000001);
#22166=CIRCLE('',#102791,2.75);
#22167=CIRCLE('',#102792,0.0219999999999998);
#22168=CIRCLE('',#102794,2.7435563491861);
#22169=CIRCLE('',#102795,0.022);
#22170=CIRCLE('',#102796,2.75);
#22171=CIRCLE('',#102797,0.0220000000000002);
#22172=CIRCLE('',#102799,2.7435563491861);
#22173=CIRCLE('',#102800,0.0219999999999998);
#22174=CIRCLE('',#102801,2.75);
#22175=CIRCLE('',#102802,0.022);
#22176=CIRCLE('',#102804,2.7435563491861);
#22177=CIRCLE('',#102805,0.0219999999999998);
#22178=CIRCLE('',#102806,2.75);
#22179=CIRCLE('',#102807,0.0220000000000002);
#22180=CIRCLE('',#102809,2.7435563491861);
#22181=CIRCLE('',#102810,0.022);
#22182=CIRCLE('',#102811,2.75);
#22183=CIRCLE('',#102812,0.022);
#22184=CIRCLE('',#102814,2.7435563491861);
#22185=CIRCLE('',#102815,0.0219999999999999);
#22186=CIRCLE('',#102816,2.75);
#22187=CIRCLE('',#102817,0.0220000000000001);
#22188=CIRCLE('',#102819,2.7435563491861);
#22189=CIRCLE('',#102820,0.022);
#22190=CIRCLE('',#102821,2.75);
#22191=CIRCLE('',#102822,0.0220000000000001);
#22192=CIRCLE('',#102824,2.7435563491861);
#22193=CIRCLE('',#102825,0.0220000000000001);
#22194=CIRCLE('',#102826,2.75);
#22195=CIRCLE('',#102827,0.022);
#22196=CIRCLE('',#102829,2.7435563491861);
#22197=CIRCLE('',#102830,0.022);
#22198=CIRCLE('',#102831,2.75);
#22199=CIRCLE('',#102832,0.0219999999999999);
#22200=CIRCLE('',#102834,2.7435563491861);
#22201=CIRCLE('',#102835,0.022);
#22202=CIRCLE('',#102836,2.75);
#22203=CIRCLE('',#102837,0.0219999999999998);
#22204=CIRCLE('',#102839,2.74355634918611);
#22205=CIRCLE('',#102840,0.0220000000000002);
#22206=CIRCLE('',#102841,2.75);
#22207=CIRCLE('',#102842,0.022);
#22208=CIRCLE('',#102844,2.7435563491861);
#22209=CIRCLE('',#102845,0.0220000000000001);
#22210=CIRCLE('',#102846,2.75);
#22211=CIRCLE('',#102847,0.0219999999999998);
#22212=CIRCLE('',#102849,2.7435563491861);
#22213=CIRCLE('',#102850,0.0220000000000001);
#22214=CIRCLE('',#102851,2.75);
#22215=CIRCLE('',#102852,0.0219999999999998);
#22216=CIRCLE('',#102854,2.7435563491861);
#22217=CIRCLE('',#102855,0.0219999999999999);
#22218=CIRCLE('',#102856,2.75);
#22219=CIRCLE('',#102857,0.0219999999999999);
#22220=CIRCLE('',#102859,2.74355634918611);
#22221=CIRCLE('',#102860,0.0219999999999999);
#22222=CIRCLE('',#102861,2.75);
#22223=CIRCLE('',#102862,0.0220000000000002);
#22224=CIRCLE('',#102864,2.7435563491861);
#22225=CIRCLE('',#102865,0.0220000000000002);
#22226=CIRCLE('',#102866,2.75);
#22227=CIRCLE('',#102867,0.0219999999999999);
#22228=CIRCLE('',#102869,2.74355634918611);
#22229=CIRCLE('',#102870,0.0219999999999999);
#22230=CIRCLE('',#102871,2.75);
#22231=CIRCLE('',#102872,0.0219999999999999);
#22232=CIRCLE('',#102874,2.7435563491861);
#22233=CIRCLE('',#102875,0.0219999999999998);
#22234=CIRCLE('',#102876,2.75);
#22235=CIRCLE('',#102877,0.022);
#22236=CIRCLE('',#102879,2.7435563491861);
#22237=CIRCLE('',#102880,0.0220000000000001);
#22238=CIRCLE('',#102881,2.75);
#22239=CIRCLE('',#102882,0.022);
#22240=CIRCLE('',#102884,2.7435563491861);
#22241=CIRCLE('',#102885,0.022);
#22242=CIRCLE('',#102886,2.75);
#22243=CIRCLE('',#102887,0.022);
#22244=CIRCLE('',#102889,2.7435563491861);
#22245=CIRCLE('',#102890,0.0220000000000001);
#22246=CIRCLE('',#102891,2.75);
#22247=CIRCLE('',#102892,0.0219999999999998);
#22248=CIRCLE('',#102894,2.7435563491861);
#22249=CIRCLE('',#102895,0.0220000000000002);
#22250=CIRCLE('',#102896,2.75);
#22251=CIRCLE('',#102897,0.0220000000000001);
#22252=CIRCLE('',#102899,2.7435563491861);
#22253=CIRCLE('',#102900,0.0220000000000002);
#22254=CIRCLE('',#102901,2.75);
#22255=CIRCLE('',#102902,0.022);
#22256=CIRCLE('',#102904,2.7435563491861);
#22257=CIRCLE('',#102905,0.022);
#22258=CIRCLE('',#102906,2.75);
#22259=CIRCLE('',#102907,0.0219999999999998);
#22260=CIRCLE('',#102909,2.7435563491861);
#22261=CIRCLE('',#102910,0.0220000000000001);
#22262=CIRCLE('',#102911,2.75);
#22263=CIRCLE('',#102912,0.0220000000000001);
#22264=CIRCLE('',#102914,2.7435563491861);
#22265=CIRCLE('',#102915,0.0220000000000001);
#22266=CIRCLE('',#102916,2.75);
#22267=CIRCLE('',#102917,0.0219999999999999);
#22268=CIRCLE('',#102919,2.7435563491861);
#22269=CIRCLE('',#102920,0.022);
#22270=CIRCLE('',#102921,2.75);
#22271=CIRCLE('',#102922,0.0219999999999999);
#22272=CIRCLE('',#102924,2.7435563491861);
#22273=CIRCLE('',#102925,0.0219999999999998);
#22274=CIRCLE('',#102926,2.75);
#22275=CIRCLE('',#102927,0.022);
#22276=CIRCLE('',#102929,2.7435563491861);
#22277=CIRCLE('',#102930,0.0219999999999999);
#22278=CIRCLE('',#102931,2.75);
#22279=CIRCLE('',#102932,0.0220000000000001);
#22280=CIRCLE('',#102934,2.7435563491861);
#22281=CIRCLE('',#102935,0.0219999999999999);
#22282=CIRCLE('',#102936,2.75);
#22283=CIRCLE('',#102937,0.0220000000000002);
#22284=CIRCLE('',#102939,2.74355634918611);
#22285=CIRCLE('',#102940,0.0219999999999999);
#22286=CIRCLE('',#102941,2.75);
#22287=CIRCLE('',#102942,0.022);
#22288=CIRCLE('',#102944,2.7435563491861);
#22289=CIRCLE('',#102945,0.0219999999999999);
#22290=CIRCLE('',#102946,2.75);
#22291=CIRCLE('',#102947,0.0219999999999999);
#22292=CIRCLE('',#102949,2.7435563491861);
#22293=CIRCLE('',#102950,0.0219999999999998);
#22294=CIRCLE('',#102951,2.75);
#22295=CIRCLE('',#102952,0.0219999999999998);
#22296=CIRCLE('',#102954,2.74355634918611);
#22297=CIRCLE('',#102955,0.022);
#22298=CIRCLE('',#102956,2.75);
#22299=CIRCLE('',#102957,0.0220000000000002);
#22300=CIRCLE('',#102959,2.7435563491861);
#22301=CIRCLE('',#102960,0.0219999999999998);
#22302=CIRCLE('',#102961,2.75);
#22303=CIRCLE('',#102962,0.022);
#22304=CIRCLE('',#102964,2.7435563491861);
#22305=CIRCLE('',#102965,0.022);
#22306=CIRCLE('',#102966,2.75);
#22307=CIRCLE('',#102967,0.0220000000000001);
#22308=CIRCLE('',#102969,2.7435563491861);
#22309=CIRCLE('',#102970,0.0220000000000001);
#22310=CIRCLE('',#102971,2.75);
#22311=CIRCLE('',#102972,0.022);
#22312=CIRCLE('',#102974,2.7435563491861);
#22313=CIRCLE('',#102975,0.0220000000000002);
#22314=CIRCLE('',#102976,2.75);
#22315=CIRCLE('',#102977,0.0219999999999999);
#22316=CIRCLE('',#102979,2.74355634918611);
#22317=CIRCLE('',#102980,0.022);
#22318=CIRCLE('',#102981,2.75);
#22319=CIRCLE('',#102982,0.0220000000000002);
#22320=CIRCLE('',#102984,2.7435563491861);
#22321=CIRCLE('',#102985,0.022);
#22322=CIRCLE('',#102986,2.75);
#22323=CIRCLE('',#102987,0.0219999999999999);
#22324=CIRCLE('',#102989,2.7435563491861);
#22325=CIRCLE('',#102990,0.0220000000000002);
#22326=CIRCLE('',#102991,2.75);
#22327=CIRCLE('',#102992,0.0220000000000001);
#22328=CIRCLE('',#102994,2.7435563491861);
#22329=CIRCLE('',#102995,0.0220000000000001);
#22330=CIRCLE('',#102996,2.75);
#22331=CIRCLE('',#102997,0.022);
#22332=CIRCLE('',#102999,2.7435563491861);
#22333=CIRCLE('',#103000,0.0220000000000001);
#22334=CIRCLE('',#103001,2.75);
#22335=CIRCLE('',#103002,0.022);
#22336=CIRCLE('',#103004,2.7435563491861);
#22337=CIRCLE('',#103005,0.0220000000000001);
#22338=CIRCLE('',#103006,2.75);
#22339=CIRCLE('',#103007,0.0220000000000001);
#22340=CIRCLE('',#103009,2.7435563491861);
#22341=CIRCLE('',#103010,0.0220000000000001);
#22342=CIRCLE('',#103011,2.75);
#22343=CIRCLE('',#103012,0.0219999999999999);
#22344=CIRCLE('',#103014,2.7435563491861);
#22345=CIRCLE('',#103015,0.0219999999999999);
#22346=CIRCLE('',#103016,2.75);
#22347=CIRCLE('',#103017,0.0220000000000001);
#22348=CIRCLE('',#103019,2.7435563491861);
#22349=CIRCLE('',#103020,0.0220000000000001);
#22350=CIRCLE('',#103021,2.75);
#22351=CIRCLE('',#103022,0.0220000000000001);
#22352=CIRCLE('',#103024,2.7435563491861);
#22353=CIRCLE('',#103025,0.0219999999999998);
#22354=CIRCLE('',#103026,2.75);
#22355=CIRCLE('',#103027,0.022);
#22356=CIRCLE('',#103029,2.7435563491861);
#22357=CIRCLE('',#103030,0.0219999999999999);
#22358=CIRCLE('',#103031,2.75);
#22359=CIRCLE('',#103032,0.022);
#22360=CIRCLE('',#103034,2.74355634918611);
#22361=CIRCLE('',#103035,0.0219999999999999);
#22362=CIRCLE('',#103036,2.75);
#22363=CIRCLE('',#103037,0.0220000000000001);
#22364=CIRCLE('',#103039,2.7435563491861);
#22365=CIRCLE('',#103040,0.0219999999999998);
#22366=CIRCLE('',#103041,2.75);
#22367=CIRCLE('',#103042,0.022);
#22368=CIRCLE('',#103044,2.7435563491861);
#22369=CIRCLE('',#103045,0.022);
#22370=CIRCLE('',#103046,2.75);
#22371=CIRCLE('',#103047,0.0219999999999999);
#22372=CIRCLE('',#103049,2.74355634918611);
#22373=CIRCLE('',#103050,0.0220000000000001);
#22374=CIRCLE('',#103051,2.75);
#22375=CIRCLE('',#103052,0.0219999999999999);
#22376=CIRCLE('',#103054,2.74355634918611);
#22377=CIRCLE('',#103055,0.0219999999999999);
#22378=CIRCLE('',#103056,2.75);
#22379=CIRCLE('',#103057,0.022);
#22380=CIRCLE('',#103059,2.7435563491861);
#22381=CIRCLE('',#103060,0.0220000000000001);
#22382=CIRCLE('',#103061,2.75);
#22383=CIRCLE('',#103062,0.0219999999999999);
#22384=CIRCLE('',#103064,2.7435563491861);
#22385=CIRCLE('',#103065,0.022);
#22386=CIRCLE('',#103066,2.75);
#22387=CIRCLE('',#103067,0.0220000000000001);
#22388=CIRCLE('',#103069,2.7435563491861);
#22389=CIRCLE('',#103070,0.022);
#22390=CIRCLE('',#103071,2.75);
#22391=CIRCLE('',#103072,0.022);
#22392=CIRCLE('',#103074,2.74355634918611);
#22393=CIRCLE('',#103075,0.0219999999999999);
#22394=CIRCLE('',#103076,2.75);
#22395=CIRCLE('',#103077,0.0220000000000001);
#22396=CIRCLE('',#103079,2.7435563491861);
#22397=CIRCLE('',#103080,0.0219999999999999);
#22398=CIRCLE('',#103081,2.75);
#22399=CIRCLE('',#103082,0.0220000000000002);
#22400=CIRCLE('',#103084,2.7435563491861);
#22401=CIRCLE('',#103085,0.022);
#22402=CIRCLE('',#103086,2.75);
#22403=CIRCLE('',#103087,0.0219999999999998);
#22404=CIRCLE('',#103089,2.7435563491861);
#22405=CIRCLE('',#103090,0.0219999999999999);
#22406=CIRCLE('',#103091,2.75);
#22407=CIRCLE('',#103092,0.0220000000000002);
#22408=CIRCLE('',#103094,2.74355634918611);
#22409=CIRCLE('',#103095,0.0219999999999999);
#22410=CIRCLE('',#103096,2.75);
#22411=CIRCLE('',#103097,0.0219999999999999);
#22412=CIRCLE('',#103099,2.7435563491861);
#22413=CIRCLE('',#103100,0.0220000000000001);
#22414=CIRCLE('',#103101,2.75);
#22415=CIRCLE('',#103102,0.0219999999999999);
#22416=CIRCLE('',#103104,2.7435563491861);
#22417=CIRCLE('',#103105,0.0219999999999999);
#22418=CIRCLE('',#103106,2.75);
#22419=CIRCLE('',#103107,0.0220000000000001);
#22420=CIRCLE('',#103109,2.7435563491861);
#22421=CIRCLE('',#103110,0.0220000000000001);
#22422=CIRCLE('',#103111,2.75);
#22423=CIRCLE('',#103112,2.75);
#22424=CIRCLE('',#103113,0.0220000000000001);
#22425=CIRCLE('',#103116,1.17524047358087);
#22426=CIRCLE('',#103118,1.62500000000006);
#22427=CIRCLE('',#103121,1.25);
#22428=CIRCLE('',#103122,1.25);
#22429=CIRCLE('',#103123,1.25);
#22430=CIRCLE('',#103124,1.25);
#22431=CIRCLE('',#103125,1.25);
#22432=CIRCLE('',#103126,1.25);
#22433=CIRCLE('',#103128,1.44337567297406);
#22434=CIRCLE('',#103130,2.55577460325564);
#22435=CIRCLE('',#103131,0.0879999999999989);
#22436=CIRCLE('',#103132,2.49354920651122);
#22437=CIRCLE('',#103134,2.72422539674443);
#22438=CIRCLE('',#103136,2.75);
#22439=CIRCLE('',#103137,0.088000000000018);
#22440=CIRCLE('',#103139,2.72422539674441);
#22441=CIRCLE('',#103140,2.72422539674441);
#22442=CIRCLE('',#103141,2.72422539674441);
#22443=CIRCLE('',#103142,2.72422539674441);
#22444=CIRCLE('',#103143,2.72422539674441);
#22445=CIRCLE('',#103144,2.72422539674441);
#22446=CIRCLE('',#103145,2.72422539674441);
#22447=CIRCLE('',#103146,2.72422539674441);
#22448=CIRCLE('',#103147,2.72422539674441);
#22449=CIRCLE('',#103148,2.72422539674441);
#22450=CIRCLE('',#103149,2.72422539674441);
#22451=CIRCLE('',#103150,2.72422539674441);
#22452=CIRCLE('',#103151,2.72422539674441);
#22453=CIRCLE('',#103152,2.72422539674441);
#22454=CIRCLE('',#103153,2.72422539674441);
#22455=CIRCLE('',#103154,2.72422539674441);
#22456=CIRCLE('',#103155,2.72422539674441);
#22457=CIRCLE('',#103156,2.72422539674441);
#22458=CIRCLE('',#103157,2.72422539674441);
#22459=CIRCLE('',#103158,2.72422539674441);
#22460=CIRCLE('',#103159,2.72422539674441);
#22461=CIRCLE('',#103160,2.72422539674441);
#22462=CIRCLE('',#103161,2.72422539674441);
#22463=CIRCLE('',#103162,2.72422539674441);
#22464=CIRCLE('',#103163,2.72422539674441);
#22465=CIRCLE('',#103164,2.72422539674441);
#22466=CIRCLE('',#103165,2.72422539674441);
#22467=CIRCLE('',#103166,2.72422539674441);
#22468=CIRCLE('',#103167,2.72422539674441);
#22469=CIRCLE('',#103168,2.72422539674441);
#22470=CIRCLE('',#103169,2.72422539674441);
#22471=CIRCLE('',#103170,2.72422539674441);
#22472=CIRCLE('',#103171,2.72422539674441);
#22473=CIRCLE('',#103172,2.72422539674441);
#22474=CIRCLE('',#103173,2.72422539674441);
#22475=CIRCLE('',#103174,2.72422539674441);
#22476=CIRCLE('',#103175,2.72422539674441);
#22477=CIRCLE('',#103176,2.72422539674441);
#22478=CIRCLE('',#103177,2.72422539674441);
#22479=CIRCLE('',#103178,2.55577460325558);
#22480=CIRCLE('',#103179,2.55577460325558);
#22481=CIRCLE('',#103180,2.72422539674441);
#22482=CIRCLE('',#103181,2.72422539674441);
#22483=CIRCLE('',#103182,2.72422539674441);
#22484=CIRCLE('',#103183,2.72422539674441);
#22485=CIRCLE('',#103184,2.72422539674441);
#22486=CIRCLE('',#103185,2.72422539674441);
#22487=CIRCLE('',#103186,2.72422539674441);
#22488=CIRCLE('',#103187,2.72422539674441);
#22489=CIRCLE('',#103188,2.72422539674441);
#22490=CIRCLE('',#103189,2.72422539674441);
#22491=CIRCLE('',#103190,2.72422539674441);
#22492=CIRCLE('',#103191,2.72422539674441);
#22493=CIRCLE('',#103192,2.72422539674441);
#22494=CIRCLE('',#103193,2.72422539674441);
#22495=CIRCLE('',#103194,2.72422539674441);
#22496=CIRCLE('',#103195,2.72422539674441);
#22497=CIRCLE('',#103196,2.72422539674441);
#22498=CIRCLE('',#103197,2.72422539674441);
#22499=CIRCLE('',#103198,2.72422539674441);
#22500=CIRCLE('',#103199,2.72422539674441);
#22501=CIRCLE('',#103200,2.72422539674441);
#22502=CIRCLE('',#103201,2.72422539674441);
#22503=CIRCLE('',#103202,2.72422539674441);
#22504=CIRCLE('',#103203,2.72422539674441);
#22505=CIRCLE('',#103204,2.72422539674441);
#22506=CIRCLE('',#103205,2.72422539674441);
#22507=CIRCLE('',#103206,2.72422539674441);
#22508=CIRCLE('',#103207,2.72422539674441);
#22509=CIRCLE('',#103208,2.72422539674441);
#22510=CIRCLE('',#103209,2.72422539674441);
#22511=CIRCLE('',#103210,2.72422539674441);
#22512=CIRCLE('',#103211,2.72422539674441);
#22513=CIRCLE('',#103212,2.72422539674441);
#22514=CIRCLE('',#103213,2.72422539674441);
#22515=CIRCLE('',#103214,2.72422539674441);
#22516=CIRCLE('',#103215,2.72422539674441);
#22517=CIRCLE('',#103216,2.72422539674441);
#22518=CIRCLE('',#103217,2.72422539674441);
#22519=CIRCLE('',#103218,2.72422539674441);
#22520=CIRCLE('',#103220,2.49354920651117);
#22521=CIRCLE('',#103221,0.0879999999999994);
#22522=CIRCLE('',#103223,2.75);
#22523=CIRCLE('',#103224,2.75);
#22524=CIRCLE('',#103225,2.75);
#22525=CIRCLE('',#103226,2.75);
#22526=CIRCLE('',#103227,2.75);
#22527=CIRCLE('',#103228,2.75);
#22528=CIRCLE('',#103229,2.75);
#22529=CIRCLE('',#103230,2.75);
#22530=CIRCLE('',#103231,2.75);
#22531=CIRCLE('',#103232,2.75);
#22532=CIRCLE('',#103233,2.75);
#22533=CIRCLE('',#103234,2.75);
#22534=CIRCLE('',#103235,2.75);
#22535=CIRCLE('',#103236,2.75);
#22536=CIRCLE('',#103237,2.75);
#22537=CIRCLE('',#103238,2.75);
#22538=CIRCLE('',#103239,2.75);
#22539=CIRCLE('',#103240,2.75);
#22540=CIRCLE('',#103241,2.75);
#22541=CIRCLE('',#103242,2.75);
#22542=CIRCLE('',#103243,2.75);
#22543=CIRCLE('',#103244,2.75);
#22544=CIRCLE('',#103245,2.75);
#22545=CIRCLE('',#103246,2.75);
#22546=CIRCLE('',#103247,2.75);
#22547=CIRCLE('',#103248,2.75);
#22548=CIRCLE('',#103249,2.75);
#22549=CIRCLE('',#103250,2.75);
#22550=CIRCLE('',#103251,2.75);
#22551=CIRCLE('',#103252,2.75);
#22552=CIRCLE('',#103253,2.75);
#22553=CIRCLE('',#103254,2.75);
#22554=CIRCLE('',#103255,2.75);
#22555=CIRCLE('',#103256,2.75);
#22556=CIRCLE('',#103257,2.75);
#22557=CIRCLE('',#103258,2.75);
#22558=CIRCLE('',#103259,2.75);
#22559=CIRCLE('',#103260,2.75);
#22560=CIRCLE('',#103261,2.75);
#22561=CIRCLE('',#103262,2.75);
#22562=CIRCLE('',#103263,2.75);
#22563=CIRCLE('',#103264,2.75);
#22564=CIRCLE('',#103265,2.75);
#22565=CIRCLE('',#103266,2.75);
#22566=CIRCLE('',#103267,2.75);
#22567=CIRCLE('',#103268,2.75);
#22568=CIRCLE('',#103269,2.75);
#22569=CIRCLE('',#103270,2.75);
#22570=CIRCLE('',#103271,2.75);
#22571=CIRCLE('',#103272,2.75);
#22572=CIRCLE('',#103273,2.75);
#22573=CIRCLE('',#103274,2.75);
#22574=CIRCLE('',#103275,2.75);
#22575=CIRCLE('',#103276,2.75);
#22576=CIRCLE('',#103277,2.75);
#22577=CIRCLE('',#103278,2.75);
#22578=CIRCLE('',#103279,2.75);
#22579=CIRCLE('',#103280,2.75);
#22580=CIRCLE('',#103281,2.75);
#22581=CIRCLE('',#103282,2.75);
#22582=CIRCLE('',#103283,2.75);
#22583=CIRCLE('',#103284,2.75);
#22584=CIRCLE('',#103285,2.75);
#22585=CIRCLE('',#103286,2.75);
#22586=CIRCLE('',#103287,2.75);
#22587=CIRCLE('',#103288,2.75);
#22588=CIRCLE('',#103289,2.75);
#22589=CIRCLE('',#103290,2.75);
#22590=CIRCLE('',#103291,2.75);
#22591=CIRCLE('',#103292,2.75);
#22592=CIRCLE('',#103293,2.75);
#22593=CIRCLE('',#103294,2.75);
#22594=CIRCLE('',#103295,2.75);
#22595=CIRCLE('',#103296,2.75);
#22596=CIRCLE('',#103297,2.75);
#22597=CIRCLE('',#103298,2.75);
#22598=CIRCLE('',#103299,2.75);
#22599=CIRCLE('',#103542,1.44337567297406);
#22600=CIRCLE('',#103543,1.44337567297406);
#22601=CIRCLE('',#103544,1.44337567297406);
#22602=CIRCLE('',#103545,1.44337567297406);
#22603=CIRCLE('',#103546,1.44337567297406);
#22604=CIRCLE('',#103566,0.0220000000000002);
#22605=CIRCLE('',#103568,0.022);
#22606=CIRCLE('',#103569,0.022);
#22607=CIRCLE('',#103570,0.0220000000000002);
#22608=CIRCLE('',#103571,0.0219999999999993);
#22609=CIRCLE('',#103572,0.0220000000000001);
#22610=CIRCLE('',#103573,0.022);
#22611=CIRCLE('',#103574,0.0220000000000001);
#22612=CIRCLE('',#103576,0.022);
#22613=CIRCLE('',#103577,0.0219999999999993);
#22614=CIRCLE('',#103585,0.0220000000000002);
#22615=CIRCLE('',#103586,0.0220000000000002);
#22616=CIRCLE('',#103588,0.022);
#22617=CIRCLE('',#103590,0.022);
#22618=CIRCLE('',#103591,0.0219999999999995);
#22619=CIRCLE('',#103592,0.022);
#22620=CIRCLE('',#103593,0.0220000000000001);
#22621=CIRCLE('',#103594,0.0219999999999995);
#22622=CIRCLE('',#103595,0.022);
#22623=CIRCLE('',#103597,0.022);
#22624=CIRCLE('',#103606,0.0220000000000002);
#22625=CIRCLE('',#103607,0.0220000000000002);
#22626=CIRCLE('',#103609,0.022);
#22627=CIRCLE('',#103611,0.022);
#22628=CIRCLE('',#103612,0.0219999999999995);
#22629=CIRCLE('',#103613,0.022);
#22630=CIRCLE('',#103614,0.022);
#22631=CIRCLE('',#103615,0.0219999999999995);
#22632=CIRCLE('',#103616,0.022);
#22633=CIRCLE('',#103618,0.022);
#22634=CIRCLE('',#103627,0.0220000000000004);
#22635=CIRCLE('',#103628,0.0220000000000004);
#22636=CIRCLE('',#103630,0.022);
#22637=CIRCLE('',#103632,0.022);
#22638=CIRCLE('',#103633,0.0219999999999993);
#22639=CIRCLE('',#103634,0.0220000000000002);
#22640=CIRCLE('',#103635,0.0220000000000002);
#22641=CIRCLE('',#103636,0.0219999999999993);
#22642=CIRCLE('',#103637,0.022);
#22643=CIRCLE('',#103639,0.022);
#22644=CIRCLE('',#103648,0.0220000000000002);
#22645=CIRCLE('',#103649,0.0220000000000002);
#22646=CIRCLE('',#103651,0.022);
#22647=CIRCLE('',#103653,0.022);
#22648=CIRCLE('',#103654,0.0219999999999996);
#22649=CIRCLE('',#103655,0.0220000000000001);
#22650=CIRCLE('',#103656,0.0220000000000001);
#22651=CIRCLE('',#103657,0.0219999999999993);
#22652=CIRCLE('',#103658,0.022);
#22653=CIRCLE('',#103660,0.022);
#22654=CIRCLE('',#103669,0.0220000000000002);
#22655=CIRCLE('',#103670,0.0220000000000002);
#22656=CIRCLE('',#103672,0.022);
#22657=CIRCLE('',#103674,0.022);
#22658=CIRCLE('',#103675,0.0219999999999993);
#22659=CIRCLE('',#103676,0.0220000000000002);
#22660=CIRCLE('',#103677,0.0220000000000002);
#22661=CIRCLE('',#103678,0.0219999999999993);
#22662=CIRCLE('',#103679,0.022);
#22663=CIRCLE('',#103681,0.0220000000000001);
#22664=CIRCLE('',#103690,0.0220000000000004);
#22665=CIRCLE('',#103691,0.0220000000000004);
#22666=CIRCLE('',#103693,0.022);
#22667=CIRCLE('',#103695,0.022);
#22668=CIRCLE('',#103696,0.0219999999999993);
#22669=CIRCLE('',#103697,0.0220000000000002);
#22670=CIRCLE('',#103698,0.0220000000000002);
#22671=CIRCLE('',#103699,0.0219999999999993);
#22672=CIRCLE('',#103700,0.022);
#22673=CIRCLE('',#103702,0.022);
#22674=CIRCLE('',#103711,0.0220000000000004);
#22675=CIRCLE('',#103712,0.0220000000000004);
#22676=CIRCLE('',#103714,0.022);
#22677=CIRCLE('',#103716,0.022);
#22678=CIRCLE('',#103717,0.0219999999999995);
#22679=CIRCLE('',#103718,0.0220000000000001);
#22680=CIRCLE('',#103719,0.0220000000000001);
#22681=CIRCLE('',#103720,0.0219999999999995);
#22682=CIRCLE('',#103721,0.022);
#22683=CIRCLE('',#103723,0.022);
#22684=CIRCLE('',#103732,0.0220000000000003);
#22685=CIRCLE('',#103733,0.0220000000000003);
#22686=CIRCLE('',#103735,0.022);
#22687=CIRCLE('',#103737,0.022);
#22688=CIRCLE('',#103738,0.0219999999999994);
#22689=CIRCLE('',#103739,0.0220000000000003);
#22690=CIRCLE('',#103740,0.0220000000000003);
#22691=CIRCLE('',#103741,0.0219999999999994);
#22692=CIRCLE('',#103742,0.022);
#22693=CIRCLE('',#103744,0.0219999999999999);
#22694=CIRCLE('',#103753,0.0220000000000003);
#22695=CIRCLE('',#103754,0.0220000000000003);
#22696=CIRCLE('',#103756,0.0219999999999999);
#22697=CIRCLE('',#103758,0.0219999999999999);
#22698=CIRCLE('',#103759,0.0219999999999994);
#22699=CIRCLE('',#103760,0.0220000000000002);
#22700=CIRCLE('',#103761,0.0220000000000002);
#22701=CIRCLE('',#103762,0.0219999999999994);
#22702=CIRCLE('',#103763,0.0219999999999999);
#22703=CIRCLE('',#103765,0.022);
#22704=CIRCLE('',#103774,0.0220000000000003);
#22705=CIRCLE('',#103775,0.0220000000000003);
#22706=CIRCLE('',#103777,0.022);
#22707=CIRCLE('',#103779,0.022);
#22708=CIRCLE('',#103780,0.0219999999999994);
#22709=CIRCLE('',#103781,0.0220000000000002);
#22710=CIRCLE('',#103782,0.0220000000000001);
#22711=CIRCLE('',#103783,0.0219999999999994);
#22712=CIRCLE('',#103784,0.022);
#22713=CIRCLE('',#103786,0.0219999999999999);
#22714=CIRCLE('',#103795,0.0220000000000003);
#22715=CIRCLE('',#103796,0.0220000000000003);
#22716=CIRCLE('',#103798,0.022);
#22717=CIRCLE('',#103800,0.022);
#22718=CIRCLE('',#103801,0.0219999999999995);
#22719=CIRCLE('',#103802,0.0220000000000001);
#22720=CIRCLE('',#103803,0.0220000000000001);
#22721=CIRCLE('',#103804,0.0219999999999995);
#22722=CIRCLE('',#103805,0.0220000000000002);
#22723=CIRCLE('',#103807,0.0219999999999999);
#22724=CIRCLE('',#103816,0.0220000000000002);
#22725=CIRCLE('',#103817,0.0220000000000002);
#22726=CIRCLE('',#103819,0.0219999999999999);
#22727=CIRCLE('',#103821,0.0219999999999999);
#22728=CIRCLE('',#103822,0.0219999999999996);
#22729=CIRCLE('',#103823,0.0220000000000001);
#22730=CIRCLE('',#103824,0.0220000000000001);
#22731=CIRCLE('',#103825,0.0219999999999996);
#22732=CIRCLE('',#103826,0.0219999999999999);
#22733=CIRCLE('',#103828,0.0220000000000001);
#22734=CIRCLE('',#103837,0.0220000000000004);
#22735=CIRCLE('',#103838,0.0220000000000004);
#22736=CIRCLE('',#103840,0.022);
#22737=CIRCLE('',#103842,0.022);
#22738=CIRCLE('',#103843,0.0219999999999994);
#22739=CIRCLE('',#103844,0.0220000000000002);
#22740=CIRCLE('',#103845,0.0220000000000002);
#22741=CIRCLE('',#103846,0.0219999999999994);
#22742=CIRCLE('',#103847,0.022);
#22743=CIRCLE('',#103849,0.022);
#22744=CIRCLE('',#103858,0.0220000000000002);
#22745=CIRCLE('',#103859,0.0220000000000002);
#22746=CIRCLE('',#103861,0.022);
#22747=CIRCLE('',#103863,0.022);
#22748=CIRCLE('',#103864,0.0219999999999994);
#22749=CIRCLE('',#103865,0.0220000000000002);
#22750=CIRCLE('',#103866,0.0220000000000002);
#22751=CIRCLE('',#103867,0.0219999999999994);
#22752=CIRCLE('',#103868,0.022);
#22753=CIRCLE('',#103870,0.022);
#22754=CIRCLE('',#103879,0.0220000000000003);
#22755=CIRCLE('',#103880,0.0220000000000003);
#22756=CIRCLE('',#103882,0.022);
#22757=CIRCLE('',#103884,0.0220000000000001);
#22758=CIRCLE('',#103885,0.0219999999999994);
#22759=CIRCLE('',#103886,0.0220000000000002);
#22760=CIRCLE('',#103887,0.0220000000000002);
#22761=CIRCLE('',#103888,0.0219999999999994);
#22762=CIRCLE('',#103889,0.0220000000000001);
#22763=CIRCLE('',#103891,0.0220000000000001);
#22764=CIRCLE('',#103900,0.0220000000000004);
#22765=CIRCLE('',#103901,0.0220000000000004);
#22766=CIRCLE('',#103903,0.022);
#22767=CIRCLE('',#103905,0.022);
#22768=CIRCLE('',#103906,0.0219999999999994);
#22769=CIRCLE('',#103907,0.0220000000000003);
#22770=CIRCLE('',#103908,0.0220000000000003);
#22771=CIRCLE('',#103909,0.0219999999999994);
#22772=CIRCLE('',#103910,0.022);
#22773=CIRCLE('',#103912,0.022);
#22774=CIRCLE('',#103921,0.0220000000000004);
#22775=CIRCLE('',#103922,0.0220000000000004);
#22776=CIRCLE('',#103924,0.022);
#22777=CIRCLE('',#103926,0.022);
#22778=CIRCLE('',#103927,0.0219999999999996);
#22779=CIRCLE('',#103928,0.0220000000000002);
#22780=CIRCLE('',#103929,0.0220000000000002);
#22781=CIRCLE('',#103930,0.0219999999999996);
#22782=CIRCLE('',#103931,0.022);
#22783=CIRCLE('',#103933,0.022);
#22784=CIRCLE('',#103942,0.0220000000000004);
#22785=CIRCLE('',#103943,0.0220000000000004);
#22786=CIRCLE('',#103945,0.022);
#22787=CIRCLE('',#103947,0.022);
#22788=CIRCLE('',#103948,0.0219999999999994);
#22789=CIRCLE('',#103949,0.0220000000000001);
#22790=CIRCLE('',#103950,0.0220000000000001);
#22791=CIRCLE('',#103951,0.0219999999999994);
#22792=CIRCLE('',#103952,0.022);
#22793=CIRCLE('',#103954,0.022);
#22794=CIRCLE('',#103963,0.0220000000000004);
#22795=CIRCLE('',#103964,0.0220000000000004);
#22796=CIRCLE('',#103966,0.022);
#22797=CIRCLE('',#103968,0.022);
#22798=CIRCLE('',#103969,0.0219999999999995);
#22799=CIRCLE('',#103970,0.0220000000000001);
#22800=CIRCLE('',#103971,0.0220000000000001);
#22801=CIRCLE('',#103972,0.0219999999999995);
#22802=CIRCLE('',#103973,0.022);
#22803=CIRCLE('',#103975,0.022);
#22804=CIRCLE('',#103984,0.0220000000000004);
#22805=CIRCLE('',#103985,0.0220000000000004);
#22806=CIRCLE('',#103987,0.0220000000000001);
#22807=CIRCLE('',#103989,0.0220000000000001);
#22808=CIRCLE('',#103990,0.0219999999999995);
#22809=CIRCLE('',#103991,0.0220000000000001);
#22810=CIRCLE('',#103992,0.0220000000000002);
#22811=CIRCLE('',#103993,0.0219999999999995);
#22812=CIRCLE('',#103994,0.0220000000000001);
#22813=CIRCLE('',#103996,0.022);
#22814=CIRCLE('',#104005,0.0220000000000002);
#22815=CIRCLE('',#104006,0.0220000000000003);
#22816=CIRCLE('',#104008,0.022);
#22817=CIRCLE('',#104010,0.022);
#22818=CIRCLE('',#104011,0.0219999999999994);
#22819=CIRCLE('',#104012,0.022);
#22820=CIRCLE('',#104013,0.0220000000000002);
#22821=CIRCLE('',#104014,0.0219999999999995);
#22822=CIRCLE('',#104015,0.022);
#22823=CIRCLE('',#104017,0.022);
#22824=CIRCLE('',#104026,0.0220000000000004);
#22825=CIRCLE('',#104027,0.0220000000000004);
#22826=CIRCLE('',#104029,0.0220000000000001);
#22827=CIRCLE('',#104031,0.0220000000000001);
#22828=CIRCLE('',#104032,0.0219999999999995);
#22829=CIRCLE('',#104033,0.0220000000000001);
#22830=CIRCLE('',#104034,0.0220000000000001);
#22831=CIRCLE('',#104035,0.0219999999999995);
#22832=CIRCLE('',#104036,0.0220000000000001);
#22833=CIRCLE('',#104038,0.022);
#22834=CIRCLE('',#104047,0.0220000000000004);
#22835=CIRCLE('',#104048,0.0220000000000004);
#22836=CIRCLE('',#104050,0.0219999999999999);
#22837=CIRCLE('',#104052,0.0219999999999999);
#22838=CIRCLE('',#104053,0.0219999999999995);
#22839=CIRCLE('',#104054,0.0220000000000001);
#22840=CIRCLE('',#104055,0.0220000000000001);
#22841=CIRCLE('',#104056,0.0219999999999995);
#22842=CIRCLE('',#104057,0.0219999999999999);
#22843=CIRCLE('',#104059,0.022);
#22844=CIRCLE('',#104068,0.0220000000000003);
#22845=CIRCLE('',#104069,0.0220000000000003);
#22846=CIRCLE('',#104071,0.0220000000000001);
#22847=CIRCLE('',#104073,0.0220000000000001);
#22848=CIRCLE('',#104074,0.0219999999999996);
#22849=CIRCLE('',#104075,0.0220000000000003);
#22850=CIRCLE('',#104076,0.0220000000000003);
#22851=CIRCLE('',#104077,0.0219999999999996);
#22852=CIRCLE('',#104078,0.0220000000000001);
#22853=CIRCLE('',#104080,0.0220000000000001);
#22854=CIRCLE('',#104089,0.0220000000000002);
#22855=CIRCLE('',#104090,0.0220000000000002);
#22856=CIRCLE('',#104092,0.022);
#22857=CIRCLE('',#104094,0.022);
#22858=CIRCLE('',#104095,0.0219999999999996);
#22859=CIRCLE('',#104096,0.0220000000000002);
#22860=CIRCLE('',#104097,0.0220000000000002);
#22861=CIRCLE('',#104098,0.0219999999999993);
#22862=CIRCLE('',#104099,0.022);
#22863=CIRCLE('',#104101,0.022);
#22864=CIRCLE('',#104110,0.0220000000000003);
#22865=CIRCLE('',#104111,0.0220000000000003);
#22866=CIRCLE('',#104113,0.0220000000000001);
#22867=CIRCLE('',#104115,0.0220000000000001);
#22868=CIRCLE('',#104116,0.0219999999999994);
#22869=CIRCLE('',#104117,0.0220000000000002);
#22870=CIRCLE('',#104118,0.0220000000000002);
#22871=CIRCLE('',#104119,0.0219999999999994);
#22872=CIRCLE('',#104120,0.0220000000000001);
#22873=CIRCLE('',#104122,0.0219999999999999);
#22874=CIRCLE('',#104131,0.0220000000000003);
#22875=CIRCLE('',#104132,0.0220000000000003);
#22876=CIRCLE('',#104134,0.022);
#22877=CIRCLE('',#104136,0.022);
#22878=CIRCLE('',#104137,0.0219999999999994);
#22879=CIRCLE('',#104138,0.0220000000000002);
#22880=CIRCLE('',#104139,0.0220000000000002);
#22881=CIRCLE('',#104140,0.0219999999999994);
#22882=CIRCLE('',#104141,0.022);
#22883=CIRCLE('',#104143,0.022);
#22884=CIRCLE('',#104152,0.0220000000000002);
#22885=CIRCLE('',#104153,0.0220000000000002);
#22886=CIRCLE('',#104155,0.022);
#22887=CIRCLE('',#104157,0.022);
#22888=CIRCLE('',#104158,0.0219999999999993);
#22889=CIRCLE('',#104159,0.0220000000000001);
#22890=CIRCLE('',#104160,0.0220000000000001);
#22891=CIRCLE('',#104161,0.0219999999999993);
#22892=CIRCLE('',#104162,0.022);
#22893=CIRCLE('',#104164,0.022);
#22894=CIRCLE('',#104173,0.0220000000000002);
#22895=CIRCLE('',#104174,0.0220000000000002);
#22896=CIRCLE('',#104176,0.022);
#22897=CIRCLE('',#104178,0.022);
#22898=CIRCLE('',#104179,0.0219999999999995);
#22899=CIRCLE('',#104180,0.0220000000000003);
#22900=CIRCLE('',#104181,0.0220000000000003);
#22901=CIRCLE('',#104182,0.0219999999999995);
#22902=CIRCLE('',#104183,0.022);
#22903=CIRCLE('',#104185,0.022);
#22904=CIRCLE('',#104194,0.0220000000000003);
#22905=CIRCLE('',#104195,0.0220000000000003);
#22906=CIRCLE('',#104197,0.022);
#22907=CIRCLE('',#104199,0.022);
#22908=CIRCLE('',#104200,0.0219999999999994);
#22909=CIRCLE('',#104201,0.0220000000000002);
#22910=CIRCLE('',#104202,0.0220000000000002);
#22911=CIRCLE('',#104203,0.0219999999999994);
#22912=CIRCLE('',#104204,0.022);
#22913=CIRCLE('',#104206,0.022);
#22914=CIRCLE('',#104215,0.0220000000000004);
#22915=CIRCLE('',#104216,0.0220000000000004);
#22916=CIRCLE('',#104218,0.022);
#22917=CIRCLE('',#104220,0.022);
#22918=CIRCLE('',#104221,0.0219999999999996);
#22919=CIRCLE('',#104222,0.0220000000000002);
#22920=CIRCLE('',#104223,0.0220000000000002);
#22921=CIRCLE('',#104224,0.0219999999999996);
#22922=CIRCLE('',#104225,0.022);
#22923=CIRCLE('',#104227,0.022);
#22924=CIRCLE('',#104236,0.0220000000000004);
#22925=CIRCLE('',#104237,0.0220000000000004);
#22926=CIRCLE('',#104239,0.022);
#22927=CIRCLE('',#104241,0.022);
#22928=CIRCLE('',#104242,0.0219999999999996);
#22929=CIRCLE('',#104243,0.0220000000000002);
#22930=CIRCLE('',#104244,0.0220000000000002);
#22931=CIRCLE('',#104245,0.0219999999999993);
#22932=CIRCLE('',#104246,0.022);
#22933=CIRCLE('',#104248,0.022);
#22934=CIRCLE('',#104257,0.0220000000000002);
#22935=CIRCLE('',#104258,0.0220000000000002);
#22936=CIRCLE('',#104260,0.022);
#22937=CIRCLE('',#104262,0.022);
#22938=CIRCLE('',#104263,0.0219999999999995);
#22939=CIRCLE('',#104264,0.0220000000000003);
#22940=CIRCLE('',#104265,0.0220000000000003);
#22941=CIRCLE('',#104266,0.0219999999999995);
#22942=CIRCLE('',#104267,0.022);
#22943=CIRCLE('',#104269,0.022);
#22944=CIRCLE('',#104278,0.0220000000000004);
#22945=CIRCLE('',#104279,0.0220000000000004);
#22946=CIRCLE('',#104281,0.022);
#22947=CIRCLE('',#104283,0.022);
#22948=CIRCLE('',#104284,0.0219999999999996);
#22949=CIRCLE('',#104285,0.0220000000000001);
#22950=CIRCLE('',#104286,0.0220000000000001);
#22951=CIRCLE('',#104287,0.0219999999999996);
#22952=CIRCLE('',#104288,0.022);
#22953=CIRCLE('',#104290,0.0220000000000001);
#22954=CIRCLE('',#104299,0.0220000000000003);
#22955=CIRCLE('',#104300,0.0220000000000003);
#22956=CIRCLE('',#104302,0.022);
#22957=CIRCLE('',#104304,0.022);
#22958=CIRCLE('',#104305,0.0219999999999996);
#22959=CIRCLE('',#104306,0.0220000000000002);
#22960=CIRCLE('',#104307,0.0220000000000002);
#22961=CIRCLE('',#104308,0.0219999999999996);
#22962=CIRCLE('',#104309,0.022);
#22963=CIRCLE('',#104311,0.022);
#22964=CIRCLE('',#104320,0.0220000000000004);
#22965=CIRCLE('',#104321,0.0220000000000004);
#22966=CIRCLE('',#104323,0.0219999999999998);
#22967=CIRCLE('',#104325,0.0219999999999998);
#22968=CIRCLE('',#104326,0.0219999999999995);
#22969=CIRCLE('',#104327,0.0220000000000002);
#22970=CIRCLE('',#104328,0.0220000000000002);
#22971=CIRCLE('',#104329,0.0219999999999995);
#22972=CIRCLE('',#104330,0.0219999999999998);
#22973=CIRCLE('',#104332,0.022);
#22974=CIRCLE('',#104341,0.0220000000000003);
#22975=CIRCLE('',#104342,0.0220000000000003);
#22976=CIRCLE('',#104344,0.022);
#22977=CIRCLE('',#104346,0.022);
#22978=CIRCLE('',#104347,0.0219999999999996);
#22979=CIRCLE('',#104348,0.0220000000000002);
#22980=CIRCLE('',#104349,0.0220000000000002);
#22981=CIRCLE('',#104350,0.0219999999999996);
#22982=CIRCLE('',#104351,0.022);
#22983=CIRCLE('',#104353,0.0219999999999999);
#22984=CIRCLE('',#104362,0.0220000000000002);
#22985=CIRCLE('',#104363,0.0220000000000002);
#22986=CIRCLE('',#104365,0.0219999999999999);
#22987=CIRCLE('',#104367,0.0219999999999999);
#22988=CIRCLE('',#104368,0.0219999999999994);
#22989=CIRCLE('',#104369,0.0220000000000001);
#22990=CIRCLE('',#104370,0.0220000000000001);
#22991=CIRCLE('',#104371,0.0219999999999994);
#22992=CIRCLE('',#104372,0.0219999999999999);
#22993=CIRCLE('',#104374,0.0219999999999998);
#22994=CIRCLE('',#104383,0.0220000000000004);
#22995=CIRCLE('',#104384,0.0220000000000004);
#22996=CIRCLE('',#104386,0.0219999999999998);
#22997=CIRCLE('',#104388,0.0219999999999998);
#22998=CIRCLE('',#104389,0.0219999999999995);
#22999=CIRCLE('',#104390,0.0220000000000003);
#23000=CIRCLE('',#104391,0.0220000000000003);
#23001=CIRCLE('',#104392,0.0219999999999995);
#23002=CIRCLE('',#104393,0.0219999999999998);
#23003=CIRCLE('',#104395,0.0219999999999999);
#23004=CIRCLE('',#104404,0.0220000000000003);
#23005=CIRCLE('',#104405,0.0220000000000003);
#23006=CIRCLE('',#104407,0.0220000000000002);
#23007=CIRCLE('',#104409,0.0220000000000002);
#23008=CIRCLE('',#104410,0.0219999999999995);
#23009=CIRCLE('',#104411,0.0220000000000001);
#23010=CIRCLE('',#104412,0.0220000000000001);
#23011=CIRCLE('',#104413,0.0219999999999995);
#23012=CIRCLE('',#104414,0.0219999999999999);
#23013=CIRCLE('',#104416,0.022);
#23014=CIRCLE('',#104425,0.0220000000000003);
#23015=CIRCLE('',#104426,0.0220000000000003);
#23016=CIRCLE('',#104428,0.0219999999999999);
#23017=CIRCLE('',#104430,0.0219999999999999);
#23018=CIRCLE('',#104431,0.0219999999999996);
#23019=CIRCLE('',#104432,0.0220000000000002);
#23020=CIRCLE('',#104433,0.0220000000000002);
#23021=CIRCLE('',#104434,0.0219999999999996);
#23022=CIRCLE('',#104435,0.0219999999999999);
#23023=CIRCLE('',#104437,0.022);
#23024=CIRCLE('',#104446,0.0220000000000003);
#23025=CIRCLE('',#104447,0.0220000000000003);
#23026=CIRCLE('',#104449,0.0220000000000001);
#23027=CIRCLE('',#104451,0.0220000000000001);
#23028=CIRCLE('',#104452,0.0219999999999995);
#23029=CIRCLE('',#104453,0.0220000000000003);
#23030=CIRCLE('',#104454,0.0220000000000003);
#23031=CIRCLE('',#104455,0.0219999999999995);
#23032=CIRCLE('',#104456,0.0220000000000001);
#23033=CIRCLE('',#104458,0.0219999999999999);
#23034=CIRCLE('',#104467,0.0220000000000004);
#23035=CIRCLE('',#104468,0.0220000000000004);
#23036=CIRCLE('',#104470,0.022);
#23037=CIRCLE('',#104472,0.022);
#23038=CIRCLE('',#104473,0.0219999999999994);
#23039=CIRCLE('',#104474,0.0220000000000001);
#23040=CIRCLE('',#104475,0.0220000000000001);
#23041=CIRCLE('',#104476,0.0219999999999994);
#23042=CIRCLE('',#104477,0.022);
#23043=CIRCLE('',#104479,0.0220000000000001);
#23044=CIRCLE('',#104488,0.0220000000000003);
#23045=CIRCLE('',#104489,0.0220000000000003);
#23046=CIRCLE('',#104491,0.0220000000000001);
#23047=CIRCLE('',#104493,0.0220000000000001);
#23048=CIRCLE('',#104494,0.0219999999999994);
#23049=CIRCLE('',#104495,0.0220000000000001);
#23050=CIRCLE('',#104496,0.0220000000000001);
#23051=CIRCLE('',#104497,0.0219999999999994);
#23052=CIRCLE('',#104498,0.0220000000000001);
#23053=CIRCLE('',#104500,0.0220000000000001);
#23054=CIRCLE('',#104509,0.0220000000000003);
#23055=CIRCLE('',#104510,0.0220000000000003);
#23056=CIRCLE('',#104512,0.022);
#23057=CIRCLE('',#104514,0.0219999999999999);
#23058=CIRCLE('',#104515,0.0219999999999994);
#23059=CIRCLE('',#104516,0.0220000000000003);
#23060=CIRCLE('',#104517,0.0220000000000003);
#23061=CIRCLE('',#104518,0.0219999999999994);
#23062=CIRCLE('',#104519,0.0219999999999999);
#23063=CIRCLE('',#104521,0.0220000000000001);
#23064=CIRCLE('',#104530,0.0220000000000002);
#23065=CIRCLE('',#104531,0.0220000000000002);
#23066=CIRCLE('',#104533,0.0219999999999999);
#23067=CIRCLE('',#104535,0.0219999999999999);
#23068=CIRCLE('',#104536,0.0219999999999994);
#23069=CIRCLE('',#104537,0.0220000000000001);
#23070=CIRCLE('',#104538,0.0220000000000001);
#23071=CIRCLE('',#104539,0.0219999999999994);
#23072=CIRCLE('',#104540,0.0219999999999999);
#23073=CIRCLE('',#104542,0.022);
#23074=CIRCLE('',#104551,0.0220000000000003);
#23075=CIRCLE('',#104552,0.0220000000000003);
#23076=CIRCLE('',#104554,0.022);
#23077=CIRCLE('',#104556,0.0220000000000001);
#23078=CIRCLE('',#104557,0.0219999999999994);
#23079=CIRCLE('',#104558,0.0220000000000001);
#23080=CIRCLE('',#104559,0.022);
#23081=CIRCLE('',#104560,0.0219999999999994);
#23082=CIRCLE('',#104561,0.022);
#23083=CIRCLE('',#104563,0.022);
#23084=CIRCLE('',#104572,0.0220000000000003);
#23085=CIRCLE('',#104573,0.0220000000000003);
#23086=CIRCLE('',#104575,0.022);
#23087=CIRCLE('',#104577,0.022);
#23088=CIRCLE('',#104578,0.0219999999999994);
#23089=CIRCLE('',#104579,0.0220000000000002);
#23090=CIRCLE('',#104580,0.0220000000000002);
#23091=CIRCLE('',#104581,0.0219999999999994);
#23092=CIRCLE('',#104582,0.022);
#23093=CIRCLE('',#104584,0.022);
#23094=CIRCLE('',#104593,0.0220000000000004);
#23095=CIRCLE('',#104594,0.0220000000000004);
#23096=CIRCLE('',#104596,0.022);
#23097=CIRCLE('',#104598,0.022);
#23098=CIRCLE('',#104599,0.0219999999999994);
#23099=CIRCLE('',#104600,0.022);
#23100=CIRCLE('',#104601,0.022);
#23101=CIRCLE('',#104602,0.0219999999999994);
#23102=CIRCLE('',#104603,0.022);
#23103=CIRCLE('',#104605,0.022);
#23104=CIRCLE('',#104614,0.0220000000000004);
#23105=CIRCLE('',#104615,0.0220000000000004);
#23106=CIRCLE('',#104617,0.022);
#23107=CIRCLE('',#104619,0.022);
#23108=CIRCLE('',#104620,0.0219999999999994);
#23109=CIRCLE('',#104621,0.022);
#23110=CIRCLE('',#104622,0.022);
#23111=CIRCLE('',#104623,0.0219999999999994);
#23112=CIRCLE('',#104624,0.022);
#23113=CIRCLE('',#104626,0.022);
#23114=CIRCLE('',#104635,0.0220000000000003);
#23115=CIRCLE('',#104636,0.0220000000000003);
#23116=CIRCLE('',#104638,0.022);
#23117=CIRCLE('',#104640,0.022);
#23118=CIRCLE('',#104641,0.0219999999999994);
#23119=CIRCLE('',#104642,0.0220000000000002);
#23120=CIRCLE('',#104643,0.0220000000000002);
#23121=CIRCLE('',#104644,0.0219999999999994);
#23122=CIRCLE('',#104645,0.022);
#23123=CIRCLE('',#104647,0.022);
#23124=CIRCLE('',#104656,0.0220000000000003);
#23125=CIRCLE('',#104657,0.0220000000000003);
#23126=CIRCLE('',#104659,0.022);
#23127=CIRCLE('',#104661,0.022);
#23128=CIRCLE('',#104662,0.0219999999999994);
#23129=CIRCLE('',#104663,0.0220000000000001);
#23130=CIRCLE('',#104664,0.0220000000000001);
#23131=CIRCLE('',#104665,0.0219999999999994);
#23132=CIRCLE('',#104666,0.022);
#23133=CIRCLE('',#104668,0.022);
#23134=CIRCLE('',#104677,0.0220000000000002);
#23135=CIRCLE('',#104678,0.0220000000000002);
#23136=CIRCLE('',#104680,0.022);
#23137=CIRCLE('',#104682,0.022);
#23138=CIRCLE('',#104683,0.0219999999999995);
#23139=CIRCLE('',#104684,0.0220000000000001);
#23140=CIRCLE('',#104685,0.0220000000000001);
#23141=CIRCLE('',#104686,0.0219999999999995);
#23142=CIRCLE('',#104687,0.022);
#23143=CIRCLE('',#104689,0.022);
#23144=CIRCLE('',#104698,0.0220000000000004);
#23145=CIRCLE('',#104699,0.0220000000000004);
#23146=CIRCLE('',#104701,0.0220000000000001);
#23147=CIRCLE('',#104703,0.0220000000000001);
#23148=CIRCLE('',#104704,0.0219999999999995);
#23149=CIRCLE('',#104705,0.022);
#23150=CIRCLE('',#104706,0.0220000000000001);
#23151=CIRCLE('',#104707,0.0219999999999995);
#23152=CIRCLE('',#104708,0.0220000000000001);
#23153=CIRCLE('',#104710,0.022);
#23154=CIRCLE('',#104719,0.0220000000000003);
#23155=CIRCLE('',#104720,0.0220000000000003);
#23156=CIRCLE('',#104722,0.0219999999999999);
#23157=CIRCLE('',#104724,0.0219999999999999);
#23158=CIRCLE('',#104725,0.0219999999999995);
#23159=CIRCLE('',#104726,0.0220000000000002);
#23160=CIRCLE('',#104727,0.0220000000000002);
#23161=CIRCLE('',#104728,0.0219999999999995);
#23162=CIRCLE('',#104729,0.0219999999999999);
#23163=CIRCLE('',#104731,0.0220000000000001);
#23164=CIRCLE('',#104740,0.0220000000000002);
#23165=CIRCLE('',#104741,0.0220000000000002);
#23166=CIRCLE('',#104743,0.0220000000000001);
#23167=CIRCLE('',#104745,0.0220000000000001);
#23168=CIRCLE('',#104746,0.0219999999999995);
#23169=CIRCLE('',#104747,0.0220000000000002);
#23170=CIRCLE('',#104748,0.0220000000000002);
#23171=CIRCLE('',#104749,0.0219999999999995);
#23172=CIRCLE('',#104750,0.0220000000000001);
#23173=CIRCLE('',#104752,0.0219999999999998);
#23174=CIRCLE('',#104761,0.0220000000000003);
#23175=CIRCLE('',#104762,0.0220000000000003);
#23176=CIRCLE('',#104764,0.0219999999999999);
#23177=CIRCLE('',#104766,0.0219999999999999);
#23178=CIRCLE('',#104767,0.0219999999999996);
#23179=CIRCLE('',#104768,0.0220000000000001);
#23180=CIRCLE('',#104769,0.0220000000000001);
#23181=CIRCLE('',#104770,0.0219999999999995);
#23182=CIRCLE('',#104771,0.0219999999999999);
#23183=CIRCLE('',#104773,0.0219999999999999);
#23184=CIRCLE('',#104782,0.0220000000000003);
#23185=CIRCLE('',#104783,0.0220000000000003);
#23186=CIRCLE('',#104785,0.022);
#23187=CIRCLE('',#104787,0.022);
#23188=CIRCLE('',#104788,0.0219999999999994);
#23189=CIRCLE('',#104789,0.0220000000000002);
#23190=CIRCLE('',#104790,0.0220000000000002);
#23191=CIRCLE('',#104791,0.0219999999999994);
#23192=CIRCLE('',#104792,0.022);
#23193=CIRCLE('',#104794,0.022);
#23194=CIRCLE('',#104803,0.0220000000000003);
#23195=CIRCLE('',#104804,0.0220000000000003);
#23196=CIRCLE('',#104806,0.022);
#23197=CIRCLE('',#104808,0.022);
#23198=CIRCLE('',#104809,0.0219999999999995);
#23199=CIRCLE('',#104810,0.0220000000000001);
#23200=CIRCLE('',#104811,0.0220000000000003);
#23201=CIRCLE('',#104812,0.0219999999999995);
#23202=CIRCLE('',#104813,0.022);
#23203=CIRCLE('',#104815,0.0219999999999999);
#23204=CIRCLE('',#104824,0.0220000000000003);
#23205=CIRCLE('',#104825,0.0220000000000003);
#23206=CIRCLE('',#104827,0.022);
#23207=CIRCLE('',#104829,0.022);
#23208=CIRCLE('',#104830,0.0219999999999994);
#23209=CIRCLE('',#104831,0.0220000000000002);
#23210=CIRCLE('',#104832,0.0220000000000002);
#23211=CIRCLE('',#104833,0.0219999999999994);
#23212=CIRCLE('',#104834,0.022);
#23213=CIRCLE('',#104836,0.022);
#23214=CIRCLE('',#104845,0.0220000000000004);
#23215=CIRCLE('',#104846,0.0220000000000004);
#23216=CIRCLE('',#104848,0.0220000000000001);
#23217=CIRCLE('',#104850,0.0220000000000001);
#23218=CIRCLE('',#104851,0.0219999999999993);
#23219=CIRCLE('',#104852,0.0220000000000003);
#23220=CIRCLE('',#104853,0.0220000000000003);
#23221=CIRCLE('',#104854,0.0219999999999993);
#23222=CIRCLE('',#104855,0.0220000000000001);
#23223=CIRCLE('',#104857,0.0219999999999999);
#23224=CIRCLE('',#104866,0.0220000000000002);
#23225=CIRCLE('',#104867,0.0220000000000002);
#23226=CIRCLE('',#104869,0.022);
#23227=CIRCLE('',#104871,0.022);
#23228=CIRCLE('',#104872,0.0219999999999995);
#23229=CIRCLE('',#104873,0.0220000000000002);
#23230=CIRCLE('',#104874,0.0220000000000002);
#23231=CIRCLE('',#104875,0.0219999999999995);
#23232=CIRCLE('',#104876,0.022);
#23233=CIRCLE('',#104878,0.022);
#23234=CIRCLE('',#104887,0.0220000000000003);
#23235=CIRCLE('',#104888,0.0220000000000003);
#23236=CIRCLE('',#104890,0.022);
#23237=CIRCLE('',#104892,0.022);
#23238=CIRCLE('',#104893,0.0219999999999995);
#23239=CIRCLE('',#104894,0.0220000000000002);
#23240=CIRCLE('',#104895,0.0220000000000002);
#23241=CIRCLE('',#104896,0.0219999999999994);
#23242=CIRCLE('',#104897,0.022);
#23243=CIRCLE('',#104899,0.022);
#23244=CIRCLE('',#104908,0.0220000000000002);
#23245=CIRCLE('',#104909,0.0220000000000002);
#23246=CIRCLE('',#104911,0.0219999999999999);
#23247=CIRCLE('',#104913,0.022);
#23248=CIRCLE('',#104914,0.0219999999999995);
#23249=CIRCLE('',#104915,0.0220000000000002);
#23250=CIRCLE('',#104916,0.0220000000000002);
#23251=CIRCLE('',#104917,0.0219999999999995);
#23252=CIRCLE('',#104918,0.022);
#23253=CIRCLE('',#104920,0.022);
#23254=CIRCLE('',#104929,0.0220000000000004);
#23255=CIRCLE('',#104930,0.0220000000000004);
#23256=CIRCLE('',#104932,0.0220000000000001);
#23257=CIRCLE('',#104934,0.0220000000000001);
#23258=CIRCLE('',#104935,0.0219999999999995);
#23259=CIRCLE('',#104936,0.0220000000000001);
#23260=CIRCLE('',#104937,0.022);
#23261=CIRCLE('',#104938,0.0219999999999995);
#23262=CIRCLE('',#104939,0.0220000000000001);
#23263=CIRCLE('',#104941,0.022);
#23264=CIRCLE('',#104950,0.0220000000000004);
#23265=CIRCLE('',#104951,0.0220000000000004);
#23266=CIRCLE('',#104953,0.022);
#23267=CIRCLE('',#104955,0.022);
#23268=CIRCLE('',#104956,0.0219999999999995);
#23269=CIRCLE('',#104957,0.0220000000000002);
#23270=CIRCLE('',#104958,0.0220000000000002);
#23271=CIRCLE('',#104959,0.0219999999999995);
#23272=CIRCLE('',#104960,0.022);
#23273=CIRCLE('',#104962,0.022);
#23274=CIRCLE('',#104971,0.0220000000000004);
#23275=CIRCLE('',#104972,0.0220000000000004);
#23276=CIRCLE('',#104974,0.022);
#23277=CIRCLE('',#104976,0.022);
#23278=CIRCLE('',#104977,0.0219999999999996);
#23279=CIRCLE('',#104978,0.0220000000000002);
#23280=CIRCLE('',#104979,0.0220000000000002);
#23281=CIRCLE('',#104980,0.0219999999999996);
#23282=CIRCLE('',#104981,0.022);
#23283=CIRCLE('',#104983,0.022);
#23284=CIRCLE('',#104992,0.0220000000000004);
#23285=CIRCLE('',#104993,0.0220000000000004);
#23286=CIRCLE('',#104995,0.022);
#23287=CIRCLE('',#104997,0.022);
#23288=CIRCLE('',#104998,0.0219999999999996);
#23289=CIRCLE('',#104999,0.0220000000000002);
#23290=CIRCLE('',#105000,0.0220000000000002);
#23291=CIRCLE('',#105001,0.0219999999999996);
#23292=CIRCLE('',#105002,0.022);
#23293=CIRCLE('',#105004,0.022);
#23294=CIRCLE('',#105013,0.0220000000000003);
#23295=CIRCLE('',#105014,0.0220000000000003);
#23296=CIRCLE('',#105016,0.022);
#23297=CIRCLE('',#105018,0.022);
#23298=CIRCLE('',#105019,0.0219999999999994);
#23299=CIRCLE('',#105020,0.0220000000000002);
#23300=CIRCLE('',#105021,0.0220000000000002);
#23301=CIRCLE('',#105022,0.0219999999999994);
#23302=CIRCLE('',#105023,0.022);
#23303=CIRCLE('',#105025,0.022);
#23304=CIRCLE('',#105034,0.0220000000000003);
#23305=CIRCLE('',#105035,0.0220000000000003);
#23306=CIRCLE('',#105037,0.022);
#23307=CIRCLE('',#105039,0.022);
#23308=CIRCLE('',#105040,0.0219999999999995);
#23309=CIRCLE('',#105041,0.0220000000000003);
#23310=CIRCLE('',#105042,0.0220000000000003);
#23311=CIRCLE('',#105043,0.0219999999999995);
#23312=CIRCLE('',#105044,0.022);
#23313=CIRCLE('',#105046,0.022);
#23314=CIRCLE('',#105055,0.0220000000000002);
#23315=CIRCLE('',#105056,0.0220000000000002);
#23316=CIRCLE('',#105058,0.022);
#23317=CIRCLE('',#105060,0.022);
#23318=CIRCLE('',#105061,0.0219999999999994);
#23319=CIRCLE('',#105062,0.0220000000000001);
#23320=CIRCLE('',#105063,0.0220000000000001);
#23321=CIRCLE('',#105064,0.0219999999999994);
#23322=CIRCLE('',#105065,0.022);
#23323=CIRCLE('',#105067,0.022);
#23324=CIRCLE('',#105076,0.0220000000000004);
#23325=CIRCLE('',#105077,0.0220000000000004);
#23326=CIRCLE('',#105079,0.022);
#23327=CIRCLE('',#105081,0.022);
#23328=CIRCLE('',#105082,0.0219999999999994);
#23329=CIRCLE('',#105083,0.0220000000000003);
#23330=CIRCLE('',#105084,0.0220000000000003);
#23331=CIRCLE('',#105085,0.0219999999999994);
#23332=CIRCLE('',#105086,0.022);
#23333=CIRCLE('',#105088,0.022);
#23334=CIRCLE('',#105097,0.0220000000000003);
#23335=CIRCLE('',#105098,0.0220000000000003);
#23336=CIRCLE('',#105100,0.0219999999999999);
#23337=CIRCLE('',#105102,0.022);
#23338=CIRCLE('',#105103,0.0219999999999995);
#23339=CIRCLE('',#105104,0.0220000000000002);
#23340=CIRCLE('',#105105,0.0220000000000002);
#23341=CIRCLE('',#105106,0.0219999999999995);
#23342=CIRCLE('',#105107,0.022);
#23343=CIRCLE('',#105109,0.0219999999999999);
#23344=CIRCLE('',#105118,0.0220000000000002);
#23345=CIRCLE('',#105119,0.0220000000000002);
#23346=CIRCLE('',#105121,0.022);
#23347=CIRCLE('',#105123,0.022);
#23348=CIRCLE('',#105124,0.0219999999999994);
#23349=CIRCLE('',#105125,0.0220000000000003);
#23350=CIRCLE('',#105126,0.0220000000000003);
#23351=CIRCLE('',#105127,0.0219999999999994);
#23352=CIRCLE('',#105128,0.022);
#23353=CIRCLE('',#105130,0.022);
#23354=CIRCLE('',#105139,0.0220000000000004);
#23355=CIRCLE('',#105140,0.0220000000000004);
#23356=CIRCLE('',#105142,0.0219999999999999);
#23357=CIRCLE('',#105144,0.0219999999999999);
#23358=CIRCLE('',#105145,0.0219999999999994);
#23359=CIRCLE('',#105146,0.0220000000000003);
#23360=CIRCLE('',#105147,0.0220000000000003);
#23361=CIRCLE('',#105148,0.0219999999999994);
#23362=CIRCLE('',#105149,0.0219999999999999);
#23363=CIRCLE('',#105151,0.0220000000000001);
#23364=CIRCLE('',#105160,0.0220000000000002);
#23365=CIRCLE('',#105161,0.0220000000000002);
#23366=CIRCLE('',#105163,0.022);
#23367=CIRCLE('',#105165,0.022);
#23368=CIRCLE('',#105166,0.0219999999999996);
#23369=CIRCLE('',#105167,0.0220000000000002);
#23370=CIRCLE('',#105168,0.0220000000000002);
#23371=CIRCLE('',#105169,0.0219999999999995);
#23372=CIRCLE('',#105170,0.022);
#23373=CIRCLE('',#105172,0.0220000000000001);
#23374=CIRCLE('',#105177,1.03775);
#23375=CIRCLE('',#105179,1.03775);
#23376=CIRCLE('',#105186,1.03775);
#23377=CIRCLE('',#105188,1.29);
#23378=CIRCLE('',#105196,1.29);
#23379=CIRCLE('',#105198,1.03775);
#23380=CIRCLE('',#105200,1.03775);
#23381=CIRCLE('',#105207,1.03775);
#23382=CIRCLE('',#105209,1.29);
#23383=CIRCLE('',#105217,1.29);
#23384=CIRCLE('',#105219,1.03775);
#23385=CIRCLE('',#105221,1.03775);
#23386=CIRCLE('',#105228,1.03775);
#23387=CIRCLE('',#105230,1.29);
#23388=CIRCLE('',#105238,1.29);
#23389=CIRCLE('',#105240,1.03775);
#23390=CIRCLE('',#105242,1.03775);
#23391=CIRCLE('',#105249,1.03775);
#23392=CIRCLE('',#105251,1.29);
#23393=CIRCLE('',#105259,1.29);
#23394=CIRCLE('',#105261,2.4);
#23395=CIRCLE('',#105262,2.1);
#23396=CIRCLE('',#105264,2.1);
#23397=CIRCLE('',#105265,2.1);
#23398=CIRCLE('',#105267,10.5);
#23399=CIRCLE('',#105270,10.5);
#23400=CIRCLE('',#105271,4.95184441433916);
#23401=CIRCLE('',#105274,9.8);
#23402=CIRCLE('',#105275,9.8);
#23403=CIRCLE('',#105277,3.5);
#23404=CIRCLE('',#105279,3.5);
#23405=CIRCLE('',#105281,10.5);
#23406=CIRCLE('',#105283,10.5);
#23407=CIRCLE('',#105285,4.95184441433916);
#23408=CIRCLE('',#105287,10.5);
#23409=CIRCLE('',#105288,10.5);
#23410=CIRCLE('',#105290,5.08286386254677);
#23411=CIRCLE('',#105291,5.08286386254677);
#23412=CIRCLE('',#105293,10.5);
#23413=CIRCLE('',#105294,10.5);
#23414=CIRCLE('',#105296,5.21388331075437);
#23415=CIRCLE('',#105297,5.21388331075437);
#23416=CIRCLE('',#105299,10.5);
#23417=CIRCLE('',#105300,10.5);
#23418=CIRCLE('',#105302,5.34490275896198);
#23419=CIRCLE('',#105303,5.34490275896198);
#23420=CIRCLE('',#105305,10.5);
#23421=CIRCLE('',#105306,10.5);
#23422=CIRCLE('',#105308,5.47592220716958);
#23423=CIRCLE('',#105309,5.47592220716958);
#23424=CIRCLE('',#105311,10.5);
#23425=CIRCLE('',#105312,10.5);
#23426=CIRCLE('',#105314,5.60694165537719);
#23427=CIRCLE('',#105315,5.60694165537719);
#23428=CIRCLE('',#105317,10.5);
#23429=CIRCLE('',#105318,10.5);
#23430=CIRCLE('',#105320,5.73796110358479);
#23431=CIRCLE('',#105321,5.73796110358479);
#23432=CIRCLE('',#105323,10.5);
#23433=CIRCLE('',#105324,10.5);
#23434=CIRCLE('',#105326,5.8689805517924);
#23435=CIRCLE('',#105327,5.8689805517924);
#23436=CIRCLE('',#105329,10.5);
#23437=CIRCLE('',#105330,10.5);
#23438=CIRCLE('',#105332,6.);
#23439=CIRCLE('',#105333,6.);
#23440=CIRCLE('',#105335,10.5);
#23441=CIRCLE('',#105336,10.5);
#23442=CIRCLE('',#105365,3.442);
#23443=CIRCLE('',#105376,2.872);
#23444=CIRCLE('',#105378,2.872);
#23445=CIRCLE('',#105388,2.942);
#23446=CIRCLE('',#105394,2.37175);
#23447=CIRCLE('',#105400,2.37175);
#23448=CIRCLE('',#105402,2.942);
#23449=CIRCLE('',#105403,1.4);
#23450=CIRCLE('',#105406,3.);
#23451=CIRCLE('',#105407,3.);
#23452=CIRCLE('',#105409,2.872);
#23453=CIRCLE('',#105411,3.);
#23454=CIRCLE('',#105412,3.);
#23455=CIRCLE('',#105413,2.5);
#23456=CIRCLE('',#105415,1.4);
#23457=CIRCLE('',#105417,3.442);
#23458=CIRCLE('',#105419,3.);
#23459=CIRCLE('',#105421,2.1);
#23460=CIRCLE('',#105422,2.1);
#23461=CIRCLE('',#105424,1.);
#23462=CIRCLE('',#105426,1.);
#23463=CIRCLE('',#105433,2.);
#23464=CIRCLE('',#105434,1.);
#23465=CIRCLE('',#105436,1.);
#23466=CIRCLE('',#105438,2.);
#23467=CIRCLE('',#105442,2.942);
#23468=CIRCLE('',#105449,2.37175);
#23469=CIRCLE('',#105456,2.5);
#23470=CIRCLE('',#105457,2.37175);
#23471=CIRCLE('',#105460,2.5);
#23472=CIRCLE('',#105461,2.5);
#23473=CIRCLE('',#105463,2.942);
#23474=CIRCLE('',#105464,1.5);
#23475=CIRCLE('',#105467,0.75);
#23476=CIRCLE('',#105468,1.);
#23477=CIRCLE('',#105469,1.);
#23478=CIRCLE('',#105471,0.75);
#23479=CIRCLE('',#105473,0.2);
#23480=CIRCLE('',#105475,2.49999999999999);
#23481=CIRCLE('',#105476,0.5);
#23482=CIRCLE('',#105478,2.5);
#23483=CIRCLE('',#105480,1.);
#23484=CIRCLE('',#105481,1.);
#23485=CIRCLE('',#105484,0.2);
#23486=CIRCLE('',#105496,3.);
#23487=CIRCLE('',#105497,3.);
#23488=CIRCLE('',#105499,1.5);
#23489=CIRCLE('',#105500,1.5);
#23490=CIRCLE('',#105502,1.5);
#23491=CIRCLE('',#105503,1.5);
#23492=CIRCLE('',#105505,0.750000000000001);
#23493=CIRCLE('',#105506,0.750000000000001);
#23494=CIRCLE('',#105508,1.5);
#23495=CIRCLE('',#105509,1.5);
#23496=CIRCLE('',#105511,3.);
#23497=CIRCLE('',#105512,3.);
#23498=B_SPLINE_CURVE_WITH_KNOTS('',3,(#130727,#130728,#130729,#130730,
#130731,#130732,#130733,#130734,#130735,#130736,#130737,#130738,#130739,
#130740,#130741,#130742,#130743,#130744,#130745,#130746,#130747,#130748,
#130749,#130750,#130751,#130752,#130753,#130754,#130755,#130756,#130757,
#130758,#130759,#130760,#130761,#130762,#130763,#130764,#130765,#130766,
#130767,#130768,#130769,#130770,#130771,#130772,#130773,#130774,#130775,
#130776,#130777,#130778,#130779,#130780,#130781,#130782,#130783,#130784,
#130785,#130786,#130787,#130788,#130789,#130790,#130791,#130792,#130793),
 .UNSPECIFIED.,.F.,.F.,(4,3,3,3,3,3,3,3,3,3,3,3,3,3,3,3,3,3,3,3,3,3,4),
(24.5160776815829,24.6338502836512,24.7515779097144,24.8693943986912,24.9872495119034,
25.105327266425,25.2137469589919,25.2137913118699,25.3221913605844,25.3350114624077,
25.4518815112335,25.5686444395478,25.6853513110055,25.8020530911996,25.9188834125999,
26.0357913091352,26.1452292168737,26.1529168472848,26.1835170015641,26.1835525161726,
26.3016558198144,26.3399124732618,26.4422968683701),.UNSPECIFIED.);
#23499=B_SPLINE_CURVE_WITH_KNOTS('',3,(#130795,#130796,#130797,#130798,
#130799,#130800,#130801,#130802,#130803,#130804,#130805,#130806,#130807,
#130808,#130809,#130810,#130811,#130812,#130813,#130814,#130815,#130816),
 .UNSPECIFIED.,.F.,.F.,(4,3,3,3,3,3,3,4),(-0.0902749387754822,-0.0742826152768497,
-0.0647281330592198,-0.0554146586505969,-0.0451640473161138,-0.033509184847726,
-0.00675287661166353,0.),.UNSPECIFIED.);
#23500=B_SPLINE_CURVE_WITH_KNOTS('',3,(#130819,#130820,#130821,#130822,
#130823,#130824,#130825,#130826,#130827,#130828,#130829,#130830,#130831,
#130832,#130833,#130834,#130835,#130836,#130837,#130838,#130839,#130840,
#130841,#130842,#130843,#130844,#130845,#130846,#130847,#130848,#130849,
#130850,#130851,#130852,#130853,#130854,#130855,#130856,#130857,#130858,
#130859,#130860,#130861,#130862,#130863,#130864,#130865,#130866,#130867,
#130868,#130869,#130870,#130871,#130872,#130873,#130874,#130875,#130876,
#130877,#130878,#130879,#130880,#130881,#130882,#130883,#130884,#130885,
#130886,#130887,#130888,#130889,#130890,#130891,#130892,#130893,#130894,
#130895,#130896,#130897,#130898,#130899,#130900,#130901,#130902),
 .UNSPECIFIED.,.F.,.F.,(4,2,2,2,2,2,2,2,2,2,2,2,2,2,2,2,2,2,2,2,2,2,2,2,
2,2,2,2,2,2,2,2,2,2,2,2,2,2,2,2,2,4),(-3.18439516658457,-3.15974881539495,
-3.14750129282652,-3.13703041818299,-3.12844802307121,-3.11639166588861,
-3.08592199300131,-3.07681556285727,-3.07174260228611,-3.06513991741923,
-3.03589139873531,-3.02003342723502,-3.01118711648019,-3.0019557243139,
-2.97314287852745,-2.96147727551602,-2.9533181918626,-2.94843288600149,
-2.94182402102507,-2.91271400453299,-2.89692673378685,-2.88814855910042,
-2.87904381531293,-2.8610699969371,-2.84219439832436,-2.83162052918509,
-2.82647232988103,-2.82058879757083,-2.79817695746129,-2.77549565690187,
-2.76631068751743,-2.75747581459958,-2.74152565839784,-2.72017905583269,
-2.71215881373051,-2.70573910057196,-2.70073398133747,-2.69173779062522,
-2.66793712484695,-2.65135784589242,-2.64248009746824,-2.63341280352093),
 .UNSPECIFIED.);
#23501=B_SPLINE_CURVE_WITH_KNOTS('',3,(#130908,#130909,#130910,#130911,
#130912,#130913,#130914,#130915,#130916,#130917,#130918,#130919,#130920,
#130921,#130922,#130923,#130924,#130925,#130926,#130927,#130928,#130929,
#130930,#130931,#130932,#130933,#130934,#130935,#130936,#130937,#130938,
#130939,#130940,#130941,#130942,#130943,#130944,#130945,#130946,#130947,
#130948,#130949,#130950,#130951,#130952,#130953,#130954,#130955,#130956,
#130957,#130958,#130959,#130960,#130961,#130962,#130963,#130964,#130965,
#130966,#130967,#130968,#130969,#130970,#130971,#130972,#130973,#130974,
#130975,#130976,#130977),.UNSPECIFIED.,.F.,.F.,(4,3,3,3,3,3,3,3,3,3,3,3,
3,3,3,3,3,3,3,3,3,3,3,4),(18.2318964876154,18.3499056532152,18.4254225164394,
18.4254628817511,18.534901772586,18.5466830322889,18.6645202599371,18.7822476497643,
18.89991442255,19.0237418384259,19.1415118943581,19.2593532998693,19.3681535102728,
19.3773894458933,19.3951836495535,19.3952240860538,19.5034482315185,19.5116532718969,
19.6279187937169,19.7440728916638,19.8602107593755,19.9763360740262,20.0925768794781,
20.1591190620682),.UNSPECIFIED.);
#23502=B_SPLINE_CURVE_WITH_KNOTS('',3,(#130978,#130979,#130980,#130981,
#130982,#130983,#130984,#130985,#130986,#130987,#130988,#130989,#130990,
#130991,#130992,#130993,#130994,#130995,#130996,#130997,#130998,#130999,
#131000,#131001,#131002,#131003,#131004,#131005,#131006,#131007,#131008,
#131009,#131010,#131011,#131012,#131013,#131014,#131015,#131016,#131017,
#131018,#131019,#131020,#131021,#131022,#131023,#131024,#131025,#131026,
#131027,#131028,#131029,#131030,#131031,#131032,#131033,#131034,#131035,
#131036,#131037,#131038,#131039,#131040,#131041,#131042,#131043,#131044,
#131045,#131046,#131047,#131048,#131049,#131050,#131051,#131052,#131053,
#131054,#131055,#131056,#131057,#131058,#131059,#131060,#131061,#131062,
#131063,#131064,#131065,#131066,#131067,#131068,#131069,#131070,#131071,
#131072,#131073,#131074,#131075,#131076,#131077,#131078,#131079,#131080,
#131081,#131082,#131083,#131084,#131085,#131086,#131087,#131088,#131089,
#131090,#131091,#131092,#131093,#131094,#131095,#131096,#131097,#131098,
#131099,#131100,#131101,#131102,#131103,#131104,#131105,#131106,#131107,
#131108,#131109,#131110,#131111,#131112,#131113,#131114,#131115,#131116,
#131117,#131118,#131119,#131120,#131121,#131122,#131123,#131124,#131125,
#131126,#131127,#131128,#131129,#131130,#131131,#131132,#131133,#131134,
#131135,#131136,#131137,#131138,#131139,#131140,#131141,#131142,#131143,
#131144,#131145,#131146),.UNSPECIFIED.,.F.,.F.,(4,3,3,3,3,3,3,3,3,3,3,3,
3,3,3,3,3,3,3,3,3,3,3,3,3,3,3,3,3,3,3,3,3,3,3,3,3,3,3,3,3,3,3,3,3,3,3,3,
3,3,3,3,3,3,3,3,4),(20.1591190625159,20.2764390861516,20.3187722441127,
20.3649448921207,20.3649852903565,20.4744178307227,20.4862054408943,20.6040549110511,
20.7217943849732,20.8394730597834,20.9632914185023,21.081072765058,21.198925234886,
21.3077530804529,21.3169720402184,21.3347063043336,21.3347464946591,21.4442281539202,
21.4559666451969,21.5738204779957,21.6915646661758,21.8092483924545,21.9330632190813,
22.0508503771043,22.1687089093655,22.2774753621084,22.2867620791089,22.3044668695445,
22.3045076989618,22.4138254986466,22.4257278494996,22.5434478115752,22.6610580097667,
22.7786079083108,22.8961468703754,23.0137997695757,23.1315225935855,23.2408830638024,
23.2494441255917,23.2742286828635,23.2742689032645,23.3837602833423,23.3954890538023,
23.5135003420354,23.6314006664449,23.7492388874001,23.8729366924419,23.9908721599826,
24.10887664777,24.2178717905383,24.227071312369,24.243991123088,24.2440301075672,
24.3536754995663,24.3621270739351,24.480036883431,24.5160776809557),
 .UNSPECIFIED.);
#23503=B_SPLINE_CURVE_WITH_KNOTS('',3,(#131147,#131148,#131149,#131150,
#131151,#131152,#131153,#131154,#131155,#131156,#131157,#131158,#131159,
#131160,#131161,#131162,#131163,#131164,#131165,#131166,#131167,#131168,
#131169,#131170,#131171,#131172,#131173,#131174,#131175,#131176,#131177,
#131178,#131179,#131180,#131181,#131182,#131183,#131184,#131185,#131186,
#131187,#131188,#131189,#131190,#131191,#131192,#131193,#131194,#131195,
#131196,#131197,#131198,#131199,#131200,#131201,#131202,#131203,#131204,
#131205,#131206,#131207,#131208,#131209,#131210,#131211,#131212,#131213,
#131214,#131215,#131216,#131217,#131218,#131219,#131220,#131221,#131222,
#131223,#131224,#131225,#131226,#131227,#131228,#131229,#131230,#131231,
#131232,#131233,#131234,#131235,#131236,#131237,#131238,#131239,#131240,
#131241,#131242,#131243,#131244,#131245,#131246,#131247,#131248,#131249,
#131250,#131251,#131252,#131253,#131254,#131255,#131256,#131257,#131258,
#131259,#131260,#131261,#131262,#131263,#131264,#131265,#131266,#131267,
#131268,#131269,#131270,#131271,#131272,#131273,#131274,#131275,#131276,
#131277,#131278),.UNSPECIFIED.,.F.,.F.,(4,2,2,2,2,2,2,2,2,2,2,2,2,2,2,2,
2,2,2,2,2,2,2,2,2,2,2,2,2,2,2,2,2,2,2,2,2,2,2,2,2,2,2,2,2,2,2,2,2,2,2,2,
2,2,2,2,2,2,2,2,2,2,2,2,2,4),(-2.63341280352093,-2.63338908590916,-2.61475077252263,
-2.59625974636104,-2.58578420982809,-2.58063284435739,-2.57470277043636,
-2.5603653957494,-2.54033455876387,-2.53026043017817,-2.52097003372362,
-2.51223669831331,-2.49728887792193,-2.47471711241325,-2.46325775592071,
-2.45800484991181,-2.45225752364046,-2.43791426300124,-2.41757964125372,
-2.40744820567261,-2.39812483100095,-2.38939762360827,-2.37457182362478,
-2.35186459507239,-2.34365529463354,-2.33713766240529,-2.33216521116693,
-2.32346121809268,-2.2995507987335,-2.2875813199158,-2.27729863580044,-2.26882022586542,
-2.25694334169315,-2.23001808279554,-2.2212988600583,-2.21451702781106,
-2.20958429245329,-2.20138147088039,-2.17574348926931,-2.16413634608837,
-2.1540388650897,-2.14553861920783,-2.13331947430134,-2.10696134396377,
-2.09830456306287,-2.09155462124085,-2.0866177365907,-2.07835966124171,
-2.05425218617961,-2.03700607791523,-2.02807903382094,-2.01905076582828,
-1.98720884630738,-1.97243327564618,-1.96690070443741,-1.96147826300303,
-1.95047478829063,-1.92724571493476,-1.91274763706247,-1.90405001510231,
-1.89466835474604,-1.86490369174868,-1.85426067665749,-1.84655505358699,
-1.84164637788602,-1.83698289437714),.UNSPECIFIED.);
#23504=B_SPLINE_CURVE_WITH_KNOTS('',3,(#131284,#131285,#131286,#131287,
#131288,#131289,#131290,#131291,#131292,#131293,#131294,#131295,#131296,
#131297,#131298,#131299,#131300,#131301,#131302,#131303,#131304,#131305,
#131306,#131307,#131308,#131309,#131310,#131311,#131312,#131313,#131314,
#131315,#131316,#131317,#131318,#131319,#131320,#131321,#131322,#131323,
#131324,#131325,#131326,#131327,#131328,#131329,#131330,#131331,#131332,
#131333,#131334,#131335,#131336,#131337,#131338,#131339,#131340,#131341,
#131342,#131343,#131344,#131345,#131346,#131347,#131348,#131349,#131350,
#131351,#131352,#131353,#131354,#131355,#131356),.UNSPECIFIED.,.F.,.F.,
(4,3,3,3,3,3,3,3,3,3,3,3,3,3,3,3,3,3,3,3,3,3,3,3,4),(11.949635603067,12.0673156376958,
12.1849657013768,12.3027149435704,12.4205166426525,12.5385271257885,12.6068552638494,
12.6068956559349,12.7163278647347,12.7281158064727,12.8459491616131,12.9636726575015,
13.081335523404,13.2051658576124,13.3229320283064,13.4407695618705,13.549573048494,
13.5588018855446,13.5766164679027,13.5766568602376,13.6924275886706,13.7171311440579,
13.8384365525919,13.8560591163181,13.8759337548445),.UNSPECIFIED.);
#23505=B_SPLINE_CURVE_WITH_KNOTS('',3,(#131357,#131358,#131359,#131360,
#131361,#131362,#131363,#131364,#131365,#131366,#131367,#131368,#131369,
#131370,#131371,#131372,#131373,#131374,#131375,#131376,#131377,#131378,
#131379,#131380,#131381,#131382,#131383,#131384,#131385,#131386,#131387,
#131388,#131389,#131390,#131391,#131392,#131393,#131394,#131395,#131396,
#131397,#131398,#131399,#131400,#131401,#131402,#131403,#131404,#131405,
#131406,#131407,#131408,#131409,#131410,#131411,#131412,#131413,#131414,
#131415,#131416,#131417,#131418,#131419,#131420,#131421,#131422,#131423,
#131424,#131425,#131426,#131427,#131428,#131429,#131430,#131431,#131432,
#131433,#131434,#131435,#131436,#131437,#131438,#131439,#131440,#131441,
#131442,#131443,#131444,#131445,#131446,#131447,#131448,#131449,#131450,
#131451,#131452,#131453,#131454,#131455,#131456,#131457,#131458,#131459,
#131460,#131461,#131462,#131463,#131464,#131465,#131466,#131467,#131468,
#131469,#131470,#131471,#131472,#131473,#131474,#131475,#131476,#131477,
#131478,#131479,#131480,#131481,#131482,#131483,#131484,#131485,#131486,
#131487,#131488,#131489,#131490,#131491,#131492,#131493,#131494,#131495,
#131496,#131497,#131498,#131499,#131500,#131501,#131502,#131503,#131504,
#131505,#131506,#131507,#131508,#131509,#131510),.UNSPECIFIED.,.F.,.F.,
(4,3,3,3,3,3,3,3,3,3,3,3,3,3,3,3,3,3,3,3,3,3,3,3,3,3,3,3,3,3,3,3,3,3,3,
3,3,3,3,3,3,3,3,3,3,3,3,3,3,3,3,4),(13.8759337553363,13.9931001932589,14.1102297434989,
14.227456018938,14.344730230585,14.4622230561964,14.5463776723912,14.5464180645403,
14.6558502206054,14.6676382150781,14.7854717016337,14.9031953297728,15.0208583284965,
15.1446885635831,15.2624548668063,15.3802925326214,15.4890963578799,15.4983249871425,
15.5161388802809,15.516179268843,15.6256123754232,15.6373994193808,15.7552334260967,
15.8729575772568,15.9906211007147,16.1144509438225,16.2322177687725,16.3500559544883,
16.4588592317635,16.4680889221782,16.4859000772313,16.4859404731457,16.5953716279568,
16.6071606236835,16.7249924873266,16.8427144992418,16.9603758917638,17.0842073381849,
17.2019720818873,17.3198082065096,17.4286109026081,17.4378391578116,17.4556612819127,
17.4557016774484,17.5649968567153,17.5737108697352,17.6915524576925,17.8092758653084,
17.9269654710807,18.0446320306057,18.1623925787244,18.2318964870053),
 .UNSPECIFIED.);
#23506=B_SPLINE_CURVE_WITH_KNOTS('',3,(#131511,#131512,#131513,#131514,
#131515,#131516,#131517,#131518,#131519,#131520,#131521,#131522,#131523,
#131524,#131525,#131526,#131527,#131528,#131529,#131530,#131531,#131532,
#131533,#131534,#131535,#131536,#131537,#131538,#131539,#131540,#131541,
#131542,#131543,#131544,#131545,#131546,#131547,#131548,#131549,#131550,
#131551,#131552,#131553,#131554,#131555,#131556,#131557,#131558,#131559,
#131560,#131561,#131562,#131563,#131564,#131565,#131566,#131567,#131568,
#131569,#131570,#131571,#131572,#131573,#131574,#131575,#131576,#131577,
#131578,#131579,#131580,#131581,#131582,#131583,#131584,#131585,#131586,
#131587,#131588,#131589,#131590,#131591,#131592,#131593,#131594,#131595,
#131596,#131597,#131598,#131599,#131600,#131601,#131602,#131603,#131604,
#131605,#131606,#131607,#131608,#131609,#131610,#131611,#131612,#131613,
#131614,#131615,#131616,#131617,#131618,#131619,#131620,#131621,#131622,
#131623,#131624,#131625,#131626,#131627,#131628,#131629,#131630,#131631,
#131632,#131633,#131634,#131635,#131636),.UNSPECIFIED.,.F.,.F.,(4,2,2,2,
2,2,2,2,2,2,2,2,2,2,2,2,2,2,2,2,2,2,2,2,2,2,2,2,2,2,2,2,2,2,2,2,2,2,2,2,
2,2,2,2,2,2,2,2,2,2,2,2,2,2,2,2,2,2,2,2,2,2,4),(-1.83698289437714,-1.83450952322168,
-1.80608476101656,-1.79042517070769,-1.78162444808961,-1.77243081013779,
-1.7503408384697,-1.73456941244788,-1.7249015434468,-1.71983535496605,-1.71368757517374,
-1.6837109178935,-1.67220860664121,-1.66216542597266,-1.65365749763611,
-1.64132646297389,-1.61515183154271,-1.60298920152642,-1.59766578617113,
-1.59201641470727,-1.57475374211352,-1.5466611850744,-1.53741065722368,
-1.52864837761914,-1.51340581989546,-1.48699773037434,-1.47841600401358,
-1.47345504174387,-1.46688302543023,-1.45856799126273,-1.435069853613,-1.42085695998277,
-1.4122731987527,-1.40286934027383,-1.39258460820883,-1.37134319401564,
-1.35810032092574,-1.35246748979556,-1.34713280090652,-1.33484535845507,
-1.30796723459815,-1.29605786773587,-1.28757933475715,-1.27732000283747,
-1.26539595606936,-1.24153571280251,-1.23276161007615,-1.22778473505187,
-1.22130699705758,-1.21317068503583,-1.19100494486867,-1.17570953094654,
-1.16694325088905,-1.15770293996463,-1.13397037665446,-1.11328131781741,
-1.10727342224715,-1.10215365759373,-1.09197859212924,-1.0745490245242,
-1.05465390886544,-1.04551395773332,-1.04064761107749),.UNSPECIFIED.);
#23507=B_SPLINE_CURVE_WITH_KNOTS('',3,(#131642,#131643,#131644,#131645,
#131646,#131647,#131648,#131649,#131650,#131651,#131652,#131653,#131654,
#131655,#131656,#131657,#131658,#131659,#131660,#131661,#131662,#131663,
#131664,#131665,#131666,#131667,#131668,#131669,#131670,#131671,#131672,
#131673,#131674,#131675,#131676,#131677,#131678,#131679,#131680,#131681,
#131682,#131683),.UNSPECIFIED.,.F.,.F.,(4,2,2,2,2,2,2,2,2,2,2,2,2,2,2,2,
2,2,2,2,4),(-0.244126851835458,-0.242266589745228,-0.232767411029632,-0.20227844630268,
-0.189805359946467,-0.181570707052886,-0.172343713890524,-0.162123567604387,
-0.140240762435818,-0.128266635619279,-0.12281204083496,-0.117496476174122,
-0.105970253642188,-0.0842702830154775,-0.066515665373926,-0.0566811651008963,
-0.0466317253481053,-0.025601938924746,-0.00728212488525174,-0.00327759413548372,
-9.99999999390377E-7),.UNSPECIFIED.);
#23508=B_SPLINE_CURVE_WITH_KNOTS('',3,(#131686,#131687,#131688,#131689,
#131690,#131691,#131692,#131693,#131694,#131695,#131696,#131697,#131698,
#131699,#131700,#131701,#131702,#131703,#131704,#131705,#131706,#131707,
#131708,#131709,#131710,#131711,#131712,#131713,#131714,#131715,#131716,
#131717,#131718,#131719,#131720,#131721,#131722,#131723,#131724,#131725,
#131726,#131727,#131728,#131729,#131730,#131731,#131732,#131733,#131734,
#131735,#131736,#131737,#131738,#131739,#131740,#131741,#131742,#131743,
#131744,#131745,#131746,#131747,#131748,#131749,#131750,#131751,#131752,
#131753,#131754,#131755,#131756,#131757,#131758,#131759,#131760,#131761,
#131762,#131763,#131764,#131765,#131766,#131767,#131768,#131769,#131770,
#131771,#131772,#131773,#131774,#131775,#131776,#131777,#131778,#131779,
#131780,#131781,#131782,#131783,#131784,#131785,#131786,#131787,#131788,
#131789,#131790,#131791,#131792,#131793,#131794,#131795,#131796,#131797,
#131798,#131799,#131800,#131801,#131802,#131803,#131804,#131805,#131806,
#131807,#131808,#131809),.UNSPECIFIED.,.F.,.F.,(4,3,3,3,3,3,3,3,3,3,3,3,
3,3,3,3,3,3,3,3,3,3,3,3,3,3,3,3,3,3,3,3,3,3,3,3,3,3,3,3,3,4),(2.02979676262917,
2.13731224702246,2.25387842932559,2.37034643280507,2.48676778078347,2.60327116203147,
2.71981651592146,2.83656470629628,2.90924454559889,2.90928361290806,3.01897299074406,
3.0305037634459,3.14850451785552,3.26639853642502,3.3842346685647,3.50793720572621,
3.62588111593657,3.74389766548153,3.85268061258365,3.86210939485147,3.87900455825299,
3.87904481721075,3.98841323710296,4.00026496774859,4.11798860660234,4.23560100936115,
4.35315164410215,4.47068987590689,4.58833990365881,4.70605859647816,4.8153662846805,
4.82397422696118,4.84876523421727,4.84880602151344,4.95807676401619,4.96683180286505,
5.08469155674416,5.20243465709765,5.32015563758868,5.43785412192805,5.55567628577564,
5.66554986544235),.UNSPECIFIED.);
#23509=B_SPLINE_CURVE_WITH_KNOTS('',3,(#131815,#131816,#131817,#131818,
#131819,#131820,#131821,#131822,#131823,#131824,#131825,#131826,#131827,
#131828,#131829,#131830,#131831,#131832,#131833,#131834,#131835,#131836,
#131837,#131838,#131839,#131840,#131841,#131842,#131843,#131844,#131845,
#131846,#131847,#131848,#131849,#131850,#131851,#131852,#131853,#131854,
#131855,#131856,#131857,#131858,#131859,#131860,#131861,#131862,#131863,
#131864,#131865,#131866,#131867,#131868,#131869,#131870,#131871,#131872,
#131873,#131874,#131875,#131876,#131877,#131878,#131879,#131880,#131881),
 .UNSPECIFIED.,.F.,.F.,(4,3,3,3,3,3,3,3,3,3,3,3,3,3,3,3,3,3,3,3,3,3,4),
(24.5160781364108,24.6338513924193,24.7515796689379,24.8693967972321,24.9872525443042,
25.1053309156037,25.2137469623114,25.2137913118699,25.3221904411987,25.3350114624077,
25.4518800492476,25.5686415181165,25.68534693484,25.8020472671814,25.9188761600837,
26.0357826375004,26.1452199094595,26.1529067833318,26.1835169867254,26.1835525161726,
26.3016565030475,26.3399218786873,26.4422968782847),.UNSPECIFIED.);
#23510=B_SPLINE_CURVE_WITH_KNOTS('',3,(#131883,#131884,#131885,#131886,
#131887,#131888,#131889,#131890,#131891,#131892,#131893,#131894,#131895,
#131896,#131897,#131898,#131899,#131900,#131901,#131902,#131903,#131904),
 .UNSPECIFIED.,.F.,.F.,(4,3,3,3,3,3,3,4),(-0.0902748495005752,-0.074282404340397,
-0.0647286421966786,-0.0554142010493536,-0.045164026211744,-0.0335103866407499,
-0.00675201620121094,0.),.UNSPECIFIED.);
#23511=B_SPLINE_CURVE_WITH_KNOTS('',3,(#131907,#131908,#131909,#131910,
#131911,#131912,#131913,#131914,#131915,#131916,#131917,#131918,#131919,
#131920,#131921,#131922,#131923,#131924,#131925,#131926,#131927,#131928,
#131929,#131930,#131931,#131932,#131933,#131934,#131935,#131936,#131937,
#131938,#131939,#131940,#131941,#131942,#131943,#131944,#131945,#131946,
#131947,#131948,#131949,#131950,#131951,#131952,#131953,#131954,#131955,
#131956,#131957,#131958,#131959,#131960,#131961,#131962,#131963,#131964,
#131965,#131966,#131967,#131968,#131969,#131970,#131971,#131972,#131973,
#131974,#131975,#131976,#131977,#131978,#131979,#131980,#131981,#131982,
#131983,#131984,#131985,#131986,#131987,#131988,#131989,#131990,#131991,
#131992),.UNSPECIFIED.,.F.,.F.,(4,2,2,2,2,2,2,2,2,2,2,2,2,2,2,2,2,2,2,2,
2,2,2,2,2,2,2,2,2,2,2,2,2,2,2,2,2,2,2,2,2,2,4),(-3.18475804076959,-3.15980016638694,
-3.14273948012479,-3.13374539783552,-3.12454062706717,-3.10423748937383,
-3.08760027365706,-3.07766771004778,-3.07251605124589,-3.06621772700951,
-3.03649018045794,-3.02050583915172,-3.01165074901096,-3.00243773194935,
-2.98151171764926,-2.9592535975697,-2.95250011400159,-2.94757330454844,
-2.93935856742012,-2.91247851666974,-2.89715062959167,-2.88841337344926,
-2.87924916601703,-2.85742178608931,-2.83610768400626,-2.82941275923196,
-2.82448685551502,-2.81623443939348,-2.7921150364245,-2.77989286674714,
-2.76947546235326,-2.76098995901444,-2.74925789120506,-2.7221445396627,
-2.71340473293917,-2.70661000614579,-2.70166558365389,-2.69341637264005,
-2.66929546992004,-2.65205014777285,-2.6431216788472,-2.63409010065303,
-2.63384867082664),.UNSPECIFIED.);
#23512=B_SPLINE_CURVE_WITH_KNOTS('',3,(#131998,#131999,#132000,#132001,
#132002,#132003,#132004,#132005,#132006,#132007,#132008,#132009,#132010,
#132011,#132012,#132013,#132014,#132015,#132016,#132017,#132018,#132019,
#132020,#132021,#132022,#132023,#132024,#132025,#132026,#132027,#132028,
#132029,#132030,#132031,#132032,#132033,#132034,#132035,#132036,#132037,
#132038,#132039,#132040,#132041,#132042,#132043,#132044,#132045,#132046,
#132047,#132048,#132049,#132050,#132051,#132052,#132053,#132054,#132055,
#132056,#132057,#132058,#132059,#132060,#132061,#132062,#132063,#132064,
#132065,#132066,#132067),.UNSPECIFIED.,.F.,.F.,(4,3,3,3,3,3,3,3,3,3,3,3,
3,3,3,3,3,3,3,3,3,3,3,4),(18.2318968787514,18.3499060448615,18.4254225216423,
18.4254628817511,18.5349017943127,18.5466830322889,18.6645202762246,18.7822476823724,
18.8999144714775,19.0237418751216,19.1415119471466,19.2593533686491,19.3681535768292,
19.3773895303943,19.3951836545557,19.3952240860538,19.5034482068642,19.5116532354367,
19.6279187208041,19.7440727823547,19.8602106139534,19.9763358926106,20.0925766625481,
20.1591190620686),.UNSPECIFIED.);
#23513=B_SPLINE_CURVE_WITH_KNOTS('',3,(#132068,#132069,#132070,#132071,
#132072,#132073,#132074,#132075,#132076,#132077,#132078,#132079,#132080,
#132081,#132082,#132083,#132084,#132085,#132086,#132087,#132088,#132089,
#132090,#132091,#132092,#132093,#132094,#132095,#132096,#132097,#132098,
#132099,#132100,#132101,#132102,#132103,#132104,#132105,#132106,#132107,
#132108,#132109,#132110,#132111,#132112,#132113,#132114,#132115,#132116,
#132117,#132118,#132119,#132120,#132121,#132122,#132123,#132124,#132125,
#132126,#132127,#132128,#132129,#132130,#132131,#132132,#132133,#132134,
#132135,#132136,#132137,#132138,#132139,#132140,#132141,#132142,#132143,
#132144,#132145,#132146,#132147,#132148,#132149,#132150,#132151,#132152,
#132153,#132154,#132155,#132156,#132157,#132158,#132159,#132160,#132161,
#132162,#132163,#132164,#132165,#132166,#132167,#132168,#132169,#132170,
#132171,#132172,#132173,#132174,#132175,#132176,#132177,#132178,#132179,
#132180,#132181,#132182,#132183,#132184,#132185,#132186,#132187,#132188,
#132189,#132190,#132191,#132192,#132193,#132194,#132195,#132196,#132197,
#132198,#132199,#132200,#132201,#132202,#132203,#132204,#132205,#132206,
#132207,#132208,#132209,#132210,#132211,#132212,#132213,#132214,#132215,
#132216,#132217,#132218,#132219,#132220,#132221,#132222,#132223,#132224,
#132225,#132226,#132227,#132228,#132229,#132230,#132231,#132232,#132233,
#132234,#132235,#132236),.UNSPECIFIED.,.F.,.F.,(4,3,3,3,3,3,3,3,3,3,3,3,
3,3,3,3,3,3,3,3,3,3,3,3,3,3,3,3,3,3,3,3,3,3,3,3,3,3,3,3,3,3,3,3,3,3,3,3,
3,3,3,3,3,3,3,3,4),(20.1591190625159,20.2764390510706,20.3187721935057,
20.3649448970694,20.3649852903564,20.474417801013,20.4862054408942,20.6040549230358,
20.7217944086693,20.8394730948977,20.963291444838,21.0810728019401,21.1989252820012,
21.3077531878469,21.3169720970495,21.3347063100803,21.3347464946591,21.4442282833429,
21.4559666451969,21.5738205697139,21.6915648498455,21.8092486681115,21.9330634258241,
22.0508506746636,22.1687092972027,22.2774757196079,22.286762555749,22.3044668739246,
22.3045076989618,22.4138253643461,22.4257278494996,22.5434476083366,22.6610576036881,
22.7786073001942,22.8961460614269,23.0137987630076,23.1315213911073,23.2408817617996,
23.2494427315033,23.2742286871683,23.2742689032645,23.3837601059622,23.3954890538023,
23.5135004049658,23.6314007909792,23.7492390721056,23.872936830971,23.9908723543834,
24.1088768964893,24.2178723756311,24.227071612826,24.243991132142,24.2440301075672,
24.3536763359503,24.36212772944,24.4800381950529,24.5160781357833),
 .UNSPECIFIED.);
#23514=B_SPLINE_CURVE_WITH_KNOTS('',3,(#132237,#132238,#132239,#132240,
#132241,#132242,#132243,#132244,#132245,#132246,#132247,#132248,#132249,
#132250,#132251,#132252,#132253,#132254,#132255,#132256,#132257,#132258,
#132259,#132260,#132261,#132262,#132263,#132264,#132265,#132266,#132267,
#132268,#132269,#132270,#132271,#132272,#132273,#132274,#132275,#132276,
#132277,#132278,#132279,#132280,#132281,#132282,#132283,#132284,#132285,
#132286,#132287,#132288,#132289,#132290,#132291,#132292,#132293,#132294,
#132295,#132296,#132297,#132298,#132299,#132300,#132301,#132302,#132303,
#132304,#132305,#132306,#132307,#132308,#132309,#132310,#132311,#132312,
#132313,#132314,#132315,#132316,#132317,#132318,#132319,#132320,#132321,
#132322,#132323,#132324,#132325,#132326,#132327,#132328,#132329,#132330,
#132331,#132332,#132333,#132334,#132335,#132336,#132337,#132338,#132339,
#132340,#132341,#132342,#132343,#132344,#132345,#132346,#132347,#132348,
#132349,#132350,#132351,#132352,#132353,#132354,#132355,#132356,#132357,
#132358,#132359,#132360,#132361,#132362,#132363,#132364),.UNSPECIFIED.,
 .F.,.F.,(4,2,2,2,2,2,2,2,2,2,2,2,2,2,2,2,2,2,2,2,2,2,2,2,2,2,2,2,2,2,2,
2,2,2,2,2,2,2,2,2,2,2,2,2,2,2,2,2,2,2,2,2,2,2,2,2,2,2,2,2,2,2,2,4),(-2.63384867082664,
-2.60067956115208,-2.59119414892037,-2.58402991229563,-2.57912411549598,
-2.57146069037577,-2.5473132317638,-2.53466143758753,-2.52403834163957,
-2.5155862270938,-2.50422460492688,-2.4778500674872,-2.46829890759395,-2.4611038002552,
-2.45619820385995,-2.44856786564464,-2.42444097166765,-2.41174747505461,
-2.40110117074743,-2.39264221378778,-2.38128293886777,-2.35344473355548,
-2.34099561201416,-2.33564330964062,-2.33002410084309,-2.31728322222918,
-2.29564491923898,-2.28528930652753,-2.27584719821023,-2.26727488092526,
-2.25321574587793,-2.22951661748433,-2.22117593417236,-2.21458911856265,
-2.20962903418765,-2.20107179807238,-2.17709296678601,-2.16011550663879,
-2.1512076056052,-2.14215607868278,-2.12531024847009,-2.1054024507707,-2.09455795636171,
-2.08936637732718,-2.08350642644974,-2.05509108134002,-2.04263269994247,
-2.03210378346703,-2.02364244755537,-2.01213803513009,-1.98581119979471,
-1.97640028808093,-1.9692728629665,-1.96436386244352,-1.95664639724681,
-1.93246646956722,-1.91455841226969,-1.905585369101,-1.89660593350099,-1.86360397177841,
-1.85380258767236,-1.84648679371643,-1.84158243035126,-1.83725267846888),
 .UNSPECIFIED.);
#23515=B_SPLINE_CURVE_WITH_KNOTS('',3,(#132370,#132371,#132372,#132373,
#132374,#132375,#132376,#132377,#132378,#132379,#132380,#132381,#132382,
#132383,#132384,#132385,#132386,#132387,#132388,#132389,#132390,#132391,
#132392,#132393,#132394,#132395,#132396,#132397,#132398,#132399,#132400,
#132401,#132402,#132403,#132404,#132405,#132406,#132407,#132408,#132409,
#132410,#132411,#132412,#132413,#132414,#132415,#132416,#132417,#132418,
#132419,#132420,#132421,#132422,#132423,#132424,#132425,#132426,#132427,
#132428,#132429,#132430,#132431,#132432,#132433,#132434,#132435,#132436,
#132437,#132438,#132439,#132440,#132441,#132442),.UNSPECIFIED.,.F.,.F.,
(4,3,3,3,3,3,3,3,3,3,3,3,3,3,3,3,3,3,3,3,3,3,3,3,4),(11.9496359932348,12.0673160274323,
12.1849660908497,12.3027153329077,12.4205170320056,12.5385275150523,12.6068552689481,
12.6068956559349,12.716327864626,12.7281158064727,12.8459491614091,12.9636726570828,
13.0813355227604,13.2051658571297,13.322932027576,13.4407695608851,13.5495730494168,
13.5588018842955,13.5766164730029,13.5766568602376,13.6924275909584,13.7171311431147,
13.8384365563071,13.8560591145712,13.8759337548442),.UNSPECIFIED.);
#23516=B_SPLINE_CURVE_WITH_KNOTS('',3,(#132443,#132444,#132445,#132446,
#132447,#132448,#132449,#132450,#132451,#132452,#132453,#132454,#132455,
#132456,#132457,#132458,#132459,#132460,#132461,#132462,#132463,#132464,
#132465,#132466,#132467,#132468,#132469,#132470,#132471,#132472,#132473,
#132474,#132475,#132476,#132477,#132478,#132479,#132480,#132481,#132482,
#132483,#132484,#132485,#132486,#132487,#132488,#132489,#132490,#132491,
#132492,#132493,#132494,#132495,#132496,#132497,#132498,#132499,#132500,
#132501,#132502,#132503,#132504,#132505,#132506,#132507,#132508,#132509,
#132510,#132511,#132512,#132513,#132514,#132515,#132516,#132517,#132518,
#132519,#132520,#132521,#132522,#132523,#132524,#132525,#132526,#132527,
#132528,#132529,#132530,#132531,#132532,#132533,#132534,#132535,#132536,
#132537,#132538,#132539,#132540,#132541,#132542,#132543,#132544,#132545,
#132546,#132547,#132548,#132549,#132550,#132551,#132552,#132553,#132554,
#132555,#132556,#132557,#132558,#132559,#132560,#132561,#132562,#132563,
#132564,#132565,#132566,#132567,#132568,#132569,#132570,#132571,#132572,
#132573,#132574,#132575,#132576,#132577,#132578,#132579,#132580,#132581,
#132582,#132583,#132584,#132585,#132586,#132587,#132588,#132589,#132590,
#132591,#132592,#132593,#132594,#132595,#132596),.UNSPECIFIED.,.F.,.F.,
(4,3,3,3,3,3,3,3,3,3,3,3,3,3,3,3,3,3,3,3,3,3,3,3,3,3,3,3,3,3,3,3,3,3,3,
3,3,3,3,3,3,3,3,3,3,3,3,3,3,3,3,4),(13.8759337553363,13.9931001931372,14.1102297432661,
14.227456018611,14.3447302301731,14.4622230557154,14.5463776774895,14.5464180645403,
14.6558502199931,14.6676382150781,14.7854717014034,14.9031953293054,15.0208583277855,
15.1446885630499,15.2624548660176,15.3802925315736,15.4890963596955,15.4983249858325,
15.5161388853966,15.516179268843,15.6256123789708,15.6373994193808,15.7552334287766,
15.8729575826182,15.9906211087535,16.1144509498516,16.2322177774323,16.350055965759,
16.4588592445964,16.468088936011,16.4859000823221,16.4859404731457,16.5953716256398,
16.6071606236835,16.72499248228,16.8427144891674,16.9603758766909,17.0842073268803,
17.201972065724,17.3198081855426,17.4286108793835,17.4378391321563,17.4556612869848,
17.4557016774484,17.5649968511712,17.5737108704674,17.691552459125,17.809275867409,
17.9269654738832,18.0446320340746,18.1623925830577,18.2318968781416),
 .UNSPECIFIED.);
#23517=B_SPLINE_CURVE_WITH_KNOTS('',3,(#132597,#132598,#132599,#132600,
#132601,#132602,#132603,#132604,#132605,#132606,#132607,#132608,#132609,
#132610,#132611,#132612,#132613,#132614,#132615,#132616,#132617,#132618,
#132619,#132620,#132621,#132622,#132623,#132624,#132625,#132626,#132627,
#132628,#132629,#132630,#132631,#132632,#132633,#132634,#132635,#132636,
#132637,#132638,#132639,#132640,#132641,#132642,#132643,#132644,#132645,
#132646,#132647,#132648,#132649,#132650,#132651,#132652,#132653,#132654,
#132655,#132656,#132657,#132658,#132659,#132660,#132661,#132662,#132663,
#132664,#132665,#132666,#132667,#132668,#132669,#132670,#132671,#132672,
#132673,#132674,#132675,#132676,#132677,#132678,#132679,#132680,#132681,
#132682,#132683,#132684,#132685,#132686,#132687,#132688,#132689,#132690,
#132691,#132692,#132693,#132694,#132695,#132696,#132697,#132698,#132699,
#132700,#132701,#132702,#132703,#132704,#132705,#132706,#132707,#132708,
#132709,#132710,#132711,#132712,#132713,#132714,#132715,#132716,#132717,
#132718,#132719,#132720,#132721,#132722),.UNSPECIFIED.,.F.,.F.,(4,2,2,2,
2,2,2,2,2,2,2,2,2,2,2,2,2,2,2,2,2,2,2,2,2,2,2,2,2,2,2,2,2,2,2,2,2,2,2,2,
2,2,2,2,2,2,2,2,2,2,2,2,2,2,2,2,2,2,2,2,2,2,4),(-1.83725267846888,-1.83540027261704,
-1.80649375697848,-1.7907382655999,-1.78192911062747,-1.77274762825419,
-1.75171025246169,-1.72954720864117,-1.72288070231471,-1.71793252782111,
-1.70952556097505,-1.68548227945112,-1.67335330776921,-1.66298902805841,
-1.65451607444484,-1.64276697738429,-1.61561732441011,-1.60328339766176,
-1.5979428133892,-1.59231277798626,-1.57562459927013,-1.54653158396036,
-1.53736727038257,-1.52854686968659,-1.51265221693632,-1.4832057820726,
-1.47673981772376,-1.47175743220665,-1.46294422715869,-1.44962073482292,
-1.42498282195484,-1.41544140299866,-1.4068077330654,-1.39301630384327,
-1.3723064328929,-1.35832268342317,-1.3526594265846,-1.34734360822437,-1.33527350157431,
-1.30963880664845,-1.29693930152237,-1.28840114107177,-1.27851407155737,
-1.26731537638929,-1.23958430815731,-1.23198506747337,-1.22707912560906,
-1.21985226203874,-1.21023587080884,-1.18383288203522,-1.17252500208232,
-1.16406968181561,-1.15338946439338,-1.14062577328499,-1.11656054394905,
-1.10900138834538,-1.10409489772297,-1.09682586225881,-1.08712210264066,
-1.06070683511646,-1.0494855520871,-1.04103037475671,-1.04064001717697),
 .UNSPECIFIED.);
#23518=B_SPLINE_CURVE_WITH_KNOTS('',3,(#132728,#132729,#132730,#132731,
#132732,#132733,#132734,#132735,#132736,#132737,#132738,#132739,#132740,
#132741,#132742,#132743,#132744,#132745,#132746,#132747,#132748,#132749,
#132750,#132751,#132752,#132753,#132754,#132755,#132756,#132757,#132758,
#132759,#132760,#132761,#132762,#132763,#132764,#132765,#132766,#132767),
 .UNSPECIFIED.,.F.,.F.,(4,2,2,2,2,2,2,2,2,2,2,2,2,2,2,2,2,2,2,4),(-0.244113824073537,
-0.239274607958611,-0.232075560584042,-0.215284623761484,-0.193721270389367,
-0.184734703888983,-0.176413733489245,-0.162966360303477,-0.142799703874305,
-0.128605522576123,-0.123032716585563,-0.117806633684679,-0.106999069803744,
-0.088067278378308,-0.0671333114716234,-0.0571684315808229,-0.0472634875266598,
-0.0365466086441564,-0.00613189374829842,-9.999999997512E-7),
 .UNSPECIFIED.);
#23519=B_SPLINE_CURVE_WITH_KNOTS('',3,(#132770,#132771,#132772,#132773,
#132774,#132775,#132776,#132777,#132778,#132779,#132780,#132781,#132782,
#132783,#132784,#132785,#132786,#132787,#132788,#132789,#132790,#132791,
#132792,#132793,#132794,#132795,#132796,#132797,#132798,#132799,#132800,
#132801,#132802,#132803,#132804,#132805,#132806,#132807,#132808,#132809,
#132810,#132811,#132812,#132813,#132814,#132815,#132816,#132817,#132818,
#132819,#132820,#132821,#132822,#132823,#132824,#132825,#132826,#132827,
#132828,#132829,#132830,#132831,#132832,#132833,#132834,#132835,#132836,
#132837,#132838,#132839,#132840,#132841,#132842,#132843,#132844,#132845,
#132846,#132847,#132848,#132849,#132850,#132851,#132852,#132853,#132854,
#132855,#132856,#132857,#132858,#132859,#132860,#132861,#132862,#132863,
#132864,#132865,#132866,#132867,#132868,#132869,#132870,#132871,#132872,
#132873,#132874,#132875,#132876,#132877,#132878,#132879,#132880,#132881,
#132882,#132883,#132884,#132885,#132886,#132887,#132888,#132889,#132890,
#132891,#132892,#132893),.UNSPECIFIED.,.F.,.F.,(4,3,3,3,3,3,3,3,3,3,3,3,
3,3,3,3,3,3,3,3,3,3,3,3,3,3,3,3,3,3,3,3,3,3,3,3,3,3,3,3,3,4),(2.02979616106461,
2.13731278964836,2.25387952414295,2.37034808538608,2.48676999582052,2.60327394271786,
2.7198198649459,2.83656862171718,2.90924455446903,2.90928361290806,3.01897333379382,
3.0305037634459,3.14850457265912,3.26639864796982,3.38423483867336,3.50793733330771,
3.62588130590733,3.74389791908222,3.85268065170137,3.86210971336039,3.87900456259159,
3.87904481721075,3.98841302401164,4.00026496774859,4.1179884109348,4.23560061539567,
4.3531510496196,4.47068907909621,4.58833890332437,4.70605739173758,4.81536506782819,
4.82397281846676,4.84876523864822,4.84880602151344,4.95807677792782,4.96683189172654,
5.0846917355895,5.20243492684846,5.32015599904385,5.43785457553909,5.55567683153886,
5.66555025291942),.UNSPECIFIED.);
#23520=B_SPLINE_CURVE_WITH_KNOTS('',3,(#132899,#132900,#132901,#132902,
#132903,#132904,#132905,#132906,#132907,#132908,#132909,#132910,#132911,
#132912,#132913,#132914,#132915,#132916,#132917,#132918,#132919,#132920,
#132921,#132922,#132923,#132924,#132925,#132926,#132927,#132928,#132929,
#132930,#132931,#132932,#132933,#132934,#132935,#132936,#132937,#132938,
#132939,#132940,#132941,#132942,#132943,#132944,#132945,#132946,#132947,
#132948,#132949,#132950),.UNSPECIFIED.,.F.,.F.,(4,2,2,2,2,2,2,2,2,2,2,2,
2,2,2,2,2,2,2,2,2,2,2,2,2,4),(0.344554558968716,0.344695447752049,0.370408719319506,
0.382229545579032,0.387689649352779,0.39262279171678,0.401708900904157,
0.414890311351945,0.450541662365071,0.460731339588076,0.468816672676823,
0.47883136281416,0.501888851608725,0.531468925320272,0.537561368006789,
0.542411001121594,0.549967383213274,0.559703908103843,0.587319345975018,
0.607371005886695,0.617729857954321,0.627231554499862,0.642213057001694,
0.678980954192163,0.68447448160504,0.688655615358866),.UNSPECIFIED.);
#23521=B_SPLINE_CURVE_WITH_KNOTS('',3,(#132953,#132954,#132955,#132956,
#132957,#132958,#132959,#132960,#132961,#132962,#132963,#132964,#132965,
#132966,#132967,#132968,#132969,#132970,#132971,#132972,#132973,#132974,
#132975,#132976,#132977,#132978,#132979,#132980,#132981,#132982,#132983,
#132984,#132985,#132986,#132987,#132988,#132989,#132990,#132991,#132992,
#132993,#132994,#132995,#132996,#132997,#132998,#132999,#133000,#133001,
#133002,#133003,#133004,#133005,#133006,#133007,#133008,#133009,#133010),
 .UNSPECIFIED.,.F.,.F.,(4,2,2,2,2,2,2,2,2,2,2,2,2,2,2,2,2,2,2,2,2,2,2,2,
2,2,2,2,4),(0.00011252101050449,0.041699780384492,0.0557287632500945,0.0645534172788003,
0.0737635674151307,0.091079388371737,0.11795996984337,0.12736070271703,
0.134692008622996,0.13962170386702,0.14639769538055,0.168035682739452,0.196617660235601,
0.207522562098428,0.215900590072862,0.226230086770072,0.247670796581079,
0.276081175629665,0.28396280928484,0.28886530845821,0.295003459806395,0.311857396532249,
0.336823282175015,0.352803198578938,0.36176534231516,0.370488610565894,
0.384591414707687,0.404098492780895,0.424937847293283),.UNSPECIFIED.);
#23522=B_SPLINE_CURVE_WITH_KNOTS('',3,(#133016,#133017,#133018,#133019,
#133020,#133021,#133022,#133023,#133024,#133025,#133026,#133027,#133028,
#133029,#133030,#133031,#133032,#133033,#133034,#133035,#133036,#133037,
#133038,#133039,#133040,#133041,#133042,#133043,#133044,#133045,#133046,
#133047,#133048,#133049,#133050,#133051,#133052,#133053,#133054,#133055,
#133056,#133057,#133058,#133059,#133060,#133061,#133062,#133063,#133064,
#133065,#133066,#133067,#133068,#133069,#133070,#133071,#133072,#133073,
#133074,#133075,#133076,#133077,#133078,#133079,#133080,#133081,#133082,
#133083,#133084,#133085,#133086,#133087,#133088,#133089,#133090,#133091,
#133092,#133093,#133094,#133095,#133096,#133097,#133098,#133099,#133100,
#133101,#133102,#133103),.UNSPECIFIED.,.F.,.F.,(4,2,2,2,2,2,2,2,2,2,2,2,
2,2,2,2,2,2,2,2,2,2,2,2,2,2,2,2,2,2,2,2,2,2,2,2,2,2,2,2,2,2,2,4),(0.344313126688005,
0.354918123843971,0.374366698299649,0.383748143804426,0.392345335212504,
0.405089284051333,0.43908719147313,0.44932272354443,0.457074657025849,0.461929493923398,
0.468150394212971,0.485829073431582,0.521852174852332,0.531959348747117,
0.54039981992874,0.551557879687373,0.564757640353234,0.601877414689068,
0.608288344649744,0.613149924500441,0.620466415978113,0.62986210726005,
0.656605319920672,0.67473191285089,0.683983704285279,0.692636320584211,
0.705836061138201,0.738781598773739,0.752533255556161,0.758702667603722,
0.763630337873969,0.77159418253717,0.782246926162731,0.820662279048881,
0.831090532659605,0.839537414282043,0.850354499700508,0.862914796418882,
0.894352883679797,0.904852002876094,0.910126945759735,0.91548779764376,
0.926695144009761,0.971534887947364),.UNSPECIFIED.);
#23523=B_SPLINE_CURVE_WITH_KNOTS('',3,(#133104,#133105,#133106,#133107,
#133108,#133109,#133110,#133111,#133112,#133113,#133114,#133115,#133116,
#133117,#133118,#133119,#133120,#133121,#133122,#133123,#133124,#133125,
#133126,#133127,#133128,#133129,#133130,#133131,#133132,#133133,#133134,
#133135,#133136,#133137,#133138,#133139,#133140,#133141,#133142,#133143,
#133144,#133145,#133146,#133147,#133148,#133149,#133150,#133151,#133152,
#133153,#133154,#133155,#133156,#133157),.UNSPECIFIED.,.F.,.F.,(4,2,2,2,
2,2,2,2,2,2,2,2,2,2,2,2,2,2,2,2,2,2,2,2,2,2,4),(0.000524566479899316,0.0077941571992236,
0.0151826284352965,0.0243122873221318,0.0406590091156156,0.0706586396051979,
0.0795091358994713,0.0865255523349244,0.0913709499927136,0.0981326219554219,
0.120805284763708,0.141285174801549,0.155804101380645,0.164653423760952,
0.173690646419438,0.189720230658505,0.218883157209673,0.228605882077984,
0.236105313658492,0.241047335047455,0.247603430811587,0.277711278906036,
0.293614276409027,0.306144255402436,0.314795925305086,0.324451976165178,
0.344554558968716),.UNSPECIFIED.);
#23524=B_SPLINE_CURVE_WITH_KNOTS('',3,(#133159,#133160,#133161,#133162,
#133163,#133164,#133165,#133166,#133167,#133168,#133169,#133170,#133171,
#133172,#133173,#133174,#133175,#133176,#133177,#133178,#133179,#133180,
#133181,#133182,#133183,#133184,#133185,#133186,#133187,#133188,#133189,
#133190,#133191,#133192,#133193,#133194,#133195,#133196,#133197,#133198,
#133199,#133200,#133201,#133202,#133203,#133204,#133205,#133206,#133207,
#133208,#133209,#133210,#133211,#133212,#133213,#133214,#133215,#133216),
 .UNSPECIFIED.,.F.,.F.,(4,2,2,2,2,2,2,2,2,2,2,2,2,2,2,2,2,2,2,2,2,2,2,2,
2,2,2,2,4),(0.424937847293283,0.428436000227204,0.435138620818605,0.43996872558882,
0.446986518277264,0.455831102636226,0.47890579835249,0.500189470027702,
0.509890346462041,0.518397659520366,0.530311411427524,0.544957168344203,
0.570901333375234,0.581808427089302,0.587145609789906,0.592482767170828,
0.603425566592698,0.621365986001914,0.647390935126662,0.657912395158918,
0.666329996071405,0.676963193949592,0.689209727077069,0.718398075004121,
0.730491079418018,0.736216066718949,0.74125824996203,0.750232951729319,
0.768709662504308),.UNSPECIFIED.);
#23525=B_SPLINE_CURVE_WITH_KNOTS('',3,(#133217,#133218,#133219,#133220,
#133221,#133222,#133223,#133224,#133225,#133226,#133227,#133228,#133229,
#133230,#133231,#133232,#133233,#133234,#133235,#133236,#133237,#133238,
#133239,#133240,#133241,#133242,#133243,#133244,#133245,#133246,#133247,
#133248,#133249,#133250,#133251,#133252,#133253,#133254,#133255,#133256,
#133257,#133258,#133259,#133260,#133261,#133262,#133263,#133264,#133265,
#133266,#133267,#133268,#133269,#133270,#133271,#133272,#133273,#133274,
#133275,#133276,#133277,#133278,#133279,#133280,#133281,#133282,#133283,
#133284,#133285,#133286,#133287,#133288,#133289,#133290,#133291,#133292,
#133293,#133294,#133295,#133296,#133297,#133298,#133299,#133300,#133301,
#133302,#133303,#133304),.UNSPECIFIED.,.F.,.F.,(4,2,2,2,2,2,2,2,2,2,2,2,
2,2,2,2,2,2,2,2,2,2,2,2,2,2,2,2,2,2,2,2,2,2,2,2,2,2,2,2,2,2,2,4),(0.000419544874521375,
0.0233932134995514,0.0364089109472125,0.045024068885147,0.0542931007919817,
0.0727142211952471,0.0991310565398044,0.108478695324941,0.11576629488603,
0.120620066616287,0.127033193154977,0.154085931685306,0.172261793514291,
0.185823684729299,0.194512570147632,0.203658292275543,0.220896432485435,
0.248636272349738,0.258162051746496,0.265544985518916,0.270406918789259,
0.276760764395479,0.313958603043289,0.332675935597904,0.341976982539643,
0.350487698338711,0.363314427355328,0.395002516451318,0.40635216444106,
0.414650374305314,0.419602519578251,0.425571305817675,0.441130025493829,
0.473089485352324,0.486094575418098,0.494625666168507,0.503874867646591,
0.522087704793587,0.556582967638413,0.564691773798812,0.569620959574018,
0.575673323302464,0.594016680923033,0.627725856927242),.UNSPECIFIED.);
#23526=B_SPLINE_CURVE_WITH_KNOTS('',3,(#133310,#133311,#133312,#133313,
#133314,#133315,#133316,#133317,#133318,#133319,#133320,#133321,#133322,
#133323,#133324,#133325,#133326,#133327,#133328,#133329,#133330,#133331,
#133332,#133333,#133334,#133335,#133336,#133337,#133338,#133339,#133340,
#133341,#133342,#133343,#133344,#133345,#133346,#133347,#133348,#133349,
#133350,#133351,#133352,#133353,#133354,#133355,#133356,#133357,#133358,
#133359,#133360,#133361,#133362,#133363,#133364,#133365,#133366,#133367,
#133368,#133369,#133370,#133371,#133372,#133373,#133374,#133375,#133376,
#133377,#133378,#133379,#133380,#133381,#133382,#133383,#133384,#133385,
#133386,#133387,#133388,#133389,#133390,#133391,#133392,#133393,#133394,
#133395,#133396,#133397,#133398,#133399,#133400,#133401,#133402,#133403,
#133404,#133405,#133406,#133407,#133408,#133409,#133410,#133411,#133412,
#133413,#133414,#133415,#133416,#133417,#133418,#133419,#133420,#133421,
#133422,#133423,#133424,#133425,#133426,#133427,#133428,#133429,#133430,
#133431,#133432,#133433,#133434,#133435,#133436,#133437,#133438,#133439,
#133440,#133441,#133442,#133443,#133444,#133445,#133446,#133447,#133448,
#133449,#133450,#133451,#133452,#133453,#133454),.UNSPECIFIED.,.F.,.F.,
(4,3,3,3,3,3,3,3,3,3,3,3,3,3,3,3,3,3,3,3,3,3,3,3,3,3,3,3,3,3,3,3,3,3,3,
3,3,3,3,3,3,3,3,3,3,3,3,3,4),(24.2160877562439,24.3282107851649,24.433568916188,
24.4405143049486,24.4622569195143,24.4622900504513,24.5642705178838,24.5745672323181,
24.6866901662804,24.7987091946534,24.9106667311218,25.0226050998941,25.134641377221,
25.2467284172589,25.3590102867046,25.432018123817,25.4320512548983,25.534031744494,
25.5443284200344,25.6564513436384,25.7684703654884,25.8804278992591,25.9923662691535,
26.104402553425,26.2164896036862,26.3287714884588,26.4017793281197,26.401812458991,
26.5037928807345,26.5140897641856,26.6262128229447,26.7382319769481,26.8501896396517,
26.9621281350364,27.074164538597,27.1862517048167,27.2985336989236,27.3715405324224,
27.3715736606472,27.4729397858348,27.4843897011581,27.5954688646583,27.7064470869093,
27.8173685700046,27.9316098980805,28.0426142213783,28.1584740518432,28.2669736810215,
28.2743338823082),.UNSPECIFIED.);
#23527=B_SPLINE_CURVE_WITH_KNOTS('',3,(#133455,#133456,#133457,#133458,
#133459,#133460,#133461,#133462,#133463,#133464,#133465,#133466,#133467,
#133468,#133469,#133470,#133471,#133472,#133473,#133474,#133475,#133476,
#133477,#133478,#133479,#133480,#133481,#133482,#133483,#133484,#133485,
#133486,#133487,#133488,#133489,#133490,#133491,#133492,#133493,#133494,
#133495,#133496,#133497,#133498,#133499,#133500,#133501,#133502,#133503,
#133504,#133505,#133506,#133507,#133508),.UNSPECIFIED.,.F.,.F.,(4,2,2,2,
2,2,2,2,2,2,2,2,2,2,2,2,2,2,2,2,2,2,2,2,2,2,4),(0.000401295307783161,0.00458155931597832,
0.00839099750411614,0.0129621842065248,0.0197180999475689,0.0416315109177654,
0.0701737326177952,0.0810165741531973,0.0894483718434477,0.0998096768753931,
0.122012873596538,0.14963882305013,0.157349664678133,0.162242769337582,
0.168520511947801,0.201417066394714,0.216783128127933,0.229060063100129,
0.237602488290952,0.247142420184493,0.26607663779579,0.295650400186901,
0.305631985080099,0.310829084887432,0.316325587180611,0.328401515947946,
0.344313126688005),.UNSPECIFIED.);
#23528=B_SPLINE_CURVE_WITH_KNOTS('',3,(#133510,#133511,#133512,#133513,
#133514,#133515,#133516,#133517,#133518,#133519,#133520,#133521,#133522,
#133523,#133524,#133525,#133526,#133527,#133528,#133529,#133530,#133531,
#133532,#133533,#133534,#133535,#133536,#133537,#133538,#133539,#133540,
#133541,#133542,#133543,#133544,#133545,#133546,#133547,#133548,#133549,
#133550,#133551,#133552,#133553,#133554,#133555,#133556,#133557,#133558,
#133559,#133560,#133561,#133562,#133563,#133564,#133565),.UNSPECIFIED.,
 .F.,.F.,(4,2,2,2,2,2,2,2,2,2,2,2,2,2,2,2,2,2,2,2,2,2,2,2,2,2,2,4),(0.627725856927242,
0.629596283308658,0.63975508292202,0.648183324876226,0.659243417114572,
0.672267110924607,0.707923783258628,0.715270239128067,0.720128254355387,
0.726620854841594,0.734528358704402,0.752578944641735,0.778447337204221,
0.788968913601055,0.797384035844684,0.808010516682078,0.820247867992551,
0.849396806529477,0.861503718464746,0.867231013069058,0.872275104599302,
0.881253555536561,0.894085492808777,0.929024211645749,0.939294873057738,
0.947636430899488,0.955772098337237,0.971766832159165),.UNSPECIFIED.);
#23529=B_SPLINE_CURVE_WITH_KNOTS('',3,(#133566,#133567,#133568,#133569,
#133570,#133571,#133572,#133573,#133574,#133575,#133576,#133577,#133578,
#133579,#133580,#133581,#133582,#133583,#133584,#133585,#133586,#133587,
#133588,#133589,#133590,#133591,#133592,#133593,#133594,#133595,#133596,
#133597,#133598,#133599,#133600,#133601,#133602,#133603,#133604,#133605,
#133606,#133607,#133608,#133609,#133610,#133611,#133612,#133613,#133614,
#133615,#133616,#133617,#133618,#133619,#133620,#133621,#133622,#133623,
#133624,#133625,#133626,#133627,#133628,#133629,#133630,#133631,#133632,
#133633,#133634,#133635,#133636,#133637,#133638,#133639,#133640,#133641,
#133642,#133643,#133644,#133645,#133646,#133647,#133648,#133649,#133650,
#133651,#133652,#133653,#133654,#133655,#133656,#133657),.UNSPECIFIED.,
 .F.,.F.,(4,2,2,2,2,2,2,2,2,2,2,2,2,2,2,2,2,2,2,2,2,2,2,2,2,2,2,2,2,2,2,
2,2,2,2,2,2,2,2,2,2,2,2,2,2,4),(1.73404294796756E-6,0.020495970861449,0.0330996216089653,
0.0419769718929025,0.0470070872550434,0.0527666339134735,0.0650876584115866,
0.0904623397779247,0.110007353955857,0.119387901293855,0.127964585074818,
0.140630912374979,0.174747727887424,0.184991269521981,0.192745046791807,
0.197595130754773,0.203800086830298,0.237149346034272,0.252367379953921,
0.26456711247523,0.273090986304503,0.282637514331492,0.302760301073997,
0.327070486930191,0.33981886423407,0.345394133876651,0.350521619915592,
0.360068857625006,0.392612595549552,0.405291587671783,0.416164293246166,
0.424507136403704,0.434770583644445,0.469617551530864,0.48253403595284,
0.491549675797676,0.496599330746143,0.502315871090777,0.514353726955077,
0.543561663310129,0.555805376093377,0.566436169494636,0.574851582309342,
0.585369517699426,0.610556750243185,0.627052488170293),.UNSPECIFIED.);
#23530=B_SPLINE_CURVE_WITH_KNOTS('',3,(#133663,#133664,#133665,#133666,
#133667,#133668,#133669,#133670,#133671,#133672,#133673,#133674,#133675,
#133676,#133677,#133678,#133679,#133680,#133681,#133682,#133683,#133684,
#133685,#133686,#133687,#133688,#133689,#133690,#133691,#133692,#133693,
#133694,#133695,#133696,#133697,#133698,#133699,#133700,#133701,#133702,
#133703,#133704,#133705,#133706,#133707,#133708,#133709,#133710,#133711,
#133712,#133713,#133714,#133715,#133716),.UNSPECIFIED.,.F.,.F.,(4,2,2,2,
2,2,2,2,2,2,2,2,2,2,2,2,2,2,2,2,2,2,2,2,2,2,4),(1.59817392798203,1.60932378016397,
1.61869868697383,1.62733365173653,1.64023726404545,1.67162575265904,1.68787810507124,
1.69389407117143,1.69895843539788,1.70764196400482,1.71979547470253,1.75709173714892,
1.76672103445419,1.77536478897417,1.78788251698795,1.80364999662174,1.83572560451703,
1.84214503875942,1.84685370433738,1.85369583926341,1.86232249408446,1.88440038256527,
1.90842251392954,1.91795674849125,1.92605688782117,1.93359256393498,1.94232018637391),
 .UNSPECIFIED.);
#23531=B_SPLINE_CURVE_WITH_KNOTS('',3,(#133718,#133719,#133720,#133721,
#133722,#133723,#133724,#133725,#133726,#133727,#133728,#133729,#133730,
#133731,#133732,#133733,#133734,#133735,#133736,#133737,#133738,#133739,
#133740,#133741,#133742,#133743,#133744,#133745,#133746,#133747,#133748,
#133749,#133750,#133751,#133752,#133753,#133754),.UNSPECIFIED.,.F.,.F.,
(4,3,3,3,3,3,3,3,3,3,3,3,4),(14.3984001269719,14.5130169718746,14.6275760065012,
14.7421062972226,14.8566423616352,14.9712187150792,15.0859565871695,15.2007827297925,
15.3158271617794,15.3681613312745,15.4944256857545,15.6197345261748,15.7079562980946),
 .UNSPECIFIED.);
#23532=B_SPLINE_CURVE_WITH_KNOTS('',3,(#133757,#133758,#133759,#133760,
#133761,#133762,#133763,#133764,#133765,#133766,#133767,#133768,#133769,
#133770,#133771,#133772,#133773,#133774,#133775,#133776,#133777,#133778,
#133779,#133780,#133781,#133782,#133783,#133784,#133785,#133786,#133787,
#133788,#133789,#133790,#133791,#133792,#133793,#133794,#133795,#133796,
#133797,#133798,#133799,#133800,#133801,#133802,#133803,#133804,#133805,
#133806,#133807,#133808,#133809,#133810,#133811,#133812,#133813,#133814,
#133815,#133816,#133817,#133818,#133819,#133820,#133821,#133822,#133823,
#133824,#133825,#133826,#133827,#133828,#133829,#133830,#133831,#133832,
#133833,#133834,#133835,#133836,#133837,#133838,#133839,#133840,#133841,
#133842,#133843,#133844,#133845,#133846,#133847,#133848),.UNSPECIFIED.,
 .F.,.F.,(4,2,2,2,2,2,2,2,2,2,2,2,2,2,2,2,2,2,2,2,2,2,2,2,2,2,2,2,2,2,2,
2,2,2,2,2,2,2,2,2,2,2,2,2,2,4),(0.000112843943640144,0.0344150395793074,
0.0475816383246325,0.0587690200146398,0.0673109693046341,0.0776742746139821,
0.0997465742391462,0.120127448680401,0.128509317525733,0.135289254975537,
0.140224646298994,0.146345892304485,0.168696721055489,0.196539466620812,
0.207476193689828,0.215867687975004,0.226204619100925,0.247590733136208,
0.276058306765157,0.283949747422056,0.28885942341835,0.295012543149614,
0.313697765545896,0.348258091607679,0.358533951062235,0.366921877714486,
0.37772491479056,0.406049849906477,0.428390921355262,0.435131777856181,
0.439968748744472,0.446972097379517,0.455786368887416,0.478655399225098,
0.480245614245873,0.500209382896845,0.509923033894279,0.518443987479708,
0.530386213932781,0.545079578918335,0.571611007075396,0.582071175294309,
0.587347021723258,0.592768778481349,0.604275570470769,0.627287656344573),
 .UNSPECIFIED.);
#23533=B_SPLINE_CURVE_WITH_KNOTS('',3,(#133854,#133855,#133856,#133857,
#133858,#133859,#133860,#133861,#133862,#133863,#133864,#133865,#133866,
#133867,#133868,#133869,#133870,#133871,#133872,#133873,#133874,#133875,
#133876,#133877,#133878,#133879,#133880,#133881,#133882,#133883,#133884,
#133885,#133886,#133887,#133888,#133889,#133890,#133891,#133892,#133893,
#133894,#133895,#133896,#133897,#133898,#133899,#133900,#133901,#133902,
#133903,#133904,#133905),.UNSPECIFIED.,.F.,.F.,(4,2,2,2,2,2,2,2,2,2,2,2,
2,2,2,2,2,2,2,2,2,2,2,2,2,4),(0.344554570308029,0.344695448033953,0.370408941196683,
0.382229429901131,0.387689512308191,0.392622655474436,0.401708908818249,
0.41489071511473,0.450540373360975,0.460730051156682,0.468815157898141,
0.478829209174333,0.501882341826355,0.531471648486518,0.537563112243419,
0.542412822498976,0.549970252815005,0.559708722388719,0.587337746402744,
0.607377527237151,0.617735207153022,0.627237693725668,0.642225757460128,
0.679011372906002,0.684485385955298,0.688655730947878),.UNSPECIFIED.);
#23534=B_SPLINE_CURVE_WITH_KNOTS('',3,(#133908,#133909,#133910,#133911,
#133912,#133913,#133914,#133915,#133916,#133917,#133918,#133919,#133920,
#133921,#133922,#133923,#133924,#133925,#133926,#133927,#133928,#133929,
#133930,#133931,#133932,#133933,#133934,#133935,#133936,#133937,#133938,
#133939,#133940,#133941,#133942,#133943,#133944,#133945,#133946,#133947,
#133948,#133949,#133950,#133951,#133952,#133953,#133954,#133955,#133956,
#133957,#133958,#133959,#133960,#133961,#133962,#133963,#133964,#133965,
#133966,#133967),.UNSPECIFIED.,.F.,.F.,(4,2,2,2,2,2,2,2,2,2,2,2,2,2,2,2,
2,2,2,2,2,2,2,2,2,2,2,2,2,4),(0.000112529988380809,0.0345718936956457,0.0476665506061721,
0.0588107019507166,0.0673388910924087,0.0777033809483279,0.0999073175585236,
0.120174202012848,0.128531762294313,0.135296104779885,0.140224046995345,
0.146336449042626,0.169040670185855,0.196595790121934,0.207502067193846,
0.215880876797446,0.226211031245187,0.247646363014807,0.276065348337023,
0.283948227631305,0.288851260167232,0.294989820414519,0.311844188310828,
0.336813210391308,0.352794826152219,0.361757836185347,0.370481925336095,
0.384586044921021,0.404094984019906,0.424935994621487),.UNSPECIFIED.);
#23535=B_SPLINE_CURVE_WITH_KNOTS('',3,(#133973,#133974,#133975,#133976,
#133977,#133978,#133979,#133980,#133981,#133982,#133983,#133984,#133985,
#133986,#133987,#133988,#133989,#133990,#133991,#133992,#133993,#133994,
#133995,#133996,#133997,#133998,#133999,#134000,#134001,#134002,#134003,
#134004,#134005,#134006,#134007,#134008,#134009,#134010,#134011,#134012,
#134013,#134014,#134015,#134016,#134017,#134018,#134019,#134020,#134021,
#134022,#134023,#134024,#134025,#134026,#134027,#134028,#134029,#134030,
#134031,#134032,#134033,#134034,#134035,#134036,#134037,#134038,#134039,
#134040,#134041,#134042,#134043,#134044,#134045,#134046,#134047,#134048,
#134049,#134050,#134051,#134052,#134053,#134054,#134055,#134056,#134057,
#134058,#134059,#134060,#134061,#134062),.UNSPECIFIED.,.F.,.F.,(4,2,2,2,
2,2,2,2,2,2,2,2,2,2,2,2,2,2,2,2,2,2,2,2,2,2,2,2,2,2,2,2,2,2,2,2,2,2,2,2,
2,2,2,2,4),(0.344313486464405,0.354919217679905,0.374367251033343,0.383748646768653,
0.392345856556732,0.405089960994582,0.439087634345528,0.449323145453929,
0.457075068601599,0.461929902784375,0.468150800236277,0.48582949980041,
0.521852601311326,0.531959774696942,0.540400237948904,0.551558272143675,
0.564757988389301,0.601877506238842,0.608288600784844,0.613150160477552,
0.620466393709948,0.629861599602323,0.656601237072781,0.674731088755373,
0.683983221220231,0.692635665603424,0.705834051066166,0.738772359850567,
0.75252375532549,0.758697268725943,0.76362408390867,0.771579943092398,0.782216588592994,
0.820503819569033,0.830989708733161,0.839435301198206,0.850187787984699,
0.862631532694381,0.893170698525703,0.904467358894393,0.909859092781245,
0.915105460942586,0.92552656820499,0.957906589824195,0.971485427032841),
 .UNSPECIFIED.);
#23536=B_SPLINE_CURVE_WITH_KNOTS('',3,(#134063,#134064,#134065,#134066,
#134067,#134068,#134069,#134070,#134071,#134072,#134073,#134074,#134075,
#134076,#134077,#134078,#134079,#134080,#134081,#134082,#134083,#134084,
#134085,#134086,#134087,#134088,#134089,#134090,#134091,#134092,#134093,
#134094,#134095,#134096,#134097,#134098,#134099,#134100,#134101,#134102,
#134103,#134104,#134105,#134106,#134107,#134108,#134109,#134110,#134111,
#134112,#134113,#134114,#134115,#134116),.UNSPECIFIED.,.F.,.F.,(4,2,2,2,
2,2,2,2,2,2,2,2,2,2,2,2,2,2,2,2,2,2,2,2,2,2,4),(0.000524579872864791,0.0077944514346942,
0.0151832658544194,0.0243130963212922,0.0406614428251173,0.0706592319194637,
0.0795094358608527,0.0865256870499652,0.0913710570366877,0.0981327838735026,
0.120801828274982,0.141283992141634,0.155803797723929,0.164653221110243,
0.173690270313448,0.189718555331087,0.218883005374065,0.228605913263831,
0.236105442162938,0.241047510735411,0.247603705193052,0.277710767663671,
0.293613869820421,0.306143913315913,0.31479567257371,0.324451901360994,
0.344554570308029),.UNSPECIFIED.);
#23537=B_SPLINE_CURVE_WITH_KNOTS('',3,(#134118,#134119,#134120,#134121,
#134122,#134123,#134124,#134125,#134126,#134127,#134128,#134129,#134130,
#134131,#134132,#134133,#134134,#134135,#134136,#134137,#134138,#134139,
#134140,#134141,#134142,#134143,#134144,#134145,#134146,#134147,#134148,
#134149,#134150,#134151,#134152,#134153,#134154,#134155,#134156,#134157,
#134158,#134159,#134160,#134161,#134162,#134163,#134164,#134165,#134166,
#134167,#134168,#134169,#134170,#134171,#134172,#134173,#134174,#134175),
 .UNSPECIFIED.,.F.,.F.,(4,2,2,2,2,2,2,2,2,2,2,2,2,2,2,2,2,2,2,2,2,2,2,2,
2,2,2,2,4),(0.424935994621487,0.428434306985777,0.435137547766552,0.439968088825602,
0.446986518483714,0.455831924158091,0.478908971408985,0.500193935217088,
0.509895637397591,0.518403653917941,0.53031833398969,0.544965154453378,
0.570911351546204,0.581820017785732,0.587157739882083,0.592495244586144,
0.603438191516193,0.621377752544442,0.647408712093355,0.65793107966815,
0.666349427953283,0.676983602628536,0.689231289510795,0.718422809269537,
0.730516198872072,0.736241588425334,0.741284281142336,0.750260193385671,
0.768737819720641),.UNSPECIFIED.);
#23538=B_SPLINE_CURVE_WITH_KNOTS('',3,(#134176,#134177,#134178,#134179,
#134180,#134181,#134182,#134183,#134184,#134185,#134186,#134187,#134188,
#134189,#134190,#134191,#134192,#134193,#134194,#134195,#134196,#134197,
#134198,#134199,#134200,#134201,#134202,#134203,#134204,#134205,#134206,
#134207,#134208,#134209,#134210,#134211,#134212,#134213,#134214,#134215,
#134216,#134217,#134218,#134219,#134220,#134221,#134222,#134223,#134224,
#134225,#134226,#134227,#134228,#134229,#134230,#134231,#134232,#134233,
#134234,#134235,#134236,#134237,#134238,#134239,#134240,#134241,#134242,
#134243,#134244,#134245,#134246,#134247,#134248,#134249,#134250,#134251,
#134252,#134253,#134254,#134255,#134256,#134257,#134258,#134259,#134260,
#134261,#134262,#134263),.UNSPECIFIED.,.F.,.F.,(4,2,2,2,2,2,2,2,2,2,2,2,
2,2,2,2,2,2,2,2,2,2,2,2,2,2,2,2,2,2,2,2,2,2,2,2,2,2,2,2,2,2,2,4),(0.000419556825689101,
0.0234235476872869,0.0364236724353723,0.0450369352546755,0.0543102946946294,
0.0727735427684984,0.0991442428415436,0.108485488127689,0.115769686914703,
0.120623273375649,0.127038864838353,0.154066218248185,0.172253033302996,
0.185819599851877,0.194509080518614,0.203653767132057,0.220882755561306,
0.248633390164057,0.258160573644001,0.265544247933525,0.27040623125339,
0.276759577475357,0.313958277312445,0.332675852622128,0.341976930682322,
0.35048764788506,0.363314326813168,0.395002420075205,0.406352115160209,
0.414650349205732,0.419602502276444,0.425571294009416,0.441130002729049,
0.473089471258454,0.486094566989405,0.494625665793476,0.503874881633195,
0.522087790581881,0.556583428730765,0.564691981827064,0.569621141859567,
0.575673634105917,0.59401933078766,0.627725845557793),.UNSPECIFIED.);
#23539=B_SPLINE_CURVE_WITH_KNOTS('',3,(#134269,#134270,#134271,#134272,
#134273,#134274,#134275,#134276,#134277,#134278,#134279,#134280,#134281,
#134282,#134283,#134284,#134285,#134286,#134287,#134288,#134289,#134290,
#134291,#134292,#134293,#134294,#134295,#134296,#134297,#134298,#134299,
#134300,#134301,#134302,#134303,#134304,#134305,#134306,#134307,#134308,
#134309,#134310,#134311,#134312,#134313,#134314,#134315,#134316,#134317,
#134318,#134319,#134320,#134321,#134322,#134323,#134324,#134325,#134326,
#134327,#134328,#134329,#134330,#134331,#134332,#134333,#134334,#134335,
#134336,#134337,#134338,#134339,#134340,#134341,#134342,#134343,#134344,
#134345,#134346,#134347,#134348,#134349,#134350,#134351,#134352,#134353,
#134354,#134355,#134356,#134357,#134358,#134359,#134360,#134361,#134362,
#134363,#134364,#134365,#134366,#134367,#134368,#134369,#134370,#134371,
#134372,#134373,#134374,#134375,#134376,#134377,#134378,#134379,#134380,
#134381,#134382,#134383,#134384,#134385,#134386,#134387,#134388,#134389,
#134390,#134391,#134392,#134393,#134394,#134395,#134396,#134397,#134398,
#134399,#134400,#134401,#134402,#134403,#134404,#134405,#134406,#134407,
#134408,#134409,#134410,#134411,#134412,#134413),.UNSPECIFIED.,.F.,.F.,
(4,3,3,3,3,3,3,3,3,3,3,3,3,3,3,3,3,3,3,3,3,3,3,3,3,3,3,3,3,3,3,3,3,3,3,
3,3,3,3,3,3,3,3,3,3,3,3,3,4),(24.216087767712,24.3282107965545,24.4335689263792,
24.4405143162603,24.4622569195143,24.4622900487738,24.5642705166895,24.5745672322469,
24.6866901661316,24.7987091944231,24.9106667308059,25.022605099489,25.134641376722,
25.246728416663,25.3590102860085,25.432018123817,25.4320512532201,25.5340317434683,
25.5443284199335,25.6564513434411,25.7684703651978,25.8804278988782,25.9923662686856,
26.1044025528757,26.2164896030587,26.3287714877585,26.4017793281197,26.4018124573133,
26.5037928793349,26.5140897641019,26.6262128227728,26.7382319766855,26.8501896392961,
26.9621281345857,27.0741645380486,27.1862517041689,27.2985336981754,27.3715405324224,
27.3715736589642,27.4729397859234,27.4843897011581,27.5954688655842,27.7064470887626,
27.8173685727851,27.9316099001658,28.0426142243821,28.1584740533451,28.2669736829371,
28.2743338823081),.UNSPECIFIED.);
#23540=B_SPLINE_CURVE_WITH_KNOTS('',3,(#134414,#134415,#134416,#134417,
#134418,#134419,#134420,#134421,#134422,#134423,#134424,#134425,#134426,
#134427,#134428,#134429,#134430,#134431,#134432,#134433,#134434,#134435,
#134436,#134437,#134438,#134439,#134440,#134441,#134442,#134443,#134444,
#134445,#134446,#134447,#134448,#134449,#134450,#134451,#134452,#134453,
#134454,#134455,#134456,#134457,#134458,#134459,#134460,#134461,#134462,
#134463,#134464,#134465,#134466,#134467),.UNSPECIFIED.,.F.,.F.,(4,2,2,2,
2,2,2,2,2,2,2,2,2,2,2,2,2,2,2,2,2,2,2,2,2,2,4),(0.000401297033932362,0.0045833394714876,
0.0083941896639838,0.0129672560599783,0.0197274769357702,0.04145800294407,
0.0701402862518669,0.0809963173745193,0.0894284984122356,0.0997787062367564,
0.121842191887511,0.149636983875748,0.157348925773996,0.162242131051256,
0.168519227062528,0.201420136837407,0.216784837708568,0.229061105347135,
0.237603455717508,0.247143637717364,0.266080261220836,0.29565142444061,
0.305632575109507,0.310829609526097,0.31632619907144,0.328402795445856,
0.344313486464405),.UNSPECIFIED.);
#23541=B_SPLINE_CURVE_WITH_KNOTS('',3,(#134469,#134470,#134471,#134472,
#134473,#134474,#134475,#134476,#134477,#134478,#134479,#134480,#134481,
#134482,#134483,#134484,#134485,#134486,#134487,#134488,#134489,#134490,
#134491,#134492,#134493,#134494,#134495,#134496,#134497,#134498,#134499,
#134500,#134501,#134502,#134503,#134504,#134505,#134506,#134507,#134508,
#134509,#134510,#134511,#134512,#134513,#134514,#134515,#134516,#134517,
#134518,#134519,#134520,#134521,#134522,#134523,#134524),.UNSPECIFIED.,
 .F.,.F.,(4,2,2,2,2,2,2,2,2,2,2,2,2,2,2,2,2,2,2,2,2,2,2,2,2,2,2,4),(0.627725845557793,
0.62959455629134,0.639753947806432,0.648182156686605,0.659241458900321,
0.672263694044832,0.707905999391311,0.715261384704962,0.720119965754627,
0.726606149982481,0.734502457838602,0.752500166433806,0.778447993536197,
0.788969327470095,0.797384452912912,0.808011191745445,0.820249004924034,
0.849401196897434,0.861505005868494,0.867231817069353,0.872276138310599,
0.881256199040214,0.894091794706562,0.929020784219794,0.93929260184998,
0.947634105787937,0.955769439433221,0.9717666708796),.UNSPECIFIED.);
#23542=B_SPLINE_CURVE_WITH_KNOTS('',3,(#134525,#134526,#134527,#134528,
#134529,#134530,#134531,#134532,#134533,#134534,#134535,#134536,#134537,
#134538,#134539,#134540,#134541,#134542,#134543,#134544,#134545,#134546,
#134547,#134548,#134549,#134550,#134551,#134552,#134553,#134554,#134555,
#134556,#134557,#134558,#134559,#134560,#134561,#134562,#134563,#134564,
#134565,#134566,#134567,#134568,#134569,#134570,#134571,#134572,#134573,
#134574,#134575,#134576,#134577,#134578,#134579,#134580,#134581,#134582,
#134583,#134584,#134585,#134586,#134587,#134588,#134589,#134590,#134591,
#134592,#134593,#134594,#134595,#134596,#134597,#134598,#134599,#134600,
#134601,#134602,#134603,#134604,#134605,#134606,#134607,#134608,#134609,
#134610,#134611,#134612,#134613,#134614,#134615,#134616),.UNSPECIFIED.,
 .F.,.F.,(4,2,2,2,2,2,2,2,2,2,2,2,2,2,2,2,2,2,2,2,2,2,2,2,2,2,2,2,2,2,2,
2,2,2,2,2,2,2,2,2,2,2,2,2,2,4),(1.73076609795579E-6,0.0308260776152478,
0.0411297792638463,0.0463705483701984,0.0517900282356288,0.0633270135787932,
0.0935679054319864,0.105955696862113,0.116667427218672,0.125085191458525,
0.135531025496316,0.158996962229642,0.178864854816529,0.187140885339661,
0.193842621044572,0.19868886428263,0.20577258821334,0.238558230006278,0.253108382173655,
0.264973594391783,0.273464235953274,0.283156214173948,0.304287981588959,
0.327474597593947,0.339946740811486,0.345488585806428,0.350638405712978,
0.360333271332897,0.392697215803507,0.405355520705415,0.416217202360555,
0.424560368605396,0.434834518734227,0.469613318366356,0.48255615819977,
0.491583663593267,0.496635375565032,0.502349192799566,0.514367772548698,
0.543600330747344,0.555848314144331,0.566481856131924,0.574898085660617,
0.585415364687804,0.610520755007593,0.627106652223347),.UNSPECIFIED.);
#23543=B_SPLINE_CURVE_WITH_KNOTS('',3,(#134622,#134623,#134624,#134625,
#134626,#134627,#134628,#134629,#134630,#134631,#134632,#134633,#134634,
#134635,#134636,#134637,#134638,#134639,#134640,#134641,#134642,#134643,
#134644,#134645,#134646,#134647,#134648,#134649,#134650,#134651,#134652,
#134653,#134654,#134655,#134656,#134657,#134658,#134659,#134660,#134661,
#134662,#134663,#134664,#134665,#134666,#134667,#134668,#134669,#134670,
#134671,#134672,#134673,#134674,#134675),.UNSPECIFIED.,.F.,.F.,(4,2,2,2,
2,2,2,2,2,2,2,2,2,2,2,2,2,2,2,2,2,2,2,2,2,2,4),(1.5983191600895,1.60946910178581,
1.61884493097629,1.62748074613801,1.64038564951555,1.67177729836047,1.68803128256708,
1.69404778312266,1.69911242113056,1.70779607100985,1.7199492720761,1.75725320746205,
1.76688312348883,1.77552740817065,1.7880457114298,1.80381364377214,1.83589481074534,
1.84231437036927,1.84702348653321,1.85386689188086,1.86249540869345,1.88458083085954,
1.90859939226412,1.91813484301809,1.92623635583885,1.93377128574619,1.94249761222262),
 .UNSPECIFIED.);
#23544=B_SPLINE_CURVE_WITH_KNOTS('',3,(#134677,#134678,#134679,#134680,
#134681,#134682,#134683,#134684,#134685,#134686,#134687,#134688,#134689,
#134690,#134691,#134692,#134693,#134694,#134695,#134696,#134697,#134698,
#134699,#134700,#134701,#134702,#134703,#134704,#134705,#134706,#134707,
#134708,#134709,#134710,#134711,#134712,#134713),.UNSPECIFIED.,.F.,.F.,
(4,3,3,3,3,3,3,3,3,3,3,3,4),(14.3984001269719,14.5130159814057,14.6275739868434,
14.7421032271326,14.856638223687,14.9712134956359,15.0859502774624,15.2007753249216,
15.3158186683707,15.3681613312746,15.4944270641862,15.6197373683541,15.7079562990334),
 .UNSPECIFIED.);
#23545=B_SPLINE_CURVE_WITH_KNOTS('',3,(#134716,#134717,#134718,#134719,
#134720,#134721,#134722,#134723,#134724,#134725,#134726,#134727,#134728,
#134729,#134730,#134731,#134732,#134733,#134734,#134735,#134736,#134737,
#134738,#134739,#134740,#134741,#134742,#134743,#134744,#134745,#134746,
#134747,#134748,#134749,#134750,#134751,#134752,#134753,#134754,#134755,
#134756,#134757,#134758,#134759,#134760,#134761,#134762,#134763,#134764,
#134765,#134766,#134767,#134768,#134769,#134770,#134771,#134772,#134773,
#134774,#134775,#134776,#134777,#134778,#134779,#134780,#134781,#134782,
#134783,#134784,#134785,#134786,#134787,#134788,#134789,#134790,#134791,
#134792,#134793,#134794,#134795,#134796,#134797,#134798,#134799,#134800,
#134801,#134802,#134803,#134804,#134805,#134806,#134807),.UNSPECIFIED.,
 .F.,.F.,(4,2,2,2,2,2,2,2,2,2,2,2,2,2,2,2,2,2,2,2,2,2,2,2,2,2,2,2,2,2,2,
2,2,2,2,2,2,2,2,2,2,2,2,2,2,4),(0.000112838215867501,0.0344137848853368,
0.0475811293693514,0.0587689530819971,0.0673110177778552,0.0776742517777449,
0.0997450585740924,0.120126913328797,0.128508978000661,0.135289040547425,
0.140224478619107,0.146345772442547,0.16869308144312,0.19653936634855,0.207475967120287,
0.2158674386007,0.226204420266539,0.247591969570469,0.276058453560075,0.283949792254572,
0.2888594371998,0.295012537477586,0.313697743449704,0.348258117572018,0.358533952470444,
0.366921848083298,0.377724819707815,0.406049259932434,0.428390970158201,
0.435131806471044,0.439968768855761,0.446972104919837,0.45578635292522,
0.478655233889584,0.480248254062548,0.500217393499176,0.50992868790014,
0.518450149366918,0.530397555504147,0.545101171597835,0.57166148007292,
0.582088430897414,0.587359340365255,0.592786863115678,0.604335610698444,
0.627287566072145),.UNSPECIFIED.);
#23546=B_SPLINE_CURVE_WITH_KNOTS('',3,(#134809,#134810,#134811,#134812,
#134813,#134814,#134815,#134816,#134817,#134818,#134819,#134820,#134821,
#134822,#134823,#134824,#134825,#134826,#134827,#134828,#134829,#134830,
#134831,#134832,#134833,#134834,#134835,#134836,#134837,#134838,#134839,
#134840,#134841,#134842,#134843,#134844,#134845,#134846,#134847,#134848,
#134849,#134850,#134851,#134852,#134853,#134854,#134855,#134856,#134857,
#134858,#134859,#134860,#134861,#134862,#134863,#134864,#134865,#134866,
#134867,#134868,#134869,#134870,#134871,#134872,#134873,#134874,#134875,
#134876,#134877,#134878,#134879,#134880,#134881,#134882,#134883,#134884,
#134885,#134886,#134887,#134888,#134889,#134890,#134891,#134892,#134893,
#134894,#134895,#134896,#134897,#134898,#134899,#134900,#134901,#134902,
#134903,#134904,#134905,#134906,#134907,#134908,#134909,#134910,#134911,
#134912,#134913,#134914,#134915,#134916,#134917,#134918,#134919,#134920,
#134921,#134922,#134923,#134924,#134925,#134926,#134927,#134928,#134929,
#134930,#134931,#134932,#134933,#134934,#134935,#134936,#134937,#134938,
#134939,#134940,#134941,#134942,#134943,#134944,#134945,#134946,#134947,
#134948,#134949,#134950),.UNSPECIFIED.,.F.,.F.,(4,2,2,2,2,2,2,2,2,2,2,2,
2,2,2,2,2,2,2,2,2,2,2,2,2,2,2,2,2,2,2,2,2,2,2,2,2,2,2,2,2,2,2,2,2,2,2,2,
2,2,2,2,2,2,2,2,2,2,2,2,2,2,2,2,2,2,2,2,2,2,4),(6.82072967247012E-5,0.020612855930782,
0.0289793048578245,0.0374722935793014,0.0472454148643254,0.07016917077208,
0.0985873974547638,0.106463587934993,0.111372235066616,0.117553851921224,
0.151088051442694,0.166252240727669,0.178428109610994,0.186956007413909,
0.196526979493893,0.216053714943285,0.240778730125056,0.249885028192609,
0.257045289735006,0.26189945094549,0.268555116618211,0.293782279264809,
0.312773881779431,0.326680982466161,0.335423165916425,0.344515934354849,
0.361220486014547,0.389600788076956,0.399211608413098,0.406641268814885,
0.411512630137261,0.417855827415522,0.445667228247553,0.463517194718252,
0.476941553742677,0.485620356841447,0.494812971120406,0.512407478679775,
0.543683969011262,0.554307856288399,0.55960027585328,0.564977267092943,
0.576182088279459,0.594918799241663,0.619813282836159,0.630332419720432,
0.638760589222806,0.649426524278923,0.66172664418531,0.691277440738422,
0.703020891435863,0.708692813393365,0.713778154448283,0.72300524960665,
0.736403914840773,0.772023656998422,0.781766847232403,0.790263071456699,
0.802074302205074,0.816511714099025,0.842313969786416,0.853715704411164,
0.859120950462794,0.864389723841491,0.874851519250536,0.907457399377032,
0.924306359097852,0.933414594761016,0.942143430186657,0.952991945071345,
0.971189088135237),.UNSPECIFIED.);
#23547=B_SPLINE_CURVE_WITH_KNOTS('',3,(#134951,#134952,#134953,#134954,
#134955,#134956,#134957,#134958,#134959,#134960,#134961,#134962,#134963,
#134964,#134965,#134966,#134967,#134968,#134969,#134970,#134971,#134972,
#134973,#134974,#134975,#134976,#134977,#134978,#134979,#134980,#134981,
#134982,#134983,#134984,#134985,#134986,#134987,#134988,#134989,#134990,
#134991,#134992,#134993,#134994,#134995,#134996,#134997,#134998,#134999,
#135000,#135001,#135002,#135003,#135004,#135005,#135006,#135007,#135008,
#135009,#135010,#135011,#135012,#135013,#135014,#135015,#135016,#135017,
#135018,#135019,#135020,#135021,#135022,#135023,#135024,#135025,#135026,
#135027,#135028,#135029,#135030,#135031,#135032,#135033,#135034,#135035,
#135036,#135037,#135038,#135039,#135040,#135041,#135042,#135043,#135044,
#135045,#135046,#135047,#135048,#135049,#135050,#135051,#135052,#135053,
#135054,#135055,#135056,#135057,#135058,#135059,#135060,#135061,#135062,
#135063,#135064,#135065,#135066,#135067,#135068,#135069,#135070,#135071,
#135072,#135073,#135074,#135075,#135076,#135077,#135078,#135079,#135080,
#135081,#135082,#135083,#135084,#135085,#135086,#135087,#135088,#135089,
#135090,#135091,#135092,#135093,#135094,#135095,#135096),.UNSPECIFIED.,
 .F.,.F.,(4,2,2,2,2,2,2,2,2,2,2,2,2,2,2,2,2,2,2,2,2,2,2,2,2,2,2,2,2,2,2,
2,2,2,2,2,2,2,2,2,2,2,2,2,2,2,2,2,2,2,2,2,2,2,2,2,2,2,2,2,2,2,2,2,2,2,2,
2,2,2,2,2,4),(0.627106652223347,0.629123486082643,0.637147607467664,0.643706619587023,
0.648559944568491,0.655817785236257,0.691615180300921,0.704651951605286,
0.71572056621102,0.724150494292224,0.734305893756065,0.769953866615976,
0.782592043807738,0.791484964292521,0.796517901061968,0.802275928685794,
0.814579293200728,0.839961023065592,0.859510168351007,0.868892561545163,
0.87747217535699,0.890146638219859,0.924255507357647,0.93449884137058,0.942252760621376,
0.947102244961131,0.953303129879324,0.971212130986432,1.00691574265751,
1.01705796596725,1.02548279599575,1.0365510806174,1.04959199381931,1.08542572379961,
1.09266652813928,1.09751725079561,1.10408354879256,1.11211938894129,1.1307803944364,
1.1558058844306,1.16632418249714,1.17474254277447,1.18538093246616,1.19763834622744,
1.22692259217994,1.23889768048791,1.24460810929962,1.24967941946219,1.25878977346316,
1.27191966404575,1.3060112483004,1.31636527760657,1.324801785069,1.33566829156301,
1.3644093641721,1.38612043426777,1.39287886762142,1.39770785637703,1.40466892816411,
1.41342214606773,1.43598649976264,1.45827454192538,1.4678799978639,1.47633265693326,
1.4881884256979,1.5027503126632,1.53685237531525,1.54323909784667,1.54809120222948,
1.55538695180452,1.56473743996364,1.5910810217434,1.5983191600895),
 .UNSPECIFIED.);
#23548=B_SPLINE_CURVE_WITH_KNOTS('',3,(#135098,#135099,#135100,#135101,
#135102,#135103,#135104,#135105,#135106,#135107,#135108,#135109,#135110,
#135111,#135112,#135113,#135114,#135115,#135116,#135117,#135118,#135119,
#135120,#135121,#135122,#135123,#135124,#135125,#135126,#135127,#135128,
#135129,#135130,#135131,#135132,#135133,#135134,#135135,#135136,#135137,
#135138,#135139,#135140,#135141,#135142,#135143,#135144,#135145,#135146,
#135147,#135148,#135149,#135150,#135151,#135152,#135153,#135154,#135155,
#135156,#135157,#135158,#135159,#135160,#135161,#135162,#135163,#135164,
#135165,#135166,#135167,#135168,#135169,#135170,#135171,#135172,#135173,
#135174,#135175,#135176,#135177,#135178,#135179,#135180,#135181,#135182,
#135183,#135184,#135185,#135186,#135187,#135188,#135189,#135190,#135191,
#135192,#135193,#135194,#135195,#135196,#135197,#135198,#135199,#135200,
#135201,#135202,#135203,#135204,#135205,#135206,#135207,#135208,#135209,
#135210,#135211,#135212,#135213,#135214,#135215,#135216,#135217,#135218,
#135219,#135220,#135221,#135222,#135223,#135224,#135225,#135226,#135227,
#135228,#135229,#135230,#135231,#135232,#135233,#135234,#135235,#135236,
#135237,#135238,#135239),.UNSPECIFIED.,.F.,.F.,(4,2,2,2,2,2,2,2,2,2,2,2,
2,2,2,2,2,2,2,2,2,2,2,2,2,2,2,2,2,2,2,2,2,2,2,2,2,2,2,2,2,2,2,2,2,2,2,2,
2,2,2,2,2,2,2,2,2,2,2,2,2,2,2,2,2,2,2,2,2,2,4),(6.82064154310527E-5,0.0206122609103592,
0.0289788297288812,0.0374718670697915,0.0472447831254516,0.0701612291856842,
0.0985862746444113,0.106463074562659,0.111371791601236,0.117553109412752,
0.151089409067014,0.166252939478315,0.178428485624057,0.186956358547689,
0.196527482397229,0.216052479328968,0.240778433475478,0.249884875574736,
0.257045216509811,0.261899385421799,0.26855500119635,0.293782789437433,
0.312774097284305,0.326681078434405,0.335423249713859,0.344516048076797,
0.361220826901406,0.389600866084423,0.399211654980418,0.406641299612127,
0.411512662197177,0.417855877817988,0.445667116793014,0.463517154956275,
0.476941547929924,0.485620361207113,0.494812979986727,0.512407480102826,
0.543683926524452,0.554307847707887,0.559600275259536,0.564977269815557,
0.576182094468019,0.594918810755804,0.619813286211509,0.630332428002734,
0.638760605202319,0.649426557329208,0.661726703277235,0.691277663257335,
0.703020968280399,0.70869286743362,0.713778228110877,0.723005439231197,
0.736404372936923,0.772023388484475,0.781766664709639,0.790262880809526,
0.802073962519849,0.816511078884114,0.842313178009023,0.853715464178983,
0.85912078949944,0.86438950272873,0.874850875776926,0.907453929464112,0.924305179270456,
0.933413686956909,0.942142364010327,0.952991291839689,0.97118908114431),
 .UNSPECIFIED.);
#23549=B_SPLINE_CURVE_WITH_KNOTS('',3,(#135240,#135241,#135242,#135243,
#135244,#135245,#135246,#135247,#135248,#135249,#135250,#135251,#135252,
#135253,#135254,#135255,#135256,#135257,#135258,#135259,#135260,#135261,
#135262,#135263,#135264,#135265,#135266,#135267,#135268,#135269,#135270,
#135271,#135272,#135273,#135274,#135275,#135276,#135277,#135278,#135279,
#135280,#135281,#135282,#135283,#135284,#135285,#135286,#135287,#135288,
#135289,#135290,#135291,#135292,#135293,#135294,#135295,#135296,#135297,
#135298,#135299,#135300,#135301,#135302,#135303,#135304,#135305,#135306,
#135307,#135308,#135309,#135310,#135311,#135312,#135313,#135314,#135315,
#135316,#135317,#135318,#135319,#135320,#135321,#135322,#135323,#135324,
#135325,#135326,#135327,#135328,#135329,#135330,#135331,#135332,#135333,
#135334,#135335,#135336,#135337,#135338,#135339,#135340,#135341,#135342,
#135343,#135344,#135345,#135346,#135347,#135348,#135349,#135350,#135351,
#135352,#135353,#135354,#135355,#135356,#135357,#135358,#135359,#135360,
#135361,#135362,#135363,#135364,#135365,#135366,#135367,#135368,#135369,
#135370,#135371,#135372,#135373,#135374,#135375,#135376,#135377,#135378,
#135379,#135380,#135381,#135382,#135383,#135384,#135385),.UNSPECIFIED.,
 .F.,.F.,(4,2,2,2,2,2,2,2,2,2,2,2,2,2,2,2,2,2,2,2,2,2,2,2,2,2,2,2,2,2,2,
2,2,2,2,2,2,2,2,2,2,2,2,2,2,2,2,2,2,2,2,2,2,2,2,2,2,2,2,2,2,2,2,2,2,2,2,
2,2,2,2,2,4),(0.627052488170293,0.629097476923593,0.637108433107913,0.643659753834069,
0.648513112425859,0.655779516904756,0.691558478122418,0.704592503143053,
0.715659250357901,0.724088338715216,0.734243367480604,0.769883613171745,
0.782522117280072,0.791414875982714,0.796447434225467,0.802204710988669,
0.814505448463294,0.839885179036521,0.859433710725933,0.868815335481488,
0.877394104971846,0.890067035347798,0.924173302861861,0.934415734856313,
0.94216895647577,0.947017985429099,0.95321825645414,0.971126021556437,1.00682566147047,
1.01696700696627,1.02539102365338,1.0364581126144,1.04949752150781,1.08532515497896,
1.092566953772,1.09741729528189,1.10398164108412,1.11201438539871,1.13066222401229,
1.15570127483238,1.16621895058941,1.17463650550304,1.18527347923898,1.1975290058821,
1.22680537517602,1.23878404896918,1.24449471591593,1.24956519975383,1.25867215500841,
1.27179493028354,1.30589953622533,1.31625036145358,1.32468619493319,1.33555446558064,
1.36432230424464,1.38599368746079,1.39275208831188,1.39758059777592,1.40454029987336,
1.41329140989759,1.43584607482569,1.458141909584,1.4677465454054,1.47619830951384,
1.48805249355466,1.50261212623886,1.53671332499098,1.54309921399244,1.54795081627567,
1.55524594764188,1.5645956971375,1.59093771395068,1.59817392798203),
 .UNSPECIFIED.);
#23550=B_SPLINE_CURVE_WITH_KNOTS('',3,(#135388,#135389,#135390,#135391,
#135392,#135393,#135394,#135395,#135396,#135397,#135398,#135399,#135400,
#135401,#135402,#135403,#135404,#135405,#135406,#135407,#135408,#135409,
#135410,#135411,#135412,#135413,#135414,#135415,#135416,#135417,#135418,
#135419,#135420,#135421,#135422,#135423,#135424,#135425,#135426,#135427,
#135428,#135429,#135430,#135431,#135432,#135433,#135434,#135435,#135436,
#135437,#135438,#135439,#135440,#135441,#135442,#135443,#135444,#135445,
#135446,#135447,#135448,#135449,#135450,#135451,#135452,#135453,#135454,
#135455,#135456,#135457,#135458,#135459,#135460),.UNSPECIFIED.,.F.,.F.,
(4,3,3,3,3,3,3,3,3,3,3,3,3,3,3,3,3,3,3,3,3,3,3,3,4),(5.66555025349161,5.77596501629269,
5.78359419481329,5.81852702745744,5.81856722581613,5.92802936256689,5.93978737635397,
6.05763571976858,6.17537452312111,6.29305298232785,6.41687184427559,6.53465411287049,
6.65250789513665,6.76130413452367,6.77055655343442,6.78828803449599,6.78832843011882,
6.89648185188166,6.90464476357801,7.02079948264988,7.13684497738031,7.25288906167345,
7.36892199840986,7.48510590926794,7.59274844756046),.UNSPECIFIED.);
#23551=B_SPLINE_CURVE_WITH_KNOTS('',3,(#135461,#135462,#135463,#135464,
#135465,#135466,#135467,#135468,#135469,#135470,#135471,#135472,#135473,
#135474,#135475,#135476,#135477,#135478,#135479,#135480,#135481,#135482,
#135483,#135484,#135485,#135486,#135487,#135488,#135489,#135490,#135491,
#135492,#135493,#135494,#135495,#135496,#135497,#135498,#135499,#135500,
#135501,#135502,#135503,#135504,#135505,#135506,#135507,#135508,#135509,
#135510,#135511,#135512,#135513,#135514,#135515,#135516,#135517,#135518,
#135519,#135520,#135521,#135522,#135523,#135524,#135525,#135526,#135527,
#135528,#135529,#135530,#135531,#135532,#135533,#135534,#135535,#135536,
#135537,#135538,#135539,#135540,#135541,#135542,#135543,#135544,#135545,
#135546,#135547,#135548,#135549,#135550,#135551,#135552,#135553,#135554,
#135555,#135556,#135557,#135558,#135559,#135560,#135561,#135562,#135563,
#135564,#135565,#135566,#135567,#135568,#135569,#135570,#135571,#135572,
#135573,#135574,#135575,#135576,#135577,#135578,#135579,#135580,#135581,
#135582,#135583,#135584,#135585,#135586,#135587,#135588,#135589,#135590,
#135591,#135592,#135593,#135594,#135595,#135596,#135597,#135598,#135599,
#135600,#135601,#135602,#135603,#135604,#135605,#135606,#135607,#135608,
#135609,#135610,#135611,#135612,#135613,#135614,#135615,#135616,#135617,
#135618,#135619,#135620,#135621,#135622,#135623,#135624,#135625,#135626),
 .UNSPECIFIED.,.F.,.F.,(4,3,3,3,3,3,3,3,3,3,3,3,3,3,3,3,3,3,3,3,3,3,3,3,
3,3,3,3,3,3,3,3,3,3,3,3,3,3,3,3,3,3,3,3,3,3,3,3,3,3,3,3,3,3,3,4),(7.5927484481567,
7.70848931082287,7.75804920753855,7.75808963442151,7.86752047919751,7.87930978495934,
7.99714701095087,8.11487440634642,8.23254119187242,8.35636860358536,8.47413868997202,
8.59198013199231,8.70078884284455,8.71001632278144,8.72781047661061,8.72785083872419,
8.83728642518644,8.84907098926203,8.96690551936438,9.08463022262083,9.20229432567408,
9.32612375501228,9.44389122085705,9.56173006773944,9.67053220577472,9.67976372019558,
9.69757165256406,9.69761204302688,9.80704288732126,9.81883219356472,9.9366641213659,
10.0543861697222,10.1720475710507,10.2958789901204,10.413643673577,10.5314797142669,
10.6402827589719,10.6495105488693,10.6673328569863,10.6673732473296,10.7768055714159,
10.7885933978674,10.9064273960726,11.0241515432087,11.1418150671119,11.265644913242,
11.383411749779,11.5012499509012,11.6100540546258,11.6192829392659,11.6370940679108,
11.6371344516323,11.7464312636471,11.7551568359126,11.8729941352346,11.9496359926862),
 .UNSPECIFIED.);
#23552=B_SPLINE_CURVE_WITH_KNOTS('',3,(#135627,#135628,#135629,#135630,
#135631,#135632,#135633,#135634,#135635,#135636,#135637,#135638,#135639,
#135640,#135641,#135642,#135643,#135644,#135645,#135646,#135647,#135648,
#135649,#135650,#135651,#135652,#135653,#135654,#135655,#135656,#135657,
#135658,#135659,#135660,#135661,#135662,#135663,#135664,#135665,#135666,
#135667,#135668,#135669,#135670,#135671,#135672,#135673,#135674,#135675,
#135676,#135677,#135678,#135679,#135680,#135681,#135682,#135683,#135684,
#135685,#135686,#135687,#135688,#135689,#135690,#135691,#135692,#135693,
#135694,#135695,#135696,#135697,#135698,#135699,#135700,#135701,#135702,
#135703,#135704,#135705,#135706,#135707,#135708,#135709,#135710,#135711,
#135712,#135713,#135714,#135715,#135716,#135717,#135718,#135719,#135720,
#135721,#135722,#135723,#135724,#135725,#135726,#135727,#135728,#135729,
#135730,#135731,#135732,#135733,#135734,#135735,#135736,#135737,#135738,
#135739,#135740,#135741,#135742,#135743,#135744,#135745,#135746,#135747,
#135748,#135749,#135750),.UNSPECIFIED.,.F.,.F.,(4,2,2,2,2,2,2,2,2,2,2,2,
2,2,2,2,2,2,2,2,2,2,2,2,2,2,2,2,2,2,2,2,2,2,2,2,2,2,2,2,2,2,2,2,2,2,2,2,
2,2,2,2,2,2,2,2,2,2,2,2,2,4),(-1.04064001717697,-1.03027141349264,-1.0173478683752,
-0.993383177184256,-0.985957107213174,-0.981054610570191,-0.973672075358925,
-0.963727412468284,-0.931041109103776,-0.922049514266625,-0.913099173519084,
-0.895464554635867,-0.870256799917985,-0.86291344632528,-0.85801155538961,
-0.85054911280665,-0.840436223537567,-0.808127266458275,-0.79911329869858,
-0.790169851509594,-0.772700593908835,-0.748480260777749,-0.740479819189106,
-0.73555036712696,-0.728595208219088,-0.719535862834643,-0.689428311189464,
-0.679207808539281,-0.670704191720385,-0.658644789437106,-0.625055523110738,
-0.617373530048558,-0.612479565454441,-0.605389999076659,-0.596042434022061,
-0.569689584841247,-0.55810877463022,-0.549686257406334,-0.53933660593639,
-0.527203875983819,-0.50322166815262,-0.494849075582067,-0.489911422424503,
-0.483248975275109,-0.461281902412592,-0.439891122091201,-0.43066811618859,
-0.421820971123292,-0.405920071611398,-0.376490662455969,-0.370021060472215,
-0.364920156106881,-0.355495588887186,-0.34045320617814,-0.317839437214019,
-0.308616145284517,-0.299638728241579,-0.282779212407393,-0.258916192866437,
-0.250058535195703,-0.245187517922973,-0.244113824073537),.UNSPECIFIED.);
#23553=B_SPLINE_CURVE_WITH_KNOTS('',3,(#135753,#135754,#135755,#135756,
#135757,#135758,#135759,#135760,#135761,#135762,#135763,#135764,#135765,
#135766,#135767,#135768,#135769,#135770,#135771,#135772,#135773,#135774,
#135775,#135776,#135777,#135778,#135779,#135780,#135781,#135782,#135783,
#135784,#135785,#135786,#135787,#135788,#135789,#135790,#135791,#135792,
#135793,#135794,#135795,#135796,#135797,#135798,#135799,#135800,#135801,
#135802,#135803,#135804,#135805,#135806,#135807,#135808,#135809,#135810,
#135811,#135812,#135813,#135814,#135815,#135816,#135817,#135818,#135819,
#135820,#135821,#135822,#135823,#135824,#135825),.UNSPECIFIED.,.F.,.F.,
(4,3,3,3,3,3,3,3,3,3,3,3,3,3,3,3,3,3,3,3,3,3,3,3,4),(5.66554986601471,5.77596453150268,
5.78359371610427,5.81852702174705,5.81856722581613,5.92802930197335,5.93978737635397,
6.0576357094371,6.17537450206838,6.29305295018594,6.41687182016916,6.53465407689312,
6.65250784703394,6.76130412196615,6.77055649293766,6.78828802954264,6.78832843011882,
6.8964818874404,6.90464479286087,7.02079954171015,7.13684506667047,7.25288918170985,
7.36892214952182,7.48510609168556,7.59274844756024),.UNSPECIFIED.);
#23554=B_SPLINE_CURVE_WITH_KNOTS('',3,(#135826,#135827,#135828,#135829,
#135830,#135831,#135832,#135833,#135834,#135835,#135836,#135837,#135838,
#135839,#135840,#135841,#135842,#135843,#135844,#135845,#135846,#135847,
#135848,#135849,#135850,#135851,#135852,#135853,#135854,#135855,#135856,
#135857,#135858,#135859,#135860,#135861,#135862,#135863,#135864,#135865,
#135866,#135867,#135868,#135869,#135870,#135871,#135872,#135873,#135874,
#135875,#135876,#135877,#135878,#135879,#135880,#135881,#135882,#135883,
#135884,#135885,#135886,#135887,#135888,#135889,#135890,#135891,#135892,
#135893,#135894,#135895,#135896,#135897,#135898,#135899,#135900,#135901,
#135902,#135903,#135904,#135905,#135906,#135907,#135908,#135909,#135910,
#135911,#135912,#135913,#135914,#135915,#135916,#135917,#135918,#135919,
#135920,#135921,#135922,#135923,#135924,#135925,#135926,#135927,#135928,
#135929,#135930,#135931,#135932,#135933,#135934,#135935,#135936,#135937,
#135938,#135939,#135940,#135941,#135942,#135943,#135944,#135945,#135946,
#135947,#135948,#135949,#135950,#135951,#135952,#135953,#135954,#135955,
#135956,#135957,#135958,#135959,#135960,#135961,#135962,#135963,#135964,
#135965,#135966,#135967,#135968,#135969,#135970,#135971,#135972,#135973,
#135974,#135975,#135976,#135977,#135978,#135979,#135980,#135981,#135982,
#135983,#135984,#135985,#135986,#135987,#135988,#135989,#135990,#135991),
 .UNSPECIFIED.,.F.,.F.,(4,3,3,3,3,3,3,3,3,3,3,3,3,3,3,3,3,3,3,3,3,3,3,3,
3,3,3,3,3,3,3,3,3,3,3,3,3,3,3,3,3,3,3,3,3,3,3,3,3,3,3,3,3,3,3,4),(7.59274844815668,
7.70848933226218,7.75804920252765,7.7580896344215,7.86752047552237,7.87930978495934,
7.99714699496723,8.11487437422409,8.23254114349144,8.35636856729962,8.47413863735006,
8.59198006303149,8.70078875715278,8.71001623760722,8.72781047141427,8.72785083872419,
8.83728641600613,8.84907098926203,8.96690551890705,9.08463022165414,9.20229432414697,
9.32612375386695,9.44389121902953,9.56173006518838,9.67053220806784,9.67976371686772,
9.6975716474907,9.69761204302688,9.80704289295715,9.81883219356472,9.93666412617729,
10.0543861794204,10.1720475857004,10.2958790011077,10.4136436896112,10.5314797353737,
10.6402827787652,10.6495105750451,10.6673328518942,10.6673732473296,10.7768055701125,
10.7885933978674,10.9064273934618,11.0241515379578,11.1418150591975,11.2656449073062,
11.3834117411574,11.5012499395899,11.6100540394642,11.6192829252808,11.6370940627961,
11.6371344516323,11.7464312623365,11.7551568362625,11.8729941358588,11.9496356025186),
 .UNSPECIFIED.);
#23555=B_SPLINE_CURVE_WITH_KNOTS('',3,(#135992,#135993,#135994,#135995,
#135996,#135997,#135998,#135999,#136000,#136001,#136002,#136003,#136004,
#136005,#136006,#136007,#136008,#136009,#136010,#136011,#136012,#136013,
#136014,#136015,#136016,#136017,#136018,#136019,#136020,#136021,#136022,
#136023,#136024,#136025,#136026,#136027,#136028,#136029,#136030,#136031,
#136032,#136033,#136034,#136035,#136036,#136037,#136038,#136039,#136040,
#136041,#136042,#136043,#136044,#136045,#136046,#136047,#136048,#136049,
#136050,#136051,#136052,#136053,#136054,#136055,#136056,#136057,#136058,
#136059,#136060,#136061,#136062,#136063,#136064,#136065,#136066,#136067,
#136068,#136069,#136070,#136071,#136072,#136073,#136074,#136075,#136076,
#136077,#136078,#136079,#136080,#136081,#136082,#136083,#136084,#136085,
#136086,#136087,#136088,#136089,#136090,#136091,#136092,#136093,#136094,
#136095,#136096,#136097,#136098,#136099,#136100,#136101,#136102,#136103,
#136104,#136105,#136106,#136107,#136108,#136109,#136110,#136111,#136112,
#136113,#136114,#136115),.UNSPECIFIED.,.F.,.F.,(4,2,2,2,2,2,2,2,2,2,2,2,
2,2,2,2,2,2,2,2,2,2,2,2,2,2,2,2,2,2,2,2,2,2,2,2,2,2,2,2,2,2,2,2,2,2,2,2,
2,2,2,2,2,2,2,2,2,2,2,2,2,4),(-1.04064761107749,-1.03667653359214,-1.02057252852155,
-0.9903553805898,-0.984358690916432,-0.979237994977344,-0.969036797980125,
-0.951517128197997,-0.931710771399382,-0.922578938958349,-0.913747451701676,
-0.897661246305512,-0.867498616782207,-0.861470377670638,-0.856362594494266,
-0.846294480025667,-0.829237260592109,-0.808850442624188,-0.799685899242007,
-0.790862380332336,-0.774944861212517,-0.745412546770826,-0.739002804337929,
-0.733993752195202,-0.72497767286612,-0.695095836313415,-0.682350248058098,
-0.673795801795949,-0.663890116730539,-0.652668140312166,-0.62480111204984,
-0.617288212082119,-0.612398318438083,-0.605161188422243,-0.595510337990656,
-0.569063629920645,-0.557792264867719,-0.549381259618363,-0.538805352598925,
-0.526220113176564,-0.502072016440112,-0.49438018345918,-0.489478824102436,
-0.482360419432393,-0.472978497189683,-0.44657915995887,-0.434969508366888,
-0.426469154547465,-0.415917996104292,-0.403435536234545,-0.379226701275057,
-0.37140085348607,-0.366413756853001,-0.359021254014121,-0.349080449971626,
-0.317055397661656,-0.30800989081409,-0.298869341415305,-0.279457361709301,
-0.253038691613122,-0.247188096201178,-0.244126851835458),.UNSPECIFIED.);
#23556=B_SPLINE_CURVE_WITH_KNOTS('',3,(#136240,#136241,#136242,#136243,
#136244,#136245,#136246,#136247,#136248,#136249,#136250,#136251,#136252,
#136253),.UNSPECIFIED.,.F.,.F.,(4,2,2,2,2,2,4),(1.58567647220938E-6,0.0466881077856908,
0.0920988348773926,0.143330833613337,0.192991558600317,0.240911899931117,
0.29038450507933),.UNSPECIFIED.);
#23557=B_SPLINE_CURVE_WITH_KNOTS('',3,(#136254,#136255,#136256,#136257,
#136258,#136259,#136260,#136261,#136262,#136263,#136264,#136265,#136266,
#136267,#136268,#136269,#136270,#136271,#136272,#136273,#136274,#136275,
#136276,#136277,#136278,#136279,#136280,#136281,#136282,#136283,#136284,
#136285,#136286,#136287,#136288,#136289,#136290,#136291,#136292,#136293,
#136294,#136295,#136296,#136297,#136298,#136299,#136300,#136301,#136302,
#136303,#136304,#136305,#136306,#136307,#136308,#136309,#136310,#136311,
#136312,#136313,#136314,#136315,#136316,#136317,#136318,#136319,#136320,
#136321,#136322,#136323,#136324,#136325,#136326,#136327,#136328,#136329,
#136330,#136331,#136332,#136333,#136334,#136335),.UNSPECIFIED.,.F.,.F.,
(4,3,3,3,3,3,3,3,3,3,3,3,3,3,3,3,3,3,3,3,3,3,3,3,3,3,3,4),(0.,0.0154790975076392,
0.0309581950152783,0.043346867455363,0.0480167577448785,0.052157240862597,
0.0686255293071033,0.085061105479412,0.0963127227435478,0.100794587159636,
0.104383686997236,0.12145541211408,0.130067574535955,0.146660502151626,
0.15583969909837,0.158551507968915,0.175605845203202,0.193054946625637,
0.204601396301158,0.210946851258842,0.215063043944209,0.233049916450152,
0.242953934326418,0.247562205886623,0.251095943169411,0.269300892692474,
0.272665987955216,0.285115833988478),.UNSPECIFIED.);
#23558=B_SPLINE_CURVE_WITH_KNOTS('',3,(#136460,#136461,#136462,#136463,
#136464,#136465,#136466,#136467,#136468,#136469,#136470,#136471,#136472,
#136473,#136474,#136475,#136476,#136477,#136478,#136479,#136480,#136481,
#136482,#136483,#136484,#136485,#136486,#136487,#136488,#136489,#136490,
#136491,#136492,#136493,#136494,#136495,#136496,#136497,#136498,#136499,
#136500,#136501,#136502,#136503,#136504,#136505,#136506,#136507,#136508,
#136509,#136510,#136511,#136512,#136513,#136514,#136515,#136516,#136517,
#136518,#136519,#136520,#136521,#136522,#136523,#136524,#136525,#136526,
#136527,#136528,#136529,#136530,#136531,#136532,#136533,#136534,#136535,
#136536,#136537,#136538,#136539,#136540,#136541),.UNSPECIFIED.,.F.,.F.,
(4,3,3,3,3,3,3,3,3,3,3,3,3,3,3,3,3,3,3,3,3,3,3,3,3,3,3,4),(0.,0.0154790634400372,
0.0309581268800745,0.0433468078370607,0.048016628498302,0.0521572525180448,
0.0684584781979448,0.0850610915406634,0.0963127122894887,0.10079456566722,
0.104383680276898,0.121455407850578,0.130067574535964,0.146660523123985,
0.155839744528338,0.158551576529395,0.175605937118379,0.193095393916,0.204601449529331,
0.21094683907126,0.215063044511372,0.233049918293188,0.2429539357087,0.247562235404507,
0.251095975207792,0.269300923802189,0.272665987955236,0.285115831934067),
 .UNSPECIFIED.);
#23559=B_SPLINE_CURVE_WITH_KNOTS('',3,(#136543,#136544,#136545,#136546),
 .UNSPECIFIED.,.F.,.F.,(4,4),(0.,0.00918658431906933),.UNSPECIFIED.);
#23560=B_SPLINE_CURVE_WITH_KNOTS('',3,(#136547,#136548,#136549,#136550,
#136551,#136552,#136553,#136554,#136555,#136556,#136557,#136558,#136559,
#136560,#136561,#136562,#136563,#136564,#136565,#136566,#136567,#136568,
#136569,#136570,#136571,#136572,#136573,#136574,#136575,#136576,#136577,
#136578,#136579,#136580,#136581,#136582,#136583,#136584,#136585,#136586,
#136587,#136588,#136589,#136590,#136591,#136592,#136593,#136594,#136595,
#136596,#136597,#136598,#136599,#136600,#136601,#136602,#136603,#136604,
#136605,#136606,#136607,#136608,#136609,#136610,#136611,#136612,#136613,
#136614,#136615,#136616,#136617,#136618,#136619,#136620,#136621,#136622,
#136623,#136624,#136625),.UNSPECIFIED.,.F.,.F.,(4,3,3,3,3,3,3,3,3,3,3,3,
3,3,3,3,3,3,3,3,3,3,3,3,3,3,4),(0.,0.0178509406758339,0.0360833708446063,
0.0497914557540533,0.0564440624232981,0.0594975215358368,0.0772253906875525,
0.0946647317535434,0.107092444205114,0.114964947860173,0.118088073305871,
0.134959943033528,0.144375581559826,0.160821883027944,0.168625126520761,
0.173118085073618,0.189888464885431,0.206622922460632,0.217641805290516,
0.223770976991618,0.22717570174071,0.243238325838015,0.252063979588582,
0.255940334406271,0.271478860666626,0.275945993304769,0.286347380332248),
 .UNSPECIFIED.);
#23561=B_SPLINE_CURVE_WITH_KNOTS('',3,(#136763,#136764,#136765,#136766,
#136767,#136768,#136769,#136770,#136771,#136772,#136773,#136774,#136775,
#136776),.UNSPECIFIED.,.F.,.F.,(4,2,2,2,2,2,4),(1.58595928405246E-6,0.0466880966579777,
0.0920988245562084,0.143330891570577,0.192991652192899,0.240911943591573,
0.290384482497107),.UNSPECIFIED.);
#23562=B_SPLINE_CURVE_WITH_KNOTS('',3,(#136777,#136778,#136779,#136780,
#136781,#136782,#136783,#136784,#136785,#136786,#136787,#136788,#136789,
#136790,#136791,#136792,#136793,#136794,#136795,#136796,#136797,#136798,
#136799,#136800,#136801,#136802,#136803,#136804,#136805,#136806,#136807,
#136808,#136809,#136810,#136811,#136812,#136813,#136814,#136815,#136816,
#136817,#136818,#136819,#136820,#136821,#136822,#136823,#136824,#136825,
#136826,#136827,#136828,#136829,#136830,#136831,#136832,#136833,#136834,
#136835,#136836,#136837,#136838,#136839,#136840,#136841,#136842,#136843,
#136844,#136845,#136846,#136847,#136848,#136849,#136850,#136851,#136852,
#136853,#136854,#136855,#136856,#136857,#136858),.UNSPECIFIED.,.F.,.F.,
(4,3,3,3,3,3,3,3,3,3,3,3,3,3,3,3,3,3,3,3,3,3,3,3,3,3,3,4),(0.,0.0151429849951974,
0.0309514432426294,0.0433468474135511,0.048016714296136,0.0521572447792291,
0.0684584883549305,0.0850611007943578,0.0963127192297611,0.100794579936147,
0.104383684737716,0.121455410665747,0.130067574535971,0.146660509203611,
0.155839714374814,0.15855153100884,0.17580325611013,0.19305498121142,0.204601414194011,
0.21094684716519,0.215063044140779,0.233049917075482,0.242953934795423,
0.247562215827255,0.25109595394491,0.269300903176924,0.272665987955243,
0.285115833302671),.UNSPECIFIED.);
#23563=B_SPLINE_CURVE_WITH_KNOTS('',3,(#136983,#136984,#136985,#136986,
#136987,#136988,#136989,#136990,#136991,#136992,#136993,#136994,#136995,
#136996,#136997,#136998,#136999,#137000,#137001,#137002,#137003,#137004,
#137005,#137006,#137007,#137008,#137009,#137010,#137011,#137012,#137013,
#137014,#137015,#137016,#137017,#137018,#137019,#137020,#137021,#137022,
#137023,#137024,#137025,#137026,#137027,#137028,#137029,#137030,#137031,
#137032,#137033,#137034,#137035,#137036,#137037,#137038,#137039,#137040,
#137041,#137042,#137043,#137044,#137045,#137046,#137047,#137048,#137049,
#137050,#137051,#137052,#137053,#137054,#137055,#137056,#137057,#137058,
#137059,#137060,#137061,#137062,#137063,#137064),.UNSPECIFIED.,.F.,.F.,
(4,3,3,3,3,3,3,3,3,3,3,3,3,3,3,3,3,3,3,3,3,3,3,3,3,3,3,4),(0.,0.0154790919518317,
0.0309581839036635,0.0433468577327002,0.0480167366668755,0.0521572427623293,
0.0686255280202576,0.0850611032056772,0.0963127210382473,0.100794583654536,
0.104383685901981,0.121455411399997,0.130067574535958,0.146660505573429,
0.155839706510775,0.158551519167426,0.175777335672888,0.193003152178349,
0.20460140499342,0.210946849266856,0.215063044035708,0.233049916749299,
0.242953934550777,0.247562210700648,0.251095948378327,0.26930089774997,
0.27266598795521,0.285115833656387),.UNSPECIFIED.);
#23564=B_SPLINE_CURVE_WITH_KNOTS('',3,(#137066,#137067,#137068,#137069),
 .UNSPECIFIED.,.F.,.F.,(4,4),(0.,0.00918599106546198),.UNSPECIFIED.);
#23565=B_SPLINE_CURVE_WITH_KNOTS('',3,(#137070,#137071,#137072,#137073,
#137074,#137075,#137076,#137077,#137078,#137079,#137080,#137081,#137082,
#137083,#137084,#137085,#137086,#137087,#137088,#137089,#137090,#137091,
#137092,#137093,#137094,#137095,#137096,#137097,#137098,#137099,#137100,
#137101,#137102,#137103,#137104,#137105,#137106,#137107,#137108,#137109,
#137110,#137111,#137112,#137113,#137114,#137115,#137116,#137117,#137118,
#137119,#137120,#137121,#137122,#137123,#137124,#137125,#137126,#137127,
#137128,#137129,#137130,#137131,#137132,#137133,#137134,#137135,#137136,
#137137,#137138,#137139,#137140,#137141,#137142,#137143,#137144,#137145),
 .UNSPECIFIED.,.F.,.F.,(4,3,3,3,3,3,3,3,3,3,3,3,3,3,3,3,3,3,3,3,3,3,3,3,
3,4),(0.,0.018046947694979,0.0362795627609177,0.049791457513174,0.0564440668188989,
0.0594975271731172,0.0772383217588031,0.0946647290647785,0.107092442188542,
0.114964949714838,0.11808807535994,0.134959936152474,0.144375581559832,
0.161646751661216,0.168625123295882,0.173118085365167,0.189917788602839,
0.206622922507054,0.223770964019213,0.227175695758215,0.243238311868422,
0.252063959651552,0.25594031760387,0.271478831695925,0.27594599330477,0.286347380332248),
 .UNSPECIFIED.);
#23566=B_SPLINE_CURVE_WITH_KNOTS('',3,(#137185,#137186,#137187,#137188),
 .UNSPECIFIED.,.F.,.F.,(4,4),(-1.89742724654025,-1.84562728381663),
 .UNSPECIFIED.);
#23567=B_SPLINE_CURVE_WITH_KNOTS('',3,(#137195,#137196,#137197,#137198),
 .UNSPECIFIED.,.F.,.F.,(4,4),(-1.94922720926386,-1.89742724654024),
 .UNSPECIFIED.);
#23568=B_SPLINE_CURVE_WITH_KNOTS('',3,(#137200,#137201,#137202,#137203),
 .UNSPECIFIED.,.F.,.F.,(4,4),(-1.89742724654023,-1.84562728381661),
 .UNSPECIFIED.);
#23569=B_SPLINE_CURVE_WITH_KNOTS('',3,(#137210,#137211,#137212,#137213),
 .UNSPECIFIED.,.F.,.F.,(4,4),(-1.94922720926387,-1.89742724654024),
 .UNSPECIFIED.);
#23570=B_SPLINE_CURVE_WITH_KNOTS('',3,(#137383,#137384,#137385,#137386,
#137387,#137388),.UNSPECIFIED.,.F.,.F.,(4,1,1,4),(0.,0.285714285714286,
0.571428571428571,1.),.UNSPECIFIED.);
#23571=B_SPLINE_CURVE_WITH_KNOTS('',3,(#137392,#137393,#137394,#137395,
#137396,#137397),.UNSPECIFIED.,.F.,.F.,(4,2,4),(0.,0.483208689475554,1.),
 .UNSPECIFIED.);
#23572=B_SPLINE_CURVE_WITH_KNOTS('',3,(#137405,#137406,#137407,#137408,
#137409,#137410),.UNSPECIFIED.,.F.,.F.,(4,1,1,4),(0.,0.285714285714286,
0.571428571428571,1.),.UNSPECIFIED.);
#23573=B_SPLINE_CURVE_WITH_KNOTS('',3,(#137414,#137415,#137416,#137417,
#137418,#137419),.UNSPECIFIED.,.F.,.F.,(4,2,4),(0.,0.483208689475554,1.),
 .UNSPECIFIED.);
#23574=B_SPLINE_CURVE_WITH_KNOTS('',3,(#137427,#137428,#137429,#137430,
#137431,#137432),.UNSPECIFIED.,.F.,.F.,(4,1,1,4),(0.,0.285714285714286,
0.571428571428571,1.),.UNSPECIFIED.);
#23575=B_SPLINE_CURVE_WITH_KNOTS('',3,(#137436,#137437,#137438,#137439,
#137440,#137441),.UNSPECIFIED.,.F.,.F.,(4,2,4),(0.,0.483208689475554,1.),
 .UNSPECIFIED.);
#23576=B_SPLINE_CURVE_WITH_KNOTS('',3,(#137449,#137450,#137451,#137452,
#137453,#137454),.UNSPECIFIED.,.F.,.F.,(4,1,1,4),(0.,0.285714285714286,
0.571428571428571,1.),.UNSPECIFIED.);
#23577=B_SPLINE_CURVE_WITH_KNOTS('',3,(#137458,#137459,#137460,#137461,
#137462,#137463),.UNSPECIFIED.,.F.,.F.,(4,2,4),(0.,0.483208689475554,1.),
 .UNSPECIFIED.);
#23578=B_SPLINE_CURVE_WITH_KNOTS('',3,(#137471,#137472,#137473,#137474,
#137475,#137476),.UNSPECIFIED.,.F.,.F.,(4,1,1,4),(0.,0.285714285714286,
0.571428571428571,1.),.UNSPECIFIED.);
#23579=B_SPLINE_CURVE_WITH_KNOTS('',3,(#137480,#137481,#137482,#137483,
#137484,#137485),.UNSPECIFIED.,.F.,.F.,(4,2,4),(0.,0.483208689475554,1.),
 .UNSPECIFIED.);
#23580=B_SPLINE_CURVE_WITH_KNOTS('',3,(#137493,#137494,#137495,#137496,
#137497,#137498),.UNSPECIFIED.,.F.,.F.,(4,1,1,4),(0.,0.285714285714286,
0.571428571428571,1.),.UNSPECIFIED.);
#23581=B_SPLINE_CURVE_WITH_KNOTS('',3,(#137502,#137503,#137504,#137505,
#137506,#137507),.UNSPECIFIED.,.F.,.F.,(4,2,4),(0.,0.483208689475554,1.),
 .UNSPECIFIED.);
#23582=B_SPLINE_CURVE_WITH_KNOTS('',3,(#137515,#137516,#137517,#137518,
#137519,#137520),.UNSPECIFIED.,.F.,.F.,(4,1,1,4),(0.,0.285714285714286,
0.571428571428571,1.),.UNSPECIFIED.);
#23583=B_SPLINE_CURVE_WITH_KNOTS('',3,(#137524,#137525,#137526,#137527,
#137528,#137529),.UNSPECIFIED.,.F.,.F.,(4,2,4),(0.,0.483208689475554,1.),
 .UNSPECIFIED.);
#23584=B_SPLINE_CURVE_WITH_KNOTS('',3,(#137537,#137538,#137539,#137540,
#137541,#137542),.UNSPECIFIED.,.F.,.F.,(4,1,1,4),(0.,0.285714285714286,
0.571428571428571,1.),.UNSPECIFIED.);
#23585=B_SPLINE_CURVE_WITH_KNOTS('',3,(#137546,#137547,#137548,#137549,
#137550,#137551),.UNSPECIFIED.,.F.,.F.,(4,2,4),(0.,0.483208689475554,1.),
 .UNSPECIFIED.);
#23586=B_SPLINE_CURVE_WITH_KNOTS('',3,(#137559,#137560,#137561,#137562,
#137563,#137564),.UNSPECIFIED.,.F.,.F.,(4,1,1,4),(0.,0.285714285714286,
0.571428571428571,1.),.UNSPECIFIED.);
#23587=B_SPLINE_CURVE_WITH_KNOTS('',3,(#137568,#137569,#137570,#137571,
#137572,#137573),.UNSPECIFIED.,.F.,.F.,(4,2,4),(0.,0.483208689475554,1.),
 .UNSPECIFIED.);
#23588=B_SPLINE_CURVE_WITH_KNOTS('',3,(#137581,#137582,#137583,#137584,
#137585,#137586),.UNSPECIFIED.,.F.,.F.,(4,1,1,4),(0.,0.285714285714286,
0.571428571428571,1.),.UNSPECIFIED.);
#23589=B_SPLINE_CURVE_WITH_KNOTS('',3,(#137590,#137591,#137592,#137593,
#137594,#137595),.UNSPECIFIED.,.F.,.F.,(4,2,4),(0.,0.483208689475554,1.),
 .UNSPECIFIED.);
#23590=B_SPLINE_CURVE_WITH_KNOTS('',3,(#137605,#137606,#137607,#137608,
#137609,#137610),.UNSPECIFIED.,.F.,.F.,(4,2,4),(0.,0.483208689475554,1.),
 .UNSPECIFIED.);
#23591=B_SPLINE_CURVE_WITH_KNOTS('',3,(#137614,#137615,#137616,#137617,
#137618,#137619),.UNSPECIFIED.,.F.,.F.,(4,1,1,4),(0.,0.285714285714286,
0.571428571428571,1.),.UNSPECIFIED.);
#23592=B_SPLINE_CURVE_WITH_KNOTS('',3,(#137627,#137628,#137629,#137630,
#137631,#137632),.UNSPECIFIED.,.F.,.F.,(4,2,4),(0.,0.483208689475554,1.),
 .UNSPECIFIED.);
#23593=B_SPLINE_CURVE_WITH_KNOTS('',3,(#137636,#137637,#137638,#137639,
#137640,#137641),.UNSPECIFIED.,.F.,.F.,(4,1,1,4),(0.,0.285714285714286,
0.571428571428571,1.),.UNSPECIFIED.);
#23594=B_SPLINE_CURVE_WITH_KNOTS('',3,(#137649,#137650,#137651,#137652,
#137653,#137654),.UNSPECIFIED.,.F.,.F.,(4,2,4),(0.,0.483208689475554,1.),
 .UNSPECIFIED.);
#23595=B_SPLINE_CURVE_WITH_KNOTS('',3,(#137658,#137659,#137660,#137661,
#137662,#137663),.UNSPECIFIED.,.F.,.F.,(4,1,1,4),(0.,0.285714285714286,
0.571428571428571,1.),.UNSPECIFIED.);
#23596=B_SPLINE_CURVE_WITH_KNOTS('',3,(#137671,#137672,#137673,#137674,
#137675,#137676),.UNSPECIFIED.,.F.,.F.,(4,2,4),(0.,0.483208689475554,1.),
 .UNSPECIFIED.);
#23597=B_SPLINE_CURVE_WITH_KNOTS('',3,(#137680,#137681,#137682,#137683,
#137684,#137685),.UNSPECIFIED.,.F.,.F.,(4,1,1,4),(0.,0.285714285714286,
0.571428571428571,1.),.UNSPECIFIED.);
#23598=B_SPLINE_CURVE_WITH_KNOTS('',3,(#137693,#137694,#137695,#137696,
#137697,#137698),.UNSPECIFIED.,.F.,.F.,(4,2,4),(0.,0.483208689475554,1.),
 .UNSPECIFIED.);
#23599=B_SPLINE_CURVE_WITH_KNOTS('',3,(#137702,#137703,#137704,#137705,
#137706,#137707),.UNSPECIFIED.,.F.,.F.,(4,1,1,4),(0.,0.285714285714286,
0.571428571428571,1.),.UNSPECIFIED.);
#23600=B_SPLINE_CURVE_WITH_KNOTS('',3,(#137715,#137716,#137717,#137718,
#137719,#137720),.UNSPECIFIED.,.F.,.F.,(4,2,4),(0.,0.483208689475554,1.),
 .UNSPECIFIED.);
#23601=B_SPLINE_CURVE_WITH_KNOTS('',3,(#137724,#137725,#137726,#137727,
#137728,#137729),.UNSPECIFIED.,.F.,.F.,(4,1,1,4),(0.,0.285714285714286,
0.571428571428571,1.),.UNSPECIFIED.);
#23602=B_SPLINE_CURVE_WITH_KNOTS('',3,(#137737,#137738,#137739,#137740,
#137741,#137742),.UNSPECIFIED.,.F.,.F.,(4,2,4),(0.,0.483208689475554,1.),
 .UNSPECIFIED.);
#23603=B_SPLINE_CURVE_WITH_KNOTS('',3,(#137746,#137747,#137748,#137749,
#137750,#137751),.UNSPECIFIED.,.F.,.F.,(4,1,1,4),(0.,0.285714285714286,
0.571428571428571,1.),.UNSPECIFIED.);
#23604=B_SPLINE_CURVE_WITH_KNOTS('',3,(#137759,#137760,#137761,#137762,
#137763,#137764),.UNSPECIFIED.,.F.,.F.,(4,2,4),(0.,0.483208689475554,1.),
 .UNSPECIFIED.);
#23605=B_SPLINE_CURVE_WITH_KNOTS('',3,(#137768,#137769,#137770,#137771,
#137772,#137773),.UNSPECIFIED.,.F.,.F.,(4,1,1,4),(0.,0.285714285714286,
0.571428571428571,1.),.UNSPECIFIED.);
#23606=B_SPLINE_CURVE_WITH_KNOTS('',3,(#137781,#137782,#137783,#137784,
#137785,#137786),.UNSPECIFIED.,.F.,.F.,(4,2,4),(0.,0.483208689475554,1.),
 .UNSPECIFIED.);
#23607=B_SPLINE_CURVE_WITH_KNOTS('',3,(#137790,#137791,#137792,#137793,
#137794,#137795),.UNSPECIFIED.,.F.,.F.,(4,1,1,4),(0.,0.285714285714286,
0.571428571428571,1.),.UNSPECIFIED.);
#23608=B_SPLINE_CURVE_WITH_KNOTS('',3,(#137803,#137804,#137805,#137806,
#137807,#137808),.UNSPECIFIED.,.F.,.F.,(4,2,4),(0.,0.483208689475554,1.),
 .UNSPECIFIED.);
#23609=B_SPLINE_CURVE_WITH_KNOTS('',3,(#137812,#137813,#137814,#137815,
#137816,#137817),.UNSPECIFIED.,.F.,.F.,(4,1,1,4),(0.,0.285714285714286,
0.571428571428571,1.),.UNSPECIFIED.);
#23610=B_SPLINE_CURVE_WITH_KNOTS('',3,(#138846,#138847,#138848,#138849,
#138850,#138851,#138852),.UNSPECIFIED.,.F.,.F.,(4,1,1,1,4),(0.,0.0576772753326012,
0.115354550665202,0.173031825997804,0.403740927328209),.UNSPECIFIED.);
#23611=B_SPLINE_CURVE_WITH_KNOTS('',3,(#140166,#140167,#140168,#140169,
#140170,#140171,#140172,#140173,#140174,#140175,#140176,#140177,#140178,
#140179,#140180,#140181,#140182,#140183,#140184,#140185,#140186,#140187,
#140188,#140189,#140190,#140191,#140192,#140193,#140194,#140195,#140196),
 .UNSPECIFIED.,.F.,.F.,(4,3,3,3,3,3,3,3,3,3,4),(0.,0.00461311763943398,
0.0108962108513953,0.0174429809772217,0.0241024188265093,0.025565721040406,
0.0266315692284618,0.0334300723314571,0.0405906131676447,0.0477511540038322,
0.0479851889522872),.UNSPECIFIED.);
#23612=B_SPLINE_CURVE_WITH_KNOTS('',3,(#140198,#140199,#140200,#140201,
#140202,#140203,#140204,#140205,#140206),.UNSPECIFIED.,.F.,.F.,(4,1,1,1,
1,1,4),(0.461365642517441,0.594297668650691,0.72722969478394,0.793695707850564,
0.860161720917189,0.893394727450501,0.926627733983813),.UNSPECIFIED.);
#23613=B_SPLINE_CURVE_WITH_KNOTS('',3,(#140209,#140210,#140211,#140212,
#140213,#140214,#140215,#140216,#140217),.UNSPECIFIED.,.F.,.F.,(4,1,1,1,
1,1,4),(-0.926627733983813,-0.893394727450501,-0.860161720917189,-0.793695707850564,
-0.72722969478394,-0.594297668650691,-0.500154675194955),.UNSPECIFIED.);
#23614=B_SPLINE_CURVE_WITH_KNOTS('',3,(#140244,#140245,#140246,#140247,
#140248,#140249),.UNSPECIFIED.,.F.,.F.,(4,1,1,4),(-0.0834766168470346,-0.0596261548907622,
-0.0357756929344898,-8.11743420200643E-14),.UNSPECIFIED.);
#23615=B_SPLINE_CURVE_WITH_KNOTS('',3,(#140250,#140251,#140252,#140253,
#140254,#140255),.UNSPECIFIED.,.F.,.F.,(4,1,1,4),(8.11743420200643E-14,
0.0357756929344898,0.0596261548907622,0.0834766168470346),.UNSPECIFIED.);
#23616=B_SPLINE_CURVE_WITH_KNOTS('',3,(#140292,#140293,#140294,#140295,
#140296,#140297,#140298,#140299,#140300,#140301,#140302,#140303,#140304,
#140305,#140306,#140307,#140308,#140309,#140310,#140311,#140312,#140313,
#140314,#140315,#140316,#140317,#140318,#140319),.UNSPECIFIED.,.F.,.F.,
(4,3,3,3,3,3,3,3,3,4),(-0.000214859095644161,0.,0.00693142052454231,0.0137691687551713,
0.0194026267134537,0.0225967132655498,0.0291207852027703,0.0354961538326274,
0.0414739990602825,0.0439088685276748),.UNSPECIFIED.);
#23617=B_SPLINE_CURVE_WITH_KNOTS('',3,(#140320,#140321,#140322,#140323,
#140324,#140325,#140326),.UNSPECIFIED.,.F.,.F.,(4,1,1,1,4),(-0.368376389772111,
-0.173031825997804,-0.115354550665202,-0.0576772753326012,0.),
 .UNSPECIFIED.);
#23618=B_SPLINE_CURVE_WITH_KNOTS('',3,(#140341,#140342,#140343,#140344,
#140345,#140346),.UNSPECIFIED.,.F.,.F.,(4,2,4),(2.16893938526046,2.18932185224566,
2.29478437652477),.UNSPECIFIED.);
#23619=B_SPLINE_CURVE_WITH_KNOTS('',3,(#140350,#140351,#140352,#140353,
#140354,#140355,#140356),.UNSPECIFIED.,.F.,.F.,(4,3,4),(1.53576065525224,
1.55048490763555,1.65559071935948),.UNSPECIFIED.);
#23620=B_SPLINE_CURVE_WITH_KNOTS('',3,(#140372,#140373,#140374,#140375,
#140376,#140377),.UNSPECIFIED.,.F.,.F.,(4,2,4),(0.341286253546736,0.361143619795883,
0.363320956651565),.UNSPECIFIED.);
#23621=B_SPLINE_CURVE_WITH_KNOTS('',3,(#140378,#140379,#140380,#140381,
#140382,#140383),.UNSPECIFIED.,.F.,.F.,(4,2,4),(0.313750555620341,0.321428887297588,
0.341286253546736),.UNSPECIFIED.);
#23622=B_SPLINE_CURVE_WITH_KNOTS('',3,(#140980,#140981,#140982,#140983,
#140984,#140985,#140986,#140987,#140988,#140989),.UNSPECIFIED.,.F.,.F.,
(4,2,2,2,4),(1.67380554977791,1.72330946760875,1.82115803507338,1.91900660253801,
1.92968955045032),.UNSPECIFIED.);
#23623=B_SPLINE_CURVE_WITH_KNOTS('',3,(#140991,#140992,#140993,#140994,
#140995,#140996,#140997,#140998),.UNSPECIFIED.,.F.,.F.,(4,2,2,4),(1.16203916326871,
1.24446130754331,1.33480896870603,1.33871262848189),.UNSPECIFIED.);
#23624=B_SPLINE_CURVE_WITH_KNOTS('',3,(#141202,#141203,#141204,#141205,
#141206,#141207,#141208,#141209,#141210,#141211,#141212,#141213,#141214,
#141215),.UNSPECIFIED.,.F.,.F.,(4,2,2,2,2,2,4),(-0.0644438520828007,-0.049420098065367,
-0.0340805324627365,-0.0180381900027908,-0.00905381728536003,0.,0.000302476647115217),
 .UNSPECIFIED.);
#23625=B_SPLINE_CURVE_WITH_KNOTS('',3,(#141224,#141225,#141226,#141227,
#141228,#141229,#141230,#141231,#141232,#141233,#141234,#141235,#141236,
#141237),.UNSPECIFIED.,.F.,.F.,(4,2,2,2,2,2,4),(-0.0645192623114328,-0.0495220659688513,
-0.034197838940368,-0.0181427477062707,-0.00910662411509301,0.,0.000307206838262488),
 .UNSPECIFIED.);
#23626=B_SPLINE_CURVE_WITH_KNOTS('',3,(#141255,#141256,#141257,#141258,
#141259,#141260,#141261,#141262,#141263,#141264,#141265,#141266,#141267,
#141268),.UNSPECIFIED.,.F.,.F.,(4,2,2,2,2,2,4),(-0.076933286852498,-0.0656628947840389,
-0.0527777497222598,-0.0355412965898649,-0.0182549906540077,0.,0.000407112356477986),
 .UNSPECIFIED.);
#23627=B_SPLINE_CURVE_WITH_KNOTS('',3,(#141277,#141278,#141279,#141280,
#141281,#141282,#141283,#141284,#141285,#141286,#141287,#141288,#141289,
#141290,#141291,#141292),.UNSPECIFIED.,.F.,.F.,(4,2,2,2,2,2,2,4),(-0.17484883404941,
-0.17438352547713,-0.154057828687025,-0.134514112676025,-0.113669604374028,
-0.0979724065437587,-0.0842463799815946,-0.0840619732027956),
 .UNSPECIFIED.);
#23628=B_SPLINE_CURVE_WITH_KNOTS('',3,(#141318,#141319,#141320,#141321,
#141322,#141323,#141324,#141325,#141326,#141327,#141328,#141329),
 .UNSPECIFIED.,.F.,.F.,(4,2,2,2,2,4),(-0.000388459955655831,0.,0.0324366524825953,
0.0672148594225315,0.0883338786734475,0.0887070234931564),.UNSPECIFIED.);
#23629=B_SPLINE_CURVE_WITH_KNOTS('',3,(#141336,#141337,#141338,#141339,
#141340,#141341,#141342,#141343),.UNSPECIFIED.,.F.,.F.,(4,2,2,4),(0.209727352355126,
0.221639359053507,0.227267824689401,0.231641458293049),.UNSPECIFIED.);
#23630=B_SPLINE_CURVE_WITH_KNOTS('',3,(#141367,#141368,#141369,#141370,
#141371,#141372),.UNSPECIFIED.,.F.,.F.,(4,2,4),(-0.085422632899438,-0.0599779172305395,
-0.00660946384348909),.UNSPECIFIED.);
#23631=B_SPLINE_CURVE_WITH_KNOTS('',3,(#141376,#141377,#141378,#141379,
#141380,#141381,#141382,#141383,#141384,#141385,#141386,#141387,#141388,
#141389),.UNSPECIFIED.,.F.,.F.,(4,2,2,2,2,2,4),(0.000112134656694737,0.0132030014333664,
0.0271656495376335,0.0434063776045854,0.0557452168635409,0.0681403897390113,
0.0684503648574364),.UNSPECIFIED.);
#23632=B_SPLINE_CURVE_WITH_KNOTS('',3,(#141393,#141394,#141395,#141396,
#141397,#141398),.UNSPECIFIED.,.F.,.F.,(4,2,4),(0.0919390414530091,0.15020057139645,
0.150889093198151),.UNSPECIFIED.);
#23633=B_SPLINE_CURVE_WITH_KNOTS('',3,(#141403,#141404,#141405,#141406),
 .UNSPECIFIED.,.F.,.F.,(4,4),(0.324870734299899,0.389015211548213),
 .UNSPECIFIED.);
#23634=B_SPLINE_CURVE_WITH_KNOTS('',3,(#141410,#141411,#141412,#141413),
 .UNSPECIFIED.,.F.,.F.,(4,4),(1.82536907488932,1.86305287236042),
 .UNSPECIFIED.);
#23635=B_SPLINE_CURVE_WITH_KNOTS('',3,(#141421,#141422,#141423,#141424,
#141425,#141426),.UNSPECIFIED.,.F.,.F.,(4,2,4),(0.746025828133808,0.777852575214063,
0.79046455586539),.UNSPECIFIED.);
#23636=B_SPLINE_CURVE_WITH_KNOTS('',3,(#141428,#141429,#141430,#141431,
#141432,#141433),.UNSPECIFIED.,.F.,.F.,(4,2,4),(0.303437751782123,0.312479563833371,
0.470690179622201),.UNSPECIFIED.);
#23637=B_SPLINE_CURVE_WITH_KNOTS('',3,(#141435,#141436,#141437,#141438,
#141439,#141440,#141441,#141442,#141443,#141444,#141445,#141446,#141447,
#141448),.UNSPECIFIED.,.F.,.F.,(4,2,2,2,2,2,4),(1.16336684881612,1.24052856460303,
1.33090755793504,1.42128655126704,1.51166554459905,1.60204453793105,1.67920625371796),
 .UNSPECIFIED.);
#23638=B_SPLINE_CURVE_WITH_KNOTS('',3,(#141450,#141451,#141452,#141453),
 .UNSPECIFIED.,.F.,.F.,(4,4),(1.24043822694661,1.24960607382757),
 .UNSPECIFIED.);
#23639=B_SPLINE_CURVE_WITH_KNOTS('',3,(#141458,#141459,#141460,#141461,
#141462,#141463,#141464,#141465,#141466,#141467,#141468,#141469),
 .UNSPECIFIED.,.F.,.F.,(4,2,2,2,2,4),(0.10066778259603,0.120892907264577,
0.141118031933124,0.171226798562592,0.201335565192059,0.222479033048159),
 .UNSPECIFIED.);
#23640=B_SPLINE_CURVE_WITH_KNOTS('',3,(#141476,#141477,#141478,#141479,
#141480,#141481,#141482,#141483,#141484,#141485,#141486,#141487,#141488,
#141489,#141490),.UNSPECIFIED.,.F.,.F.,(4,2,2,3,2,2,4),(1.95413674175165,
1.9749623939079,2.06883224877398,2.18440456807724,2.27009756469335,2.3998891015239,
2.43069177712689),.UNSPECIFIED.);
#23641=B_SPLINE_CURVE_WITH_KNOTS('',3,(#141492,#141493,#141494,#141495,
#141496,#141497,#141498,#141499,#141500,#141501,#141502,#141503,#141504,
#141505,#141506),.UNSPECIFIED.,.F.,.F.,(4,2,2,3,2,2,4),(0.132343968988449,
0.206008897163555,0.279486022780957,0.290162010211257,0.448048634858984,
0.517599926787915,0.527299151805233),.UNSPECIFIED.);
#23642=B_SPLINE_CURVE_WITH_KNOTS('',3,(#141536,#141537,#141538,#141539,
#141540,#141541,#141542,#141543),.UNSPECIFIED.,.F.,.F.,(4,2,2,4),(-0.117541017236412,
-0.105671481013589,-0.0875214169518554,-0.0677213667893671),
 .UNSPECIFIED.);
#23643=B_SPLINE_CURVE_WITH_KNOTS('',3,(#141578,#141579,#141580,#141581,
#141582,#141583,#141584,#141585,#141586,#141587,#141588,#141589,#141590,
#141591),.UNSPECIFIED.,.F.,.F.,(4,2,2,2,2,2,4),(0.18312537356055,0.188512137502322,
0.20364370582247,0.220110749285725,0.236577792748981,0.260891780441132,
0.285205768133283),.UNSPECIFIED.);
#23644=B_SPLINE_CURVE_WITH_KNOTS('',3,(#141646,#141647,#141648,#141649,
#141650,#141651,#141652,#141653,#141654,#141655,#141656,#141657,#141658,
#141659,#141660,#141661),.UNSPECIFIED.,.F.,.F.,(4,2,2,2,2,2,2,4),(-0.000477658155061879,
0.,0.0247302092914747,0.0480741684085018,0.0685297927666644,0.0821332220389815,
0.0925411876291308,0.0950579615863738),.UNSPECIFIED.);
#23645=B_SPLINE_CURVE_WITH_KNOTS('',3,(#141733,#141734,#141735,#141736,
#141737,#141738,#141739,#141740,#141741,#141742),.UNSPECIFIED.,.F.,.F.,
(4,2,2,2,4),(0.13732942536332,0.150614929788285,0.166747654183265,0.186151203326564,
0.207424187379634),.UNSPECIFIED.);
#23646=B_SPLINE_CURVE_WITH_KNOTS('',3,(#141751,#141752,#141753,#141754),
 .UNSPECIFIED.,.F.,.F.,(4,4),(0.142599130795278,0.144346706380812),
 .UNSPECIFIED.);
#23647=B_SPLINE_CURVE_WITH_KNOTS('',3,(#141758,#141759,#141760,#141761),
 .UNSPECIFIED.,.F.,.F.,(4,4),(0.00025811192102492,0.00165664283540655),
 .UNSPECIFIED.);
#23648=B_SPLINE_CURVE_WITH_KNOTS('',3,(#141763,#141764,#141765,#141766,
#141767,#141768,#141769,#141770,#141771,#141772,#141773,#141774,#141775,
#141776),.UNSPECIFIED.,.F.,.F.,(4,2,2,2,2,2,4),(-0.000346312484341596,0.,
0.0150312784786187,0.0297106940471177,0.0467215668210816,0.0602423017367392,
0.0722722728378001),.UNSPECIFIED.);
#23649=B_SPLINE_CURVE_WITH_KNOTS('',3,(#141780,#141781,#141782,#141783,
#141784,#141785,#141786,#141787),.UNSPECIFIED.,.F.,.F.,(4,2,2,4),(0.0136627898201133,
0.125132828407067,0.152540787048518,0.156243805314172),.UNSPECIFIED.);
#23650=B_SPLINE_CURVE_WITH_KNOTS('',3,(#141789,#141790,#141791,#141792,
#141793,#141794,#141795,#141796),.UNSPECIFIED.,.F.,.F.,(4,2,2,4),(0.00660661411091279,
0.14470344735553,0.251350868103014,0.347057593360392),.UNSPECIFIED.);
#23651=B_SPLINE_CURVE_WITH_KNOTS('',3,(#141797,#141798,#141799,#141800,
#141801,#141802,#141803,#141804,#141805,#141806,#141807,#141808,#141809,
#141810),.UNSPECIFIED.,.F.,.F.,(4,2,2,2,2,2,4),(-0.107017806276282,-0.0978369539163657,
-0.0882519488889954,-0.0704169759838092,-0.0478776048900307,-0.0237745956474009,
-0.0129771129663482),.UNSPECIFIED.);
#23652=B_SPLINE_CURVE_WITH_KNOTS('',3,(#141904,#141905,#141906,#141907,
#141908,#141909,#141910,#141911,#141912),.UNSPECIFIED.,.F.,.F.,(4,2,3,4),
(0.828293167562194,0.869881225451604,0.954778354838245,0.973139317003065),
 .UNSPECIFIED.);
#23653=B_SPLINE_CURVE_WITH_KNOTS('',3,(#141946,#141947,#141948,#141949,
#141950,#141951,#141952,#141953,#141954,#141955,#141956,#141957,#141958,
#141959,#141960,#141961,#141962,#141963,#141964,#141965,#141966,#141967,
#141968,#141969,#141970),.UNSPECIFIED.,.F.,.F.,(4,2,2,2,2,2,2,2,2,2,3,4),
(1.15977853242372,1.20026581496982,1.28836339099528,1.37646096702074,1.45628348069954,
1.53610599437834,1.61592850805714,1.69575102173595,1.78384859776141,1.87194617378687,
2.04246365813963,2.06103131106925),.UNSPECIFIED.);
#23654=B_SPLINE_CURVE_WITH_KNOTS('',3,(#141982,#141983,#141984,#141985,
#141986,#141987),.UNSPECIFIED.,.F.,.F.,(4,2,4),(0.,0.0366955352357751,0.0584007125994646),
 .UNSPECIFIED.);
#23655=B_SPLINE_CURVE_WITH_KNOTS('',3,(#141989,#141990,#141991,#141992,
#141993,#141994,#141995,#141996,#141997,#141998,#141999,#142000,#142001,
#142002,#142003,#142004,#142005,#142006,#142007,#142008,#142009,#142010,
#142011,#142012),.UNSPECIFIED.,.F.,.F.,(4,2,2,2,2,2,2,2,2,2,2,4),(0.603586482438603,
0.690548157104178,0.7776775531107,0.814909478184255,0.841789702690823,0.855229814944108,
0.868669927197392,0.882110039450676,0.89555015170396,0.922430376210528,
0.959662301284084,0.988423011761695),.UNSPECIFIED.);
#23656=B_SPLINE_CURVE_WITH_KNOTS('',3,(#142014,#142015,#142016,#142017,
#142018,#142019,#142020,#142021,#142022,#142023,#142024,#142025,#142026),
 .UNSPECIFIED.,.F.,.F.,(4,3,3,3,4),(0.,0.00510825104781711,0.00881483564204352,
0.0138582618694087,0.0184324970853374),.UNSPECIFIED.);
#23657=B_SPLINE_CURVE_WITH_KNOTS('',3,(#142451,#142452,#142453,#142454,
#142455,#142456,#142457,#142458,#142459,#142460,#142461,#142462,#142463),
 .UNSPECIFIED.,.F.,.F.,(4,3,3,3,4),(0.,0.00495757901231158,0.00803114212030837,
0.0131782094120615,0.0156274267007913),.UNSPECIFIED.);
#23658=B_SPLINE_CURVE_WITH_KNOTS('',3,(#142465,#142466,#142467,#142468,
#142469,#142470,#142471,#142472,#142473,#142474,#142475,#142476,#142477,
#142478,#142479,#142480,#142481,#142482,#142483,#142484,#142485,#142486,
#142487,#142488,#142489,#142490,#142491,#142492),.UNSPECIFIED.,.F.,.F.,
(4,2,2,2,2,3,2,2,2,2,3,2,4),(1.57820587984966,1.64634748030809,1.68357940538165,
1.71045962988822,1.7238997421415,1.73733985439478,1.75515538094126,1.77739368952689,
1.81480798197786,1.90628850472617,1.92355226704702,1.99122268110966,2.03565025170069),
 .UNSPECIFIED.);
#23659=B_SPLINE_CURVE_WITH_KNOTS('',3,(#142494,#142495,#142496,#142497,
#142498,#142499,#142500,#142501,#142502,#142503,#142504,#142505,#142506,
#142507,#142508,#142509,#142510,#142511,#142512,#142513,#142514,#142515,
#142516,#142517,#142518),.UNSPECIFIED.,.F.,.F.,(4,3,3,3,3,3,3,3,4),(0.,
0.00579507786607313,0.00734016029473464,0.0138775194884377,0.0157142860932645,
0.0230358256114078,0.0255587459307486,0.0326896693983427,0.0375637041363583),
 .UNSPECIFIED.);
#23660=B_SPLINE_CURVE_WITH_KNOTS('',3,(#142541,#142542,#142543,#142544,
#142545,#142546,#142547,#142548,#142549,#142550,#142551,#142552,#142553,
#142554),.UNSPECIFIED.,.F.,.F.,(4,2,2,2,2,2,4),(-0.0758814738778919,-0.0645512346483667,
-0.0515933744670232,-0.0342983873642865,-0.0175181259639588,0.,0.000393270258763866),
 .UNSPECIFIED.);
#23661=B_SPLINE_CURVE_WITH_KNOTS('',3,(#142610,#142611,#142612,#142613),
 .UNSPECIFIED.,.F.,.F.,(4,4),(0.239784037589408,0.24117260623475),
 .UNSPECIFIED.);
#23662=B_SPLINE_CURVE_WITH_KNOTS('',3,(#142639,#142640,#142641,#142642,
#142643,#142644,#142645,#142646,#142647,#142648,#142649,#142650,#142651,
#142652,#142653,#142654,#142655),.UNSPECIFIED.,.F.,.F.,(4,3,2,2,2,2,2,4),
(-0.0128577538036982,0.00567052604397339,0.139467562250634,0.278935124501267,
0.421402366816533,0.563869609131798,0.720032639200108,0.790946603218797),
 .UNSPECIFIED.);
#23663=B_SPLINE_CURVE_WITH_KNOTS('',3,(#142664,#142665,#142666,#142667,
#142668,#142669,#142670,#142671,#142672,#142673),.UNSPECIFIED.,.F.,.F.,
(4,2,2,2,4),(0.603059033985991,0.640749534408183,0.678440034830375,0.716154939786789,
0.753869844743204),.UNSPECIFIED.);
#23664=B_SPLINE_CURVE_WITH_KNOTS('',3,(#142677,#142678,#142679,#142680,
#142681,#142682,#142683,#142684,#142685,#142686,#142687,#142688,#142689,
#142690,#142691,#142692,#142693,#142694),.UNSPECIFIED.,.F.,.F.,(4,2,2,2,
2,2,2,2,4),(0.,0.0939769400668632,0.187953880133726,0.285086724461635,0.382219568789543,
0.485399452153548,0.588579335517553,0.683402310815935,0.778225286114316),
 .UNSPECIFIED.);
#23665=B_SPLINE_CURVE_WITH_KNOTS('',3,(#142698,#142699,#142700,#142701,
#142702,#142703,#142704,#142705,#142706,#142707),.UNSPECIFIED.,.F.,.F.,
(4,2,2,2,4),(-0.168397624102938,-0.121332479144638,-0.074267334186339,-0.0371336670931696,
0.),.UNSPECIFIED.);
#23666=B_SPLINE_CURVE_WITH_KNOTS('',3,(#142713,#142714,#142715,#142716,
#142717,#142718,#142719,#142720,#142721,#142722,#142723,#142724),
 .UNSPECIFIED.,.F.,.F.,(4,2,2,2,2,4),(1.37984672511584,1.40611061616659,
1.50164662943263,1.59718264269866,1.71238091394357,1.79261814476496),
 .UNSPECIFIED.);
#23667=B_SPLINE_CURVE_WITH_KNOTS('',3,(#142912,#142913,#142914,#142915,
#142916,#142917,#142918,#142919,#142920,#142921,#142922,#142923,#142924,
#142925),.UNSPECIFIED.,.F.,.F.,(4,2,2,2,2,2,4),(-0.142919155679814,-0.142584878197208,
-0.131628599743153,-0.109600735717745,-0.0922149909757629,-0.0785268178472592,
-0.0721276294223837),.UNSPECIFIED.);
#23668=B_SPLINE_CURVE_WITH_KNOTS('',3,(#143028,#143029,#143030,#143031,
#143032,#143033,#143034,#143035,#143036,#143037,#143038,#143039,#143040,
#143041),.UNSPECIFIED.,.F.,.F.,(4,2,2,2,2,2,4),(-0.144508400855472,-0.144147613097621,
-0.129519379467225,-0.115275397220758,-0.098017254785151,-0.0843295892561403,
-0.0720738065488153),.UNSPECIFIED.);
#23669=B_SPLINE_CURVE_WITH_KNOTS('',3,(#143046,#143047,#143048,#143049),
 .UNSPECIFIED.,.F.,.F.,(4,4),(0.126555917274389,0.127955709526028),
 .UNSPECIFIED.);
#23670=B_SPLINE_CURVE_WITH_KNOTS('',3,(#143051,#143052,#143053,#143054,
#143055,#143056),.UNSPECIFIED.,.F.,.F.,(4,2,4),(0.12515823369475,0.125586430963453,
0.12655591727435),.UNSPECIFIED.);
#23671=B_SPLINE_CURVE_WITH_KNOTS('',3,(#143068,#143069,#143070,#143071,
#143072,#143073,#143074,#143075,#143076,#143077,#143078,#143079,#143080,
#143081,#143082,#143083,#143084,#143085,#143086,#143087,#143088,#143089,
#143090,#143091,#143092,#143093,#143094,#143095),.UNSPECIFIED.,.F.,.F.,
(4,3,2,2,2,2,2,2,2,2,2,3,4),(1.00649313055325,1.02506097707024,1.19486303676886,
1.28260286113604,1.37034268550322,1.44970888377749,1.52907508205176,1.60844128032603,
1.68780747860031,1.77554730296748,1.86328712733466,2.03308918703329,2.05164843706349),
 .UNSPECIFIED.);
#23672=B_SPLINE_CURVE_WITH_KNOTS('',3,(#143109,#143110,#143111,#143112,
#143113,#143114,#143115,#143116,#143117,#143118,#143119,#143120,#143121,
#143122,#143123,#143124,#143125,#143126,#143127),.UNSPECIFIED.,.F.,.F.,
(4,3,3,3,3,3,4),(0.,0.00601946685722754,0.0114877407859627,0.0130556988279324,
0.0185846512727586,0.0238133106387385,0.0241136037175848),.UNSPECIFIED.);
#23673=B_SPLINE_CURVE_WITH_KNOTS('',3,(#143129,#143130,#143131,#143132,
#143133,#143134,#143135,#143136,#143137,#143138,#143139,#143140,#143141,
#143142),.UNSPECIFIED.,.F.,.F.,(4,2,2,2,2,2,4),(2.23207184191967,2.29687645546178,
2.38015427484409,2.41565949974496,2.44114532275338,2.45388823425759,2.4666311457618),
 .UNSPECIFIED.);
#23674=B_SPLINE_CURVE_WITH_KNOTS('',3,(#143144,#143145,#143146,#143147,
#143148,#143149,#143150,#143151,#143152,#143153,#143154,#143155),
 .UNSPECIFIED.,.F.,.F.,(4,2,2,2,2,4),(2.4666311457618,2.47937405726601,
2.49211696877022,2.51760279177863,2.55310801667951,2.57292617100586),
 .UNSPECIFIED.);
#23675=B_SPLINE_CURVE_WITH_KNOTS('',3,(#143157,#143158,#143159,#143160,
#143161,#143162,#143163),.UNSPECIFIED.,.F.,.F.,(4,3,4),(-2.6313632032836E-5,
0.00282304343927375,0.00571245680678869),.UNSPECIFIED.);
#23676=B_SPLINE_CURVE_WITH_KNOTS('',3,(#143313,#143314,#143315,#143316,
#143317,#143318),.UNSPECIFIED.,.F.,.F.,(4,2,4),(0.,0.0412614986637767,0.0652763436524788),
 .UNSPECIFIED.);
#23677=B_SPLINE_CURVE_WITH_KNOTS('',3,(#143320,#143321,#143322,#143323,
#143324,#143325,#143326,#143327,#143328,#143329,#143330,#143331),
 .UNSPECIFIED.,.F.,.F.,(4,2,2,2,2,4),(1.53706718335664,1.55794389292349,
1.59344911782436,1.61893494083278,1.63167785233699,1.6444207638412),
 .UNSPECIFIED.);
#23678=B_SPLINE_CURVE_WITH_KNOTS('',3,(#143333,#143334,#143335,#143336,
#143337,#143338,#143339,#143340,#143341,#143342,#143343,#143344,#143345,
#143346),.UNSPECIFIED.,.F.,.F.,(4,2,2,2,2,2,4),(1.6444207638412,1.65716367534541,
1.66990658684962,1.69539240985803,1.73089763475891,1.81417545414122,1.90238360165616),
 .UNSPECIFIED.);
#23679=B_SPLINE_CURVE_WITH_KNOTS('',3,(#143348,#143349,#143350,#143351,
#143352,#143353),.UNSPECIFIED.,.F.,.F.,(4,2,4),(0.,0.00532881829401623,
0.0217063037167981),.UNSPECIFIED.);
#23680=B_SPLINE_CURVE_WITH_KNOTS('',3,(#143556,#143557,#143558,#143559,
#143560,#143561,#143562,#143563,#143564,#143565,#143566,#143567,#143568,
#143569,#143570,#143571,#143572,#143573),.UNSPECIFIED.,.F.,.F.,(4,2,2,2,
2,2,2,2,4),(0.,0.0948259003515225,0.189651800703045,0.292563142700536,0.395474484698028,
0.492438634253719,0.589402783809411,0.683398079037316,0.777393374265221),
 .UNSPECIFIED.);
#23681=B_SPLINE_CURVE_WITH_KNOTS('',3,(#143577,#143578,#143579,#143580,
#143581,#143582,#143583,#143584,#143585,#143586,#143587,#143588,#143589,
#143590,#143591,#143592,#143593,#143594),.UNSPECIFIED.,.F.,.F.,(4,2,2,2,
2,2,2,2,4),(0.,0.0944195222117657,0.188839044423531,0.286064822200348,0.383290599977165,
0.488790377679475,0.594290155381785,0.689433686163349,0.784577216944913),
 .UNSPECIFIED.);
#23682=B_SPLINE_CURVE_WITH_KNOTS('',3,(#143600,#143601,#143602,#143603,
#143604,#143605,#143606,#143607,#143608,#143609,#143610,#143611,#143612,
#143613,#143614,#143615,#143616,#143617),.UNSPECIFIED.,.F.,.F.,(4,2,2,2,
2,2,2,2,4),(0.,0.098362147606416,0.196724295212832,0.299373551861381,0.40202280850993,
0.499926681532627,0.597830554555324,0.691757138564027,0.785683722572729),
 .UNSPECIFIED.);
#23683=B_SPLINE_CURVE_WITH_KNOTS('',3,(#143801,#143802,#143803,#143804,
#143805,#143806,#143807,#143808,#143809,#143810),.UNSPECIFIED.,.F.,.F.,
(4,2,2,2,4),(0.189270674477839,0.211763257145919,0.234255839813999,0.258231413480196,
0.282206987146393),.UNSPECIFIED.);
#23684=B_SPLINE_CURVE_WITH_KNOTS('',3,(#143813,#143814,#143815,#143816,
#143817,#143818,#143819,#143820,#143821,#143822,#143823,#143824,#143825,
#143826),.UNSPECIFIED.,.F.,.F.,(4,2,2,2,2,2,4),(0.18925639316843,0.212017765594377,
0.234779138020324,0.258485907400251,0.282192676780179,0.306887761301932,
0.326562144225016),.UNSPECIFIED.);
#23685=B_SPLINE_CURVE_WITH_KNOTS('',3,(#143842,#143843,#143844,#143845,
#143846,#143847,#143848,#143849,#143850,#143851,#143852,#143853,#143854,
#143855),.UNSPECIFIED.,.F.,.F.,(4,2,2,2,2,2,4),(0.241932234759915,0.261279320323699,
0.286037147223808,0.309784118650402,0.333531090076996,0.356299951830059,
0.379068813583121),.UNSPECIFIED.);
#23686=B_SPLINE_CURVE_WITH_KNOTS('',3,(#143875,#143876,#143877,#143878,
#143879,#143880,#143881,#143882,#143883,#143884),.UNSPECIFIED.,.F.,.F.,
(4,2,2,2,4),(0.286037128270882,0.310064366617074,0.334091604963267,0.3565802092733,
0.379068813583334),.UNSPECIFIED.);
#23687=B_SPLINE_CURVE_WITH_KNOTS('',3,(#143886,#143887,#143888,#143889,
#143890,#143891,#143892,#143893,#143894,#143895),.UNSPECIFIED.,.F.,.F.,
(4,2,2,2,4),(1.01847209163261,1.09614224834082,1.21102278725762,1.30659119635196,
1.40215960544631),.UNSPECIFIED.);
#23688=B_SPLINE_CURVE_WITH_KNOTS('',3,(#143909,#143910,#143911,#143912,
#143913,#143914,#143915,#143916,#143917,#143918,#143919,#143920,#143921,
#143922,#143923,#143924,#143925),.UNSPECIFIED.,.F.,.F.,(4,2,2,2,3,2,2,4),
(0.928216827061862,0.932389730285405,0.992769022880904,1.0531483154764,
1.1739069006674,1.2946654858584,1.3550447784539,1.39738911925677),
 .UNSPECIFIED.);
#23689=B_SPLINE_CURVE_WITH_KNOTS('',3,(#143951,#143952,#143953,#143954,
#143955,#143956),.UNSPECIFIED.,.F.,.F.,(4,2,4),(0.104086067281323,0.108489006128221,
0.168304783933614),.UNSPECIFIED.);
#23690=B_SPLINE_CURVE_WITH_KNOTS('',3,(#143958,#143959,#143960,#143961,
#143962,#143963,#143964,#143965,#143966,#143967,#143968,#143969),
 .UNSPECIFIED.,.F.,.F.,(4,2,2,2,2,4),(0.371222277774226,0.439583636064719,
0.595306530197309,0.737554434553936,0.879802338910563,0.949739845591811),
 .UNSPECIFIED.);
#23691=B_SPLINE_CURVE_WITH_KNOTS('',3,(#143970,#143971,#143972,#143973,
#143974,#143975),.UNSPECIFIED.,.F.,.F.,(4,2,4),(0.0529943431633899,0.0577411969641437,
0.162437857102921),.UNSPECIFIED.);
#23692=B_SPLINE_CURVE_WITH_KNOTS('',3,(#143995,#143996,#143997,#143998,
#143999,#144000,#144001,#144002),.UNSPECIFIED.,.F.,.F.,(4,2,2,4),(0.454924391717627,
0.46478463553666,0.487557239675925,0.503332474617141),.UNSPECIFIED.);
#23693=B_SPLINE_CURVE_WITH_KNOTS('',3,(#144013,#144014,#144015,#144016,
#144017,#144018,#144019,#144020,#144021,#144022),.UNSPECIFIED.,.F.,.F.,
(4,2,2,2,4),(0.301557475483223,0.33925269209598,0.376947908708738,0.414656148075488,
0.452364387442238),.UNSPECIFIED.);
#23694=B_SPLINE_CURVE_WITH_KNOTS('',3,(#144024,#144025,#144026,#144027,
#144028,#144029,#144030,#144031),.UNSPECIFIED.,.F.,.F.,(4,2,2,4),(-0.108303883771064,
-0.0753798988372107,-0.0376899494186054,0.),.UNSPECIFIED.);
#23695=B_SPLINE_CURVE_WITH_KNOTS('',3,(#144040,#144041,#144042,#144043,
#144044,#144045,#144046,#144047,#144048,#144049),.UNSPECIFIED.,.F.,.F.,
(4,2,2,2,4),(0.344103183736344,0.381242716027575,0.418382248318806,0.465288723179234,
0.512195198039662),.UNSPECIFIED.);
#23696=B_SPLINE_CURVE_WITH_KNOTS('',3,(#144061,#144062,#144063,#144064,
#144065,#144066,#144067,#144068,#144069,#144070),.UNSPECIFIED.,.F.,.F.,
(4,2,2,2,4),(0.363197033462642,0.4031110869448,0.443025140426958,0.490684930222813,
0.538344720018669),.UNSPECIFIED.);
#23697=B_SPLINE_CURVE_WITH_KNOTS('',3,(#144074,#144075,#144076,#144077,
#144078,#144079,#144080,#144081,#144082,#144083),.UNSPECIFIED.,.F.,.F.,
(4,2,2,2,4),(0.150729427408656,0.188455603969964,0.226181780531272,0.263877644175159,
0.301573507819046),.UNSPECIFIED.);
#23698=B_SPLINE_CURVE_WITH_KNOTS('',3,(#144089,#144090,#144091,#144092,
#144093,#144094,#144095,#144096,#144097,#144098),.UNSPECIFIED.,.F.,.F.,
(4,2,2,2,4),(0.550254856554737,0.59775876613801,0.645262675721284,0.685134618848566,
0.725006561975848),.UNSPECIFIED.);
#23699=B_SPLINE_CURVE_WITH_KNOTS('',3,(#144118,#144119,#144120,#144121,
#144122,#144123,#144124,#144125,#144126,#144127,#144128,#144129,#144130),
 .UNSPECIFIED.,.F.,.F.,(4,2,2,2,3,4),(-0.100223122044128,-0.0800989314803924,
-0.0599747409166565,-0.0299873704583282,0.,0.0243767134003336),
 .UNSPECIFIED.);
#23700=B_SPLINE_CURVE_WITH_KNOTS('',3,(#144138,#144139,#144140,#144141,
#144142,#144143,#144144,#144145,#144146,#144147,#144148,#144149),
 .UNSPECIFIED.,.F.,.F.,(4,2,2,2,2,4),(0.21639017325191,0.239839563382432,
0.26982693384076,0.299814304299088,0.319938494862824,0.34006268542656),
 .UNSPECIFIED.);
#23701=B_SPLINE_CURVE_WITH_KNOTS('',3,(#144156,#144157,#144158,#144159,
#144160,#144161),.UNSPECIFIED.,.F.,.F.,(4,2,4),(1.4463380141481,1.46636753961024,
1.5045533789501),.UNSPECIFIED.);
#23702=B_SPLINE_CURVE_WITH_KNOTS('',3,(#144163,#144164,#144165,#144166),
 .UNSPECIFIED.,.F.,.F.,(4,4),(2.02040063642927,2.03639014323659),
 .UNSPECIFIED.);
#23703=B_SPLINE_CURVE_WITH_KNOTS('',3,(#144169,#144170,#144171,#144172,
#144173,#144174,#144175,#144176,#144177,#144178,#144179,#144180,#144181,
#144182,#144183),.UNSPECIFIED.,.F.,.F.,(4,2,2,2,3,2,4),(0.225773787410195,
0.239394753865059,0.253015720319924,0.273253708378096,0.293491696436268,
0.315181887462217,0.333911176073498),.UNSPECIFIED.);
#23704=B_SPLINE_CURVE_WITH_KNOTS('',3,(#144185,#144186,#144187,#144188,
#144189,#144190,#144191,#144192,#144193,#144194,#144195,#144196,#144197,
#144198,#144199),.UNSPECIFIED.,.F.,.F.,(4,2,2,2,3,2,4),(-0.068263214221219,
-0.0545185069182086,-0.0407737996151983,-0.0203868998075991,0.,0.0215381797259622,
0.0362085650374704),.UNSPECIFIED.);
#23705=B_SPLINE_CURVE_WITH_KNOTS('',3,(#144207,#144208,#144209,#144210,
#144211,#144212,#144213,#144214,#144215,#144216,#144217,#144218,#144219,
#144220,#144221,#144222),.UNSPECIFIED.,.F.,.F.,(4,2,2,2,2,2,2,4),(0.763245415685139,
0.772656167228652,0.890067929002265,1.00747969077588,1.12489145254949,1.2423032143231,
1.34066137334052,1.34318636064082),.UNSPECIFIED.);
#23706=B_SPLINE_CURVE_WITH_KNOTS('',3,(#144234,#144235,#144236,#144237),
 .UNSPECIFIED.,.F.,.F.,(4,4),(1.52365417396437,1.52591840699516),
 .UNSPECIFIED.);
#23707=B_SPLINE_CURVE_WITH_KNOTS('',3,(#144238,#144239,#144240,#144241),
 .UNSPECIFIED.,.F.,.F.,(4,4),(1.80468312171546,1.87869184978489),
 .UNSPECIFIED.);
#23708=B_SPLINE_CURVE_WITH_KNOTS('',3,(#144242,#144243,#144244,#144245),
 .UNSPECIFIED.,.F.,.F.,(4,4),(6.05153047053036,6.12780351388147),
 .UNSPECIFIED.);
#23709=B_SPLINE_CURVE_WITH_KNOTS('',3,(#144249,#144250,#144251,#144252,
#144253,#144254,#144255,#144256,#144257,#144258,#144259,#144260,#144261,
#144262,#144263,#144264),.UNSPECIFIED.,.F.,.F.,(4,2,2,2,2,2,2,4),(0.156606736308253,
0.180805448767024,0.20508734783811,0.217228297373654,0.229369246909197,
0.24151019644474,0.253651145980283,0.264578837334174),.UNSPECIFIED.);
#23710=B_SPLINE_CURVE_WITH_KNOTS('',3,(#144276,#144277,#144278,#144279,
#144280,#144281),.UNSPECIFIED.,.F.,.F.,(4,2,4),(2.05087433026329,2.07604853698334,
2.22480786223231),.UNSPECIFIED.);
#23711=B_SPLINE_CURVE_WITH_KNOTS('',3,(#144283,#144284,#144285,#144286,
#144287,#144288),.UNSPECIFIED.,.F.,.F.,(4,2,4),(3.23765002225092,3.43215209198459,
3.58086556096453),.UNSPECIFIED.);
#23712=B_SPLINE_CURVE_WITH_KNOTS('',3,(#144290,#144291,#144292,#144293,
#144294,#144295,#144296,#144297),.UNSPECIFIED.,.F.,.F.,(4,2,2,4),(0.193941715876439,
0.365833717405826,0.459726527436784,0.496146962294632),.UNSPECIFIED.);
#23713=B_SPLINE_CURVE_WITH_KNOTS('',3,(#144298,#144299,#144300,#144301,
#144302,#144303,#144304,#144305),.UNSPECIFIED.,.F.,.F.,(4,2,2,4),(1.19119064358888,
1.25304900366289,1.35089757112752,1.40777544238509),.UNSPECIFIED.);
#23714=B_SPLINE_CURVE_WITH_KNOTS('',3,(#144308,#144309,#144310,#144311,
#144312,#144313,#144314,#144315,#144316,#144317,#144318,#144319,#144320,
#144321),.UNSPECIFIED.,.F.,.F.,(4,2,2,2,2,2,4),(0.0724967244197842,0.0766714820213276,
0.114986644138398,0.153301806255469,0.19149984850442,0.229697890753371,
0.234669900956502),.UNSPECIFIED.);
#23715=B_SPLINE_CURVE_WITH_KNOTS('',3,(#144327,#144328,#144329,#144330),
 .UNSPECIFIED.,.F.,.F.,(4,4),(1.62317914932141,1.69306789581112),
 .UNSPECIFIED.);
#23716=B_SPLINE_CURVE_WITH_KNOTS('',3,(#144332,#144333,#144334,#144335,
#144336,#144337),.UNSPECIFIED.,.F.,.F.,(4,2,4),(0.410526643667809,0.556855217300137,
0.576452875080128),.UNSPECIFIED.);
#23717=B_SPLINE_CURVE_WITH_KNOTS('',3,(#144338,#144339,#144340,#144341,
#144342,#144343),.UNSPECIFIED.,.F.,.F.,(4,2,4),(0.257017510558728,0.263940899519207,
0.300168261034611),.UNSPECIFIED.);
#23718=B_SPLINE_CURVE_WITH_KNOTS('',3,(#144369,#144370,#144371,#144372,
#144373,#144374,#144375,#144376,#144377,#144378),.UNSPECIFIED.,.F.,.F.,
(4,2,2,2,4),(1.31489350131146,1.33456157653928,1.41236011898755,1.49015866143582,
1.50084837281906),.UNSPECIFIED.);
#23719=B_SPLINE_CURVE_WITH_KNOTS('',3,(#144388,#144389,#144390,#144391,
#144392,#144393,#144394,#144395,#144396,#144397,#144398,#144399,#144400),
 .UNSPECIFIED.,.F.,.F.,(4,3,2,2,2,4),(0.417573720644144,0.440269087673341,
0.470377854302809,0.500486620932276,0.520711745600823,0.540936870269371),
 .UNSPECIFIED.);
#23720=B_SPLINE_CURVE_WITH_KNOTS('',3,(#144455,#144456,#144457,#144458,
#144459,#144460),.UNSPECIFIED.,.F.,.F.,(4,2,4),(1.28130036614749,1.3304475484929,
1.37533827653421),.UNSPECIFIED.);
#23721=B_SPLINE_CURVE_WITH_KNOTS('',3,(#144462,#144463,#144464,#144465,
#144466,#144467,#144468,#144469),.UNSPECIFIED.,.F.,.F.,(4,2,2,4),(0.372364396932915,
0.435374241191316,0.532988843711153,0.599542108482719),.UNSPECIFIED.);
#23722=B_SPLINE_CURVE_WITH_KNOTS('',3,(#144483,#144484,#144485,#144486,
#144487,#144488,#144489,#144490,#144491,#144492,#144493),.UNSPECIFIED.,
 .F.,.F.,(4,2,3,2,4),(-0.149195468638109,-0.0954898081619349,0.,0.105194370875322,
0.138905665786208),.UNSPECIFIED.);
#23723=B_SPLINE_CURVE_WITH_KNOTS('',3,(#144509,#144510,#144511,#144512),
 .UNSPECIFIED.,.F.,.F.,(4,4),(2.8612825744839,2.89469550090435),
 .UNSPECIFIED.);
#23724=B_SPLINE_CURVE_WITH_KNOTS('',3,(#144565,#144566,#144567,#144568,
#144569,#144570),.UNSPECIFIED.,.F.,.F.,(4,2,4),(2.59711974020287,2.67846990390876,
2.74436889115826),.UNSPECIFIED.);
#23725=B_SPLINE_CURVE_WITH_KNOTS('',3,(#144573,#144574,#144575,#144576,
#144577,#144578,#144579,#144580,#144581,#144582,#144583,#144584,#144585),
 .UNSPECIFIED.,.F.,.F.,(4,2,2,2,3,4),(0.3424697429409,0.362070187841933,
0.381670632742966,0.411028407725618,0.440386182708269,0.473071910942229),
 .UNSPECIFIED.);
#23726=B_SPLINE_CURVE_WITH_KNOTS('',3,(#144587,#144588,#144589,#144590,
#144591,#144592),.UNSPECIFIED.,.F.,.F.,(4,2,4),(6.1917354885447,6.24887728986414,
6.34659932277937),.UNSPECIFIED.);
#23727=B_SPLINE_CURVE_WITH_KNOTS('',3,(#144596,#144597,#144598,#144599,
#144600,#144601,#144602,#144603,#144604,#144605,#144606,#144607,#144608),
 .UNSPECIFIED.,.F.,.F.,(4,3,2,2,2,4),(0.40770045386894,0.440386182708269,
0.46974395769092,0.499101732673572,0.518702177574605,0.538302622475638),
 .UNSPECIFIED.);
#23728=B_SPLINE_CURVE_WITH_KNOTS('',3,(#144609,#144610,#144611,#144612),
 .UNSPECIFIED.,.F.,.F.,(4,4),(7.0054188597794,7.15111856184614),
 .UNSPECIFIED.);
#23729=B_SPLINE_CURVE_WITH_KNOTS('',3,(#144618,#144619,#144620,#144621,
#144622,#144623,#144624,#144625,#144626,#144627),.UNSPECIFIED.,.F.,.F.,
(4,2,2,2,4),(0.959941045056019,1.01793558590819,1.10632333107227,1.1957800913699,
1.2405102505028),.UNSPECIFIED.);
#23730=B_SPLINE_CURVE_WITH_KNOTS('',3,(#144650,#144651,#144652,#144653,
#144654,#144655,#144656,#144657,#144658,#144659,#144660,#144661,#144662),
 .UNSPECIFIED.,.F.,.F.,(4,1,1,1,1,1,1,1,1,1,4),(-0.194615646314672,-0.191966963306305,
-0.188476654882554,-0.181496038035052,-0.167534804340048,-0.13961233695004,
-0.125651103255036,-0.111689869560032,-0.0837674021700239,-0.0558449347800159,
0.),.UNSPECIFIED.);
#23731=B_SPLINE_CURVE_WITH_KNOTS('',3,(#144663,#144664,#144665,#144666,
#144667,#144668,#144669,#144670,#144671,#144672,#144673,#144674,#144675,
#144676,#144677,#144678,#144679,#144680,#144681,#144682,#144683),
 .UNSPECIFIED.,.F.,.F.,(4,2,2,2,2,3,2,2,2,4),(-0.184532964552272,-0.110069111897134,
-0.0293037936841922,-0.0146518968420961,-0.00732594842104806,0.,0.00444223893322424,
0.00888447786644848,0.017768955732897,0.0282169626580737),.UNSPECIFIED.);
#23732=B_SPLINE_CURVE_WITH_KNOTS('',3,(#144704,#144705,#144706,#144707,
#144708),.UNSPECIFIED.,.F.,.F.,(4,1,4),(-0.148760844879958,-0.0637546478056962,
0.),.UNSPECIFIED.);
#23733=B_SPLINE_CURVE_WITH_KNOTS('',3,(#144719,#144720,#144721,#144722,
#144723),.UNSPECIFIED.,.F.,.F.,(4,1,4),(0.,0.0637546478056962,0.148760844879958),
 .UNSPECIFIED.);
#23734=B_SPLINE_CURVE_WITH_KNOTS('',3,(#144725,#144726,#144727,#144728,
#144729,#144730,#144731,#144732,#144733,#144734,#144735,#144736),
 .UNSPECIFIED.,.F.,.F.,(4,2,2,2,2,4),(0.125732173566188,0.141264421553229,
0.170878065072357,0.200491708591485,0.260959450514356,0.268438600062818),
 .UNSPECIFIED.);
#23735=B_SPLINE_CURVE_WITH_KNOTS('',3,(#144782,#144783,#144784,#144785,
#144786,#144787,#144788,#144789,#144790,#144791,#144792,#144793),
 .UNSPECIFIED.,.F.,.F.,(4,2,2,2,2,4),(0.449858469158036,0.479607229821293,
0.553740396055668,0.642656295652044,0.695378146353882,0.704137329267106),
 .UNSPECIFIED.);
#23736=B_SPLINE_CURVE_WITH_KNOTS('',3,(#144796,#144797,#144798,#144799,
#144800,#144801,#144802,#144803,#144804,#144805,#144806,#144807,#144808),
 .UNSPECIFIED.,.F.,.F.,(4,3,2,2,2,4),(0.407700454474756,0.44038618270827,
0.469743957690921,0.499101732673573,0.518702177574606,0.538302622475639),
 .UNSPECIFIED.);
#23737=B_SPLINE_CURVE_WITH_KNOTS('',3,(#144814,#144815,#144816,#144817,
#144818,#144819,#144820),.UNSPECIFIED.,.F.,.F.,(4,3,4),(2.40353495487923,
2.40579815042619,2.52067239352636),.UNSPECIFIED.);
#23738=B_SPLINE_CURVE_WITH_KNOTS('',3,(#144823,#144824,#144825,#144826,
#144827,#144828,#144829,#144830,#144831,#144832,#144833,#144834,#144835),
 .UNSPECIFIED.,.F.,.F.,(4,2,2,2,3,4),(0.342469742940901,0.362070187841934,
0.381670632742967,0.411028407725619,0.44038618270827,0.473071910941784),
 .UNSPECIFIED.);
#23739=B_SPLINE_CURVE_WITH_KNOTS('',3,(#144903,#144904,#144905,#144906,
#144907,#144908,#144909),.UNSPECIFIED.,.F.,.F.,(4,3,4),(0.,0.00387940189952665,
0.00751236288843331),.UNSPECIFIED.);
#23740=B_SPLINE_CURVE_WITH_KNOTS('',3,(#144972,#144973,#144974,#144975,
#144976,#144977),.UNSPECIFIED.,.F.,.F.,(4,2,4),(1.82331017716016,1.90750204863416,
2.02800814763992),.UNSPECIFIED.);
#23741=B_SPLINE_CURVE_WITH_KNOTS('',3,(#145072,#145073,#145074,#145075,
#145076,#145077),.UNSPECIFIED.,.F.,.F.,(4,2,4),(2.32014740388574,2.402277537928,
2.48440767197027),.UNSPECIFIED.);
#23742=B_SPLINE_CURVE_WITH_KNOTS('',3,(#145178,#145179,#145180,#145181),
 .UNSPECIFIED.,.F.,.F.,(4,4),(0.,0.00120017992069814),.UNSPECIFIED.);
#23743=B_SPLINE_CURVE_WITH_KNOTS('',3,(#145202,#145203,#145204,#145205),
 .UNSPECIFIED.,.F.,.F.,(4,4),(0.,0.00271678269554457),.UNSPECIFIED.);
#23744=B_SPLINE_CURVE_WITH_KNOTS('',3,(#145267,#145268,#145269,#145270,
#145271,#145272),.UNSPECIFIED.,.F.,.F.,(4,1,1,4),(0.304018832611615,0.312633818864471,
0.321815335614959,0.346299380282928),.UNSPECIFIED.);
#23745=B_SPLINE_CURVE_WITH_KNOTS('',3,(#145559,#145560,#145561,#145562,
#145563,#145564),.UNSPECIFIED.,.F.,.F.,(4,2,4),(1.70223819819958,1.73108544940882,
1.82543924719591),.UNSPECIFIED.);
#23746=B_SPLINE_CURVE_WITH_KNOTS('',3,(#145675,#145676,#145677,#145678,
#145679,#145680),.UNSPECIFIED.,.F.,.F.,(4,2,4),(3.10863777787119,3.15979788758472,
3.18717384259103),.UNSPECIFIED.);
#23747=B_SPLINE_CURVE_WITH_KNOTS('',3,(#145682,#145683,#145684,#145685,
#145686,#145687),.UNSPECIFIED.,.F.,.F.,(4,2,4),(0.820560587522253,0.903541428390679,
0.986302965827679),.UNSPECIFIED.);
#23748=B_SPLINE_CURVE_WITH_KNOTS('',3,(#145690,#145691,#145692,#145693,
#145694,#145695,#145696,#145697),.UNSPECIFIED.,.F.,.F.,(4,2,2,4),(1.04408314569026,
1.07700516790035,1.159852876147,1.19188777117613),.UNSPECIFIED.);
#23749=B_SPLINE_CURVE_WITH_KNOTS('',3,(#145700,#145701,#145702,#145703,
#145704,#145705),.UNSPECIFIED.,.F.,.F.,(4,2,4),(0.461890211108374,0.489266166114685,
0.540426267783997),.UNSPECIFIED.);
#23750=B_SPLINE_CURVE_WITH_KNOTS('',3,(#145707,#145708,#145709,#145710,
#145711,#145712),.UNSPECIFIED.,.F.,.F.,(4,2,4),(1.94461759101078,2.03897139402255,
2.06781864523179),.UNSPECIFIED.);
#23751=B_SPLINE_CURVE_WITH_KNOTS('',3,(#145714,#145715,#145716,#145717,
#145718,#145719,#145720,#145721),.UNSPECIFIED.,.F.,.F.,(4,2,2,4),(0.734169017530397,
0.766203907566677,0.84905161581333,0.881973638023425),.UNSPECIFIED.);
#23752=B_SPLINE_CURVE_WITH_KNOTS('',3,(#145724,#145725,#145726,#145727,
#145728,#145729),.UNSPECIFIED.,.F.,.F.,(4,2,4),(0.991122094940072,1.07388363237707,
1.15686448098652),.UNSPECIFIED.);
#23753=B_SPLINE_CURVE_WITH_KNOTS('',3,(#145748,#145749,#145750,#145751),
 .UNSPECIFIED.,.F.,.F.,(4,4),(0.938179827022778,0.986302965827679),
 .UNSPECIFIED.);
#23754=B_SPLINE_CURVE_WITH_KNOTS('',3,(#145754,#145755,#145756,#145757,
#145758,#145759),.UNSPECIFIED.,.F.,.F.,(4,2,4),(1.04408314569026,1.07700516790035,
1.10576357261676),.UNSPECIFIED.);
#23755=B_SPLINE_CURVE_WITH_KNOTS('',3,(#145762,#145763,#145764,#145765,
#145766,#145767),.UNSPECIFIED.,.F.,.F.,(4,2,4),(0.820293211096921,0.84905161581333,
0.881973638023425),.UNSPECIFIED.);
#23756=B_SPLINE_CURVE_WITH_KNOTS('',3,(#145770,#145771,#145772,#145773),
 .UNSPECIFIED.,.F.,.F.,(4,4),(0.991122094940074,1.03924523374497),
 .UNSPECIFIED.);
#23757=B_SPLINE_CURVE_WITH_KNOTS('',3,(#145877,#145878,#145879,#145880,
#145881,#145882,#145883,#145884,#145885,#145886),.UNSPECIFIED.,.F.,.F.,
(4,2,2,2,4),(-0.67890407197508,-0.638811382079944,-0.567890404574991,-0.49694871747295,
-0.466428520808092),.UNSPECIFIED.);
#23758=B_SPLINE_CURVE_WITH_KNOTS('',3,(#145890,#145891,#145892,#145893,
#145894,#145895,#145896,#145897,#145898,#145899),.UNSPECIFIED.,.F.,.F.,
(4,2,2,2,4),(-0.678904071966558,-0.638811382082276,-0.567890404578285,-0.496948717476777,
-0.466428520822623),.UNSPECIFIED.);
#23759=B_SPLINE_CURVE_WITH_KNOTS('',3,(#145904,#145905,#145906,#145907,
#145908,#145909,#145910,#145911,#145912,#145913),.UNSPECIFIED.,.F.,.F.,
(4,2,2,2,4),(-0.678904071957372,-0.638811382080974,-0.567890404576434,-0.496948717474622,
-0.466428520828439),.UNSPECIFIED.);
#23760=B_SPLINE_CURVE_WITH_KNOTS('',3,(#145917,#145918,#145919,#145920,
#145921,#145922,#145923,#145924,#145925,#145926),.UNSPECIFIED.,.F.,.F.,
(4,2,2,2,4),(-0.678904071960599,-0.638811382082355,-0.567890404578383,-0.496948717476885,
-0.466428520828765),.UNSPECIFIED.);
#23761=B_SPLINE_CURVE_WITH_KNOTS('',3,(#145931,#145932,#145933,#145934,
#145935,#145936,#145937,#145938,#145939,#145940),.UNSPECIFIED.,.F.,.F.,
(4,2,2,2,4),(-0.678904071989196,-0.638811382078946,-0.567890404573567,-0.496948717471288,
-0.466428520791381),.UNSPECIFIED.);
#23762=B_SPLINE_CURVE_WITH_KNOTS('',3,(#145944,#145945,#145946,#145947,
#145948,#145949,#145950,#145951,#145952,#145953),.UNSPECIFIED.,.F.,.F.,
(4,2,2,2,4),(-0.67890407198423,-0.638811382082675,-0.567890404578853,-0.496948717477438,
-0.466428520805978),.UNSPECIFIED.);
#23763=B_SPLINE_CURVE_WITH_KNOTS('',3,(#145958,#145959,#145960,#145961,
#145962,#145963,#145964,#145965,#145966,#145967),.UNSPECIFIED.,.F.,.F.,
(4,2,2,2,4),(-0.67890407199097,-0.638811382078488,-0.567890404572896,-0.496948717470497,
-0.466428520788399),.UNSPECIFIED.);
#23764=B_SPLINE_CURVE_WITH_KNOTS('',3,(#145971,#145972,#145973,#145974,
#145975,#145976,#145977,#145978,#145979,#145980),.UNSPECIFIED.,.F.,.F.,
(4,2,2,2,4),(-0.678904071978841,-0.63881138207855,-0.567890404573014,-0.496948717470648,
-0.466428520800727),.UNSPECIFIED.);
#23765=B_SPLINE_CURVE_WITH_KNOTS('',3,(#145985,#145986,#145987,#145988,
#145989,#145990,#145991,#145992,#145993,#145994),.UNSPECIFIED.,.F.,.F.,
(4,2,2,2,4),(-0.678904071978394,-0.638811382081562,-0.567890404577268,-0.496948717475591,
-0.466428520789366),.UNSPECIFIED.);
#23766=B_SPLINE_CURVE_WITH_KNOTS('',3,(#145998,#145999,#146000,#146001,
#146002,#146003,#146004,#146005,#146006,#146007),.UNSPECIFIED.,.F.,.F.,
(4,2,2,2,4),(-0.67890407196277,-0.638811382079109,-0.567890404573782,-0.49694871747153,
-0.466428520818205),.UNSPECIFIED.);
#23767=B_SPLINE_CURVE_WITH_KNOTS('',3,(#146012,#146013,#146014,#146015,
#146016,#146017,#146018,#146019,#146020,#146021),.UNSPECIFIED.,.F.,.F.,
(4,2,2,2,4),(-0.678904071951945,-0.63881138208195,-0.567890404577823,-0.496948717476241,
-0.466428520836395),.UNSPECIFIED.);
#23768=B_SPLINE_CURVE_WITH_KNOTS('',3,(#146025,#146026,#146027,#146028,
#146029,#146030,#146031,#146032,#146033,#146034),.UNSPECIFIED.,.F.,.F.,
(4,2,2,2,4),(-0.678904071984223,-0.638811382077183,-0.567890404571043,-0.496948717468339,
-0.46642852079177),.UNSPECIFIED.);
#23769=B_SPLINE_CURVE_WITH_KNOTS('',3,(#146039,#146040,#146041,#146042,
#146043,#146044,#146045,#146046,#146047,#146048),.UNSPECIFIED.,.F.,.F.,
(4,2,2,2,4),(-0.678904071946678,-0.638811382083569,-0.567890404580107,-0.496948717478892,
-0.466428520817328),.UNSPECIFIED.);
#23770=B_SPLINE_CURVE_WITH_KNOTS('',3,(#146052,#146053,#146054,#146055,
#146056,#146057,#146058,#146059,#146060,#146061),.UNSPECIFIED.,.F.,.F.,
(4,2,2,2,4),(-0.678904071981315,-0.638811382080222,-0.567890404575361,-0.496948717473367,
-0.466428520802537),.UNSPECIFIED.);
#23771=B_SPLINE_CURVE_WITH_KNOTS('',3,(#146066,#146067,#146068,#146069,
#146070,#146071,#146072,#146073,#146074,#146075),.UNSPECIFIED.,.F.,.F.,
(4,2,2,2,4),(-0.678904071991326,-0.638811382081232,-0.567890404576792,-0.496948717475035,
-0.466428520807193),.UNSPECIFIED.);
#23772=B_SPLINE_CURVE_WITH_KNOTS('',3,(#146079,#146080,#146081,#146082,
#146083,#146084,#146085,#146086,#146087,#146088),.UNSPECIFIED.,.F.,.F.,
(4,2,2,2,4),(-0.678904071999347,-0.638811382081042,-0.567890404576521,-0.496948717474717,
-0.466428520786623),.UNSPECIFIED.);
#23773=B_SPLINE_CURVE_WITH_KNOTS('',3,(#146093,#146094,#146095,#146096,
#146097,#146098,#146099,#146100,#146101,#146102),.UNSPECIFIED.,.F.,.F.,
(4,2,2,2,4),(-0.678904071986479,-0.638811382080361,-0.56789040457558,-0.496948717473635,
-0.466428520797767),.UNSPECIFIED.);
#23774=B_SPLINE_CURVE_WITH_KNOTS('',3,(#146106,#146107,#146108,#146109,
#146110,#146111,#146112,#146113,#146114,#146115),.UNSPECIFIED.,.F.,.F.,
(4,2,2,2,4),(-0.678904071955915,-0.6388113820817,-0.567890404577456,-0.496948717475805,
-0.466428520793425),.UNSPECIFIED.);
#23775=B_SPLINE_CURVE_WITH_KNOTS('',3,(#146120,#146121,#146122,#146123,
#146124,#146125,#146126,#146127,#146128,#146129),.UNSPECIFIED.,.F.,.F.,
(4,2,2,2,4),(-0.67890407199572,-0.63881138208008,-0.567890404575174,-0.49694871747316,
-0.466428520827877),.UNSPECIFIED.);
#23776=B_SPLINE_CURVE_WITH_KNOTS('',3,(#146133,#146134,#146135,#146136,
#146137,#146138,#146139,#146140,#146141,#146142),.UNSPECIFIED.,.F.,.F.,
(4,2,2,2,4),(-0.678904071968026,-0.638811382077951,-0.567890404572114,-0.496948717469576,
-0.466428520809921),.UNSPECIFIED.);
#23777=B_SPLINE_CURVE_WITH_KNOTS('',3,(#146147,#146148,#146149,#146150,
#146151,#146152,#146153,#146154,#146155,#146156),.UNSPECIFIED.,.F.,.F.,
(4,2,2,2,4),(-0.678904071991079,-0.63881138208447,-0.567890404581382,-0.496948717480376,
-0.466428520838142),.UNSPECIFIED.);
#23778=B_SPLINE_CURVE_WITH_KNOTS('',3,(#146160,#146161,#146162,#146163,
#146164,#146165,#146166,#146167,#146168,#146169),.UNSPECIFIED.,.F.,.F.,
(4,2,2,2,4),(-0.678904072013284,-0.638811382084366,-0.567890404581246,-0.496948717480222,
-0.466428520827388),.UNSPECIFIED.);
#23779=B_SPLINE_CURVE_WITH_KNOTS('',3,(#146174,#146175,#146176,#146177,
#146178,#146179,#146180,#146181,#146182,#146183),.UNSPECIFIED.,.F.,.F.,
(4,2,2,2,4),(-0.678904071986053,-0.638811382076461,-0.567890404570022,-0.49694871746715,
-0.466428520788073),.UNSPECIFIED.);
#23780=B_SPLINE_CURVE_WITH_KNOTS('',3,(#146187,#146188,#146189,#146190,
#146191,#146192,#146193,#146194,#146195,#146196),.UNSPECIFIED.,.F.,.F.,
(4,2,2,2,4),(-0.67890407199352,-0.638811382083378,-0.567890404579852,-0.496948717478602,
-0.466428520817659),.UNSPECIFIED.);
#23781=B_SPLINE_CURVE_WITH_KNOTS('',3,(#146201,#146202,#146203,#146204,
#146205,#146206,#146207,#146208,#146209,#146210),.UNSPECIFIED.,.F.,.F.,
(4,2,2,2,4),(-0.678904071973262,-0.638811382076435,-0.567890404569995,-0.496948717467124,
-0.466428520774712),.UNSPECIFIED.);
#23782=B_SPLINE_CURVE_WITH_KNOTS('',3,(#146214,#146215,#146216,#146217,
#146218,#146219,#146220,#146221,#146222,#146223),.UNSPECIFIED.,.F.,.F.,
(4,2,2,2,4),(-0.678904071987068,-0.638811382078544,-0.567890404572966,-0.496948717470576,
-0.466428520843256),.UNSPECIFIED.);
#23783=B_SPLINE_CURVE_WITH_KNOTS('',3,(#146228,#146229,#146230,#146231,
#146232,#146233,#146234,#146235,#146236,#146237),.UNSPECIFIED.,.F.,.F.,
(4,2,2,2,4),(-0.678904071987881,-0.638811382084155,-0.567890404580941,-0.496948717479863,
-0.466428520806137),.UNSPECIFIED.);
#23784=B_SPLINE_CURVE_WITH_KNOTS('',3,(#146241,#146242,#146243,#146244,
#146245,#146246,#146247,#146248,#146249,#146250),.UNSPECIFIED.,.F.,.F.,
(4,2,2,2,4),(-0.678904072009282,-0.638811382083207,-0.567890404579597,-0.496948717478301,
-0.466428520834868),.UNSPECIFIED.);
#23785=B_SPLINE_CURVE_WITH_KNOTS('',3,(#146255,#146256,#146257,#146258,
#146259,#146260,#146261,#146262,#146263,#146264),.UNSPECIFIED.,.F.,.F.,
(4,2,2,2,4),(-0.678904071972205,-0.638811382079633,-0.567890404574503,-0.496948717472359,
-0.466428520810097),.UNSPECIFIED.);
#23786=B_SPLINE_CURVE_WITH_KNOTS('',3,(#146268,#146269,#146270,#146271,
#146272,#146273,#146274,#146275,#146276,#146277),.UNSPECIFIED.,.F.,.F.,
(4,2,2,2,4),(-0.678904071979395,-0.63881138208103,-0.567890404576514,-0.496948717474714,
-0.466428520794118),.UNSPECIFIED.);
#23787=B_SPLINE_CURVE_WITH_KNOTS('',3,(#146282,#146283,#146284,#146285,
#146286,#146287,#146288,#146289,#146290,#146291),.UNSPECIFIED.,.F.,.F.,
(4,2,2,2,4),(-0.678904071999173,-0.638811382081402,-0.567890404577046,-0.496948717475338,
-0.466428520787755),.UNSPECIFIED.);
#23788=B_SPLINE_CURVE_WITH_KNOTS('',3,(#146295,#146296,#146297,#146298,
#146299,#146300,#146301,#146302,#146303,#146304),.UNSPECIFIED.,.F.,.F.,
(4,2,2,2,4),(-0.678904071953474,-0.638811382080186,-0.567890404575329,-0.496948717473341,
-0.466428520830318),.UNSPECIFIED.);
#23789=B_SPLINE_CURVE_WITH_KNOTS('',3,(#146309,#146310,#146311,#146312,
#146313,#146314,#146315,#146316,#146317,#146318),.UNSPECIFIED.,.F.,.F.,
(4,2,2,2,4),(-0.678904072002962,-0.638811382083278,-0.567890404578545,-0.496948717476505,
-0.466428520787081),.UNSPECIFIED.);
#23790=B_SPLINE_CURVE_WITH_KNOTS('',3,(#146322,#146323,#146324,#146325,
#146326,#146327,#146328,#146329,#146330,#146331),.UNSPECIFIED.,.F.,.F.,
(4,2,2,2,4),(-0.678904071991591,-0.638811382082784,-0.567890404578999,-0.496948717477604,
-0.466428520798887),.UNSPECIFIED.);
#23791=B_SPLINE_CURVE_WITH_KNOTS('',3,(#146336,#146337,#146338,#146339,
#146340,#146341,#146342,#146343,#146344,#146345),.UNSPECIFIED.,.F.,.F.,
(4,2,2,2,4),(-0.678904071964557,-0.638811382077309,-0.567890404571244,-0.496948717468583,
-0.466428520811788),.UNSPECIFIED.);
#23792=B_SPLINE_CURVE_WITH_KNOTS('',3,(#146349,#146350,#146351,#146352,
#146353,#146354,#146355,#146356,#146357,#146358),.UNSPECIFIED.,.F.,.F.,
(4,2,2,2,4),(-0.678904071968788,-0.638811382079797,-0.567890404574743,-0.496948717472643,
-0.466428520813952),.UNSPECIFIED.);
#23793=B_SPLINE_CURVE_WITH_KNOTS('',3,(#146363,#146364,#146365,#146366,
#146367,#146368,#146369,#146370,#146371,#146372),.UNSPECIFIED.,.F.,.F.,
(4,2,2,2,4),(-0.678904071989876,-0.638811382082106,-0.567890404578026,-0.496948717476466,
-0.466428520798835),.UNSPECIFIED.);
#23794=B_SPLINE_CURVE_WITH_KNOTS('',3,(#146376,#146377,#146378,#146379,
#146380,#146381,#146382,#146383,#146384,#146385),.UNSPECIFIED.,.F.,.F.,
(4,2,2,2,4),(-0.678904072003597,-0.63881138208164,-0.567890404577412,-0.496948717475776,
-0.466428520791274),.UNSPECIFIED.);
#23795=B_SPLINE_CURVE_WITH_KNOTS('',3,(#146390,#146391,#146392,#146393,
#146394,#146395,#146396,#146397,#146398,#146399),.UNSPECIFIED.,.F.,.F.,
(4,2,2,2,4),(-0.678904071951742,-0.638811382079469,-0.567890404574304,-0.496948717472142,
-0.46642852083018),.UNSPECIFIED.);
#23796=B_SPLINE_CURVE_WITH_KNOTS('',3,(#146403,#146404,#146405,#146406,
#146407,#146408,#146409,#146410,#146411,#146412),.UNSPECIFIED.,.F.,.F.,
(4,2,2,2,4),(-0.678904071999128,-0.638811382080533,-0.567890404575816,-0.496948717473904,
-0.466428520785546),.UNSPECIFIED.);
#23797=B_SPLINE_CURVE_WITH_KNOTS('',3,(#146417,#146418,#146419,#146420,
#146421,#146422,#146423,#146424,#146425,#146426),.UNSPECIFIED.,.F.,.F.,
(4,2,2,2,4),(-0.678904071974422,-0.638811382079115,-0.567890404573812,-0.496948717471574,
-0.466428520806596),.UNSPECIFIED.);
#23798=B_SPLINE_CURVE_WITH_KNOTS('',3,(#146430,#146431,#146432,#146433,
#146434,#146435,#146436,#146437,#146438,#146439),.UNSPECIFIED.,.F.,.F.,
(4,2,2,2,4),(-0.678904071970067,-0.638811382078595,-0.567890404573052,-0.49694871747068,
-0.46642852080958),.UNSPECIFIED.);
#23799=B_SPLINE_CURVE_WITH_KNOTS('',3,(#146444,#146445,#146446,#146447,
#146448,#146449,#146450,#146451,#146452,#146453),.UNSPECIFIED.,.F.,.F.,
(4,2,2,2,4),(-0.678904071989481,-0.63881138208252,-0.567890404578625,-0.496948717477172,
-0.466428520800322),.UNSPECIFIED.);
#23800=B_SPLINE_CURVE_WITH_KNOTS('',3,(#146457,#146458,#146459,#146460,
#146461,#146462,#146463,#146464,#146465,#146466),.UNSPECIFIED.,.F.,.F.,
(4,2,2,2,4),(-0.678904071985814,-0.638811382083261,-0.567890404579705,-0.49694871747844,
-0.46642852080594),.UNSPECIFIED.);
#23801=B_SPLINE_CURVE_WITH_KNOTS('',3,(#146471,#146472,#146473,#146474,
#146475,#146476,#146477,#146478,#146479,#146480),.UNSPECIFIED.,.F.,.F.,
(4,2,2,2,4),(-0.678904071977239,-0.638811382076132,-0.567890404569544,-0.496948717466588,
-0.46642852081418),.UNSPECIFIED.);
#23802=B_SPLINE_CURVE_WITH_KNOTS('',3,(#146484,#146485,#146486,#146487,
#146488,#146489,#146490,#146491,#146492,#146493),.UNSPECIFIED.,.F.,.F.,
(4,2,2,2,4),(-0.678904071975199,-0.638811382077187,-0.567890404571049,-0.496948717468346,
-0.466428520800801),.UNSPECIFIED.);
#23803=B_SPLINE_CURVE_WITH_KNOTS('',3,(#146498,#146499,#146500,#146501,
#146502,#146503,#146504,#146505,#146506,#146507),.UNSPECIFIED.,.F.,.F.,
(4,2,2,2,4),(-0.678904071948059,-0.638811382083722,-0.567890404580332,-0.496948717479159,
-0.466428520818515),.UNSPECIFIED.);
#23804=B_SPLINE_CURVE_WITH_KNOTS('',3,(#146511,#146512,#146513,#146514,
#146515,#146516,#146517,#146518,#146519,#146520),.UNSPECIFIED.,.F.,.F.,
(4,2,2,2,4),(-0.678904071957727,-0.638811382077612,-0.567890404571677,-0.496948717469091,
-0.466428520789048),.UNSPECIFIED.);
#23805=B_SPLINE_CURVE_WITH_KNOTS('',3,(#146525,#146526,#146527,#146528,
#146529,#146530,#146531,#146532,#146533,#146534),.UNSPECIFIED.,.F.,.F.,
(4,2,2,2,4),(-0.678904071980107,-0.638811382084215,-0.567890404581017,-0.496948717479948,
-0.466428520814056),.UNSPECIFIED.);
#23806=B_SPLINE_CURVE_WITH_KNOTS('',3,(#146538,#146539,#146540,#146541,
#146542,#146543,#146544,#146545,#146546,#146547),.UNSPECIFIED.,.F.,.F.,
(4,2,2,2,4),(-0.678904071988661,-0.638811382083323,-0.567890404579782,-0.496948717478526,
-0.466428520803241),.UNSPECIFIED.);
#23807=B_SPLINE_CURVE_WITH_KNOTS('',3,(#146552,#146553,#146554,#146555,
#146556,#146557,#146558,#146559,#146560,#146561),.UNSPECIFIED.,.F.,.F.,
(4,2,2,2,4),(-0.678904071967123,-0.638811382077973,-0.567890404572164,-0.496948717469645,
-0.46642852080234),.UNSPECIFIED.);
#23808=B_SPLINE_CURVE_WITH_KNOTS('',3,(#146565,#146566,#146567,#146568,
#146569,#146570,#146571,#146572,#146573,#146574),.UNSPECIFIED.,.F.,.F.,
(4,2,2,2,4),(-0.678904071996527,-0.638811382080123,-0.567890404575202,-0.496948717473172,
-0.466428520787041),.UNSPECIFIED.);
#23809=B_SPLINE_CURVE_WITH_KNOTS('',3,(#146579,#146580,#146581,#146582,
#146583,#146584,#146585,#146586,#146587,#146588),.UNSPECIFIED.,.F.,.F.,
(4,2,2,2,4),(-0.678904071994029,-0.638811382081138,-0.567890404576668,-0.496948717474894,
-0.4664285208321),.UNSPECIFIED.);
#23810=B_SPLINE_CURVE_WITH_KNOTS('',3,(#146592,#146593,#146594,#146595,
#146596,#146597,#146598,#146599,#146600,#146601),.UNSPECIFIED.,.F.,.F.,
(4,2,2,2,4),(-0.678904071987538,-0.638811382080587,-0.567890404575871,-0.496948717473957,
-0.466428520797245),.UNSPECIFIED.);
#23811=B_SPLINE_CURVE_WITH_KNOTS('',3,(#146606,#146607,#146608,#146609,
#146610,#146611,#146612,#146613,#146614,#146615),.UNSPECIFIED.,.F.,.F.,
(4,2,2,2,4),(-0.678904071998108,-0.638811382080726,-0.567890404576086,-0.496948717474218,
-0.466428520787065),.UNSPECIFIED.);
#23812=B_SPLINE_CURVE_WITH_KNOTS('',3,(#146619,#146620,#146621,#146622,
#146623,#146624,#146625,#146626,#146627,#146628),.UNSPECIFIED.,.F.,.F.,
(4,2,2,2,4),(-0.678904071979078,-0.638811382081879,-0.567890404577713,-0.496948717476107,
-0.466428520806676),.UNSPECIFIED.);
#23813=B_SPLINE_CURVE_WITH_KNOTS('',3,(#146633,#146634,#146635,#146636,
#146637,#146638,#146639,#146640,#146641,#146642),.UNSPECIFIED.,.F.,.F.,
(4,2,2,2,4),(-0.678904072012607,-0.638811382080162,-0.567890404575286,-0.496948717473285,
-0.466428520771103),.UNSPECIFIED.);
#23814=B_SPLINE_CURVE_WITH_KNOTS('',3,(#146646,#146647,#146648,#146649,
#146650,#146651,#146652,#146653,#146654,#146655),.UNSPECIFIED.,.F.,.F.,
(4,2,2,2,4),(-0.678904071978783,-0.638811382085326,-0.5678904045826,-0.496948717481796,
-0.466428520818266),.UNSPECIFIED.);
#23815=B_SPLINE_CURVE_WITH_KNOTS('',3,(#146660,#146661,#146662,#146663,
#146664,#146665,#146666,#146667,#146668,#146669),.UNSPECIFIED.,.F.,.F.,
(4,2,2,2,4),(-0.678904071984418,-0.638811382077011,-0.567890404570846,-0.496948717468133,
-0.466428520791198),.UNSPECIFIED.);
#23816=B_SPLINE_CURVE_WITH_KNOTS('',3,(#146673,#146674,#146675,#146676,
#146677,#146678,#146679,#146680,#146681,#146682),.UNSPECIFIED.,.F.,.F.,
(4,2,2,2,4),(-0.678904072001018,-0.638811382081384,-0.567890404576977,-0.496948717475233,
-0.466428520835578),.UNSPECIFIED.);
#23817=B_SPLINE_CURVE_WITH_KNOTS('',3,(#146687,#146688,#146689,#146690,
#146691,#146692,#146693,#146694,#146695,#146696),.UNSPECIFIED.,.F.,.F.,
(4,2,2,2,4),(-0.678904071963263,-0.638811382080034,-0.567890404575033,-0.496948717472957,
-0.466428520820018),.UNSPECIFIED.);
#23818=B_SPLINE_CURVE_WITH_KNOTS('',3,(#146700,#146701,#146702,#146703,
#146704,#146705,#146706,#146707,#146708,#146709),.UNSPECIFIED.,.F.,.F.,
(4,2,2,2,4),(-0.678904071978785,-0.63881138208184,-0.567890404577665,-0.496948717476054,
-0.466428520809261),.UNSPECIFIED.);
#23819=B_SPLINE_CURVE_WITH_KNOTS('',3,(#146714,#146715,#146716,#146717,
#146718,#146719,#146720,#146721,#146722,#146723),.UNSPECIFIED.,.F.,.F.,
(4,2,2,2,4),(-0.678904071979651,-0.638811382078958,-0.567890404573559,-0.496948717471267,
-0.466428520800927),.UNSPECIFIED.);
#23820=B_SPLINE_CURVE_WITH_KNOTS('',3,(#146727,#146728,#146729,#146730,
#146731,#146732,#146733,#146734,#146735,#146736),.UNSPECIFIED.,.F.,.F.,
(4,2,2,2,4),(-0.678904071992989,-0.638811382079457,-0.567890404574321,-0.496948717472181,
-0.46642852078896),.UNSPECIFIED.);
#23821=B_SPLINE_CURVE_WITH_KNOTS('',3,(#146741,#146742,#146743,#146744,
#146745,#146746,#146747,#146748,#146749,#146750),.UNSPECIFIED.,.F.,.F.,
(4,2,2,2,4),(-0.67890407199661,-0.638811382082501,-0.567890404578577,-0.496948717477103,
-0.466428520807697),.UNSPECIFIED.);
#23822=B_SPLINE_CURVE_WITH_KNOTS('',3,(#146754,#146755,#146756,#146757,
#146758,#146759,#146760,#146761,#146762,#146763),.UNSPECIFIED.,.F.,.F.,
(4,2,2,2,4),(-0.678904071992571,-0.638811382080303,-0.567890404575509,-0.496948717473556,
-0.466428520781529),.UNSPECIFIED.);
#23823=B_SPLINE_CURVE_WITH_KNOTS('',3,(#146768,#146769,#146770,#146771,
#146772,#146773,#146774,#146775,#146776,#146777),.UNSPECIFIED.,.F.,.F.,
(4,2,2,2,4),(-0.678904071957711,-0.63881138208108,-0.567890404576584,-0.496948717474795,
-0.466428520828368),.UNSPECIFIED.);
#23824=B_SPLINE_CURVE_WITH_KNOTS('',3,(#146781,#146782,#146783,#146784,
#146785,#146786,#146787,#146788,#146789,#146790),.UNSPECIFIED.,.F.,.F.,
(4,2,2,2,4),(-0.678904071955128,-0.638811382079591,-0.567890404574442,-0.496948717472286,
-0.466428520827057),.UNSPECIFIED.);
#23825=B_SPLINE_CURVE_WITH_KNOTS('',3,(#146795,#146796,#146797,#146798,
#146799,#146800,#146801,#146802,#146803,#146804),.UNSPECIFIED.,.F.,.F.,
(4,2,2,2,4),(-0.67890407196334,-0.638811382080692,-0.567890404576,-0.496948717474097,
-0.466428520821681),.UNSPECIFIED.);
#23826=B_SPLINE_CURVE_WITH_KNOTS('',3,(#146808,#146809,#146810,#146811,
#146812,#146813,#146814,#146815,#146816,#146817),.UNSPECIFIED.,.F.,.F.,
(4,2,2,2,4),(-0.678904071975058,-0.638811382079965,-0.567890404575,-0.49694871747295,
-0.466428520808137),.UNSPECIFIED.);
#23827=B_SPLINE_CURVE_WITH_KNOTS('',3,(#146822,#146823,#146824,#146825,
#146826,#146827,#146828,#146829,#146830,#146831),.UNSPECIFIED.,.F.,.F.,
(4,2,2,2,4),(-0.678904071975006,-0.638811382079877,-0.567890404574935,-0.496948717472904,
-0.46642852080805),.UNSPECIFIED.);
#23828=B_SPLINE_CURVE_WITH_KNOTS('',3,(#146835,#146836,#146837,#146838,
#146839,#146840,#146841,#146842,#146843,#146844),.UNSPECIFIED.,.F.,.F.,
(4,2,2,2,4),(-0.678904071966622,-0.638811382082333,-0.567890404578333,-0.496948717476817,
-0.46642852082266),.UNSPECIFIED.);
#23829=B_SPLINE_CURVE_WITH_KNOTS('',3,(#146849,#146850,#146851,#146852,
#146853,#146854,#146855,#146856,#146857,#146858),.UNSPECIFIED.,.F.,.F.,
(4,2,2,2,4),(-0.678904071957464,-0.638811382081058,-0.567890404576504,-0.496948717474678,
-0.46642852082849),.UNSPECIFIED.);
#23830=B_SPLINE_CURVE_WITH_KNOTS('',3,(#146862,#146863,#146864,#146865,
#146866,#146867,#146868,#146869,#146870,#146871),.UNSPECIFIED.,.F.,.F.,
(4,2,2,2,4),(-0.678904071960602,-0.63881138208236,-0.567890404578389,-0.496948717476892,
-0.466428520828773),.UNSPECIFIED.);
#23831=B_SPLINE_CURVE_WITH_KNOTS('',3,(#146876,#146877,#146878,#146879,
#146880,#146881,#146882,#146883,#146884,#146885),.UNSPECIFIED.,.F.,.F.,
(4,2,2,2,4),(-0.678904071989264,-0.638811382079008,-0.567890404573618,-0.496948717471328,
-0.466428520791417),.UNSPECIFIED.);
#23832=B_SPLINE_CURVE_WITH_KNOTS('',3,(#146889,#146890,#146891,#146892,
#146893,#146894,#146895,#146896,#146897,#146898),.UNSPECIFIED.,.F.,.F.,
(4,2,2,2,4),(-0.678904071984124,-0.638811382082578,-0.567890404578774,-0.496948717477375,
-0.46642852080592),.UNSPECIFIED.);
#23833=B_SPLINE_CURVE_WITH_KNOTS('',3,(#146903,#146904,#146905,#146906,
#146907,#146908,#146909,#146910,#146911,#146912),.UNSPECIFIED.,.F.,.F.,
(4,2,2,2,4),(-0.678904071990912,-0.638811382078438,-0.567890404572854,-0.496948717470463,
-0.466428520788367),.UNSPECIFIED.);
#23834=B_SPLINE_CURVE_WITH_KNOTS('',3,(#146916,#146917,#146918,#146919,
#146920,#146921,#146922,#146923,#146924,#146925),.UNSPECIFIED.,.F.,.F.,
(4,2,2,2,4),(-0.67890407197895,-0.63881138207865,-0.567890404573101,-0.496948717470721,
-0.466428520800793),.UNSPECIFIED.);
#23835=B_SPLINE_CURVE_WITH_KNOTS('',3,(#146930,#146931,#146932,#146933,
#146934,#146935,#146936,#146937,#146938,#146939),.UNSPECIFIED.,.F.,.F.,
(4,2,2,2,4),(-0.67890407197844,-0.638811382081603,-0.567890404577301,-0.496948717475618,
-0.46642852078939),.UNSPECIFIED.);
#23836=B_SPLINE_CURVE_WITH_KNOTS('',3,(#146943,#146944,#146945,#146946,
#146947,#146948,#146949,#146950,#146951,#146952),.UNSPECIFIED.,.F.,.F.,
(4,2,2,2,4),(-0.678904071962693,-0.638811382079039,-0.567890404573721,-0.496948717471478,
-0.466428520818159),.UNSPECIFIED.);
#23837=B_SPLINE_CURVE_WITH_KNOTS('',3,(#146957,#146958,#146959,#146960,
#146961,#146962,#146963,#146964,#146965,#146966),.UNSPECIFIED.,.F.,.F.,
(4,2,2,2,4),(-0.678904071951875,-0.638811382081886,-0.56789040457777,-0.496948717476197,
-0.466428520836353),.UNSPECIFIED.);
#23838=B_SPLINE_CURVE_WITH_KNOTS('',3,(#146970,#146971,#146972,#146973,
#146974,#146975,#146976,#146977,#146978,#146979),.UNSPECIFIED.,.F.,.F.,
(4,2,2,2,4),(-0.678904071984224,-0.638811382077184,-0.567890404571044,-0.496948717468341,
-0.466428520791771),.UNSPECIFIED.);
#23839=B_SPLINE_CURVE_WITH_KNOTS('',3,(#146984,#146985,#146986,#146987,
#146988,#146989,#146990,#146991,#146992,#146993),.UNSPECIFIED.,.F.,.F.,
(4,2,2,2,4),(-0.678904071946679,-0.638811382083566,-0.567890404580102,-0.496948717478886,
-0.466428520817321),.UNSPECIFIED.);
#23840=B_SPLINE_CURVE_WITH_KNOTS('',3,(#146997,#146998,#146999,#147000,
#147001,#147002,#147003,#147004,#147005,#147006),.UNSPECIFIED.,.F.,.F.,
(4,2,2,2,4),(-0.678904071981425,-0.638811382080321,-0.567890404575443,-0.496948717473436,
-0.4664285208026),.UNSPECIFIED.);
#23841=B_SPLINE_CURVE_WITH_KNOTS('',3,(#147011,#147012,#147013,#147014,
#147015,#147016,#147017,#147018,#147019,#147020),.UNSPECIFIED.,.F.,.F.,
(4,2,2,2,4),(-0.678904071991316,-0.638811382081223,-0.567890404576789,-0.496948717475035,
-0.466428520807192),.UNSPECIFIED.);
#23842=B_SPLINE_CURVE_WITH_KNOTS('',3,(#147024,#147025,#147026,#147027,
#147028,#147029,#147030,#147031,#147032,#147033),.UNSPECIFIED.,.F.,.F.,
(4,2,2,2,4),(-0.678904071999418,-0.638811382081107,-0.567890404576574,-0.496948717474759,
-0.466428520786662),.UNSPECIFIED.);
#23843=B_SPLINE_CURVE_WITH_KNOTS('',3,(#147038,#147039,#147040,#147041,
#147042,#147043,#147044,#147045,#147046,#147047),.UNSPECIFIED.,.F.,.F.,
(4,2,2,2,4),(-0.678904071986371,-0.63881138208026,-0.567890404575494,-0.496948717473567,
-0.466428520797708),.UNSPECIFIED.);
#23844=B_SPLINE_CURVE_WITH_KNOTS('',3,(#147051,#147052,#147053,#147054,
#147055,#147056,#147057,#147058,#147059,#147060),.UNSPECIFIED.,.F.,.F.,
(4,2,2,2,4),(-0.678904071955908,-0.638811382081694,-0.56789040457745,-0.496948717475802,
-0.466428520793422),.UNSPECIFIED.);
#23845=B_SPLINE_CURVE_WITH_KNOTS('',3,(#147065,#147066,#147067,#147068,
#147069,#147070,#147071,#147072,#147073,#147074),.UNSPECIFIED.,.F.,.F.,
(4,2,2,2,4),(-0.678904071995711,-0.638811382080074,-0.567890404575169,-0.496948717473153,
-0.466428520827868),.UNSPECIFIED.);
#23846=B_SPLINE_CURVE_WITH_KNOTS('',3,(#147078,#147079,#147080,#147081,
#147082,#147083,#147084,#147085,#147086,#147087),.UNSPECIFIED.,.F.,.F.,
(4,2,2,2,4),(-0.6789040719681,-0.638811382078021,-0.567890404572175,-0.496948717469627,
-0.466428520809968),.UNSPECIFIED.);
#23847=B_SPLINE_CURVE_WITH_KNOTS('',3,(#147092,#147093,#147094,#147095,
#147096,#147097,#147098,#147099,#147100,#147101),.UNSPECIFIED.,.F.,.F.,
(4,2,2,2,4),(-0.678904071991019,-0.638811382084413,-0.567890404581332,-0.496948717480334,
-0.466428520838104),.UNSPECIFIED.);
#23848=B_SPLINE_CURVE_WITH_KNOTS('',3,(#147105,#147106,#147107,#147108,
#147109,#147110,#147111,#147112,#147113,#147114),.UNSPECIFIED.,.F.,.F.,
(4,2,2,2,4),(-0.678904072013258,-0.638811382084341,-0.567890404581218,-0.496948717480194,
-0.466428520827364),.UNSPECIFIED.);
#23849=B_SPLINE_CURVE_WITH_KNOTS('',3,(#147119,#147120,#147121,#147122,
#147123,#147124,#147125,#147126,#147127,#147128),.UNSPECIFIED.,.F.,.F.,
(4,2,2,2,4),(-0.678904071985943,-0.638811382076362,-0.567890404569934,-0.496948717467075,
-0.466428520788006),.UNSPECIFIED.);
#23850=B_SPLINE_CURVE_WITH_KNOTS('',3,(#147132,#147133,#147134,#147135,
#147136,#147137,#147138,#147139,#147140,#147141),.UNSPECIFIED.,.F.,.F.,
(4,2,2,2,4),(-0.678904071993597,-0.63881138208345,-0.567890404579917,-0.49694871747866,
-0.466428520817712),.UNSPECIFIED.);
#23851=B_SPLINE_CURVE_WITH_KNOTS('',3,(#147146,#147147,#147148,#147149,
#147150,#147151,#147152,#147153,#147154,#147155),.UNSPECIFIED.,.F.,.F.,
(4,2,2,2,4),(-0.678904071973235,-0.638811382076413,-0.567890404569979,-0.496948717467112,
-0.466428520774701),.UNSPECIFIED.);
#23852=B_SPLINE_CURVE_WITH_KNOTS('',3,(#147159,#147160,#147161,#147162,
#147163,#147164,#147165,#147166,#147167,#147168),.UNSPECIFIED.,.F.,.F.,
(4,2,2,2,4),(-0.67890407198703,-0.638811382078511,-0.567890404572937,-0.496948717470548,
-0.46642852084323),.UNSPECIFIED.);
#23853=B_SPLINE_CURVE_WITH_KNOTS('',3,(#147173,#147174,#147175,#147176,
#147177,#147178,#147179,#147180,#147181,#147182),.UNSPECIFIED.,.F.,.F.,
(4,2,2,2,4),(-0.678904071987918,-0.63881138208419,-0.567890404580971,-0.496948717479887,
-0.466428520806156),.UNSPECIFIED.);
#23854=B_SPLINE_CURVE_WITH_KNOTS('',3,(#147186,#147187,#147188,#147189,
#147190,#147191,#147192,#147193,#147194,#147195),.UNSPECIFIED.,.F.,.F.,
(4,2,2,2,4),(-0.678904072009243,-0.638811382083172,-0.567890404579565,-0.496948717478273,
-0.466428520834842),.UNSPECIFIED.);
#23855=B_SPLINE_CURVE_WITH_KNOTS('',3,(#147200,#147201,#147202,#147203,
#147204,#147205,#147206,#147207,#147208,#147209),.UNSPECIFIED.,.F.,.F.,
(4,2,2,2,4),(-0.678904071972171,-0.638811382079603,-0.567890404574478,-0.496948717472339,
-0.466428520810079),.UNSPECIFIED.);
#23856=B_SPLINE_CURVE_WITH_KNOTS('',3,(#147213,#147214,#147215,#147216,
#147217,#147218,#147219,#147220,#147221,#147222),.UNSPECIFIED.,.F.,.F.,
(4,2,2,2,4),(-0.67890407197948,-0.63881138208111,-0.567890404576586,-0.496948717474778,
-0.466428520794178),.UNSPECIFIED.);
#23857=B_SPLINE_CURVE_WITH_KNOTS('',3,(#147227,#147228,#147229,#147230,
#147231,#147232,#147233,#147234,#147235,#147236),.UNSPECIFIED.,.F.,.F.,
(4,2,2,2,4),(-0.67890407199919,-0.638811382081417,-0.567890404577054,-0.496948717475335,
-0.466428520787747),.UNSPECIFIED.);
#23858=B_SPLINE_CURVE_WITH_KNOTS('',3,(#147240,#147241,#147242,#147243,
#147244,#147245,#147246,#147247,#147248,#147249),.UNSPECIFIED.,.F.,.F.,
(4,2,2,2,4),(-0.678904071953487,-0.638811382080193,-0.567890404575326,-0.496948717473333,
-0.466428520830309),.UNSPECIFIED.);
#23859=B_SPLINE_CURVE_WITH_KNOTS('',3,(#147254,#147255,#147256,#147257,
#147258,#147259,#147260,#147261,#147262,#147263),.UNSPECIFIED.,.F.,.F.,
(4,2,2,2,4),(-0.678904072000796,-0.638811382081297,-0.567890404576874,-0.496948717475125,
-0.466428520785821),.UNSPECIFIED.);
#23860=B_SPLINE_CURVE_WITH_KNOTS('',3,(#147267,#147268,#147269,#147270,
#147271,#147272,#147273,#147274,#147275,#147276),.UNSPECIFIED.,.F.,.F.,
(4,2,2,2,4),(-0.678904071991668,-0.638811382082854,-0.567890404579058,-0.496948717477653,
-0.466428520798932),.UNSPECIFIED.);
#23861=B_SPLINE_CURVE_WITH_KNOTS('',3,(#147281,#147282,#147283,#147284,
#147285,#147286,#147287,#147288,#147289,#147290),.UNSPECIFIED.,.F.,.F.,
(4,2,2,2,4),(-0.678904071964471,-0.638811382077228,-0.567890404571169,-0.496948717468516,
-0.466428520811726),.UNSPECIFIED.);
#23862=B_SPLINE_CURVE_WITH_KNOTS('',3,(#147294,#147295,#147296,#147297,
#147298,#147299,#147300,#147301,#147302,#147303),.UNSPECIFIED.,.F.,.F.,
(4,2,2,2,4),(-0.678904071968841,-0.638811382079846,-0.567890404574781,-0.496948717472671,
-0.466428520813977),.UNSPECIFIED.);
#23863=B_SPLINE_CURVE_WITH_KNOTS('',3,(#147308,#147309,#147310,#147311,
#147312,#147313,#147314,#147315,#147316,#147317),.UNSPECIFIED.,.F.,.F.,
(4,2,2,2,4),(-0.678904071990042,-0.638811382082262,-0.567890404578158,-0.496948717476576,
-0.466428520798937),.UNSPECIFIED.);
#23864=B_SPLINE_CURVE_WITH_KNOTS('',3,(#147321,#147322,#147323,#147324,
#147325,#147326,#147327,#147328,#147329,#147330),.UNSPECIFIED.,.F.,.F.,
(4,2,2,2,4),(-0.678904072003725,-0.638811382081756,-0.567890404577507,-0.496948717475853,
-0.466428520791346),.UNSPECIFIED.);
#23865=B_SPLINE_CURVE_WITH_KNOTS('',3,(#147335,#147336,#147337,#147338,
#147339,#147340,#147341,#147342,#147343,#147344),.UNSPECIFIED.,.F.,.F.,
(4,2,2,2,4),(-0.678904071951667,-0.638811382079402,-0.567890404574249,-0.4969487174721,
-0.466428520830143),.UNSPECIFIED.);
#23866=B_SPLINE_CURVE_WITH_KNOTS('',3,(#147348,#147349,#147350,#147351,
#147352,#147353,#147354,#147355,#147356,#147357),.UNSPECIFIED.,.F.,.F.,
(4,2,2,2,4),(-0.678904071999203,-0.638811382080604,-0.567890404575878,-0.496948717473956,
-0.466428520785595),.UNSPECIFIED.);
#23867=B_SPLINE_CURVE_WITH_KNOTS('',3,(#147362,#147363,#147364,#147365,
#147366,#147367,#147368,#147369,#147370,#147371),.UNSPECIFIED.,.F.,.F.,
(4,2,2,2,4),(-0.678904071974462,-0.638811382079151,-0.567890404573839,-0.496948717471593,
-0.466428520806612),.UNSPECIFIED.);
#23868=B_SPLINE_CURVE_WITH_KNOTS('',3,(#147375,#147376,#147377,#147378,
#147379,#147380,#147381,#147382,#147383,#147384),.UNSPECIFIED.,.F.,.F.,
(4,2,2,2,4),(-0.678904071970275,-0.638811382078786,-0.567890404573214,-0.496948717470815,
-0.466428520809705),.UNSPECIFIED.);
#23869=B_SPLINE_CURVE_WITH_KNOTS('',3,(#147389,#147390,#147391,#147392,
#147393,#147394,#147395,#147396,#147397,#147398),.UNSPECIFIED.,.F.,.F.,
(4,2,2,2,4),(-0.678904071989522,-0.638811382082555,-0.567890404578647,-0.496948717477185,
-0.466428520800335),.UNSPECIFIED.);
#23870=B_SPLINE_CURVE_WITH_KNOTS('',3,(#147402,#147403,#147404,#147405,
#147406,#147407,#147408,#147409,#147410,#147411),.UNSPECIFIED.,.F.,.F.,
(4,2,2,2,4),(-0.678904071985921,-0.638811382083359,-0.56789040457979,-0.496948717478515,
-0.466428520806011),.UNSPECIFIED.);
#23871=B_SPLINE_CURVE_WITH_KNOTS('',3,(#147416,#147417,#147418,#147419,
#147420,#147421,#147422,#147423,#147424,#147425),.UNSPECIFIED.,.F.,.F.,
(4,2,2,2,4),(-0.678904071977173,-0.63881138207607,-0.567890404569492,-0.496948717466546,
-0.466428520814141),.UNSPECIFIED.);
#23872=B_SPLINE_CURVE_WITH_KNOTS('',3,(#147429,#147430,#147431,#147432,
#147433,#147434,#147435,#147436,#147437,#147438),.UNSPECIFIED.,.F.,.F.,
(4,2,2,2,4),(-0.678904071975169,-0.63881138207716,-0.567890404571027,-0.496948717468329,
-0.466428520800785),.UNSPECIFIED.);
#23873=B_SPLINE_CURVE_WITH_KNOTS('',3,(#147443,#147444,#147445,#147446,
#147447,#147448,#147449,#147450,#147451,#147452),.UNSPECIFIED.,.F.,.F.,
(4,2,2,2,4),(-0.67890407194793,-0.638811382083603,-0.567890404580231,-0.496948717479076,
-0.466428520818441),.UNSPECIFIED.);
#23874=B_SPLINE_CURVE_WITH_KNOTS('',3,(#147456,#147457,#147458,#147459,
#147460,#147461,#147462,#147463,#147464,#147465),.UNSPECIFIED.,.F.,.F.,
(4,2,2,2,4),(-0.678904071957711,-0.638811382077597,-0.567890404571664,-0.496948717469078,
-0.466428520789034),.UNSPECIFIED.);
#23875=B_SPLINE_CURVE_WITH_KNOTS('',3,(#147470,#147471,#147472,#147473,
#147474,#147475,#147476,#147477,#147478,#147479),.UNSPECIFIED.,.F.,.F.,
(4,2,2,2,4),(-0.678904071980114,-0.638811382084221,-0.567890404581019,-0.496948717479949,
-0.46642852081406),.UNSPECIFIED.);
#23876=B_SPLINE_CURVE_WITH_KNOTS('',3,(#147483,#147484,#147485,#147486,
#147487,#147488,#147489,#147490,#147491,#147492),.UNSPECIFIED.,.F.,.F.,
(4,2,2,2,4),(-0.678904071988688,-0.638811382083351,-0.567890404579804,-0.496948717478542,
-0.466428520803256),.UNSPECIFIED.);
#23877=B_SPLINE_CURVE_WITH_KNOTS('',3,(#147497,#147498,#147499,#147500,
#147501,#147502,#147503,#147504,#147505,#147506),.UNSPECIFIED.,.F.,.F.,
(4,2,2,2,4),(-0.678904071967103,-0.638811382077954,-0.567890404572145,-0.496948717469628,
-0.466428520802325),.UNSPECIFIED.);
#23878=B_SPLINE_CURVE_WITH_KNOTS('',3,(#147510,#147511,#147512,#147513,
#147514,#147515,#147516,#147517,#147518,#147519),.UNSPECIFIED.,.F.,.F.,
(4,2,2,2,4),(-0.678904071996367,-0.638811382079977,-0.567890404575077,-0.496948717473068,
-0.466428520786947),.UNSPECIFIED.);
#23879=B_SPLINE_CURVE_WITH_KNOTS('',3,(#147524,#147525,#147526,#147527,
#147528,#147529,#147530,#147531,#147532,#147533),.UNSPECIFIED.,.F.,.F.,
(4,2,2,2,4),(-0.678904071994096,-0.6388113820812,-0.567890404576721,-0.496948717474939,
-0.466428520832143),.UNSPECIFIED.);
#23880=B_SPLINE_CURVE_WITH_KNOTS('',3,(#147537,#147538,#147539,#147540,
#147541,#147542,#147543,#147544,#147545,#147546),.UNSPECIFIED.,.F.,.F.,
(4,2,2,2,4),(-0.678904071987513,-0.638811382080565,-0.567890404575855,-0.496948717473948,
-0.46642852079724),.UNSPECIFIED.);
#23881=B_SPLINE_CURVE_WITH_KNOTS('',3,(#147551,#147552,#147553,#147554,
#147555,#147556,#147557,#147558,#147559,#147560),.UNSPECIFIED.,.F.,.F.,
(4,2,2,2,4),(-0.678904071998105,-0.638811382080726,-0.567890404576089,-0.496948717474222,
-0.466428520787071),.UNSPECIFIED.);
#23882=B_SPLINE_CURVE_WITH_KNOTS('',3,(#147564,#147565,#147566,#147567,
#147568,#147569,#147570,#147571,#147572,#147573),.UNSPECIFIED.,.F.,.F.,
(4,2,2,2,4),(-0.678904071978989,-0.6388113820818,-0.567890404577646,-0.496948717476053,
-0.466428520806628),.UNSPECIFIED.);
#23883=B_SPLINE_CURVE_WITH_KNOTS('',3,(#147578,#147579,#147580,#147581,
#147582,#147583,#147584,#147585,#147586,#147587),.UNSPECIFIED.,.F.,.F.,
(4,2,2,2,4),(-0.678904072012599,-0.638811382080154,-0.56789040457528,-0.496948717473282,
-0.466428520771101),.UNSPECIFIED.);
#23884=B_SPLINE_CURVE_WITH_KNOTS('',3,(#147591,#147592,#147593,#147594,
#147595,#147596,#147597,#147598,#147599,#147600),.UNSPECIFIED.,.F.,.F.,
(4,2,2,2,4),(-0.678904071978745,-0.638811382085293,-0.567890404582573,-0.496948717481774,
-0.466428520818246),.UNSPECIFIED.);
#23885=B_SPLINE_CURVE_WITH_KNOTS('',3,(#147605,#147606,#147607,#147608,
#147609,#147610,#147611,#147612,#147613,#147614),.UNSPECIFIED.,.F.,.F.,
(4,2,2,2,4),(-0.678904071984472,-0.638811382077059,-0.567890404570888,-0.496948717468167,
-0.466428520791229),.UNSPECIFIED.);
#23886=B_SPLINE_CURVE_WITH_KNOTS('',3,(#147618,#147619,#147620,#147621,
#147622,#147623,#147624,#147625,#147626,#147627),.UNSPECIFIED.,.F.,.F.,
(4,2,2,2,4),(-0.678904072000963,-0.638811382081332,-0.567890404576933,-0.496948717475197,
-0.466428520835545),.UNSPECIFIED.);
#23887=B_SPLINE_CURVE_WITH_KNOTS('',3,(#147632,#147633,#147634,#147635,
#147636,#147637,#147638,#147639,#147640,#147641),.UNSPECIFIED.,.F.,.F.,
(4,2,2,2,4),(-0.678904071963139,-0.63881138207992,-0.567890404574934,-0.496948717472875,
-0.466428520819943),.UNSPECIFIED.);
#23888=B_SPLINE_CURVE_WITH_KNOTS('',3,(#147645,#147646,#147647,#147648,
#147649,#147650,#147651,#147652,#147653,#147654),.UNSPECIFIED.,.F.,.F.,
(4,2,2,2,4),(-0.678904071978786,-0.638811382081839,-0.567890404577663,-0.496948717476051,
-0.466428520809257),.UNSPECIFIED.);
#23889=B_SPLINE_CURVE_WITH_KNOTS('',3,(#147659,#147660,#147661,#147662,
#147663,#147664,#147665,#147666,#147667,#147668),.UNSPECIFIED.,.F.,.F.,
(4,2,2,2,4),(-0.678904071979581,-0.638811382078899,-0.567890404573514,-0.496948717471234,
-0.466428520800896),.UNSPECIFIED.);
#23890=B_SPLINE_CURVE_WITH_KNOTS('',3,(#147672,#147673,#147674,#147675,
#147676,#147677,#147678,#147679,#147680,#147681),.UNSPECIFIED.,.F.,.F.,
(4,2,2,2,4),(-0.6789040719931,-0.638811382079555,-0.567890404574399,-0.496948717472244,
-0.466428520789016),.UNSPECIFIED.);
#23891=B_SPLINE_CURVE_WITH_KNOTS('',3,(#147686,#147687,#147688,#147689,
#147690,#147691,#147692,#147693,#147694,#147695),.UNSPECIFIED.,.F.,.F.,
(4,2,2,2,4),(-0.678904071996576,-0.63881138208247,-0.567890404578552,-0.496948717477086,
-0.466428520807683),.UNSPECIFIED.);
#23892=B_SPLINE_CURVE_WITH_KNOTS('',3,(#147699,#147700,#147701,#147702,
#147703,#147704,#147705,#147706,#147707,#147708),.UNSPECIFIED.,.F.,.F.,
(4,2,2,2,4),(-0.678904071992612,-0.638811382080339,-0.567890404575539,-0.496948717473582,
-0.466428520781553),.UNSPECIFIED.);
#23893=B_SPLINE_CURVE_WITH_KNOTS('',3,(#147713,#147714,#147715,#147716,
#147717,#147718,#147719,#147720,#147721,#147722),.UNSPECIFIED.,.F.,.F.,
(4,2,2,2,4),(-0.678904071957699,-0.638811382081068,-0.567890404576578,-0.496948717474793,
-0.466428520828367),.UNSPECIFIED.);
#23894=B_SPLINE_CURVE_WITH_KNOTS('',3,(#147726,#147727,#147728,#147729,
#147730,#147731,#147732,#147733,#147734,#147735),.UNSPECIFIED.,.F.,.F.,
(4,2,2,2,4),(-0.678904071955071,-0.638811382079537,-0.567890404574392,-0.496948717472241,
-0.466428520827014),.UNSPECIFIED.);
#23895=B_SPLINE_CURVE_WITH_KNOTS('',3,(#147740,#147741,#147742,#147743,
#147744,#147745,#147746,#147747,#147748,#147749),.UNSPECIFIED.,.F.,.F.,
(4,2,2,2,4),(-0.678904071963275,-0.638811382080631,-0.567890404575947,-0.496948717474053,
-0.466428520821643),.UNSPECIFIED.);
#23896=B_SPLINE_CURVE_WITH_KNOTS('',3,(#147753,#147754,#147755,#147756,
#147757,#147758,#147759,#147760,#147761,#147762),.UNSPECIFIED.,.F.,.F.,
(4,2,2,2,4),(-0.678904071975039,-0.638811382079947,-0.567890404574985,-0.496948717472938,
-0.466428520808125),.UNSPECIFIED.);
#23897=B_SPLINE_CURVE_WITH_KNOTS('',3,(#147829,#147830,#147831,#147832,
#147833,#147834,#147835,#147836,#147837,#147838,#147839,#147840,#147841,
#147842,#147843,#147844,#147845),.UNSPECIFIED.,.F.,.F.,(4,2,2,3,2,2,2,4),
(-0.0105482508477054,-0.00774017959540533,-0.00385609988520743,0.,0.00219233319325163,
0.00438738203112965,0.0083182289718649,0.0105383937687012),
 .UNSPECIFIED.);
#23898=B_SPLINE_CURVE_WITH_KNOTS('',3,(#147846,#147847,#147848,#147849),
 .UNSPECIFIED.,.F.,.F.,(4,4),(2.06733813101515,2.11814920351283),
 .UNSPECIFIED.);
#23899=B_SPLINE_CURVE_WITH_KNOTS('',3,(#147851,#147852,#147853,#147854),
 .UNSPECIFIED.,.F.,.F.,(4,4),(3.73816266103403,3.78897373354396),
 .UNSPECIFIED.);
#23900=B_SPLINE_CURVE_WITH_KNOTS('',3,(#147856,#147857,#147858,#147859,
#147860,#147861,#147862,#147863,#147864,#147865,#147866,#147867,#147868,
#147869,#147870,#147871,#147872),.UNSPECIFIED.,.F.,.F.,(4,2,2,2,3,2,2,4),
(0.0529024353036734,0.0551226000958153,0.0590534470366397,0.0612484958745396,
0.0634408290678051,0.0672969289529751,0.0711810086631009,0.0739890798907039),
 .UNSPECIFIED.);
#23901=B_SPLINE_CURVE_WITH_KNOTS('',3,(#147873,#147874,#147875,#147876),
 .UNSPECIFIED.,.F.,.F.,(4,4),(2.06733813100459,2.11814920352257),
 .UNSPECIFIED.);
#23902=B_SPLINE_CURVE_WITH_KNOTS('',3,(#147878,#147879,#147880,#147881),
 .UNSPECIFIED.,.F.,.F.,(4,4),(3.73816266106249,3.78897373354877),
 .UNSPECIFIED.);
#23903=B_SPLINE_CURVE_WITH_KNOTS('',3,(#147883,#147884,#147885,#147886,
#147887,#147888,#147889,#147890,#147891,#147892,#147893,#147894,#147895,
#147896,#147897,#147898,#147899),.UNSPECIFIED.,.F.,.F.,(4,2,2,2,3,2,2,4),
(0.0529024352792957,0.0551226000955082,0.0590534470363172,0.0612484958742291,
0.0634408290675084,0.067296928952713,0.0711810086628562,0.0739890798962668),
 .UNSPECIFIED.);
#23904=B_SPLINE_CURVE_WITH_KNOTS('',3,(#147900,#147901,#147902,#147903),
 .UNSPECIFIED.,.F.,.F.,(4,4),(2.06733813090294,2.11814920352042),
 .UNSPECIFIED.);
#23905=B_SPLINE_CURVE_WITH_KNOTS('',3,(#147905,#147906,#147907,#147908),
 .UNSPECIFIED.,.F.,.F.,(4,4),(3.73816266145575,3.78897373392225),
 .UNSPECIFIED.);
#23906=B_SPLINE_CURVE_WITH_KNOTS('',3,(#147910,#147911,#147912,#147913,
#147914,#147915,#147916,#147917,#147918,#147919,#147920,#147921,#147922,
#147923,#147924,#147925,#147926),.UNSPECIFIED.,.F.,.F.,(4,2,2,2,3,2,2,4),
(0.0529024352448051,0.0551226000948243,0.0590534470358053,0.0612484958738077,
0.0634408290671648,0.067296928952395,0.0711810086624211,0.0739890799479556),
 .UNSPECIFIED.);
#23907=B_SPLINE_CURVE_WITH_KNOTS('',3,(#147927,#147928,#147929,#147930),
 .UNSPECIFIED.,.F.,.F.,(4,4),(2.06733813079829,2.11814920332747),
 .UNSPECIFIED.);
#23908=B_SPLINE_CURVE_WITH_KNOTS('',3,(#147932,#147933,#147934,#147935),
 .UNSPECIFIED.,.F.,.F.,(4,4),(3.7381626605244,3.78897373310771),
 .UNSPECIFIED.);
#23909=B_SPLINE_CURVE_WITH_KNOTS('',3,(#147937,#147938,#147939,#147940,
#147941,#147942,#147943,#147944,#147945,#147946,#147947,#147948,#147949,
#147950,#147951,#147952,#147953),.UNSPECIFIED.,.F.,.F.,(4,2,2,2,3,2,2,4),
(0.0529024352696854,0.0551226000951222,0.0590534470356417,0.0612484958734864,
0.063440829066722,0.0672969289520468,0.0711810086624219,0.0739890799428532),
 .UNSPECIFIED.);
#23910=B_SPLINE_CURVE_WITH_KNOTS('',3,(#147954,#147955,#147956,#147957),
 .UNSPECIFIED.,.F.,.F.,(4,4),(2.06733813108993,2.11814920359329),
 .UNSPECIFIED.);
#23911=B_SPLINE_CURVE_WITH_KNOTS('',3,(#147959,#147960,#147961,#147962),
 .UNSPECIFIED.,.F.,.F.,(4,4),(3.73816266065588,3.7889737331094),
 .UNSPECIFIED.);
#23912=B_SPLINE_CURVE_WITH_KNOTS('',3,(#147964,#147965,#147966,#147967,
#147968,#147969,#147970,#147971,#147972,#147973,#147974,#147975,#147976,
#147977,#147978,#147979,#147980),.UNSPECIFIED.,.F.,.F.,(4,2,2,2,3,2,2,4),
(0.0529024352500414,0.0551226000953574,0.0590534470359871,0.0612484958738545,
0.0634408290671024,0.0672969289523756,0.0711810086626638,0.073989079946815),
 .UNSPECIFIED.);
#23913=B_SPLINE_CURVE_WITH_KNOTS('',3,(#147981,#147982,#147983,#147984),
 .UNSPECIFIED.,.F.,.F.,(4,4),(2.06733813108585,2.1181492035795),
 .UNSPECIFIED.);
#23914=B_SPLINE_CURVE_WITH_KNOTS('',3,(#147986,#147987,#147988,#147989),
 .UNSPECIFIED.,.F.,.F.,(4,4),(3.73816265997327,3.78897373253894),
 .UNSPECIFIED.);
#23915=B_SPLINE_CURVE_WITH_KNOTS('',3,(#147991,#147992,#147993,#147994,
#147995,#147996,#147997,#147998,#147999,#148000,#148001,#148002,#148003,
#148004,#148005,#148006,#148007),.UNSPECIFIED.,.F.,.F.,(4,2,2,2,3,2,2,4),
(0.0529024352877033,0.055122600096207,0.0590534470365002,0.061248495874216,
0.063440829067339,0.0672969289526178,0.0711810086631494,0.0739890799430888),
 .UNSPECIFIED.);
#23916=B_SPLINE_CURVE_WITH_KNOTS('',3,(#148008,#148009,#148010,#148011),
 .UNSPECIFIED.,.F.,.F.,(4,4),(2.06733813118465,2.11814920367701),
 .UNSPECIFIED.);
#23917=B_SPLINE_CURVE_WITH_KNOTS('',3,(#148013,#148014,#148015,#148016),
 .UNSPECIFIED.,.F.,.F.,(4,4),(3.73816266083586,3.78897373340649),
 .UNSPECIFIED.);
#23918=B_SPLINE_CURVE_WITH_KNOTS('',3,(#148018,#148019,#148020,#148021,
#148022,#148023,#148024,#148025,#148026,#148027,#148028,#148029,#148030,
#148031,#148032,#148033,#148034),.UNSPECIFIED.,.F.,.F.,(4,2,2,2,3,2,2,4),
(0.0529024353274146,0.0551226000958684,0.0590534470366202,0.0612484958744934,
0.063440829067739,0.0672969289529286,0.071181008663116,0.0739890799286134),
 .UNSPECIFIED.);
#23919=B_SPLINE_CURVE_WITH_KNOTS('',3,(#148035,#148036,#148037,#148038),
 .UNSPECIFIED.,.F.,.F.,(4,4),(2.06733813097796,2.11814920353602),
 .UNSPECIFIED.);
#23920=B_SPLINE_CURVE_WITH_KNOTS('',3,(#148040,#148041,#148042,#148043),
 .UNSPECIFIED.,.F.,.F.,(4,4),(3.73816266096225,3.78897373348547),
 .UNSPECIFIED.);
#23921=B_SPLINE_CURVE_WITH_KNOTS('',3,(#148045,#148046,#148047,#148048,
#148049,#148050,#148051,#148052,#148053,#148054,#148055,#148056,#148057,
#148058,#148059,#148060,#148061),.UNSPECIFIED.,.F.,.F.,(4,2,2,2,3,2,2,4),
(0.0529024352352074,0.0551226000951276,0.0590534470358563,0.0612484958737609,
0.0634408290670414,0.067296928952303,0.0711810086625111,0.073989079927302),
 .UNSPECIFIED.);
#23922=B_SPLINE_CURVE_WITH_KNOTS('',3,(#148062,#148063,#148064,#148065),
 .UNSPECIFIED.,.F.,.F.,(4,4),(2.06733813095919,2.11814920352003),
 .UNSPECIFIED.);
#23923=B_SPLINE_CURVE_WITH_KNOTS('',3,(#148067,#148068,#148069,#148070),
 .UNSPECIFIED.,.F.,.F.,(4,4),(3.73816266110557,3.78897373362394),
 .UNSPECIFIED.);
#23924=B_SPLINE_CURVE_WITH_KNOTS('',3,(#148072,#148073,#148074,#148075,
#148076,#148077,#148078,#148079,#148080,#148081,#148082,#148083,#148084,
#148085,#148086,#148087,#148088),.UNSPECIFIED.,.F.,.F.,(4,2,2,2,3,2,2,4),
(0.0529024352526763,0.0551226000943946,0.0590534470351668,0.0612484958731182,
0.0634408290664451,0.0672969289517592,0.0711810086619386,0.0739890799932635),
 .UNSPECIFIED.);
#23925=B_SPLINE_CURVE_WITH_KNOTS('',3,(#148089,#148090,#148091,#148092),
 .UNSPECIFIED.,.F.,.F.,(4,4),(2.06733813088428,2.11814920342807),
 .UNSPECIFIED.);
#23926=B_SPLINE_CURVE_WITH_KNOTS('',3,(#148094,#148095,#148096,#148097),
 .UNSPECIFIED.,.F.,.F.,(4,4),(3.73816266018992,3.78897373275654),
 .UNSPECIFIED.);
#23927=B_SPLINE_CURVE_WITH_KNOTS('',3,(#148099,#148100,#148101,#148102,
#148103,#148104,#148105,#148106,#148107,#148108,#148109,#148110,#148111,
#148112,#148113,#148114,#148115),.UNSPECIFIED.,.F.,.F.,(4,2,2,2,3,2,2,4),
(0.0529024352594984,0.0551226000959426,0.0590534470363031,0.0612484958740503,
0.0634408290672013,0.0672969289524806,0.0711810086629572,0.0739890799144632),
 .UNSPECIFIED.);
#23928=B_SPLINE_CURVE_WITH_KNOTS('',3,(#148116,#148117,#148118,#148119),
 .UNSPECIFIED.,.F.,.F.,(4,4),(2.06733813112861,2.11814920361968),
 .UNSPECIFIED.);
#23929=B_SPLINE_CURVE_WITH_KNOTS('',3,(#148121,#148122,#148123,#148124),
 .UNSPECIFIED.,.F.,.F.,(4,4),(3.7381626617959,3.78897373426471),
 .UNSPECIFIED.);
#23930=B_SPLINE_CURVE_WITH_KNOTS('',3,(#148126,#148127,#148128,#148129,
#148130,#148131,#148132,#148133,#148134,#148135,#148136,#148137,#148138,
#148139,#148140,#148141,#148142),.UNSPECIFIED.,.F.,.F.,(4,2,2,2,3,2,2,4),
(0.0529024352876146,0.055122600094267,0.0590534470354298,0.0612484958735101,
0.0634408290669359,0.067296928952156,0.0711810086620328,0.0739890800128771),
 .UNSPECIFIED.);
#23931=B_SPLINE_CURVE_WITH_KNOTS('',3,(#148143,#148144,#148145,#148146),
 .UNSPECIFIED.,.F.,.F.,(4,4),(2.06733813072275,2.11814920323567),
 .UNSPECIFIED.);
#23932=B_SPLINE_CURVE_WITH_KNOTS('',3,(#148148,#148149,#148150,#148151),
 .UNSPECIFIED.,.F.,.F.,(4,4),(3.73816266167531,3.78897373415517),
 .UNSPECIFIED.);
#23933=B_SPLINE_CURVE_WITH_KNOTS('',3,(#148153,#148154,#148155,#148156,
#148157,#148158,#148159,#148160,#148161,#148162,#148163,#148164,#148165,
#148166,#148167,#148168,#148169),.UNSPECIFIED.,.F.,.F.,(4,2,2,2,3,2,2,4),
(0.0529024353277011,0.0551226000949243,0.0590534470360282,0.0612484958740575,
0.0634408290674342,0.0672969289526096,0.0711810086625277,0.0739890799254628),
 .UNSPECIFIED.);
#23934=B_SPLINE_CURVE_WITH_KNOTS('',3,(#148170,#148171,#148172,#148173),
 .UNSPECIFIED.,.F.,.F.,(4,4),(2.06733813079588,2.11814920335918),
 .UNSPECIFIED.);
#23935=B_SPLINE_CURVE_WITH_KNOTS('',3,(#148175,#148176,#148177,#148178),
 .UNSPECIFIED.,.F.,.F.,(4,4),(3.73816265995722,3.78897373248134),
 .UNSPECIFIED.);
#23936=B_SPLINE_CURVE_WITH_KNOTS('',3,(#148180,#148181,#148182,#148183,
#148184,#148185,#148186,#148187,#148188,#148189,#148190,#148191,#148192,
#148193,#148194,#148195,#148196),.UNSPECIFIED.,.F.,.F.,(4,2,2,2,3,2,2,4),
(0.0529024352480456,0.0551226000967675,0.0590534470371181,0.0612484958748231,
0.0634408290679309,0.0672969289531626,0.0711810086636647,0.0739890798763888),
 .UNSPECIFIED.);
#23937=B_SPLINE_CURVE_WITH_KNOTS('',3,(#148197,#148198,#148199,#148200),
 .UNSPECIFIED.,.F.,.F.,(4,4),(2.0673381312259,2.11814920375009),
 .UNSPECIFIED.);
#23938=B_SPLINE_CURVE_WITH_KNOTS('',3,(#148202,#148203,#148204,#148205),
 .UNSPECIFIED.,.F.,.F.,(4,4),(3.73816266135447,3.78897373388667),
 .UNSPECIFIED.);
#23939=B_SPLINE_CURVE_WITH_KNOTS('',3,(#148207,#148208,#148209,#148210,
#148211,#148212,#148213,#148214,#148215,#148216,#148217,#148218,#148219,
#148220,#148221,#148222,#148223),.UNSPECIFIED.,.F.,.F.,(4,2,2,2,3,2,2,4),
(0.0529024352811202,0.055122600094669,0.0590534470355693,0.0612484958735547,
0.0634408290669023,0.0672969289521659,0.0711810086622503,0.0739890799314381),
 .UNSPECIFIED.);
#23940=B_SPLINE_CURVE_WITH_KNOTS('',3,(#148224,#148225,#148226,#148227),
 .UNSPECIFIED.,.F.,.F.,(4,4),(2.06733813088284,2.11814920343982),
 .UNSPECIFIED.);
#23941=B_SPLINE_CURVE_WITH_KNOTS('',3,(#148229,#148230,#148231,#148232),
 .UNSPECIFIED.,.F.,.F.,(4,4),(3.73816266067428,3.78897373321881),
 .UNSPECIFIED.);
#23942=B_SPLINE_CURVE_WITH_KNOTS('',3,(#148234,#148235,#148236,#148237,
#148238,#148239,#148240,#148241,#148242,#148243,#148244,#148245,#148246,
#148247,#148248,#148249,#148250),.UNSPECIFIED.,.F.,.F.,(4,2,2,2,3,2,2,4),
(0.052902435264904,0.0551226000944819,0.0590534470351052,0.0612484958730058,
0.0634408290662948,0.0672969289516403,0.0711810086619305,0.0739890800019837),
 .UNSPECIFIED.);
#23943=B_SPLINE_CURVE_WITH_KNOTS('',3,(#148251,#148252,#148253,#148254),
 .UNSPECIFIED.,.F.,.F.,(4,4),(2.06733813102832,2.11814920355794),
 .UNSPECIFIED.);
#23944=B_SPLINE_CURVE_WITH_KNOTS('',3,(#148256,#148257,#148258,#148259),
 .UNSPECIFIED.,.F.,.F.,(4,4),(3.73816266066757,3.78897373314875),
 .UNSPECIFIED.);
#23945=B_SPLINE_CURVE_WITH_KNOTS('',3,(#148261,#148262,#148263,#148264,
#148265,#148266,#148267,#148268,#148269,#148270,#148271,#148272,#148273,
#148274,#148275,#148276,#148277),.UNSPECIFIED.,.F.,.F.,(4,2,2,2,3,2,2,4),
(0.052902435234979,0.0551226000954227,0.0590534470359989,0.0612484958738436,
0.063440829067074,0.067296928952351,0.0711810086626759,0.0739890799320362),
 .UNSPECIFIED.);
#23946=B_SPLINE_CURVE_WITH_KNOTS('',3,(#148278,#148279,#148280,#148281),
 .UNSPECIFIED.,.F.,.F.,(4,4),(2.06733813103431,2.11814920362238),
 .UNSPECIFIED.);
#23947=B_SPLINE_CURVE_WITH_KNOTS('',3,(#148283,#148284,#148285,#148286),
 .UNSPECIFIED.,.F.,.F.,(4,4),(3.73816266144136,3.7889737339741),
 .UNSPECIFIED.);
#23948=B_SPLINE_CURVE_WITH_KNOTS('',3,(#148288,#148289,#148290,#148291,
#148292,#148293,#148294,#148295,#148296,#148297,#148298,#148299,#148300,
#148301,#148302,#148303,#148304),.UNSPECIFIED.,.F.,.F.,(4,2,2,2,3,2,2,4),
(0.0529024352960807,0.0551226000944865,0.0590534470355066,0.0612484958735405,
0.0634408290669255,0.0672969289521807,0.0711810086621846,0.0739890800026948),
 .UNSPECIFIED.);
#23949=B_SPLINE_CURVE_WITH_KNOTS('',3,(#148305,#148306,#148307,#148308),
 .UNSPECIFIED.,.F.,.F.,(4,4),(2.06733813083286,2.11814920335294),
 .UNSPECIFIED.);
#23950=B_SPLINE_CURVE_WITH_KNOTS('',3,(#148310,#148311,#148312,#148313),
 .UNSPECIFIED.,.F.,.F.,(4,4),(3.73816266015891,3.78897373268002),
 .UNSPECIFIED.);
#23951=B_SPLINE_CURVE_WITH_KNOTS('',3,(#148315,#148316,#148317,#148318,
#148319,#148320,#148321,#148322,#148323,#148324,#148325,#148326,#148327,
#148328,#148329,#148330,#148331),.UNSPECIFIED.,.F.,.F.,(4,2,2,2,3,2,2,4),
(0.0529024352569361,0.0551226000955349,0.0590534470359355,0.0612484958737216,
0.0634408290669069,0.0672969289522366,0.0711810086627126,0.0739890799167341),
 .UNSPECIFIED.);
#23952=B_SPLINE_CURVE_WITH_KNOTS('',3,(#148332,#148333,#148334,#148335),
 .UNSPECIFIED.,.F.,.F.,(4,4),(2.06733813113835,2.11814920367071),
 .UNSPECIFIED.);
#23953=B_SPLINE_CURVE_WITH_KNOTS('',3,(#148337,#148338,#148339,#148340),
 .UNSPECIFIED.,.F.,.F.,(4,4),(3.7381626611044,3.78897373365368),
 .UNSPECIFIED.);
#23954=B_SPLINE_CURVE_WITH_KNOTS('',3,(#148342,#148343,#148344,#148345,
#148346,#148347,#148348,#148349,#148350,#148351,#148352,#148353,#148354,
#148355,#148356,#148357,#148358),.UNSPECIFIED.,.F.,.F.,(4,2,2,2,3,2,2,4),
(0.0529024352810775,0.0551226000949388,0.059053447035779,0.061248495873723,
0.0634408290670364,0.0672969289522796,0.071181008662396,0.0739890799780723),
 .UNSPECIFIED.);
#23955=B_SPLINE_CURVE_WITH_KNOTS('',3,(#148359,#148360,#148361,#148362),
 .UNSPECIFIED.,.F.,.F.,(4,4),(2.06733813095668,2.11814920343747),
 .UNSPECIFIED.);
#23956=B_SPLINE_CURVE_WITH_KNOTS('',3,(#148364,#148365,#148366,#148367),
 .UNSPECIFIED.,.F.,.F.,(4,4),(3.73816266102959,3.78897373355911),
 .UNSPECIFIED.);
#23957=B_SPLINE_CURVE_WITH_KNOTS('',3,(#148369,#148370,#148371,#148372,
#148373,#148374,#148375,#148376,#148377,#148378,#148379,#148380,#148381,
#148382,#148383,#148384,#148385),.UNSPECIFIED.,.F.,.F.,(4,2,2,2,3,2,2,4),
(0.0529024352095704,0.0551226000943593,0.0590534470350723,0.0612484958730129,
0.0634408290663316,0.0672969289516666,0.0711810086618903,0.0739890799467104),
 .UNSPECIFIED.);
#23958=B_SPLINE_CURVE_WITH_KNOTS('',3,(#148386,#148387,#148388,#148389),
 .UNSPECIFIED.,.F.,.F.,(4,4),(2.06733813091365,2.11814920351671),
 .UNSPECIFIED.);
#23959=B_SPLINE_CURVE_WITH_KNOTS('',3,(#148391,#148392,#148393,#148394),
 .UNSPECIFIED.,.F.,.F.,(4,4),(3.73816266050385,3.78897373306035),
 .UNSPECIFIED.);
#23960=B_SPLINE_CURVE_WITH_KNOTS('',3,(#148396,#148397,#148398,#148399,
#148400,#148401,#148402,#148403,#148404,#148405,#148406,#148407,#148408,
#148409,#148410,#148411,#148412),.UNSPECIFIED.,.F.,.F.,(4,2,2,2,3,2,2,4),
(0.0529024352813181,0.055122600095314,0.0590534470358095,0.061248495873635,
0.0634408290668542,0.0672969289521644,0.0711810086625508,0.073989079997811),
 .UNSPECIFIED.);
#23961=B_SPLINE_CURVE_WITH_KNOTS('',3,(#148413,#148414,#148415,#148416),
 .UNSPECIFIED.,.F.,.F.,(4,4),(2.06733813112279,2.11814920361366),
 .UNSPECIFIED.);
#23962=B_SPLINE_CURVE_WITH_KNOTS('',3,(#148418,#148419,#148420,#148421),
 .UNSPECIFIED.,.F.,.F.,(4,4),(3.73816266180585,3.78897373432959),
 .UNSPECIFIED.);
#23963=B_SPLINE_CURVE_WITH_KNOTS('',3,(#148423,#148424,#148425,#148426,
#148427,#148428,#148429,#148430,#148431,#148432,#148433,#148434,#148435,
#148436,#148437,#148438,#148439),.UNSPECIFIED.,.F.,.F.,(4,2,2,2,3,2,2,4),
(0.0529024353383817,0.0551226000952313,0.0590534470363804,0.0612484958744086,
0.0634408290677798,0.0672969289529119,0.0711810086627874,0.0739890799666121),
 .UNSPECIFIED.);
#23964=B_SPLINE_CURVE_WITH_KNOTS('',3,(#148440,#148441,#148442,#148443),
 .UNSPECIFIED.,.F.,.F.,(4,4),(2.06733813079015,2.11814920328276),
 .UNSPECIFIED.);
#23965=B_SPLINE_CURVE_WITH_KNOTS('',3,(#148445,#148446,#148447,#148448),
 .UNSPECIFIED.,.F.,.F.,(4,4),(3.73816266000277,3.78897373256649),
 .UNSPECIFIED.);
#23966=B_SPLINE_CURVE_WITH_KNOTS('',3,(#148450,#148451,#148452,#148453,
#148454,#148455,#148456,#148457,#148458,#148459,#148460,#148461,#148462,
#148463,#148464,#148465,#148466),.UNSPECIFIED.,.F.,.F.,(4,2,2,2,3,2,2,4),
(0.0529024352886305,0.0551226000964549,0.0590534470368377,0.0612484958745884,
0.06344082906773,0.0672969289529962,0.0711810086634918,0.0739890798865082),
 .UNSPECIFIED.);
#23967=B_SPLINE_CURVE_WITH_KNOTS('',3,(#148467,#148468,#148469,#148470),
 .UNSPECIFIED.,.F.,.F.,(4,4),(2.0673381311841,2.11814920373392),
 .UNSPECIFIED.);
#23968=B_SPLINE_CURVE_WITH_KNOTS('',3,(#148472,#148473,#148474,#148475),
 .UNSPECIFIED.,.F.,.F.,(4,4),(3.7381626598156,3.78897373232901),
 .UNSPECIFIED.);
#23969=B_SPLINE_CURVE_WITH_KNOTS('',3,(#148477,#148478,#148479,#148480,
#148481,#148482,#148483,#148484,#148485,#148486,#148487,#148488,#148489,
#148490,#148491,#148492,#148493),.UNSPECIFIED.,.F.,.F.,(4,2,2,2,3,2,2,4),
(0.0529024351998522,0.0551226000957807,0.0590534470360129,0.0612484958737305,
0.063440829066862,0.0672969289521915,0.0711810086627707,0.0739890799251832),
 .UNSPECIFIED.);
#23970=B_SPLINE_CURVE_WITH_KNOTS('',3,(#148494,#148495,#148496,#148497),
 .UNSPECIFIED.,.F.,.F.,(4,4),(2.06733813124236,2.11814920376004),
 .UNSPECIFIED.);
#23971=B_SPLINE_CURVE_WITH_KNOTS('',3,(#148499,#148500,#148501,#148502),
 .UNSPECIFIED.,.F.,.F.,(4,4),(3.73816266168604,3.78897373417607),
 .UNSPECIFIED.);
#23972=B_SPLINE_CURVE_WITH_KNOTS('',3,(#148504,#148505,#148506,#148507,
#148508,#148509,#148510,#148511,#148512,#148513,#148514,#148515,#148516,
#148517,#148518,#148519,#148520),.UNSPECIFIED.,.F.,.F.,(4,2,2,2,3,2,2,4),
(0.0529024352984763,0.0551226000947986,0.0590534470358693,0.0612484958738993,
0.0634408290672777,0.0672969289524761,0.0711810086624219,0.0739890800310639),
 .UNSPECIFIED.);
#23973=B_SPLINE_CURVE_WITH_KNOTS('',3,(#148521,#148522,#148523,#148524),
 .UNSPECIFIED.,.F.,.F.,(4,4),(2.06733813082859,2.11814920332163),
 .UNSPECIFIED.);
#23974=B_SPLINE_CURVE_WITH_KNOTS('',3,(#148526,#148527,#148528,#148529),
 .UNSPECIFIED.,.F.,.F.,(4,4),(3.73816266070724,3.78897373325739),
 .UNSPECIFIED.);
#23975=B_SPLINE_CURVE_WITH_KNOTS('',3,(#148531,#148532,#148533,#148534,
#148535,#148536,#148537,#148538,#148539,#148540,#148541,#148542,#148543,
#148544,#148545,#148546,#148547),.UNSPECIFIED.,.F.,.F.,(4,2,2,2,3,2,2,4),
(0.0529024352251564,0.0551226000947543,0.059053447035343,0.0612484958732276,
0.0634408290664983,0.0672969289518344,0.0711810086621559,0.0739890799592365),
 .UNSPECIFIED.);
#23976=B_SPLINE_CURVE_WITH_KNOTS('',3,(#148548,#148549,#148550,#148551),
 .UNSPECIFIED.,.F.,.F.,(4,4),(2.06733813102794,2.1181492036115),
 .UNSPECIFIED.);
#23977=B_SPLINE_CURVE_WITH_KNOTS('',3,(#148553,#148554,#148555,#148556),
 .UNSPECIFIED.,.F.,.F.,(4,4),(3.73816266082592,3.78897373338695),
 .UNSPECIFIED.);
#23978=B_SPLINE_CURVE_WITH_KNOTS('',3,(#148558,#148559,#148560,#148561,
#148562,#148563,#148564,#148565,#148566,#148567,#148568,#148569,#148570,
#148571,#148572,#148573,#148574),.UNSPECIFIED.,.F.,.F.,(4,2,2,2,3,2,2,4),
(0.052902435285732,0.0551226000951503,0.0590534470358304,0.0612484958737189,
0.0634408290669877,0.0672969289522547,0.0711810086624951,0.0739890799777724),
 .UNSPECIFIED.);
#23979=B_SPLINE_CURVE_WITH_KNOTS('',3,(#148575,#148576,#148577,#148578),
 .UNSPECIFIED.,.F.,.F.,(4,4),(2.06733813096253,2.11814920348551),
 .UNSPECIFIED.);
#23980=B_SPLINE_CURVE_WITH_KNOTS('',3,(#148580,#148581,#148582,#148583),
 .UNSPECIFIED.,.F.,.F.,(4,4),(3.73816266099154,3.78897373347697),
 .UNSPECIFIED.);
#23981=B_SPLINE_CURVE_WITH_KNOTS('',3,(#148585,#148586,#148587,#148588,
#148589,#148590,#148591,#148592,#148593,#148594,#148595,#148596,#148597,
#148598,#148599,#148600,#148601),.UNSPECIFIED.,.F.,.F.,(4,2,2,2,3,2,2,4),
(0.0529024352653158,0.0551226000958512,0.0590534470365838,0.0612484958744501,
0.0634408290676912,0.0672969289528806,0.0711810086630735,0.0739890798870407),
 .UNSPECIFIED.);
#23982=B_SPLINE_CURVE_WITH_KNOTS('',3,(#148602,#148603,#148604,#148605),
 .UNSPECIFIED.,.F.,.F.,(4,4),(2.06733813099677,2.11814920357114),
 .UNSPECIFIED.);
#23983=B_SPLINE_CURVE_WITH_KNOTS('',3,(#148607,#148608,#148609,#148610),
 .UNSPECIFIED.,.F.,.F.,(4,4),(3.73816266177325,3.78897373423991),
 .UNSPECIFIED.);
#23984=B_SPLINE_CURVE_WITH_KNOTS('',3,(#148612,#148613,#148614,#148615,
#148616,#148617,#148618,#148619,#148620,#148621,#148622,#148623,#148624,
#148625,#148626,#148627,#148628),.UNSPECIFIED.,.F.,.F.,(4,2,2,2,3,2,2,4),
(0.0529024353174922,0.0551226000947562,0.0590534470359121,0.0612484958739641,
0.0634408290673591,0.0672969289525375,0.0711810086624227,0.0739890799148762),
 .UNSPECIFIED.);
#23985=B_SPLINE_CURVE_WITH_KNOTS('',3,(#148629,#148630,#148631,#148632),
 .UNSPECIFIED.,.F.,.F.,(4,4),(2.06733813072299,2.11814920329931),
 .UNSPECIFIED.);
#23986=B_SPLINE_CURVE_WITH_KNOTS('',3,(#148634,#148635,#148636,#148637),
 .UNSPECIFIED.,.F.,.F.,(4,4),(3.73816266115613,3.78897373364958),
 .UNSPECIFIED.);
#23987=B_SPLINE_CURVE_WITH_KNOTS('',3,(#148639,#148640,#148641,#148642,
#148643,#148644,#148645,#148646,#148647,#148648,#148649,#148650,#148651,
#148652,#148653,#148654,#148655),.UNSPECIFIED.,.F.,.F.,(4,2,2,2,3,2,2,4),
(0.0529024352663877,0.0551226000951005,0.0590534470359006,0.061248495873833,
0.0634408290671345,0.0672969289523877,0.071181008662549,0.0739890799450588),
 .UNSPECIFIED.);
#23988=B_SPLINE_CURVE_WITH_KNOTS('',3,(#148656,#148657,#148658,#148659),
 .UNSPECIFIED.,.F.,.F.,(4,4),(2.06733813096761,2.11814920343851),
 .UNSPECIFIED.);
#23989=B_SPLINE_CURVE_WITH_KNOTS('',3,(#148661,#148662,#148663,#148664),
 .UNSPECIFIED.,.F.,.F.,(4,4),(3.73816266123958,3.78897373374303),
 .UNSPECIFIED.);
#23990=B_SPLINE_CURVE_WITH_KNOTS('',3,(#148666,#148667,#148668,#148669,
#148670,#148671,#148672,#148673,#148674,#148675,#148676,#148677,#148678,
#148679,#148680,#148681,#148682),.UNSPECIFIED.,.F.,.F.,(4,2,2,2,3,2,2,4),
(0.0529024352695806,0.0551226000945445,0.0590534470354143,0.0612484958733957,
0.0634408290667422,0.0672969289520255,0.0711810086621362,0.0739890799729577),
 .UNSPECIFIED.);
#23991=B_SPLINE_CURVE_WITH_KNOTS('',3,(#148683,#148684,#148685,#148686),
 .UNSPECIFIED.,.F.,.F.,(4,4),(2.06733813089893,2.11814920345364),
 .UNSPECIFIED.);
#23992=B_SPLINE_CURVE_WITH_KNOTS('',3,(#148688,#148689,#148690,#148691),
 .UNSPECIFIED.,.F.,.F.,(4,4),(3.73816266031907,3.78897373284873),
 .UNSPECIFIED.);
#23993=B_SPLINE_CURVE_WITH_KNOTS('',3,(#148693,#148694,#148695,#148696,
#148697,#148698,#148699,#148700,#148701,#148702,#148703,#148704,#148705,
#148706,#148707,#148708,#148709),.UNSPECIFIED.,.F.,.F.,(4,2,2,2,3,2,2,4),
(0.052902435265286,0.0551226000956631,0.0590534470361102,0.0612484958739062,
0.0634408290670971,0.0672969289523889,0.0711810086628101,0.0739890799683972),
 .UNSPECIFIED.);
#23994=B_SPLINE_CURVE_WITH_KNOTS('',3,(#148710,#148711,#148712,#148713),
 .UNSPECIFIED.,.F.,.F.,(4,4),(2.06733813117357,2.11814920366994),
 .UNSPECIFIED.);
#23995=B_SPLINE_CURVE_WITH_KNOTS('',3,(#148715,#148716,#148717,#148718),
 .UNSPECIFIED.,.F.,.F.,(4,4),(3.73816266063489,3.78897373319568),
 .UNSPECIFIED.);
#23996=B_SPLINE_CURVE_WITH_KNOTS('',3,(#148720,#148721,#148722,#148723,
#148724,#148725,#148726,#148727,#148728,#148729,#148730,#148731,#148732,
#148733,#148734,#148735,#148736),.UNSPECIFIED.,.F.,.F.,(4,2,2,2,3,2,2,4),
(0.0529024353177154,0.0551226000957153,0.0590534470363672,0.0612484958742148,
0.0634408290674435,0.067296928952665,0.07118100866292,0.0739890799725188),
 .UNSPECIFIED.);
#23997=B_SPLINE_CURVE_WITH_KNOTS('',3,(#148737,#148738,#148739,#148740),
 .UNSPECIFIED.,.F.,.F.,(4,4),(2.06733813102884,2.1181492034784),
 .UNSPECIFIED.);
#23998=B_SPLINE_CURVE_WITH_KNOTS('',3,(#148742,#148743,#148744,#148745),
 .UNSPECIFIED.,.F.,.F.,(4,4),(3.73816266078816,3.78897373330558),
 .UNSPECIFIED.);
#23999=B_SPLINE_CURVE_WITH_KNOTS('',3,(#148747,#148748,#148749,#148750,
#148751,#148752,#148753,#148754,#148755,#148756,#148757,#148758,#148759,
#148760,#148761,#148762,#148763),.UNSPECIFIED.,.F.,.F.,(4,2,2,2,3,2,2,4),
(0.0529024353240009,0.0551226000961563,0.0590534470368356,0.0612484958746766,
0.0634408290678929,0.0672969289530824,0.0711810086633302,0.0739890799110409),
 .UNSPECIFIED.);
#24000=B_SPLINE_CURVE_WITH_KNOTS('',3,(#148764,#148765,#148766,#148767),
 .UNSPECIFIED.,.F.,.F.,(4,4),(2.0673381310135,2.11814920352267),
 .UNSPECIFIED.);
#24001=B_SPLINE_CURVE_WITH_KNOTS('',3,(#148769,#148770,#148771,#148772),
 .UNSPECIFIED.,.F.,.F.,(4,4),(3.73816266085092,3.78897373334858),
 .UNSPECIFIED.);
#24002=B_SPLINE_CURVE_WITH_KNOTS('',3,(#148774,#148775,#148776,#148777,
#148778,#148779,#148780,#148781,#148782,#148783),.UNSPECIFIED.,.F.,.F.,
(4,2,2,2,4),(0.0529024352988807,0.0551226000957205,0.0590534470364613,0.0612484958743386,
0.0634408290675894),.UNSPECIFIED.);
#24003=B_SPLINE_CURVE_WITH_KNOTS('',3,(#148788,#148789,#148790,#148791,
#148792,#148793,#148794,#148795),.UNSPECIFIED.,.F.,.F.,(4,2,2,4),(0.0634408290675894,
0.0672969289527968,0.0711810086629958,0.073989079915298),.UNSPECIFIED.);
#24004=B_SPLINE_CURVE_WITH_KNOTS('',3,(#148796,#148797,#148798,#148799),
 .UNSPECIFIED.,.F.,.F.,(4,4),(2.06733813101515,2.11814920351282),
 .UNSPECIFIED.);
#24005=B_SPLINE_CURVE_WITH_KNOTS('',3,(#148801,#148802,#148803,#148804),
 .UNSPECIFIED.,.F.,.F.,(4,4),(3.73816266103402,3.78897373354396),
 .UNSPECIFIED.);
#24006=B_SPLINE_CURVE_WITH_KNOTS('',3,(#148806,#148807,#148808,#148809,
#148810,#148811,#148812,#148813,#148814,#148815,#148816,#148817,#148818,
#148819,#148820,#148821,#148822),.UNSPECIFIED.,.F.,.F.,(4,2,2,2,3,2,2,4),
(0.0529024353036826,0.0551226000958266,0.0590534470366519,0.0612484958745524,
0.0634408290678181,0.0672969289529889,0.0711810086631166,0.07398907989072),
 .UNSPECIFIED.);
#24007=B_SPLINE_CURVE_WITH_KNOTS('',3,(#148823,#148824,#148825,#148826),
 .UNSPECIFIED.,.F.,.F.,(4,4),(2.06733813100458,2.11814920352257),
 .UNSPECIFIED.);
#24008=B_SPLINE_CURVE_WITH_KNOTS('',3,(#148828,#148829,#148830,#148831),
 .UNSPECIFIED.,.F.,.F.,(4,4),(3.73816266106249,3.78897373354877),
 .UNSPECIFIED.);
#24009=B_SPLINE_CURVE_WITH_KNOTS('',3,(#148833,#148834,#148835,#148836,
#148837,#148838,#148839,#148840,#148841,#148842,#148843,#148844,#148845,
#148846,#148847,#148848,#148849),.UNSPECIFIED.,.F.,.F.,(4,2,2,2,3,2,2,4),
(0.0529024352792874,0.0551226000954993,0.0590534470363064,0.0612484958742183,
0.0634408290674978,0.0672969289527032,0.0711810086628473,0.0739890798962569),
 .UNSPECIFIED.);
#24010=B_SPLINE_CURVE_WITH_KNOTS('',3,(#148850,#148851,#148852,#148853),
 .UNSPECIFIED.,.F.,.F.,(4,4),(2.06733813090294,2.11814920352042),
 .UNSPECIFIED.);
#24011=B_SPLINE_CURVE_WITH_KNOTS('',3,(#148855,#148856,#148857,#148858),
 .UNSPECIFIED.,.F.,.F.,(4,4),(3.73816266145574,3.78897373392224),
 .UNSPECIFIED.);
#24012=B_SPLINE_CURVE_WITH_KNOTS('',3,(#148860,#148861,#148862,#148863,
#148864,#148865,#148866,#148867,#148868,#148869,#148870,#148871,#148872,
#148873,#148874,#148875,#148876),.UNSPECIFIED.,.F.,.F.,(4,2,2,2,3,2,2,4),
(0.0529024352447713,0.0551226000947896,0.059053447035766,0.0612484958737659,
0.0634408290671224,0.0672969289523521,0.0711810086623765,0.073989079947909),
 .UNSPECIFIED.);
#24013=B_SPLINE_CURVE_WITH_KNOTS('',3,(#148877,#148878,#148879,#148880),
 .UNSPECIFIED.,.F.,.F.,(4,4),(2.06733813079829,2.11814920332747),
 .UNSPECIFIED.);
#24014=B_SPLINE_CURVE_WITH_KNOTS('',3,(#148882,#148883,#148884,#148885),
 .UNSPECIFIED.,.F.,.F.,(4,4),(3.73816266052439,3.7889737331077),
 .UNSPECIFIED.);
#24015=B_SPLINE_CURVE_WITH_KNOTS('',3,(#148887,#148888,#148889,#148890,
#148891,#148892,#148893,#148894,#148895,#148896,#148897,#148898,#148899,
#148900,#148901,#148902,#148903),.UNSPECIFIED.,.F.,.F.,(4,2,2,2,3,2,2,4),
(0.0529024352696748,0.0551226000951075,0.0590534470356228,0.061248495873468,
0.0634408290667037,0.0672969289520287,0.0711810086624032,0.0739890799428344),
 .UNSPECIFIED.);
#24016=B_SPLINE_CURVE_WITH_KNOTS('',3,(#148904,#148905,#148906,#148907),
 .UNSPECIFIED.,.F.,.F.,(4,4),(2.06733813108993,2.11814920359329),
 .UNSPECIFIED.);
#24017=B_SPLINE_CURVE_WITH_KNOTS('',3,(#148909,#148910,#148911,#148912),
 .UNSPECIFIED.,.F.,.F.,(4,4),(3.73816266065588,3.7889737331094),
 .UNSPECIFIED.);
#24018=B_SPLINE_CURVE_WITH_KNOTS('',3,(#148914,#148915,#148916,#148917,
#148918,#148919,#148920,#148921,#148922,#148923,#148924,#148925,#148926,
#148927,#148928,#148929,#148930),.UNSPECIFIED.,.F.,.F.,(4,2,2,2,3,2,2,4),
(0.0529024352500216,0.0551226000953363,0.0590534470359648,0.0612484958738279,
0.0634408290670738,0.0672969289523469,0.0711810086626337,0.0739890799467816),
 .UNSPECIFIED.);
#24019=B_SPLINE_CURVE_WITH_KNOTS('',3,(#148931,#148932,#148933,#148934),
 .UNSPECIFIED.,.F.,.F.,(4,4),(2.06733813108585,2.1181492035795),
 .UNSPECIFIED.);
#24020=B_SPLINE_CURVE_WITH_KNOTS('',3,(#148936,#148937,#148938,#148939),
 .UNSPECIFIED.,.F.,.F.,(4,4),(3.73816265997327,3.78897373253894),
 .UNSPECIFIED.);
#24021=B_SPLINE_CURVE_WITH_KNOTS('',3,(#148941,#148942,#148943,#148944,
#148945,#148946,#148947,#148948,#148949,#148950,#148951,#148952,#148953,
#148954,#148955,#148956,#148957),.UNSPECIFIED.,.F.,.F.,(4,2,2,2,3,2,2,4),
(0.0529024352877148,0.0551226000962212,0.0590534470365158,0.0612484958742325,
0.063440829067356,0.0672969289526359,0.0711810086631708,0.0739890799431124),
 .UNSPECIFIED.);
#24022=B_SPLINE_CURVE_WITH_KNOTS('',3,(#148958,#148959,#148960,#148961),
 .UNSPECIFIED.,.F.,.F.,(4,4),(2.06733813118465,2.11814920367701),
 .UNSPECIFIED.);
#24023=B_SPLINE_CURVE_WITH_KNOTS('',3,(#148963,#148964,#148965,#148966),
 .UNSPECIFIED.,.F.,.F.,(4,4),(3.73816266083586,3.78897373340648),
 .UNSPECIFIED.);
#24024=B_SPLINE_CURVE_WITH_KNOTS('',3,(#148968,#148969,#148970,#148971,
#148972,#148973,#148974,#148975,#148976,#148977,#148978,#148979,#148980,
#148981,#148982,#148983,#148984),.UNSPECIFIED.,.F.,.F.,(4,2,2,2,3,2,2,4),
(0.0529024353273861,0.0551226000958364,0.0590534470365822,0.0612484958744578,
0.0634408290677049,0.0672969289528934,0.0711810086630778,0.0739890799285735),
 .UNSPECIFIED.);
#24025=B_SPLINE_CURVE_WITH_KNOTS('',3,(#148985,#148986,#148987,#148988),
 .UNSPECIFIED.,.F.,.F.,(4,4),(2.06733813097796,2.11814920353602),
 .UNSPECIFIED.);
#24026=B_SPLINE_CURVE_WITH_KNOTS('',3,(#148990,#148991,#148992,#148993),
 .UNSPECIFIED.,.F.,.F.,(4,4),(3.73816266096225,3.78897373348547),
 .UNSPECIFIED.);
#24027=B_SPLINE_CURVE_WITH_KNOTS('',3,(#148995,#148996,#148997,#148998,
#148999,#149000,#149001,#149002,#149003,#149004,#149005,#149006,#149007,
#149008,#149009,#149010,#149011),.UNSPECIFIED.,.F.,.F.,(4,2,2,2,3,2,2,4),
(0.052902435235209,0.0551226000951272,0.0590534470358533,0.0612484958737601,
0.0634408290670416,0.0672969289523034,0.0711810086625133,0.0739890799273062),
 .UNSPECIFIED.);
#24028=B_SPLINE_CURVE_WITH_KNOTS('',3,(#149012,#149013,#149014,#149015),
 .UNSPECIFIED.,.F.,.F.,(4,4),(2.06733813095919,2.11814920352003),
 .UNSPECIFIED.);
#24029=B_SPLINE_CURVE_WITH_KNOTS('',3,(#149017,#149018,#149019,#149020),
 .UNSPECIFIED.,.F.,.F.,(4,4),(3.73816266110557,3.78897373362395),
 .UNSPECIFIED.);
#24030=B_SPLINE_CURVE_WITH_KNOTS('',3,(#149022,#149023,#149024,#149025,
#149026,#149027,#149028,#149029,#149030,#149031,#149032,#149033,#149034,
#149035,#149036,#149037,#149038),.UNSPECIFIED.,.F.,.F.,(4,2,2,2,3,2,2,4),
(0.0529024352527248,0.0551226000944423,0.0590534470352124,0.0612484958731709,
0.0634408290665012,0.0672969289518157,0.0711810086619979,0.0739890799933279),
 .UNSPECIFIED.);
#24031=B_SPLINE_CURVE_WITH_KNOTS('',3,(#149039,#149040,#149041,#149042),
 .UNSPECIFIED.,.F.,.F.,(4,4),(2.06733813088428,2.11814920342807),
 .UNSPECIFIED.);
#24032=B_SPLINE_CURVE_WITH_KNOTS('',3,(#149044,#149045,#149046,#149047),
 .UNSPECIFIED.,.F.,.F.,(4,4),(3.73816266018992,3.78897373275654),
 .UNSPECIFIED.);
#24033=B_SPLINE_CURVE_WITH_KNOTS('',3,(#149049,#149050,#149051,#149052,
#149053,#149054,#149055,#149056,#149057,#149058,#149059,#149060,#149061,
#149062,#149063,#149064,#149065),.UNSPECIFIED.,.F.,.F.,(4,2,2,2,3,2,2,4),
(0.0529024352595687,0.0551226000960166,0.0590534470363857,0.0612484958741364,
0.0634408290672885,0.0672969289525699,0.0711810086630519,0.0739890799145621),
 .UNSPECIFIED.);
#24034=B_SPLINE_CURVE_WITH_KNOTS('',3,(#149066,#149067,#149068,#149069),
 .UNSPECIFIED.,.F.,.F.,(4,4),(2.06733813112861,2.11814920361968),
 .UNSPECIFIED.);
#24035=B_SPLINE_CURVE_WITH_KNOTS('',3,(#149071,#149072,#149073,#149074),
 .UNSPECIFIED.,.F.,.F.,(4,4),(3.73816266179589,3.78897373426471),
 .UNSPECIFIED.);
#24036=B_SPLINE_CURVE_WITH_KNOTS('',3,(#149076,#149077,#149078,#149079,
#149080,#149081,#149082,#149083,#149084,#149085,#149086,#149087,#149088,
#149089,#149090,#149091,#149092),.UNSPECIFIED.,.F.,.F.,(4,2,2,2,3,2,2,4),
(0.0529024352876567,0.0551226000943113,0.0590534470354802,0.0612484958735684,
0.0634408290669972,0.0672969289522185,0.0711810086620985,0.0739890800129455),
 .UNSPECIFIED.);
#24037=B_SPLINE_CURVE_WITH_KNOTS('',3,(#149093,#149094,#149095,#149096),
 .UNSPECIFIED.,.F.,.F.,(4,4),(2.06733813072275,2.11814920323567),
 .UNSPECIFIED.);
#24038=B_SPLINE_CURVE_WITH_KNOTS('',3,(#149098,#149099,#149100,#149101),
 .UNSPECIFIED.,.F.,.F.,(4,4),(3.73816266167531,3.78897373415517),
 .UNSPECIFIED.);
#24039=B_SPLINE_CURVE_WITH_KNOTS('',3,(#149103,#149104,#149105,#149106,
#149107,#149108,#149109,#149110,#149111,#149112,#149113,#149114,#149115,
#149116,#149117,#149118,#149119),.UNSPECIFIED.,.F.,.F.,(4,2,2,2,3,2,2,4),
(0.0529024353277232,0.0551226000949464,0.0590534470360541,0.0612484958740863,
0.0634408290674636,0.0672969289526391,0.0711810086625577,0.0739890799254936),
 .UNSPECIFIED.);
#24040=B_SPLINE_CURVE_WITH_KNOTS('',3,(#149120,#149121,#149122,#149123),
 .UNSPECIFIED.,.F.,.F.,(4,4),(2.06733813079588,2.11814920335918),
 .UNSPECIFIED.);
#24041=B_SPLINE_CURVE_WITH_KNOTS('',3,(#149125,#149126,#149127,#149128),
 .UNSPECIFIED.,.F.,.F.,(4,4),(3.73816265995722,3.78897373248134),
 .UNSPECIFIED.);
#24042=B_SPLINE_CURVE_WITH_KNOTS('',3,(#149130,#149131,#149132,#149133,
#149134,#149135,#149136,#149137,#149138,#149139,#149140,#149141,#149142,
#149143,#149144,#149145,#149146),.UNSPECIFIED.,.F.,.F.,(4,2,2,2,3,2,2,4),
(0.0529024352479053,0.0551226000966192,0.0590534470369545,0.0612484958746632,
0.0634408290677745,0.0672969289530026,0.0711810086634966,0.0739890798762164),
 .UNSPECIFIED.);
#24043=B_SPLINE_CURVE_WITH_KNOTS('',3,(#149147,#149148,#149149,#149150),
 .UNSPECIFIED.,.F.,.F.,(4,4),(2.0673381312259,2.11814920375009),
 .UNSPECIFIED.);
#24044=B_SPLINE_CURVE_WITH_KNOTS('',3,(#149152,#149153,#149154,#149155),
 .UNSPECIFIED.,.F.,.F.,(4,4),(3.73816266135447,3.78897373388666),
 .UNSPECIFIED.);
#24045=B_SPLINE_CURVE_WITH_KNOTS('',3,(#149157,#149158,#149159,#149160,
#149161,#149162,#149163,#149164,#149165,#149166,#149167,#149168,#149169,
#149170,#149171,#149172,#149173),.UNSPECIFIED.,.F.,.F.,(4,2,2,2,3,2,2,4),
(0.0529024352810996,0.0551226000946487,0.0590534470355495,0.0612484958735367,
0.0634408290668853,0.0672969289521484,0.0711810086622316,0.0739890799314191),
 .UNSPECIFIED.);
#24046=B_SPLINE_CURVE_WITH_KNOTS('',3,(#149174,#149175,#149176,#149177),
 .UNSPECIFIED.,.F.,.F.,(4,4),(2.06733813088284,2.11814920343982),
 .UNSPECIFIED.);
#24047=B_SPLINE_CURVE_WITH_KNOTS('',3,(#149179,#149180,#149181,#149182),
 .UNSPECIFIED.,.F.,.F.,(4,4),(3.73816266067428,3.78897373321881),
 .UNSPECIFIED.);
#24048=B_SPLINE_CURVE_WITH_KNOTS('',3,(#149184,#149185,#149186,#149187,
#149188,#149189,#149190,#149191,#149192,#149193,#149194,#149195,#149196,
#149197,#149198,#149199,#149200),.UNSPECIFIED.,.F.,.F.,(4,2,2,2,3,2,2,4),
(0.0529024352649618,0.0551226000945426,0.0590534470351731,0.0612484958730819,
0.0634408290663741,0.0672969289517207,0.0711810086620141,0.07398908000207),
 .UNSPECIFIED.);
#24049=B_SPLINE_CURVE_WITH_KNOTS('',3,(#149201,#149202,#149203,#149204),
 .UNSPECIFIED.,.F.,.F.,(4,4),(2.06733813102838,2.118149203558),
 .UNSPECIFIED.);
#24050=B_SPLINE_CURVE_WITH_KNOTS('',3,(#149206,#149207,#149208,#149209),
 .UNSPECIFIED.,.F.,.F.,(4,4),(3.73816266066757,3.78897373314874),
 .UNSPECIFIED.);
#24051=B_SPLINE_CURVE_WITH_KNOTS('',3,(#149211,#149212,#149213,#149214,
#149215,#149216,#149217,#149218,#149219,#149220,#149221,#149222,#149223,
#149224,#149225,#149226,#149227),.UNSPECIFIED.,.F.,.F.,(4,2,2,2,3,2,2,4),
(0.0529024352349786,0.055122600095423,0.0590534470359997,0.0612484958738441,
0.0634408290670744,0.0672969289523512,0.071181008662676,0.0739890799320359),
 .UNSPECIFIED.);
#24052=B_SPLINE_CURVE_WITH_KNOTS('',3,(#149228,#149229,#149230,#149231),
 .UNSPECIFIED.,.F.,.F.,(4,4),(2.06733813103437,2.11814920362244),
 .UNSPECIFIED.);
#24053=B_SPLINE_CURVE_WITH_KNOTS('',3,(#149233,#149234,#149235,#149236),
 .UNSPECIFIED.,.F.,.F.,(4,4),(3.73816266144136,3.78897373397411),
 .UNSPECIFIED.);
#24054=B_SPLINE_CURVE_WITH_KNOTS('',3,(#149238,#149239,#149240,#149241,
#149242,#149243,#149244,#149245,#149246,#149247,#149248,#149249,#149250,
#149251,#149252,#149253,#149254),.UNSPECIFIED.,.F.,.F.,(4,2,2,2,3,2,2,4),
(0.052902435296,0.0551226000943973,0.0590534470353996,0.061248495873431,
0.0634408290668166,0.067296928952072,0.0711810086620752,0.0739890800025833),
 .UNSPECIFIED.);
#24055=B_SPLINE_CURVE_WITH_KNOTS('',3,(#149255,#149256,#149257,#149258),
 .UNSPECIFIED.,.F.,.F.,(4,4),(2.06733813083286,2.11814920335294),
 .UNSPECIFIED.);
#24056=B_SPLINE_CURVE_WITH_KNOTS('',3,(#149260,#149261,#149262,#149263),
 .UNSPECIFIED.,.F.,.F.,(4,4),(3.73816266015891,3.78897373268002),
 .UNSPECIFIED.);
#24057=B_SPLINE_CURVE_WITH_KNOTS('',3,(#149265,#149266,#149267,#149268,
#149269,#149270,#149271,#149272,#149273,#149274,#149275,#149276,#149277,
#149278,#149279,#149280,#149281),.UNSPECIFIED.,.F.,.F.,(4,2,2,2,3,2,2,4),
(0.0529024352568632,0.0551226000954583,0.0590534470358464,0.0612484958736338,
0.0634408290668215,0.0672969289521498,0.0711810086626215,0.0739890799166402),
 .UNSPECIFIED.);
#24058=B_SPLINE_CURVE_WITH_KNOTS('',3,(#149282,#149283,#149284,#149285),
 .UNSPECIFIED.,.F.,.F.,(4,4),(2.06733813113834,2.11814920367071),
 .UNSPECIFIED.);
#24059=B_SPLINE_CURVE_WITH_KNOTS('',3,(#149287,#149288,#149289,#149290),
 .UNSPECIFIED.,.F.,.F.,(4,4),(3.7381626611044,3.78897373365368),
 .UNSPECIFIED.);
#24060=B_SPLINE_CURVE_WITH_KNOTS('',3,(#149292,#149293,#149294,#149295,
#149296,#149297,#149298,#149299,#149300,#149301,#149302,#149303,#149304,
#149305,#149306,#149307,#149308),.UNSPECIFIED.,.F.,.F.,(4,2,2,2,3,2,2,4),
(0.0529024352810882,0.0551226000949496,0.0590534470357903,0.0612484958737411,
0.063440829067058,0.0672969289523027,0.0711810086624234,0.0739890799781007),
 .UNSPECIFIED.);
#24061=B_SPLINE_CURVE_WITH_KNOTS('',3,(#149309,#149310,#149311,#149312),
 .UNSPECIFIED.,.F.,.F.,(4,4),(2.06733813095668,2.11814920343747),
 .UNSPECIFIED.);
#24062=B_SPLINE_CURVE_WITH_KNOTS('',3,(#149314,#149315,#149316,#149317),
 .UNSPECIFIED.,.F.,.F.,(4,4),(3.73816266102959,3.78897373355911),
 .UNSPECIFIED.);
#24063=B_SPLINE_CURVE_WITH_KNOTS('',3,(#149319,#149320,#149321,#149322,
#149323,#149324,#149325,#149326,#149327,#149328,#149329,#149330,#149331,
#149332,#149333,#149334,#149335),.UNSPECIFIED.,.F.,.F.,(4,2,2,2,3,2,2,4),
(0.0529024352096333,0.0551226000944241,0.0590534470351423,0.0612484958730844,
0.0634408290664034,0.0672969289517397,0.071181008661968,0.0739890799467927),
 .UNSPECIFIED.);
#24064=B_SPLINE_CURVE_WITH_KNOTS('',3,(#149336,#149337,#149338,#149339),
 .UNSPECIFIED.,.F.,.F.,(4,4),(2.06733813091365,2.11814920351671),
 .UNSPECIFIED.);
#24065=B_SPLINE_CURVE_WITH_KNOTS('',3,(#149341,#149342,#149343,#149344),
 .UNSPECIFIED.,.F.,.F.,(4,4),(3.73816266050385,3.78897373306035),
 .UNSPECIFIED.);
#24066=B_SPLINE_CURVE_WITH_KNOTS('',3,(#149346,#149347,#149348,#149349,
#149350,#149351,#149352,#149353,#149354,#149355,#149356,#149357,#149358,
#149359,#149360,#149361,#149362),.UNSPECIFIED.,.F.,.F.,(4,2,2,2,3,2,2,4),
(0.0529024352812999,0.0551226000952955,0.0590534470357909,0.0612484958736166,
0.0634408290668356,0.0672969289521453,0.0711810086625308,0.0739890799977917),
 .UNSPECIFIED.);
#24067=B_SPLINE_CURVE_WITH_KNOTS('',3,(#149363,#149364,#149365,#149366),
 .UNSPECIFIED.,.F.,.F.,(4,4),(2.06733813112279,2.11814920361366),
 .UNSPECIFIED.);
#24068=B_SPLINE_CURVE_WITH_KNOTS('',3,(#149368,#149369,#149370,#149371),
 .UNSPECIFIED.,.F.,.F.,(4,4),(3.73816266180585,3.78897373432959),
 .UNSPECIFIED.);
#24069=B_SPLINE_CURVE_WITH_KNOTS('',3,(#149373,#149374,#149375,#149376,
#149377,#149378,#149379,#149380,#149381,#149382,#149383,#149384,#149385,
#149386,#149387,#149388,#149389),.UNSPECIFIED.,.F.,.F.,(4,2,2,2,3,2,2,4),
(0.0529024353383955,0.0551226000952457,0.0590534470363997,0.0612484958744295,
0.063440829067801,0.0672969289529328,0.0711810086628092,0.0739890799666374),
 .UNSPECIFIED.);
#24070=B_SPLINE_CURVE_WITH_KNOTS('',3,(#149390,#149391,#149392,#149393),
 .UNSPECIFIED.,.F.,.F.,(4,4),(2.06733813079015,2.11814920328276),
 .UNSPECIFIED.);
#24071=B_SPLINE_CURVE_WITH_KNOTS('',3,(#149395,#149396,#149397,#149398),
 .UNSPECIFIED.,.F.,.F.,(4,4),(3.73816266000277,3.78897373256649),
 .UNSPECIFIED.);
#24072=B_SPLINE_CURVE_WITH_KNOTS('',3,(#149400,#149401,#149402,#149403,
#149404,#149405,#149406,#149407,#149408,#149409,#149410,#149411,#149412,
#149413,#149414,#149415,#149416),.UNSPECIFIED.,.F.,.F.,(4,2,2,2,3,2,2,4),
(0.0529024352884472,0.0551226000962587,0.0590534470366154,0.0612484958743516,
0.0634408290674888,0.0672969289527537,0.0711810086632452,0.0739890798862568),
 .UNSPECIFIED.);
#24073=B_SPLINE_CURVE_WITH_KNOTS('',3,(#149417,#149418,#149419,#149420),
 .UNSPECIFIED.,.F.,.F.,(4,4),(2.06733813118411,2.11814920373392),
 .UNSPECIFIED.);
#24074=B_SPLINE_CURVE_WITH_KNOTS('',3,(#149422,#149423,#149424,#149425),
 .UNSPECIFIED.,.F.,.F.,(4,4),(3.73816265981561,3.78897373232902),
 .UNSPECIFIED.);
#24075=B_SPLINE_CURVE_WITH_KNOTS('',3,(#149427,#149428,#149429,#149430,
#149431,#149432,#149433,#149434,#149435,#149436,#149437,#149438,#149439,
#149440,#149441,#149442,#149443),.UNSPECIFIED.,.F.,.F.,(4,2,2,2,3,2,2,4),
(0.0529024351998951,0.0551226000958251,0.0590534470360602,0.0612484958737785,
0.0634408290669098,0.0672969289522405,0.0711810086628216,0.0739890799252331),
 .UNSPECIFIED.);
#24076=B_SPLINE_CURVE_WITH_KNOTS('',3,(#149444,#149445,#149446,#149447),
 .UNSPECIFIED.,.F.,.F.,(4,4),(2.06733813124236,2.11814920376004),
 .UNSPECIFIED.);
#24077=B_SPLINE_CURVE_WITH_KNOTS('',3,(#149449,#149450,#149451,#149452),
 .UNSPECIFIED.,.F.,.F.,(4,4),(3.73816266168605,3.78897373417608),
 .UNSPECIFIED.);
#24078=B_SPLINE_CURVE_WITH_KNOTS('',3,(#149454,#149455,#149456,#149457,
#149458,#149459,#149460,#149461,#149462,#149463,#149464,#149465,#149466,
#149467,#149468,#149469,#149470),.UNSPECIFIED.,.F.,.F.,(4,2,2,2,3,2,2,4),
(0.0529024352984499,0.05512260009477,0.0590534470358401,0.0612484958738678,
0.0634408290672449,0.0672969289524419,0.0711810086623853,0.0739890800310274),
 .UNSPECIFIED.);
#24079=B_SPLINE_CURVE_WITH_KNOTS('',3,(#149471,#149472,#149473,#149474),
 .UNSPECIFIED.,.F.,.F.,(4,4),(2.06733813082859,2.11814920332163),
 .UNSPECIFIED.);
#24080=B_SPLINE_CURVE_WITH_KNOTS('',3,(#149476,#149477,#149478,#149479),
 .UNSPECIFIED.,.F.,.F.,(4,4),(3.73816266070724,3.78897373325739),
 .UNSPECIFIED.);
#24081=B_SPLINE_CURVE_WITH_KNOTS('',3,(#149481,#149482,#149483,#149484,
#149485,#149486,#149487,#149488,#149489,#149490,#149491,#149492,#149493,
#149494,#149495,#149496,#149497),.UNSPECIFIED.,.F.,.F.,(4,2,2,2,3,2,2,4),
(0.0529024352251411,0.0551226000947361,0.0590534470353222,0.0612484958732058,
0.0634408290664763,0.0672969289518134,0.0711810086621348,0.0739890799592117),
 .UNSPECIFIED.);
#24082=B_SPLINE_CURVE_WITH_KNOTS('',3,(#149498,#149499,#149500,#149501),
 .UNSPECIFIED.,.F.,.F.,(4,4),(2.06733813102795,2.1181492036115),
 .UNSPECIFIED.);
#24083=B_SPLINE_CURVE_WITH_KNOTS('',3,(#149503,#149504,#149505,#149506),
 .UNSPECIFIED.,.F.,.F.,(4,4),(3.73816266082592,3.78897373338695),
 .UNSPECIFIED.);
#24084=B_SPLINE_CURVE_WITH_KNOTS('',3,(#149508,#149509,#149510,#149511,
#149512,#149513,#149514,#149515,#149516,#149517,#149518,#149519,#149520,
#149521,#149522,#149523,#149524),.UNSPECIFIED.,.F.,.F.,(4,2,2,2,3,2,2,4),
(0.0529024352857602,0.0551226000951809,0.0590534470358672,0.0612484958737567,
0.0634408290670247,0.0672969289522904,0.0711810086625272,0.0739890799778034),
 .UNSPECIFIED.);
#24085=B_SPLINE_CURVE_WITH_KNOTS('',3,(#149525,#149526,#149527,#149528),
 .UNSPECIFIED.,.F.,.F.,(4,4),(2.06733813096253,2.11814920348551),
 .UNSPECIFIED.);
#24086=B_SPLINE_CURVE_WITH_KNOTS('',3,(#149530,#149531,#149532,#149533),
 .UNSPECIFIED.,.F.,.F.,(4,4),(3.73816266099154,3.78897373347697),
 .UNSPECIFIED.);
#24087=B_SPLINE_CURVE_WITH_KNOTS('',3,(#149535,#149536,#149537,#149538,
#149539,#149540,#149541,#149542,#149543,#149544,#149545,#149546,#149547,
#149548,#149549,#149550,#149551),.UNSPECIFIED.,.F.,.F.,(4,2,2,2,3,2,2,4),
(0.0529024352652794,0.0551226000958151,0.0590534470365479,0.061248495874416,
0.0634408290676581,0.0672969289528476,0.0711810086630389,0.0739890798870025),
 .UNSPECIFIED.);
#24088=B_SPLINE_CURVE_WITH_KNOTS('',3,(#149552,#149553,#149554,#149555),
 .UNSPECIFIED.,.F.,.F.,(4,4),(2.06733813099677,2.11814920357114),
 .UNSPECIFIED.);
#24089=B_SPLINE_CURVE_WITH_KNOTS('',3,(#149557,#149558,#149559,#149560),
 .UNSPECIFIED.,.F.,.F.,(4,4),(3.73816266177326,3.78897373423991),
 .UNSPECIFIED.);
#24090=B_SPLINE_CURVE_WITH_KNOTS('',3,(#149562,#149563,#149564,#149565,
#149566,#149567,#149568,#149569,#149570,#149571,#149572,#149573,#149574,
#149575,#149576,#149577,#149578),.UNSPECIFIED.,.F.,.F.,(4,2,2,2,3,2,2,4),
(0.0529024353175172,0.0551226000947811,0.0590534470359366,0.0612484958739924,
0.06344082906739,0.0672969289525678,0.0711810086624502,0.0739890799149026),
 .UNSPECIFIED.);
#24091=B_SPLINE_CURVE_WITH_KNOTS('',3,(#149579,#149580,#149581,#149582),
 .UNSPECIFIED.,.F.,.F.,(4,4),(2.06733813072299,2.11814920329931),
 .UNSPECIFIED.);
#24092=B_SPLINE_CURVE_WITH_KNOTS('',3,(#149584,#149585,#149586,#149587),
 .UNSPECIFIED.,.F.,.F.,(4,4),(3.73816266115613,3.78897373364958),
 .UNSPECIFIED.);
#24093=B_SPLINE_CURVE_WITH_KNOTS('',3,(#149589,#149590,#149591,#149592,
#149593,#149594,#149595,#149596,#149597,#149598,#149599,#149600,#149601,
#149602,#149603,#149604,#149605),.UNSPECIFIED.,.F.,.F.,(4,2,2,2,3,2,2,4),
(0.0529024352663513,0.0551226000950634,0.0590534470358615,0.0612484958737945,
0.063440829067096,0.0672969289523489,0.0711810086625087,0.0739890799450185),
 .UNSPECIFIED.);
#24094=B_SPLINE_CURVE_WITH_KNOTS('',3,(#149606,#149607,#149608,#149609),
 .UNSPECIFIED.,.F.,.F.,(4,4),(2.0673381309676,2.11814920343851),
 .UNSPECIFIED.);
#24095=B_SPLINE_CURVE_WITH_KNOTS('',3,(#149611,#149612,#149613,#149614),
 .UNSPECIFIED.,.F.,.F.,(4,4),(3.73816266123958,3.78897373374303),
 .UNSPECIFIED.);
#24096=B_SPLINE_CURVE_WITH_KNOTS('',3,(#149616,#149617,#149618,#149619,
#149620,#149621,#149622,#149623,#149624,#149625,#149626,#149627,#149628,
#149629,#149630,#149631,#149632),.UNSPECIFIED.,.F.,.F.,(4,2,2,2,3,2,2,4),
(0.0529024352695509,0.0551226000945128,0.0590534470353782,0.0612484958733598,
0.0634408290667064,0.0672969289519894,0.0711810086620986,0.0739890799729215),
 .UNSPECIFIED.);
#24097=B_SPLINE_CURVE_WITH_KNOTS('',3,(#149633,#149634,#149635,#149636),
 .UNSPECIFIED.,.F.,.F.,(4,4),(2.06733813089893,2.11814920345363),
 .UNSPECIFIED.);
#24098=B_SPLINE_CURVE_WITH_KNOTS('',3,(#149638,#149639,#149640,#149641),
 .UNSPECIFIED.,.F.,.F.,(4,4),(3.73816266031907,3.78897373284873),
 .UNSPECIFIED.);
#24099=B_SPLINE_CURVE_WITH_KNOTS('',3,(#149643,#149644,#149645,#149646,
#149647,#149648,#149649,#149650,#149651,#149652,#149653,#149654,#149655,
#149656,#149657,#149658,#149659),.UNSPECIFIED.,.F.,.F.,(4,2,2,2,3,2,2,4),
(0.0529024352652488,0.0551226000956238,0.0590534470360699,0.0612484958738631,
0.0634408290670526,0.0672969289523439,0.0711810086627632,0.0739890799683483),
 .UNSPECIFIED.);
#24100=B_SPLINE_CURVE_WITH_KNOTS('',3,(#149660,#149661,#149662,#149663),
 .UNSPECIFIED.,.F.,.F.,(4,4),(2.06733813117357,2.11814920366994),
 .UNSPECIFIED.);
#24101=B_SPLINE_CURVE_WITH_KNOTS('',3,(#149665,#149666,#149667,#149668),
 .UNSPECIFIED.,.F.,.F.,(4,4),(3.73816266063489,3.78897373319568),
 .UNSPECIFIED.);
#24102=B_SPLINE_CURVE_WITH_KNOTS('',3,(#149670,#149671,#149672,#149673,
#149674,#149675,#149676,#149677,#149678,#149679,#149680,#149681,#149682,
#149683,#149684,#149685,#149686),.UNSPECIFIED.,.F.,.F.,(4,2,2,2,3,2,2,4),
(0.0529024353177713,0.0551226000957727,0.0590534470364281,0.0612484958742786,
0.0634408290675083,0.0672969289527308,0.0711810086629895,0.0739890799725923),
 .UNSPECIFIED.);
#24103=B_SPLINE_CURVE_WITH_KNOTS('',3,(#149687,#149688,#149689,#149690),
 .UNSPECIFIED.,.F.,.F.,(4,4),(2.06733813102884,2.1181492034784),
 .UNSPECIFIED.);
#24104=B_SPLINE_CURVE_WITH_KNOTS('',3,(#149692,#149693,#149694,#149695),
 .UNSPECIFIED.,.F.,.F.,(4,4),(3.73816266078816,3.78897373330558),
 .UNSPECIFIED.);
#24105=B_SPLINE_CURVE_WITH_KNOTS('',3,(#149697,#149698,#149699,#149700,
#149701,#149702,#149703,#149704,#149705,#149706,#149707,#149708,#149709,
#149710,#149711,#149712,#149713),.UNSPECIFIED.,.F.,.F.,(4,2,2,2,3,2,2,4),
(0.052902435323927,0.0551226000960778,0.0590534470367477,0.061248495874586,
0.063440829067802,0.0672969289529904,0.0711810086632352,0.0739890799109451),
 .UNSPECIFIED.);
#24106=B_SPLINE_CURVE_WITH_KNOTS('',3,(#149714,#149715,#149716,#149717),
 .UNSPECIFIED.,.F.,.F.,(4,4),(2.0673381310135,2.11814920352267),
 .UNSPECIFIED.);
#24107=B_SPLINE_CURVE_WITH_KNOTS('',3,(#149718,#149719,#149720,#149721),
 .UNSPECIFIED.,.F.,.F.,(4,4),(3.73816266085093,3.78897373334859),
 .UNSPECIFIED.);
#24108=B_SPLINE_CURVE_WITH_KNOTS('',3,(#149726,#149727,#149728,#149729,
#149730,#149731,#149732,#149733,#149734,#149735),.UNSPECIFIED.,.F.,.F.,
(4,2,2,2,4),(0.0714824588585375,0.0744292845751612,0.0776622687682114,0.0817097633455992,
0.0826589280268188),.UNSPECIFIED.);
#24109=B_SPLINE_CURVE_WITH_KNOTS('',3,(#149736,#149737,#149738,#149739,
#149740,#149741),.UNSPECIFIED.,.F.,.F.,(4,2,4),(1.49996604605074,1.51351365753382,
1.57686258981781),.UNSPECIFIED.);
#24110=B_SPLINE_CURVE_WITH_KNOTS('',3,(#149743,#149744,#149745,#149746,
#149747,#149748),.UNSPECIFIED.,.F.,.F.,(4,2,4),(1.33957856730954,1.40292749963475,
1.41647511111458),.UNSPECIFIED.);
#24111=B_SPLINE_CURVE_WITH_KNOTS('',3,(#149750,#149751,#149752,#149753,
#149754,#149755,#149756,#149757,#149758,#149759,#149760,#149761,#149762,
#149763,#149764,#149765,#149766,#149767,#149768),.UNSPECIFIED.,.F.,.F.,
(4,2,2,2,3,2,2,2,4),(0.060099258269106,0.0615656153041754,0.0659612937711943,
0.0687970446775909,0.0714824588631871,0.074429284579545,0.0776622687720683,
0.0817097633487688,0.0826589280202759),.UNSPECIFIED.);
#24112=B_SPLINE_CURVE_WITH_KNOTS('',3,(#149769,#149770,#149771,#149772,
#149773,#149774),.UNSPECIFIED.,.F.,.F.,(4,2,4),(1.499966046113,1.51351365756774,
1.57686258990272),.UNSPECIFIED.);
#24113=B_SPLINE_CURVE_WITH_KNOTS('',3,(#149776,#149777,#149778,#149779,
#149780,#149781),.UNSPECIFIED.,.F.,.F.,(4,2,4),(1.33957856732956,1.40292749963323,
1.41647511110724),.UNSPECIFIED.);
#24114=B_SPLINE_CURVE_WITH_KNOTS('',3,(#149783,#149784,#149785,#149786,
#149787,#149788,#149789,#149790,#149791,#149792,#149793,#149794,#149795,
#149796,#149797,#149798,#149799,#149800,#149801),.UNSPECIFIED.,.F.,.F.,
(4,2,2,2,3,2,2,2,4),(0.060099258231316,0.0615656153015067,0.0659612937681578,
0.0687970446741911,0.0714824588595198,0.0744292845761485,0.077662268768905,
0.081709763345669,0.0826589280244342),.UNSPECIFIED.);
#24115=B_SPLINE_CURVE_WITH_KNOTS('',3,(#149802,#149803,#149804,#149805,
#149806,#149807),.UNSPECIFIED.,.F.,.F.,(4,2,4),(1.49996604607687,1.51351365757256,
1.5768625898645),.UNSPECIFIED.);
#24116=B_SPLINE_CURVE_WITH_KNOTS('',3,(#149809,#149810,#149811,#149812,
#149813,#149814),.UNSPECIFIED.,.F.,.F.,(4,2,4),(1.33957856716701,1.40292749942639,
1.41647511094955),.UNSPECIFIED.);
#24117=B_SPLINE_CURVE_WITH_KNOTS('',3,(#149816,#149817,#149818,#149819,
#149820,#149821,#149822,#149823,#149824,#149825,#149826,#149827,#149828,
#149829,#149830,#149831,#149832,#149833,#149834),.UNSPECIFIED.,.F.,.F.,
(4,2,2,2,3,2,2,2,4),(0.0600992582102493,0.0615656152977947,0.0659612937657737,
0.0687970446720995,0.0714824588576289,0.0744292845745221,0.0776622687668052,
0.0817097633421903,0.0826589280636074),.UNSPECIFIED.);
#24118=B_SPLINE_CURVE_WITH_KNOTS('',3,(#149835,#149836,#149837,#149838,
#149839,#149840),.UNSPECIFIED.,.F.,.F.,(4,2,4),(1.49996604614834,1.51351365759482,
1.5768625899084),.UNSPECIFIED.);
#24119=B_SPLINE_CURVE_WITH_KNOTS('',3,(#149842,#149843,#149844,#149845,
#149846,#149847),.UNSPECIFIED.,.F.,.F.,(4,2,4),(1.33957856752927,1.40292749981418,
1.41647511131301),.UNSPECIFIED.);
#24120=B_SPLINE_CURVE_WITH_KNOTS('',3,(#149849,#149850,#149851,#149852,
#149853,#149854,#149855,#149856,#149857,#149858,#149859,#149860,#149861,
#149862,#149863,#149864,#149865,#149866,#149867),.UNSPECIFIED.,.F.,.F.,
(4,2,2,2,3,2,2,2,4),(0.0600992581695721,0.0615656152962615,0.0659612937594313,
0.0687970446634821,0.0714824588473559,0.0744292845648293,0.0776622687592538,
0.0817097633381737,0.0826589280790036),.UNSPECIFIED.);
#24121=B_SPLINE_CURVE_WITH_KNOTS('',3,(#149868,#149869,#149870,#149871,
#149872,#149873),.UNSPECIFIED.,.F.,.F.,(4,2,4),(1.49996604595889,1.51351365749176,
1.57686258972957),.UNSPECIFIED.);
#24122=B_SPLINE_CURVE_WITH_KNOTS('',3,(#149875,#149876,#149877,#149878,
#149879,#149880),.UNSPECIFIED.,.F.,.F.,(4,2,4),(1.33957856752258,1.40292749978992,
1.41647511126154),.UNSPECIFIED.);
#24123=B_SPLINE_CURVE_WITH_KNOTS('',3,(#149882,#149883,#149884,#149885,
#149886,#149887,#149888,#149889,#149890,#149891,#149892,#149893,#149894,
#149895,#149896,#149897,#149898,#149899,#149900),.UNSPECIFIED.,.F.,.F.,
(4,2,2,2,3,2,2,2,4),(0.0600992582011184,0.0615656152986744,0.0659612937631065,
0.0687970446679523,0.0714824588524144,0.0744292845695169,0.0776622687632943,
0.0817097633414514,0.082658928035348),.UNSPECIFIED.);
#24124=B_SPLINE_CURVE_WITH_KNOTS('',3,(#149901,#149902,#149903,#149904,
#149905,#149906),.UNSPECIFIED.,.F.,.F.,(4,2,4),(1.49996604601399,1.51351365750487,
1.57686258982041),.UNSPECIFIED.);
#24125=B_SPLINE_CURVE_WITH_KNOTS('',3,(#149908,#149909,#149910,#149911,
#149912,#149913),.UNSPECIFIED.,.F.,.F.,(4,2,4),(1.33957856772149,1.40292750006868,
1.41647511150785),.UNSPECIFIED.);
#24126=B_SPLINE_CURVE_WITH_KNOTS('',3,(#149915,#149916,#149917,#149918,
#149919,#149920,#149921,#149922,#149923,#149924,#149925,#149926,#149927,
#149928,#149929,#149930,#149931,#149932,#149933),.UNSPECIFIED.,.F.,.F.,
(4,2,2,2,3,2,2,2,4),(0.0600992582193096,0.0615656153013013,0.0659612937627021,
0.0687970446664693,0.0714824588501472,0.0744292845671558,0.0776622687621161,
0.0817097633428454,0.0826589280107226),.UNSPECIFIED.);
#24127=B_SPLINE_CURVE_WITH_KNOTS('',3,(#149934,#149935,#149936,#149937,
#149938,#149939),.UNSPECIFIED.,.F.,.F.,(4,2,4),(1.49996604587209,1.51351365743327,
1.57686258967902),.UNSPECIFIED.);
#24128=B_SPLINE_CURVE_WITH_KNOTS('',3,(#149941,#149942,#149943,#149944,
#149945,#149946),.UNSPECIFIED.,.F.,.F.,(4,2,4),(1.33957856735936,1.40292749966726,
1.41647511117744),.UNSPECIFIED.);
#24129=B_SPLINE_CURVE_WITH_KNOTS('',3,(#149948,#149949,#149950,#149951,
#149952,#149953,#149954,#149955,#149956,#149957,#149958,#149959,#149960,
#149961,#149962,#149963,#149964,#149965,#149966),.UNSPECIFIED.,.F.,.F.,
(4,2,2,2,3,2,2,2,4),(0.0600992582674632,0.0615656153040191,0.065961293770234,
0.0687970446762131,0.071482458861508,0.0744292845779795,0.0776622687708636,
0.081709763348141,0.0826589280360798),.UNSPECIFIED.);
#24130=B_SPLINE_CURVE_WITH_KNOTS('',3,(#149967,#149968,#149969,#149970,
#149971,#149972),.UNSPECIFIED.,.F.,.F.,(4,2,4),(1.49996604600416,1.51351365750855,
1.57686258981381),.UNSPECIFIED.);
#24131=B_SPLINE_CURVE_WITH_KNOTS('',3,(#149974,#149975,#149976,#149977,
#149978,#149979),.UNSPECIFIED.,.F.,.F.,(4,2,4),(1.33957856738494,1.40292749967249,
1.41647511116503),.UNSPECIFIED.);
#24132=B_SPLINE_CURVE_WITH_KNOTS('',3,(#149981,#149982,#149983,#149984,
#149985,#149986,#149987,#149988,#149989,#149990,#149991,#149992,#149993,
#149994,#149995,#149996,#149997,#149998,#149999),.UNSPECIFIED.,.F.,.F.,
(4,2,2,2,3,2,2,2,4),(0.0600992582017652,0.0615656152976751,0.0659612937631273,
0.0687970446684009,0.0714824588531702,0.0744292845702252,0.0776622687635618,
0.0817097633408794,0.0826589280495392),.UNSPECIFIED.);
#24133=B_SPLINE_CURVE_WITH_KNOTS('',3,(#150000,#150001,#150002,#150003,
#150004,#150005),.UNSPECIFIED.,.F.,.F.,(4,2,4),(1.49996604604657,1.51351365754362,
1.57686258983577),.UNSPECIFIED.);
#24134=B_SPLINE_CURVE_WITH_KNOTS('',3,(#150007,#150008,#150009,#150010,
#150011,#150012),.UNSPECIFIED.,.F.,.F.,(4,2,4),(1.33957856727904,1.40292749957447,
1.41647511106941),.UNSPECIFIED.);
#24135=B_SPLINE_CURVE_WITH_KNOTS('',3,(#150014,#150015,#150016,#150017,
#150018,#150019,#150020,#150021,#150022,#150023,#150024,#150025,#150026,
#150027,#150028,#150029,#150030,#150031,#150032),.UNSPECIFIED.,.F.,.F.,
(4,2,2,2,3,2,2,2,4),(0.0600992581799993,0.0615656152943915,0.0659612937600584,
0.068797044664993,0.0714824588495034,0.0744292845670047,0.0776622687604493,
0.0817097633372922,0.0826589280917478),.UNSPECIFIED.);
#24136=B_SPLINE_CURVE_WITH_KNOTS('',3,(#150033,#150034,#150035,#150036,
#150037,#150038),.UNSPECIFIED.,.F.,.F.,(4,2,4),(1.49996604606282,1.51351365753196,
1.57686258981422),.UNSPECIFIED.);
#24137=B_SPLINE_CURVE_WITH_KNOTS('',3,(#150040,#150041,#150042,#150043,
#150044,#150045),.UNSPECIFIED.,.F.,.F.,(4,2,4),(1.33957856759873,1.40292749993747,
1.41647511140743),.UNSPECIFIED.);
#24138=B_SPLINE_CURVE_WITH_KNOTS('',3,(#150047,#150048,#150049,#150050,
#150051,#150052,#150053,#150054,#150055,#150056,#150057,#150058,#150059,
#150060,#150061,#150062,#150063,#150064,#150065),.UNSPECIFIED.,.F.,.F.,
(4,2,2,2,3,2,2,2,4),(0.0600992581996879,0.0615656152994879,0.0659612937614183,
0.0687970446653839,0.0714824588492078,0.0744292845662641,0.0776622687609925,
0.0817097633411702,0.0826589280132682),.UNSPECIFIED.);
#24139=B_SPLINE_CURVE_WITH_KNOTS('',3,(#150066,#150067,#150068,#150069,
#150070,#150071),.UNSPECIFIED.,.F.,.F.,(4,2,4),(1.49996604591879,1.51351365743313,
1.57686258971772),.UNSPECIFIED.);
#24140=B_SPLINE_CURVE_WITH_KNOTS('',3,(#150073,#150074,#150075,#150076,
#150077,#150078),.UNSPECIFIED.,.F.,.F.,(4,2,4),(1.3395785670504,1.40292749929253,
1.41647511082944),.UNSPECIFIED.);
#24141=B_SPLINE_CURVE_WITH_KNOTS('',3,(#150080,#150081,#150082,#150083,
#150084,#150085,#150086,#150087,#150088,#150089,#150090,#150091,#150092,
#150093,#150094,#150095,#150096,#150097,#150098),.UNSPECIFIED.,.F.,.F.,
(4,2,2,2,3,2,2,2,4),(0.0600992582212704,0.0615656152959939,0.065961293765843,
0.0687970446728489,0.0714824588588726,0.0744292845757802,0.0776622687673179,
0.0817097633411337,0.0826589280883185),.UNSPECIFIED.);
#24142=B_SPLINE_CURVE_WITH_KNOTS('',3,(#150099,#150100,#150101,#150102,
#150103,#150104),.UNSPECIFIED.,.F.,.F.,(4,2,4),(1.49996604617379,1.51351365761947,
1.5768625899443),.UNSPECIFIED.);
#24143=B_SPLINE_CURVE_WITH_KNOTS('',3,(#150106,#150107,#150108,#150109,
#150110,#150111),.UNSPECIFIED.,.F.,.F.,(4,2,4),(1.33957856714172,1.40292749936937,
1.41647511087422),.UNSPECIFIED.);
#24144=B_SPLINE_CURVE_WITH_KNOTS('',3,(#150113,#150114,#150115,#150116,
#150117,#150118,#150119,#150120,#150121,#150122,#150123,#150124,#150125,
#150126,#150127,#150128,#150129,#150130,#150131),.UNSPECIFIED.,.F.,.F.,
(4,2,2,2,3,2,2,2,4),(0.0600992582306656,0.0615656152998404,0.065961293769387,
0.0687970446765956,0.0714824588627838,0.0744292845793006,0.0776622687708418,
0.0817097633452896,0.0826589280442809),.UNSPECIFIED.);
#24145=B_SPLINE_CURVE_WITH_KNOTS('',3,(#150132,#150133,#150134,#150135,
#150136,#150137),.UNSPECIFIED.,.F.,.F.,(4,2,4),(1.4999660461885,1.51351365763824,
1.57686258995467),.UNSPECIFIED.);
#24146=B_SPLINE_CURVE_WITH_KNOTS('',3,(#150139,#150140,#150141,#150142,
#150143,#150144),.UNSPECIFIED.,.F.,.F.,(4,2,4),(1.33957856767546,1.402927500014,
1.41647511143919),.UNSPECIFIED.);
#24147=B_SPLINE_CURVE_WITH_KNOTS('',3,(#150146,#150147,#150148,#150149,
#150150,#150151,#150152,#150153,#150154,#150155,#150156,#150157,#150158,
#150159,#150160,#150161,#150162,#150163,#150164),.UNSPECIFIED.,.F.,.F.,
(4,2,2,2,3,2,2,2,4),(0.0600992582048306,0.0615656153055392,0.0659612937676691,
0.0687970446720172,0.0714824588561295,0.0744292845727573,0.0776622687673379,
0.081709763347868,0.082658927996682),.UNSPECIFIED.);
#24148=B_SPLINE_CURVE_WITH_KNOTS('',3,(#150165,#150166,#150167,#150168,
#150169,#150170),.UNSPECIFIED.,.F.,.F.,(4,2,4),(1.49996604592438,1.51351365744584,
1.57686258971838),.UNSPECIFIED.);
#24149=B_SPLINE_CURVE_WITH_KNOTS('',3,(#150172,#150173,#150174,#150175,
#150176,#150177),.UNSPECIFIED.,.F.,.F.,(4,2,4),(1.33957856718658,1.40292749947563,
1.41647511098612),.UNSPECIFIED.);
#24150=B_SPLINE_CURVE_WITH_KNOTS('',3,(#150179,#150180,#150181,#150182,
#150183,#150184,#150185,#150186,#150187,#150188,#150189,#150190,#150191,
#150192,#150193,#150194,#150195,#150196,#150197),.UNSPECIFIED.,.F.,.F.,
(4,2,2,2,3,2,2,2,4),(0.0600992581919431,0.0615656152953891,0.0659612937624275,
0.0687970446682301,0.0714824588533791,0.0744292845705114,0.0776622687632403,
0.0817097633391975,0.082658928079642),.UNSPECIFIED.);
#24151=B_SPLINE_CURVE_WITH_KNOTS('',3,(#150198,#150199,#150200,#150201,
#150202,#150203),.UNSPECIFIED.,.F.,.F.,(4,2,4),(1.49996604614892,1.51351365760524,
1.57686258992143),.UNSPECIFIED.);
#24152=B_SPLINE_CURVE_WITH_KNOTS('',3,(#150205,#150206,#150207,#150208,
#150209,#150210),.UNSPECIFIED.,.F.,.F.,(4,2,4),(1.33957856738739,1.40292749971882,
1.41647511118057),.UNSPECIFIED.);
#24153=B_SPLINE_CURVE_WITH_KNOTS('',3,(#150212,#150213,#150214,#150215,
#150216,#150217,#150218,#150219,#150220,#150221,#150222,#150223,#150224,
#150225,#150226,#150227,#150228,#150229,#150230),.UNSPECIFIED.,.F.,.F.,
(4,2,2,2,3,2,2,2,4),(0.0600992581812674,0.0615656152920304,0.0659612937560849,
0.0687970446603106,0.0714824588443023,0.0744292845619897,0.0776622687560912,
0.0817097633340036,0.0826589280667293),.UNSPECIFIED.);
#24154=B_SPLINE_CURVE_WITH_KNOTS('',3,(#150231,#150232,#150233,#150234,
#150235,#150236),.UNSPECIFIED.,.F.,.F.,(4,2,4),(1.49996604599013,1.51351365748729,
1.57686258978608),.UNSPECIFIED.);
#24155=B_SPLINE_CURVE_WITH_KNOTS('',3,(#150238,#150239,#150240,#150241,
#150242,#150243),.UNSPECIFIED.,.F.,.F.,(4,2,4),(1.33957856745805,1.40292749978122,
1.41647511124377),.UNSPECIFIED.);
#24156=B_SPLINE_CURVE_WITH_KNOTS('',3,(#150245,#150246,#150247,#150248,
#150249,#150250,#150251,#150252,#150253,#150254,#150255,#150256,#150257,
#150258,#150259,#150260,#150261,#150262,#150263),.UNSPECIFIED.,.F.,.F.,
(4,2,2,2,3,2,2,2,4),(0.0600992581991858,0.0615656152976462,0.0659612937615794,
0.0687970446662435,0.0714824588505711,0.074429284567676,0.0776622687616273,
0.08170976334013,0.0826589280525907),.UNSPECIFIED.);
#24157=B_SPLINE_CURVE_WITH_KNOTS('',3,(#150264,#150265,#150266,#150267,
#150268,#150269),.UNSPECIFIED.,.F.,.F.,(4,2,4),(1.49996604596708,1.51351365748614,
1.57686258973189),.UNSPECIFIED.);
#24158=B_SPLINE_CURVE_WITH_KNOTS('',3,(#150271,#150272,#150273,#150274,
#150275,#150276),.UNSPECIFIED.,.F.,.F.,(4,2,4),(1.33957856720859,1.40292749944731,
1.41647511096857),.UNSPECIFIED.);
#24159=B_SPLINE_CURVE_WITH_KNOTS('',3,(#150278,#150279,#150280,#150281,
#150282,#150283,#150284,#150285,#150286,#150287,#150288,#150289,#150290,
#150291,#150292,#150293,#150294,#150295,#150296),.UNSPECIFIED.,.F.,.F.,
(4,2,2,2,3,2,2,2,4),(0.0600992582031889,0.0615656152966673,0.0659612937648836,
0.0687970446710848,0.0714824588565221,0.0744292845736361,0.0776622687659337,
0.0817097633410083,0.0826589280509826),.UNSPECIFIED.);
#24160=B_SPLINE_CURVE_WITH_KNOTS('',3,(#150297,#150298,#150299,#150300,
#150301,#150302),.UNSPECIFIED.,.F.,.F.,(4,2,4),(1.49996604614752,1.51351365761189,
1.57686258994074),.UNSPECIFIED.);
#24161=B_SPLINE_CURVE_WITH_KNOTS('',3,(#150304,#150305,#150306,#150307,
#150308,#150309),.UNSPECIFIED.,.F.,.F.,(4,2,4),(1.33957856755016,1.40292749991405,
1.41647511134939),.UNSPECIFIED.);
#24162=B_SPLINE_CURVE_WITH_KNOTS('',3,(#150311,#150312,#150313,#150314,
#150315,#150316,#150317,#150318,#150319,#150320,#150321,#150322,#150323,
#150324,#150325,#150326,#150327,#150328,#150329),.UNSPECIFIED.,.F.,.F.,
(4,2,2,2,3,2,2,2,4),(0.0600992581724971,0.0615656152971063,0.0659612937590036,
0.0687970446626092,0.071482458846168,0.074429284563624,0.077662268758557,
0.0817097633385553,0.0826589280552966),.UNSPECIFIED.);
#24163=B_SPLINE_CURVE_WITH_KNOTS('',3,(#150330,#150331,#150332,#150333,
#150334,#150335),.UNSPECIFIED.,.F.,.F.,(4,2,4),(1.49996604592509,1.51351365746294,
1.57686258968125),.UNSPECIFIED.);
#24164=B_SPLINE_CURVE_WITH_KNOTS('',3,(#150337,#150338,#150339,#150340,
#150341,#150342),.UNSPECIFIED.,.F.,.F.,(4,2,4),(1.33957856728706,1.40292749954936,
1.41647511104989),.UNSPECIFIED.);
#24165=B_SPLINE_CURVE_WITH_KNOTS('',3,(#150344,#150345,#150346,#150347,
#150348,#150349,#150350,#150351,#150352,#150353,#150354,#150355,#150356,
#150357,#150358,#150359,#150360,#150361,#150362),.UNSPECIFIED.,.F.,.F.,
(4,2,2,2,3,2,2,2,4),(0.0600992581983925,0.0615656152984988,0.0659612937652178,
0.068797044671002,0.0714824588561452,0.0744292845731096,0.0776622687659398,
0.0817097633423463,0.0826589280639838),.UNSPECIFIED.);
#24166=B_SPLINE_CURVE_WITH_KNOTS('',3,(#150363,#150364,#150365,#150366,
#150367,#150368),.UNSPECIFIED.,.F.,.F.,(4,2,4),(1.49996604606541,1.51351365754495,
1.5768625898475),.UNSPECIFIED.);
#24167=B_SPLINE_CURVE_WITH_KNOTS('',3,(#150370,#150371,#150372,#150373,
#150374,#150375),.UNSPECIFIED.,.F.,.F.,(4,2,4),(1.339578567325,1.40292749961837,
1.41647511112636),.UNSPECIFIED.);
#24168=B_SPLINE_CURVE_WITH_KNOTS('',3,(#150377,#150378,#150379,#150380,
#150381,#150382,#150383,#150384,#150385,#150386,#150387,#150388,#150389,
#150390,#150391,#150392,#150393,#150394,#150395),.UNSPECIFIED.,.F.,.F.,
(4,2,2,2,3,2,2,2,4),(0.0600992581805974,0.0615656152925331,0.0659612937574204,
0.068797044661994,0.0714824588462428,0.0744292845638862,0.0776622687576387,
0.0817097633349189,0.0826589280661421),.UNSPECIFIED.);
#24169=B_SPLINE_CURVE_WITH_KNOTS('',3,(#150396,#150397,#150398,#150399,
#150400,#150401),.UNSPECIFIED.,.F.,.F.,(4,2,4),(1.49996604604551,1.51351365755335,
1.57686258982728),.UNSPECIFIED.);
#24170=B_SPLINE_CURVE_WITH_KNOTS('',3,(#150403,#150404,#150405,#150406,
#150407,#150408),.UNSPECIFIED.,.F.,.F.,(4,2,4),(1.33957856756908,1.40292749985976,
1.41647511133802),.UNSPECIFIED.);
#24171=B_SPLINE_CURVE_WITH_KNOTS('',3,(#150410,#150411,#150412,#150413,
#150414,#150415,#150416,#150417,#150418,#150419,#150420,#150421,#150422,
#150423,#150424,#150425,#150426,#150427,#150428),.UNSPECIFIED.,.F.,.F.,
(4,2,2,2,3,2,2,2,4),(0.0600992581791887,0.061565615297314,0.0659612937603919,
0.0687970446645219,0.071482458848452,0.0744292845657981,0.0776622687602112,
0.0817097633392904,0.0826589280661775),.UNSPECIFIED.);
#24172=B_SPLINE_CURVE_WITH_KNOTS('',3,(#150429,#150430,#150431,#150432,
#150433,#150434),.UNSPECIFIED.,.F.,.F.,(4,2,4),(1.4999660459877,1.51351365748924,
1.57686258975018),.UNSPECIFIED.);
#24173=B_SPLINE_CURVE_WITH_KNOTS('',3,(#150436,#150437,#150438,#150439,
#150440,#150441),.UNSPECIFIED.,.F.,.F.,(4,2,4),(1.33957856709288,1.40292749934161,
1.41647511088272),.UNSPECIFIED.);
#24174=B_SPLINE_CURVE_WITH_KNOTS('',3,(#150443,#150444,#150445,#150446,
#150447,#150448,#150449,#150450,#150451,#150452,#150453,#150454,#150455,
#150456,#150457,#150458,#150459,#150460,#150461),.UNSPECIFIED.,.F.,.F.,
(4,2,2,2,3,2,2,2,4),(0.0600992582807806,0.0615656153031256,0.0659612937734699,
0.0687970446812232,0.0714824588678127,0.0744292845840066,0.0776622687751647,
0.081709763349313,0.0826589280274163),.UNSPECIFIED.);
#24175=B_SPLINE_CURVE_WITH_KNOTS('',3,(#150462,#150463,#150464,#150465,
#150466,#150467),.UNSPECIFIED.,.F.,.F.,(4,2,4),(1.4999660461432,1.51351365759822,
1.57686258991855),.UNSPECIFIED.);
#24176=B_SPLINE_CURVE_WITH_KNOTS('',3,(#150469,#150470,#150471,#150472,
#150473,#150474),.UNSPECIFIED.,.F.,.F.,(4,2,4),(1.33957856765486,1.40292749999358,
1.41647511145339),.UNSPECIFIED.);
#24177=B_SPLINE_CURVE_WITH_KNOTS('',3,(#150476,#150477,#150478,#150479,
#150480,#150481,#150482,#150483,#150484,#150485,#150486,#150487,#150488,
#150489,#150490,#150491,#150492,#150493,#150494),.UNSPECIFIED.,.F.,.F.,
(4,2,2,2,3,2,2,2,4),(0.0600992582266854,0.0615656153023148,0.0659612937643017,
0.0687970446683665,0.0714824588522693,0.074429284569195,0.0776622687639236,
0.0817097633443078,0.0826589280394227),.UNSPECIFIED.);
#24178=B_SPLINE_CURVE_WITH_KNOTS('',3,(#150495,#150496,#150497,#150498,
#150499,#150500),.UNSPECIFIED.,.F.,.F.,(4,2,4),(1.49996604590169,1.51351365744857,
1.57686258967832),.UNSPECIFIED.);
#24179=B_SPLINE_CURVE_WITH_KNOTS('',3,(#150502,#150503,#150504,#150505,
#150506,#150507),.UNSPECIFIED.,.F.,.F.,(4,2,4),(1.33957856772042,1.40292750007181,
1.41647511151978),.UNSPECIFIED.);
#24180=B_SPLINE_CURVE_WITH_KNOTS('',3,(#150509,#150510,#150511,#150512,
#150513,#150514,#150515,#150516,#150517,#150518,#150519,#150520,#150521,
#150522,#150523,#150524,#150525,#150526,#150527),.UNSPECIFIED.,.F.,.F.,
(4,2,2,2,3,2,2,2,4),(0.0600992581728462,0.0615656152980507,0.0659612937585695,
0.068797044661703,0.0714824588449131,0.0744292845623147,0.0776622687577505,
0.0817097633388566,0.0826589280376275),.UNSPECIFIED.);
#24181=B_SPLINE_CURVE_WITH_KNOTS('',3,(#150528,#150529,#150530,#150531,
#150532,#150533),.UNSPECIFIED.,.F.,.F.,(4,2,4),(1.4999660458686,1.5135136573944,
1.576862589611),.UNSPECIFIED.);
#24182=B_SPLINE_CURVE_WITH_KNOTS('',3,(#150535,#150536,#150537,#150538,
#150539,#150540),.UNSPECIFIED.,.F.,.F.,(4,2,4),(1.33957856717928,1.4029274994472,
1.416475110961),.UNSPECIFIED.);
#24183=B_SPLINE_CURVE_WITH_KNOTS('',3,(#150542,#150543,#150544,#150545,
#150546,#150547,#150548,#150549,#150550,#150551,#150552,#150553,#150554,
#150555,#150556,#150557,#150558,#150559,#150560),.UNSPECIFIED.,.F.,.F.,
(4,2,2,2,3,2,2,2,4),(0.0600992582615478,0.061565615298571,0.0659612937676607,
0.0687970446745707,0.0714824588605384,0.0744292845772193,0.0776622687689834,
0.081709763343638,0.082658928152003),.UNSPECIFIED.);
#24184=B_SPLINE_CURVE_WITH_KNOTS('',3,(#150561,#150562,#150563,#150564,
#150565,#150566),.UNSPECIFIED.,.F.,.F.,(4,2,4),(1.49996604619025,1.51351365761973,
1.57686258985598),.UNSPECIFIED.);
#24185=B_SPLINE_CURVE_WITH_KNOTS('',3,(#150568,#150569,#150570,#150571,
#150572,#150573),.UNSPECIFIED.,.F.,.F.,(4,2,4),(1.33957856748694,1.40292749977602,
1.41647511126263),.UNSPECIFIED.);
#24186=B_SPLINE_CURVE_WITH_KNOTS('',3,(#150575,#150576,#150577,#150578,
#150579,#150580,#150581,#150582,#150583,#150584,#150585,#150586,#150587,
#150588,#150589,#150590,#150591,#150592,#150593),.UNSPECIFIED.,.F.,.F.,
(4,2,2,2,3,2,2,2,4),(0.0600992581602822,0.0615656152932241,0.0659612937568336,
0.0687970446610076,0.0714824588449648,0.0744292845625697,0.0776622687567982,
0.0817097633351034,0.0826589280710592),.UNSPECIFIED.);
#24187=B_SPLINE_CURVE_WITH_KNOTS('',3,(#150594,#150595,#150596,#150597,
#150598,#150599),.UNSPECIFIED.,.F.,.F.,(4,2,4),(1.49996604600395,1.51351365751376,
1.57686258978941),.UNSPECIFIED.);
#24188=B_SPLINE_CURVE_WITH_KNOTS('',3,(#150601,#150602,#150603,#150604,
#150605,#150606),.UNSPECIFIED.,.F.,.F.,(4,2,4),(1.33957856740119,1.40292749970377,
1.41647511119406),.UNSPECIFIED.);
#24189=B_SPLINE_CURVE_WITH_KNOTS('',3,(#150608,#150609,#150610,#150611,
#150612,#150613,#150614,#150615,#150616,#150617,#150618,#150619,#150620,
#150621,#150622,#150623,#150624,#150625,#150626),.UNSPECIFIED.,.F.,.F.,
(4,2,2,2,3,2,2,2,4),(0.060099258212016,0.0615656152975696,0.065961293762618,
0.0687970446677243,0.0714824588523708,0.0744292845694441,0.077662268762938,
0.0817097633405424,0.0826589280599493),.UNSPECIFIED.);
#24190=B_SPLINE_CURVE_WITH_KNOTS('',3,(#150627,#150628,#150629,#150630,
#150631,#150632),.UNSPECIFIED.,.F.,.F.,(4,2,4),(1.49996604599116,1.51351365749285,
1.57686258976734),.UNSPECIFIED.);
#24191=B_SPLINE_CURVE_WITH_KNOTS('',3,(#150634,#150635,#150636,#150637,
#150638,#150639),.UNSPECIFIED.,.F.,.F.,(4,2,4),(1.33957856732668,1.4029274996563,
1.41647511113565),.UNSPECIFIED.);
#24192=B_SPLINE_CURVE_WITH_KNOTS('',3,(#150641,#150642,#150643,#150644,
#150645,#150646,#150647,#150648,#150649,#150650,#150651,#150652,#150653,
#150654,#150655,#150656,#150657,#150658,#150659),.UNSPECIFIED.,.F.,.F.,
(4,2,2,2,3,2,2,2,4),(0.0600992582419533,0.0615656153042786,0.0659612937703273,
0.0687970446762605,0.0714824588615259,0.0744292845780137,0.0776622687709749,
0.0817097633483941,0.0826589280099401),.UNSPECIFIED.);
#24193=B_SPLINE_CURVE_WITH_KNOTS('',3,(#150660,#150661,#150662,#150663,
#150664,#150665),.UNSPECIFIED.,.F.,.F.,(4,2,4),(1.49996604605517,1.51351365754508,
1.57686258984243),.UNSPECIFIED.);
#24194=B_SPLINE_CURVE_WITH_KNOTS('',3,(#150667,#150668,#150669,#150670,
#150671,#150672),.UNSPECIFIED.,.F.,.F.,(4,2,4),(1.33957856704589,1.4029274993359,
1.41647511085871),.UNSPECIFIED.);
#24195=B_SPLINE_CURVE_WITH_KNOTS('',3,(#150674,#150675,#150676,#150677,
#150678,#150679,#150680,#150681,#150682,#150683,#150684,#150685,#150686,
#150687,#150688,#150689,#150690,#150691,#150692),.UNSPECIFIED.,.F.,.F.,
(4,2,2,2,3,2,2,2,4),(0.060099258257199,0.0615656153000239,0.0659612937700476,
0.0687970446774007,0.0714824588636833,0.0744292845802365,0.0776622687716015,
0.0817097633456108,0.0826589280505602),.UNSPECIFIED.);
#24196=B_SPLINE_CURVE_WITH_KNOTS('',3,(#150693,#150694,#150695,#150696,
#150697,#150698),.UNSPECIFIED.,.F.,.F.,(4,2,4),(1.49996604621862,1.51351365765759,
1.57686259000692),.UNSPECIFIED.);
#24197=B_SPLINE_CURVE_WITH_KNOTS('',3,(#150700,#150701,#150702,#150703,
#150704,#150705),.UNSPECIFIED.,.F.,.F.,(4,2,4),(1.3395785672913,1.40292749959559,
1.41647511108348),.UNSPECIFIED.);
#24198=B_SPLINE_CURVE_WITH_KNOTS('',3,(#150707,#150708,#150709,#150710,
#150711,#150712,#150713,#150714,#150715,#150716,#150717,#150718,#150719,
#150720,#150721,#150722,#150723,#150724,#150725),.UNSPECIFIED.,.F.,.F.,
(4,2,2,2,3,2,2,2,4),(0.0600992582270211,0.0615656152977835,0.0659612937639702,
0.0687970446695299,0.0714824588545066,0.074429284571517,0.0776622687645759,
0.0817097633413757,0.0826589280368495),.UNSPECIFIED.);
#24199=B_SPLINE_CURVE_WITH_KNOTS('',3,(#150726,#150727,#150728,#150729,
#150730,#150731),.UNSPECIFIED.,.F.,.F.,(4,2,4),(1.49996604605924,1.51351365751903,
1.57686258982276),.UNSPECIFIED.);
#24200=B_SPLINE_CURVE_WITH_KNOTS('',3,(#150733,#150734,#150735,#150736,
#150737,#150738),.UNSPECIFIED.,.F.,.F.,(4,2,4),(1.33957856731211,1.40292749955525,
1.4164751110542),.UNSPECIFIED.);
#24201=B_SPLINE_CURVE_WITH_KNOTS('',3,(#150740,#150741,#150742,#150743,
#150744,#150745,#150746,#150747,#150748,#150749,#150750,#150751,#150752,
#150753,#150754,#150755,#150756,#150757,#150758),.UNSPECIFIED.,.F.,.F.,
(4,2,2,2,3,2,2,2,4),(0.060099258176978,0.0615656152948672,0.0659612937615021,
0.0687970446670143,0.0714824588519459,0.074429284569227,0.0776622687621662,
0.0817097633383036,0.0826589280868534),.UNSPECIFIED.);
#24202=B_SPLINE_CURVE_WITH_KNOTS('',3,(#150759,#150760,#150761,#150762,
#150763,#150764),.UNSPECIFIED.,.F.,.F.,(4,2,4),(1.49996604610752,1.51351365759858,
1.57686258989254),.UNSPECIFIED.);
#24203=B_SPLINE_CURVE_WITH_KNOTS('',3,(#150766,#150767,#150768,#150769,
#150770,#150771),.UNSPECIFIED.,.F.,.F.,(4,2,4),(1.33957856760233,1.4029274999419,
1.41647511136569),.UNSPECIFIED.);
#24204=B_SPLINE_CURVE_WITH_KNOTS('',3,(#150773,#150774,#150775,#150776,
#150777,#150778,#150779,#150780,#150781,#150782,#150783,#150784,#150785,
#150786,#150787,#150788,#150789,#150790,#150791),.UNSPECIFIED.,.F.,.F.,
(4,2,2,2,3,2,2,2,4),(0.0600992582006083,0.0615656152993787,0.0659612937621229,
0.0687970446662533,0.0714824588501957,0.074429284567377,0.077662268761885,
0.0817097633414269,0.0826589280679091),.UNSPECIFIED.);
#24205=B_SPLINE_CURVE_WITH_KNOTS('',3,(#150792,#150793,#150794,#150795,
#150796,#150797),.UNSPECIFIED.,.F.,.F.,(4,2,4),(1.49996604589159,1.51351365742793,
1.5768625896485),.UNSPECIFIED.);
#24206=B_SPLINE_CURVE_WITH_KNOTS('',3,(#150799,#150800,#150801,#150802,
#150803,#150804),.UNSPECIFIED.,.F.,.F.,(4,2,4),(1.33957856743351,1.40292749973926,
1.41647511120219),.UNSPECIFIED.);
#24207=B_SPLINE_CURVE_WITH_KNOTS('',3,(#150806,#150807,#150808,#150809,
#150810,#150811,#150812,#150813,#150814,#150815,#150816,#150817,#150818,
#150819,#150820,#150821,#150822,#150823,#150824),.UNSPECIFIED.,.F.,.F.,
(4,2,2,2,3,2,2,2,4),(0.060099258224181,0.0615656153018815,0.0659612937669439,
0.0687970446723313,0.071482458857192,0.0744292845739036,0.0776622687673117,
0.0817097633452999,0.0826589280405905),.UNSPECIFIED.);
#24208=B_SPLINE_CURVE_WITH_KNOTS('',3,(#150825,#150826,#150827,#150828,
#150829,#150830),.UNSPECIFIED.,.F.,.F.,(4,2,4),(1.4999660459941,1.51351365749675,
1.57686258976619),.UNSPECIFIED.);
#24209=B_SPLINE_CURVE_WITH_KNOTS('',3,(#150832,#150833,#150834,#150835,
#150836,#150837),.UNSPECIFIED.,.F.,.F.,(4,2,4),(1.33957856743393,1.40292749973875,
1.41647511122195),.UNSPECIFIED.);
#24210=B_SPLINE_CURVE_WITH_KNOTS('',3,(#150839,#150840,#150841,#150842,
#150843,#150844,#150845,#150846,#150847,#150848,#150849,#150850,#150851,
#150852,#150853,#150854,#150855,#150856,#150857),.UNSPECIFIED.,.F.,.F.,
(4,2,2,2,3,2,2,2,4),(0.0600992582578962,0.0615656153040005,0.0659612937693774,
0.0687970446751162,0.0714824588602392,0.0744292845766818,0.0776622687698639,
0.0817097633478017,0.0826589280085131),.UNSPECIFIED.);
#24211=B_SPLINE_CURVE_WITH_KNOTS('',3,(#150858,#150859,#150860,#150861,
#150862,#150863),.UNSPECIFIED.,.F.,.F.,(4,2,4),(1.49996604599272,1.51351365750804,
1.5768625897927),.UNSPECIFIED.);
#24212=B_SPLINE_CURVE_WITH_KNOTS('',3,(#150865,#150866,#150867,#150868,
#150869,#150870),.UNSPECIFIED.,.F.,.F.,(4,2,4),(1.33957856741527,1.40292749969865,
1.41647511118214),.UNSPECIFIED.);
#24213=B_SPLINE_CURVE_WITH_KNOTS('',3,(#150872,#150873,#150874,#150875,
#150876,#150877,#150878,#150879,#150880,#150881,#150882,#150883,#150884,
#150885,#150886,#150887,#150888,#150889,#150890),.UNSPECIFIED.,.F.,.F.,
(4,2,2,2,3,2,2,2,4),(-0.0111764691682505,-0.0102273044870354,-0.00617980990966401,
-0.00294682571662145,0.,0.00268541418514354,0.005521165090919,0.00991684355683096,
0.0113832006132941),.UNSPECIFIED.);
#24214=B_SPLINE_CURVE_WITH_KNOTS('',3,(#150891,#150892,#150893,#150894,
#150895,#150896),.UNSPECIFIED.,.F.,.F.,(4,2,4),(1.49996604605074,1.51351365753382,
1.57686258981781),.UNSPECIFIED.);
#24215=B_SPLINE_CURVE_WITH_KNOTS('',3,(#150898,#150899,#150900,#150901,
#150902,#150903),.UNSPECIFIED.,.F.,.F.,(4,2,4),(1.33957856730954,1.40292749963475,
1.41647511111458),.UNSPECIFIED.);
#24216=B_SPLINE_CURVE_WITH_KNOTS('',3,(#150905,#150906,#150907,#150908,
#150909,#150910,#150911,#150912,#150913,#150914,#150915,#150916,#150917,
#150918,#150919,#150920,#150921,#150922,#150923),.UNSPECIFIED.,.F.,.F.,
(4,2,2,2,3,2,2,2,4),(0.0600992582697307,0.061565615304837,0.065961293771895,
0.0687970446782751,0.0714824588638683,0.0744292845802308,0.0776622687727685,
0.0817097633495057,0.0826589280210248),.UNSPECIFIED.);
#24217=B_SPLINE_CURVE_WITH_KNOTS('',3,(#150924,#150925,#150926,#150927,
#150928,#150929),.UNSPECIFIED.,.F.,.F.,(4,2,4),(1.499966046113,1.51351365756774,
1.57686258990272),.UNSPECIFIED.);
#24218=B_SPLINE_CURVE_WITH_KNOTS('',3,(#150931,#150932,#150933,#150934,
#150935,#150936),.UNSPECIFIED.,.F.,.F.,(4,2,4),(1.33957856732956,1.40292749963323,
1.41647511110724),.UNSPECIFIED.);
#24219=B_SPLINE_CURVE_WITH_KNOTS('',3,(#150938,#150939,#150940,#150941,
#150942,#150943,#150944,#150945,#150946,#150947,#150948,#150949,#150950,
#150951,#150952,#150953,#150954,#150955,#150956),.UNSPECIFIED.,.F.,.F.,
(4,2,2,2,3,2,2,2,4),(0.0600992582313051,0.06156561530149,0.0659612937681241,
0.0687970446741513,0.0714824588594794,0.0744292845761104,0.0776622687688761,
0.0817097633456649,0.0826589280244371),.UNSPECIFIED.);
#24220=B_SPLINE_CURVE_WITH_KNOTS('',3,(#150957,#150958,#150959,#150960,
#150961,#150962),.UNSPECIFIED.,.F.,.F.,(4,2,4),(1.49996604607698,1.51351365757267,
1.57686258986461),.UNSPECIFIED.);
#24221=B_SPLINE_CURVE_WITH_KNOTS('',3,(#150964,#150965,#150966,#150967,
#150968,#150969),.UNSPECIFIED.,.F.,.F.,(4,2,4),(1.33957856716701,1.40292749942639,
1.41647511094955),.UNSPECIFIED.);
#24222=B_SPLINE_CURVE_WITH_KNOTS('',3,(#150971,#150972,#150973,#150974,
#150975,#150976,#150977,#150978,#150979,#150980,#150981,#150982,#150983,
#150984,#150985,#150986,#150987,#150988,#150989),.UNSPECIFIED.,.F.,.F.,
(4,2,2,2,3,2,2,2,4),(0.0600992582098331,0.0615656152973585,0.0659612937652959,
0.0687970446716145,0.0714824588571425,0.0744292845740375,0.0776622687663252,
0.081709763341718,0.0826589280631378),.UNSPECIFIED.);
#24223=B_SPLINE_CURVE_WITH_KNOTS('',3,(#150990,#150991,#150992,#150993,
#150994,#150995),.UNSPECIFIED.,.F.,.F.,(4,2,4),(1.49996604614834,1.51351365759482,
1.5768625899084),.UNSPECIFIED.);
#24224=B_SPLINE_CURVE_WITH_KNOTS('',3,(#150997,#150998,#150999,#151000,
#151001,#151002),.UNSPECIFIED.,.F.,.F.,(4,2,4),(1.33957856752927,1.40292749981418,
1.41647511131301),.UNSPECIFIED.);
#24225=B_SPLINE_CURVE_WITH_KNOTS('',3,(#151004,#151005,#151006,#151007,
#151008,#151009,#151010,#151011,#151012,#151013,#151014,#151015,#151016,
#151017,#151018,#151019,#151020,#151021,#151022),.UNSPECIFIED.,.F.,.F.,
(4,2,2,2,3,2,2,2,4),(0.0600992581691034,0.0615656152957655,0.0659612937588952,
0.0687970446629439,0.0714824588468164,0.0744292845642891,0.0776622687587119,
0.0817097633376232,0.08265892807845),.UNSPECIFIED.);
#24226=B_SPLINE_CURVE_WITH_KNOTS('',3,(#151023,#151024,#151025,#151026,
#151027,#151028),.UNSPECIFIED.,.F.,.F.,(4,2,4),(1.49996604595889,1.51351365749176,
1.57686258972957),.UNSPECIFIED.);
#24227=B_SPLINE_CURVE_WITH_KNOTS('',3,(#151030,#151031,#151032,#151033,
#151034,#151035),.UNSPECIFIED.,.F.,.F.,(4,2,4),(1.33957856752258,1.40292749978992,
1.41647511126154),.UNSPECIFIED.);
#24228=B_SPLINE_CURVE_WITH_KNOTS('',3,(#151037,#151038,#151039,#151040,
#151041,#151042,#151043,#151044,#151045,#151046,#151047,#151048,#151049,
#151050,#151051,#151052,#151053,#151054,#151055),.UNSPECIFIED.,.F.,.F.,
(4,2,2,2,3,2,2,2,4),(0.0600992582008816,0.06156561529844,0.0659612937628877,
0.0687970446677415,0.0714824588522039,0.0744292845693024,0.0776622687630662,
0.0817097633411937,0.0826589280350822),.UNSPECIFIED.);
#24229=B_SPLINE_CURVE_WITH_KNOTS('',3,(#151056,#151057,#151058,#151059,
#151060,#151061),.UNSPECIFIED.,.F.,.F.,(4,2,4),(1.49996604601405,1.51351365750494,
1.57686258982047),.UNSPECIFIED.);
#24230=B_SPLINE_CURVE_WITH_KNOTS('',3,(#151063,#151064,#151065,#151066,
#151067,#151068),.UNSPECIFIED.,.F.,.F.,(4,2,4),(1.33957856772149,1.40292750006868,
1.41647511150784),.UNSPECIFIED.);
#24231=B_SPLINE_CURVE_WITH_KNOTS('',3,(#151070,#151071,#151072,#151073,
#151074,#151075,#151076,#151077,#151078,#151079,#151080,#151081,#151082,
#151083,#151084,#151085,#151086,#151087,#151088),.UNSPECIFIED.,.F.,.F.,
(4,2,2,2,3,2,2,2,4),(0.0600992582202586,0.0615656153022612,0.0659612937636604,
0.0687970446674222,0.0714824588511022,0.0744292845681201,0.0776622687631126,
0.0817097633439068,0.0826589280118024),.UNSPECIFIED.);
#24232=B_SPLINE_CURVE_WITH_KNOTS('',3,(#151089,#151090,#151091,#151092,
#151093,#151094),.UNSPECIFIED.,.F.,.F.,(4,2,4),(1.49996604587209,1.51351365743327,
1.57686258967902),.UNSPECIFIED.);
#24233=B_SPLINE_CURVE_WITH_KNOTS('',3,(#151096,#151097,#151098,#151099,
#151100,#151101),.UNSPECIFIED.,.F.,.F.,(4,2,4),(1.33957856735936,1.40292749966726,
1.41647511117744),.UNSPECIFIED.);
#24234=B_SPLINE_CURVE_WITH_KNOTS('',3,(#151103,#151104,#151105,#151106,
#151107,#151108,#151109,#151110,#151111,#151112,#151113,#151114,#151115,
#151116,#151117,#151118,#151119,#151120,#151121),.UNSPECIFIED.,.F.,.F.,
(4,2,2,2,3,2,2,2,4),(0.060099258266917,0.0615656153034342,0.0659612937695933,
0.0687970446755725,0.0714824588608685,0.0744292845773433,0.0776622687702354,
0.08170976334752,0.0826589280354621),.UNSPECIFIED.);
#24235=B_SPLINE_CURVE_WITH_KNOTS('',3,(#151122,#151123,#151124,#151125,
#151126,#151127),.UNSPECIFIED.,.F.,.F.,(4,2,4),(1.49996604600415,1.51351365750855,
1.57686258981381),.UNSPECIFIED.);
#24236=B_SPLINE_CURVE_WITH_KNOTS('',3,(#151129,#151130,#151131,#151132,
#151133,#151134),.UNSPECIFIED.,.F.,.F.,(4,2,4),(1.33957856738494,1.40292749967249,
1.41647511116503),.UNSPECIFIED.);
#24237=B_SPLINE_CURVE_WITH_KNOTS('',3,(#151136,#151137,#151138,#151139,
#151140,#151141,#151142,#151143,#151144,#151145,#151146,#151147,#151148,
#151149,#151150,#151151,#151152,#151153,#151154),.UNSPECIFIED.,.F.,.F.,
(4,2,2,2,3,2,2,2,4),(0.0600992582018194,0.0615656152977379,0.0659612937632103,
0.0687970446684834,0.0714824588532511,0.0744292845703054,0.0776622687636379,
0.0817097633409366,0.0826589280495915),.UNSPECIFIED.);
#24238=B_SPLINE_CURVE_WITH_KNOTS('',3,(#151155,#151156,#151157,#151158,
#151159,#151160),.UNSPECIFIED.,.F.,.F.,(4,2,4),(1.49996604604657,1.51351365754362,
1.57686258983577),.UNSPECIFIED.);
#24239=B_SPLINE_CURVE_WITH_KNOTS('',3,(#151162,#151163,#151164,#151165,
#151166,#151167),.UNSPECIFIED.,.F.,.F.,(4,2,4),(1.33957856727904,1.40292749957447,
1.41647511106942),.UNSPECIFIED.);
#24240=B_SPLINE_CURVE_WITH_KNOTS('',3,(#151169,#151170,#151171,#151172,
#151173,#151174,#151175,#151176,#151177,#151178,#151179,#151180,#151181,
#151182,#151183,#151184,#151185,#151186,#151187),.UNSPECIFIED.,.F.,.F.,
(4,2,2,2,3,2,2,2,4),(0.0600992581788355,0.0615656152931474,0.0659612937586987,
0.0687970446636357,0.071482458848146,0.0744292845656479,0.077662268759093,
0.0817097633359387,0.082658928090395),.UNSPECIFIED.);
#24241=B_SPLINE_CURVE_WITH_KNOTS('',3,(#151188,#151189,#151190,#151191,
#151192,#151193),.UNSPECIFIED.,.F.,.F.,(4,2,4),(1.49996604606282,1.51351365753196,
1.57686258981422),.UNSPECIFIED.);
#24242=B_SPLINE_CURVE_WITH_KNOTS('',3,(#151195,#151196,#151197,#151198,
#151199,#151200),.UNSPECIFIED.,.F.,.F.,(4,2,4),(1.33957856759874,1.40292749993747,
1.41647511140743),.UNSPECIFIED.);
#24243=B_SPLINE_CURVE_WITH_KNOTS('',3,(#151202,#151203,#151204,#151205,
#151206,#151207,#151208,#151209,#151210,#151211,#151212,#151213,#151214,
#151215,#151216,#151217,#151218,#151219,#151220),.UNSPECIFIED.,.F.,.F.,
(4,2,2,2,3,2,2,2,4),(0.0600992582012018,0.0615656153010839,0.0659612937631288,
0.0687970446670921,0.0714824588509169,0.0744292845679796,0.0776622687627298,
0.0817097633429504,0.08265892801506),.UNSPECIFIED.);
#24244=B_SPLINE_CURVE_WITH_KNOTS('',3,(#151221,#151222,#151223,#151224,
#151225,#151226),.UNSPECIFIED.,.F.,.F.,(4,2,4),(1.49996604591879,1.51351365743313,
1.57686258971772),.UNSPECIFIED.);
#24245=B_SPLINE_CURVE_WITH_KNOTS('',3,(#151228,#151229,#151230,#151231,
#151232,#151233),.UNSPECIFIED.,.F.,.F.,(4,2,4),(1.3395785670504,1.40292749929253,
1.41647511082944),.UNSPECIFIED.);
#24246=B_SPLINE_CURVE_WITH_KNOTS('',3,(#151235,#151236,#151237,#151238,
#151239,#151240,#151241,#151242,#151243,#151244,#151245,#151246,#151247,
#151248,#151249,#151250,#151251,#151252,#151253),.UNSPECIFIED.,.F.,.F.,
(4,2,2,2,3,2,2,2,4),(0.0600992582211251,0.0615656152958374,0.0659612937656703,
0.0687970446726791,0.0714824588587041,0.0744292845756083,0.0776622687671392,
0.0817097633409514,0.0826589280881341),.UNSPECIFIED.);
#24247=B_SPLINE_CURVE_WITH_KNOTS('',3,(#151254,#151255,#151256,#151257,
#151258,#151259),.UNSPECIFIED.,.F.,.F.,(4,2,4),(1.49996604617379,1.51351365761947,
1.5768625899443),.UNSPECIFIED.);
#24248=B_SPLINE_CURVE_WITH_KNOTS('',3,(#151261,#151262,#151263,#151264,
#151265,#151266),.UNSPECIFIED.,.F.,.F.,(4,2,4),(1.33957856714172,1.40292749936937,
1.41647511087422),.UNSPECIFIED.);
#24249=B_SPLINE_CURVE_WITH_KNOTS('',3,(#151268,#151269,#151270,#151271,
#151272,#151273,#151274,#151275,#151276,#151277,#151278,#151279,#151280,
#151281,#151282,#151283,#151284,#151285,#151286),.UNSPECIFIED.,.F.,.F.,
(4,2,2,2,3,2,2,2,4),(0.0600992582311416,0.0615656153003289,0.0659612937699029,
0.0687970446771266,0.0714824588633188,0.0744292845798336,0.0776622687713656,
0.0817097633457816,0.0826589280447636),.UNSPECIFIED.);
#24250=B_SPLINE_CURVE_WITH_KNOTS('',3,(#151287,#151288,#151289,#151290,
#151291,#151292),.UNSPECIFIED.,.F.,.F.,(4,2,4),(1.4999660461885,1.51351365763824,
1.57686258995467),.UNSPECIFIED.);
#24251=B_SPLINE_CURVE_WITH_KNOTS('',3,(#151294,#151295,#151296,#151297,
#151298,#151299),.UNSPECIFIED.,.F.,.F.,(4,2,4),(1.33957856767546,1.402927500014,
1.41647511143919),.UNSPECIFIED.);
#24252=B_SPLINE_CURVE_WITH_KNOTS('',3,(#151301,#151302,#151303,#151304,
#151305,#151306,#151307,#151308,#151309,#151310,#151311,#151312,#151313,
#151314,#151315,#151316,#151317,#151318,#151319),.UNSPECIFIED.,.F.,.F.,
(4,2,2,2,3,2,2,2,4),(0.0600992582047541,0.0615656153054466,0.0659612937675513,
0.0687970446718945,0.0714824588560064,0.0744292845726366,0.0776622687672277,
0.0817097633477888,0.0826589279966098),.UNSPECIFIED.);
#24253=B_SPLINE_CURVE_WITH_KNOTS('',3,(#151320,#151321,#151322,#151323,
#151324,#151325),.UNSPECIFIED.,.F.,.F.,(4,2,4),(1.49996604592437,1.51351365744584,
1.57686258971838),.UNSPECIFIED.);
#24254=B_SPLINE_CURVE_WITH_KNOTS('',3,(#151327,#151328,#151329,#151330,
#151331,#151332),.UNSPECIFIED.,.F.,.F.,(4,2,4),(1.33957856718658,1.40292749947563,
1.41647511098612),.UNSPECIFIED.);
#24255=B_SPLINE_CURVE_WITH_KNOTS('',3,(#151334,#151335,#151336,#151337,
#151338,#151339,#151340,#151341,#151342,#151343,#151344,#151345,#151346,
#151347,#151348,#151349,#151350,#151351,#151352),.UNSPECIFIED.,.F.,.F.,
(4,2,2,2,3,2,2,2,4),(0.0600992581925589,0.0615656152960413,0.0659612937631332,
0.0687970446689342,0.0714824588540824,0.0744292845712135,0.0776622687639362,
0.0817097633398639,0.0826589280802992),.UNSPECIFIED.);
#24256=B_SPLINE_CURVE_WITH_KNOTS('',3,(#151353,#151354,#151355,#151356,
#151357,#151358),.UNSPECIFIED.,.F.,.F.,(4,2,4),(1.49996604614893,1.51351365760524,
1.57686258992143),.UNSPECIFIED.);
#24257=B_SPLINE_CURVE_WITH_KNOTS('',3,(#151360,#151361,#151362,#151363,
#151364,#151365),.UNSPECIFIED.,.F.,.F.,(4,2,4),(1.33957856738739,1.40292749971882,
1.41647511118057),.UNSPECIFIED.);
#24258=B_SPLINE_CURVE_WITH_KNOTS('',3,(#151367,#151368,#151369,#151370,
#151371,#151372,#151373,#151374,#151375,#151376,#151377,#151378,#151379,
#151380,#151381,#151382,#151383,#151384,#151385),.UNSPECIFIED.,.F.,.F.,
(4,2,2,2,3,2,2,2,4),(0.0600992581815467,0.0615656152923098,0.0659612937563671,
0.0687970446605909,0.0714824588445816,0.0744292845622686,0.07766226875637,
0.0817097633342855,0.082658928067012),.UNSPECIFIED.);
#24259=B_SPLINE_CURVE_WITH_KNOTS('',3,(#151386,#151387,#151388,#151389,
#151390,#151391),.UNSPECIFIED.,.F.,.F.,(4,2,4),(1.49996604599013,1.51351365748729,
1.57686258978608),.UNSPECIFIED.);
#24260=B_SPLINE_CURVE_WITH_KNOTS('',3,(#151393,#151394,#151395,#151396,
#151397,#151398),.UNSPECIFIED.,.F.,.F.,(4,2,4),(1.33957856745805,1.40292749978122,
1.41647511124377),.UNSPECIFIED.);
#24261=B_SPLINE_CURVE_WITH_KNOTS('',3,(#151400,#151401,#151402,#151403,
#151404,#151405,#151406,#151407,#151408,#151409,#151410,#151411,#151412,
#151413,#151414,#151415,#151416,#151417,#151418),.UNSPECIFIED.,.F.,.F.,
(4,2,2,2,3,2,2,2,4),(0.060099258200665,0.0615656152991906,0.0659612937632194,
0.0687970446678825,0.0714824588522107,0.0744292845693193,0.0776622687632825,
0.0817097633418088,0.0826589280542763),.UNSPECIFIED.);
#24262=B_SPLINE_CURVE_WITH_KNOTS('',3,(#151419,#151420,#151421,#151422,
#151423,#151424),.UNSPECIFIED.,.F.,.F.,(4,2,4),(1.49996604596708,1.51351365748613,
1.57686258973189),.UNSPECIFIED.);
#24263=B_SPLINE_CURVE_WITH_KNOTS('',3,(#151426,#151427,#151428,#151429,
#151430,#151431),.UNSPECIFIED.,.F.,.F.,(4,2,4),(1.33957856720859,1.40292749944731,
1.41647511096857),.UNSPECIFIED.);
#24264=B_SPLINE_CURVE_WITH_KNOTS('',3,(#151433,#151434,#151435,#151436,
#151437,#151438,#151439,#151440,#151441,#151442,#151443,#151444,#151445,
#151446,#151447,#151448,#151449,#151450,#151451),.UNSPECIFIED.,.F.,.F.,
(4,2,2,2,3,2,2,2,4),(0.0600992582017895,0.0615656152951978,0.0659612937633217,
0.0687970446695219,0.0714824588549564,0.0744292845720686,0.0776622687643598,
0.0817097633394204,0.0826589280493914),.UNSPECIFIED.);
#24265=B_SPLINE_CURVE_WITH_KNOTS('',3,(#151452,#151453,#151454,#151455,
#151456,#151457),.UNSPECIFIED.,.F.,.F.,(4,2,4),(1.49996604614752,1.51351365761189,
1.57686258994074),.UNSPECIFIED.);
#24266=B_SPLINE_CURVE_WITH_KNOTS('',3,(#151459,#151460,#151461,#151462,
#151463,#151464),.UNSPECIFIED.,.F.,.F.,(4,2,4),(1.33957856755016,1.40292749991405,
1.41647511134939),.UNSPECIFIED.);
#24267=B_SPLINE_CURVE_WITH_KNOTS('',3,(#151466,#151467,#151468,#151469,
#151470,#151471,#151472,#151473,#151474,#151475,#151476,#151477,#151478,
#151479,#151480,#151481,#151482,#151483,#151484),.UNSPECIFIED.,.F.,.F.,
(4,2,2,2,3,2,2,2,4),(0.0600992581724155,0.0615656152970366,0.0659612937589684,
0.0687970446625868,0.0714824588461473,0.074429284563595,0.0776622687585028,
0.0817097633384532,0.0826589280551801),.UNSPECIFIED.);
#24268=B_SPLINE_CURVE_WITH_KNOTS('',3,(#151485,#151486,#151487,#151488,
#151489,#151490),.UNSPECIFIED.,.F.,.F.,(4,2,4),(1.49996604592509,1.51351365746294,
1.57686258968125),.UNSPECIFIED.);
#24269=B_SPLINE_CURVE_WITH_KNOTS('',3,(#151492,#151493,#151494,#151495,
#151496,#151497),.UNSPECIFIED.,.F.,.F.,(4,2,4),(1.33957856728705,1.40292749954936,
1.41647511104988),.UNSPECIFIED.);
#24270=B_SPLINE_CURVE_WITH_KNOTS('',3,(#151499,#151500,#151501,#151502,
#151503,#151504,#151505,#151506,#151507,#151508,#151509,#151510,#151511,
#151512,#151513,#151514,#151515,#151516,#151517),.UNSPECIFIED.,.F.,.F.,
(4,2,2,2,3,2,2,2,4),(0.0600992581982055,0.0615656152983017,0.0659612937650131,
0.0687970446708029,0.0714824588559478,0.0744292845729105,0.0776622687657356,
0.0817097633421375,0.0826589280637736),.UNSPECIFIED.);
#24271=B_SPLINE_CURVE_WITH_KNOTS('',3,(#151518,#151519,#151520,#151521,
#151522,#151523),.UNSPECIFIED.,.F.,.F.,(4,2,4),(1.49996604606541,1.51351365754495,
1.5768625898475),.UNSPECIFIED.);
#24272=B_SPLINE_CURVE_WITH_KNOTS('',3,(#151525,#151526,#151527,#151528,
#151529,#151530),.UNSPECIFIED.,.F.,.F.,(4,2,4),(1.339578567325,1.40292749961837,
1.41647511112636),.UNSPECIFIED.);
#24273=B_SPLINE_CURVE_WITH_KNOTS('',3,(#151532,#151533,#151534,#151535,
#151536,#151537,#151538,#151539,#151540,#151541,#151542,#151543,#151544,
#151545,#151546,#151547,#151548,#151549,#151550),.UNSPECIFIED.,.F.,.F.,
(4,2,2,2,3,2,2,2,4),(0.0600992581809373,0.0615656152928883,0.0659612937578001,
0.0687970446623745,0.0714824588466231,0.074429284564271,0.0776622687580358,
0.0817097633353215,0.0826589280665468),.UNSPECIFIED.);
#24274=B_SPLINE_CURVE_WITH_KNOTS('',3,(#151551,#151552,#151553,#151554,
#151555,#151556),.UNSPECIFIED.,.F.,.F.,(4,2,4),(1.49996604604552,1.51351365755335,
1.57686258982728),.UNSPECIFIED.);
#24275=B_SPLINE_CURVE_WITH_KNOTS('',3,(#151558,#151559,#151560,#151561,
#151562,#151563),.UNSPECIFIED.,.F.,.F.,(4,2,4),(1.33957856756908,1.40292749985976,
1.41647511133802),.UNSPECIFIED.);
#24276=B_SPLINE_CURVE_WITH_KNOTS('',3,(#151565,#151566,#151567,#151568,
#151569,#151570,#151571,#151572,#151573,#151574,#151575,#151576,#151577,
#151578,#151579,#151580,#151581,#151582,#151583),.UNSPECIFIED.,.F.,.F.,
(4,2,2,2,3,2,2,2,4),(0.0600992581792367,0.061565615297372,0.0659612937604539,
0.0687970446645766,0.0714824588485057,0.0744292845658528,0.0776622687602686,
0.0817097633393586,0.0826589280662485),.UNSPECIFIED.);
#24277=B_SPLINE_CURVE_WITH_KNOTS('',3,(#151584,#151585,#151586,#151587,
#151588,#151589),.UNSPECIFIED.,.F.,.F.,(4,2,4),(1.4999660459877,1.51351365748924,
1.57686258975018),.UNSPECIFIED.);
#24278=B_SPLINE_CURVE_WITH_KNOTS('',3,(#151591,#151592,#151593,#151594,
#151595,#151596),.UNSPECIFIED.,.F.,.F.,(4,2,4),(1.33957856709288,1.40292749934161,
1.41647511088272),.UNSPECIFIED.);
#24279=B_SPLINE_CURVE_WITH_KNOTS('',3,(#151598,#151599,#151600,#151601,
#151602,#151603,#151604,#151605,#151606,#151607,#151608,#151609,#151610,
#151611,#151612,#151613,#151614,#151615,#151616),.UNSPECIFIED.,.F.,.F.,
(4,2,2,2,3,2,2,2,4),(0.0600992582805735,0.0615656153028816,0.065961293773175,
0.0687970446809335,0.0714824588675231,0.07442928458371,0.0776622687748456,
0.0817097633489511,0.0826589280270409),.UNSPECIFIED.);
#24280=B_SPLINE_CURVE_WITH_KNOTS('',3,(#151617,#151618,#151619,#151620,
#151621,#151622),.UNSPECIFIED.,.F.,.F.,(4,2,4),(1.4999660461432,1.51351365759822,
1.57686258991855),.UNSPECIFIED.);
#24281=B_SPLINE_CURVE_WITH_KNOTS('',3,(#151624,#151625,#151626,#151627,
#151628,#151629),.UNSPECIFIED.,.F.,.F.,(4,2,4),(1.33957856765486,1.40292749999358,
1.41647511145339),.UNSPECIFIED.);
#24282=B_SPLINE_CURVE_WITH_KNOTS('',3,(#151631,#151632,#151633,#151634,
#151635,#151636,#151637,#151638,#151639,#151640,#151641,#151642,#151643,
#151644,#151645,#151646,#151647,#151648,#151649),.UNSPECIFIED.,.F.,.F.,
(4,2,2,2,3,2,2,2,4),(0.0600992582262742,0.0615656153018907,0.0659612937638662,
0.0687970446679375,0.0714824588518414,0.0744292845687624,0.0776622687634731,
0.0817097633438245,0.0826589280389295),.UNSPECIFIED.);
#24283=B_SPLINE_CURVE_WITH_KNOTS('',3,(#151650,#151651,#151652,#151653,
#151654,#151655),.UNSPECIFIED.,.F.,.F.,(4,2,4),(1.49996604590169,1.51351365744857,
1.57686258967832),.UNSPECIFIED.);
#24284=B_SPLINE_CURVE_WITH_KNOTS('',3,(#151657,#151658,#151659,#151660,
#151661,#151662),.UNSPECIFIED.,.F.,.F.,(4,2,4),(1.33957856772042,1.40292750007181,
1.41647511151978),.UNSPECIFIED.);
#24285=B_SPLINE_CURVE_WITH_KNOTS('',3,(#151664,#151665,#151666,#151667,
#151668,#151669,#151670,#151671,#151672,#151673,#151674,#151675,#151676,
#151677,#151678,#151679,#151680,#151681,#151682),.UNSPECIFIED.,.F.,.F.,
(4,2,2,2,3,2,2,2,4),(0.0600992581730512,0.0615656152982502,0.0659612937587487,
0.0687970446618746,0.0714824588450843,0.0744292845624935,0.0776622687579553,
0.0817097633391145,0.0826589280378999),.UNSPECIFIED.);
#24286=B_SPLINE_CURVE_WITH_KNOTS('',3,(#151683,#151684,#151685,#151686,
#151687,#151688),.UNSPECIFIED.,.F.,.F.,(4,2,4),(1.4999660458686,1.5135136573944,
1.576862589611),.UNSPECIFIED.);
#24287=B_SPLINE_CURVE_WITH_KNOTS('',3,(#151690,#151691,#151692,#151693,
#151694,#151695),.UNSPECIFIED.,.F.,.F.,(4,2,4),(1.33957856717928,1.4029274994472,
1.416475110961),.UNSPECIFIED.);
#24288=B_SPLINE_CURVE_WITH_KNOTS('',3,(#151697,#151698,#151699,#151700,
#151701,#151702,#151703,#151704,#151705,#151706,#151707,#151708,#151709,
#151710,#151711,#151712,#151713,#151714,#151715),.UNSPECIFIED.,.F.,.F.,
(4,2,2,2,3,2,2,2,4),(0.0600992582613176,0.0615656152983437,0.0659612937674522,
0.0687970446743743,0.0714824588603425,0.0744292845770165,0.0776622687687574,
0.0817097633433523,0.082658928151699),.UNSPECIFIED.);
#24289=B_SPLINE_CURVE_WITH_KNOTS('',3,(#151716,#151717,#151718,#151719,
#151720,#151721),.UNSPECIFIED.,.F.,.F.,(4,2,4),(1.49996604619025,1.51351365761973,
1.57686258985598),.UNSPECIFIED.);
#24290=B_SPLINE_CURVE_WITH_KNOTS('',3,(#151723,#151724,#151725,#151726,
#151727,#151728),.UNSPECIFIED.,.F.,.F.,(4,2,4),(1.33957856748694,1.40292749977602,
1.41647511126263),.UNSPECIFIED.);
#24291=B_SPLINE_CURVE_WITH_KNOTS('',3,(#151730,#151731,#151732,#151733,
#151734,#151735,#151736,#151737,#151738,#151739,#151740,#151741,#151742,
#151743,#151744,#151745,#151746,#151747,#151748),.UNSPECIFIED.,.F.,.F.,
(4,2,2,2,3,2,2,2,4),(0.0600992581608641,0.0615656152938688,0.0659612937575722,
0.0687970446617445,0.0714824588456999,0.0744292845632993,0.0776622687575126,
0.0817097633357957,0.0826589280717446),.UNSPECIFIED.);
#24292=B_SPLINE_CURVE_WITH_KNOTS('',3,(#151749,#151750,#151751,#151752,
#151753,#151754),.UNSPECIFIED.,.F.,.F.,(4,2,4),(1.49996604600395,1.51351365751376,
1.57686258978941),.UNSPECIFIED.);
#24293=B_SPLINE_CURVE_WITH_KNOTS('',3,(#151756,#151757,#151758,#151759,
#151760,#151761),.UNSPECIFIED.,.F.,.F.,(4,2,4),(1.33957856740119,1.40292749970377,
1.41647511119406),.UNSPECIFIED.);
#24294=B_SPLINE_CURVE_WITH_KNOTS('',3,(#151763,#151764,#151765,#151766,
#151767,#151768,#151769,#151770,#151771,#151772,#151773,#151774,#151775,
#151776,#151777,#151778,#151779,#151780,#151781),.UNSPECIFIED.,.F.,.F.,
(4,2,2,2,3,2,2,2,4),(0.0600992582120315,0.0615656152975978,0.0659612937626651,
0.0687970446677665,0.071482458852412,0.0744292845694908,0.077662268763002,
0.0817097633406405,0.0826589280600578),.UNSPECIFIED.);
#24295=B_SPLINE_CURVE_WITH_KNOTS('',3,(#151782,#151783,#151784,#151785,
#151786,#151787),.UNSPECIFIED.,.F.,.F.,(4,2,4),(1.49996604599116,1.51351365749285,
1.57686258976734),.UNSPECIFIED.);
#24296=B_SPLINE_CURVE_WITH_KNOTS('',3,(#151789,#151790,#151791,#151792,
#151793,#151794),.UNSPECIFIED.,.F.,.F.,(4,2,4),(1.33957856732664,1.40292749965626,
1.4164751111356),.UNSPECIFIED.);
#24297=B_SPLINE_CURVE_WITH_KNOTS('',3,(#151796,#151797,#151798,#151799,
#151800,#151801,#151802,#151803,#151804,#151805,#151806,#151807,#151808,
#151809,#151810,#151811,#151812,#151813,#151814),.UNSPECIFIED.,.F.,.F.,
(4,2,2,2,3,2,2,2,4),(0.0600992582417298,0.0615656153040711,0.0659612937701545,
0.0687970446760882,0.0714824588613524,0.0744292845778339,0.0776622687707767,
0.0817097633481624,0.0826589280096967),.UNSPECIFIED.);
#24298=B_SPLINE_CURVE_WITH_KNOTS('',3,(#151815,#151816,#151817,#151818,
#151819,#151820),.UNSPECIFIED.,.F.,.F.,(4,2,4),(1.49996604605517,1.51351365754508,
1.57686258984243),.UNSPECIFIED.);
#24299=B_SPLINE_CURVE_WITH_KNOTS('',3,(#151822,#151823,#151824,#151825,
#151826,#151827),.UNSPECIFIED.,.F.,.F.,(4,2,4),(1.33957856704589,1.4029274993359,
1.41647511085871),.UNSPECIFIED.);
#24300=B_SPLINE_CURVE_WITH_KNOTS('',3,(#151829,#151830,#151831,#151832,
#151833,#151834,#151835,#151836,#151837,#151838,#151839,#151840,#151841,
#151842,#151843,#151844,#151845,#151846,#151847),.UNSPECIFIED.,.F.,.F.,
(4,2,2,2,3,2,2,2,4),(0.0600992582564895,0.0615656152993143,0.065961293769343,
0.0687970446766933,0.0714824588629754,0.07442928457953,0.0776622687708993,
0.0817097633449113,0.0826589280498623),.UNSPECIFIED.);
#24301=B_SPLINE_CURVE_WITH_KNOTS('',3,(#151848,#151849,#151850,#151851,
#151852,#151853),.UNSPECIFIED.,.F.,.F.,(4,2,4),(1.49996604621862,1.51351365765759,
1.57686259000693),.UNSPECIFIED.);
#24302=B_SPLINE_CURVE_WITH_KNOTS('',3,(#151855,#151856,#151857,#151858,
#151859,#151860),.UNSPECIFIED.,.F.,.F.,(4,2,4),(1.3395785672913,1.40292749959559,
1.41647511108348),.UNSPECIFIED.);
#24303=B_SPLINE_CURVE_WITH_KNOTS('',3,(#151862,#151863,#151864,#151865,
#151866,#151867,#151868,#151869,#151870,#151871,#151872,#151873,#151874,
#151875,#151876,#151877,#151878,#151879,#151880),.UNSPECIFIED.,.F.,.F.,
(4,2,2,2,3,2,2,2,4),(0.0600992582278879,0.0615656152986711,0.0659612937648786,
0.0687970446704373,0.0714824588554149,0.0744292845724269,0.0776622687654903,
0.0817097633423073,0.0826589280377865),.UNSPECIFIED.);
#24304=B_SPLINE_CURVE_WITH_KNOTS('',3,(#151881,#151882,#151883,#151884,
#151885,#151886),.UNSPECIFIED.,.F.,.F.,(4,2,4),(1.49996604605924,1.51351365751903,
1.57686258982277),.UNSPECIFIED.);
#24305=B_SPLINE_CURVE_WITH_KNOTS('',3,(#151888,#151889,#151890,#151891,
#151892,#151893),.UNSPECIFIED.,.F.,.F.,(4,2,4),(1.33957856731205,1.4029274995552,
1.41647511105415),.UNSPECIFIED.);
#24306=B_SPLINE_CURVE_WITH_KNOTS('',3,(#151895,#151896,#151897,#151898,
#151899,#151900,#151901,#151902,#151903,#151904,#151905,#151906,#151907,
#151908,#151909,#151910,#151911,#151912,#151913),.UNSPECIFIED.,.F.,.F.,
(4,2,2,2,3,2,2,2,4),(0.0600992581771638,0.0615656152950589,0.0659612937616956,
0.0687970446672038,0.0714824588521353,0.0744292845694206,0.0776622687623728,
0.0817097633385307,0.0826589280870864),.UNSPECIFIED.);
#24307=B_SPLINE_CURVE_WITH_KNOTS('',3,(#151914,#151915,#151916,#151917,
#151918,#151919),.UNSPECIFIED.,.F.,.F.,(4,2,4),(1.49996604610752,1.51351365759858,
1.57686258989254),.UNSPECIFIED.);
#24308=B_SPLINE_CURVE_WITH_KNOTS('',3,(#151921,#151922,#151923,#151924,
#151925,#151926),.UNSPECIFIED.,.F.,.F.,(4,2,4),(1.33957856760233,1.4029274999419,
1.41647511136569),.UNSPECIFIED.);
#24309=B_SPLINE_CURVE_WITH_KNOTS('',3,(#151928,#151929,#151930,#151931,
#151932,#151933,#151934,#151935,#151936,#151937,#151938,#151939,#151940,
#151941,#151942,#151943,#151944,#151945,#151946),.UNSPECIFIED.,.F.,.F.,
(4,2,2,2,3,2,2,2,4),(0.0600992582006101,0.0615656152993682,0.0659612937620992,
0.068797044666235,0.0714824588501786,0.0744292845673599,0.0776622687618674,
0.0817097633414001,0.0826589280678798),.UNSPECIFIED.);
#24310=B_SPLINE_CURVE_WITH_KNOTS('',3,(#151947,#151948,#151949,#151950,
#151951,#151952),.UNSPECIFIED.,.F.,.F.,(4,2,4),(1.49996604589165,1.51351365742799,
1.57686258964856),.UNSPECIFIED.);
#24311=B_SPLINE_CURVE_WITH_KNOTS('',3,(#151954,#151955,#151956,#151957,
#151958,#151959),.UNSPECIFIED.,.F.,.F.,(4,2,4),(1.33957856743351,1.40292749973926,
1.41647511120219),.UNSPECIFIED.);
#24312=B_SPLINE_CURVE_WITH_KNOTS('',3,(#151961,#151962,#151963,#151964,
#151965,#151966,#151967,#151968,#151969,#151970,#151971,#151972,#151973,
#151974,#151975,#151976,#151977,#151978,#151979),.UNSPECIFIED.,.F.,.F.,
(4,2,2,2,3,2,2,2,4),(0.060099258224775,0.0615656153025146,0.0659612937676359,
0.0687970446730238,0.0714824588578852,0.0744292845745959,0.0776622687680001,
0.0817097633459842,0.0826589280412753),.UNSPECIFIED.);
#24313=B_SPLINE_CURVE_WITH_KNOTS('',3,(#151980,#151981,#151982,#151983,
#151984,#151985),.UNSPECIFIED.,.F.,.F.,(4,2,4),(1.49996604599409,1.51351365749675,
1.57686258976619),.UNSPECIFIED.);
#24314=B_SPLINE_CURVE_WITH_KNOTS('',3,(#151987,#151988,#151989,#151990,
#151991,#151992),.UNSPECIFIED.,.F.,.F.,(4,2,4),(1.33957856743393,1.40292749973875,
1.41647511122195),.UNSPECIFIED.);
#24315=B_SPLINE_CURVE_WITH_KNOTS('',3,(#151994,#151995,#151996,#151997,
#151998,#151999,#152000,#152001,#152002,#152003,#152004,#152005,#152006,
#152007,#152008,#152009,#152010,#152011,#152012),.UNSPECIFIED.,.F.,.F.,
(4,2,2,2,3,2,2,2,4),(0.0600992582585029,0.0615656153046349,0.0659612937700477,
0.0687970446757806,0.0714824588609026,0.0744292845773481,0.0776622687705401,
0.0817097633484953,0.0826589280092112),.UNSPECIFIED.);
#24316=B_SPLINE_CURVE_WITH_KNOTS('',3,(#152013,#152014,#152015,#152016,
#152017,#152018),.UNSPECIFIED.,.F.,.F.,(4,2,4),(1.49996604599272,1.51351365750805,
1.5768625897927),.UNSPECIFIED.);
#24317=B_SPLINE_CURVE_WITH_KNOTS('',3,(#152020,#152021,#152022,#152023,
#152024,#152025),.UNSPECIFIED.,.F.,.F.,(4,2,4),(1.33957856741527,1.40292749969865,
1.41647511118214),.UNSPECIFIED.);
#24318=B_SPLINE_CURVE_WITH_KNOTS('',3,(#152026,#152027,#152028,#152029,
#152030,#152031,#152032,#152033,#152034,#152035),.UNSPECIFIED.,.F.,.F.,
(4,2,2,2,4),(0.0600992582453176,0.0615656153017531,0.0659612937676228,0.0687970446733949,
0.0714824588585375),.UNSPECIFIED.);
#24319=B_SPLINE_CURVE_WITH_KNOTS('',5,(#154494,#154495,#154496,#154497,
#154498,#154499,#154500,#154501,#154502,#154503,#154504,#154505,#154506,
#154507,#154508,#154509,#154510,#154511,#154512,#154513,#154514,#154515,
#154516,#154517,#154518,#154519,#154520,#154521,#154522,#154523,#154524,
#154525,#154526,#154527,#154528,#154529,#154530,#154531,#154532,#154533,
#154534,#154535,#154536,#154537,#154538,#154539,#154540,#154541,#154542,
#154543,#154544,#154545,#154546,#154547,#154548,#154549,#154550,#154551,
#154552,#154553,#154554,#154555,#154556,#154557,#154558,#154559,#154560,
#154561,#154562,#154563,#154564,#154565,#154566,#154567,#154568,#154569,
#154570,#154571,#154572,#154573,#154574,#154575,#154576,#154577,#154578,
#154579,#154580,#154581,#154582,#154583,#154584,#154585,#154586,#154587,
#154588,#154589,#154590,#154591,#154592,#154593,#154594,#154595,#154596,
#154597,#154598,#154599,#154600,#154601,#154602,#154603,#154604,#154605,
#154606,#154607,#154608,#154609,#154610,#154611,#154612,#154613,#154614,
#154615,#154616,#154617,#154618,#154619,#154620,#154621,#154622,#154623,
#154624,#154625,#154626,#154627,#154628,#154629,#154630,#154631,#154632,
#154633,#154634,#154635,#154636,#154637,#154638,#154639,#154640,#154641,
#154642,#154643,#154644,#154645,#154646,#154647,#154648,#154649,#154650,
#154651,#154652,#154653,#154654,#154655,#154656,#154657,#154658,#154659,
#154660,#154661,#154662,#154663,#154664,#154665,#154666,#154667,#154668,
#154669,#154670,#154671,#154672,#154673,#154674,#154675,#154676,#154677,
#154678,#154679,#154680,#154681,#154682,#154683,#154684,#154685,#154686,
#154687,#154688,#154689,#154690,#154691,#154692,#154693,#154694,#154695,
#154696,#154697,#154698,#154699,#154700,#154701,#154702,#154703,#154704,
#154705,#154706,#154707,#154708,#154709,#154710,#154711,#154712,#154713,
#154714,#154715,#154716,#154717,#154718,#154719,#154720,#154721,#154722,
#154723,#154724,#154725,#154726,#154727,#154728,#154729,#154730,#154731,
#154732,#154733,#154734,#154735,#154736,#154737,#154738,#154739,#154740,
#154741,#154742,#154743,#154744,#154745,#154746,#154747,#154748,#154749,
#154750,#154751,#154752,#154753,#154754,#154755,#154756,#154757,#154758,
#154759,#154760,#154761,#154762,#154763,#154764,#154765,#154766,#154767,
#154768,#154769,#154770,#154771,#154772,#154773,#154774,#154775,#154776,
#154777,#154778,#154779,#154780,#154781,#154782,#154783,#154784,#154785,
#154786,#154787,#154788,#154789,#154790,#154791,#154792,#154793,#154794,
#154795,#154796,#154797,#154798,#154799,#154800,#154801,#154802,#154803,
#154804,#154805,#154806,#154807,#154808,#154809,#154810,#154811,#154812,
#154813,#154814,#154815,#154816,#154817,#154818,#154819,#154820,#154821,
#154822,#154823,#154824,#154825,#154826,#154827,#154828,#154829,#154830,
#154831,#154832,#154833,#154834,#154835,#154836,#154837,#154838,#154839,
#154840,#154841,#154842,#154843,#154844,#154845,#154846,#154847,#154848,
#154849,#154850,#154851,#154852,#154853,#154854,#154855,#154856,#154857,
#154858,#154859,#154860,#154861,#154862,#154863,#154864,#154865,#154866,
#154867,#154868,#154869,#154870,#154871,#154872,#154873,#154874,#154875,
#154876,#154877,#154878,#154879,#154880,#154881,#154882,#154883,#154884,
#154885,#154886,#154887,#154888,#154889,#154890,#154891,#154892,#154893,
#154894,#154895,#154896,#154897,#154898,#154899,#154900,#154901,#154902,
#154903,#154904,#154905,#154906,#154907,#154908,#154909,#154910,#154911,
#154912,#154913,#154914,#154915,#154916,#154917,#154918,#154919,#154920,
#154921,#154922,#154923,#154924,#154925,#154926,#154927,#154928,#154929,
#154930,#154931,#154932,#154933,#154934,#154935,#154936,#154937,#154938,
#154939,#154940,#154941,#154942,#154943,#154944,#154945,#154946,#154947,
#154948,#154949,#154950,#154951,#154952,#154953,#154954,#154955,#154956,
#154957,#154958,#154959,#154960,#154961,#154962,#154963,#154964),
 .UNSPECIFIED.,.F.,.F.,(6,1,1,1,1,1,1,1,1,1,1,1,1,1,1,1,1,1,1,1,1,1,1,1,
1,1,1,1,1,1,1,1,1,1,1,1,1,1,1,1,1,1,1,1,1,1,1,1,1,1,1,1,1,1,1,1,1,1,1,1,
1,1,1,1,1,1,1,1,1,1,1,1,1,1,1,1,1,1,1,1,1,1,1,1,1,1,1,1,1,1,1,1,1,1,1,1,
1,1,1,1,1,1,1,1,1,1,1,1,1,1,1,1,1,1,1,1,1,1,1,1,1,1,1,1,1,1,1,1,1,1,1,1,
1,1,1,1,1,1,1,1,1,1,1,1,1,1,1,1,1,1,1,1,1,1,1,1,1,1,1,1,1,1,1,1,1,1,1,1,
1,1,1,1,1,1,1,1,1,1,1,1,1,1,1,1,1,1,1,1,1,1,1,1,1,1,1,1,1,1,1,1,1,1,1,1,
1,1,1,1,1,1,1,1,1,1,1,1,1,1,1,1,1,1,1,1,1,1,1,1,1,1,1,1,1,1,1,1,1,1,1,1,
1,1,1,1,1,1,1,1,1,1,1,1,1,1,1,1,1,1,1,1,1,1,1,1,1,1,1,1,1,1,1,1,1,1,1,1,
1,1,1,1,1,1,1,1,1,1,1,1,1,1,1,1,1,1,1,1,1,1,1,1,1,1,1,1,1,1,1,1,1,1,1,1,
1,1,1,1,1,1,1,1,1,1,1,1,1,1,1,1,1,1,1,1,1,1,1,1,1,1,1,1,1,1,1,1,1,1,1,1,
1,1,1,1,1,1,1,1,1,1,1,1,1,1,1,1,1,1,1,1,1,1,1,1,1,1,1,1,1,1,1,1,1,1,1,1,
1,1,1,1,1,1,1,1,1,1,1,1,1,1,1,1,1,1,1,1,1,1,1,1,1,1,1,1,1,1,1,1,1,1,1,1,
1,1,1,1,1,1,1,1,1,1,1,1,1,1,1,1,1,1,1,1,1,1,1,1,1,1,1,1,1,1,1,1,1,1,1,1,
1,1,1,1,1,1,1,1,1,1,6),(0.143172102,0.144954128,0.146788991,0.148623853,
0.150458716,0.152293578,0.15412844,0.155963303,0.157798165,0.159633028,
0.16146789,0.163302752,0.165137615,0.166972477,0.168807339,0.170642202,
0.172477064,0.174311927,0.176146789,0.177981651,0.179816514,0.181651376,
0.183486239,0.185321101,0.187155963,0.188990826,0.190825688,0.19266055,
0.194495413,0.196330275,0.198165138,0.2,0.201834862,0.203669725,0.205504587,
0.20733945,0.209174312,0.211009174,0.212844037,0.214678899,0.216513761,
0.218348624,0.220183486,0.222018349,0.223853211,0.225688073,0.227522936,
0.231192661,0.233027523,0.234862385,0.236697248,0.23853211,0.240366972,
0.242201835,0.244036697,0.24587156,0.247706422,0.249541284,0.251376147,
0.253211009,0.255045872,0.256880734,0.258715596,0.260550459,0.262385321,
0.264220183,0.266055046,0.267889908,0.269724771,0.271559633,0.273394495,
0.275229358,0.27706422,0.278899083,0.280733945,0.282568807,0.28440367,0.286238532,
0.288073394,0.289908257,0.291743119,0.293577982,0.295412844,0.297247706,
0.299082569,0.300917431,0.302752294,0.304587156,0.306422018,0.308256881,
0.310091743,0.311926606,0.313761468,0.31559633,0.317431193,0.319266055,
0.321100917,0.32293578,0.324770642,0.326605505,0.328440367,0.330275229,
0.332110092,0.333944954,0.335779817,0.337614679,0.339449541,0.341284404,
0.343119266,0.344954128,0.346788991,0.348623853,0.350458716,0.352293578,
0.35412844,0.355963303,0.357798165,0.359633028,0.36146789,0.363302752,0.365137615,
0.366972477,0.368807339,0.370642202,0.372477064,0.374311927,0.376146789,
0.377981651,0.379816514,0.381651376,0.383486239,0.385321101,0.387155963,
0.388990826,0.390825688,0.39266055,0.394495413,0.396330275,0.398165138,
0.4,0.401834862,0.403669725,0.405504587,0.40733945,0.409174312,0.411009174,
0.412844037,0.414678899,0.416513761,0.418348624,0.420183486,0.422018349,
0.423853211,0.425688073,0.427522936,0.429357798,0.431192661,0.433027523,
0.434862385,0.436697248,0.43853211,0.440366972,0.442201835,0.444036697,
0.44587156,0.447706422,0.449541284,0.451376147,0.453211009,0.455045872,
0.456880734,0.458715596,0.460550459,0.462385321,0.464220183,0.466055046,
0.467889908,0.469724771,0.471559633,0.473394495,0.475229358,0.47706422,
0.478899083,0.480733945,0.482568807,0.48440367,0.486238532,0.488073394,
0.489908257,0.491743119,0.493577982,0.495412844,0.497247706,0.499082569,
0.500917431,0.502752294,0.504587156,0.506422018,0.508256881,0.510091743,
0.511926606,0.513761468,0.51559633,0.517431193,0.519266055,0.521100917,
0.52293578,0.524770642,0.526605505,0.528440367,0.530275229,0.532110092,
0.533944954,0.535779817,0.537614679,0.539449541,0.541284404,0.543119266,
0.544954128,0.546788991,0.548623853,0.550458716,0.552293578,0.55412844,
0.555963303,0.557798165,0.559633028,0.56146789,0.563302752,0.565137615,
0.566972477,0.568807339,0.570642202,0.572477064,0.574311927,0.576146789,
0.577981651,0.579816514,0.581651376,0.583486239,0.585321101,0.587155963,
0.588990826,0.590825688,0.59266055,0.594495413,0.596330275,0.598165138,
0.6,0.601834862,0.603669725,0.605504587,0.60733945,0.609174312,0.611009174,
0.612844037,0.614678899,0.616513761,0.618348624,0.620183486,0.622018349,
0.623853211,0.625688073,0.627522936,0.629357798,0.631192661,0.633027523,
0.634862385,0.636697248,0.63853211,0.640366972,0.642201835,0.644036697,
0.64587156,0.647706422,0.649541284,0.651376147,0.653211009,0.655045872,
0.656880734,0.658715596,0.660550459,0.662385321,0.664220183,0.666055046,
0.667889908,0.669724771,0.671559633,0.673394495,0.675229358,0.67706422,
0.678899083,0.680733945,0.682568807,0.68440367,0.686238532,0.688073394,
0.689908257,0.691743119,0.693577982,0.695412844,0.697247706,0.699082569,
0.700917431,0.702752294,0.704587156,0.706422018,0.708256881,0.710091743,
0.711926606,0.713761468,0.71559633,0.717431193,0.719266055,0.721100917,
0.72293578,0.724770642,0.726605505,0.728440367,0.730275229,0.732110092,
0.733944954,0.735779817,0.737614679,0.739449541,0.741284404,0.743119266,
0.744954128,0.746788991,0.748623853,0.750458716,0.752293578,0.75412844,
0.755963303,0.757798165,0.759633028,0.76146789,0.763302752,0.765137615,
0.766972477,0.768807339,0.770642202,0.772477064,0.774311927,0.776146789,
0.777981651,0.779816514,0.781651376,0.783486239,0.785321101,0.787155963,
0.788990826,0.790825688,0.79266055,0.794495413,0.796330275,0.798165138,
0.8,0.801834862,0.803669725,0.805504587,0.80733945,0.809174312,0.811009174,
0.812844037,0.814678899,0.816513761,0.818348624,0.820183486,0.822018349,
0.823853211,0.825688073,0.827522936,0.829357798,0.831192661,0.833027523,
0.834862385,0.836697248,0.83853211,0.840366972,0.842201835,0.844036697,
0.84587156,0.847706422,0.849541284,0.851376147,0.853211009,0.855045872,
0.856880734,0.858715596,0.860550459,0.862385321,0.864220183,0.866055046,
0.867889908,0.869724771,0.871559633,0.873394495,0.875229358,0.87706422,
0.878899083,0.880733945,0.882568807,0.88440367,0.886238532,0.888073394,
0.889908257,0.891743119,0.893577982,0.895412844,0.897247706,0.899082569,
0.900917431,0.902752294,0.904587156,0.906422018,0.908256881,0.910091743,
0.911926606,0.913761468,0.91559633,0.917431193,0.919266055,0.921100917,
0.92293578,0.924770642,0.926605505,0.928440367,0.930275229,0.932110092,
0.933944954,0.935779817,0.937614679,0.939449541,0.941284404,0.943119266,
0.944954128,0.946788991,0.948623853,0.950458716,0.952293578,0.95412844,
0.955963303,0.957798165,0.959633028,0.96146789,0.963302752,0.965137615,
0.966972477,0.968807339,0.970642202,0.972477064,0.974311927,0.976146789,
0.977981651,0.979816514,0.981651376,0.983486239,0.985321101,0.987155963,
0.988990826,0.990825688,0.99266055,0.994495413,0.996330275,0.998165138,
1.),.UNSPECIFIED.);
#24320=B_SPLINE_CURVE_WITH_KNOTS('',5,(#154965,#154966,#154967,#154968,
#154969,#154970,#154971,#154972,#154973,#154974,#154975,#154976,#154977,
#154978,#154979,#154980,#154981,#154982,#154983,#154984,#154985,#154986,
#154987,#154988,#154989,#154990,#154991,#154992,#154993,#154994,#154995,
#154996,#154997,#154998,#154999,#155000,#155001,#155002,#155003,#155004,
#155005,#155006,#155007,#155008,#155009,#155010,#155011,#155012,#155013,
#155014,#155015,#155016,#155017,#155018,#155019,#155020,#155021,#155022,
#155023,#155024,#155025,#155026,#155027,#155028,#155029,#155030,#155031,
#155032,#155033,#155034,#155035,#155036,#155037,#155038,#155039,#155040,
#155041,#155042,#155043,#155044,#155045,#155046,#155047,#155048,#155049,
#155050,#155051,#155052,#155053,#155054,#155055,#155056,#155057,#155058,
#155059,#155060,#155061,#155062,#155063,#155064,#155065,#155066,#155067,
#155068,#155069,#155070,#155071,#155072,#155073,#155074,#155075,#155076,
#155077,#155078,#155079,#155080,#155081,#155082,#155083,#155084,#155085,
#155086,#155087,#155088,#155089,#155090,#155091,#155092,#155093,#155094,
#155095,#155096,#155097,#155098,#155099,#155100,#155101,#155102,#155103,
#155104,#155105,#155106,#155107,#155108,#155109,#155110,#155111,#155112,
#155113,#155114,#155115,#155116,#155117,#155118,#155119,#155120,#155121,
#155122,#155123,#155124,#155125,#155126,#155127,#155128,#155129,#155130,
#155131,#155132,#155133,#155134,#155135,#155136,#155137,#155138,#155139,
#155140,#155141,#155142,#155143,#155144,#155145,#155146,#155147,#155148,
#155149,#155150,#155151,#155152,#155153,#155154,#155155,#155156,#155157,
#155158,#155159,#155160,#155161,#155162,#155163,#155164,#155165,#155166,
#155167,#155168,#155169,#155170,#155171,#155172,#155173,#155174,#155175,
#155176,#155177,#155178,#155179,#155180,#155181,#155182,#155183,#155184,
#155185,#155186,#155187,#155188,#155189,#155190,#155191,#155192,#155193,
#155194,#155195,#155196,#155197,#155198,#155199,#155200,#155201,#155202,
#155203,#155204,#155205,#155206,#155207,#155208,#155209,#155210,#155211,
#155212,#155213,#155214,#155215,#155216,#155217,#155218,#155219,#155220,
#155221,#155222,#155223,#155224,#155225,#155226,#155227,#155228,#155229,
#155230,#155231,#155232,#155233,#155234,#155235,#155236,#155237,#155238,
#155239,#155240,#155241,#155242,#155243,#155244,#155245,#155246,#155247,
#155248,#155249,#155250,#155251,#155252,#155253,#155254,#155255,#155256,
#155257,#155258,#155259,#155260,#155261,#155262,#155263,#155264,#155265,
#155266,#155267,#155268,#155269,#155270,#155271,#155272,#155273,#155274,
#155275,#155276,#155277,#155278,#155279,#155280,#155281,#155282,#155283,
#155284,#155285,#155286,#155287,#155288,#155289,#155290,#155291,#155292,
#155293,#155294,#155295,#155296,#155297,#155298,#155299,#155300,#155301,
#155302,#155303,#155304,#155305,#155306,#155307,#155308,#155309,#155310,
#155311,#155312,#155313,#155314,#155315,#155316,#155317,#155318,#155319,
#155320,#155321,#155322,#155323,#155324,#155325,#155326,#155327,#155328,
#155329,#155330,#155331,#155332,#155333,#155334,#155335,#155336,#155337,
#155338,#155339,#155340,#155341,#155342,#155343,#155344,#155345,#155346,
#155347,#155348,#155349,#155350,#155351,#155352,#155353,#155354,#155355,
#155356,#155357,#155358,#155359,#155360,#155361,#155362,#155363,#155364,
#155365,#155366,#155367,#155368,#155369,#155370,#155371,#155372,#155373,
#155374,#155375,#155376,#155377,#155378,#155379,#155380,#155381,#155382,
#155383,#155384,#155385,#155386,#155387,#155388,#155389,#155390,#155391,
#155392,#155393,#155394,#155395,#155396,#155397,#155398,#155399,#155400,
#155401,#155402,#155403,#155404,#155405,#155406,#155407,#155408,#155409,
#155410,#155411,#155412,#155413,#155414,#155415,#155416,#155417,#155418,
#155419,#155420,#155421,#155422,#155423,#155424,#155425,#155426,#155427,
#155428,#155429,#155430,#155431,#155432,#155433,#155434,#155435),
 .UNSPECIFIED.,.F.,.F.,(6,1,1,1,1,1,1,1,1,1,1,1,1,1,1,1,1,1,1,1,1,1,1,1,
1,1,1,1,1,1,1,1,1,1,1,1,1,1,1,1,1,1,1,1,1,1,1,1,1,1,1,1,1,1,1,1,1,1,1,1,
1,1,1,1,1,1,1,1,1,1,1,1,1,1,1,1,1,1,1,1,1,1,1,1,1,1,1,1,1,1,1,1,1,1,1,1,
1,1,1,1,1,1,1,1,1,1,1,1,1,1,1,1,1,1,1,1,1,1,1,1,1,1,1,1,1,1,1,1,1,1,1,1,
1,1,1,1,1,1,1,1,1,1,1,1,1,1,1,1,1,1,1,1,1,1,1,1,1,1,1,1,1,1,1,1,1,1,1,1,
1,1,1,1,1,1,1,1,1,1,1,1,1,1,1,1,1,1,1,1,1,1,1,1,1,1,1,1,1,1,1,1,1,1,1,1,
1,1,1,1,1,1,1,1,1,1,1,1,1,1,1,1,1,1,1,1,1,1,1,1,1,1,1,1,1,1,1,1,1,1,1,1,
1,1,1,1,1,1,1,1,1,1,1,1,1,1,1,1,1,1,1,1,1,1,1,1,1,1,1,1,1,1,1,1,1,1,1,1,
1,1,1,1,1,1,1,1,1,1,1,1,1,1,1,1,1,1,1,1,1,1,1,1,1,1,1,1,1,1,1,1,1,1,1,1,
1,1,1,1,1,1,1,1,1,1,1,1,1,1,1,1,1,1,1,1,1,1,1,1,1,1,1,1,1,1,1,1,1,1,1,1,
1,1,1,1,1,1,1,1,1,1,1,1,1,1,1,1,1,1,1,1,1,1,1,1,1,1,1,1,1,1,1,1,1,1,1,1,
1,1,1,1,1,1,1,1,1,1,1,1,1,1,1,1,1,1,1,1,1,1,1,1,1,1,1,1,1,1,1,1,1,1,1,1,
1,1,1,1,1,1,1,1,1,1,1,1,1,1,1,1,1,1,1,1,1,1,1,1,1,1,1,1,1,1,1,1,1,1,1,1,
1,1,1,1,1,1,1,1,1,1,6),(0.143172102,0.144954128,0.146788991,0.148623853,
0.150458716,0.152293578,0.15412844,0.155963303,0.157798165,0.159633028,
0.16146789,0.163302752,0.165137615,0.166972477,0.168807339,0.170642202,
0.172477064,0.174311927,0.176146789,0.177981651,0.179816514,0.181651376,
0.183486239,0.185321101,0.187155963,0.188990826,0.190825688,0.19266055,
0.194495413,0.196330275,0.198165138,0.2,0.201834862,0.203669725,0.205504587,
0.20733945,0.209174312,0.211009174,0.212844037,0.214678899,0.216513761,
0.218348624,0.220183486,0.222018349,0.223853211,0.225688073,0.227522936,
0.231192661,0.233027523,0.234862385,0.236697248,0.23853211,0.240366972,
0.242201835,0.244036697,0.24587156,0.247706422,0.249541284,0.251376147,
0.253211009,0.255045872,0.256880734,0.258715596,0.260550459,0.262385321,
0.264220183,0.266055046,0.267889908,0.269724771,0.271559633,0.273394495,
0.275229358,0.27706422,0.278899083,0.280733945,0.282568807,0.28440367,0.286238532,
0.288073394,0.289908257,0.291743119,0.293577982,0.295412844,0.297247706,
0.299082569,0.300917431,0.302752294,0.304587156,0.306422018,0.308256881,
0.310091743,0.311926606,0.313761468,0.31559633,0.317431193,0.319266055,
0.321100917,0.32293578,0.324770642,0.326605505,0.328440367,0.330275229,
0.332110092,0.333944954,0.335779817,0.337614679,0.339449541,0.341284404,
0.343119266,0.344954128,0.346788991,0.348623853,0.350458716,0.352293578,
0.35412844,0.355963303,0.357798165,0.359633028,0.36146789,0.363302752,0.365137615,
0.366972477,0.368807339,0.370642202,0.372477064,0.374311927,0.376146789,
0.377981651,0.379816514,0.381651376,0.383486239,0.385321101,0.387155963,
0.388990826,0.390825688,0.39266055,0.394495413,0.396330275,0.398165138,
0.4,0.401834862,0.403669725,0.405504587,0.40733945,0.409174312,0.411009174,
0.412844037,0.414678899,0.416513761,0.418348624,0.420183486,0.422018349,
0.423853211,0.425688073,0.427522936,0.429357798,0.431192661,0.433027523,
0.434862385,0.436697248,0.43853211,0.440366972,0.442201835,0.444036697,
0.44587156,0.447706422,0.449541284,0.451376147,0.453211009,0.455045872,
0.456880734,0.458715596,0.460550459,0.462385321,0.464220183,0.466055046,
0.467889908,0.469724771,0.471559633,0.473394495,0.475229358,0.47706422,
0.478899083,0.480733945,0.482568807,0.48440367,0.486238532,0.488073394,
0.489908257,0.491743119,0.493577982,0.495412844,0.497247706,0.499082569,
0.500917431,0.502752294,0.504587156,0.506422018,0.508256881,0.510091743,
0.511926606,0.513761468,0.51559633,0.517431193,0.519266055,0.521100917,
0.52293578,0.524770642,0.526605505,0.528440367,0.530275229,0.532110092,
0.533944954,0.535779817,0.537614679,0.539449541,0.541284404,0.543119266,
0.544954128,0.546788991,0.548623853,0.550458716,0.552293578,0.55412844,
0.555963303,0.557798165,0.559633028,0.56146789,0.563302752,0.565137615,
0.566972477,0.568807339,0.570642202,0.572477064,0.574311927,0.576146789,
0.577981651,0.579816514,0.581651376,0.583486239,0.585321101,0.587155963,
0.588990826,0.590825688,0.59266055,0.594495413,0.596330275,0.598165138,
0.6,0.601834862,0.603669725,0.605504587,0.60733945,0.609174312,0.611009174,
0.612844037,0.614678899,0.616513761,0.618348624,0.620183486,0.622018349,
0.623853211,0.625688073,0.627522936,0.629357798,0.631192661,0.633027523,
0.634862385,0.636697248,0.63853211,0.640366972,0.642201835,0.644036697,
0.64587156,0.647706422,0.649541284,0.651376147,0.653211009,0.655045872,
0.656880734,0.658715596,0.660550459,0.662385321,0.664220183,0.666055046,
0.667889908,0.669724771,0.671559633,0.673394495,0.675229358,0.67706422,
0.678899083,0.680733945,0.682568807,0.68440367,0.686238532,0.688073394,
0.689908257,0.691743119,0.693577982,0.695412844,0.697247706,0.699082569,
0.700917431,0.702752294,0.704587156,0.706422018,0.708256881,0.710091743,
0.711926606,0.713761468,0.71559633,0.717431193,0.719266055,0.721100917,
0.72293578,0.724770642,0.726605505,0.728440367,0.730275229,0.732110092,
0.733944954,0.735779817,0.737614679,0.739449541,0.741284404,0.743119266,
0.744954128,0.746788991,0.748623853,0.750458716,0.752293578,0.75412844,
0.755963303,0.757798165,0.759633028,0.76146789,0.763302752,0.765137615,
0.766972477,0.768807339,0.770642202,0.772477064,0.774311927,0.776146789,
0.777981651,0.779816514,0.781651376,0.783486239,0.785321101,0.787155963,
0.788990826,0.790825688,0.79266055,0.794495413,0.796330275,0.798165138,
0.8,0.801834862,0.803669725,0.805504587,0.80733945,0.809174312,0.811009174,
0.812844037,0.814678899,0.816513761,0.818348624,0.820183486,0.822018349,
0.823853211,0.825688073,0.827522936,0.829357798,0.831192661,0.833027523,
0.834862385,0.836697248,0.83853211,0.840366972,0.842201835,0.844036697,
0.84587156,0.847706422,0.849541284,0.851376147,0.853211009,0.855045872,
0.856880734,0.858715596,0.860550459,0.862385321,0.864220183,0.866055046,
0.867889908,0.869724771,0.871559633,0.873394495,0.875229358,0.87706422,
0.878899083,0.880733945,0.882568807,0.88440367,0.886238532,0.888073394,
0.889908257,0.891743119,0.893577982,0.895412844,0.897247706,0.899082569,
0.900917431,0.902752294,0.904587156,0.906422018,0.908256881,0.910091743,
0.911926606,0.913761468,0.91559633,0.917431193,0.919266055,0.921100917,
0.92293578,0.924770642,0.926605505,0.928440367,0.930275229,0.932110092,
0.933944954,0.935779817,0.937614679,0.939449541,0.941284404,0.943119266,
0.944954128,0.946788991,0.948623853,0.950458716,0.952293578,0.95412844,
0.955963303,0.957798165,0.959633028,0.96146789,0.963302752,0.965137615,
0.966972477,0.968807339,0.970642202,0.972477064,0.974311927,0.976146789,
0.977981651,0.979816514,0.981651376,0.983486239,0.985321101,0.987155963,
0.988990826,0.990825688,0.99266055,0.994495413,0.996330275,0.998165138,
1.),.UNSPECIFIED.);
#24321=B_SPLINE_CURVE_WITH_KNOTS('',5,(#156383,#156384,#156385,#156386,
#156387,#156388,#156389,#156390,#156391,#156392,#156393,#156394,#156395,
#156396,#156397,#156398,#156399,#156400,#156401,#156402,#156403,#156404,
#156405,#156406,#156407,#156408,#156409,#156410,#156411,#156412,#156413,
#156414,#156415,#156416,#156417,#156418,#156419,#156420,#156421,#156422,
#156423,#156424,#156425,#156426,#156427,#156428,#156429,#156430,#156431,
#156432,#156433,#156434,#156435,#156436,#156437,#156438,#156439,#156440,
#156441,#156442,#156443,#156444,#156445,#156446,#156447,#156448,#156449,
#156450,#156451,#156452,#156453,#156454,#156455,#156456,#156457,#156458,
#156459,#156460,#156461,#156462,#156463,#156464,#156465,#156466,#156467,
#156468,#156469,#156470,#156471,#156472,#156473,#156474,#156475,#156476,
#156477,#156478,#156479,#156480,#156481,#156482,#156483,#156484,#156485,
#156486,#156487,#156488,#156489,#156490,#156491,#156492,#156493,#156494,
#156495,#156496,#156497,#156498,#156499,#156500,#156501,#156502,#156503,
#156504,#156505,#156506,#156507,#156508,#156509,#156510,#156511,#156512,
#156513,#156514,#156515,#156516,#156517,#156518,#156519,#156520,#156521,
#156522,#156523,#156524,#156525,#156526,#156527,#156528,#156529,#156530,
#156531,#156532,#156533,#156534,#156535,#156536,#156537,#156538,#156539,
#156540,#156541,#156542,#156543,#156544,#156545,#156546,#156547,#156548,
#156549,#156550,#156551,#156552,#156553,#156554,#156555,#156556,#156557,
#156558,#156559,#156560,#156561,#156562,#156563,#156564,#156565,#156566,
#156567,#156568,#156569,#156570,#156571,#156572,#156573,#156574,#156575,
#156576,#156577,#156578,#156579,#156580,#156581,#156582,#156583,#156584,
#156585,#156586,#156587,#156588,#156589,#156590,#156591,#156592,#156593,
#156594,#156595,#156596,#156597,#156598,#156599,#156600,#156601,#156602,
#156603,#156604,#156605,#156606,#156607,#156608,#156609,#156610,#156611,
#156612,#156613,#156614,#156615,#156616,#156617,#156618,#156619,#156620,
#156621,#156622,#156623,#156624,#156625,#156626,#156627,#156628,#156629,
#156630,#156631,#156632,#156633,#156634,#156635,#156636,#156637,#156638,
#156639,#156640,#156641,#156642,#156643,#156644,#156645,#156646,#156647,
#156648,#156649,#156650,#156651,#156652,#156653,#156654,#156655,#156656,
#156657,#156658,#156659,#156660,#156661,#156662,#156663,#156664,#156665,
#156666,#156667,#156668,#156669,#156670,#156671,#156672,#156673,#156674,
#156675,#156676,#156677,#156678,#156679,#156680,#156681,#156682,#156683,
#156684,#156685,#156686,#156687,#156688,#156689,#156690,#156691,#156692,
#156693,#156694,#156695,#156696,#156697,#156698,#156699,#156700,#156701,
#156702,#156703,#156704,#156705,#156706,#156707,#156708,#156709,#156710,
#156711,#156712,#156713,#156714,#156715,#156716,#156717,#156718,#156719,
#156720,#156721,#156722,#156723,#156724,#156725,#156726,#156727,#156728,
#156729,#156730,#156731,#156732,#156733,#156734,#156735,#156736,#156737,
#156738,#156739,#156740,#156741,#156742,#156743,#156744,#156745,#156746,
#156747,#156748,#156749,#156750,#156751,#156752,#156753,#156754,#156755,
#156756,#156757,#156758,#156759,#156760,#156761,#156762,#156763,#156764,
#156765,#156766,#156767,#156768,#156769,#156770,#156771,#156772,#156773,
#156774,#156775,#156776,#156777,#156778,#156779,#156780,#156781,#156782,
#156783,#156784,#156785,#156786,#156787,#156788,#156789,#156790,#156791,
#156792,#156793,#156794,#156795,#156796,#156797,#156798,#156799,#156800,
#156801,#156802,#156803,#156804,#156805,#156806,#156807,#156808,#156809,
#156810,#156811,#156812,#156813,#156814,#156815,#156816,#156817,#156818,
#156819,#156820,#156821,#156822,#156823,#156824,#156825,#156826,#156827,
#156828,#156829,#156830,#156831,#156832,#156833,#156834,#156835,#156836,
#156837,#156838,#156839,#156840,#156841,#156842,#156843,#156844,#156845,
#156846,#156847,#156848,#156849,#156850,#156851,#156852,#156853,#156854),
 .UNSPECIFIED.,.F.,.F.,(6,1,1,1,1,1,1,1,1,1,1,1,1,1,1,1,1,1,1,1,1,1,1,1,
1,1,1,1,1,1,1,1,1,1,1,1,1,1,1,1,1,1,1,1,1,1,1,1,1,1,1,1,1,1,1,1,1,1,1,1,
1,1,1,1,1,1,1,1,1,1,1,1,1,1,1,1,1,1,1,1,1,1,1,1,1,1,1,1,1,1,1,1,1,1,1,1,
1,1,1,1,1,1,1,1,1,1,1,1,1,1,1,1,1,1,1,1,1,1,1,1,1,1,1,1,1,1,1,1,1,1,1,1,
1,1,1,1,1,1,1,1,1,1,1,1,1,1,1,1,1,1,1,1,1,1,1,1,1,1,1,1,1,1,1,1,1,1,1,1,
1,1,1,1,1,1,1,1,1,1,1,1,1,1,1,1,1,1,1,1,1,1,1,1,1,1,1,1,1,1,1,1,1,1,1,1,
1,1,1,1,1,1,1,1,1,1,1,1,1,1,1,1,1,1,1,1,1,1,1,1,1,1,1,1,1,1,1,1,1,1,1,1,
1,1,1,1,1,1,1,1,1,1,1,1,1,1,1,1,1,1,1,1,1,1,1,1,1,1,1,1,1,1,1,1,1,1,1,1,
1,1,1,1,1,1,1,1,1,1,1,1,1,1,1,1,1,1,1,1,1,1,1,1,1,1,1,1,1,1,1,1,1,1,1,1,
1,1,1,1,1,1,1,1,1,1,1,1,1,1,1,1,1,1,1,1,1,1,1,1,1,1,1,1,1,1,1,1,1,1,1,1,
1,1,1,1,1,1,1,1,1,1,1,1,1,1,1,1,1,1,1,1,1,1,1,1,1,1,1,1,1,1,1,1,1,1,1,1,
1,1,1,1,1,1,1,1,1,1,1,1,1,1,1,1,1,1,1,1,1,1,1,1,1,1,1,1,1,1,1,1,1,1,1,1,
1,1,1,1,1,1,1,1,1,1,1,1,1,1,1,1,1,1,1,1,1,1,1,1,1,1,1,1,1,1,1,1,1,1,1,1,
1,1,1,1,1,1,1,1,1,1,1,6),(-1.,-0.998165138,-0.996330275,-0.994495413,-0.99266055,
-0.990825688,-0.988990826,-0.987155963,-0.985321101,-0.983486239,-0.981651376,
-0.979816514,-0.977981651,-0.976146789,-0.974311927,-0.972477064,-0.970642202,
-0.968807339,-0.966972477,-0.965137615,-0.963302752,-0.96146789,-0.959633028,
-0.957798165,-0.955963303,-0.95412844,-0.952293578,-0.950458716,-0.948623853,
-0.946788991,-0.944954128,-0.943119266,-0.941284404,-0.939449541,-0.937614679,
-0.935779817,-0.933944954,-0.932110092,-0.930275229,-0.928440367,-0.926605505,
-0.924770642,-0.92293578,-0.921100917,-0.919266055,-0.917431193,-0.91559633,
-0.913761468,-0.911926606,-0.910091743,-0.908256881,-0.906422018,-0.904587156,
-0.902752294,-0.900917431,-0.899082569,-0.897247706,-0.895412844,-0.893577982,
-0.891743119,-0.889908257,-0.888073394,-0.886238532,-0.88440367,-0.882568807,
-0.880733945,-0.878899083,-0.87706422,-0.875229358,-0.873394495,-0.871559633,
-0.869724771,-0.867889908,-0.866055046,-0.864220183,-0.862385321,-0.860550459,
-0.858715596,-0.856880734,-0.855045872,-0.853211009,-0.851376147,-0.849541284,
-0.847706422,-0.84587156,-0.844036697,-0.842201835,-0.840366972,-0.83853211,
-0.836697248,-0.834862385,-0.833027523,-0.831192661,-0.829357798,-0.827522936,
-0.825688073,-0.823853211,-0.822018349,-0.820183486,-0.818348624,-0.816513761,
-0.814678899,-0.812844037,-0.811009174,-0.809174312,-0.80733945,-0.805504587,
-0.803669725,-0.801834862,-0.8,-0.798165138,-0.796330275,-0.794495413,-0.79266055,
-0.790825688,-0.788990826,-0.787155963,-0.785321101,-0.783486239,-0.781651376,
-0.779816514,-0.777981651,-0.776146789,-0.774311927,-0.772477064,-0.770642202,
-0.768807339,-0.766972477,-0.765137615,-0.763302752,-0.76146789,-0.759633028,
-0.757798165,-0.755963303,-0.75412844,-0.752293578,-0.750458716,-0.748623853,
-0.746788991,-0.744954128,-0.743119266,-0.741284404,-0.739449541,-0.737614679,
-0.735779817,-0.733944954,-0.732110092,-0.730275229,-0.728440367,-0.726605505,
-0.724770642,-0.72293578,-0.721100917,-0.719266055,-0.717431193,-0.71559633,
-0.713761468,-0.711926606,-0.710091743,-0.708256881,-0.706422018,-0.704587156,
-0.702752294,-0.700917431,-0.699082569,-0.697247706,-0.695412844,-0.693577982,
-0.691743119,-0.689908257,-0.688073394,-0.686238532,-0.68440367,-0.682568807,
-0.680733945,-0.678899083,-0.67706422,-0.675229358,-0.673394495,-0.671559633,
-0.669724771,-0.667889908,-0.666055046,-0.664220183,-0.662385321,-0.660550459,
-0.658715596,-0.656880734,-0.655045872,-0.653211009,-0.651376147,-0.649541284,
-0.647706422,-0.64587156,-0.644036697,-0.642201835,-0.640366972,-0.63853211,
-0.636697248,-0.634862385,-0.633027523,-0.631192661,-0.629357798,-0.627522936,
-0.625688073,-0.623853211,-0.622018349,-0.620183486,-0.618348624,-0.616513761,
-0.614678899,-0.612844037,-0.611009174,-0.609174312,-0.60733945,-0.605504587,
-0.603669725,-0.601834862,-0.6,-0.598165138,-0.596330275,-0.594495413,-0.59266055,
-0.590825688,-0.588990826,-0.587155963,-0.585321101,-0.583486239,-0.581651376,
-0.579816514,-0.577981651,-0.576146789,-0.574311927,-0.572477064,-0.570642202,
-0.568807339,-0.566972477,-0.565137615,-0.563302752,-0.56146789,-0.559633028,
-0.557798165,-0.555963303,-0.55412844,-0.552293578,-0.550458716,-0.548623853,
-0.546788991,-0.544954128,-0.543119266,-0.541284404,-0.539449541,-0.537614679,
-0.535779817,-0.533944954,-0.532110092,-0.530275229,-0.528440367,-0.526605505,
-0.524770642,-0.52293578,-0.521100917,-0.519266055,-0.517431193,-0.51559633,
-0.513761468,-0.511926606,-0.510091743,-0.508256881,-0.506422018,-0.504587156,
-0.502752294,-0.500917431,-0.499082569,-0.497247706,-0.495412844,-0.493577982,
-0.491743119,-0.489908257,-0.488073394,-0.486238532,-0.48440367,-0.482568807,
-0.480733945,-0.478899083,-0.47706422,-0.475229358,-0.473394495,-0.471559633,
-0.469724771,-0.467889908,-0.466055046,-0.464220183,-0.462385321,-0.460550459,
-0.458715596,-0.456880734,-0.455045872,-0.453211009,-0.451376147,-0.449541284,
-0.447706422,-0.44587156,-0.444036697,-0.442201835,-0.440366972,-0.43853211,
-0.436697248,-0.434862385,-0.433027523,-0.431192661,-0.429357798,-0.427522936,
-0.425688073,-0.423853211,-0.422018349,-0.420183486,-0.418348624,-0.416513761,
-0.414678899,-0.412844037,-0.411009174,-0.409174312,-0.40733945,-0.405504587,
-0.403669725,-0.401834862,-0.4,-0.398165138,-0.396330275,-0.394495413,-0.39266055,
-0.390825688,-0.388990826,-0.387155963,-0.385321101,-0.383486239,-0.381651376,
-0.379816514,-0.377981651,-0.376146789,-0.374311927,-0.372477064,-0.370642202,
-0.368807339,-0.366972477,-0.365137615,-0.363302752,-0.36146789,-0.359633028,
-0.357798165,-0.355963303,-0.35412844,-0.352293578,-0.350458716,-0.348623853,
-0.346788991,-0.344954128,-0.343119266,-0.341284404,-0.339449541,-0.337614679,
-0.335779817,-0.333944954,-0.332110092,-0.330275229,-0.328440367,-0.326605505,
-0.324770642,-0.32293578,-0.321100917,-0.319266055,-0.317431193,-0.31559633,
-0.313761468,-0.311926606,-0.310091743,-0.308256881,-0.306422018,-0.304587156,
-0.302752294,-0.300917431,-0.299082569,-0.297247706,-0.295412844,-0.293577982,
-0.291743119,-0.289908257,-0.288073394,-0.286238532,-0.28440367,-0.282568807,
-0.280733945,-0.278899083,-0.27706422,-0.275229358,-0.273394495,-0.271559633,
-0.269724771,-0.267889908,-0.266055046,-0.264220183,-0.262385321,-0.260550459,
-0.258715596,-0.256880734,-0.255045872,-0.253211009,-0.251376147,-0.249541284,
-0.247706422,-0.24587156,-0.244036697,-0.242201835,-0.240366972,-0.23853211,
-0.236697248,-0.234862385,-0.233027523,-0.231192661,-0.229357798,-0.227522936,
-0.225688073,-0.223853211,-0.222018349,-0.220183486,-0.218348624,-0.216513761,
-0.214678899,-0.212844037,-0.211009174,-0.209174312,-0.20733945,-0.205504587,
-0.203669725,-0.201834862,-0.2,-0.198165138,-0.196330275,-0.194495413,-0.19266055,
-0.190825688,-0.188990826,-0.187155963,-0.185321101,-0.183486239,-0.181651376,
-0.179816514,-0.177981651,-0.176146789,-0.174311927,-0.172477064,-0.170642202,
-0.168807339,-0.166972477,-0.165137615,-0.163302752,-0.16146789,-0.159633028,
-0.157798165,-0.155963303,-0.15412844,-0.152293578,-0.150458716,-0.148623853,
-0.146788991,-0.144954128,-0.143172102),.UNSPECIFIED.);
#24322=B_SPLINE_CURVE_WITH_KNOTS('',5,(#156855,#156856,#156857,#156858,
#156859,#156860,#156861,#156862,#156863,#156864,#156865,#156866,#156867,
#156868,#156869,#156870,#156871,#156872,#156873,#156874,#156875,#156876,
#156877,#156878,#156879,#156880,#156881,#156882,#156883,#156884,#156885,
#156886,#156887,#156888,#156889,#156890,#156891,#156892,#156893,#156894,
#156895,#156896,#156897,#156898,#156899,#156900,#156901,#156902,#156903,
#156904,#156905,#156906,#156907,#156908,#156909,#156910,#156911,#156912,
#156913,#156914,#156915,#156916,#156917,#156918,#156919,#156920,#156921,
#156922,#156923,#156924,#156925,#156926,#156927,#156928,#156929,#156930,
#156931,#156932,#156933,#156934,#156935,#156936,#156937,#156938,#156939,
#156940,#156941,#156942,#156943,#156944,#156945,#156946,#156947,#156948,
#156949,#156950,#156951,#156952,#156953,#156954,#156955,#156956,#156957,
#156958,#156959,#156960,#156961,#156962,#156963,#156964,#156965,#156966,
#156967,#156968,#156969,#156970,#156971,#156972,#156973,#156974,#156975,
#156976,#156977,#156978,#156979,#156980,#156981,#156982,#156983,#156984,
#156985,#156986,#156987,#156988,#156989,#156990,#156991,#156992,#156993,
#156994,#156995,#156996,#156997,#156998,#156999,#157000,#157001,#157002,
#157003,#157004,#157005,#157006,#157007,#157008,#157009,#157010,#157011,
#157012,#157013,#157014,#157015,#157016,#157017,#157018,#157019,#157020,
#157021,#157022,#157023,#157024,#157025,#157026,#157027,#157028,#157029,
#157030,#157031,#157032,#157033,#157034,#157035,#157036,#157037,#157038,
#157039,#157040,#157041,#157042,#157043,#157044,#157045,#157046,#157047,
#157048,#157049,#157050,#157051,#157052,#157053,#157054,#157055,#157056,
#157057,#157058,#157059,#157060,#157061,#157062,#157063,#157064,#157065,
#157066,#157067,#157068,#157069,#157070,#157071,#157072,#157073,#157074,
#157075,#157076,#157077,#157078,#157079,#157080,#157081,#157082,#157083,
#157084,#157085,#157086,#157087,#157088,#157089,#157090,#157091,#157092,
#157093,#157094,#157095,#157096,#157097,#157098,#157099,#157100,#157101,
#157102,#157103,#157104,#157105,#157106,#157107,#157108,#157109,#157110,
#157111,#157112,#157113,#157114,#157115,#157116,#157117,#157118,#157119,
#157120,#157121,#157122,#157123,#157124,#157125,#157126,#157127,#157128,
#157129,#157130,#157131,#157132,#157133,#157134,#157135,#157136,#157137,
#157138,#157139,#157140,#157141,#157142,#157143,#157144,#157145,#157146,
#157147,#157148,#157149,#157150,#157151,#157152,#157153,#157154,#157155,
#157156,#157157,#157158,#157159,#157160,#157161,#157162,#157163,#157164,
#157165,#157166,#157167,#157168,#157169,#157170,#157171,#157172,#157173,
#157174,#157175,#157176,#157177,#157178,#157179,#157180,#157181,#157182,
#157183,#157184,#157185,#157186,#157187,#157188,#157189,#157190,#157191,
#157192,#157193,#157194,#157195,#157196,#157197,#157198,#157199,#157200,
#157201,#157202,#157203,#157204,#157205,#157206,#157207,#157208,#157209,
#157210,#157211,#157212,#157213,#157214,#157215,#157216,#157217,#157218,
#157219,#157220,#157221,#157222,#157223,#157224,#157225,#157226,#157227,
#157228,#157229,#157230,#157231,#157232,#157233,#157234,#157235,#157236,
#157237,#157238,#157239,#157240,#157241,#157242,#157243,#157244,#157245,
#157246,#157247,#157248,#157249,#157250,#157251,#157252,#157253,#157254,
#157255,#157256,#157257,#157258,#157259,#157260,#157261,#157262,#157263,
#157264,#157265,#157266,#157267,#157268,#157269,#157270,#157271,#157272,
#157273,#157274,#157275,#157276,#157277,#157278,#157279,#157280,#157281,
#157282,#157283,#157284,#157285,#157286,#157287,#157288,#157289,#157290,
#157291,#157292,#157293,#157294,#157295,#157296,#157297,#157298,#157299,
#157300,#157301,#157302,#157303,#157304,#157305,#157306,#157307,#157308,
#157309,#157310,#157311,#157312,#157313,#157314,#157315,#157316,#157317,
#157318,#157319,#157320,#157321,#157322,#157323,#157324,#157325,#157326),
 .UNSPECIFIED.,.F.,.F.,(6,1,1,1,1,1,1,1,1,1,1,1,1,1,1,1,1,1,1,1,1,1,1,1,
1,1,1,1,1,1,1,1,1,1,1,1,1,1,1,1,1,1,1,1,1,1,1,1,1,1,1,1,1,1,1,1,1,1,1,1,
1,1,1,1,1,1,1,1,1,1,1,1,1,1,1,1,1,1,1,1,1,1,1,1,1,1,1,1,1,1,1,1,1,1,1,1,
1,1,1,1,1,1,1,1,1,1,1,1,1,1,1,1,1,1,1,1,1,1,1,1,1,1,1,1,1,1,1,1,1,1,1,1,
1,1,1,1,1,1,1,1,1,1,1,1,1,1,1,1,1,1,1,1,1,1,1,1,1,1,1,1,1,1,1,1,1,1,1,1,
1,1,1,1,1,1,1,1,1,1,1,1,1,1,1,1,1,1,1,1,1,1,1,1,1,1,1,1,1,1,1,1,1,1,1,1,
1,1,1,1,1,1,1,1,1,1,1,1,1,1,1,1,1,1,1,1,1,1,1,1,1,1,1,1,1,1,1,1,1,1,1,1,
1,1,1,1,1,1,1,1,1,1,1,1,1,1,1,1,1,1,1,1,1,1,1,1,1,1,1,1,1,1,1,1,1,1,1,1,
1,1,1,1,1,1,1,1,1,1,1,1,1,1,1,1,1,1,1,1,1,1,1,1,1,1,1,1,1,1,1,1,1,1,1,1,
1,1,1,1,1,1,1,1,1,1,1,1,1,1,1,1,1,1,1,1,1,1,1,1,1,1,1,1,1,1,1,1,1,1,1,1,
1,1,1,1,1,1,1,1,1,1,1,1,1,1,1,1,1,1,1,1,1,1,1,1,1,1,1,1,1,1,1,1,1,1,1,1,
1,1,1,1,1,1,1,1,1,1,1,1,1,1,1,1,1,1,1,1,1,1,1,1,1,1,1,1,1,1,1,1,1,1,1,1,
1,1,1,1,1,1,1,1,1,1,1,1,1,1,1,1,1,1,1,1,1,1,1,1,1,1,1,1,1,1,1,1,1,1,1,1,
1,1,1,1,1,1,1,1,1,1,1,6),(0.143172102,0.144954128,0.146788991,0.148623853,
0.150458716,0.152293578,0.15412844,0.155963303,0.157798165,0.159633028,
0.16146789,0.163302752,0.165137615,0.166972477,0.168807339,0.170642202,
0.172477064,0.174311927,0.176146789,0.177981651,0.179816514,0.181651376,
0.183486239,0.185321101,0.187155963,0.188990826,0.190825688,0.19266055,
0.194495413,0.196330275,0.198165138,0.2,0.201834862,0.203669725,0.205504587,
0.20733945,0.209174312,0.211009174,0.212844037,0.214678899,0.216513761,
0.218348624,0.220183486,0.222018349,0.223853211,0.225688073,0.227522936,
0.229357798,0.231192661,0.233027523,0.234862385,0.236697248,0.23853211,
0.240366972,0.242201835,0.244036697,0.24587156,0.247706422,0.249541284,
0.251376147,0.253211009,0.255045872,0.256880734,0.258715596,0.260550459,
0.262385321,0.264220183,0.266055046,0.267889908,0.269724771,0.271559633,
0.273394495,0.275229358,0.27706422,0.278899083,0.280733945,0.282568807,
0.28440367,0.286238532,0.288073394,0.289908257,0.291743119,0.293577982,
0.295412844,0.297247706,0.299082569,0.300917431,0.302752294,0.304587156,
0.306422018,0.308256881,0.310091743,0.311926606,0.313761468,0.31559633,
0.317431193,0.319266055,0.321100917,0.32293578,0.324770642,0.326605505,
0.328440367,0.330275229,0.332110092,0.333944954,0.335779817,0.337614679,
0.339449541,0.341284404,0.343119266,0.344954128,0.346788991,0.348623853,
0.350458716,0.352293578,0.35412844,0.355963303,0.357798165,0.359633028,
0.36146789,0.363302752,0.365137615,0.366972477,0.368807339,0.370642202,
0.372477064,0.374311927,0.376146789,0.377981651,0.379816514,0.381651376,
0.383486239,0.385321101,0.387155963,0.388990826,0.390825688,0.39266055,
0.394495413,0.396330275,0.398165138,0.4,0.401834862,0.403669725,0.405504587,
0.40733945,0.409174312,0.411009174,0.412844037,0.414678899,0.416513761,
0.418348624,0.420183486,0.422018349,0.423853211,0.425688073,0.427522936,
0.429357798,0.431192661,0.433027523,0.434862385,0.436697248,0.43853211,
0.440366972,0.442201835,0.444036697,0.44587156,0.447706422,0.449541284,
0.451376147,0.453211009,0.455045872,0.456880734,0.458715596,0.460550459,
0.462385321,0.464220183,0.466055046,0.467889908,0.469724771,0.471559633,
0.473394495,0.475229358,0.47706422,0.478899083,0.480733945,0.482568807,
0.48440367,0.486238532,0.488073394,0.489908257,0.491743119,0.493577982,
0.495412844,0.497247706,0.499082569,0.500917431,0.502752294,0.504587156,
0.506422018,0.508256881,0.510091743,0.511926606,0.513761468,0.51559633,
0.517431193,0.519266055,0.521100917,0.52293578,0.524770642,0.526605505,
0.528440367,0.530275229,0.532110092,0.533944954,0.535779817,0.537614679,
0.539449541,0.541284404,0.543119266,0.544954128,0.546788991,0.548623853,
0.550458716,0.552293578,0.55412844,0.555963303,0.557798165,0.559633028,
0.56146789,0.563302752,0.565137615,0.566972477,0.568807339,0.570642202,
0.572477064,0.574311927,0.576146789,0.577981651,0.579816514,0.581651376,
0.583486239,0.585321101,0.587155963,0.588990826,0.590825688,0.59266055,
0.594495413,0.596330275,0.598165138,0.6,0.601834862,0.603669725,0.605504587,
0.60733945,0.609174312,0.611009174,0.612844037,0.614678899,0.616513761,
0.618348624,0.620183486,0.622018349,0.623853211,0.625688073,0.627522936,
0.629357798,0.631192661,0.633027523,0.634862385,0.636697248,0.63853211,
0.640366972,0.642201835,0.644036697,0.64587156,0.647706422,0.649541284,
0.651376147,0.653211009,0.655045872,0.656880734,0.658715596,0.660550459,
0.662385321,0.664220183,0.666055046,0.667889908,0.669724771,0.671559633,
0.673394495,0.675229358,0.67706422,0.678899083,0.680733945,0.682568807,
0.68440367,0.686238532,0.688073394,0.689908257,0.691743119,0.693577982,
0.695412844,0.697247706,0.699082569,0.700917431,0.702752294,0.704587156,
0.706422018,0.708256881,0.710091743,0.711926606,0.713761468,0.71559633,
0.717431193,0.719266055,0.721100917,0.72293578,0.724770642,0.726605505,
0.728440367,0.730275229,0.732110092,0.733944954,0.735779817,0.737614679,
0.739449541,0.741284404,0.743119266,0.744954128,0.746788991,0.748623853,
0.750458716,0.752293578,0.75412844,0.755963303,0.757798165,0.759633028,
0.76146789,0.763302752,0.765137615,0.766972477,0.768807339,0.770642202,
0.772477064,0.774311927,0.776146789,0.777981651,0.779816514,0.781651376,
0.783486239,0.785321101,0.787155963,0.788990826,0.790825688,0.79266055,
0.794495413,0.796330275,0.798165138,0.8,0.801834862,0.803669725,0.805504587,
0.80733945,0.809174312,0.811009174,0.812844037,0.814678899,0.816513761,
0.818348624,0.820183486,0.822018349,0.823853211,0.825688073,0.827522936,
0.829357798,0.831192661,0.833027523,0.834862385,0.836697248,0.83853211,
0.840366972,0.842201835,0.844036697,0.84587156,0.847706422,0.849541284,
0.851376147,0.853211009,0.855045872,0.856880734,0.858715596,0.860550459,
0.862385321,0.864220183,0.866055046,0.867889908,0.869724771,0.871559633,
0.873394495,0.875229358,0.87706422,0.878899083,0.880733945,0.882568807,
0.88440367,0.886238532,0.888073394,0.889908257,0.891743119,0.893577982,
0.895412844,0.897247706,0.899082569,0.900917431,0.902752294,0.904587156,
0.906422018,0.908256881,0.910091743,0.911926606,0.913761468,0.91559633,
0.917431193,0.919266055,0.921100917,0.92293578,0.924770642,0.926605505,
0.928440367,0.930275229,0.932110092,0.933944954,0.935779817,0.937614679,
0.939449541,0.941284404,0.943119266,0.944954128,0.946788991,0.948623853,
0.950458716,0.952293578,0.95412844,0.955963303,0.957798165,0.959633028,
0.96146789,0.963302752,0.965137615,0.966972477,0.968807339,0.970642202,
0.972477064,0.974311927,0.976146789,0.977981651,0.979816514,0.981651376,
0.983486239,0.985321101,0.987155963,0.988990826,0.990825688,0.99266055,
0.994495413,0.996330275,0.998165138,1.),.UNSPECIFIED.);
#24323=B_SPLINE_CURVE_WITH_KNOTS('',3,(#158289,#158290,#158291,#158292,
#158293,#158294,#158295,#158296,#158297,#158298,#158299,#158300,#158301,
#158302,#158303,#158304,#158305,#158306,#158307,#158308,#158309,#158310,
#158311,#158312,#158313,#158314,#158315,#158316,#158317,#158318,#158319,
#158320,#158321,#158322,#158323,#158324,#158325,#158326,#158327,#158328,
#158329,#158330,#158331,#158332,#158333,#158334,#158335,#158336,#158337,
#158338,#158339,#158340,#158341,#158342,#158343,#158344,#158345,#158346,
#158347,#158348,#158349,#158350,#158351,#158352,#158353,#158354,#158355,
#158356,#158357,#158358,#158359,#158360,#158361,#158362,#158363,#158364,
#158365,#158366,#158367,#158368,#158369,#158370,#158371,#158372,#158373,
#158374,#158375,#158376,#158377,#158378,#158379,#158380,#158381,#158382,
#158383,#158384,#158385,#158386,#158387,#158388,#158389,#158390,#158391,
#158392,#158393,#158394,#158395,#158396,#158397,#158398,#158399,#158400,
#158401,#158402,#158403,#158404,#158405,#158406,#158407,#158408,#158409,
#158410,#158411,#158412,#158413,#158414,#158415,#158416,#158417,#158418,
#158419,#158420,#158421,#158422,#158423,#158424,#158425,#158426,#158427,
#158428,#158429,#158430,#158431,#158432,#158433,#158434,#158435,#158436,
#158437,#158438,#158439,#158440,#158441,#158442,#158443,#158444,#158445,
#158446,#158447,#158448,#158449,#158450,#158451,#158452,#158453,#158454,
#158455,#158456,#158457,#158458,#158459,#158460,#158461,#158462,#158463,
#158464,#158465,#158466,#158467,#158468,#158469,#158470,#158471,#158472,
#158473,#158474,#158475,#158476,#158477,#158478,#158479,#158480,#158481,
#158482,#158483,#158484,#158485,#158486,#158487,#158488,#158489,#158490,
#158491,#158492,#158493,#158494,#158495,#158496,#158497,#158498,#158499,
#158500,#158501,#158502,#158503,#158504,#158505,#158506,#158507,#158508,
#158509,#158510,#158511,#158512,#158513,#158514,#158515,#158516,#158517,
#158518,#158519,#158520,#158521,#158522,#158523,#158524,#158525,#158526,
#158527,#158528,#158529,#158530,#158531,#158532,#158533,#158534,#158535,
#158536,#158537,#158538,#158539,#158540,#158541,#158542,#158543,#158544,
#158545,#158546,#158547,#158548,#158549,#158550,#158551,#158552,#158553,
#158554,#158555,#158556,#158557,#158558,#158559,#158560,#158561,#158562,
#158563,#158564,#158565,#158566,#158567,#158568,#158569,#158570,#158571,
#158572,#158573,#158574,#158575,#158576,#158577,#158578,#158579,#158580,
#158581,#158582,#158583,#158584,#158585,#158586,#158587,#158588,#158589,
#158590,#158591,#158592,#158593,#158594,#158595,#158596,#158597,#158598,
#158599,#158600,#158601,#158602,#158603,#158604,#158605,#158606,#158607,
#158608,#158609,#158610),.UNSPECIFIED.,.F.,.F.,(4,3,3,3,3,3,3,3,3,3,3,3,
3,3,3,3,3,3,3,3,3,3,3,3,3,3,3,3,3,3,3,3,3,3,3,3,3,3,3,3,3,3,3,3,3,3,3,3,
3,3,3,3,3,3,3,3,3,3,3,3,3,3,3,3,3,3,3,3,3,3,3,3,3,3,3,3,3,3,3,3,3,3,3,3,
3,3,3,3,3,3,3,3,3,3,3,3,3,3,3,3,3,3,3,3,3,3,3,4),(-1.,-0.994495413,-0.988990826,
-0.983486239,-0.977981651,-0.968807339,-0.963302752,-0.957798165,-0.952293578,
-0.946788991,-0.941284404,-0.935779817,-0.930275229,-0.924770642,-0.919266055,
-0.913761468,-0.908256881,-0.902752294,-0.897247706,-0.891743119,-0.886238532,
-0.880733945,-0.875229358,-0.867889908,-0.862385321,-0.856880734,-0.849541284,
-0.842201835,-0.836697248,-0.831192661,-0.825688073,-0.820183486,-0.814678899,
-0.809174312,-0.801834862,-0.794495413,-0.787155963,-0.779816514,-0.772477064,
-0.765137615,-0.757798165,-0.750458716,-0.741284404,-0.733944954,-0.726605505,
-0.719266055,-0.711926606,-0.704587156,-0.697247706,-0.689908257,-0.678899083,
-0.671559633,-0.664220183,-0.656880734,-0.649541284,-0.642201835,-0.631192661,
-0.623853211,-0.616513761,-0.609174312,-0.601834862,-0.594495413,-0.587155963,
-0.579816514,-0.572477064,-0.565137615,-0.557798165,-0.550458716,-0.543119266,
-0.533944954,-0.524770642,-0.51559633,-0.506422018,-0.497247706,-0.488073394,
-0.478899083,-0.469724771,-0.460550459,-0.451376147,-0.442201835,-0.433027523,
-0.423853211,-0.414678899,-0.405504587,-0.396330275,-0.387155963,-0.374311927,
-0.363302752,-0.352293578,-0.341284404,-0.330275229,-0.319266055,-0.308256881,
-0.297247706,-0.286238532,-0.275229358,-0.264220183,-0.253211009,-0.242201835,
-0.231192661,-0.220183486,-0.209174312,-0.198165138,-0.187155963,-0.176146789,
-0.165137615,-0.15412844,-0.143172102),.UNSPECIFIED.);
#24324=B_SPLINE_CURVE_WITH_KNOTS('',3,(#158611,#158612,#158613,#158614,
#158615,#158616,#158617,#158618,#158619,#158620,#158621,#158622,#158623,
#158624,#158625,#158626,#158627,#158628,#158629,#158630,#158631,#158632,
#158633,#158634,#158635,#158636,#158637,#158638,#158639,#158640,#158641,
#158642,#158643,#158644,#158645,#158646,#158647,#158648,#158649,#158650,
#158651,#158652,#158653,#158654,#158655,#158656,#158657,#158658,#158659,
#158660,#158661,#158662,#158663,#158664,#158665,#158666,#158667,#158668,
#158669,#158670,#158671,#158672,#158673,#158674,#158675,#158676,#158677,
#158678,#158679,#158680,#158681,#158682,#158683,#158684,#158685,#158686,
#158687,#158688,#158689,#158690,#158691,#158692,#158693,#158694,#158695,
#158696,#158697,#158698,#158699,#158700,#158701,#158702,#158703,#158704,
#158705,#158706,#158707,#158708,#158709,#158710,#158711,#158712,#158713,
#158714,#158715,#158716,#158717,#158718,#158719,#158720,#158721,#158722,
#158723,#158724,#158725,#158726,#158727,#158728,#158729,#158730,#158731,
#158732,#158733,#158734,#158735,#158736,#158737,#158738,#158739,#158740,
#158741,#158742,#158743,#158744,#158745,#158746,#158747,#158748,#158749,
#158750,#158751,#158752,#158753,#158754,#158755,#158756,#158757,#158758,
#158759,#158760,#158761,#158762,#158763,#158764,#158765,#158766,#158767,
#158768,#158769,#158770,#158771,#158772,#158773,#158774,#158775,#158776,
#158777,#158778,#158779,#158780,#158781,#158782,#158783,#158784,#158785,
#158786,#158787,#158788,#158789,#158790,#158791,#158792,#158793,#158794,
#158795,#158796,#158797,#158798,#158799,#158800,#158801,#158802,#158803,
#158804,#158805,#158806,#158807,#158808,#158809,#158810,#158811,#158812,
#158813,#158814,#158815,#158816,#158817,#158818,#158819,#158820,#158821,
#158822,#158823,#158824,#158825,#158826,#158827,#158828,#158829,#158830,
#158831,#158832,#158833,#158834,#158835,#158836,#158837,#158838,#158839,
#158840,#158841,#158842,#158843,#158844,#158845,#158846,#158847,#158848,
#158849,#158850,#158851,#158852,#158853,#158854,#158855,#158856,#158857,
#158858,#158859,#158860,#158861,#158862,#158863,#158864,#158865,#158866,
#158867,#158868,#158869,#158870,#158871,#158872,#158873,#158874,#158875,
#158876,#158877,#158878,#158879,#158880,#158881,#158882,#158883,#158884,
#158885,#158886,#158887,#158888,#158889,#158890,#158891,#158892,#158893,
#158894,#158895,#158896,#158897,#158898,#158899,#158900,#158901,#158902,
#158903,#158904,#158905,#158906,#158907,#158908,#158909,#158910,#158911,
#158912,#158913,#158914,#158915,#158916,#158917,#158918,#158919,#158920,
#158921,#158922,#158923,#158924,#158925,#158926),.UNSPECIFIED.,.F.,.F.,
(4,3,3,3,3,3,3,3,3,3,3,3,3,3,3,3,3,3,3,3,3,3,3,3,3,3,3,3,3,3,3,3,3,3,3,
3,3,3,3,3,3,3,3,3,3,3,3,3,3,3,3,3,3,3,3,3,3,3,3,3,3,3,3,3,3,3,3,3,3,3,3,
3,3,3,3,3,3,3,3,3,3,3,3,3,3,3,3,3,3,3,3,3,3,3,3,3,3,3,3,3,3,3,3,3,3,4),
(0.143172102,0.15412844,0.165137615,0.176146789,0.187155963,0.198165138,
0.209174312,0.220183486,0.231192661,0.242201835,0.253211009,0.264220183,
0.275229358,0.286238532,0.297247706,0.310091743,0.321100917,0.332110092,
0.343119266,0.35412844,0.365137615,0.377981651,0.390825688,0.4,0.411009174,
0.420183486,0.429357798,0.43853211,0.447706422,0.456880734,0.466055046,
0.475229358,0.48440367,0.493577982,0.502752294,0.513761468,0.524770642,
0.533944954,0.541284404,0.548623853,0.557798165,0.565137615,0.572477064,
0.579816514,0.587155963,0.594495413,0.601834862,0.609174312,0.616513761,
0.623853211,0.631192661,0.63853211,0.64587156,0.653211009,0.660550459,0.667889908,
0.675229358,0.682568807,0.691743119,0.700917431,0.708256881,0.71559633,
0.72293578,0.730275229,0.737614679,0.744954128,0.752293578,0.759633028,
0.766972477,0.776146789,0.783486239,0.790825688,0.798165138,0.805504587,
0.812844037,0.820183486,0.825688073,0.831192661,0.840366972,0.84587156,
0.853211009,0.858715596,0.864220183,0.869724771,0.87706422,0.882568807,
0.888073394,0.893577982,0.900917431,0.906422018,0.911926606,0.919266055,
0.924770642,0.930275229,0.935779817,0.941284404,0.946788991,0.952293578,
0.957798165,0.963302752,0.968807339,0.974311927,0.979816514,0.985321101,
0.990825688,1.),.UNSPECIFIED.);
#24325=B_SPLINE_CURVE_WITH_KNOTS('',5,(#159871,#159872,#159873,#159874,
#159875,#159876,#159877,#159878,#159879,#159880,#159881,#159882,#159883,
#159884,#159885,#159886,#159887,#159888,#159889,#159890,#159891,#159892,
#159893,#159894,#159895,#159896,#159897,#159898,#159899,#159900,#159901,
#159902,#159903,#159904,#159905,#159906,#159907,#159908,#159909,#159910,
#159911,#159912,#159913,#159914,#159915,#159916,#159917,#159918,#159919,
#159920,#159921,#159922,#159923,#159924,#159925,#159926,#159927,#159928,
#159929,#159930,#159931,#159932,#159933,#159934,#159935,#159936,#159937,
#159938,#159939,#159940,#159941,#159942,#159943,#159944,#159945,#159946,
#159947,#159948,#159949,#159950,#159951,#159952,#159953,#159954,#159955,
#159956,#159957,#159958,#159959,#159960,#159961,#159962,#159963,#159964,
#159965,#159966,#159967,#159968,#159969,#159970,#159971,#159972,#159973,
#159974,#159975,#159976,#159977,#159978,#159979,#159980,#159981,#159982,
#159983,#159984,#159985,#159986,#159987,#159988,#159989,#159990,#159991,
#159992,#159993,#159994,#159995,#159996,#159997,#159998,#159999,#160000,
#160001,#160002,#160003,#160004,#160005,#160006,#160007,#160008,#160009,
#160010,#160011,#160012,#160013,#160014,#160015,#160016,#160017,#160018,
#160019,#160020,#160021,#160022,#160023,#160024,#160025,#160026,#160027,
#160028,#160029,#160030,#160031,#160032,#160033,#160034,#160035,#160036,
#160037,#160038,#160039,#160040,#160041,#160042,#160043,#160044,#160045,
#160046,#160047,#160048,#160049,#160050,#160051,#160052,#160053,#160054,
#160055,#160056,#160057,#160058,#160059,#160060,#160061,#160062,#160063,
#160064,#160065,#160066,#160067,#160068,#160069,#160070,#160071,#160072,
#160073,#160074,#160075,#160076,#160077,#160078,#160079,#160080,#160081,
#160082,#160083,#160084,#160085,#160086,#160087,#160088,#160089,#160090,
#160091,#160092,#160093,#160094,#160095,#160096,#160097,#160098,#160099,
#160100,#160101,#160102,#160103,#160104,#160105,#160106,#160107,#160108,
#160109,#160110,#160111,#160112,#160113,#160114,#160115,#160116,#160117,
#160118,#160119,#160120,#160121,#160122,#160123,#160124,#160125,#160126,
#160127,#160128,#160129,#160130,#160131,#160132,#160133,#160134,#160135,
#160136,#160137,#160138,#160139,#160140,#160141,#160142,#160143,#160144,
#160145,#160146,#160147,#160148,#160149,#160150,#160151,#160152,#160153,
#160154,#160155,#160156,#160157,#160158,#160159,#160160,#160161,#160162,
#160163,#160164,#160165,#160166,#160167,#160168,#160169,#160170,#160171,
#160172,#160173,#160174,#160175,#160176,#160177,#160178,#160179,#160180,
#160181,#160182,#160183,#160184,#160185,#160186,#160187,#160188,#160189,
#160190,#160191,#160192,#160193,#160194,#160195,#160196,#160197,#160198,
#160199,#160200,#160201,#160202,#160203,#160204,#160205,#160206,#160207,
#160208,#160209,#160210,#160211,#160212,#160213,#160214,#160215,#160216,
#160217,#160218,#160219,#160220,#160221,#160222,#160223,#160224,#160225,
#160226,#160227,#160228,#160229,#160230,#160231,#160232,#160233,#160234,
#160235,#160236,#160237,#160238,#160239,#160240,#160241,#160242,#160243,
#160244,#160245,#160246,#160247,#160248,#160249,#160250,#160251,#160252,
#160253,#160254,#160255,#160256,#160257,#160258,#160259,#160260,#160261,
#160262,#160263,#160264,#160265,#160266,#160267,#160268,#160269,#160270,
#160271,#160272,#160273,#160274,#160275,#160276,#160277,#160278,#160279,
#160280,#160281,#160282,#160283,#160284,#160285,#160286,#160287,#160288,
#160289,#160290,#160291,#160292,#160293,#160294,#160295,#160296,#160297,
#160298,#160299,#160300,#160301,#160302,#160303,#160304,#160305,#160306,
#160307,#160308,#160309,#160310,#160311,#160312,#160313,#160314,#160315,
#160316,#160317,#160318,#160319,#160320,#160321,#160322,#160323,#160324,
#160325,#160326,#160327,#160328,#160329,#160330,#160331,#160332,#160333,
#160334,#160335,#160336,#160337,#160338,#160339,#160340,#160341,#160342),
 .UNSPECIFIED.,.F.,.F.,(6,1,1,1,1,1,1,1,1,1,1,1,1,1,1,1,1,1,1,1,1,1,1,1,
1,1,1,1,1,1,1,1,1,1,1,1,1,1,1,1,1,1,1,1,1,1,1,1,1,1,1,1,1,1,1,1,1,1,1,1,
1,1,1,1,1,1,1,1,1,1,1,1,1,1,1,1,1,1,1,1,1,1,1,1,1,1,1,1,1,1,1,1,1,1,1,1,
1,1,1,1,1,1,1,1,1,1,1,1,1,1,1,1,1,1,1,1,1,1,1,1,1,1,1,1,1,1,1,1,1,1,1,1,
1,1,1,1,1,1,1,1,1,1,1,1,1,1,1,1,1,1,1,1,1,1,1,1,1,1,1,1,1,1,1,1,1,1,1,1,
1,1,1,1,1,1,1,1,1,1,1,1,1,1,1,1,1,1,1,1,1,1,1,1,1,1,1,1,1,1,1,1,1,1,1,1,
1,1,1,1,1,1,1,1,1,1,1,1,1,1,1,1,1,1,1,1,1,1,1,1,1,1,1,1,1,1,1,1,1,1,1,1,
1,1,1,1,1,1,1,1,1,1,1,1,1,1,1,1,1,1,1,1,1,1,1,1,1,1,1,1,1,1,1,1,1,1,1,1,
1,1,1,1,1,1,1,1,1,1,1,1,1,1,1,1,1,1,1,1,1,1,1,1,1,1,1,1,1,1,1,1,1,1,1,1,
1,1,1,1,1,1,1,1,1,1,1,1,1,1,1,1,1,1,1,1,1,1,1,1,1,1,1,1,1,1,1,1,1,1,1,1,
1,1,1,1,1,1,1,1,1,1,1,1,1,1,1,1,1,1,1,1,1,1,1,1,1,1,1,1,1,1,1,1,1,1,1,1,
1,1,1,1,1,1,1,1,1,1,1,1,1,1,1,1,1,1,1,1,1,1,1,1,1,1,1,1,1,1,1,1,1,1,1,1,
1,1,1,1,1,1,1,1,1,1,1,1,1,1,1,1,1,1,1,1,1,1,1,1,1,1,1,1,1,1,1,1,1,1,1,1,
1,1,1,1,1,1,1,1,1,1,1,6),(0.143172102,0.144954128,0.146788991,0.148623853,
0.150458716,0.152293578,0.15412844,0.155963303,0.157798165,0.159633028,
0.16146789,0.163302752,0.165137615,0.166972477,0.168807339,0.170642202,
0.172477064,0.174311927,0.176146789,0.177981651,0.179816514,0.181651376,
0.183486239,0.185321101,0.187155963,0.188990826,0.190825688,0.19266055,
0.194495413,0.196330275,0.198165138,0.2,0.201834862,0.203669725,0.205504587,
0.20733945,0.209174312,0.211009174,0.212844037,0.214678899,0.216513761,
0.218348624,0.220183486,0.222018349,0.223853211,0.225688073,0.227522936,
0.229357798,0.231192661,0.233027523,0.234862385,0.236697248,0.23853211,
0.240366972,0.242201835,0.244036697,0.24587156,0.247706422,0.249541284,
0.251376147,0.253211009,0.255045872,0.256880734,0.258715596,0.260550459,
0.262385321,0.264220183,0.266055046,0.267889908,0.269724771,0.271559633,
0.273394495,0.275229358,0.27706422,0.278899083,0.280733945,0.282568807,
0.28440367,0.286238532,0.288073394,0.289908257,0.291743119,0.293577982,
0.295412844,0.297247706,0.299082569,0.300917431,0.302752294,0.304587156,
0.306422018,0.308256881,0.310091743,0.311926606,0.313761468,0.31559633,
0.317431193,0.319266055,0.321100917,0.32293578,0.324770642,0.326605505,
0.328440367,0.330275229,0.332110092,0.333944954,0.335779817,0.337614679,
0.339449541,0.341284404,0.343119266,0.344954128,0.346788991,0.348623853,
0.350458716,0.352293578,0.35412844,0.355963303,0.357798165,0.359633028,
0.36146789,0.363302752,0.365137615,0.366972477,0.368807339,0.370642202,
0.372477064,0.374311927,0.376146789,0.377981651,0.379816514,0.381651376,
0.383486239,0.385321101,0.387155963,0.388990826,0.390825688,0.39266055,
0.394495413,0.396330275,0.398165138,0.4,0.401834862,0.403669725,0.405504587,
0.40733945,0.409174312,0.411009174,0.412844037,0.414678899,0.416513761,
0.418348624,0.420183486,0.422018349,0.423853211,0.425688073,0.427522936,
0.429357798,0.431192661,0.433027523,0.434862385,0.436697248,0.43853211,
0.440366972,0.442201835,0.444036697,0.44587156,0.447706422,0.449541284,
0.451376147,0.453211009,0.455045872,0.456880734,0.458715596,0.460550459,
0.462385321,0.464220183,0.466055046,0.467889908,0.469724771,0.471559633,
0.473394495,0.475229358,0.47706422,0.478899083,0.480733945,0.482568807,
0.48440367,0.486238532,0.488073394,0.489908257,0.491743119,0.493577982,
0.495412844,0.497247706,0.499082569,0.500917431,0.502752294,0.504587156,
0.506422018,0.508256881,0.510091743,0.511926606,0.513761468,0.51559633,
0.517431193,0.519266055,0.521100917,0.52293578,0.524770642,0.526605505,
0.528440367,0.530275229,0.532110092,0.533944954,0.535779817,0.537614679,
0.539449541,0.541284404,0.543119266,0.544954128,0.546788991,0.548623853,
0.550458716,0.552293578,0.55412844,0.555963303,0.557798165,0.559633028,
0.56146789,0.563302752,0.565137615,0.566972477,0.568807339,0.570642202,
0.572477064,0.574311927,0.576146789,0.577981651,0.579816514,0.581651376,
0.583486239,0.585321101,0.587155963,0.588990826,0.590825688,0.59266055,
0.594495413,0.596330275,0.598165138,0.6,0.601834862,0.603669725,0.605504587,
0.60733945,0.609174312,0.611009174,0.612844037,0.614678899,0.616513761,
0.618348624,0.620183486,0.622018349,0.623853211,0.625688073,0.627522936,
0.629357798,0.631192661,0.633027523,0.634862385,0.636697248,0.63853211,
0.640366972,0.642201835,0.644036697,0.64587156,0.647706422,0.649541284,
0.651376147,0.653211009,0.655045872,0.656880734,0.658715596,0.660550459,
0.662385321,0.664220183,0.666055046,0.667889908,0.669724771,0.671559633,
0.673394495,0.675229358,0.67706422,0.678899083,0.680733945,0.682568807,
0.68440367,0.686238532,0.688073394,0.689908257,0.691743119,0.693577982,
0.695412844,0.697247706,0.699082569,0.700917431,0.702752294,0.704587156,
0.706422018,0.708256881,0.710091743,0.711926606,0.713761468,0.71559633,
0.717431193,0.719266055,0.721100917,0.72293578,0.724770642,0.726605505,
0.728440367,0.730275229,0.732110092,0.733944954,0.735779817,0.737614679,
0.739449541,0.741284404,0.743119266,0.744954128,0.746788991,0.748623853,
0.750458716,0.752293578,0.75412844,0.755963303,0.757798165,0.759633028,
0.76146789,0.763302752,0.765137615,0.766972477,0.768807339,0.770642202,
0.772477064,0.774311927,0.776146789,0.777981651,0.779816514,0.781651376,
0.783486239,0.785321101,0.787155963,0.788990826,0.790825688,0.79266055,
0.794495413,0.796330275,0.798165138,0.8,0.801834862,0.803669725,0.805504587,
0.80733945,0.809174312,0.811009174,0.812844037,0.814678899,0.816513761,
0.818348624,0.820183486,0.822018349,0.823853211,0.825688073,0.827522936,
0.829357798,0.831192661,0.833027523,0.834862385,0.836697248,0.83853211,
0.840366972,0.842201835,0.844036697,0.84587156,0.847706422,0.849541284,
0.851376147,0.853211009,0.855045872,0.856880734,0.858715596,0.860550459,
0.862385321,0.864220183,0.866055046,0.867889908,0.869724771,0.871559633,
0.873394495,0.875229358,0.87706422,0.878899083,0.880733945,0.882568807,
0.88440367,0.886238532,0.888073394,0.889908257,0.891743119,0.893577982,
0.895412844,0.897247706,0.899082569,0.900917431,0.902752294,0.904587156,
0.906422018,0.908256881,0.910091743,0.911926606,0.913761468,0.91559633,
0.917431193,0.919266055,0.921100917,0.92293578,0.924770642,0.926605505,
0.928440367,0.930275229,0.932110092,0.933944954,0.935779817,0.937614679,
0.939449541,0.941284404,0.943119266,0.944954128,0.946788991,0.948623853,
0.950458716,0.952293578,0.95412844,0.955963303,0.957798165,0.959633028,
0.96146789,0.963302752,0.965137615,0.966972477,0.968807339,0.970642202,
0.972477064,0.974311927,0.976146789,0.977981651,0.979816514,0.981651376,
0.983486239,0.985321101,0.987155963,0.988990826,0.990825688,0.99266055,
0.994495413,0.996330275,0.998165138,1.),.UNSPECIFIED.);
#24326=B_SPLINE_CURVE_WITH_KNOTS('',5,(#160343,#160344,#160345,#160346,
#160347,#160348,#160349,#160350,#160351,#160352,#160353,#160354,#160355,
#160356,#160357,#160358,#160359,#160360,#160361,#160362,#160363,#160364,
#160365,#160366,#160367,#160368,#160369,#160370,#160371,#160372,#160373,
#160374,#160375,#160376,#160377,#160378,#160379,#160380,#160381,#160382,
#160383,#160384,#160385,#160386,#160387,#160388,#160389,#160390,#160391,
#160392,#160393,#160394,#160395,#160396,#160397,#160398,#160399,#160400,
#160401,#160402,#160403,#160404,#160405,#160406,#160407,#160408,#160409,
#160410,#160411,#160412,#160413,#160414,#160415,#160416,#160417,#160418,
#160419,#160420,#160421,#160422,#160423,#160424,#160425,#160426,#160427,
#160428,#160429,#160430,#160431,#160432,#160433,#160434,#160435,#160436,
#160437,#160438,#160439,#160440,#160441,#160442,#160443,#160444,#160445,
#160446,#160447,#160448,#160449,#160450,#160451,#160452,#160453,#160454,
#160455,#160456,#160457,#160458,#160459,#160460,#160461,#160462,#160463,
#160464,#160465,#160466,#160467,#160468,#160469,#160470,#160471,#160472,
#160473,#160474,#160475,#160476,#160477,#160478,#160479,#160480,#160481,
#160482,#160483,#160484,#160485,#160486,#160487,#160488,#160489,#160490,
#160491,#160492,#160493,#160494,#160495,#160496,#160497,#160498,#160499,
#160500,#160501,#160502,#160503,#160504,#160505,#160506,#160507,#160508,
#160509,#160510,#160511,#160512,#160513,#160514,#160515,#160516,#160517,
#160518,#160519,#160520,#160521,#160522,#160523,#160524,#160525,#160526,
#160527,#160528,#160529,#160530,#160531,#160532,#160533,#160534,#160535,
#160536,#160537,#160538,#160539,#160540,#160541,#160542,#160543,#160544,
#160545,#160546,#160547,#160548,#160549,#160550,#160551,#160552,#160553,
#160554,#160555,#160556,#160557,#160558,#160559,#160560,#160561,#160562,
#160563,#160564,#160565,#160566,#160567,#160568,#160569,#160570,#160571,
#160572,#160573,#160574,#160575,#160576,#160577,#160578,#160579,#160580,
#160581,#160582,#160583,#160584,#160585,#160586,#160587,#160588,#160589,
#160590,#160591,#160592,#160593,#160594,#160595,#160596,#160597,#160598,
#160599,#160600,#160601,#160602,#160603,#160604,#160605,#160606,#160607,
#160608,#160609,#160610,#160611,#160612,#160613,#160614,#160615,#160616,
#160617,#160618,#160619,#160620,#160621,#160622,#160623,#160624,#160625,
#160626,#160627,#160628,#160629,#160630,#160631,#160632,#160633,#160634,
#160635,#160636,#160637,#160638,#160639,#160640,#160641,#160642,#160643,
#160644,#160645,#160646,#160647,#160648,#160649,#160650,#160651,#160652,
#160653,#160654,#160655,#160656,#160657,#160658,#160659,#160660,#160661,
#160662,#160663,#160664,#160665,#160666,#160667,#160668,#160669,#160670,
#160671,#160672,#160673,#160674,#160675,#160676,#160677,#160678,#160679,
#160680,#160681,#160682,#160683,#160684,#160685,#160686,#160687,#160688,
#160689,#160690,#160691,#160692,#160693,#160694,#160695,#160696,#160697,
#160698,#160699,#160700,#160701,#160702,#160703,#160704,#160705,#160706,
#160707,#160708,#160709,#160710,#160711,#160712,#160713,#160714,#160715,
#160716,#160717,#160718,#160719,#160720,#160721,#160722,#160723,#160724,
#160725,#160726,#160727,#160728,#160729,#160730,#160731,#160732,#160733,
#160734,#160735,#160736,#160737,#160738,#160739,#160740,#160741,#160742,
#160743,#160744,#160745,#160746,#160747,#160748,#160749,#160750,#160751,
#160752,#160753,#160754,#160755,#160756,#160757,#160758,#160759,#160760,
#160761,#160762,#160763,#160764,#160765,#160766,#160767,#160768,#160769,
#160770,#160771,#160772,#160773,#160774,#160775,#160776,#160777,#160778,
#160779,#160780,#160781,#160782,#160783,#160784,#160785,#160786,#160787,
#160788,#160789,#160790,#160791,#160792,#160793,#160794,#160795,#160796,
#160797,#160798,#160799,#160800,#160801,#160802,#160803,#160804,#160805,
#160806,#160807,#160808,#160809,#160810,#160811,#160812,#160813,#160814),
 .UNSPECIFIED.,.F.,.F.,(6,1,1,1,1,1,1,1,1,1,1,1,1,1,1,1,1,1,1,1,1,1,1,1,
1,1,1,1,1,1,1,1,1,1,1,1,1,1,1,1,1,1,1,1,1,1,1,1,1,1,1,1,1,1,1,1,1,1,1,1,
1,1,1,1,1,1,1,1,1,1,1,1,1,1,1,1,1,1,1,1,1,1,1,1,1,1,1,1,1,1,1,1,1,1,1,1,
1,1,1,1,1,1,1,1,1,1,1,1,1,1,1,1,1,1,1,1,1,1,1,1,1,1,1,1,1,1,1,1,1,1,1,1,
1,1,1,1,1,1,1,1,1,1,1,1,1,1,1,1,1,1,1,1,1,1,1,1,1,1,1,1,1,1,1,1,1,1,1,1,
1,1,1,1,1,1,1,1,1,1,1,1,1,1,1,1,1,1,1,1,1,1,1,1,1,1,1,1,1,1,1,1,1,1,1,1,
1,1,1,1,1,1,1,1,1,1,1,1,1,1,1,1,1,1,1,1,1,1,1,1,1,1,1,1,1,1,1,1,1,1,1,1,
1,1,1,1,1,1,1,1,1,1,1,1,1,1,1,1,1,1,1,1,1,1,1,1,1,1,1,1,1,1,1,1,1,1,1,1,
1,1,1,1,1,1,1,1,1,1,1,1,1,1,1,1,1,1,1,1,1,1,1,1,1,1,1,1,1,1,1,1,1,1,1,1,
1,1,1,1,1,1,1,1,1,1,1,1,1,1,1,1,1,1,1,1,1,1,1,1,1,1,1,1,1,1,1,1,1,1,1,1,
1,1,1,1,1,1,1,1,1,1,1,1,1,1,1,1,1,1,1,1,1,1,1,1,1,1,1,1,1,1,1,1,1,1,1,1,
1,1,1,1,1,1,1,1,1,1,1,1,1,1,1,1,1,1,1,1,1,1,1,1,1,1,1,1,1,1,1,1,1,1,1,1,
1,1,1,1,1,1,1,1,1,1,1,1,1,1,1,1,1,1,1,1,1,1,1,1,1,1,1,1,1,1,1,1,1,1,1,1,
1,1,1,1,1,1,1,1,1,1,1,6),(0.143172102,0.144954128,0.146788991,0.148623853,
0.150458716,0.152293578,0.15412844,0.155963303,0.157798165,0.159633028,
0.16146789,0.163302752,0.165137615,0.166972477,0.168807339,0.170642202,
0.172477064,0.174311927,0.176146789,0.177981651,0.179816514,0.181651376,
0.183486239,0.185321101,0.187155963,0.188990826,0.190825688,0.19266055,
0.194495413,0.196330275,0.198165138,0.2,0.201834862,0.203669725,0.205504587,
0.20733945,0.209174312,0.211009174,0.212844037,0.214678899,0.216513761,
0.218348624,0.220183486,0.222018349,0.223853211,0.225688073,0.227522936,
0.229357798,0.231192661,0.233027523,0.234862385,0.236697248,0.23853211,
0.240366972,0.242201835,0.244036697,0.24587156,0.247706422,0.249541284,
0.251376147,0.253211009,0.255045872,0.256880734,0.258715596,0.260550459,
0.262385321,0.264220183,0.266055046,0.267889908,0.269724771,0.271559633,
0.273394495,0.275229358,0.27706422,0.278899083,0.280733945,0.282568807,
0.28440367,0.286238532,0.288073394,0.289908257,0.291743119,0.293577982,
0.295412844,0.297247706,0.299082569,0.300917431,0.302752294,0.304587156,
0.306422018,0.308256881,0.310091743,0.311926606,0.313761468,0.31559633,
0.317431193,0.319266055,0.321100917,0.32293578,0.324770642,0.326605505,
0.328440367,0.330275229,0.332110092,0.333944954,0.335779817,0.337614679,
0.339449541,0.341284404,0.343119266,0.344954128,0.346788991,0.348623853,
0.350458716,0.352293578,0.35412844,0.355963303,0.357798165,0.359633028,
0.36146789,0.363302752,0.365137615,0.366972477,0.368807339,0.370642202,
0.372477064,0.374311927,0.376146789,0.377981651,0.379816514,0.381651376,
0.383486239,0.385321101,0.387155963,0.388990826,0.390825688,0.39266055,
0.394495413,0.396330275,0.398165138,0.4,0.401834862,0.403669725,0.405504587,
0.40733945,0.409174312,0.411009174,0.412844037,0.414678899,0.416513761,
0.418348624,0.420183486,0.422018349,0.423853211,0.425688073,0.427522936,
0.429357798,0.431192661,0.433027523,0.434862385,0.436697248,0.43853211,
0.440366972,0.442201835,0.444036697,0.44587156,0.447706422,0.449541284,
0.451376147,0.453211009,0.455045872,0.456880734,0.458715596,0.460550459,
0.462385321,0.464220183,0.466055046,0.467889908,0.469724771,0.471559633,
0.473394495,0.475229358,0.47706422,0.478899083,0.480733945,0.482568807,
0.48440367,0.486238532,0.488073394,0.489908257,0.491743119,0.493577982,
0.495412844,0.497247706,0.499082569,0.500917431,0.502752294,0.504587156,
0.506422018,0.508256881,0.510091743,0.511926606,0.513761468,0.51559633,
0.517431193,0.519266055,0.521100917,0.52293578,0.524770642,0.526605505,
0.528440367,0.530275229,0.532110092,0.533944954,0.535779817,0.537614679,
0.539449541,0.541284404,0.543119266,0.544954128,0.546788991,0.548623853,
0.550458716,0.552293578,0.55412844,0.555963303,0.557798165,0.559633028,
0.56146789,0.563302752,0.565137615,0.566972477,0.568807339,0.570642202,
0.572477064,0.574311927,0.576146789,0.577981651,0.579816514,0.581651376,
0.583486239,0.585321101,0.587155963,0.588990826,0.590825688,0.59266055,
0.594495413,0.596330275,0.598165138,0.6,0.601834862,0.603669725,0.605504587,
0.60733945,0.609174312,0.611009174,0.612844037,0.614678899,0.616513761,
0.618348624,0.620183486,0.622018349,0.623853211,0.625688073,0.627522936,
0.629357798,0.631192661,0.633027523,0.634862385,0.636697248,0.63853211,
0.640366972,0.642201835,0.644036697,0.64587156,0.647706422,0.649541284,
0.651376147,0.653211009,0.655045872,0.656880734,0.658715596,0.660550459,
0.662385321,0.664220183,0.666055046,0.667889908,0.669724771,0.671559633,
0.673394495,0.675229358,0.67706422,0.678899083,0.680733945,0.682568807,
0.68440367,0.686238532,0.688073394,0.689908257,0.691743119,0.693577982,
0.695412844,0.697247706,0.699082569,0.700917431,0.702752294,0.704587156,
0.706422018,0.708256881,0.710091743,0.711926606,0.713761468,0.71559633,
0.717431193,0.719266055,0.721100917,0.72293578,0.724770642,0.726605505,
0.728440367,0.730275229,0.732110092,0.733944954,0.735779817,0.737614679,
0.739449541,0.741284404,0.743119266,0.744954128,0.746788991,0.748623853,
0.750458716,0.752293578,0.75412844,0.755963303,0.757798165,0.759633028,
0.76146789,0.763302752,0.765137615,0.766972477,0.768807339,0.770642202,
0.772477064,0.774311927,0.776146789,0.777981651,0.779816514,0.781651376,
0.783486239,0.785321101,0.787155963,0.788990826,0.790825688,0.79266055,
0.794495413,0.796330275,0.798165138,0.8,0.801834862,0.803669725,0.805504587,
0.80733945,0.809174312,0.811009174,0.812844037,0.814678899,0.816513761,
0.818348624,0.820183486,0.822018349,0.823853211,0.825688073,0.827522936,
0.829357798,0.831192661,0.833027523,0.834862385,0.836697248,0.83853211,
0.840366972,0.842201835,0.844036697,0.84587156,0.847706422,0.849541284,
0.851376147,0.853211009,0.855045872,0.856880734,0.858715596,0.860550459,
0.862385321,0.864220183,0.866055046,0.867889908,0.869724771,0.871559633,
0.873394495,0.875229358,0.87706422,0.878899083,0.880733945,0.882568807,
0.88440367,0.886238532,0.888073394,0.889908257,0.891743119,0.893577982,
0.895412844,0.897247706,0.899082569,0.900917431,0.902752294,0.904587156,
0.906422018,0.908256881,0.910091743,0.911926606,0.913761468,0.91559633,
0.917431193,0.919266055,0.921100917,0.92293578,0.924770642,0.926605505,
0.928440367,0.930275229,0.932110092,0.933944954,0.935779817,0.937614679,
0.939449541,0.941284404,0.943119266,0.944954128,0.946788991,0.948623853,
0.950458716,0.952293578,0.95412844,0.955963303,0.957798165,0.959633028,
0.96146789,0.963302752,0.965137615,0.966972477,0.968807339,0.970642202,
0.972477064,0.974311927,0.976146789,0.977981651,0.979816514,0.981651376,
0.983486239,0.985321101,0.987155963,0.988990826,0.990825688,0.99266055,
0.994495413,0.996330275,0.998165138,1.),.UNSPECIFIED.);
#24327=B_SPLINE_CURVE_WITH_KNOTS('',3,(#161774,#161775,#161776,#161777,
#161778,#161779,#161780,#161781,#161782,#161783,#161784,#161785,#161786,
#161787,#161788,#161789,#161790,#161791,#161792,#161793,#161794,#161795,
#161796,#161797,#161798,#161799,#161800,#161801,#161802,#161803,#161804,
#161805,#161806,#161807,#161808,#161809,#161810,#161811,#161812,#161813,
#161814,#161815,#161816,#161817,#161818,#161819,#161820,#161821,#161822,
#161823,#161824,#161825,#161826,#161827,#161828,#161829,#161830,#161831,
#161832,#161833,#161834,#161835,#161836,#161837,#161838,#161839,#161840,
#161841,#161842,#161843,#161844,#161845,#161846,#161847,#161848,#161849,
#161850,#161851,#161852,#161853,#161854,#161855,#161856,#161857,#161858,
#161859,#161860,#161861,#161862,#161863,#161864,#161865,#161866,#161867,
#161868,#161869,#161870,#161871,#161872,#161873,#161874,#161875,#161876,
#161877,#161878,#161879,#161880,#161881,#161882,#161883,#161884,#161885,
#161886,#161887,#161888,#161889,#161890,#161891,#161892,#161893,#161894,
#161895,#161896,#161897,#161898,#161899,#161900,#161901,#161902,#161903,
#161904,#161905,#161906,#161907,#161908,#161909,#161910,#161911,#161912,
#161913,#161914,#161915,#161916,#161917,#161918,#161919,#161920,#161921,
#161922,#161923,#161924,#161925,#161926,#161927,#161928,#161929,#161930,
#161931,#161932,#161933,#161934,#161935,#161936,#161937,#161938,#161939,
#161940,#161941,#161942,#161943,#161944,#161945,#161946,#161947,#161948,
#161949,#161950,#161951,#161952,#161953,#161954,#161955,#161956,#161957,
#161958,#161959,#161960,#161961,#161962,#161963,#161964,#161965,#161966,
#161967,#161968,#161969,#161970,#161971,#161972,#161973,#161974,#161975,
#161976,#161977,#161978,#161979,#161980,#161981,#161982,#161983,#161984,
#161985,#161986,#161987,#161988,#161989,#161990,#161991,#161992,#161993,
#161994,#161995,#161996,#161997,#161998,#161999,#162000,#162001,#162002,
#162003,#162004,#162005,#162006,#162007,#162008,#162009,#162010,#162011,
#162012,#162013,#162014,#162015,#162016,#162017,#162018,#162019,#162020,
#162021,#162022,#162023,#162024,#162025,#162026,#162027,#162028,#162029,
#162030,#162031,#162032,#162033,#162034,#162035,#162036,#162037,#162038,
#162039,#162040,#162041,#162042,#162043,#162044,#162045,#162046,#162047,
#162048,#162049,#162050,#162051,#162052,#162053,#162054,#162055,#162056,
#162057,#162058,#162059,#162060,#162061,#162062,#162063,#162064,#162065,
#162066,#162067,#162068,#162069,#162070,#162071,#162072,#162073,#162074,
#162075,#162076,#162077,#162078,#162079,#162080,#162081,#162082,#162083,
#162084,#162085,#162086,#162087,#162088,#162089,#162090,#162091,#162092,
#162093,#162094,#162095,#162096,#162097,#162098,#162099,#162100,#162101,
#162102,#162103,#162104),.UNSPECIFIED.,.F.,.F.,(4,3,3,3,3,3,3,3,3,3,3,3,
3,3,3,3,3,3,3,3,3,3,3,3,3,3,3,3,3,3,3,3,3,3,3,3,3,3,3,3,3,3,3,3,3,3,3,3,
3,3,3,3,3,3,3,3,3,3,3,3,3,3,3,3,3,3,3,3,3,3,3,3,3,3,3,3,3,3,3,3,3,3,3,3,
3,3,3,3,3,3,3,3,3,3,3,3,3,3,3,3,3,3,3,3,3,3,3,3,3,3,4),(0.143172102,0.15412844,
0.165137615,0.176146789,0.187155963,0.198165138,0.209174312,0.220183486,
0.231192661,0.242201835,0.253211009,0.264220183,0.275229358,0.286238532,
0.297247706,0.308256881,0.319266055,0.330275229,0.341284404,0.352293578,
0.365137615,0.376146789,0.388990826,0.398165138,0.40733945,0.416513761,
0.425688073,0.434862385,0.444036697,0.453211009,0.462385321,0.471559633,
0.480733945,0.489908257,0.499082569,0.508256881,0.517431193,0.526605505,
0.533944954,0.541284404,0.548623853,0.555963303,0.563302752,0.570642202,
0.577981651,0.585321101,0.59266055,0.6,0.60733945,0.614678899,0.622018349,
0.629357798,0.636697248,0.644036697,0.651376147,0.658715596,0.666055046,
0.673394495,0.680733945,0.688073394,0.695412844,0.702752294,0.711926606,
0.719266055,0.726605505,0.733944954,0.741284404,0.748623853,0.755963303,
0.763302752,0.770642202,0.777981651,0.785321101,0.79266055,0.8,0.80733945,
0.812844037,0.818348624,0.823853211,0.829357798,0.834862385,0.840366972,
0.84587156,0.851376147,0.856880734,0.862385321,0.867889908,0.873394495,
0.878899083,0.88440367,0.889908257,0.895412844,0.900917431,0.906422018,
0.911926606,0.917431193,0.92293578,0.928440367,0.933944954,0.939449541,
0.944954128,0.950458716,0.955963303,0.96146789,0.966972477,0.972477064,
0.977981651,0.983486239,0.988990826,0.994495413,1.),.UNSPECIFIED.);
#24328=B_SPLINE_CURVE_WITH_KNOTS('',3,(#162105,#162106,#162107,#162108,
#162109,#162110,#162111,#162112,#162113,#162114,#162115,#162116,#162117,
#162118,#162119,#162120,#162121,#162122,#162123,#162124,#162125,#162126,
#162127,#162128,#162129,#162130,#162131,#162132,#162133,#162134,#162135,
#162136,#162137,#162138,#162139,#162140,#162141,#162142,#162143,#162144,
#162145,#162146,#162147,#162148,#162149,#162150,#162151,#162152,#162153,
#162154,#162155,#162156,#162157,#162158,#162159,#162160,#162161,#162162,
#162163,#162164,#162165,#162166,#162167,#162168,#162169,#162170,#162171,
#162172,#162173,#162174,#162175,#162176,#162177,#162178,#162179,#162180,
#162181,#162182,#162183,#162184,#162185,#162186,#162187,#162188,#162189,
#162190,#162191,#162192,#162193,#162194,#162195,#162196,#162197,#162198,
#162199,#162200,#162201,#162202,#162203,#162204,#162205,#162206,#162207,
#162208,#162209,#162210,#162211,#162212,#162213,#162214,#162215,#162216,
#162217,#162218,#162219,#162220,#162221,#162222,#162223,#162224,#162225,
#162226,#162227,#162228,#162229,#162230,#162231,#162232,#162233,#162234,
#162235,#162236,#162237,#162238,#162239,#162240,#162241,#162242,#162243,
#162244,#162245,#162246,#162247,#162248,#162249,#162250,#162251,#162252,
#162253,#162254,#162255,#162256,#162257,#162258,#162259,#162260,#162261,
#162262,#162263,#162264,#162265,#162266,#162267,#162268,#162269,#162270,
#162271,#162272,#162273,#162274,#162275,#162276,#162277,#162278,#162279,
#162280,#162281,#162282,#162283,#162284,#162285,#162286,#162287,#162288,
#162289,#162290,#162291,#162292,#162293,#162294,#162295,#162296,#162297,
#162298,#162299,#162300,#162301,#162302,#162303,#162304,#162305,#162306,
#162307,#162308,#162309,#162310,#162311,#162312,#162313,#162314,#162315,
#162316,#162317,#162318,#162319,#162320,#162321,#162322,#162323,#162324,
#162325,#162326,#162327,#162328,#162329,#162330,#162331,#162332,#162333,
#162334,#162335,#162336,#162337,#162338,#162339,#162340,#162341,#162342,
#162343,#162344,#162345,#162346,#162347,#162348,#162349,#162350,#162351,
#162352,#162353,#162354,#162355,#162356,#162357,#162358,#162359,#162360,
#162361,#162362,#162363,#162364,#162365,#162366,#162367,#162368,#162369,
#162370,#162371,#162372,#162373,#162374,#162375,#162376,#162377,#162378,
#162379,#162380,#162381,#162382,#162383,#162384,#162385,#162386,#162387,
#162388,#162389,#162390,#162391,#162392,#162393,#162394,#162395,#162396,
#162397,#162398,#162399,#162400,#162401,#162402,#162403,#162404,#162405,
#162406,#162407,#162408,#162409,#162410,#162411,#162412,#162413,#162414,
#162415,#162416,#162417,#162418,#162419,#162420,#162421,#162422,#162423,
#162424,#162425,#162426,#162427,#162428,#162429),.UNSPECIFIED.,.F.,.F.,
(4,3,3,3,3,3,3,3,3,3,3,3,3,3,3,3,3,3,3,3,3,3,3,3,3,3,3,3,3,3,3,3,3,3,3,
3,3,3,3,3,3,3,3,3,3,3,3,3,3,3,3,3,3,3,3,3,3,3,3,3,3,3,3,3,3,3,3,3,3,3,3,
3,3,3,3,3,3,3,3,3,3,3,3,3,3,3,3,3,3,3,3,3,3,3,3,3,3,3,3,3,3,3,3,3,3,3,3,
3,4),(0.143172102,0.15412844,0.165137615,0.176146789,0.187155963,0.198165138,
0.209174312,0.220183486,0.231192661,0.242201835,0.253211009,0.264220183,
0.275229358,0.286238532,0.297247706,0.308256881,0.319266055,0.330275229,
0.341284404,0.352293578,0.363302752,0.374311927,0.385321101,0.396330275,
0.405504587,0.414678899,0.423853211,0.433027523,0.442201835,0.451376147,
0.460550459,0.469724771,0.478899083,0.488073394,0.497247706,0.506422018,
0.51559633,0.524770642,0.533944954,0.543119266,0.550458716,0.557798165,
0.565137615,0.572477064,0.579816514,0.587155963,0.594495413,0.601834862,
0.609174312,0.616513761,0.623853211,0.631192661,0.63853211,0.64587156,0.653211009,
0.660550459,0.667889908,0.67706422,0.68440367,0.691743119,0.699082569,0.706422018,
0.713761468,0.721100917,0.728440367,0.735779817,0.743119266,0.750458716,
0.757798165,0.765137615,0.772477064,0.779816514,0.787155963,0.794495413,
0.803669725,0.811009174,0.816513761,0.822018349,0.827522936,0.833027523,
0.83853211,0.844036697,0.849541284,0.855045872,0.860550459,0.866055046,
0.871559633,0.87706422,0.882568807,0.888073394,0.893577982,0.899082569,
0.904587156,0.910091743,0.91559633,0.921100917,0.926605505,0.933944954,
0.939449541,0.944954128,0.950458716,0.955963303,0.96146789,0.968807339,
0.974311927,0.979816514,0.985321101,0.990825688,1.),.UNSPECIFIED.);
#24329=B_SPLINE_CURVE_WITH_KNOTS('',3,(#163377,#163378,#163379,#163380,
#163381,#163382,#163383,#163384,#163385,#163386,#163387,#163388,#163389,
#163390,#163391,#163392,#163393,#163394,#163395,#163396,#163397,#163398,
#163399,#163400,#163401,#163402,#163403,#163404,#163405,#163406,#163407,
#163408,#163409,#163410,#163411,#163412,#163413,#163414,#163415,#163416,
#163417,#163418,#163419,#163420,#163421,#163422,#163423,#163424,#163425,
#163426,#163427,#163428,#163429,#163430,#163431,#163432,#163433,#163434,
#163435,#163436,#163437,#163438,#163439,#163440,#163441,#163442,#163443,
#163444,#163445,#163446,#163447,#163448,#163449,#163450,#163451,#163452,
#163453,#163454,#163455,#163456,#163457,#163458,#163459,#163460,#163461,
#163462,#163463,#163464,#163465,#163466,#163467,#163468,#163469,#163470,
#163471,#163472,#163473,#163474,#163475,#163476,#163477,#163478,#163479,
#163480,#163481,#163482,#163483,#163484,#163485,#163486,#163487,#163488,
#163489,#163490,#163491,#163492,#163493,#163494,#163495,#163496,#163497,
#163498,#163499,#163500,#163501,#163502,#163503,#163504,#163505,#163506,
#163507,#163508,#163509,#163510,#163511,#163512,#163513,#163514,#163515,
#163516,#163517,#163518,#163519,#163520,#163521,#163522,#163523,#163524,
#163525,#163526,#163527,#163528,#163529,#163530,#163531,#163532,#163533,
#163534,#163535,#163536,#163537,#163538,#163539,#163540,#163541,#163542,
#163543,#163544,#163545,#163546,#163547,#163548,#163549,#163550,#163551,
#163552,#163553,#163554,#163555,#163556,#163557,#163558,#163559,#163560,
#163561,#163562,#163563,#163564,#163565,#163566,#163567,#163568,#163569,
#163570,#163571,#163572,#163573,#163574,#163575,#163576,#163577,#163578,
#163579,#163580,#163581,#163582,#163583,#163584,#163585,#163586,#163587,
#163588,#163589,#163590,#163591,#163592,#163593,#163594,#163595,#163596,
#163597,#163598,#163599,#163600,#163601,#163602,#163603,#163604,#163605,
#163606,#163607,#163608,#163609,#163610,#163611,#163612,#163613,#163614,
#163615,#163616,#163617,#163618,#163619,#163620,#163621,#163622,#163623,
#163624,#163625,#163626,#163627,#163628,#163629,#163630,#163631,#163632,
#163633,#163634,#163635,#163636,#163637,#163638,#163639,#163640,#163641,
#163642,#163643,#163644,#163645,#163646,#163647,#163648,#163649,#163650,
#163651,#163652,#163653,#163654,#163655,#163656,#163657,#163658,#163659,
#163660,#163661,#163662,#163663,#163664,#163665,#163666,#163667,#163668,
#163669,#163670,#163671,#163672,#163673,#163674,#163675,#163676,#163677,
#163678,#163679,#163680,#163681,#163682,#163683,#163684,#163685,#163686,
#163687,#163688,#163689,#163690,#163691,#163692,#163693,#163694,#163695,
#163696,#163697,#163698),.UNSPECIFIED.,.F.,.F.,(4,3,3,3,3,3,3,3,3,3,3,3,
3,3,3,3,3,3,3,3,3,3,3,3,3,3,3,3,3,3,3,3,3,3,3,3,3,3,3,3,3,3,3,3,3,3,3,3,
3,3,3,3,3,3,3,3,3,3,3,3,3,3,3,3,3,3,3,3,3,3,3,3,3,3,3,3,3,3,3,3,3,3,3,3,
3,3,3,3,3,3,3,3,3,3,3,3,3,3,3,3,3,3,3,3,3,3,3,4),(-1.,-0.994495413,-0.988990826,
-0.983486239,-0.977981651,-0.972477064,-0.965137615,-0.957798165,-0.952293578,
-0.946788991,-0.939449541,-0.933944954,-0.928440367,-0.92293578,-0.917431193,
-0.911926606,-0.906422018,-0.900917431,-0.895412844,-0.889908257,-0.88440367,
-0.87706422,-0.871559633,-0.866055046,-0.860550459,-0.855045872,-0.849541284,
-0.840366972,-0.834862385,-0.829357798,-0.823853211,-0.818348624,-0.812844037,
-0.80733945,-0.8,-0.79266055,-0.783486239,-0.776146789,-0.768807339,-0.76146789,
-0.75412844,-0.746788991,-0.739449541,-0.732110092,-0.724770642,-0.717431193,
-0.708256881,-0.700917431,-0.691743119,-0.68440367,-0.67706422,-0.669724771,
-0.662385321,-0.655045872,-0.647706422,-0.640366972,-0.633027523,-0.625688073,
-0.618348624,-0.611009174,-0.603669725,-0.596330275,-0.588990826,-0.579816514,
-0.572477064,-0.565137615,-0.557798165,-0.550458716,-0.543119266,-0.535779817,
-0.528440367,-0.519266055,-0.510091743,-0.499082569,-0.489908257,-0.480733945,
-0.471559633,-0.462385321,-0.453211009,-0.444036697,-0.434862385,-0.425688073,
-0.416513761,-0.40733945,-0.398165138,-0.388990826,-0.377981651,-0.366972477,
-0.355963303,-0.344954128,-0.333944954,-0.32293578,-0.311926606,-0.300917431,
-0.289908257,-0.278899083,-0.267889908,-0.256880734,-0.24587156,-0.234862385,
-0.223853211,-0.212844037,-0.201834862,-0.190825688,-0.179816514,-0.168807339,
-0.157798165,-0.143172102),.UNSPECIFIED.);
#24330=B_SPLINE_CURVE_WITH_KNOTS('',3,(#163699,#163700,#163701,#163702,
#163703,#163704,#163705,#163706,#163707,#163708,#163709,#163710,#163711,
#163712,#163713,#163714,#163715,#163716,#163717,#163718,#163719,#163720,
#163721,#163722,#163723,#163724,#163725,#163726,#163727,#163728,#163729,
#163730,#163731,#163732,#163733,#163734,#163735,#163736,#163737,#163738,
#163739,#163740,#163741,#163742,#163743,#163744,#163745,#163746,#163747,
#163748,#163749,#163750,#163751,#163752,#163753,#163754,#163755,#163756,
#163757,#163758,#163759,#163760,#163761,#163762,#163763,#163764,#163765,
#163766,#163767,#163768,#163769,#163770,#163771,#163772,#163773,#163774,
#163775,#163776,#163777,#163778,#163779,#163780,#163781,#163782,#163783,
#163784,#163785,#163786,#163787,#163788,#163789,#163790,#163791,#163792,
#163793,#163794,#163795,#163796,#163797,#163798,#163799,#163800,#163801,
#163802,#163803,#163804,#163805,#163806,#163807,#163808,#163809,#163810,
#163811,#163812,#163813,#163814,#163815,#163816,#163817,#163818,#163819,
#163820,#163821,#163822,#163823,#163824,#163825,#163826,#163827,#163828,
#163829,#163830,#163831,#163832,#163833,#163834,#163835,#163836,#163837,
#163838,#163839,#163840,#163841,#163842,#163843,#163844,#163845,#163846,
#163847,#163848,#163849,#163850,#163851,#163852,#163853,#163854,#163855,
#163856,#163857,#163858,#163859,#163860,#163861,#163862,#163863,#163864,
#163865,#163866,#163867,#163868,#163869,#163870,#163871,#163872,#163873,
#163874,#163875,#163876,#163877,#163878,#163879,#163880,#163881,#163882,
#163883,#163884,#163885,#163886,#163887,#163888,#163889,#163890,#163891,
#163892,#163893,#163894,#163895,#163896,#163897,#163898,#163899,#163900,
#163901,#163902,#163903,#163904,#163905,#163906,#163907,#163908,#163909,
#163910,#163911,#163912,#163913,#163914,#163915,#163916,#163917,#163918,
#163919,#163920,#163921,#163922,#163923,#163924,#163925,#163926,#163927,
#163928,#163929,#163930,#163931,#163932,#163933,#163934,#163935,#163936,
#163937,#163938,#163939,#163940,#163941,#163942,#163943,#163944,#163945,
#163946,#163947,#163948,#163949,#163950,#163951,#163952,#163953,#163954,
#163955,#163956,#163957,#163958,#163959,#163960,#163961,#163962,#163963,
#163964,#163965,#163966,#163967,#163968,#163969,#163970,#163971,#163972,
#163973,#163974,#163975,#163976,#163977,#163978,#163979,#163980,#163981,
#163982,#163983,#163984,#163985,#163986,#163987,#163988,#163989,#163990,
#163991,#163992,#163993,#163994,#163995,#163996,#163997,#163998,#163999,
#164000,#164001,#164002,#164003,#164004,#164005,#164006,#164007,#164008,
#164009,#164010,#164011,#164012,#164013,#164014),.UNSPECIFIED.,.F.,.F.,
(4,3,3,3,3,3,3,3,3,3,3,3,3,3,3,3,3,3,3,3,3,3,3,3,3,3,3,3,3,3,3,3,3,3,3,
3,3,3,3,3,3,3,3,3,3,3,3,3,3,3,3,3,3,3,3,3,3,3,3,3,3,3,3,3,3,3,3,3,3,3,3,
3,3,3,3,3,3,3,3,3,3,3,3,3,3,3,3,3,3,3,3,3,3,3,3,3,3,3,3,3,3,3,3,3,3,4),
(0.143172102,0.15412844,0.165137615,0.176146789,0.187155963,0.198165138,
0.209174312,0.220183486,0.231192661,0.242201835,0.255045872,0.266055046,
0.27706422,0.288073394,0.299082569,0.310091743,0.321100917,0.332110092,
0.343119266,0.35412844,0.365137615,0.376146789,0.387155963,0.396330275,
0.405504587,0.414678899,0.423853211,0.433027523,0.442201835,0.451376147,
0.460550459,0.469724771,0.478899083,0.488073394,0.497247706,0.506422018,
0.51559633,0.524770642,0.533944954,0.541284404,0.548623853,0.557798165,
0.565137615,0.572477064,0.579816514,0.588990826,0.596330275,0.603669725,
0.611009174,0.618348624,0.625688073,0.633027523,0.640366972,0.647706422,
0.655045872,0.662385321,0.671559633,0.678899083,0.686238532,0.693577982,
0.700917431,0.710091743,0.717431193,0.724770642,0.733944954,0.743119266,
0.750458716,0.757798165,0.766972477,0.776146789,0.783486239,0.790825688,
0.798165138,0.805504587,0.811009174,0.820183486,0.825688073,0.831192661,
0.840366972,0.84587156,0.853211009,0.858715596,0.864220183,0.869724771,
0.87706422,0.882568807,0.888073394,0.893577982,0.900917431,0.906422018,
0.911926606,0.919266055,0.924770642,0.930275229,0.935779817,0.941284404,
0.946788991,0.952293578,0.957798165,0.963302752,0.968807339,0.974311927,
0.979816514,0.985321101,0.990825688,1.),.UNSPECIFIED.);
#24331=B_SPLINE_CURVE_WITH_KNOTS('',3,(#164977,#164978,#164979,#164980,
#164981,#164982,#164983,#164984,#164985,#164986,#164987,#164988,#164989,
#164990,#164991,#164992,#164993,#164994,#164995,#164996,#164997,#164998,
#164999,#165000,#165001,#165002,#165003,#165004,#165005,#165006,#165007,
#165008,#165009,#165010,#165011,#165012,#165013,#165014,#165015,#165016,
#165017,#165018,#165019,#165020,#165021,#165022,#165023,#165024,#165025,
#165026,#165027,#165028,#165029,#165030,#165031,#165032,#165033,#165034,
#165035,#165036,#165037,#165038,#165039,#165040,#165041,#165042,#165043,
#165044,#165045,#165046,#165047,#165048,#165049,#165050,#165051,#165052,
#165053,#165054,#165055,#165056,#165057,#165058,#165059,#165060,#165061,
#165062,#165063,#165064,#165065,#165066,#165067,#165068,#165069,#165070,
#165071,#165072,#165073,#165074,#165075,#165076,#165077,#165078,#165079,
#165080,#165081,#165082,#165083,#165084,#165085,#165086,#165087,#165088,
#165089,#165090,#165091,#165092,#165093,#165094,#165095,#165096,#165097,
#165098,#165099,#165100,#165101,#165102,#165103,#165104,#165105,#165106,
#165107,#165108,#165109,#165110,#165111,#165112,#165113,#165114,#165115,
#165116,#165117,#165118,#165119,#165120,#165121,#165122,#165123,#165124,
#165125,#165126,#165127,#165128,#165129,#165130,#165131,#165132,#165133,
#165134,#165135,#165136,#165137,#165138,#165139,#165140,#165141,#165142,
#165143,#165144,#165145,#165146,#165147,#165148,#165149,#165150,#165151,
#165152,#165153,#165154,#165155,#165156,#165157,#165158,#165159,#165160,
#165161,#165162,#165163,#165164,#165165,#165166,#165167,#165168,#165169,
#165170,#165171,#165172,#165173,#165174,#165175,#165176,#165177,#165178,
#165179,#165180,#165181,#165182,#165183,#165184,#165185,#165186,#165187,
#165188,#165189,#165190,#165191,#165192,#165193,#165194,#165195,#165196,
#165197,#165198,#165199,#165200,#165201,#165202,#165203,#165204,#165205,
#165206,#165207,#165208,#165209,#165210,#165211,#165212,#165213,#165214,
#165215,#165216,#165217,#165218,#165219,#165220,#165221,#165222,#165223,
#165224,#165225,#165226,#165227,#165228,#165229,#165230,#165231,#165232,
#165233,#165234,#165235,#165236,#165237,#165238,#165239,#165240,#165241,
#165242,#165243,#165244,#165245,#165246,#165247,#165248,#165249,#165250,
#165251,#165252,#165253,#165254,#165255,#165256,#165257,#165258,#165259,
#165260,#165261,#165262,#165263,#165264,#165265,#165266,#165267,#165268,
#165269,#165270,#165271,#165272,#165273,#165274,#165275,#165276,#165277,
#165278,#165279,#165280,#165281,#165282,#165283,#165284,#165285,#165286,
#165287,#165288,#165289,#165290,#165291,#165292,#165293,#165294,#165295,
#165296,#165297,#165298,#165299,#165300,#165301),.UNSPECIFIED.,.F.,.F.,
(4,3,3,3,3,3,3,3,3,3,3,3,3,3,3,3,3,3,3,3,3,3,3,3,3,3,3,3,3,3,3,3,3,3,3,
3,3,3,3,3,3,3,3,3,3,3,3,3,3,3,3,3,3,3,3,3,3,3,3,3,3,3,3,3,3,3,3,3,3,3,3,
3,3,3,3,3,3,3,3,3,3,3,3,3,3,3,3,3,3,3,3,3,3,3,3,3,3,3,3,3,3,3,3,3,3,3,3,
3,4),(-1.,-0.994495413,-0.988990826,-0.981651376,-0.976146789,-0.968807339,
-0.963302752,-0.957798165,-0.952293578,-0.946788991,-0.941284404,-0.935779817,
-0.930275229,-0.924770642,-0.919266055,-0.913761468,-0.908256881,-0.900917431,
-0.895412844,-0.889908257,-0.88440367,-0.878899083,-0.873394495,-0.867889908,
-0.862385321,-0.856880734,-0.851376147,-0.84587156,-0.840366972,-0.834862385,
-0.829357798,-0.823853211,-0.818348624,-0.812844037,-0.80733945,-0.8,-0.79266055,
-0.783486239,-0.776146789,-0.768807339,-0.76146789,-0.75412844,-0.746788991,
-0.739449541,-0.732110092,-0.724770642,-0.717431193,-0.708256881,-0.700917431,
-0.693577982,-0.686238532,-0.678899083,-0.671559633,-0.664220183,-0.656880734,
-0.649541284,-0.642201835,-0.634862385,-0.627522936,-0.620183486,-0.612844037,
-0.605504587,-0.598165138,-0.590825688,-0.583486239,-0.576146789,-0.568807339,
-0.56146789,-0.55412844,-0.546788991,-0.539449541,-0.532110092,-0.52293578,
-0.513761468,-0.504587156,-0.495412844,-0.486238532,-0.47706422,-0.467889908,
-0.458715596,-0.449541284,-0.440366972,-0.431192661,-0.422018349,-0.412844037,
-0.403669725,-0.394495413,-0.383486239,-0.372477064,-0.36146789,-0.350458716,
-0.339449541,-0.328440367,-0.31559633,-0.304587156,-0.293577982,-0.282568807,
-0.271559633,-0.258715596,-0.247706422,-0.236697248,-0.225688073,-0.214678899,
-0.203669725,-0.19266055,-0.181651376,-0.170642202,-0.159633028,-0.143172102),
 .UNSPECIFIED.);
#24332=B_SPLINE_CURVE_WITH_KNOTS('',3,(#165302,#165303,#165304,#165305,
#165306,#165307,#165308,#165309,#165310,#165311,#165312,#165313,#165314,
#165315,#165316,#165317,#165318,#165319,#165320,#165321,#165322,#165323,
#165324,#165325,#165326,#165327,#165328,#165329,#165330,#165331,#165332,
#165333,#165334,#165335,#165336,#165337,#165338,#165339,#165340,#165341,
#165342,#165343,#165344,#165345,#165346,#165347,#165348,#165349,#165350,
#165351,#165352,#165353,#165354,#165355,#165356,#165357,#165358,#165359,
#165360,#165361,#165362,#165363,#165364,#165365,#165366,#165367,#165368,
#165369,#165370,#165371,#165372,#165373,#165374,#165375,#165376,#165377,
#165378,#165379,#165380,#165381,#165382,#165383,#165384,#165385,#165386,
#165387,#165388,#165389,#165390,#165391,#165392,#165393,#165394,#165395,
#165396,#165397,#165398,#165399,#165400,#165401,#165402,#165403,#165404,
#165405,#165406,#165407,#165408,#165409,#165410,#165411,#165412,#165413,
#165414,#165415,#165416,#165417,#165418,#165419,#165420,#165421,#165422,
#165423,#165424,#165425,#165426,#165427,#165428,#165429,#165430,#165431,
#165432,#165433,#165434,#165435,#165436,#165437,#165438,#165439,#165440,
#165441,#165442,#165443,#165444,#165445,#165446,#165447,#165448,#165449,
#165450,#165451,#165452,#165453,#165454,#165455,#165456,#165457,#165458,
#165459,#165460,#165461,#165462,#165463,#165464,#165465,#165466,#165467,
#165468,#165469,#165470,#165471,#165472,#165473,#165474,#165475,#165476,
#165477,#165478,#165479,#165480,#165481,#165482,#165483,#165484,#165485,
#165486,#165487,#165488,#165489,#165490,#165491,#165492,#165493,#165494,
#165495,#165496,#165497,#165498,#165499,#165500,#165501,#165502,#165503,
#165504,#165505,#165506,#165507,#165508,#165509,#165510,#165511,#165512,
#165513,#165514,#165515,#165516,#165517,#165518,#165519,#165520,#165521,
#165522,#165523,#165524,#165525,#165526,#165527,#165528,#165529,#165530,
#165531,#165532,#165533,#165534,#165535,#165536,#165537,#165538,#165539,
#165540,#165541,#165542,#165543,#165544,#165545,#165546,#165547,#165548,
#165549,#165550,#165551,#165552,#165553,#165554,#165555,#165556,#165557,
#165558,#165559,#165560,#165561,#165562,#165563,#165564,#165565,#165566,
#165567,#165568,#165569,#165570,#165571,#165572,#165573,#165574,#165575,
#165576,#165577,#165578,#165579,#165580,#165581,#165582,#165583,#165584,
#165585,#165586,#165587,#165588,#165589,#165590,#165591,#165592,#165593,
#165594,#165595,#165596,#165597,#165598,#165599,#165600,#165601,#165602,
#165603,#165604,#165605,#165606,#165607,#165608,#165609,#165610,#165611,
#165612,#165613,#165614,#165615,#165616,#165617,#165618,#165619,#165620,
#165621,#165622,#165623,#165624,#165625,#165626),.UNSPECIFIED.,.F.,.F.,
(4,3,3,3,3,3,3,3,3,3,3,3,3,3,3,3,3,3,3,3,3,3,3,3,3,3,3,3,3,3,3,3,3,3,3,
3,3,3,3,3,3,3,3,3,3,3,3,3,3,3,3,3,3,3,3,3,3,3,3,3,3,3,3,3,3,3,3,3,3,3,3,
3,3,3,3,3,3,3,3,3,3,3,3,3,3,3,3,3,3,3,3,3,3,3,3,3,3,3,3,3,3,3,3,3,3,3,3,
3,4),(0.143172102,0.15412844,0.165137615,0.176146789,0.187155963,0.198165138,
0.209174312,0.220183486,0.231192661,0.242201835,0.256880734,0.267889908,
0.278899083,0.289908257,0.300917431,0.311926606,0.32293578,0.333944954,
0.344954128,0.355963303,0.366972477,0.377981651,0.388990826,0.398165138,
0.40733945,0.416513761,0.425688073,0.434862385,0.444036697,0.453211009,
0.462385321,0.471559633,0.480733945,0.489908257,0.499082569,0.510091743,
0.519266055,0.528440367,0.535779817,0.543119266,0.550458716,0.557798165,
0.565137615,0.572477064,0.579816514,0.587155963,0.594495413,0.601834862,
0.609174312,0.616513761,0.623853211,0.631192661,0.63853211,0.64587156,0.653211009,
0.660550459,0.667889908,0.675229358,0.682568807,0.689908257,0.697247706,
0.704587156,0.711926606,0.719266055,0.726605505,0.733944954,0.741284404,
0.748623853,0.755963303,0.763302752,0.772477064,0.779816514,0.787155963,
0.794495413,0.801834862,0.809174312,0.814678899,0.820183486,0.825688073,
0.831192661,0.840366972,0.84587156,0.851376147,0.856880734,0.862385321,
0.867889908,0.873394495,0.878899083,0.88440367,0.891743119,0.897247706,
0.902752294,0.908256881,0.913761468,0.919266055,0.924770642,0.930275229,
0.935779817,0.941284404,0.946788991,0.952293578,0.957798165,0.963302752,
0.968807339,0.974311927,0.981651376,0.987155963,0.99266055,1.),
 .UNSPECIFIED.);
#24333=B_SPLINE_CURVE_WITH_KNOTS('',3,(#166571,#166572,#166573,#166574,
#166575,#166576,#166577,#166578,#166579,#166580,#166581,#166582,#166583,
#166584,#166585,#166586,#166587,#166588,#166589,#166590,#166591,#166592,
#166593,#166594,#166595,#166596,#166597,#166598,#166599,#166600,#166601,
#166602,#166603,#166604,#166605,#166606,#166607,#166608,#166609,#166610,
#166611,#166612,#166613,#166614,#166615,#166616,#166617,#166618,#166619,
#166620,#166621,#166622,#166623,#166624,#166625,#166626,#166627,#166628,
#166629,#166630,#166631,#166632,#166633,#166634,#166635,#166636,#166637,
#166638,#166639,#166640,#166641,#166642,#166643,#166644,#166645,#166646,
#166647,#166648,#166649,#166650,#166651,#166652,#166653,#166654,#166655,
#166656,#166657,#166658,#166659,#166660,#166661,#166662,#166663,#166664,
#166665,#166666,#166667,#166668,#166669,#166670,#166671,#166672,#166673,
#166674,#166675,#166676,#166677,#166678,#166679,#166680,#166681,#166682,
#166683,#166684,#166685,#166686,#166687,#166688,#166689,#166690,#166691,
#166692,#166693,#166694,#166695,#166696,#166697,#166698,#166699,#166700,
#166701,#166702,#166703,#166704,#166705,#166706,#166707,#166708,#166709,
#166710,#166711,#166712,#166713,#166714,#166715,#166716,#166717,#166718,
#166719,#166720,#166721,#166722,#166723,#166724,#166725,#166726,#166727,
#166728,#166729,#166730,#166731,#166732,#166733,#166734,#166735,#166736,
#166737,#166738,#166739,#166740,#166741,#166742,#166743,#166744,#166745,
#166746,#166747,#166748,#166749,#166750,#166751,#166752,#166753,#166754,
#166755,#166756,#166757,#166758,#166759,#166760,#166761,#166762,#166763,
#166764,#166765,#166766,#166767,#166768,#166769,#166770,#166771,#166772,
#166773,#166774,#166775,#166776,#166777,#166778,#166779,#166780,#166781,
#166782,#166783,#166784,#166785,#166786,#166787,#166788,#166789,#166790,
#166791,#166792,#166793,#166794,#166795,#166796,#166797,#166798,#166799,
#166800,#166801,#166802,#166803,#166804,#166805,#166806,#166807,#166808,
#166809,#166810,#166811,#166812,#166813,#166814,#166815,#166816,#166817,
#166818,#166819,#166820,#166821,#166822,#166823,#166824,#166825,#166826,
#166827,#166828,#166829,#166830,#166831,#166832,#166833,#166834,#166835,
#166836,#166837,#166838,#166839,#166840,#166841,#166842,#166843,#166844,
#166845,#166846,#166847,#166848,#166849,#166850,#166851,#166852,#166853,
#166854,#166855,#166856,#166857,#166858,#166859,#166860,#166861,#166862,
#166863,#166864,#166865,#166866,#166867,#166868,#166869,#166870,#166871,
#166872,#166873,#166874,#166875,#166876,#166877,#166878,#166879,#166880,
#166881,#166882,#166883,#166884,#166885,#166886,#166887,#166888,#166889,
#166890,#166891,#166892),.UNSPECIFIED.,.F.,.F.,(4,3,3,3,3,3,3,3,3,3,3,3,
3,3,3,3,3,3,3,3,3,3,3,3,3,3,3,3,3,3,3,3,3,3,3,3,3,3,3,3,3,3,3,3,3,3,3,3,
3,3,3,3,3,3,3,3,3,3,3,3,3,3,3,3,3,3,3,3,3,3,3,3,3,3,3,3,3,3,3,3,3,3,3,3,
3,3,3,3,3,3,3,3,3,3,3,3,3,3,3,3,3,3,3,3,3,3,3,4),(0.143172102,0.15412844,
0.165137615,0.176146789,0.187155963,0.198165138,0.209174312,0.220183486,
0.231192661,0.242201835,0.253211009,0.264220183,0.275229358,0.286238532,
0.299082569,0.310091743,0.321100917,0.332110092,0.343119266,0.35412844,
0.365137615,0.376146789,0.387155963,0.398165138,0.40733945,0.416513761,
0.425688073,0.436697248,0.44587156,0.455045872,0.464220183,0.473394495,
0.482568807,0.495412844,0.504587156,0.513761468,0.52293578,0.532110092,
0.539449541,0.546788991,0.55412844,0.56146789,0.568807339,0.576146789,0.583486239,
0.590825688,0.598165138,0.60733945,0.614678899,0.622018349,0.631192661,
0.63853211,0.64587156,0.653211009,0.660550459,0.669724771,0.678899083,0.686238532,
0.693577982,0.702752294,0.710091743,0.717431193,0.724770642,0.732110092,
0.741284404,0.748623853,0.755963303,0.763302752,0.770642202,0.777981651,
0.785321101,0.79266055,0.8,0.80733945,0.812844037,0.818348624,0.823853211,
0.829357798,0.834862385,0.840366972,0.84587156,0.851376147,0.856880734,
0.862385321,0.869724771,0.875229358,0.880733945,0.886238532,0.891743119,
0.897247706,0.902752294,0.908256881,0.913761468,0.919266055,0.924770642,
0.932110092,0.937614679,0.943119266,0.948623853,0.95412844,0.959633028,
0.965137615,0.970642202,0.976146789,0.981651376,0.987155963,0.99266055,
1.),.UNSPECIFIED.);
#24334=B_SPLINE_CURVE_WITH_KNOTS('',3,(#166893,#166894,#166895,#166896,
#166897,#166898,#166899,#166900,#166901,#166902,#166903,#166904,#166905,
#166906,#166907,#166908,#166909,#166910,#166911,#166912,#166913,#166914,
#166915,#166916,#166917,#166918,#166919,#166920,#166921,#166922,#166923,
#166924,#166925,#166926,#166927,#166928,#166929,#166930,#166931,#166932,
#166933,#166934,#166935,#166936,#166937,#166938,#166939,#166940,#166941,
#166942,#166943,#166944,#166945,#166946,#166947,#166948,#166949,#166950,
#166951,#166952,#166953,#166954,#166955,#166956,#166957,#166958,#166959,
#166960,#166961,#166962,#166963,#166964,#166965,#166966,#166967,#166968,
#166969,#166970,#166971,#166972,#166973,#166974,#166975,#166976,#166977,
#166978,#166979,#166980,#166981,#166982,#166983,#166984,#166985,#166986,
#166987,#166988,#166989,#166990,#166991,#166992,#166993,#166994,#166995,
#166996,#166997,#166998,#166999,#167000,#167001,#167002,#167003,#167004,
#167005,#167006,#167007,#167008,#167009,#167010,#167011,#167012,#167013,
#167014,#167015,#167016,#167017,#167018,#167019,#167020,#167021,#167022,
#167023,#167024,#167025,#167026,#167027,#167028,#167029,#167030,#167031,
#167032,#167033,#167034,#167035,#167036,#167037,#167038,#167039,#167040,
#167041,#167042,#167043,#167044,#167045,#167046,#167047,#167048,#167049,
#167050,#167051,#167052,#167053,#167054,#167055,#167056,#167057,#167058,
#167059,#167060,#167061,#167062,#167063,#167064,#167065,#167066,#167067,
#167068,#167069,#167070,#167071,#167072,#167073,#167074,#167075,#167076,
#167077,#167078,#167079,#167080,#167081,#167082,#167083,#167084,#167085,
#167086,#167087,#167088,#167089,#167090,#167091,#167092,#167093,#167094,
#167095,#167096,#167097,#167098,#167099,#167100,#167101,#167102,#167103,
#167104,#167105,#167106,#167107,#167108,#167109,#167110,#167111,#167112,
#167113,#167114,#167115,#167116,#167117,#167118,#167119,#167120,#167121,
#167122,#167123,#167124,#167125,#167126,#167127,#167128,#167129,#167130,
#167131,#167132,#167133,#167134,#167135,#167136,#167137,#167138,#167139,
#167140,#167141,#167142,#167143,#167144,#167145,#167146,#167147,#167148,
#167149,#167150,#167151,#167152,#167153,#167154,#167155,#167156,#167157,
#167158,#167159,#167160,#167161,#167162,#167163,#167164,#167165,#167166,
#167167,#167168,#167169,#167170,#167171,#167172,#167173,#167174,#167175,
#167176,#167177,#167178,#167179,#167180,#167181,#167182,#167183,#167184,
#167185,#167186,#167187,#167188,#167189,#167190,#167191,#167192,#167193,
#167194,#167195,#167196,#167197,#167198,#167199,#167200,#167201,#167202,
#167203,#167204,#167205,#167206,#167207,#167208,#167209,#167210,#167211,
#167212,#167213,#167214),.UNSPECIFIED.,.F.,.F.,(4,3,3,3,3,3,3,3,3,3,3,3,
3,3,3,3,3,3,3,3,3,3,3,3,3,3,3,3,3,3,3,3,3,3,3,3,3,3,3,3,3,3,3,3,3,3,3,3,
3,3,3,3,3,3,3,3,3,3,3,3,3,3,3,3,3,3,3,3,3,3,3,3,3,3,3,3,3,3,3,3,3,3,3,3,
3,3,3,3,3,3,3,3,3,3,3,3,3,3,3,3,3,3,3,3,3,3,3,4),(0.143172102,0.15412844,
0.165137615,0.176146789,0.187155963,0.198165138,0.209174312,0.220183486,
0.231192661,0.242201835,0.253211009,0.264220183,0.275229358,0.286238532,
0.299082569,0.310091743,0.321100917,0.332110092,0.343119266,0.35412844,
0.365137615,0.376146789,0.387155963,0.396330275,0.405504587,0.414678899,
0.423853211,0.433027523,0.442201835,0.451376147,0.460550459,0.469724771,
0.478899083,0.488073394,0.499082569,0.508256881,0.517431193,0.526605505,
0.533944954,0.541284404,0.550458716,0.557798165,0.565137615,0.572477064,
0.579816514,0.587155963,0.594495413,0.601834862,0.609174312,0.616513761,
0.623853211,0.631192661,0.63853211,0.64587156,0.653211009,0.660550459,0.667889908,
0.67706422,0.68440367,0.691743119,0.700917431,0.710091743,0.717431193,0.724770642,
0.732110092,0.739449541,0.746788991,0.75412844,0.76146789,0.770642202,0.777981651,
0.785321101,0.794495413,0.801834862,0.809174312,0.814678899,0.820183486,
0.825688073,0.831192661,0.836697248,0.842201835,0.847706422,0.853211009,
0.858715596,0.866055046,0.871559633,0.87706422,0.882568807,0.888073394,
0.893577982,0.900917431,0.906422018,0.911926606,0.919266055,0.924770642,
0.930275229,0.935779817,0.941284404,0.946788991,0.952293578,0.959633028,
0.965137615,0.970642202,0.976146789,0.981651376,0.987155963,0.994495413,
1.),.UNSPECIFIED.);
#24335=B_SPLINE_CURVE_WITH_KNOTS('',5,(#168174,#168175,#168176,#168177,
#168178,#168179,#168180,#168181,#168182,#168183,#168184,#168185,#168186,
#168187,#168188,#168189,#168190,#168191,#168192,#168193,#168194,#168195,
#168196,#168197,#168198,#168199,#168200,#168201,#168202,#168203,#168204,
#168205,#168206,#168207,#168208,#168209,#168210,#168211,#168212,#168213,
#168214,#168215,#168216,#168217,#168218,#168219,#168220,#168221,#168222,
#168223,#168224,#168225,#168226,#168227,#168228,#168229,#168230,#168231,
#168232,#168233,#168234,#168235,#168236,#168237,#168238,#168239,#168240,
#168241,#168242,#168243,#168244,#168245,#168246,#168247,#168248,#168249,
#168250,#168251,#168252,#168253,#168254,#168255,#168256,#168257,#168258,
#168259,#168260,#168261,#168262,#168263,#168264,#168265,#168266,#168267,
#168268,#168269,#168270,#168271,#168272,#168273,#168274,#168275,#168276,
#168277,#168278,#168279,#168280,#168281,#168282,#168283,#168284,#168285,
#168286,#168287,#168288,#168289,#168290,#168291,#168292,#168293,#168294,
#168295,#168296,#168297,#168298,#168299,#168300,#168301,#168302,#168303,
#168304,#168305,#168306,#168307,#168308,#168309,#168310,#168311,#168312,
#168313,#168314,#168315,#168316,#168317,#168318,#168319,#168320,#168321,
#168322,#168323,#168324,#168325,#168326,#168327,#168328,#168329,#168330,
#168331,#168332,#168333,#168334,#168335,#168336,#168337,#168338,#168339,
#168340,#168341,#168342,#168343,#168344,#168345,#168346,#168347,#168348,
#168349,#168350,#168351,#168352,#168353,#168354,#168355,#168356,#168357,
#168358,#168359,#168360,#168361,#168362,#168363,#168364,#168365,#168366,
#168367,#168368,#168369,#168370,#168371,#168372,#168373,#168374,#168375,
#168376,#168377,#168378,#168379,#168380,#168381,#168382,#168383,#168384,
#168385,#168386,#168387,#168388,#168389,#168390,#168391,#168392,#168393,
#168394,#168395,#168396,#168397,#168398,#168399,#168400,#168401,#168402,
#168403,#168404,#168405,#168406,#168407,#168408,#168409,#168410,#168411,
#168412,#168413,#168414,#168415,#168416,#168417,#168418,#168419,#168420,
#168421,#168422,#168423,#168424,#168425,#168426,#168427,#168428,#168429,
#168430,#168431,#168432,#168433,#168434,#168435,#168436,#168437,#168438,
#168439,#168440,#168441,#168442,#168443,#168444,#168445,#168446,#168447,
#168448,#168449,#168450,#168451,#168452,#168453,#168454,#168455,#168456,
#168457,#168458,#168459,#168460,#168461,#168462,#168463,#168464,#168465,
#168466,#168467,#168468,#168469,#168470,#168471,#168472,#168473,#168474,
#168475,#168476,#168477,#168478,#168479,#168480,#168481,#168482,#168483,
#168484,#168485,#168486,#168487,#168488,#168489,#168490,#168491,#168492,
#168493,#168494,#168495,#168496,#168497,#168498,#168499,#168500,#168501,
#168502,#168503,#168504,#168505,#168506,#168507,#168508,#168509,#168510,
#168511,#168512,#168513,#168514,#168515,#168516,#168517,#168518,#168519,
#168520,#168521,#168522,#168523,#168524,#168525,#168526,#168527,#168528,
#168529,#168530,#168531,#168532,#168533,#168534,#168535,#168536,#168537,
#168538,#168539,#168540,#168541,#168542,#168543,#168544,#168545,#168546,
#168547,#168548,#168549,#168550,#168551,#168552,#168553,#168554,#168555,
#168556,#168557,#168558,#168559,#168560,#168561,#168562,#168563,#168564,
#168565,#168566,#168567,#168568,#168569,#168570,#168571,#168572,#168573,
#168574,#168575,#168576,#168577,#168578,#168579,#168580,#168581,#168582,
#168583,#168584,#168585,#168586,#168587,#168588,#168589,#168590,#168591,
#168592,#168593,#168594,#168595,#168596,#168597,#168598,#168599,#168600,
#168601,#168602,#168603,#168604,#168605,#168606,#168607,#168608,#168609,
#168610,#168611,#168612,#168613,#168614,#168615,#168616,#168617,#168618,
#168619,#168620,#168621,#168622,#168623,#168624,#168625,#168626,#168627,
#168628,#168629,#168630,#168631,#168632,#168633,#168634,#168635,#168636,
#168637,#168638,#168639,#168640,#168641,#168642,#168643,#168644,#168645),
 .UNSPECIFIED.,.F.,.F.,(6,1,1,1,1,1,1,1,1,1,1,1,1,1,1,1,1,1,1,1,1,1,1,1,
1,1,1,1,1,1,1,1,1,1,1,1,1,1,1,1,1,1,1,1,1,1,1,1,1,1,1,1,1,1,1,1,1,1,1,1,
1,1,1,1,1,1,1,1,1,1,1,1,1,1,1,1,1,1,1,1,1,1,1,1,1,1,1,1,1,1,1,1,1,1,1,1,
1,1,1,1,1,1,1,1,1,1,1,1,1,1,1,1,1,1,1,1,1,1,1,1,1,1,1,1,1,1,1,1,1,1,1,1,
1,1,1,1,1,1,1,1,1,1,1,1,1,1,1,1,1,1,1,1,1,1,1,1,1,1,1,1,1,1,1,1,1,1,1,1,
1,1,1,1,1,1,1,1,1,1,1,1,1,1,1,1,1,1,1,1,1,1,1,1,1,1,1,1,1,1,1,1,1,1,1,1,
1,1,1,1,1,1,1,1,1,1,1,1,1,1,1,1,1,1,1,1,1,1,1,1,1,1,1,1,1,1,1,1,1,1,1,1,
1,1,1,1,1,1,1,1,1,1,1,1,1,1,1,1,1,1,1,1,1,1,1,1,1,1,1,1,1,1,1,1,1,1,1,1,
1,1,1,1,1,1,1,1,1,1,1,1,1,1,1,1,1,1,1,1,1,1,1,1,1,1,1,1,1,1,1,1,1,1,1,1,
1,1,1,1,1,1,1,1,1,1,1,1,1,1,1,1,1,1,1,1,1,1,1,1,1,1,1,1,1,1,1,1,1,1,1,1,
1,1,1,1,1,1,1,1,1,1,1,1,1,1,1,1,1,1,1,1,1,1,1,1,1,1,1,1,1,1,1,1,1,1,1,1,
1,1,1,1,1,1,1,1,1,1,1,1,1,1,1,1,1,1,1,1,1,1,1,1,1,1,1,1,1,1,1,1,1,1,1,1,
1,1,1,1,1,1,1,1,1,1,1,1,1,1,1,1,1,1,1,1,1,1,1,1,1,1,1,1,1,1,1,1,1,1,1,1,
1,1,1,1,1,1,1,1,1,1,1,6),(0.143172102,0.144954128,0.146788991,0.148623853,
0.150458716,0.152293578,0.15412844,0.155963303,0.157798165,0.159633028,
0.16146789,0.163302752,0.165137615,0.166972477,0.168807339,0.170642202,
0.172477064,0.174311927,0.176146789,0.177981651,0.179816514,0.181651376,
0.183486239,0.185321101,0.187155963,0.188990826,0.190825688,0.19266055,
0.194495413,0.196330275,0.198165138,0.2,0.201834862,0.203669725,0.205504587,
0.20733945,0.209174312,0.211009174,0.212844037,0.214678899,0.216513761,
0.218348624,0.220183486,0.222018349,0.223853211,0.225688073,0.227522936,
0.229357798,0.231192661,0.233027523,0.234862385,0.236697248,0.23853211,
0.240366972,0.242201835,0.244036697,0.24587156,0.247706422,0.249541284,
0.251376147,0.253211009,0.255045872,0.256880734,0.258715596,0.260550459,
0.262385321,0.264220183,0.266055046,0.267889908,0.269724771,0.271559633,
0.273394495,0.275229358,0.27706422,0.278899083,0.280733945,0.282568807,
0.28440367,0.286238532,0.288073394,0.289908257,0.291743119,0.293577982,
0.295412844,0.297247706,0.299082569,0.300917431,0.302752294,0.304587156,
0.306422018,0.308256881,0.310091743,0.311926606,0.313761468,0.31559633,
0.317431193,0.319266055,0.321100917,0.32293578,0.324770642,0.326605505,
0.328440367,0.330275229,0.332110092,0.333944954,0.335779817,0.337614679,
0.339449541,0.341284404,0.343119266,0.344954128,0.346788991,0.348623853,
0.350458716,0.352293578,0.35412844,0.355963303,0.357798165,0.359633028,
0.36146789,0.363302752,0.365137615,0.366972477,0.368807339,0.370642202,
0.372477064,0.374311927,0.376146789,0.377981651,0.379816514,0.381651376,
0.383486239,0.385321101,0.387155963,0.388990826,0.390825688,0.39266055,
0.394495413,0.396330275,0.398165138,0.4,0.401834862,0.403669725,0.405504587,
0.40733945,0.409174312,0.411009174,0.412844037,0.414678899,0.416513761,
0.418348624,0.420183486,0.422018349,0.423853211,0.425688073,0.427522936,
0.429357798,0.431192661,0.433027523,0.434862385,0.436697248,0.43853211,
0.440366972,0.442201835,0.444036697,0.44587156,0.447706422,0.449541284,
0.451376147,0.453211009,0.455045872,0.456880734,0.458715596,0.460550459,
0.462385321,0.464220183,0.466055046,0.467889908,0.469724771,0.471559633,
0.473394495,0.475229358,0.47706422,0.478899083,0.480733945,0.482568807,
0.48440367,0.486238532,0.488073394,0.489908257,0.491743119,0.493577982,
0.495412844,0.497247706,0.499082569,0.500917431,0.502752294,0.504587156,
0.506422018,0.508256881,0.510091743,0.511926606,0.513761468,0.51559633,
0.517431193,0.519266055,0.521100917,0.52293578,0.524770642,0.526605505,
0.528440367,0.530275229,0.532110092,0.533944954,0.535779817,0.537614679,
0.539449541,0.541284404,0.543119266,0.544954128,0.546788991,0.548623853,
0.550458716,0.552293578,0.55412844,0.555963303,0.557798165,0.559633028,
0.56146789,0.563302752,0.565137615,0.566972477,0.568807339,0.570642202,
0.572477064,0.574311927,0.576146789,0.577981651,0.579816514,0.581651376,
0.583486239,0.585321101,0.587155963,0.588990826,0.590825688,0.59266055,
0.594495413,0.596330275,0.598165138,0.6,0.601834862,0.603669725,0.605504587,
0.60733945,0.609174312,0.611009174,0.612844037,0.614678899,0.616513761,
0.618348624,0.620183486,0.622018349,0.623853211,0.625688073,0.627522936,
0.629357798,0.631192661,0.633027523,0.634862385,0.636697248,0.63853211,
0.640366972,0.642201835,0.644036697,0.64587156,0.647706422,0.649541284,
0.651376147,0.653211009,0.655045872,0.656880734,0.658715596,0.660550459,
0.662385321,0.664220183,0.666055046,0.667889908,0.669724771,0.671559633,
0.673394495,0.675229358,0.67706422,0.678899083,0.680733945,0.682568807,
0.68440367,0.686238532,0.688073394,0.689908257,0.691743119,0.693577982,
0.695412844,0.697247706,0.699082569,0.700917431,0.702752294,0.704587156,
0.706422018,0.708256881,0.710091743,0.711926606,0.713761468,0.71559633,
0.717431193,0.719266055,0.721100917,0.72293578,0.724770642,0.726605505,
0.728440367,0.730275229,0.732110092,0.733944954,0.735779817,0.737614679,
0.739449541,0.741284404,0.743119266,0.744954128,0.746788991,0.748623853,
0.750458716,0.752293578,0.75412844,0.755963303,0.757798165,0.759633028,
0.76146789,0.763302752,0.765137615,0.766972477,0.768807339,0.770642202,
0.772477064,0.774311927,0.776146789,0.777981651,0.779816514,0.781651376,
0.783486239,0.785321101,0.787155963,0.788990826,0.790825688,0.79266055,
0.794495413,0.796330275,0.798165138,0.8,0.801834862,0.803669725,0.805504587,
0.80733945,0.809174312,0.811009174,0.812844037,0.814678899,0.816513761,
0.818348624,0.820183486,0.822018349,0.823853211,0.825688073,0.827522936,
0.829357798,0.831192661,0.833027523,0.834862385,0.836697248,0.83853211,
0.840366972,0.842201835,0.844036697,0.84587156,0.847706422,0.849541284,
0.851376147,0.853211009,0.855045872,0.856880734,0.858715596,0.860550459,
0.862385321,0.864220183,0.866055046,0.867889908,0.869724771,0.871559633,
0.873394495,0.875229358,0.87706422,0.878899083,0.880733945,0.882568807,
0.88440367,0.886238532,0.888073394,0.889908257,0.891743119,0.893577982,
0.895412844,0.897247706,0.899082569,0.900917431,0.902752294,0.904587156,
0.906422018,0.908256881,0.910091743,0.911926606,0.913761468,0.91559633,
0.917431193,0.919266055,0.921100917,0.92293578,0.924770642,0.926605505,
0.928440367,0.930275229,0.932110092,0.933944954,0.935779817,0.937614679,
0.939449541,0.941284404,0.943119266,0.944954128,0.946788991,0.948623853,
0.950458716,0.952293578,0.95412844,0.955963303,0.957798165,0.959633028,
0.96146789,0.963302752,0.965137615,0.966972477,0.968807339,0.970642202,
0.972477064,0.974311927,0.976146789,0.977981651,0.979816514,0.981651376,
0.983486239,0.985321101,0.987155963,0.988990826,0.990825688,0.99266055,
0.994495413,0.996330275,0.998165138,1.),.UNSPECIFIED.);
#24336=B_SPLINE_CURVE_WITH_KNOTS('',5,(#168646,#168647,#168648,#168649,
#168650,#168651,#168652,#168653,#168654,#168655,#168656,#168657,#168658,
#168659,#168660,#168661,#168662,#168663,#168664,#168665,#168666,#168667,
#168668,#168669,#168670,#168671,#168672,#168673,#168674,#168675,#168676,
#168677,#168678,#168679,#168680,#168681,#168682,#168683,#168684,#168685,
#168686,#168687,#168688,#168689,#168690,#168691,#168692,#168693,#168694,
#168695,#168696,#168697,#168698,#168699,#168700,#168701,#168702,#168703,
#168704,#168705,#168706,#168707,#168708,#168709,#168710,#168711,#168712,
#168713,#168714,#168715,#168716,#168717,#168718,#168719,#168720,#168721,
#168722,#168723,#168724,#168725,#168726,#168727,#168728,#168729,#168730,
#168731,#168732,#168733,#168734,#168735,#168736,#168737,#168738,#168739,
#168740,#168741,#168742,#168743,#168744,#168745,#168746,#168747,#168748,
#168749,#168750,#168751,#168752,#168753,#168754,#168755,#168756,#168757,
#168758,#168759,#168760,#168761,#168762,#168763,#168764,#168765,#168766,
#168767,#168768,#168769,#168770,#168771,#168772,#168773,#168774,#168775,
#168776,#168777,#168778,#168779,#168780,#168781,#168782,#168783,#168784,
#168785,#168786,#168787,#168788,#168789,#168790,#168791,#168792,#168793,
#168794,#168795,#168796,#168797,#168798,#168799,#168800,#168801,#168802,
#168803,#168804,#168805,#168806,#168807,#168808,#168809,#168810,#168811,
#168812,#168813,#168814,#168815,#168816,#168817,#168818,#168819,#168820,
#168821,#168822,#168823,#168824,#168825,#168826,#168827,#168828,#168829,
#168830,#168831,#168832,#168833,#168834,#168835,#168836,#168837,#168838,
#168839,#168840,#168841,#168842,#168843,#168844,#168845,#168846,#168847,
#168848,#168849,#168850,#168851,#168852,#168853,#168854,#168855,#168856,
#168857,#168858,#168859,#168860,#168861,#168862,#168863,#168864,#168865,
#168866,#168867,#168868,#168869,#168870,#168871,#168872,#168873,#168874,
#168875,#168876,#168877,#168878,#168879,#168880,#168881,#168882,#168883,
#168884,#168885,#168886,#168887,#168888,#168889,#168890,#168891,#168892,
#168893,#168894,#168895,#168896,#168897,#168898,#168899,#168900,#168901,
#168902,#168903,#168904,#168905,#168906,#168907,#168908,#168909,#168910,
#168911,#168912,#168913,#168914,#168915,#168916,#168917,#168918,#168919,
#168920,#168921,#168922,#168923,#168924,#168925,#168926,#168927,#168928,
#168929,#168930,#168931,#168932,#168933,#168934,#168935,#168936,#168937,
#168938,#168939,#168940,#168941,#168942,#168943,#168944,#168945,#168946,
#168947,#168948,#168949,#168950,#168951,#168952,#168953,#168954,#168955,
#168956,#168957,#168958,#168959,#168960,#168961,#168962,#168963,#168964,
#168965,#168966,#168967,#168968,#168969,#168970,#168971,#168972,#168973,
#168974,#168975,#168976,#168977,#168978,#168979,#168980,#168981,#168982,
#168983,#168984,#168985,#168986,#168987,#168988,#168989,#168990,#168991,
#168992,#168993,#168994,#168995,#168996,#168997,#168998,#168999,#169000,
#169001,#169002,#169003,#169004,#169005,#169006,#169007,#169008,#169009,
#169010,#169011,#169012,#169013,#169014,#169015,#169016,#169017,#169018,
#169019,#169020,#169021,#169022,#169023,#169024,#169025,#169026,#169027,
#169028,#169029,#169030,#169031,#169032,#169033,#169034,#169035,#169036,
#169037,#169038,#169039,#169040,#169041,#169042,#169043,#169044,#169045,
#169046,#169047,#169048,#169049,#169050,#169051,#169052,#169053,#169054,
#169055,#169056,#169057,#169058,#169059,#169060,#169061,#169062,#169063,
#169064,#169065,#169066,#169067,#169068,#169069,#169070,#169071,#169072,
#169073,#169074,#169075,#169076,#169077,#169078,#169079,#169080,#169081,
#169082,#169083,#169084,#169085,#169086,#169087,#169088,#169089,#169090,
#169091,#169092,#169093,#169094,#169095,#169096,#169097,#169098,#169099,
#169100,#169101,#169102,#169103,#169104,#169105,#169106,#169107,#169108,
#169109,#169110,#169111,#169112,#169113,#169114,#169115,#169116,#169117),
 .UNSPECIFIED.,.F.,.F.,(6,1,1,1,1,1,1,1,1,1,1,1,1,1,1,1,1,1,1,1,1,1,1,1,
1,1,1,1,1,1,1,1,1,1,1,1,1,1,1,1,1,1,1,1,1,1,1,1,1,1,1,1,1,1,1,1,1,1,1,1,
1,1,1,1,1,1,1,1,1,1,1,1,1,1,1,1,1,1,1,1,1,1,1,1,1,1,1,1,1,1,1,1,1,1,1,1,
1,1,1,1,1,1,1,1,1,1,1,1,1,1,1,1,1,1,1,1,1,1,1,1,1,1,1,1,1,1,1,1,1,1,1,1,
1,1,1,1,1,1,1,1,1,1,1,1,1,1,1,1,1,1,1,1,1,1,1,1,1,1,1,1,1,1,1,1,1,1,1,1,
1,1,1,1,1,1,1,1,1,1,1,1,1,1,1,1,1,1,1,1,1,1,1,1,1,1,1,1,1,1,1,1,1,1,1,1,
1,1,1,1,1,1,1,1,1,1,1,1,1,1,1,1,1,1,1,1,1,1,1,1,1,1,1,1,1,1,1,1,1,1,1,1,
1,1,1,1,1,1,1,1,1,1,1,1,1,1,1,1,1,1,1,1,1,1,1,1,1,1,1,1,1,1,1,1,1,1,1,1,
1,1,1,1,1,1,1,1,1,1,1,1,1,1,1,1,1,1,1,1,1,1,1,1,1,1,1,1,1,1,1,1,1,1,1,1,
1,1,1,1,1,1,1,1,1,1,1,1,1,1,1,1,1,1,1,1,1,1,1,1,1,1,1,1,1,1,1,1,1,1,1,1,
1,1,1,1,1,1,1,1,1,1,1,1,1,1,1,1,1,1,1,1,1,1,1,1,1,1,1,1,1,1,1,1,1,1,1,1,
1,1,1,1,1,1,1,1,1,1,1,1,1,1,1,1,1,1,1,1,1,1,1,1,1,1,1,1,1,1,1,1,1,1,1,1,
1,1,1,1,1,1,1,1,1,1,1,1,1,1,1,1,1,1,1,1,1,1,1,1,1,1,1,1,1,1,1,1,1,1,1,1,
1,1,1,1,1,1,1,1,1,1,1,6),(0.143172102,0.144954128,0.146788991,0.148623853,
0.150458716,0.152293578,0.15412844,0.155963303,0.157798165,0.159633028,
0.16146789,0.163302752,0.165137615,0.166972477,0.168807339,0.170642202,
0.172477064,0.174311927,0.176146789,0.177981651,0.179816514,0.181651376,
0.183486239,0.185321101,0.187155963,0.188990826,0.190825688,0.19266055,
0.194495413,0.196330275,0.198165138,0.2,0.201834862,0.203669725,0.205504587,
0.20733945,0.209174312,0.211009174,0.212844037,0.214678899,0.216513761,
0.218348624,0.220183486,0.222018349,0.223853211,0.225688073,0.227522936,
0.229357798,0.231192661,0.233027523,0.234862385,0.236697248,0.23853211,
0.240366972,0.242201835,0.244036697,0.24587156,0.247706422,0.249541284,
0.251376147,0.253211009,0.255045872,0.256880734,0.258715596,0.260550459,
0.262385321,0.264220183,0.266055046,0.267889908,0.269724771,0.271559633,
0.273394495,0.275229358,0.27706422,0.278899083,0.280733945,0.282568807,
0.28440367,0.286238532,0.288073394,0.289908257,0.291743119,0.293577982,
0.295412844,0.297247706,0.299082569,0.300917431,0.302752294,0.304587156,
0.306422018,0.308256881,0.310091743,0.311926606,0.313761468,0.31559633,
0.317431193,0.319266055,0.321100917,0.32293578,0.324770642,0.326605505,
0.328440367,0.330275229,0.332110092,0.333944954,0.335779817,0.337614679,
0.339449541,0.341284404,0.343119266,0.344954128,0.346788991,0.348623853,
0.350458716,0.352293578,0.35412844,0.355963303,0.357798165,0.359633028,
0.36146789,0.363302752,0.365137615,0.366972477,0.368807339,0.370642202,
0.372477064,0.374311927,0.376146789,0.377981651,0.379816514,0.381651376,
0.383486239,0.385321101,0.387155963,0.388990826,0.390825688,0.39266055,
0.394495413,0.396330275,0.398165138,0.4,0.401834862,0.403669725,0.405504587,
0.40733945,0.409174312,0.411009174,0.412844037,0.414678899,0.416513761,
0.418348624,0.420183486,0.422018349,0.423853211,0.425688073,0.427522936,
0.429357798,0.431192661,0.433027523,0.434862385,0.436697248,0.43853211,
0.440366972,0.442201835,0.444036697,0.44587156,0.447706422,0.449541284,
0.451376147,0.453211009,0.455045872,0.456880734,0.458715596,0.460550459,
0.462385321,0.464220183,0.466055046,0.467889908,0.469724771,0.471559633,
0.473394495,0.475229358,0.47706422,0.478899083,0.480733945,0.482568807,
0.48440367,0.486238532,0.488073394,0.489908257,0.491743119,0.493577982,
0.495412844,0.497247706,0.499082569,0.500917431,0.502752294,0.504587156,
0.506422018,0.508256881,0.510091743,0.511926606,0.513761468,0.51559633,
0.517431193,0.519266055,0.521100917,0.52293578,0.524770642,0.526605505,
0.528440367,0.530275229,0.532110092,0.533944954,0.535779817,0.537614679,
0.539449541,0.541284404,0.543119266,0.544954128,0.546788991,0.548623853,
0.550458716,0.552293578,0.55412844,0.555963303,0.557798165,0.559633028,
0.56146789,0.563302752,0.565137615,0.566972477,0.568807339,0.570642202,
0.572477064,0.574311927,0.576146789,0.577981651,0.579816514,0.581651376,
0.583486239,0.585321101,0.587155963,0.588990826,0.590825688,0.59266055,
0.594495413,0.596330275,0.598165138,0.6,0.601834862,0.603669725,0.605504587,
0.60733945,0.609174312,0.611009174,0.612844037,0.614678899,0.616513761,
0.618348624,0.620183486,0.622018349,0.623853211,0.625688073,0.627522936,
0.629357798,0.631192661,0.633027523,0.634862385,0.636697248,0.63853211,
0.640366972,0.642201835,0.644036697,0.64587156,0.647706422,0.649541284,
0.651376147,0.653211009,0.655045872,0.656880734,0.658715596,0.660550459,
0.662385321,0.664220183,0.666055046,0.667889908,0.669724771,0.671559633,
0.673394495,0.675229358,0.67706422,0.678899083,0.680733945,0.682568807,
0.68440367,0.686238532,0.688073394,0.689908257,0.691743119,0.693577982,
0.695412844,0.697247706,0.699082569,0.700917431,0.702752294,0.704587156,
0.706422018,0.708256881,0.710091743,0.711926606,0.713761468,0.71559633,
0.717431193,0.719266055,0.721100917,0.72293578,0.724770642,0.726605505,
0.728440367,0.730275229,0.732110092,0.733944954,0.735779817,0.737614679,
0.739449541,0.741284404,0.743119266,0.744954128,0.746788991,0.748623853,
0.750458716,0.752293578,0.75412844,0.755963303,0.757798165,0.759633028,
0.76146789,0.763302752,0.765137615,0.766972477,0.768807339,0.770642202,
0.772477064,0.774311927,0.776146789,0.777981651,0.779816514,0.781651376,
0.783486239,0.785321101,0.787155963,0.788990826,0.790825688,0.79266055,
0.794495413,0.796330275,0.798165138,0.8,0.801834862,0.803669725,0.805504587,
0.80733945,0.809174312,0.811009174,0.812844037,0.814678899,0.816513761,
0.818348624,0.820183486,0.822018349,0.823853211,0.825688073,0.827522936,
0.829357798,0.831192661,0.833027523,0.834862385,0.836697248,0.83853211,
0.840366972,0.842201835,0.844036697,0.84587156,0.847706422,0.849541284,
0.851376147,0.853211009,0.855045872,0.856880734,0.858715596,0.860550459,
0.862385321,0.864220183,0.866055046,0.867889908,0.869724771,0.871559633,
0.873394495,0.875229358,0.87706422,0.878899083,0.880733945,0.882568807,
0.88440367,0.886238532,0.888073394,0.889908257,0.891743119,0.893577982,
0.895412844,0.897247706,0.899082569,0.900917431,0.902752294,0.904587156,
0.906422018,0.908256881,0.910091743,0.911926606,0.913761468,0.91559633,
0.917431193,0.919266055,0.921100917,0.92293578,0.924770642,0.926605505,
0.928440367,0.930275229,0.932110092,0.933944954,0.935779817,0.937614679,
0.939449541,0.941284404,0.943119266,0.944954128,0.946788991,0.948623853,
0.950458716,0.952293578,0.95412844,0.955963303,0.957798165,0.959633028,
0.96146789,0.963302752,0.965137615,0.966972477,0.968807339,0.970642202,
0.972477064,0.974311927,0.976146789,0.977981651,0.979816514,0.981651376,
0.983486239,0.985321101,0.987155963,0.988990826,0.990825688,0.99266055,
0.994495413,0.996330275,0.998165138,1.),.UNSPECIFIED.);
#24337=B_SPLINE_CURVE_WITH_KNOTS('',5,(#170065,#170066,#170067,#170068,
#170069,#170070,#170071,#170072,#170073,#170074,#170075,#170076,#170077,
#170078,#170079,#170080,#170081,#170082,#170083,#170084,#170085,#170086,
#170087,#170088,#170089,#170090,#170091,#170092,#170093,#170094,#170095,
#170096,#170097,#170098,#170099,#170100,#170101,#170102,#170103,#170104,
#170105,#170106,#170107,#170108,#170109,#170110,#170111,#170112,#170113,
#170114,#170115,#170116,#170117,#170118,#170119,#170120,#170121,#170122,
#170123,#170124,#170125,#170126,#170127,#170128,#170129,#170130,#170131,
#170132,#170133,#170134,#170135,#170136,#170137,#170138,#170139,#170140,
#170141,#170142,#170143,#170144,#170145,#170146,#170147,#170148,#170149,
#170150,#170151,#170152,#170153,#170154,#170155,#170156,#170157,#170158,
#170159,#170160,#170161,#170162,#170163,#170164,#170165,#170166,#170167,
#170168,#170169,#170170,#170171,#170172,#170173,#170174,#170175,#170176,
#170177,#170178,#170179,#170180,#170181,#170182,#170183,#170184,#170185,
#170186,#170187,#170188,#170189,#170190,#170191,#170192,#170193,#170194,
#170195,#170196,#170197,#170198,#170199,#170200,#170201,#170202,#170203,
#170204,#170205,#170206,#170207,#170208,#170209,#170210,#170211,#170212,
#170213,#170214,#170215,#170216,#170217,#170218,#170219,#170220,#170221,
#170222,#170223,#170224,#170225,#170226,#170227,#170228,#170229,#170230,
#170231,#170232,#170233,#170234,#170235,#170236,#170237,#170238,#170239,
#170240,#170241,#170242,#170243,#170244,#170245,#170246,#170247,#170248,
#170249,#170250,#170251,#170252,#170253,#170254,#170255,#170256,#170257,
#170258,#170259,#170260,#170261,#170262,#170263,#170264,#170265,#170266,
#170267,#170268,#170269,#170270,#170271,#170272,#170273,#170274,#170275,
#170276,#170277,#170278,#170279,#170280,#170281,#170282,#170283,#170284,
#170285,#170286,#170287,#170288,#170289,#170290,#170291,#170292,#170293,
#170294,#170295,#170296,#170297,#170298,#170299,#170300,#170301,#170302,
#170303,#170304,#170305,#170306,#170307,#170308,#170309,#170310,#170311,
#170312,#170313,#170314,#170315,#170316,#170317,#170318,#170319,#170320,
#170321,#170322,#170323,#170324,#170325,#170326,#170327,#170328,#170329,
#170330,#170331,#170332,#170333,#170334,#170335,#170336,#170337,#170338,
#170339,#170340,#170341,#170342,#170343,#170344,#170345,#170346,#170347,
#170348,#170349,#170350,#170351,#170352,#170353,#170354,#170355,#170356,
#170357,#170358,#170359,#170360,#170361,#170362,#170363,#170364,#170365,
#170366,#170367,#170368,#170369,#170370,#170371,#170372,#170373,#170374,
#170375,#170376,#170377,#170378,#170379,#170380,#170381,#170382,#170383,
#170384,#170385,#170386,#170387,#170388,#170389,#170390,#170391,#170392,
#170393,#170394,#170395,#170396,#170397,#170398,#170399,#170400,#170401,
#170402,#170403,#170404,#170405,#170406,#170407,#170408,#170409,#170410,
#170411,#170412,#170413,#170414,#170415,#170416,#170417,#170418,#170419,
#170420,#170421,#170422,#170423,#170424,#170425,#170426,#170427,#170428,
#170429,#170430,#170431,#170432,#170433,#170434,#170435,#170436,#170437,
#170438,#170439,#170440,#170441,#170442,#170443,#170444,#170445,#170446,
#170447,#170448,#170449,#170450,#170451,#170452,#170453,#170454,#170455,
#170456,#170457,#170458,#170459,#170460,#170461,#170462,#170463,#170464,
#170465,#170466,#170467,#170468,#170469,#170470,#170471,#170472,#170473,
#170474,#170475,#170476,#170477,#170478,#170479,#170480,#170481,#170482,
#170483,#170484,#170485,#170486,#170487,#170488,#170489,#170490,#170491,
#170492,#170493,#170494,#170495,#170496,#170497,#170498,#170499,#170500,
#170501,#170502,#170503,#170504,#170505,#170506,#170507,#170508,#170509,
#170510,#170511,#170512,#170513,#170514,#170515,#170516,#170517,#170518,
#170519,#170520,#170521,#170522,#170523,#170524,#170525,#170526,#170527,
#170528,#170529,#170530,#170531,#170532,#170533,#170534,#170535,#170536),
 .UNSPECIFIED.,.F.,.F.,(6,1,1,1,1,1,1,1,1,1,1,1,1,1,1,1,1,1,1,1,1,1,1,1,
1,1,1,1,1,1,1,1,1,1,1,1,1,1,1,1,1,1,1,1,1,1,1,1,1,1,1,1,1,1,1,1,1,1,1,1,
1,1,1,1,1,1,1,1,1,1,1,1,1,1,1,1,1,1,1,1,1,1,1,1,1,1,1,1,1,1,1,1,1,1,1,1,
1,1,1,1,1,1,1,1,1,1,1,1,1,1,1,1,1,1,1,1,1,1,1,1,1,1,1,1,1,1,1,1,1,1,1,1,
1,1,1,1,1,1,1,1,1,1,1,1,1,1,1,1,1,1,1,1,1,1,1,1,1,1,1,1,1,1,1,1,1,1,1,1,
1,1,1,1,1,1,1,1,1,1,1,1,1,1,1,1,1,1,1,1,1,1,1,1,1,1,1,1,1,1,1,1,1,1,1,1,
1,1,1,1,1,1,1,1,1,1,1,1,1,1,1,1,1,1,1,1,1,1,1,1,1,1,1,1,1,1,1,1,1,1,1,1,
1,1,1,1,1,1,1,1,1,1,1,1,1,1,1,1,1,1,1,1,1,1,1,1,1,1,1,1,1,1,1,1,1,1,1,1,
1,1,1,1,1,1,1,1,1,1,1,1,1,1,1,1,1,1,1,1,1,1,1,1,1,1,1,1,1,1,1,1,1,1,1,1,
1,1,1,1,1,1,1,1,1,1,1,1,1,1,1,1,1,1,1,1,1,1,1,1,1,1,1,1,1,1,1,1,1,1,1,1,
1,1,1,1,1,1,1,1,1,1,1,1,1,1,1,1,1,1,1,1,1,1,1,1,1,1,1,1,1,1,1,1,1,1,1,1,
1,1,1,1,1,1,1,1,1,1,1,1,1,1,1,1,1,1,1,1,1,1,1,1,1,1,1,1,1,1,1,1,1,1,1,1,
1,1,1,1,1,1,1,1,1,1,1,1,1,1,1,1,1,1,1,1,1,1,1,1,1,1,1,1,1,1,1,1,1,1,1,1,
1,1,1,1,1,1,1,1,1,1,1,6),(-1.,-0.998165138,-0.996330275,-0.994495413,-0.99266055,
-0.990825688,-0.988990826,-0.987155963,-0.985321101,-0.983486239,-0.981651376,
-0.979816514,-0.977981651,-0.976146789,-0.974311927,-0.972477064,-0.970642202,
-0.968807339,-0.966972477,-0.965137615,-0.963302752,-0.96146789,-0.959633028,
-0.957798165,-0.955963303,-0.95412844,-0.952293578,-0.950458716,-0.948623853,
-0.946788991,-0.944954128,-0.943119266,-0.941284404,-0.939449541,-0.937614679,
-0.935779817,-0.933944954,-0.932110092,-0.930275229,-0.928440367,-0.926605505,
-0.924770642,-0.92293578,-0.921100917,-0.919266055,-0.917431193,-0.91559633,
-0.913761468,-0.911926606,-0.910091743,-0.908256881,-0.906422018,-0.904587156,
-0.902752294,-0.900917431,-0.899082569,-0.897247706,-0.895412844,-0.893577982,
-0.891743119,-0.889908257,-0.888073394,-0.886238532,-0.88440367,-0.882568807,
-0.880733945,-0.878899083,-0.87706422,-0.875229358,-0.873394495,-0.871559633,
-0.869724771,-0.867889908,-0.866055046,-0.864220183,-0.862385321,-0.860550459,
-0.858715596,-0.856880734,-0.855045872,-0.853211009,-0.851376147,-0.849541284,
-0.847706422,-0.84587156,-0.844036697,-0.842201835,-0.840366972,-0.83853211,
-0.836697248,-0.834862385,-0.833027523,-0.831192661,-0.829357798,-0.827522936,
-0.825688073,-0.823853211,-0.822018349,-0.820183486,-0.818348624,-0.816513761,
-0.814678899,-0.812844037,-0.811009174,-0.809174312,-0.80733945,-0.805504587,
-0.803669725,-0.801834862,-0.8,-0.798165138,-0.796330275,-0.794495413,-0.79266055,
-0.790825688,-0.788990826,-0.787155963,-0.785321101,-0.783486239,-0.781651376,
-0.779816514,-0.777981651,-0.776146789,-0.774311927,-0.772477064,-0.770642202,
-0.768807339,-0.766972477,-0.765137615,-0.763302752,-0.76146789,-0.759633028,
-0.757798165,-0.755963303,-0.75412844,-0.752293578,-0.750458716,-0.748623853,
-0.746788991,-0.744954128,-0.743119266,-0.741284404,-0.739449541,-0.737614679,
-0.735779817,-0.733944954,-0.732110092,-0.730275229,-0.728440367,-0.726605505,
-0.724770642,-0.72293578,-0.721100917,-0.719266055,-0.717431193,-0.71559633,
-0.713761468,-0.711926606,-0.710091743,-0.708256881,-0.706422018,-0.704587156,
-0.702752294,-0.700917431,-0.699082569,-0.697247706,-0.695412844,-0.693577982,
-0.691743119,-0.689908257,-0.688073394,-0.686238532,-0.68440367,-0.682568807,
-0.680733945,-0.678899083,-0.67706422,-0.675229358,-0.673394495,-0.671559633,
-0.669724771,-0.667889908,-0.666055046,-0.664220183,-0.662385321,-0.660550459,
-0.658715596,-0.656880734,-0.655045872,-0.653211009,-0.651376147,-0.649541284,
-0.647706422,-0.64587156,-0.644036697,-0.642201835,-0.640366972,-0.63853211,
-0.636697248,-0.634862385,-0.633027523,-0.631192661,-0.629357798,-0.627522936,
-0.625688073,-0.623853211,-0.622018349,-0.620183486,-0.618348624,-0.616513761,
-0.614678899,-0.612844037,-0.611009174,-0.609174312,-0.60733945,-0.605504587,
-0.603669725,-0.601834862,-0.6,-0.598165138,-0.596330275,-0.594495413,-0.59266055,
-0.590825688,-0.588990826,-0.587155963,-0.585321101,-0.583486239,-0.581651376,
-0.579816514,-0.577981651,-0.576146789,-0.574311927,-0.572477064,-0.570642202,
-0.568807339,-0.566972477,-0.565137615,-0.563302752,-0.56146789,-0.559633028,
-0.557798165,-0.555963303,-0.55412844,-0.552293578,-0.550458716,-0.548623853,
-0.546788991,-0.544954128,-0.543119266,-0.541284404,-0.539449541,-0.537614679,
-0.535779817,-0.533944954,-0.532110092,-0.530275229,-0.528440367,-0.526605505,
-0.524770642,-0.52293578,-0.521100917,-0.519266055,-0.517431193,-0.51559633,
-0.513761468,-0.511926606,-0.510091743,-0.508256881,-0.506422018,-0.504587156,
-0.502752294,-0.500917431,-0.499082569,-0.497247706,-0.495412844,-0.493577982,
-0.491743119,-0.489908257,-0.488073394,-0.486238532,-0.48440367,-0.482568807,
-0.480733945,-0.478899083,-0.47706422,-0.475229358,-0.473394495,-0.471559633,
-0.469724771,-0.467889908,-0.466055046,-0.464220183,-0.462385321,-0.460550459,
-0.458715596,-0.456880734,-0.455045872,-0.453211009,-0.451376147,-0.449541284,
-0.447706422,-0.44587156,-0.444036697,-0.442201835,-0.440366972,-0.43853211,
-0.436697248,-0.434862385,-0.433027523,-0.431192661,-0.429357798,-0.427522936,
-0.425688073,-0.423853211,-0.422018349,-0.420183486,-0.418348624,-0.416513761,
-0.414678899,-0.412844037,-0.411009174,-0.409174312,-0.40733945,-0.405504587,
-0.403669725,-0.401834862,-0.4,-0.398165138,-0.396330275,-0.394495413,-0.39266055,
-0.390825688,-0.388990826,-0.387155963,-0.385321101,-0.383486239,-0.381651376,
-0.379816514,-0.377981651,-0.376146789,-0.374311927,-0.372477064,-0.370642202,
-0.368807339,-0.366972477,-0.365137615,-0.363302752,-0.36146789,-0.359633028,
-0.357798165,-0.355963303,-0.35412844,-0.352293578,-0.350458716,-0.348623853,
-0.346788991,-0.344954128,-0.343119266,-0.341284404,-0.339449541,-0.337614679,
-0.335779817,-0.333944954,-0.332110092,-0.330275229,-0.328440367,-0.326605505,
-0.324770642,-0.32293578,-0.321100917,-0.319266055,-0.317431193,-0.31559633,
-0.313761468,-0.311926606,-0.310091743,-0.308256881,-0.306422018,-0.304587156,
-0.302752294,-0.300917431,-0.299082569,-0.297247706,-0.295412844,-0.293577982,
-0.291743119,-0.289908257,-0.288073394,-0.286238532,-0.28440367,-0.282568807,
-0.280733945,-0.278899083,-0.27706422,-0.275229358,-0.273394495,-0.271559633,
-0.269724771,-0.267889908,-0.266055046,-0.264220183,-0.262385321,-0.260550459,
-0.258715596,-0.256880734,-0.255045872,-0.253211009,-0.251376147,-0.249541284,
-0.247706422,-0.24587156,-0.244036697,-0.242201835,-0.240366972,-0.23853211,
-0.236697248,-0.234862385,-0.233027523,-0.231192661,-0.229357798,-0.227522936,
-0.225688073,-0.223853211,-0.222018349,-0.220183486,-0.218348624,-0.216513761,
-0.214678899,-0.212844037,-0.211009174,-0.209174312,-0.20733945,-0.205504587,
-0.203669725,-0.201834862,-0.2,-0.198165138,-0.196330275,-0.194495413,-0.19266055,
-0.190825688,-0.188990826,-0.187155963,-0.185321101,-0.183486239,-0.181651376,
-0.179816514,-0.177981651,-0.176146789,-0.174311927,-0.172477064,-0.170642202,
-0.168807339,-0.166972477,-0.165137615,-0.163302752,-0.16146789,-0.159633028,
-0.157798165,-0.155963303,-0.15412844,-0.152293578,-0.150458716,-0.148623853,
-0.146788991,-0.144954128,-0.143172102),.UNSPECIFIED.);
#24338=B_SPLINE_CURVE_WITH_KNOTS('',5,(#170537,#170538,#170539,#170540,
#170541,#170542,#170543,#170544,#170545,#170546,#170547,#170548,#170549,
#170550,#170551,#170552,#170553,#170554,#170555,#170556,#170557,#170558,
#170559,#170560,#170561,#170562,#170563,#170564,#170565,#170566,#170567,
#170568,#170569,#170570,#170571,#170572,#170573,#170574,#170575,#170576,
#170577,#170578,#170579,#170580,#170581,#170582,#170583,#170584,#170585,
#170586,#170587,#170588,#170589,#170590,#170591,#170592,#170593,#170594,
#170595,#170596,#170597,#170598,#170599,#170600,#170601,#170602,#170603,
#170604,#170605,#170606,#170607,#170608,#170609,#170610,#170611,#170612,
#170613,#170614,#170615,#170616,#170617,#170618,#170619,#170620,#170621,
#170622,#170623,#170624,#170625,#170626,#170627,#170628,#170629,#170630,
#170631,#170632,#170633,#170634,#170635,#170636,#170637,#170638,#170639,
#170640,#170641,#170642,#170643,#170644,#170645,#170646,#170647,#170648,
#170649,#170650,#170651,#170652,#170653,#170654,#170655,#170656,#170657,
#170658,#170659,#170660,#170661,#170662,#170663,#170664,#170665,#170666,
#170667,#170668,#170669,#170670,#170671,#170672,#170673,#170674,#170675,
#170676,#170677,#170678,#170679,#170680,#170681,#170682,#170683,#170684,
#170685,#170686,#170687,#170688,#170689,#170690,#170691,#170692,#170693,
#170694,#170695,#170696,#170697,#170698,#170699,#170700,#170701,#170702,
#170703,#170704,#170705,#170706,#170707,#170708,#170709,#170710,#170711,
#170712,#170713,#170714,#170715,#170716,#170717,#170718,#170719,#170720,
#170721,#170722,#170723,#170724,#170725,#170726,#170727,#170728,#170729,
#170730,#170731,#170732,#170733,#170734,#170735,#170736,#170737,#170738,
#170739,#170740,#170741,#170742,#170743,#170744,#170745,#170746,#170747,
#170748,#170749,#170750,#170751,#170752,#170753,#170754,#170755,#170756,
#170757,#170758,#170759,#170760,#170761,#170762,#170763,#170764,#170765,
#170766,#170767,#170768,#170769,#170770,#170771,#170772,#170773,#170774,
#170775,#170776,#170777,#170778,#170779,#170780,#170781,#170782,#170783,
#170784,#170785,#170786,#170787,#170788,#170789,#170790,#170791,#170792,
#170793,#170794,#170795,#170796,#170797,#170798,#170799,#170800,#170801,
#170802,#170803,#170804,#170805,#170806,#170807,#170808,#170809,#170810,
#170811,#170812,#170813,#170814,#170815,#170816,#170817,#170818,#170819,
#170820,#170821,#170822,#170823,#170824,#170825,#170826,#170827,#170828,
#170829,#170830,#170831,#170832,#170833,#170834,#170835,#170836,#170837,
#170838,#170839,#170840,#170841,#170842,#170843,#170844,#170845,#170846,
#170847,#170848,#170849,#170850,#170851,#170852,#170853,#170854,#170855,
#170856,#170857,#170858,#170859,#170860,#170861,#170862,#170863,#170864,
#170865,#170866,#170867,#170868,#170869,#170870,#170871,#170872,#170873,
#170874,#170875,#170876,#170877,#170878,#170879,#170880,#170881,#170882,
#170883,#170884,#170885,#170886,#170887,#170888,#170889,#170890,#170891,
#170892,#170893,#170894,#170895,#170896,#170897,#170898,#170899,#170900,
#170901,#170902,#170903,#170904,#170905,#170906,#170907,#170908,#170909,
#170910,#170911,#170912,#170913,#170914,#170915,#170916,#170917,#170918,
#170919,#170920,#170921,#170922,#170923,#170924,#170925,#170926,#170927,
#170928,#170929,#170930,#170931,#170932,#170933,#170934,#170935,#170936,
#170937,#170938,#170939,#170940,#170941,#170942,#170943,#170944,#170945,
#170946,#170947,#170948,#170949,#170950,#170951,#170952,#170953,#170954,
#170955,#170956,#170957,#170958,#170959,#170960,#170961,#170962,#170963,
#170964,#170965,#170966,#170967,#170968,#170969,#170970,#170971,#170972,
#170973,#170974,#170975,#170976,#170977,#170978,#170979,#170980,#170981,
#170982,#170983,#170984,#170985,#170986,#170987,#170988,#170989,#170990,
#170991,#170992,#170993,#170994,#170995,#170996,#170997,#170998,#170999,
#171000,#171001,#171002,#171003,#171004,#171005,#171006,#171007,#171008),
 .UNSPECIFIED.,.F.,.F.,(6,1,1,1,1,1,1,1,1,1,1,1,1,1,1,1,1,1,1,1,1,1,1,1,
1,1,1,1,1,1,1,1,1,1,1,1,1,1,1,1,1,1,1,1,1,1,1,1,1,1,1,1,1,1,1,1,1,1,1,1,
1,1,1,1,1,1,1,1,1,1,1,1,1,1,1,1,1,1,1,1,1,1,1,1,1,1,1,1,1,1,1,1,1,1,1,1,
1,1,1,1,1,1,1,1,1,1,1,1,1,1,1,1,1,1,1,1,1,1,1,1,1,1,1,1,1,1,1,1,1,1,1,1,
1,1,1,1,1,1,1,1,1,1,1,1,1,1,1,1,1,1,1,1,1,1,1,1,1,1,1,1,1,1,1,1,1,1,1,1,
1,1,1,1,1,1,1,1,1,1,1,1,1,1,1,1,1,1,1,1,1,1,1,1,1,1,1,1,1,1,1,1,1,1,1,1,
1,1,1,1,1,1,1,1,1,1,1,1,1,1,1,1,1,1,1,1,1,1,1,1,1,1,1,1,1,1,1,1,1,1,1,1,
1,1,1,1,1,1,1,1,1,1,1,1,1,1,1,1,1,1,1,1,1,1,1,1,1,1,1,1,1,1,1,1,1,1,1,1,
1,1,1,1,1,1,1,1,1,1,1,1,1,1,1,1,1,1,1,1,1,1,1,1,1,1,1,1,1,1,1,1,1,1,1,1,
1,1,1,1,1,1,1,1,1,1,1,1,1,1,1,1,1,1,1,1,1,1,1,1,1,1,1,1,1,1,1,1,1,1,1,1,
1,1,1,1,1,1,1,1,1,1,1,1,1,1,1,1,1,1,1,1,1,1,1,1,1,1,1,1,1,1,1,1,1,1,1,1,
1,1,1,1,1,1,1,1,1,1,1,1,1,1,1,1,1,1,1,1,1,1,1,1,1,1,1,1,1,1,1,1,1,1,1,1,
1,1,1,1,1,1,1,1,1,1,1,1,1,1,1,1,1,1,1,1,1,1,1,1,1,1,1,1,1,1,1,1,1,1,1,1,
1,1,1,1,1,1,1,1,1,1,1,6),(0.143172102,0.144954128,0.146788991,0.148623853,
0.150458716,0.152293578,0.15412844,0.155963303,0.157798165,0.159633028,
0.16146789,0.163302752,0.165137615,0.166972477,0.168807339,0.170642202,
0.172477064,0.174311927,0.176146789,0.177981651,0.179816514,0.181651376,
0.183486239,0.185321101,0.187155963,0.188990826,0.190825688,0.19266055,
0.194495413,0.196330275,0.198165138,0.2,0.201834862,0.203669725,0.205504587,
0.20733945,0.209174312,0.211009174,0.212844037,0.214678899,0.216513761,
0.218348624,0.220183486,0.222018349,0.223853211,0.225688073,0.227522936,
0.229357798,0.231192661,0.233027523,0.234862385,0.236697248,0.23853211,
0.240366972,0.242201835,0.244036697,0.24587156,0.247706422,0.249541284,
0.251376147,0.253211009,0.255045872,0.256880734,0.258715596,0.260550459,
0.262385321,0.264220183,0.266055046,0.267889908,0.269724771,0.271559633,
0.273394495,0.275229358,0.27706422,0.278899083,0.280733945,0.282568807,
0.28440367,0.286238532,0.288073394,0.289908257,0.291743119,0.293577982,
0.295412844,0.297247706,0.299082569,0.300917431,0.302752294,0.304587156,
0.306422018,0.308256881,0.310091743,0.311926606,0.313761468,0.31559633,
0.317431193,0.319266055,0.321100917,0.32293578,0.324770642,0.326605505,
0.328440367,0.330275229,0.332110092,0.333944954,0.335779817,0.337614679,
0.339449541,0.341284404,0.343119266,0.344954128,0.346788991,0.348623853,
0.350458716,0.352293578,0.35412844,0.355963303,0.357798165,0.359633028,
0.36146789,0.363302752,0.365137615,0.366972477,0.368807339,0.370642202,
0.372477064,0.374311927,0.376146789,0.377981651,0.379816514,0.381651376,
0.383486239,0.385321101,0.387155963,0.388990826,0.390825688,0.39266055,
0.394495413,0.396330275,0.398165138,0.4,0.401834862,0.403669725,0.405504587,
0.40733945,0.409174312,0.411009174,0.412844037,0.414678899,0.416513761,
0.418348624,0.420183486,0.422018349,0.423853211,0.425688073,0.427522936,
0.429357798,0.431192661,0.433027523,0.434862385,0.436697248,0.43853211,
0.440366972,0.442201835,0.444036697,0.44587156,0.447706422,0.449541284,
0.451376147,0.453211009,0.455045872,0.456880734,0.458715596,0.460550459,
0.462385321,0.464220183,0.466055046,0.467889908,0.469724771,0.471559633,
0.473394495,0.475229358,0.47706422,0.478899083,0.480733945,0.482568807,
0.48440367,0.486238532,0.488073394,0.489908257,0.491743119,0.493577982,
0.495412844,0.497247706,0.499082569,0.500917431,0.502752294,0.504587156,
0.506422018,0.508256881,0.510091743,0.511926606,0.513761468,0.51559633,
0.517431193,0.519266055,0.521100917,0.52293578,0.524770642,0.526605505,
0.528440367,0.530275229,0.532110092,0.533944954,0.535779817,0.537614679,
0.539449541,0.541284404,0.543119266,0.544954128,0.546788991,0.548623853,
0.550458716,0.552293578,0.55412844,0.555963303,0.557798165,0.559633028,
0.56146789,0.563302752,0.565137615,0.566972477,0.568807339,0.570642202,
0.572477064,0.574311927,0.576146789,0.577981651,0.579816514,0.581651376,
0.583486239,0.585321101,0.587155963,0.588990826,0.590825688,0.59266055,
0.594495413,0.596330275,0.598165138,0.6,0.601834862,0.603669725,0.605504587,
0.60733945,0.609174312,0.611009174,0.612844037,0.614678899,0.616513761,
0.618348624,0.620183486,0.622018349,0.623853211,0.625688073,0.627522936,
0.629357798,0.631192661,0.633027523,0.634862385,0.636697248,0.63853211,
0.640366972,0.642201835,0.644036697,0.64587156,0.647706422,0.649541284,
0.651376147,0.653211009,0.655045872,0.656880734,0.658715596,0.660550459,
0.662385321,0.664220183,0.666055046,0.667889908,0.669724771,0.671559633,
0.673394495,0.675229358,0.67706422,0.678899083,0.680733945,0.682568807,
0.68440367,0.686238532,0.688073394,0.689908257,0.691743119,0.693577982,
0.695412844,0.697247706,0.699082569,0.700917431,0.702752294,0.704587156,
0.706422018,0.708256881,0.710091743,0.711926606,0.713761468,0.71559633,
0.717431193,0.719266055,0.721100917,0.72293578,0.724770642,0.726605505,
0.728440367,0.730275229,0.732110092,0.733944954,0.735779817,0.737614679,
0.739449541,0.741284404,0.743119266,0.744954128,0.746788991,0.748623853,
0.750458716,0.752293578,0.75412844,0.755963303,0.757798165,0.759633028,
0.76146789,0.763302752,0.765137615,0.766972477,0.768807339,0.770642202,
0.772477064,0.774311927,0.776146789,0.777981651,0.779816514,0.781651376,
0.783486239,0.785321101,0.787155963,0.788990826,0.790825688,0.79266055,
0.794495413,0.796330275,0.798165138,0.8,0.801834862,0.803669725,0.805504587,
0.80733945,0.809174312,0.811009174,0.812844037,0.814678899,0.816513761,
0.818348624,0.820183486,0.822018349,0.823853211,0.825688073,0.827522936,
0.829357798,0.831192661,0.833027523,0.834862385,0.836697248,0.83853211,
0.840366972,0.842201835,0.844036697,0.84587156,0.847706422,0.849541284,
0.851376147,0.853211009,0.855045872,0.856880734,0.858715596,0.860550459,
0.862385321,0.864220183,0.866055046,0.867889908,0.869724771,0.871559633,
0.873394495,0.875229358,0.87706422,0.878899083,0.880733945,0.882568807,
0.88440367,0.886238532,0.888073394,0.889908257,0.891743119,0.893577982,
0.895412844,0.897247706,0.899082569,0.900917431,0.902752294,0.904587156,
0.906422018,0.908256881,0.910091743,0.911926606,0.913761468,0.91559633,
0.917431193,0.919266055,0.921100917,0.92293578,0.924770642,0.926605505,
0.928440367,0.930275229,0.932110092,0.933944954,0.935779817,0.937614679,
0.939449541,0.941284404,0.943119266,0.944954128,0.946788991,0.948623853,
0.950458716,0.952293578,0.95412844,0.955963303,0.957798165,0.959633028,
0.96146789,0.963302752,0.965137615,0.966972477,0.968807339,0.970642202,
0.972477064,0.974311927,0.976146789,0.977981651,0.979816514,0.981651376,
0.983486239,0.985321101,0.987155963,0.988990826,0.990825688,0.99266055,
0.994495413,0.996330275,0.998165138,1.),.UNSPECIFIED.);
#24339=B_SPLINE_CURVE_WITH_KNOTS('',5,(#171971,#171972,#171973,#171974,
#171975,#171976,#171977,#171978,#171979,#171980,#171981,#171982,#171983,
#171984,#171985,#171986,#171987,#171988,#171989,#171990,#171991,#171992,
#171993,#171994,#171995,#171996,#171997,#171998,#171999,#172000,#172001,
#172002,#172003,#172004,#172005,#172006,#172007,#172008,#172009,#172010,
#172011,#172012,#172013,#172014,#172015,#172016,#172017,#172018,#172019,
#172020,#172021,#172022,#172023,#172024,#172025,#172026,#172027,#172028,
#172029,#172030,#172031,#172032,#172033,#172034,#172035,#172036,#172037,
#172038,#172039,#172040,#172041,#172042,#172043,#172044,#172045,#172046,
#172047,#172048,#172049,#172050,#172051,#172052,#172053,#172054,#172055,
#172056,#172057,#172058,#172059,#172060,#172061,#172062,#172063,#172064,
#172065,#172066,#172067,#172068,#172069,#172070,#172071,#172072,#172073,
#172074,#172075,#172076,#172077,#172078,#172079,#172080,#172081,#172082,
#172083,#172084,#172085,#172086,#172087,#172088,#172089,#172090,#172091,
#172092,#172093,#172094,#172095,#172096,#172097,#172098,#172099,#172100,
#172101,#172102,#172103,#172104,#172105,#172106,#172107,#172108,#172109,
#172110,#172111,#172112,#172113,#172114,#172115,#172116,#172117,#172118,
#172119,#172120,#172121,#172122,#172123,#172124,#172125,#172126,#172127,
#172128,#172129,#172130,#172131,#172132,#172133,#172134,#172135,#172136,
#172137,#172138,#172139,#172140,#172141,#172142,#172143,#172144,#172145,
#172146,#172147,#172148,#172149,#172150,#172151,#172152,#172153,#172154,
#172155,#172156,#172157,#172158,#172159,#172160,#172161,#172162,#172163,
#172164,#172165,#172166,#172167,#172168,#172169,#172170,#172171,#172172,
#172173,#172174,#172175,#172176,#172177,#172178,#172179,#172180,#172181,
#172182,#172183,#172184,#172185,#172186,#172187,#172188,#172189,#172190,
#172191,#172192,#172193,#172194,#172195,#172196,#172197,#172198,#172199,
#172200,#172201,#172202,#172203,#172204,#172205,#172206,#172207,#172208,
#172209,#172210,#172211,#172212,#172213,#172214,#172215,#172216,#172217,
#172218,#172219,#172220,#172221,#172222,#172223,#172224,#172225,#172226,
#172227,#172228,#172229,#172230,#172231,#172232,#172233,#172234,#172235,
#172236,#172237,#172238,#172239,#172240,#172241,#172242,#172243,#172244,
#172245,#172246,#172247,#172248,#172249,#172250,#172251,#172252,#172253,
#172254,#172255,#172256,#172257,#172258,#172259,#172260,#172261,#172262,
#172263,#172264,#172265,#172266,#172267,#172268,#172269,#172270,#172271,
#172272,#172273,#172274,#172275,#172276,#172277,#172278,#172279,#172280,
#172281,#172282,#172283,#172284,#172285,#172286,#172287,#172288,#172289,
#172290,#172291,#172292,#172293,#172294,#172295,#172296,#172297,#172298,
#172299,#172300,#172301,#172302,#172303,#172304,#172305,#172306,#172307,
#172308,#172309,#172310,#172311,#172312,#172313,#172314,#172315,#172316,
#172317,#172318,#172319,#172320,#172321,#172322,#172323,#172324,#172325,
#172326,#172327,#172328,#172329,#172330,#172331,#172332,#172333,#172334,
#172335,#172336,#172337,#172338,#172339,#172340,#172341,#172342,#172343,
#172344,#172345,#172346,#172347,#172348,#172349,#172350,#172351,#172352,
#172353,#172354,#172355,#172356,#172357,#172358,#172359,#172360,#172361,
#172362,#172363,#172364,#172365,#172366,#172367,#172368,#172369,#172370,
#172371,#172372,#172373,#172374,#172375,#172376,#172377,#172378,#172379,
#172380,#172381,#172382,#172383,#172384,#172385,#172386,#172387,#172388,
#172389,#172390,#172391,#172392,#172393,#172394,#172395,#172396,#172397,
#172398,#172399,#172400,#172401,#172402,#172403,#172404,#172405,#172406,
#172407,#172408,#172409,#172410,#172411,#172412,#172413,#172414,#172415,
#172416,#172417,#172418,#172419,#172420,#172421,#172422,#172423,#172424,
#172425,#172426,#172427,#172428,#172429,#172430,#172431,#172432,#172433,
#172434,#172435,#172436,#172437,#172438,#172439),.UNSPECIFIED.,.F.,.F.,
(6,1,1,1,1,1,1,1,1,1,1,1,1,1,1,1,1,1,1,1,1,1,1,1,1,1,1,1,1,1,1,1,1,1,1,
1,1,1,1,1,1,1,1,1,1,1,1,1,1,1,1,1,1,1,1,1,1,1,1,1,1,1,1,1,1,1,1,1,1,1,1,
1,1,1,1,1,1,1,1,1,1,1,1,1,1,1,1,1,1,1,1,1,1,1,1,1,1,1,1,1,1,1,1,1,1,1,1,
1,1,1,1,1,1,1,1,1,1,1,1,1,1,1,1,1,1,1,1,1,1,1,1,1,1,1,1,1,1,1,1,1,1,1,1,
1,1,1,1,1,1,1,1,1,1,1,1,1,1,1,1,1,1,1,1,1,1,1,1,1,1,1,1,1,1,1,1,1,1,1,1,
1,1,1,1,1,1,1,1,1,1,1,1,1,1,1,1,1,1,1,1,1,1,1,1,1,1,1,1,1,1,1,1,1,1,1,1,
1,1,1,1,1,1,1,1,1,1,1,1,1,1,1,1,1,1,1,1,1,1,1,1,1,1,1,1,1,1,1,1,1,1,1,1,
1,1,1,1,1,1,1,1,1,1,1,1,1,1,1,1,1,1,1,1,1,1,1,1,1,1,1,1,1,1,1,1,1,1,1,1,
1,1,1,1,1,1,1,1,1,1,1,1,1,1,1,1,1,1,1,1,1,1,1,1,1,1,1,1,1,1,1,1,1,1,1,1,
1,1,1,1,1,1,1,1,1,1,1,1,1,1,1,1,1,1,1,1,1,1,1,1,1,1,1,1,1,1,1,1,1,1,1,1,
1,1,1,1,1,1,1,1,1,1,1,1,1,1,1,1,1,1,1,1,1,1,1,1,1,1,1,1,1,1,1,1,1,1,1,1,
1,1,1,1,1,1,1,1,1,1,1,1,1,1,1,1,1,1,1,1,1,1,1,1,1,1,1,1,1,1,1,1,1,1,1,1,
1,1,1,1,1,1,1,1,1,1,1,1,1,1,1,1,1,1,1,1,1,1,1,1,1,1,1,1,1,1,1,1,1,6),(-1.,
-0.998165138,-0.996330275,-0.994495413,-0.99266055,-0.990825688,-0.988990826,
-0.987155963,-0.985321101,-0.983486239,-0.981651376,-0.979816514,-0.977981651,
-0.974311927,-0.972477064,-0.970642202,-0.968807339,-0.966972477,-0.965137615,
-0.963302752,-0.96146789,-0.959633028,-0.957798165,-0.955963303,-0.95412844,
-0.952293578,-0.950458716,-0.948623853,-0.946788991,-0.944954128,-0.943119266,
-0.941284404,-0.939449541,-0.937614679,-0.935779817,-0.933944954,-0.932110092,
-0.930275229,-0.928440367,-0.926605505,-0.924770642,-0.92293578,-0.921100917,
-0.919266055,-0.917431193,-0.91559633,-0.913761468,-0.911926606,-0.910091743,
-0.908256881,-0.906422018,-0.904587156,-0.902752294,-0.900917431,-0.899082569,
-0.897247706,-0.895412844,-0.893577982,-0.891743119,-0.889908257,-0.888073394,
-0.886238532,-0.88440367,-0.882568807,-0.880733945,-0.878899083,-0.87706422,
-0.875229358,-0.873394495,-0.871559633,-0.869724771,-0.867889908,-0.866055046,
-0.864220183,-0.862385321,-0.860550459,-0.858715596,-0.856880734,-0.855045872,
-0.853211009,-0.851376147,-0.849541284,-0.847706422,-0.84587156,-0.844036697,
-0.842201835,-0.840366972,-0.83853211,-0.836697248,-0.834862385,-0.833027523,
-0.831192661,-0.829357798,-0.827522936,-0.825688073,-0.823853211,-0.822018349,
-0.820183486,-0.818348624,-0.816513761,-0.814678899,-0.812844037,-0.811009174,
-0.809174312,-0.80733945,-0.805504587,-0.803669725,-0.801834862,-0.8,-0.798165138,
-0.796330275,-0.794495413,-0.79266055,-0.790825688,-0.788990826,-0.787155963,
-0.785321101,-0.783486239,-0.781651376,-0.779816514,-0.777981651,-0.776146789,
-0.774311927,-0.772477064,-0.770642202,-0.768807339,-0.766972477,-0.765137615,
-0.763302752,-0.76146789,-0.759633028,-0.757798165,-0.755963303,-0.75412844,
-0.752293578,-0.750458716,-0.748623853,-0.744954128,-0.743119266,-0.741284404,
-0.739449541,-0.737614679,-0.735779817,-0.733944954,-0.732110092,-0.730275229,
-0.728440367,-0.726605505,-0.724770642,-0.72293578,-0.721100917,-0.719266055,
-0.717431193,-0.71559633,-0.713761468,-0.711926606,-0.710091743,-0.708256881,
-0.706422018,-0.704587156,-0.702752294,-0.700917431,-0.699082569,-0.697247706,
-0.695412844,-0.693577982,-0.691743119,-0.689908257,-0.688073394,-0.686238532,
-0.68440367,-0.682568807,-0.680733945,-0.678899083,-0.67706422,-0.675229358,
-0.673394495,-0.671559633,-0.669724771,-0.667889908,-0.666055046,-0.664220183,
-0.662385321,-0.660550459,-0.658715596,-0.656880734,-0.655045872,-0.653211009,
-0.651376147,-0.649541284,-0.647706422,-0.64587156,-0.644036697,-0.642201835,
-0.640366972,-0.63853211,-0.636697248,-0.634862385,-0.633027523,-0.631192661,
-0.629357798,-0.627522936,-0.625688073,-0.623853211,-0.622018349,-0.620183486,
-0.618348624,-0.616513761,-0.614678899,-0.612844037,-0.611009174,-0.609174312,
-0.60733945,-0.605504587,-0.603669725,-0.601834862,-0.6,-0.598165138,-0.596330275,
-0.594495413,-0.59266055,-0.590825688,-0.588990826,-0.587155963,-0.585321101,
-0.583486239,-0.581651376,-0.579816514,-0.577981651,-0.576146789,-0.574311927,
-0.572477064,-0.570642202,-0.568807339,-0.566972477,-0.565137615,-0.563302752,
-0.56146789,-0.559633028,-0.557798165,-0.555963303,-0.55412844,-0.552293578,
-0.550458716,-0.548623853,-0.546788991,-0.544954128,-0.543119266,-0.541284404,
-0.539449541,-0.537614679,-0.535779817,-0.533944954,-0.532110092,-0.530275229,
-0.528440367,-0.526605505,-0.524770642,-0.52293578,-0.521100917,-0.519266055,
-0.517431193,-0.51559633,-0.513761468,-0.511926606,-0.510091743,-0.508256881,
-0.506422018,-0.504587156,-0.502752294,-0.500917431,-0.499082569,-0.497247706,
-0.495412844,-0.493577982,-0.491743119,-0.489908257,-0.488073394,-0.486238532,
-0.48440367,-0.482568807,-0.480733945,-0.478899083,-0.47706422,-0.475229358,
-0.473394495,-0.471559633,-0.469724771,-0.467889908,-0.466055046,-0.464220183,
-0.462385321,-0.460550459,-0.458715596,-0.456880734,-0.455045872,-0.453211009,
-0.451376147,-0.449541284,-0.447706422,-0.44587156,-0.444036697,-0.442201835,
-0.440366972,-0.43853211,-0.436697248,-0.434862385,-0.433027523,-0.431192661,
-0.429357798,-0.427522936,-0.425688073,-0.423853211,-0.422018349,-0.420183486,
-0.418348624,-0.416513761,-0.414678899,-0.412844037,-0.411009174,-0.409174312,
-0.40733945,-0.405504587,-0.403669725,-0.401834862,-0.4,-0.398165138,-0.396330275,
-0.394495413,-0.39266055,-0.390825688,-0.388990826,-0.387155963,-0.385321101,
-0.383486239,-0.381651376,-0.379816514,-0.377981651,-0.376146789,-0.374311927,
-0.372477064,-0.370642202,-0.368807339,-0.366972477,-0.365137615,-0.363302752,
-0.36146789,-0.359633028,-0.357798165,-0.355963303,-0.35412844,-0.352293578,
-0.350458716,-0.348623853,-0.346788991,-0.344954128,-0.343119266,-0.341284404,
-0.339449541,-0.337614679,-0.335779817,-0.333944954,-0.332110092,-0.328440367,
-0.326605505,-0.324770642,-0.32293578,-0.321100917,-0.319266055,-0.317431193,
-0.31559633,-0.313761468,-0.311926606,-0.310091743,-0.308256881,-0.306422018,
-0.304587156,-0.302752294,-0.300917431,-0.299082569,-0.297247706,-0.295412844,
-0.293577982,-0.291743119,-0.289908257,-0.288073394,-0.286238532,-0.28440367,
-0.282568807,-0.280733945,-0.278899083,-0.27706422,-0.275229358,-0.273394495,
-0.271559633,-0.269724771,-0.267889908,-0.266055046,-0.264220183,-0.262385321,
-0.260550459,-0.258715596,-0.256880734,-0.255045872,-0.253211009,-0.251376147,
-0.249541284,-0.247706422,-0.24587156,-0.244036697,-0.242201835,-0.240366972,
-0.23853211,-0.236697248,-0.234862385,-0.233027523,-0.231192661,-0.229357798,
-0.227522936,-0.225688073,-0.223853211,-0.222018349,-0.220183486,-0.218348624,
-0.216513761,-0.214678899,-0.212844037,-0.211009174,-0.209174312,-0.20733945,
-0.205504587,-0.203669725,-0.201834862,-0.2,-0.198165138,-0.196330275,-0.194495413,
-0.19266055,-0.190825688,-0.188990826,-0.187155963,-0.185321101,-0.183486239,
-0.181651376,-0.179816514,-0.177981651,-0.176146789,-0.174311927,-0.172477064,
-0.170642202,-0.168807339,-0.166972477,-0.165137615,-0.163302752,-0.16146789,
-0.159633028,-0.157798165,-0.155963303,-0.15412844,-0.152293578,-0.150458716,
-0.148623853,-0.146788991,-0.144954128,-0.143172102),.UNSPECIFIED.);
#24340=B_SPLINE_CURVE_WITH_KNOTS('',5,(#172440,#172441,#172442,#172443,
#172444,#172445,#172446,#172447,#172448,#172449,#172450,#172451,#172452,
#172453,#172454,#172455,#172456,#172457,#172458,#172459,#172460,#172461,
#172462,#172463,#172464,#172465,#172466,#172467,#172468,#172469,#172470,
#172471,#172472,#172473,#172474,#172475,#172476,#172477,#172478,#172479,
#172480,#172481,#172482,#172483,#172484,#172485,#172486,#172487,#172488,
#172489,#172490,#172491,#172492,#172493,#172494,#172495,#172496,#172497,
#172498,#172499,#172500,#172501,#172502,#172503,#172504,#172505,#172506,
#172507,#172508,#172509,#172510,#172511,#172512,#172513,#172514,#172515,
#172516,#172517,#172518,#172519,#172520,#172521,#172522,#172523,#172524,
#172525,#172526,#172527,#172528,#172529,#172530,#172531,#172532,#172533,
#172534,#172535,#172536,#172537,#172538,#172539,#172540,#172541,#172542,
#172543,#172544,#172545,#172546,#172547,#172548,#172549,#172550,#172551,
#172552,#172553,#172554,#172555,#172556,#172557,#172558,#172559,#172560,
#172561,#172562,#172563,#172564,#172565,#172566,#172567,#172568,#172569,
#172570,#172571,#172572,#172573,#172574,#172575,#172576,#172577,#172578,
#172579,#172580,#172581,#172582,#172583,#172584,#172585,#172586,#172587,
#172588,#172589,#172590,#172591,#172592,#172593,#172594,#172595,#172596,
#172597,#172598,#172599,#172600,#172601,#172602,#172603,#172604,#172605,
#172606,#172607,#172608,#172609,#172610,#172611,#172612,#172613,#172614,
#172615,#172616,#172617,#172618,#172619,#172620,#172621,#172622,#172623,
#172624,#172625,#172626,#172627,#172628,#172629,#172630,#172631,#172632,
#172633,#172634,#172635,#172636,#172637,#172638,#172639,#172640,#172641,
#172642,#172643,#172644,#172645,#172646,#172647,#172648,#172649,#172650,
#172651,#172652,#172653,#172654,#172655,#172656,#172657,#172658,#172659,
#172660,#172661,#172662,#172663,#172664,#172665,#172666,#172667,#172668,
#172669,#172670,#172671,#172672,#172673,#172674,#172675,#172676,#172677,
#172678,#172679,#172680,#172681,#172682,#172683,#172684,#172685,#172686,
#172687,#172688,#172689,#172690,#172691,#172692,#172693,#172694,#172695,
#172696,#172697,#172698,#172699,#172700,#172701,#172702,#172703,#172704,
#172705,#172706,#172707,#172708,#172709,#172710,#172711,#172712,#172713,
#172714,#172715,#172716,#172717,#172718,#172719,#172720,#172721,#172722,
#172723,#172724,#172725,#172726,#172727,#172728,#172729,#172730,#172731,
#172732,#172733,#172734,#172735,#172736,#172737,#172738,#172739,#172740,
#172741,#172742,#172743,#172744,#172745,#172746,#172747,#172748,#172749,
#172750,#172751,#172752,#172753,#172754,#172755,#172756,#172757,#172758,
#172759,#172760,#172761,#172762,#172763,#172764,#172765,#172766,#172767,
#172768,#172769,#172770,#172771,#172772,#172773,#172774,#172775,#172776,
#172777,#172778,#172779,#172780,#172781,#172782,#172783,#172784,#172785,
#172786,#172787,#172788,#172789,#172790,#172791,#172792,#172793,#172794,
#172795,#172796,#172797,#172798,#172799,#172800,#172801,#172802,#172803,
#172804,#172805,#172806,#172807,#172808,#172809,#172810,#172811,#172812,
#172813,#172814,#172815,#172816,#172817,#172818,#172819,#172820,#172821,
#172822,#172823,#172824,#172825,#172826,#172827,#172828,#172829,#172830,
#172831,#172832,#172833,#172834,#172835,#172836,#172837,#172838,#172839,
#172840,#172841,#172842,#172843,#172844,#172845,#172846,#172847,#172848,
#172849,#172850,#172851,#172852,#172853,#172854,#172855,#172856,#172857,
#172858,#172859,#172860,#172861,#172862,#172863,#172864,#172865,#172866,
#172867,#172868,#172869,#172870,#172871,#172872,#172873,#172874,#172875,
#172876,#172877,#172878,#172879,#172880,#172881,#172882,#172883,#172884,
#172885,#172886,#172887,#172888,#172889,#172890,#172891,#172892,#172893,
#172894,#172895,#172896,#172897,#172898,#172899,#172900,#172901,#172902,
#172903,#172904,#172905,#172906,#172907,#172908),.UNSPECIFIED.,.F.,.F.,
(6,1,1,1,1,1,1,1,1,1,1,1,1,1,1,1,1,1,1,1,1,1,1,1,1,1,1,1,1,1,1,1,1,1,1,
1,1,1,1,1,1,1,1,1,1,1,1,1,1,1,1,1,1,1,1,1,1,1,1,1,1,1,1,1,1,1,1,1,1,1,1,
1,1,1,1,1,1,1,1,1,1,1,1,1,1,1,1,1,1,1,1,1,1,1,1,1,1,1,1,1,1,1,1,1,1,1,1,
1,1,1,1,1,1,1,1,1,1,1,1,1,1,1,1,1,1,1,1,1,1,1,1,1,1,1,1,1,1,1,1,1,1,1,1,
1,1,1,1,1,1,1,1,1,1,1,1,1,1,1,1,1,1,1,1,1,1,1,1,1,1,1,1,1,1,1,1,1,1,1,1,
1,1,1,1,1,1,1,1,1,1,1,1,1,1,1,1,1,1,1,1,1,1,1,1,1,1,1,1,1,1,1,1,1,1,1,1,
1,1,1,1,1,1,1,1,1,1,1,1,1,1,1,1,1,1,1,1,1,1,1,1,1,1,1,1,1,1,1,1,1,1,1,1,
1,1,1,1,1,1,1,1,1,1,1,1,1,1,1,1,1,1,1,1,1,1,1,1,1,1,1,1,1,1,1,1,1,1,1,1,
1,1,1,1,1,1,1,1,1,1,1,1,1,1,1,1,1,1,1,1,1,1,1,1,1,1,1,1,1,1,1,1,1,1,1,1,
1,1,1,1,1,1,1,1,1,1,1,1,1,1,1,1,1,1,1,1,1,1,1,1,1,1,1,1,1,1,1,1,1,1,1,1,
1,1,1,1,1,1,1,1,1,1,1,1,1,1,1,1,1,1,1,1,1,1,1,1,1,1,1,1,1,1,1,1,1,1,1,1,
1,1,1,1,1,1,1,1,1,1,1,1,1,1,1,1,1,1,1,1,1,1,1,1,1,1,1,1,1,1,1,1,1,1,1,1,
1,1,1,1,1,1,1,1,1,1,1,1,1,1,1,1,1,1,1,1,1,1,1,1,1,1,1,1,1,1,1,1,1,6),(0.143172102,
0.144954128,0.146788991,0.148623853,0.150458716,0.152293578,0.15412844,
0.155963303,0.157798165,0.159633028,0.16146789,0.163302752,0.165137615,
0.166972477,0.168807339,0.170642202,0.172477064,0.174311927,0.176146789,
0.177981651,0.179816514,0.181651376,0.183486239,0.185321101,0.187155963,
0.188990826,0.190825688,0.19266055,0.194495413,0.196330275,0.198165138,
0.2,0.201834862,0.203669725,0.205504587,0.20733945,0.209174312,0.211009174,
0.212844037,0.214678899,0.216513761,0.218348624,0.220183486,0.222018349,
0.223853211,0.225688073,0.227522936,0.229357798,0.231192661,0.233027523,
0.234862385,0.236697248,0.23853211,0.240366972,0.242201835,0.244036697,
0.24587156,0.247706422,0.249541284,0.251376147,0.253211009,0.255045872,
0.256880734,0.258715596,0.260550459,0.262385321,0.264220183,0.266055046,
0.267889908,0.269724771,0.271559633,0.273394495,0.275229358,0.27706422,
0.278899083,0.280733945,0.282568807,0.28440367,0.286238532,0.288073394,
0.289908257,0.291743119,0.293577982,0.295412844,0.297247706,0.299082569,
0.300917431,0.302752294,0.304587156,0.306422018,0.308256881,0.310091743,
0.311926606,0.313761468,0.31559633,0.317431193,0.319266055,0.321100917,
0.32293578,0.324770642,0.326605505,0.328440367,0.332110092,0.333944954,
0.335779817,0.337614679,0.339449541,0.341284404,0.343119266,0.344954128,
0.346788991,0.348623853,0.350458716,0.352293578,0.35412844,0.355963303,
0.357798165,0.359633028,0.36146789,0.363302752,0.365137615,0.366972477,
0.368807339,0.370642202,0.372477064,0.374311927,0.376146789,0.377981651,
0.379816514,0.381651376,0.383486239,0.385321101,0.387155963,0.388990826,
0.390825688,0.39266055,0.394495413,0.396330275,0.398165138,0.4,0.401834862,
0.403669725,0.405504587,0.40733945,0.409174312,0.411009174,0.412844037,
0.414678899,0.416513761,0.418348624,0.420183486,0.422018349,0.423853211,
0.425688073,0.427522936,0.429357798,0.431192661,0.433027523,0.434862385,
0.436697248,0.43853211,0.440366972,0.442201835,0.444036697,0.44587156,0.447706422,
0.449541284,0.451376147,0.453211009,0.455045872,0.456880734,0.458715596,
0.460550459,0.462385321,0.464220183,0.466055046,0.467889908,0.469724771,
0.471559633,0.473394495,0.475229358,0.47706422,0.478899083,0.480733945,
0.482568807,0.48440367,0.486238532,0.488073394,0.489908257,0.491743119,
0.493577982,0.495412844,0.497247706,0.499082569,0.500917431,0.502752294,
0.504587156,0.506422018,0.508256881,0.510091743,0.511926606,0.513761468,
0.51559633,0.517431193,0.519266055,0.521100917,0.52293578,0.524770642,0.526605505,
0.528440367,0.530275229,0.532110092,0.533944954,0.535779817,0.537614679,
0.539449541,0.541284404,0.543119266,0.544954128,0.546788991,0.548623853,
0.550458716,0.552293578,0.55412844,0.555963303,0.557798165,0.559633028,
0.56146789,0.563302752,0.565137615,0.566972477,0.568807339,0.570642202,
0.572477064,0.574311927,0.576146789,0.577981651,0.579816514,0.581651376,
0.583486239,0.585321101,0.587155963,0.588990826,0.590825688,0.59266055,
0.594495413,0.596330275,0.598165138,0.6,0.601834862,0.603669725,0.605504587,
0.60733945,0.609174312,0.611009174,0.612844037,0.614678899,0.616513761,
0.618348624,0.620183486,0.622018349,0.623853211,0.625688073,0.627522936,
0.629357798,0.631192661,0.633027523,0.634862385,0.636697248,0.63853211,
0.640366972,0.642201835,0.644036697,0.64587156,0.647706422,0.649541284,
0.651376147,0.653211009,0.655045872,0.656880734,0.658715596,0.660550459,
0.662385321,0.664220183,0.666055046,0.667889908,0.669724771,0.671559633,
0.673394495,0.675229358,0.67706422,0.678899083,0.680733945,0.682568807,
0.68440367,0.686238532,0.688073394,0.689908257,0.691743119,0.693577982,
0.695412844,0.697247706,0.699082569,0.700917431,0.702752294,0.704587156,
0.706422018,0.708256881,0.710091743,0.711926606,0.713761468,0.71559633,
0.717431193,0.719266055,0.721100917,0.72293578,0.724770642,0.726605505,
0.728440367,0.730275229,0.732110092,0.733944954,0.735779817,0.737614679,
0.739449541,0.741284404,0.743119266,0.744954128,0.748623853,0.750458716,
0.752293578,0.75412844,0.755963303,0.757798165,0.759633028,0.76146789,0.763302752,
0.765137615,0.766972477,0.768807339,0.770642202,0.772477064,0.774311927,
0.776146789,0.777981651,0.779816514,0.781651376,0.783486239,0.785321101,
0.787155963,0.788990826,0.790825688,0.79266055,0.794495413,0.796330275,
0.798165138,0.8,0.801834862,0.803669725,0.805504587,0.80733945,0.809174312,
0.811009174,0.812844037,0.814678899,0.816513761,0.818348624,0.820183486,
0.822018349,0.823853211,0.825688073,0.827522936,0.829357798,0.831192661,
0.833027523,0.834862385,0.836697248,0.83853211,0.840366972,0.842201835,
0.844036697,0.84587156,0.847706422,0.849541284,0.851376147,0.853211009,
0.855045872,0.856880734,0.858715596,0.860550459,0.862385321,0.864220183,
0.866055046,0.867889908,0.869724771,0.871559633,0.873394495,0.875229358,
0.87706422,0.878899083,0.880733945,0.882568807,0.88440367,0.886238532,0.888073394,
0.889908257,0.891743119,0.893577982,0.895412844,0.897247706,0.899082569,
0.900917431,0.902752294,0.904587156,0.906422018,0.908256881,0.910091743,
0.911926606,0.913761468,0.91559633,0.917431193,0.919266055,0.921100917,
0.92293578,0.924770642,0.926605505,0.928440367,0.930275229,0.932110092,
0.933944954,0.935779817,0.937614679,0.939449541,0.941284404,0.943119266,
0.944954128,0.946788991,0.948623853,0.950458716,0.952293578,0.95412844,
0.955963303,0.957798165,0.959633028,0.96146789,0.963302752,0.965137615,
0.966972477,0.968807339,0.970642202,0.972477064,0.974311927,0.977981651,
0.979816514,0.981651376,0.983486239,0.985321101,0.987155963,0.988990826,
0.990825688,0.99266055,0.994495413,0.996330275,0.998165138,1.),
 .UNSPECIFIED.);
#24341=B_SPLINE_CURVE_WITH_KNOTS('',3,(#173853,#173854,#173855,#173856,
#173857,#173858,#173859,#173860,#173861,#173862,#173863,#173864,#173865,
#173866,#173867,#173868,#173869,#173870,#173871,#173872,#173873,#173874,
#173875,#173876,#173877,#173878,#173879,#173880,#173881,#173882,#173883,
#173884,#173885,#173886,#173887,#173888,#173889,#173890,#173891,#173892,
#173893,#173894,#173895,#173896,#173897,#173898,#173899,#173900,#173901,
#173902,#173903,#173904,#173905,#173906,#173907,#173908,#173909,#173910,
#173911,#173912,#173913,#173914,#173915,#173916,#173917,#173918,#173919,
#173920,#173921,#173922,#173923,#173924,#173925,#173926,#173927,#173928,
#173929,#173930,#173931,#173932,#173933,#173934,#173935,#173936,#173937,
#173938,#173939,#173940,#173941,#173942,#173943,#173944,#173945,#173946,
#173947,#173948,#173949,#173950,#173951,#173952,#173953,#173954,#173955,
#173956,#173957,#173958,#173959,#173960,#173961,#173962,#173963,#173964,
#173965,#173966,#173967,#173968,#173969,#173970,#173971,#173972,#173973,
#173974,#173975,#173976,#173977,#173978,#173979,#173980,#173981,#173982,
#173983,#173984,#173985,#173986,#173987,#173988,#173989,#173990,#173991,
#173992,#173993,#173994,#173995,#173996,#173997,#173998,#173999,#174000,
#174001,#174002,#174003,#174004,#174005,#174006,#174007,#174008,#174009,
#174010,#174011,#174012,#174013,#174014,#174015,#174016,#174017,#174018,
#174019,#174020,#174021,#174022,#174023,#174024,#174025,#174026,#174027,
#174028,#174029,#174030,#174031,#174032,#174033,#174034,#174035,#174036,
#174037,#174038,#174039,#174040,#174041,#174042,#174043,#174044,#174045,
#174046,#174047,#174048,#174049,#174050,#174051,#174052,#174053,#174054,
#174055,#174056,#174057,#174058,#174059,#174060,#174061,#174062,#174063,
#174064,#174065,#174066,#174067,#174068,#174069,#174070,#174071,#174072,
#174073,#174074,#174075,#174076,#174077,#174078,#174079,#174080,#174081,
#174082,#174083,#174084,#174085,#174086,#174087,#174088,#174089,#174090,
#174091,#174092,#174093,#174094,#174095,#174096,#174097,#174098,#174099,
#174100,#174101,#174102,#174103,#174104,#174105,#174106,#174107,#174108,
#174109,#174110,#174111,#174112,#174113,#174114,#174115,#174116,#174117,
#174118,#174119,#174120,#174121,#174122,#174123,#174124,#174125,#174126,
#174127,#174128,#174129,#174130,#174131,#174132,#174133,#174134,#174135,
#174136,#174137,#174138,#174139,#174140,#174141,#174142,#174143,#174144,
#174145,#174146,#174147,#174148,#174149,#174150,#174151,#174152,#174153,
#174154,#174155,#174156,#174157,#174158,#174159,#174160,#174161,#174162,
#174163,#174164,#174165,#174166,#174167,#174168,#174169,#174170,#174171,
#174172,#174173,#174174),.UNSPECIFIED.,.F.,.F.,(4,3,3,3,3,3,3,3,3,3,3,3,
3,3,3,3,3,3,3,3,3,3,3,3,3,3,3,3,3,3,3,3,3,3,3,3,3,3,3,3,3,3,3,3,3,3,3,3,
3,3,3,3,3,3,3,3,3,3,3,3,3,3,3,3,3,3,3,3,3,3,3,3,3,3,3,3,3,3,3,3,3,3,3,3,
3,3,3,3,3,3,3,3,3,3,3,3,3,3,3,3,3,3,3,3,3,3,3,4),(0.143172102,0.15412844,
0.165137615,0.176146789,0.187155963,0.198165138,0.209174312,0.220183486,
0.231192661,0.242201835,0.253211009,0.264220183,0.275229358,0.286238532,
0.297247706,0.308256881,0.319266055,0.330275229,0.341284404,0.352293578,
0.365137615,0.376146789,0.387155963,0.396330275,0.405504587,0.414678899,
0.423853211,0.433027523,0.442201835,0.451376147,0.460550459,0.469724771,
0.478899083,0.488073394,0.497247706,0.508256881,0.517431193,0.526605505,
0.533944954,0.541284404,0.548623853,0.555963303,0.563302752,0.570642202,
0.577981651,0.588990826,0.598165138,0.605504587,0.612844037,0.620183486,
0.627522936,0.636697248,0.644036697,0.651376147,0.658715596,0.666055046,
0.673394495,0.680733945,0.688073394,0.695412844,0.704587156,0.711926606,
0.719266055,0.726605505,0.735779817,0.743119266,0.750458716,0.757798165,
0.765137615,0.772477064,0.779816514,0.787155963,0.794495413,0.801834862,
0.809174312,0.816513761,0.822018349,0.827522936,0.833027523,0.840366972,
0.84587156,0.851376147,0.856880734,0.862385321,0.867889908,0.873394495,
0.878899083,0.88440367,0.889908257,0.895412844,0.902752294,0.908256881,
0.913761468,0.919266055,0.924770642,0.930275229,0.935779817,0.941284404,
0.946788991,0.952293578,0.957798165,0.963302752,0.970642202,0.976146789,
0.981651376,0.987155963,0.99266055,1.),.UNSPECIFIED.);
#24342=B_SPLINE_CURVE_WITH_KNOTS('',3,(#174175,#174176,#174177,#174178,
#174179,#174180,#174181,#174182,#174183,#174184,#174185,#174186,#174187,
#174188,#174189,#174190,#174191,#174192,#174193,#174194,#174195,#174196,
#174197,#174198,#174199,#174200,#174201,#174202,#174203,#174204,#174205,
#174206,#174207,#174208,#174209,#174210,#174211,#174212,#174213,#174214,
#174215,#174216,#174217,#174218,#174219,#174220,#174221,#174222,#174223,
#174224,#174225,#174226,#174227,#174228,#174229,#174230,#174231,#174232,
#174233,#174234,#174235,#174236,#174237,#174238,#174239,#174240,#174241,
#174242,#174243,#174244,#174245,#174246,#174247,#174248,#174249,#174250,
#174251,#174252,#174253,#174254,#174255,#174256,#174257,#174258,#174259,
#174260,#174261,#174262,#174263,#174264,#174265,#174266,#174267,#174268,
#174269,#174270,#174271,#174272,#174273,#174274,#174275,#174276,#174277,
#174278,#174279,#174280,#174281,#174282,#174283,#174284,#174285,#174286,
#174287,#174288,#174289,#174290,#174291,#174292,#174293,#174294,#174295,
#174296,#174297,#174298,#174299,#174300,#174301,#174302,#174303,#174304,
#174305,#174306,#174307,#174308,#174309,#174310,#174311,#174312,#174313,
#174314,#174315,#174316,#174317,#174318,#174319,#174320,#174321,#174322,
#174323,#174324,#174325,#174326,#174327,#174328,#174329,#174330,#174331,
#174332,#174333,#174334,#174335,#174336,#174337,#174338,#174339,#174340,
#174341,#174342,#174343,#174344,#174345,#174346,#174347,#174348,#174349,
#174350,#174351,#174352,#174353,#174354,#174355,#174356,#174357,#174358,
#174359,#174360,#174361,#174362,#174363,#174364,#174365,#174366,#174367,
#174368,#174369,#174370,#174371,#174372,#174373,#174374,#174375,#174376,
#174377,#174378,#174379,#174380,#174381,#174382,#174383,#174384,#174385,
#174386,#174387,#174388,#174389,#174390,#174391,#174392,#174393,#174394,
#174395,#174396,#174397,#174398,#174399,#174400,#174401,#174402,#174403,
#174404,#174405,#174406,#174407,#174408,#174409,#174410,#174411,#174412,
#174413,#174414,#174415,#174416,#174417,#174418,#174419,#174420,#174421,
#174422,#174423,#174424,#174425,#174426,#174427,#174428,#174429,#174430,
#174431,#174432,#174433,#174434,#174435,#174436,#174437,#174438,#174439,
#174440,#174441,#174442,#174443,#174444,#174445,#174446,#174447,#174448,
#174449,#174450,#174451,#174452,#174453,#174454,#174455,#174456,#174457,
#174458,#174459,#174460,#174461,#174462,#174463,#174464,#174465,#174466,
#174467,#174468,#174469,#174470,#174471,#174472,#174473,#174474,#174475,
#174476,#174477,#174478,#174479,#174480,#174481,#174482,#174483,#174484,
#174485,#174486,#174487,#174488,#174489,#174490,#174491,#174492,#174493,
#174494,#174495,#174496),.UNSPECIFIED.,.F.,.F.,(4,3,3,3,3,3,3,3,3,3,3,3,
3,3,3,3,3,3,3,3,3,3,3,3,3,3,3,3,3,3,3,3,3,3,3,3,3,3,3,3,3,3,3,3,3,3,3,3,
3,3,3,3,3,3,3,3,3,3,3,3,3,3,3,3,3,3,3,3,3,3,3,3,3,3,3,3,3,3,3,3,3,3,3,3,
3,3,3,3,3,3,3,3,3,3,3,3,3,3,3,3,3,3,3,3,3,3,3,4),(0.143172102,0.15412844,
0.165137615,0.176146789,0.187155963,0.198165138,0.209174312,0.220183486,
0.231192661,0.242201835,0.253211009,0.264220183,0.275229358,0.286238532,
0.297247706,0.308256881,0.319266055,0.330275229,0.341284404,0.352293578,
0.363302752,0.374311927,0.385321101,0.396330275,0.405504587,0.414678899,
0.423853211,0.433027523,0.442201835,0.451376147,0.460550459,0.469724771,
0.478899083,0.488073394,0.497247706,0.508256881,0.517431193,0.526605505,
0.533944954,0.541284404,0.548623853,0.557798165,0.565137615,0.572477064,
0.579816514,0.587155963,0.594495413,0.601834862,0.609174312,0.616513761,
0.623853211,0.631192661,0.63853211,0.64587156,0.653211009,0.660550459,0.667889908,
0.675229358,0.682568807,0.689908257,0.697247706,0.704587156,0.711926606,
0.719266055,0.726605505,0.733944954,0.743119266,0.750458716,0.757798165,
0.765137615,0.772477064,0.779816514,0.787155963,0.794495413,0.801834862,
0.809174312,0.814678899,0.820183486,0.825688073,0.831192661,0.83853211,
0.844036697,0.849541284,0.855045872,0.860550459,0.867889908,0.873394495,
0.878899083,0.88440367,0.889908257,0.895412844,0.900917431,0.906422018,
0.911926606,0.917431193,0.92293578,0.930275229,0.937614679,0.943119266,
0.948623853,0.95412844,0.96146789,0.966972477,0.974311927,0.979816514,0.985321101,
0.994495413,1.),.UNSPECIFIED.);
#24343=B_SPLINE_CURVE_WITH_KNOTS('',3,(#175456,#175457,#175458,#175459,
#175460,#175461,#175462,#175463,#175464,#175465,#175466,#175467,#175468,
#175469,#175470,#175471,#175472,#175473,#175474,#175475,#175476,#175477,
#175478,#175479,#175480,#175481,#175482,#175483,#175484,#175485,#175486,
#175487,#175488,#175489,#175490,#175491,#175492,#175493,#175494,#175495,
#175496,#175497,#175498,#175499,#175500,#175501,#175502,#175503,#175504,
#175505,#175506,#175507,#175508,#175509,#175510,#175511,#175512,#175513,
#175514,#175515,#175516,#175517,#175518,#175519,#175520,#175521,#175522,
#175523,#175524,#175525,#175526,#175527,#175528,#175529,#175530,#175531,
#175532,#175533,#175534,#175535,#175536,#175537,#175538,#175539,#175540,
#175541,#175542,#175543,#175544,#175545,#175546,#175547,#175548,#175549,
#175550,#175551,#175552,#175553,#175554,#175555,#175556,#175557,#175558,
#175559,#175560,#175561,#175562,#175563,#175564,#175565,#175566,#175567,
#175568,#175569,#175570,#175571,#175572,#175573,#175574,#175575,#175576,
#175577,#175578,#175579,#175580,#175581,#175582,#175583,#175584,#175585,
#175586,#175587,#175588,#175589,#175590,#175591,#175592,#175593,#175594,
#175595,#175596,#175597,#175598,#175599,#175600,#175601,#175602,#175603,
#175604,#175605,#175606,#175607,#175608,#175609,#175610,#175611,#175612,
#175613,#175614,#175615,#175616,#175617,#175618,#175619,#175620,#175621,
#175622,#175623,#175624,#175625,#175626,#175627,#175628,#175629,#175630,
#175631,#175632,#175633,#175634,#175635,#175636,#175637,#175638,#175639,
#175640,#175641,#175642,#175643,#175644,#175645,#175646,#175647,#175648,
#175649,#175650,#175651,#175652,#175653,#175654,#175655,#175656,#175657,
#175658,#175659,#175660,#175661,#175662,#175663,#175664,#175665,#175666,
#175667,#175668,#175669,#175670,#175671,#175672,#175673,#175674,#175675,
#175676,#175677,#175678,#175679,#175680,#175681,#175682,#175683,#175684,
#175685,#175686,#175687,#175688,#175689,#175690,#175691,#175692,#175693,
#175694,#175695,#175696,#175697,#175698,#175699,#175700,#175701,#175702,
#175703,#175704,#175705,#175706,#175707,#175708,#175709,#175710,#175711,
#175712,#175713,#175714,#175715,#175716,#175717,#175718,#175719,#175720,
#175721,#175722,#175723,#175724,#175725,#175726,#175727,#175728,#175729,
#175730,#175731,#175732,#175733,#175734,#175735,#175736,#175737,#175738,
#175739,#175740,#175741,#175742,#175743,#175744,#175745,#175746,#175747,
#175748,#175749,#175750,#175751,#175752,#175753,#175754,#175755,#175756,
#175757,#175758,#175759,#175760,#175761,#175762,#175763,#175764,#175765,
#175766,#175767,#175768,#175769,#175770,#175771,#175772,#175773,#175774,
#175775,#175776,#175777,#175778,#175779,#175780),.UNSPECIFIED.,.F.,.F.,
(4,3,3,3,3,3,3,3,3,3,3,3,3,3,3,3,3,3,3,3,3,3,3,3,3,3,3,3,3,3,3,3,3,3,3,
3,3,3,3,3,3,3,3,3,3,3,3,3,3,3,3,3,3,3,3,3,3,3,3,3,3,3,3,3,3,3,3,3,3,3,3,
3,3,3,3,3,3,3,3,3,3,3,3,3,3,3,3,3,3,3,3,3,3,3,3,3,3,3,3,3,3,3,3,3,3,3,3,
3,4),(0.143172102,0.15412844,0.165137615,0.176146789,0.187155963,0.198165138,
0.209174312,0.220183486,0.231192661,0.242201835,0.253211009,0.264220183,
0.275229358,0.286238532,0.297247706,0.308256881,0.319266055,0.330275229,
0.341284404,0.352293578,0.363302752,0.374311927,0.385321101,0.396330275,
0.405504587,0.414678899,0.423853211,0.433027523,0.442201835,0.451376147,
0.462385321,0.471559633,0.480733945,0.489908257,0.499082569,0.508256881,
0.517431193,0.526605505,0.533944954,0.541284404,0.548623853,0.555963303,
0.563302752,0.570642202,0.577981651,0.585321101,0.59266055,0.6,0.60733945,
0.614678899,0.622018349,0.631192661,0.63853211,0.64587156,0.655045872,0.662385321,
0.671559633,0.678899083,0.686238532,0.693577982,0.700917431,0.708256881,
0.71559633,0.72293578,0.730275229,0.737614679,0.744954128,0.752293578,0.759633028,
0.766972477,0.774311927,0.781651376,0.788990826,0.796330275,0.803669725,
0.811009174,0.816513761,0.822018349,0.827522936,0.833027523,0.840366972,
0.84587156,0.851376147,0.856880734,0.862385321,0.867889908,0.873394495,
0.878899083,0.88440367,0.889908257,0.895412844,0.900917431,0.906422018,
0.911926606,0.917431193,0.92293578,0.928440367,0.935779817,0.941284404,
0.946788991,0.952293578,0.957798165,0.963302752,0.970642202,0.976146789,
0.983486239,0.988990826,0.994495413,1.),.UNSPECIFIED.);
#24344=B_SPLINE_CURVE_WITH_KNOTS('',3,(#175781,#175782,#175783,#175784,
#175785,#175786,#175787,#175788,#175789,#175790,#175791,#175792,#175793,
#175794,#175795,#175796,#175797,#175798,#175799,#175800,#175801,#175802,
#175803,#175804,#175805,#175806,#175807,#175808,#175809,#175810,#175811,
#175812,#175813,#175814,#175815,#175816,#175817,#175818,#175819,#175820,
#175821,#175822,#175823,#175824,#175825,#175826,#175827,#175828,#175829,
#175830,#175831,#175832,#175833,#175834,#175835,#175836,#175837,#175838,
#175839,#175840,#175841,#175842,#175843,#175844,#175845,#175846,#175847,
#175848,#175849,#175850,#175851,#175852,#175853,#175854,#175855,#175856,
#175857,#175858,#175859,#175860,#175861,#175862,#175863,#175864,#175865,
#175866,#175867,#175868,#175869,#175870,#175871,#175872,#175873,#175874,
#175875,#175876,#175877,#175878,#175879,#175880,#175881,#175882,#175883,
#175884,#175885,#175886,#175887,#175888,#175889,#175890,#175891,#175892,
#175893,#175894,#175895,#175896,#175897,#175898,#175899,#175900,#175901,
#175902,#175903,#175904,#175905,#175906,#175907,#175908,#175909,#175910,
#175911,#175912,#175913,#175914,#175915,#175916,#175917,#175918,#175919,
#175920,#175921,#175922,#175923,#175924,#175925,#175926,#175927,#175928,
#175929,#175930,#175931,#175932,#175933,#175934,#175935,#175936,#175937,
#175938,#175939,#175940,#175941,#175942,#175943,#175944,#175945,#175946,
#175947,#175948,#175949,#175950,#175951,#175952,#175953,#175954,#175955,
#175956,#175957,#175958,#175959,#175960,#175961,#175962,#175963,#175964,
#175965,#175966,#175967,#175968,#175969,#175970,#175971,#175972,#175973,
#175974,#175975,#175976,#175977,#175978,#175979,#175980,#175981,#175982,
#175983,#175984,#175985,#175986,#175987,#175988,#175989,#175990,#175991,
#175992,#175993,#175994,#175995,#175996,#175997,#175998,#175999,#176000,
#176001,#176002,#176003,#176004,#176005,#176006,#176007,#176008,#176009,
#176010,#176011,#176012,#176013,#176014,#176015,#176016,#176017,#176018,
#176019,#176020,#176021,#176022,#176023,#176024,#176025,#176026,#176027,
#176028,#176029,#176030,#176031,#176032,#176033,#176034,#176035,#176036,
#176037,#176038,#176039,#176040,#176041,#176042,#176043,#176044,#176045,
#176046,#176047,#176048,#176049,#176050,#176051,#176052,#176053,#176054,
#176055,#176056,#176057,#176058,#176059,#176060,#176061,#176062,#176063,
#176064,#176065,#176066,#176067,#176068,#176069,#176070,#176071,#176072,
#176073,#176074,#176075,#176076,#176077,#176078,#176079,#176080,#176081,
#176082,#176083,#176084,#176085,#176086,#176087,#176088,#176089,#176090,
#176091,#176092,#176093,#176094,#176095,#176096,#176097,#176098,#176099,
#176100,#176101,#176102,#176103,#176104,#176105,#176106,#176107,#176108),
 .UNSPECIFIED.,.F.,.F.,(4,3,3,3,3,3,3,3,3,3,3,3,3,3,3,3,3,3,3,3,3,3,3,3,
3,3,3,3,3,3,3,3,3,3,3,3,3,3,3,3,3,3,3,3,3,3,3,3,3,3,3,3,3,3,3,3,3,3,3,3,
3,3,3,3,3,3,3,3,3,3,3,3,3,3,3,3,3,3,3,3,3,3,3,3,3,3,3,3,3,3,3,3,3,3,3,3,
3,3,3,3,3,3,3,3,3,3,3,3,3,4),(0.143172102,0.15412844,0.165137615,0.176146789,
0.187155963,0.198165138,0.209174312,0.220183486,0.231192661,0.242201835,
0.253211009,0.264220183,0.275229358,0.286238532,0.297247706,0.308256881,
0.319266055,0.330275229,0.341284404,0.352293578,0.363302752,0.374311927,
0.385321101,0.396330275,0.405504587,0.414678899,0.423853211,0.433027523,
0.442201835,0.451376147,0.460550459,0.469724771,0.478899083,0.488073394,
0.497247706,0.506422018,0.51559633,0.524770642,0.533944954,0.541284404,
0.548623853,0.555963303,0.563302752,0.570642202,0.577981651,0.585321101,
0.59266055,0.6,0.60733945,0.614678899,0.622018349,0.629357798,0.636697248,
0.644036697,0.651376147,0.658715596,0.666055046,0.673394495,0.680733945,
0.688073394,0.695412844,0.704587156,0.711926606,0.719266055,0.726605505,
0.733944954,0.741284404,0.748623853,0.755963303,0.763302752,0.770642202,
0.777981651,0.785321101,0.79266055,0.8,0.809174312,0.814678899,0.820183486,
0.825688073,0.831192661,0.836697248,0.842201835,0.847706422,0.853211009,
0.858715596,0.864220183,0.869724771,0.875229358,0.880733945,0.886238532,
0.891743119,0.897247706,0.902752294,0.908256881,0.913761468,0.919266055,
0.924770642,0.930275229,0.935779817,0.941284404,0.946788991,0.952293578,
0.957798165,0.963302752,0.970642202,0.976146789,0.981651376,0.987155963,
0.99266055,1.),.UNSPECIFIED.);
#24345=B_SPLINE_CURVE_WITH_KNOTS('',3,(#177056,#177057,#177058,#177059,
#177060,#177061,#177062,#177063,#177064,#177065,#177066,#177067,#177068,
#177069,#177070,#177071,#177072,#177073,#177074,#177075,#177076,#177077,
#177078,#177079,#177080,#177081,#177082,#177083,#177084,#177085,#177086,
#177087,#177088,#177089,#177090,#177091,#177092,#177093,#177094,#177095,
#177096,#177097,#177098,#177099,#177100,#177101,#177102,#177103,#177104,
#177105,#177106,#177107,#177108,#177109,#177110,#177111,#177112,#177113,
#177114,#177115,#177116,#177117,#177118,#177119,#177120,#177121,#177122,
#177123,#177124,#177125,#177126,#177127,#177128,#177129,#177130,#177131,
#177132,#177133,#177134,#177135,#177136,#177137,#177138,#177139,#177140,
#177141,#177142,#177143,#177144,#177145,#177146,#177147,#177148,#177149,
#177150,#177151,#177152,#177153,#177154,#177155,#177156,#177157,#177158,
#177159,#177160,#177161,#177162,#177163,#177164,#177165,#177166,#177167,
#177168,#177169,#177170,#177171,#177172,#177173,#177174,#177175,#177176,
#177177,#177178,#177179,#177180,#177181,#177182,#177183,#177184,#177185,
#177186,#177187,#177188,#177189,#177190,#177191,#177192,#177193,#177194,
#177195,#177196,#177197,#177198,#177199,#177200,#177201,#177202,#177203,
#177204,#177205,#177206,#177207,#177208,#177209,#177210,#177211,#177212,
#177213,#177214,#177215,#177216,#177217,#177218,#177219,#177220,#177221,
#177222,#177223,#177224,#177225,#177226,#177227,#177228,#177229,#177230,
#177231,#177232,#177233,#177234,#177235,#177236,#177237,#177238,#177239,
#177240,#177241,#177242,#177243,#177244,#177245,#177246,#177247,#177248,
#177249,#177250,#177251,#177252,#177253,#177254,#177255,#177256,#177257,
#177258,#177259,#177260,#177261,#177262,#177263,#177264,#177265,#177266,
#177267,#177268,#177269,#177270,#177271,#177272,#177273,#177274,#177275,
#177276,#177277,#177278,#177279,#177280,#177281,#177282,#177283,#177284,
#177285,#177286,#177287,#177288,#177289,#177290,#177291,#177292,#177293,
#177294,#177295,#177296,#177297,#177298,#177299,#177300,#177301,#177302,
#177303,#177304,#177305,#177306,#177307,#177308,#177309,#177310,#177311,
#177312,#177313,#177314,#177315,#177316,#177317,#177318,#177319,#177320,
#177321,#177322,#177323,#177324,#177325,#177326,#177327,#177328,#177329,
#177330,#177331,#177332,#177333,#177334,#177335,#177336,#177337,#177338,
#177339,#177340,#177341,#177342,#177343,#177344,#177345,#177346,#177347,
#177348,#177349,#177350,#177351,#177352,#177353,#177354,#177355,#177356,
#177357,#177358,#177359,#177360,#177361,#177362,#177363,#177364,#177365,
#177366,#177367,#177368,#177369,#177370,#177371,#177372,#177373,#177374,
#177375,#177376,#177377,#177378,#177379,#177380),.UNSPECIFIED.,.F.,.F.,
(4,3,3,3,3,3,3,3,3,3,3,3,3,3,3,3,3,3,3,3,3,3,3,3,3,3,3,3,3,3,3,3,3,3,3,
3,3,3,3,3,3,3,3,3,3,3,3,3,3,3,3,3,3,3,3,3,3,3,3,3,3,3,3,3,3,3,3,3,3,3,3,
3,3,3,3,3,3,3,3,3,3,3,3,3,3,3,3,3,3,3,3,3,3,3,3,3,3,3,3,3,3,3,3,3,3,3,3,
3,4),(-0.999999999770594,-0.994495413,-0.988990826,-0.981651376,-0.976146789,
-0.970642202,-0.965137615,-0.957798165,-0.952293578,-0.946788991,-0.941284404,
-0.935779817,-0.930275229,-0.924770642,-0.919266055,-0.913761468,-0.908256881,
-0.902752294,-0.897247706,-0.891743119,-0.886238532,-0.880733945,-0.875229358,
-0.867889908,-0.862385321,-0.856880734,-0.851376147,-0.844036697,-0.83853211,
-0.833027523,-0.827522936,-0.822018349,-0.816513761,-0.811009174,-0.805504587,
-0.798165138,-0.790825688,-0.783486239,-0.776146789,-0.768807339,-0.76146789,
-0.75412844,-0.746788991,-0.737614679,-0.730275229,-0.72293578,-0.713761468,
-0.706422018,-0.699082569,-0.691743119,-0.68440367,-0.67706422,-0.669724771,
-0.662385321,-0.655045872,-0.647706422,-0.640366972,-0.633027523,-0.625688073,
-0.618348624,-0.611009174,-0.603669725,-0.596330275,-0.588990826,-0.581651376,
-0.574311927,-0.566972477,-0.559633028,-0.552293578,-0.544954128,-0.537614679,
-0.530275229,-0.521100917,-0.511926606,-0.502752294,-0.493577982,-0.48440367,
-0.475229358,-0.466055046,-0.456880734,-0.447706422,-0.43853211,-0.429357798,
-0.420183486,-0.411009174,-0.401834862,-0.39266055,-0.381651376,-0.370642202,
-0.359633028,-0.348623853,-0.337614679,-0.326605505,-0.31559633,-0.304587156,
-0.293577982,-0.282568807,-0.271559633,-0.260550459,-0.249541284,-0.23853211,
-0.227522936,-0.216513761,-0.205504587,-0.194495413,-0.183486239,-0.172477064,
-0.16146789,-0.143172102),.UNSPECIFIED.);
#24346=B_SPLINE_CURVE_WITH_KNOTS('',3,(#177381,#177382,#177383,#177384,
#177385,#177386,#177387,#177388,#177389,#177390,#177391,#177392,#177393,
#177394,#177395,#177396,#177397,#177398,#177399,#177400,#177401,#177402,
#177403,#177404,#177405,#177406,#177407,#177408,#177409,#177410,#177411,
#177412,#177413,#177414,#177415,#177416,#177417,#177418,#177419,#177420,
#177421,#177422,#177423,#177424,#177425,#177426,#177427,#177428,#177429,
#177430,#177431,#177432,#177433,#177434,#177435,#177436,#177437,#177438,
#177439,#177440,#177441,#177442,#177443,#177444,#177445,#177446,#177447,
#177448,#177449,#177450,#177451,#177452,#177453,#177454,#177455,#177456,
#177457,#177458,#177459,#177460,#177461,#177462,#177463,#177464,#177465,
#177466,#177467,#177468,#177469,#177470,#177471,#177472,#177473,#177474,
#177475,#177476,#177477,#177478,#177479,#177480,#177481,#177482,#177483,
#177484,#177485,#177486,#177487,#177488,#177489,#177490,#177491,#177492,
#177493,#177494,#177495,#177496,#177497,#177498,#177499,#177500,#177501,
#177502,#177503,#177504,#177505,#177506,#177507,#177508,#177509,#177510,
#177511,#177512,#177513,#177514,#177515,#177516,#177517,#177518,#177519,
#177520,#177521,#177522,#177523,#177524,#177525,#177526,#177527,#177528,
#177529,#177530,#177531,#177532,#177533,#177534,#177535,#177536,#177537,
#177538,#177539,#177540,#177541,#177542,#177543,#177544,#177545,#177546,
#177547,#177548,#177549,#177550,#177551,#177552,#177553,#177554,#177555,
#177556,#177557,#177558,#177559,#177560,#177561,#177562,#177563,#177564,
#177565,#177566,#177567,#177568,#177569,#177570,#177571,#177572,#177573,
#177574,#177575,#177576,#177577,#177578,#177579,#177580,#177581,#177582,
#177583,#177584,#177585,#177586,#177587,#177588,#177589,#177590,#177591,
#177592,#177593,#177594,#177595,#177596,#177597,#177598,#177599,#177600,
#177601,#177602,#177603,#177604,#177605,#177606,#177607,#177608,#177609,
#177610,#177611,#177612,#177613,#177614,#177615,#177616,#177617,#177618,
#177619,#177620,#177621,#177622,#177623,#177624,#177625,#177626,#177627,
#177628,#177629,#177630,#177631,#177632,#177633,#177634,#177635,#177636,
#177637,#177638,#177639,#177640,#177641,#177642,#177643,#177644,#177645,
#177646,#177647,#177648,#177649,#177650,#177651,#177652,#177653,#177654,
#177655,#177656,#177657,#177658,#177659,#177660,#177661,#177662,#177663,
#177664,#177665,#177666,#177667,#177668,#177669,#177670,#177671,#177672,
#177673,#177674,#177675,#177676,#177677,#177678,#177679,#177680,#177681,
#177682,#177683,#177684,#177685,#177686,#177687,#177688,#177689,#177690,
#177691,#177692,#177693,#177694,#177695,#177696,#177697,#177698,#177699,
#177700,#177701,#177702,#177703,#177704,#177705),.UNSPECIFIED.,.F.,.F.,
(4,3,3,3,3,3,3,3,3,3,3,3,3,3,3,3,3,3,3,3,3,3,3,3,3,3,3,3,3,3,3,3,3,3,3,
3,3,3,3,3,3,3,3,3,3,3,3,3,3,3,3,3,3,3,3,3,3,3,3,3,3,3,3,3,3,3,3,3,3,3,3,
3,3,3,3,3,3,3,3,3,3,3,3,3,3,3,3,3,3,3,3,3,3,3,3,3,3,3,3,3,3,3,3,3,3,3,3,
3,4),(0.143172102,0.15412844,0.165137615,0.176146789,0.187155963,0.198165138,
0.209174312,0.220183486,0.231192661,0.242201835,0.253211009,0.264220183,
0.275229358,0.286238532,0.297247706,0.308256881,0.319266055,0.330275229,
0.341284404,0.352293578,0.363302752,0.374311927,0.385321101,0.396330275,
0.405504587,0.414678899,0.423853211,0.433027523,0.442201835,0.451376147,
0.462385321,0.471559633,0.480733945,0.489908257,0.499082569,0.508256881,
0.517431193,0.526605505,0.533944954,0.543119266,0.550458716,0.557798165,
0.565137615,0.572477064,0.581651376,0.588990826,0.596330275,0.605504587,
0.612844037,0.620183486,0.627522936,0.634862385,0.642201835,0.649541284,
0.656880734,0.664220183,0.671559633,0.678899083,0.686238532,0.693577982,
0.700917431,0.708256881,0.71559633,0.72293578,0.730275229,0.737614679,0.744954128,
0.752293578,0.759633028,0.766972477,0.776146789,0.783486239,0.790825688,
0.798165138,0.805504587,0.811009174,0.818348624,0.823853211,0.829357798,
0.834862385,0.840366972,0.84587156,0.851376147,0.856880734,0.862385321,
0.867889908,0.873394495,0.878899083,0.88440367,0.889908257,0.895412844,
0.900917431,0.906422018,0.911926606,0.917431193,0.92293578,0.930275229,
0.935779817,0.941284404,0.946788991,0.952293578,0.957798165,0.963302752,
0.968807339,0.974311927,0.981651376,0.987155963,0.99266055,0.999999999770594),
 .UNSPECIFIED.);
#24347=B_SPLINE_CURVE_WITH_KNOTS('',5,(#178668,#178669,#178670,#178671,
#178672,#178673,#178674,#178675,#178676,#178677,#178678,#178679,#178680,
#178681,#178682,#178683,#178684,#178685,#178686,#178687,#178688,#178689,
#178690,#178691,#178692,#178693,#178694,#178695,#178696,#178697,#178698,
#178699,#178700,#178701,#178702,#178703,#178704,#178705,#178706,#178707,
#178708,#178709,#178710,#178711,#178712,#178713,#178714,#178715,#178716,
#178717,#178718,#178719,#178720,#178721,#178722,#178723,#178724,#178725,
#178726,#178727,#178728,#178729,#178730,#178731,#178732,#178733,#178734,
#178735,#178736,#178737,#178738,#178739,#178740,#178741,#178742,#178743,
#178744,#178745,#178746,#178747,#178748,#178749,#178750,#178751,#178752,
#178753,#178754,#178755,#178756,#178757,#178758,#178759,#178760,#178761,
#178762,#178763,#178764,#178765,#178766,#178767,#178768,#178769,#178770,
#178771,#178772,#178773,#178774,#178775,#178776,#178777,#178778,#178779,
#178780,#178781,#178782,#178783,#178784,#178785,#178786,#178787,#178788,
#178789,#178790,#178791,#178792,#178793,#178794,#178795,#178796,#178797,
#178798,#178799,#178800,#178801,#178802,#178803,#178804,#178805,#178806,
#178807,#178808,#178809,#178810,#178811,#178812,#178813,#178814,#178815,
#178816,#178817,#178818,#178819,#178820,#178821,#178822,#178823,#178824,
#178825,#178826,#178827,#178828,#178829,#178830,#178831,#178832,#178833,
#178834,#178835,#178836,#178837,#178838,#178839,#178840,#178841,#178842,
#178843,#178844,#178845,#178846,#178847,#178848,#178849,#178850,#178851,
#178852,#178853,#178854,#178855,#178856,#178857,#178858,#178859,#178860,
#178861,#178862,#178863,#178864,#178865,#178866,#178867,#178868,#178869,
#178870,#178871,#178872,#178873,#178874,#178875,#178876,#178877,#178878,
#178879,#178880,#178881,#178882,#178883,#178884,#178885,#178886,#178887,
#178888,#178889,#178890,#178891,#178892,#178893,#178894,#178895,#178896,
#178897,#178898,#178899,#178900,#178901,#178902,#178903,#178904,#178905,
#178906,#178907,#178908,#178909,#178910,#178911,#178912,#178913,#178914,
#178915,#178916,#178917,#178918,#178919,#178920,#178921,#178922,#178923,
#178924,#178925,#178926,#178927,#178928,#178929,#178930,#178931,#178932,
#178933,#178934,#178935,#178936,#178937,#178938,#178939,#178940,#178941,
#178942,#178943,#178944,#178945,#178946,#178947,#178948,#178949,#178950,
#178951,#178952,#178953,#178954,#178955,#178956,#178957,#178958,#178959,
#178960,#178961,#178962,#178963,#178964,#178965,#178966,#178967,#178968,
#178969,#178970,#178971,#178972,#178973,#178974,#178975,#178976,#178977,
#178978,#178979,#178980,#178981,#178982,#178983,#178984,#178985,#178986,
#178987,#178988,#178989,#178990,#178991,#178992,#178993,#178994,#178995,
#178996,#178997,#178998,#178999,#179000,#179001,#179002,#179003,#179004,
#179005,#179006,#179007,#179008,#179009,#179010,#179011,#179012,#179013,
#179014,#179015,#179016,#179017,#179018,#179019,#179020,#179021,#179022,
#179023,#179024,#179025,#179026,#179027,#179028,#179029,#179030,#179031,
#179032,#179033,#179034,#179035,#179036,#179037,#179038,#179039,#179040,
#179041,#179042,#179043,#179044,#179045,#179046,#179047,#179048,#179049,
#179050,#179051,#179052,#179053,#179054,#179055,#179056,#179057,#179058,
#179059,#179060,#179061,#179062,#179063,#179064,#179065,#179066,#179067,
#179068,#179069,#179070,#179071,#179072,#179073,#179074,#179075,#179076,
#179077,#179078,#179079,#179080,#179081,#179082,#179083,#179084,#179085,
#179086,#179087,#179088,#179089,#179090,#179091,#179092,#179093,#179094,
#179095,#179096,#179097,#179098,#179099,#179100,#179101,#179102,#179103,
#179104,#179105,#179106,#179107,#179108,#179109,#179110,#179111,#179112,
#179113,#179114,#179115,#179116,#179117,#179118,#179119,#179120,#179121,
#179122,#179123,#179124,#179125,#179126,#179127,#179128,#179129,#179130,
#179131,#179132,#179133,#179134,#179135,#179136,#179137,#179138,#179139),
 .UNSPECIFIED.,.F.,.F.,(6,1,1,1,1,1,1,1,1,1,1,1,1,1,1,1,1,1,1,1,1,1,1,1,
1,1,1,1,1,1,1,1,1,1,1,1,1,1,1,1,1,1,1,1,1,1,1,1,1,1,1,1,1,1,1,1,1,1,1,1,
1,1,1,1,1,1,1,1,1,1,1,1,1,1,1,1,1,1,1,1,1,1,1,1,1,1,1,1,1,1,1,1,1,1,1,1,
1,1,1,1,1,1,1,1,1,1,1,1,1,1,1,1,1,1,1,1,1,1,1,1,1,1,1,1,1,1,1,1,1,1,1,1,
1,1,1,1,1,1,1,1,1,1,1,1,1,1,1,1,1,1,1,1,1,1,1,1,1,1,1,1,1,1,1,1,1,1,1,1,
1,1,1,1,1,1,1,1,1,1,1,1,1,1,1,1,1,1,1,1,1,1,1,1,1,1,1,1,1,1,1,1,1,1,1,1,
1,1,1,1,1,1,1,1,1,1,1,1,1,1,1,1,1,1,1,1,1,1,1,1,1,1,1,1,1,1,1,1,1,1,1,1,
1,1,1,1,1,1,1,1,1,1,1,1,1,1,1,1,1,1,1,1,1,1,1,1,1,1,1,1,1,1,1,1,1,1,1,1,
1,1,1,1,1,1,1,1,1,1,1,1,1,1,1,1,1,1,1,1,1,1,1,1,1,1,1,1,1,1,1,1,1,1,1,1,
1,1,1,1,1,1,1,1,1,1,1,1,1,1,1,1,1,1,1,1,1,1,1,1,1,1,1,1,1,1,1,1,1,1,1,1,
1,1,1,1,1,1,1,1,1,1,1,1,1,1,1,1,1,1,1,1,1,1,1,1,1,1,1,1,1,1,1,1,1,1,1,1,
1,1,1,1,1,1,1,1,1,1,1,1,1,1,1,1,1,1,1,1,1,1,1,1,1,1,1,1,1,1,1,1,1,1,1,1,
1,1,1,1,1,1,1,1,1,1,1,1,1,1,1,1,1,1,1,1,1,1,1,1,1,1,1,1,1,1,1,1,1,1,1,1,
1,1,1,1,1,1,1,1,1,1,1,6),(-1.,-0.998165138,-0.996330275,-0.994495413,-0.99266055,
-0.990825688,-0.988990826,-0.987155963,-0.985321101,-0.983486239,-0.981651376,
-0.979816514,-0.977981651,-0.976146789,-0.974311927,-0.972477064,-0.970642202,
-0.968807339,-0.966972477,-0.965137615,-0.963302752,-0.96146789,-0.959633028,
-0.957798165,-0.955963303,-0.95412844,-0.952293578,-0.950458716,-0.948623853,
-0.946788991,-0.944954128,-0.943119266,-0.941284404,-0.939449541,-0.937614679,
-0.935779817,-0.933944954,-0.932110092,-0.930275229,-0.928440367,-0.926605505,
-0.924770642,-0.92293578,-0.921100917,-0.919266055,-0.917431193,-0.91559633,
-0.913761468,-0.911926606,-0.910091743,-0.908256881,-0.906422018,-0.904587156,
-0.902752294,-0.900917431,-0.899082569,-0.897247706,-0.895412844,-0.893577982,
-0.891743119,-0.889908257,-0.888073394,-0.886238532,-0.88440367,-0.882568807,
-0.880733945,-0.878899083,-0.87706422,-0.875229358,-0.873394495,-0.871559633,
-0.869724771,-0.867889908,-0.866055046,-0.864220183,-0.862385321,-0.860550459,
-0.858715596,-0.856880734,-0.855045872,-0.853211009,-0.851376147,-0.849541284,
-0.847706422,-0.84587156,-0.844036697,-0.842201835,-0.840366972,-0.83853211,
-0.836697248,-0.834862385,-0.833027523,-0.831192661,-0.829357798,-0.827522936,
-0.825688073,-0.823853211,-0.822018349,-0.820183486,-0.818348624,-0.816513761,
-0.814678899,-0.812844037,-0.811009174,-0.809174312,-0.80733945,-0.805504587,
-0.803669725,-0.801834862,-0.8,-0.798165138,-0.796330275,-0.794495413,-0.79266055,
-0.790825688,-0.788990826,-0.787155963,-0.785321101,-0.783486239,-0.781651376,
-0.779816514,-0.777981651,-0.776146789,-0.774311927,-0.772477064,-0.770642202,
-0.768807339,-0.766972477,-0.765137615,-0.763302752,-0.76146789,-0.759633028,
-0.757798165,-0.755963303,-0.75412844,-0.752293578,-0.750458716,-0.748623853,
-0.746788991,-0.744954128,-0.743119266,-0.741284404,-0.739449541,-0.737614679,
-0.735779817,-0.733944954,-0.732110092,-0.730275229,-0.728440367,-0.726605505,
-0.724770642,-0.72293578,-0.721100917,-0.719266055,-0.717431193,-0.71559633,
-0.713761468,-0.711926606,-0.710091743,-0.708256881,-0.706422018,-0.704587156,
-0.702752294,-0.700917431,-0.699082569,-0.697247706,-0.695412844,-0.693577982,
-0.691743119,-0.689908257,-0.688073394,-0.686238532,-0.68440367,-0.682568807,
-0.680733945,-0.678899083,-0.67706422,-0.675229358,-0.673394495,-0.671559633,
-0.669724771,-0.667889908,-0.666055046,-0.664220183,-0.662385321,-0.660550459,
-0.658715596,-0.656880734,-0.655045872,-0.653211009,-0.651376147,-0.649541284,
-0.647706422,-0.64587156,-0.644036697,-0.642201835,-0.640366972,-0.63853211,
-0.636697248,-0.634862385,-0.633027523,-0.631192661,-0.629357798,-0.627522936,
-0.625688073,-0.623853211,-0.622018349,-0.620183486,-0.618348624,-0.616513761,
-0.614678899,-0.612844037,-0.611009174,-0.609174312,-0.60733945,-0.605504587,
-0.603669725,-0.601834862,-0.6,-0.598165138,-0.596330275,-0.594495413,-0.59266055,
-0.590825688,-0.588990826,-0.587155963,-0.585321101,-0.583486239,-0.581651376,
-0.579816514,-0.577981651,-0.576146789,-0.574311927,-0.572477064,-0.570642202,
-0.568807339,-0.566972477,-0.565137615,-0.563302752,-0.56146789,-0.559633028,
-0.557798165,-0.555963303,-0.55412844,-0.552293578,-0.550458716,-0.548623853,
-0.546788991,-0.544954128,-0.543119266,-0.541284404,-0.539449541,-0.537614679,
-0.535779817,-0.533944954,-0.532110092,-0.530275229,-0.528440367,-0.526605505,
-0.524770642,-0.52293578,-0.521100917,-0.519266055,-0.517431193,-0.51559633,
-0.513761468,-0.511926606,-0.510091743,-0.508256881,-0.506422018,-0.504587156,
-0.502752294,-0.500917431,-0.499082569,-0.497247706,-0.495412844,-0.493577982,
-0.491743119,-0.489908257,-0.488073394,-0.486238532,-0.48440367,-0.482568807,
-0.480733945,-0.478899083,-0.47706422,-0.475229358,-0.473394495,-0.471559633,
-0.469724771,-0.467889908,-0.466055046,-0.464220183,-0.462385321,-0.460550459,
-0.458715596,-0.456880734,-0.455045872,-0.453211009,-0.451376147,-0.449541284,
-0.447706422,-0.44587156,-0.444036697,-0.442201835,-0.440366972,-0.43853211,
-0.436697248,-0.434862385,-0.433027523,-0.431192661,-0.429357798,-0.427522936,
-0.425688073,-0.423853211,-0.422018349,-0.420183486,-0.418348624,-0.416513761,
-0.414678899,-0.412844037,-0.411009174,-0.409174312,-0.40733945,-0.405504587,
-0.403669725,-0.401834862,-0.4,-0.398165138,-0.396330275,-0.394495413,-0.39266055,
-0.390825688,-0.388990826,-0.387155963,-0.385321101,-0.383486239,-0.381651376,
-0.379816514,-0.377981651,-0.376146789,-0.374311927,-0.372477064,-0.370642202,
-0.368807339,-0.366972477,-0.365137615,-0.363302752,-0.36146789,-0.359633028,
-0.357798165,-0.355963303,-0.35412844,-0.352293578,-0.350458716,-0.348623853,
-0.346788991,-0.344954128,-0.343119266,-0.341284404,-0.339449541,-0.337614679,
-0.335779817,-0.333944954,-0.332110092,-0.330275229,-0.328440367,-0.326605505,
-0.324770642,-0.32293578,-0.321100917,-0.319266055,-0.317431193,-0.31559633,
-0.313761468,-0.311926606,-0.310091743,-0.308256881,-0.306422018,-0.304587156,
-0.302752294,-0.300917431,-0.299082569,-0.297247706,-0.295412844,-0.293577982,
-0.291743119,-0.289908257,-0.288073394,-0.286238532,-0.28440367,-0.282568807,
-0.280733945,-0.278899083,-0.27706422,-0.275229358,-0.273394495,-0.271559633,
-0.269724771,-0.267889908,-0.266055046,-0.264220183,-0.262385321,-0.260550459,
-0.258715596,-0.256880734,-0.255045872,-0.253211009,-0.251376147,-0.249541284,
-0.247706422,-0.24587156,-0.244036697,-0.242201835,-0.240366972,-0.23853211,
-0.236697248,-0.234862385,-0.233027523,-0.231192661,-0.229357798,-0.227522936,
-0.225688073,-0.223853211,-0.222018349,-0.220183486,-0.218348624,-0.216513761,
-0.214678899,-0.212844037,-0.211009174,-0.209174312,-0.20733945,-0.205504587,
-0.203669725,-0.201834862,-0.2,-0.198165138,-0.196330275,-0.194495413,-0.19266055,
-0.190825688,-0.188990826,-0.187155963,-0.185321101,-0.183486239,-0.181651376,
-0.179816514,-0.177981651,-0.176146789,-0.174311927,-0.172477064,-0.170642202,
-0.168807339,-0.166972477,-0.165137615,-0.163302752,-0.16146789,-0.159633028,
-0.157798165,-0.155963303,-0.15412844,-0.152293578,-0.150458716,-0.148623853,
-0.146788991,-0.144954128,-0.143172102),.UNSPECIFIED.);
#24348=B_SPLINE_CURVE_WITH_KNOTS('',5,(#179140,#179141,#179142,#179143,
#179144,#179145,#179146,#179147,#179148,#179149,#179150,#179151,#179152,
#179153,#179154,#179155,#179156,#179157,#179158,#179159,#179160,#179161,
#179162,#179163,#179164,#179165,#179166,#179167,#179168,#179169,#179170,
#179171,#179172,#179173,#179174,#179175,#179176,#179177,#179178,#179179,
#179180,#179181,#179182,#179183,#179184,#179185,#179186,#179187,#179188,
#179189,#179190,#179191,#179192,#179193,#179194,#179195,#179196,#179197,
#179198,#179199,#179200,#179201,#179202,#179203,#179204,#179205,#179206,
#179207,#179208,#179209,#179210,#179211,#179212,#179213,#179214,#179215,
#179216,#179217,#179218,#179219,#179220,#179221,#179222,#179223,#179224,
#179225,#179226,#179227,#179228,#179229,#179230,#179231,#179232,#179233,
#179234,#179235,#179236,#179237,#179238,#179239,#179240,#179241,#179242,
#179243,#179244,#179245,#179246,#179247,#179248,#179249,#179250,#179251,
#179252,#179253,#179254,#179255,#179256,#179257,#179258,#179259,#179260,
#179261,#179262,#179263,#179264,#179265,#179266,#179267,#179268,#179269,
#179270,#179271,#179272,#179273,#179274,#179275,#179276,#179277,#179278,
#179279,#179280,#179281,#179282,#179283,#179284,#179285,#179286,#179287,
#179288,#179289,#179290,#179291,#179292,#179293,#179294,#179295,#179296,
#179297,#179298,#179299,#179300,#179301,#179302,#179303,#179304,#179305,
#179306,#179307,#179308,#179309,#179310,#179311,#179312,#179313,#179314,
#179315,#179316,#179317,#179318,#179319,#179320,#179321,#179322,#179323,
#179324,#179325,#179326,#179327,#179328,#179329,#179330,#179331,#179332,
#179333,#179334,#179335,#179336,#179337,#179338,#179339,#179340,#179341,
#179342,#179343,#179344,#179345,#179346,#179347,#179348,#179349,#179350,
#179351,#179352,#179353,#179354,#179355,#179356,#179357,#179358,#179359,
#179360,#179361,#179362,#179363,#179364,#179365,#179366,#179367,#179368,
#179369,#179370,#179371,#179372,#179373,#179374,#179375,#179376,#179377,
#179378,#179379,#179380,#179381,#179382,#179383,#179384,#179385,#179386,
#179387,#179388,#179389,#179390,#179391,#179392,#179393,#179394,#179395,
#179396,#179397,#179398,#179399,#179400,#179401,#179402,#179403,#179404,
#179405,#179406,#179407,#179408,#179409,#179410,#179411,#179412,#179413,
#179414,#179415,#179416,#179417,#179418,#179419,#179420,#179421,#179422,
#179423,#179424,#179425,#179426,#179427,#179428,#179429,#179430,#179431,
#179432,#179433,#179434,#179435,#179436,#179437,#179438,#179439,#179440,
#179441,#179442,#179443,#179444,#179445,#179446,#179447,#179448,#179449,
#179450,#179451,#179452,#179453,#179454,#179455,#179456,#179457,#179458,
#179459,#179460,#179461,#179462,#179463,#179464,#179465,#179466,#179467,
#179468,#179469,#179470,#179471,#179472,#179473,#179474,#179475,#179476,
#179477,#179478,#179479,#179480,#179481,#179482,#179483,#179484,#179485,
#179486,#179487,#179488,#179489,#179490,#179491,#179492,#179493,#179494,
#179495,#179496,#179497,#179498,#179499,#179500,#179501,#179502,#179503,
#179504,#179505,#179506,#179507,#179508,#179509,#179510,#179511,#179512,
#179513,#179514,#179515,#179516,#179517,#179518,#179519,#179520,#179521,
#179522,#179523,#179524,#179525,#179526,#179527,#179528,#179529,#179530,
#179531,#179532,#179533,#179534,#179535,#179536,#179537,#179538,#179539,
#179540,#179541,#179542,#179543,#179544,#179545,#179546,#179547,#179548,
#179549,#179550,#179551,#179552,#179553,#179554,#179555,#179556,#179557,
#179558,#179559,#179560,#179561,#179562,#179563,#179564,#179565,#179566,
#179567,#179568,#179569,#179570,#179571,#179572,#179573,#179574,#179575,
#179576,#179577,#179578,#179579,#179580,#179581,#179582,#179583,#179584,
#179585,#179586,#179587,#179588,#179589,#179590,#179591,#179592,#179593,
#179594,#179595,#179596,#179597,#179598,#179599,#179600,#179601,#179602,
#179603,#179604,#179605,#179606,#179607,#179608,#179609,#179610,#179611),
 .UNSPECIFIED.,.F.,.F.,(6,1,1,1,1,1,1,1,1,1,1,1,1,1,1,1,1,1,1,1,1,1,1,1,
1,1,1,1,1,1,1,1,1,1,1,1,1,1,1,1,1,1,1,1,1,1,1,1,1,1,1,1,1,1,1,1,1,1,1,1,
1,1,1,1,1,1,1,1,1,1,1,1,1,1,1,1,1,1,1,1,1,1,1,1,1,1,1,1,1,1,1,1,1,1,1,1,
1,1,1,1,1,1,1,1,1,1,1,1,1,1,1,1,1,1,1,1,1,1,1,1,1,1,1,1,1,1,1,1,1,1,1,1,
1,1,1,1,1,1,1,1,1,1,1,1,1,1,1,1,1,1,1,1,1,1,1,1,1,1,1,1,1,1,1,1,1,1,1,1,
1,1,1,1,1,1,1,1,1,1,1,1,1,1,1,1,1,1,1,1,1,1,1,1,1,1,1,1,1,1,1,1,1,1,1,1,
1,1,1,1,1,1,1,1,1,1,1,1,1,1,1,1,1,1,1,1,1,1,1,1,1,1,1,1,1,1,1,1,1,1,1,1,
1,1,1,1,1,1,1,1,1,1,1,1,1,1,1,1,1,1,1,1,1,1,1,1,1,1,1,1,1,1,1,1,1,1,1,1,
1,1,1,1,1,1,1,1,1,1,1,1,1,1,1,1,1,1,1,1,1,1,1,1,1,1,1,1,1,1,1,1,1,1,1,1,
1,1,1,1,1,1,1,1,1,1,1,1,1,1,1,1,1,1,1,1,1,1,1,1,1,1,1,1,1,1,1,1,1,1,1,1,
1,1,1,1,1,1,1,1,1,1,1,1,1,1,1,1,1,1,1,1,1,1,1,1,1,1,1,1,1,1,1,1,1,1,1,1,
1,1,1,1,1,1,1,1,1,1,1,1,1,1,1,1,1,1,1,1,1,1,1,1,1,1,1,1,1,1,1,1,1,1,1,1,
1,1,1,1,1,1,1,1,1,1,1,1,1,1,1,1,1,1,1,1,1,1,1,1,1,1,1,1,1,1,1,1,1,1,1,1,
1,1,1,1,1,1,1,1,1,1,1,6),(0.143172102,0.144954128,0.146788991,0.148623853,
0.150458716,0.152293578,0.15412844,0.155963303,0.157798165,0.159633028,
0.16146789,0.163302752,0.165137615,0.166972477,0.168807339,0.170642202,
0.172477064,0.174311927,0.176146789,0.177981651,0.179816514,0.181651376,
0.183486239,0.185321101,0.187155963,0.188990826,0.190825688,0.19266055,
0.194495413,0.196330275,0.198165138,0.2,0.201834862,0.203669725,0.205504587,
0.20733945,0.209174312,0.211009174,0.212844037,0.214678899,0.216513761,
0.218348624,0.220183486,0.222018349,0.223853211,0.225688073,0.227522936,
0.229357798,0.231192661,0.233027523,0.234862385,0.236697248,0.23853211,
0.240366972,0.242201835,0.244036697,0.24587156,0.247706422,0.249541284,
0.251376147,0.253211009,0.255045872,0.256880734,0.258715596,0.260550459,
0.262385321,0.264220183,0.266055046,0.267889908,0.269724771,0.271559633,
0.273394495,0.275229358,0.27706422,0.278899083,0.280733945,0.282568807,
0.28440367,0.286238532,0.288073394,0.289908257,0.291743119,0.293577982,
0.295412844,0.297247706,0.299082569,0.300917431,0.302752294,0.304587156,
0.306422018,0.308256881,0.310091743,0.311926606,0.313761468,0.31559633,
0.317431193,0.319266055,0.321100917,0.32293578,0.324770642,0.326605505,
0.328440367,0.330275229,0.332110092,0.333944954,0.335779817,0.337614679,
0.339449541,0.341284404,0.343119266,0.344954128,0.346788991,0.348623853,
0.350458716,0.352293578,0.35412844,0.355963303,0.357798165,0.359633028,
0.36146789,0.363302752,0.365137615,0.366972477,0.368807339,0.370642202,
0.372477064,0.374311927,0.376146789,0.377981651,0.379816514,0.381651376,
0.383486239,0.385321101,0.387155963,0.388990826,0.390825688,0.39266055,
0.394495413,0.396330275,0.398165138,0.4,0.401834862,0.403669725,0.405504587,
0.40733945,0.409174312,0.411009174,0.412844037,0.414678899,0.416513761,
0.418348624,0.420183486,0.422018349,0.423853211,0.425688073,0.427522936,
0.429357798,0.431192661,0.433027523,0.434862385,0.436697248,0.43853211,
0.440366972,0.442201835,0.444036697,0.44587156,0.447706422,0.449541284,
0.451376147,0.453211009,0.455045872,0.456880734,0.458715596,0.460550459,
0.462385321,0.464220183,0.466055046,0.467889908,0.469724771,0.471559633,
0.473394495,0.475229358,0.47706422,0.478899083,0.480733945,0.482568807,
0.48440367,0.486238532,0.488073394,0.489908257,0.491743119,0.493577982,
0.495412844,0.497247706,0.499082569,0.500917431,0.502752294,0.504587156,
0.506422018,0.508256881,0.510091743,0.511926606,0.513761468,0.51559633,
0.517431193,0.519266055,0.521100917,0.52293578,0.524770642,0.526605505,
0.528440367,0.530275229,0.532110092,0.533944954,0.535779817,0.537614679,
0.539449541,0.541284404,0.543119266,0.544954128,0.546788991,0.548623853,
0.550458716,0.552293578,0.55412844,0.555963303,0.557798165,0.559633028,
0.56146789,0.563302752,0.565137615,0.566972477,0.568807339,0.570642202,
0.572477064,0.574311927,0.576146789,0.577981651,0.579816514,0.581651376,
0.583486239,0.585321101,0.587155963,0.588990826,0.590825688,0.59266055,
0.594495413,0.596330275,0.598165138,0.6,0.601834862,0.603669725,0.605504587,
0.60733945,0.609174312,0.611009174,0.612844037,0.614678899,0.616513761,
0.618348624,0.620183486,0.622018349,0.623853211,0.625688073,0.627522936,
0.629357798,0.631192661,0.633027523,0.634862385,0.636697248,0.63853211,
0.640366972,0.642201835,0.644036697,0.64587156,0.647706422,0.649541284,
0.651376147,0.653211009,0.655045872,0.656880734,0.658715596,0.660550459,
0.662385321,0.664220183,0.666055046,0.667889908,0.669724771,0.671559633,
0.673394495,0.675229358,0.67706422,0.678899083,0.680733945,0.682568807,
0.68440367,0.686238532,0.688073394,0.689908257,0.691743119,0.693577982,
0.695412844,0.697247706,0.699082569,0.700917431,0.702752294,0.704587156,
0.706422018,0.708256881,0.710091743,0.711926606,0.713761468,0.71559633,
0.717431193,0.719266055,0.721100917,0.72293578,0.724770642,0.726605505,
0.728440367,0.730275229,0.732110092,0.733944954,0.735779817,0.737614679,
0.739449541,0.741284404,0.743119266,0.744954128,0.746788991,0.748623853,
0.750458716,0.752293578,0.75412844,0.755963303,0.757798165,0.759633028,
0.76146789,0.763302752,0.765137615,0.766972477,0.768807339,0.770642202,
0.772477064,0.774311927,0.776146789,0.777981651,0.779816514,0.781651376,
0.783486239,0.785321101,0.787155963,0.788990826,0.790825688,0.79266055,
0.794495413,0.796330275,0.798165138,0.8,0.801834862,0.803669725,0.805504587,
0.80733945,0.809174312,0.811009174,0.812844037,0.814678899,0.816513761,
0.818348624,0.820183486,0.822018349,0.823853211,0.825688073,0.827522936,
0.829357798,0.831192661,0.833027523,0.834862385,0.836697248,0.83853211,
0.840366972,0.842201835,0.844036697,0.84587156,0.847706422,0.849541284,
0.851376147,0.853211009,0.855045872,0.856880734,0.858715596,0.860550459,
0.862385321,0.864220183,0.866055046,0.867889908,0.869724771,0.871559633,
0.873394495,0.875229358,0.87706422,0.878899083,0.880733945,0.882568807,
0.88440367,0.886238532,0.888073394,0.889908257,0.891743119,0.893577982,
0.895412844,0.897247706,0.899082569,0.900917431,0.902752294,0.904587156,
0.906422018,0.908256881,0.910091743,0.911926606,0.913761468,0.91559633,
0.917431193,0.919266055,0.921100917,0.92293578,0.924770642,0.926605505,
0.928440367,0.930275229,0.932110092,0.933944954,0.935779817,0.937614679,
0.939449541,0.941284404,0.943119266,0.944954128,0.946788991,0.948623853,
0.950458716,0.952293578,0.95412844,0.955963303,0.957798165,0.959633028,
0.96146789,0.963302752,0.965137615,0.966972477,0.968807339,0.970642202,
0.972477064,0.974311927,0.976146789,0.977981651,0.979816514,0.981651376,
0.983486239,0.985321101,0.987155963,0.988990826,0.990825688,0.99266055,
0.994495413,0.996330275,0.998165138,1.),.UNSPECIFIED.);
#24349=B_SPLINE_CURVE_WITH_KNOTS('',3,(#180556,#180557,#180558,#180559,
#180560,#180561,#180562,#180563,#180564,#180565,#180566,#180567,#180568,
#180569,#180570,#180571,#180572,#180573,#180574,#180575,#180576,#180577,
#180578,#180579,#180580,#180581,#180582,#180583,#180584,#180585,#180586,
#180587,#180588,#180589,#180590,#180591,#180592,#180593,#180594,#180595,
#180596,#180597,#180598,#180599,#180600,#180601,#180602,#180603,#180604,
#180605,#180606,#180607,#180608,#180609,#180610,#180611,#180612,#180613,
#180614,#180615,#180616,#180617,#180618,#180619,#180620,#180621,#180622,
#180623,#180624,#180625,#180626,#180627,#180628,#180629,#180630,#180631,
#180632,#180633,#180634,#180635,#180636,#180637,#180638,#180639,#180640,
#180641,#180642,#180643,#180644,#180645,#180646,#180647,#180648,#180649,
#180650,#180651,#180652,#180653,#180654,#180655,#180656,#180657,#180658,
#180659,#180660,#180661,#180662,#180663,#180664,#180665,#180666,#180667,
#180668,#180669,#180670,#180671,#180672,#180673,#180674,#180675,#180676,
#180677,#180678,#180679,#180680,#180681,#180682,#180683,#180684,#180685,
#180686,#180687,#180688,#180689,#180690,#180691,#180692,#180693,#180694,
#180695,#180696,#180697,#180698,#180699,#180700,#180701,#180702,#180703,
#180704,#180705,#180706,#180707,#180708,#180709,#180710,#180711,#180712,
#180713,#180714,#180715,#180716,#180717,#180718,#180719,#180720,#180721,
#180722,#180723,#180724,#180725,#180726,#180727,#180728,#180729,#180730,
#180731,#180732,#180733,#180734,#180735,#180736,#180737,#180738,#180739,
#180740,#180741,#180742,#180743,#180744,#180745,#180746,#180747,#180748,
#180749,#180750,#180751,#180752,#180753,#180754,#180755,#180756,#180757,
#180758,#180759,#180760,#180761,#180762,#180763,#180764,#180765,#180766,
#180767,#180768,#180769,#180770,#180771,#180772,#180773,#180774,#180775,
#180776,#180777,#180778,#180779,#180780,#180781,#180782,#180783,#180784,
#180785,#180786,#180787,#180788,#180789,#180790,#180791,#180792,#180793,
#180794,#180795,#180796,#180797,#180798,#180799,#180800,#180801,#180802,
#180803,#180804,#180805,#180806,#180807,#180808,#180809,#180810,#180811,
#180812,#180813,#180814,#180815,#180816,#180817,#180818,#180819,#180820,
#180821,#180822,#180823,#180824,#180825,#180826,#180827,#180828,#180829,
#180830,#180831,#180832,#180833,#180834,#180835,#180836,#180837,#180838,
#180839,#180840,#180841,#180842,#180843,#180844,#180845,#180846,#180847,
#180848,#180849,#180850,#180851,#180852,#180853,#180854,#180855,#180856,
#180857,#180858,#180859,#180860,#180861,#180862,#180863,#180864,#180865,
#180866,#180867,#180868,#180869,#180870,#180871,#180872,#180873,#180874),
 .UNSPECIFIED.,.F.,.F.,(4,3,3,3,3,3,3,3,3,3,3,3,3,3,3,3,3,3,3,3,3,3,3,3,
3,3,3,3,3,3,3,3,3,3,3,3,3,3,3,3,3,3,3,3,3,3,3,3,3,3,3,3,3,3,3,3,3,3,3,3,
3,3,3,3,3,3,3,3,3,3,3,3,3,3,3,3,3,3,3,3,3,3,3,3,3,3,3,3,3,3,3,3,3,3,3,3,
3,3,3,3,3,3,3,3,3,3,4),(0.143172102,0.15412844,0.165137615,0.176146789,
0.187155963,0.198165138,0.209174312,0.220183486,0.231192661,0.242201835,
0.253211009,0.264220183,0.275229358,0.286238532,0.297247706,0.308256881,
0.319266055,0.330275229,0.341284404,0.352293578,0.365137615,0.376146789,
0.387155963,0.398165138,0.40733945,0.416513761,0.425688073,0.434862385,
0.444036697,0.455045872,0.464220183,0.473394495,0.48440367,0.493577982,
0.502752294,0.511926606,0.521100917,0.530275229,0.537614679,0.544954128,
0.552293578,0.559633028,0.566972477,0.574311927,0.583486239,0.590825688,
0.598165138,0.60733945,0.614678899,0.622018349,0.631192661,0.63853211,0.64587156,
0.655045872,0.662385321,0.671559633,0.678899083,0.686238532,0.693577982,
0.704587156,0.711926606,0.719266055,0.726605505,0.733944954,0.741284404,
0.748623853,0.755963303,0.763302752,0.770642202,0.777981651,0.785321101,
0.79266055,0.8,0.80733945,0.812844037,0.818348624,0.823853211,0.831192661,
0.836697248,0.842201835,0.847706422,0.853211009,0.858715596,0.864220183,
0.869724771,0.875229358,0.880733945,0.886238532,0.891743119,0.897247706,
0.902752294,0.908256881,0.913761468,0.919266055,0.928440367,0.935779817,
0.941284404,0.946788991,0.952293578,0.957798165,0.963302752,0.970642202,
0.976146789,0.983486239,0.988990826,0.994495413,1.),.UNSPECIFIED.);
#24350=B_SPLINE_CURVE_WITH_KNOTS('',3,(#180875,#180876,#180877,#180878,
#180879,#180880,#180881,#180882,#180883,#180884,#180885,#180886,#180887,
#180888,#180889,#180890,#180891,#180892,#180893,#180894,#180895,#180896,
#180897,#180898,#180899,#180900,#180901,#180902,#180903,#180904,#180905,
#180906,#180907,#180908,#180909,#180910,#180911,#180912,#180913,#180914,
#180915,#180916,#180917,#180918,#180919,#180920,#180921,#180922,#180923,
#180924,#180925,#180926,#180927,#180928,#180929,#180930,#180931,#180932,
#180933,#180934,#180935,#180936,#180937,#180938,#180939,#180940,#180941,
#180942,#180943,#180944,#180945,#180946,#180947,#180948,#180949,#180950,
#180951,#180952,#180953,#180954,#180955,#180956,#180957,#180958,#180959,
#180960,#180961,#180962,#180963,#180964,#180965,#180966,#180967,#180968,
#180969,#180970,#180971,#180972,#180973,#180974,#180975,#180976,#180977,
#180978,#180979,#180980,#180981,#180982,#180983,#180984,#180985,#180986,
#180987,#180988,#180989,#180990,#180991,#180992,#180993,#180994,#180995,
#180996,#180997,#180998,#180999,#181000,#181001,#181002,#181003,#181004,
#181005,#181006,#181007,#181008,#181009,#181010,#181011,#181012,#181013,
#181014,#181015,#181016,#181017,#181018,#181019,#181020,#181021,#181022,
#181023,#181024,#181025,#181026,#181027,#181028,#181029,#181030,#181031,
#181032,#181033,#181034,#181035,#181036,#181037,#181038,#181039,#181040,
#181041,#181042,#181043,#181044,#181045,#181046,#181047,#181048,#181049,
#181050,#181051,#181052,#181053,#181054,#181055,#181056,#181057,#181058,
#181059,#181060,#181061,#181062,#181063,#181064,#181065,#181066,#181067,
#181068,#181069,#181070,#181071,#181072,#181073,#181074,#181075,#181076,
#181077,#181078,#181079,#181080,#181081,#181082,#181083,#181084,#181085,
#181086,#181087,#181088,#181089,#181090,#181091,#181092,#181093,#181094,
#181095,#181096,#181097,#181098,#181099,#181100,#181101,#181102,#181103,
#181104,#181105,#181106,#181107,#181108,#181109,#181110,#181111,#181112,
#181113,#181114,#181115,#181116,#181117,#181118,#181119,#181120,#181121,
#181122,#181123,#181124,#181125,#181126,#181127,#181128,#181129,#181130,
#181131,#181132,#181133,#181134,#181135,#181136,#181137,#181138,#181139,
#181140,#181141,#181142,#181143,#181144,#181145,#181146,#181147,#181148,
#181149,#181150,#181151,#181152,#181153,#181154,#181155,#181156,#181157,
#181158,#181159,#181160,#181161,#181162,#181163,#181164,#181165,#181166,
#181167,#181168,#181169,#181170,#181171,#181172,#181173,#181174,#181175,
#181176,#181177,#181178,#181179,#181180,#181181,#181182,#181183,#181184,
#181185,#181186,#181187,#181188,#181189,#181190,#181191,#181192,#181193,
#181194,#181195,#181196),.UNSPECIFIED.,.F.,.F.,(4,3,3,3,3,3,3,3,3,3,3,3,
3,3,3,3,3,3,3,3,3,3,3,3,3,3,3,3,3,3,3,3,3,3,3,3,3,3,3,3,3,3,3,3,3,3,3,3,
3,3,3,3,3,3,3,3,3,3,3,3,3,3,3,3,3,3,3,3,3,3,3,3,3,3,3,3,3,3,3,3,3,3,3,3,
3,3,3,3,3,3,3,3,3,3,3,3,3,3,3,3,3,3,3,3,3,3,3,4),(0.143172102,0.15412844,
0.165137615,0.176146789,0.187155963,0.198165138,0.209174312,0.220183486,
0.231192661,0.242201835,0.253211009,0.264220183,0.275229358,0.286238532,
0.297247706,0.308256881,0.319266055,0.330275229,0.341284404,0.352293578,
0.363302752,0.374311927,0.385321101,0.396330275,0.405504587,0.414678899,
0.423853211,0.433027523,0.442201835,0.451376147,0.460550459,0.469724771,
0.478899083,0.488073394,0.497247706,0.506422018,0.51559633,0.524770642,
0.533944954,0.541284404,0.548623853,0.555963303,0.563302752,0.570642202,
0.579816514,0.588990826,0.596330275,0.603669725,0.611009174,0.618348624,
0.625688073,0.633027523,0.640366972,0.647706422,0.655045872,0.664220183,
0.671559633,0.678899083,0.686238532,0.693577982,0.700917431,0.708256881,
0.71559633,0.72293578,0.730275229,0.737614679,0.744954128,0.752293578,0.759633028,
0.766972477,0.776146789,0.783486239,0.790825688,0.798165138,0.805504587,
0.811009174,0.816513761,0.822018349,0.827522936,0.833027523,0.840366972,
0.84587156,0.853211009,0.858715596,0.864220183,0.869724771,0.875229358,
0.880733945,0.888073394,0.893577982,0.899082569,0.904587156,0.910091743,
0.91559633,0.921100917,0.928440367,0.933944954,0.939449541,0.946788991,
0.952293578,0.957798165,0.963302752,0.968807339,0.974311927,0.979816514,
0.985321101,0.990825688,1.),.UNSPECIFIED.);
#24351=B_SPLINE_CURVE_WITH_KNOTS('',3,(#182156,#182157,#182158,#182159,
#182160,#182161,#182162,#182163,#182164,#182165,#182166,#182167,#182168,
#182169,#182170,#182171,#182172,#182173,#182174,#182175,#182176,#182177,
#182178,#182179,#182180,#182181,#182182,#182183,#182184,#182185,#182186,
#182187,#182188,#182189,#182190,#182191,#182192,#182193,#182194,#182195,
#182196,#182197,#182198,#182199,#182200,#182201,#182202,#182203,#182204,
#182205,#182206,#182207,#182208,#182209,#182210,#182211,#182212,#182213,
#182214,#182215,#182216,#182217,#182218,#182219,#182220,#182221,#182222,
#182223,#182224,#182225,#182226,#182227,#182228,#182229,#182230,#182231,
#182232,#182233,#182234,#182235,#182236,#182237,#182238,#182239,#182240,
#182241,#182242,#182243,#182244,#182245,#182246,#182247,#182248,#182249,
#182250,#182251,#182252,#182253,#182254,#182255,#182256,#182257,#182258,
#182259,#182260,#182261,#182262,#182263,#182264,#182265,#182266,#182267,
#182268,#182269,#182270,#182271,#182272,#182273,#182274,#182275,#182276,
#182277,#182278,#182279,#182280,#182281,#182282,#182283,#182284,#182285,
#182286,#182287,#182288,#182289,#182290,#182291,#182292,#182293,#182294,
#182295,#182296,#182297,#182298,#182299,#182300,#182301,#182302,#182303,
#182304,#182305,#182306,#182307,#182308,#182309,#182310,#182311,#182312,
#182313,#182314,#182315,#182316,#182317,#182318,#182319,#182320,#182321,
#182322,#182323,#182324,#182325,#182326,#182327,#182328,#182329,#182330,
#182331,#182332,#182333,#182334,#182335,#182336,#182337,#182338,#182339,
#182340,#182341,#182342,#182343,#182344,#182345,#182346,#182347,#182348,
#182349,#182350,#182351,#182352,#182353,#182354,#182355,#182356,#182357,
#182358,#182359,#182360,#182361,#182362,#182363,#182364,#182365,#182366,
#182367,#182368,#182369,#182370,#182371,#182372,#182373,#182374,#182375,
#182376,#182377,#182378,#182379,#182380,#182381,#182382,#182383,#182384,
#182385,#182386,#182387,#182388,#182389,#182390,#182391,#182392,#182393,
#182394,#182395,#182396,#182397,#182398,#182399,#182400,#182401,#182402,
#182403,#182404,#182405,#182406,#182407,#182408,#182409,#182410,#182411,
#182412,#182413,#182414,#182415,#182416,#182417,#182418,#182419,#182420,
#182421,#182422,#182423,#182424,#182425,#182426,#182427,#182428,#182429,
#182430,#182431,#182432,#182433,#182434,#182435,#182436,#182437,#182438,
#182439,#182440,#182441,#182442,#182443,#182444,#182445,#182446,#182447,
#182448,#182449,#182450,#182451,#182452,#182453,#182454,#182455,#182456,
#182457,#182458,#182459,#182460,#182461,#182462,#182463,#182464,#182465,
#182466,#182467,#182468,#182469,#182470,#182471),.UNSPECIFIED.,.F.,.F.,
(4,3,3,3,3,3,3,3,3,3,3,3,3,3,3,3,3,3,3,3,3,3,3,3,3,3,3,3,3,3,3,3,3,3,3,
3,3,3,3,3,3,3,3,3,3,3,3,3,3,3,3,3,3,3,3,3,3,3,3,3,3,3,3,3,3,3,3,3,3,3,3,
3,3,3,3,3,3,3,3,3,3,3,3,3,3,3,3,3,3,3,3,3,3,3,3,3,3,3,3,3,3,3,3,3,3,4),
(0.143172102,0.15412844,0.165137615,0.176146789,0.187155963,0.198165138,
0.209174312,0.220183486,0.231192661,0.242201835,0.253211009,0.264220183,
0.275229358,0.286238532,0.297247706,0.308256881,0.319266055,0.330275229,
0.341284404,0.352293578,0.363302752,0.374311927,0.385321101,0.398165138,
0.40733945,0.416513761,0.425688073,0.434862385,0.444036697,0.453211009,
0.462385321,0.471559633,0.480733945,0.489908257,0.499082569,0.508256881,
0.517431193,0.526605505,0.533944954,0.541284404,0.550458716,0.559633028,
0.566972477,0.574311927,0.583486239,0.590825688,0.598165138,0.605504587,
0.612844037,0.620183486,0.627522936,0.634862385,0.64587156,0.653211009,
0.660550459,0.671559633,0.678899083,0.686238532,0.693577982,0.704587156,
0.711926606,0.719266055,0.726605505,0.735779817,0.743119266,0.750458716,
0.759633028,0.766972477,0.774311927,0.783486239,0.790825688,0.798165138,
0.80733945,0.812844037,0.818348624,0.823853211,0.829357798,0.834862385,
0.840366972,0.84587156,0.851376147,0.856880734,0.862385321,0.867889908,
0.873394495,0.878899083,0.88440367,0.889908257,0.895412844,0.900917431,
0.906422018,0.911926606,0.917431193,0.92293578,0.928440367,0.935779817,
0.941284404,0.946788991,0.952293578,0.96146789,0.966972477,0.974311927,
0.979816514,0.985321101,0.990825688,1.),.UNSPECIFIED.);
#24352=B_SPLINE_CURVE_WITH_KNOTS('',3,(#182472,#182473,#182474,#182475,
#182476,#182477,#182478,#182479,#182480,#182481,#182482,#182483,#182484,
#182485,#182486,#182487,#182488,#182489,#182490,#182491,#182492,#182493,
#182494,#182495,#182496,#182497,#182498,#182499,#182500,#182501,#182502,
#182503,#182504,#182505,#182506,#182507,#182508,#182509,#182510,#182511,
#182512,#182513,#182514,#182515,#182516,#182517,#182518,#182519,#182520,
#182521,#182522,#182523,#182524,#182525,#182526,#182527,#182528,#182529,
#182530,#182531,#182532,#182533,#182534,#182535,#182536,#182537,#182538,
#182539,#182540,#182541,#182542,#182543,#182544,#182545,#182546,#182547,
#182548,#182549,#182550,#182551,#182552,#182553,#182554,#182555,#182556,
#182557,#182558,#182559,#182560,#182561,#182562,#182563,#182564,#182565,
#182566,#182567,#182568,#182569,#182570,#182571,#182572,#182573,#182574,
#182575,#182576,#182577,#182578,#182579,#182580,#182581,#182582,#182583,
#182584,#182585,#182586,#182587,#182588,#182589,#182590,#182591,#182592,
#182593,#182594,#182595,#182596,#182597,#182598,#182599,#182600,#182601,
#182602,#182603,#182604,#182605,#182606,#182607,#182608,#182609,#182610,
#182611,#182612,#182613,#182614,#182615,#182616,#182617,#182618,#182619,
#182620,#182621,#182622,#182623,#182624,#182625,#182626,#182627,#182628,
#182629,#182630,#182631,#182632,#182633,#182634,#182635,#182636,#182637,
#182638,#182639,#182640,#182641,#182642,#182643,#182644,#182645,#182646,
#182647,#182648,#182649,#182650,#182651,#182652,#182653,#182654,#182655,
#182656,#182657,#182658,#182659,#182660,#182661,#182662,#182663,#182664,
#182665,#182666,#182667,#182668,#182669,#182670,#182671,#182672,#182673,
#182674,#182675,#182676,#182677,#182678,#182679,#182680,#182681,#182682,
#182683,#182684,#182685,#182686,#182687,#182688,#182689,#182690,#182691,
#182692,#182693,#182694,#182695,#182696,#182697,#182698,#182699,#182700,
#182701,#182702,#182703,#182704,#182705,#182706,#182707,#182708,#182709,
#182710,#182711,#182712,#182713,#182714,#182715,#182716,#182717,#182718,
#182719,#182720,#182721,#182722,#182723,#182724,#182725,#182726,#182727,
#182728,#182729,#182730,#182731,#182732,#182733,#182734,#182735,#182736,
#182737,#182738,#182739,#182740,#182741,#182742,#182743,#182744,#182745,
#182746,#182747,#182748,#182749,#182750,#182751,#182752,#182753,#182754,
#182755,#182756,#182757,#182758,#182759,#182760,#182761,#182762,#182763,
#182764,#182765,#182766,#182767,#182768,#182769,#182770,#182771,#182772,
#182773,#182774,#182775,#182776,#182777,#182778,#182779,#182780,#182781,
#182782,#182783,#182784,#182785,#182786,#182787),.UNSPECIFIED.,.F.,.F.,
(4,3,3,3,3,3,3,3,3,3,3,3,3,3,3,3,3,3,3,3,3,3,3,3,3,3,3,3,3,3,3,3,3,3,3,
3,3,3,3,3,3,3,3,3,3,3,3,3,3,3,3,3,3,3,3,3,3,3,3,3,3,3,3,3,3,3,3,3,3,3,3,
3,3,3,3,3,3,3,3,3,3,3,3,3,3,3,3,3,3,3,3,3,3,3,3,3,3,3,3,3,3,3,3,3,3,4),
(0.143172102,0.15412844,0.165137615,0.176146789,0.187155963,0.198165138,
0.209174312,0.220183486,0.231192661,0.242201835,0.253211009,0.264220183,
0.275229358,0.286238532,0.297247706,0.308256881,0.319266055,0.330275229,
0.341284404,0.352293578,0.363302752,0.374311927,0.385321101,0.396330275,
0.405504587,0.414678899,0.423853211,0.433027523,0.442201835,0.451376147,
0.460550459,0.469724771,0.478899083,0.488073394,0.497247706,0.506422018,
0.51559633,0.524770642,0.533944954,0.543119266,0.550458716,0.557798165,
0.565137615,0.572477064,0.579816514,0.587155963,0.594495413,0.601834862,
0.609174312,0.616513761,0.623853211,0.631192661,0.63853211,0.64587156,0.653211009,
0.662385321,0.669724771,0.67706422,0.68440367,0.691743119,0.700917431,0.710091743,
0.717431193,0.724770642,0.732110092,0.743119266,0.750458716,0.757798165,
0.766972477,0.774311927,0.781651376,0.788990826,0.796330275,0.805504587,
0.811009174,0.818348624,0.823853211,0.829357798,0.834862385,0.842201835,
0.847706422,0.853211009,0.858715596,0.864220183,0.869724771,0.875229358,
0.880733945,0.888073394,0.893577982,0.899082569,0.904587156,0.910091743,
0.91559633,0.921100917,0.930275229,0.935779817,0.941284404,0.946788991,
0.952293578,0.959633028,0.968807339,0.974311927,0.979816514,0.985321101,
0.990825688,1.),.UNSPECIFIED.);
#24353=B_SPLINE_CURVE_WITH_KNOTS('',5,(#183735,#183736,#183737,#183738,
#183739,#183740,#183741,#183742,#183743,#183744,#183745,#183746,#183747,
#183748,#183749,#183750,#183751,#183752,#183753,#183754,#183755,#183756,
#183757,#183758,#183759,#183760,#183761,#183762,#183763,#183764,#183765,
#183766,#183767,#183768,#183769,#183770,#183771,#183772,#183773,#183774,
#183775,#183776,#183777,#183778,#183779,#183780,#183781,#183782,#183783,
#183784,#183785,#183786,#183787,#183788,#183789,#183790,#183791,#183792,
#183793,#183794,#183795,#183796,#183797,#183798,#183799,#183800,#183801,
#183802,#183803,#183804,#183805,#183806,#183807,#183808,#183809,#183810,
#183811,#183812,#183813,#183814,#183815,#183816,#183817,#183818,#183819,
#183820,#183821,#183822,#183823,#183824,#183825,#183826,#183827,#183828,
#183829,#183830,#183831,#183832,#183833,#183834,#183835,#183836,#183837,
#183838,#183839,#183840,#183841,#183842,#183843,#183844,#183845,#183846,
#183847,#183848,#183849,#183850,#183851,#183852,#183853,#183854,#183855,
#183856,#183857,#183858,#183859,#183860,#183861,#183862,#183863,#183864,
#183865,#183866,#183867,#183868,#183869,#183870,#183871,#183872,#183873,
#183874,#183875,#183876,#183877,#183878,#183879,#183880,#183881,#183882,
#183883,#183884,#183885,#183886,#183887,#183888,#183889,#183890,#183891,
#183892,#183893,#183894,#183895,#183896,#183897,#183898,#183899,#183900,
#183901,#183902,#183903,#183904,#183905,#183906,#183907,#183908,#183909,
#183910,#183911,#183912,#183913,#183914,#183915,#183916,#183917,#183918,
#183919,#183920,#183921,#183922,#183923,#183924,#183925,#183926,#183927,
#183928,#183929,#183930,#183931,#183932,#183933,#183934,#183935,#183936,
#183937,#183938,#183939,#183940,#183941,#183942,#183943,#183944,#183945,
#183946,#183947,#183948,#183949,#183950,#183951,#183952,#183953,#183954,
#183955,#183956,#183957,#183958,#183959,#183960,#183961,#183962,#183963,
#183964,#183965,#183966,#183967,#183968,#183969,#183970,#183971,#183972,
#183973,#183974,#183975,#183976,#183977,#183978,#183979,#183980,#183981,
#183982,#183983,#183984,#183985,#183986,#183987,#183988,#183989,#183990,
#183991,#183992,#183993,#183994,#183995,#183996,#183997,#183998,#183999,
#184000,#184001,#184002,#184003,#184004,#184005,#184006,#184007,#184008,
#184009,#184010,#184011,#184012,#184013,#184014,#184015,#184016,#184017,
#184018,#184019,#184020,#184021,#184022,#184023,#184024,#184025,#184026,
#184027,#184028,#184029,#184030,#184031,#184032,#184033,#184034,#184035,
#184036,#184037,#184038,#184039,#184040,#184041,#184042,#184043,#184044,
#184045,#184046,#184047,#184048,#184049,#184050,#184051,#184052,#184053,
#184054,#184055,#184056,#184057,#184058,#184059,#184060,#184061,#184062,
#184063,#184064,#184065,#184066,#184067,#184068,#184069,#184070,#184071,
#184072,#184073,#184074,#184075,#184076,#184077,#184078,#184079,#184080,
#184081,#184082,#184083,#184084,#184085,#184086,#184087,#184088,#184089,
#184090,#184091,#184092,#184093,#184094,#184095,#184096,#184097,#184098,
#184099,#184100,#184101,#184102,#184103,#184104,#184105,#184106,#184107,
#184108,#184109,#184110,#184111,#184112,#184113,#184114,#184115,#184116,
#184117,#184118,#184119,#184120,#184121,#184122,#184123,#184124,#184125,
#184126,#184127,#184128,#184129,#184130,#184131,#184132,#184133,#184134,
#184135,#184136,#184137,#184138,#184139,#184140,#184141,#184142,#184143,
#184144,#184145,#184146,#184147,#184148,#184149,#184150,#184151,#184152,
#184153,#184154,#184155,#184156,#184157,#184158,#184159,#184160,#184161,
#184162,#184163,#184164,#184165,#184166,#184167,#184168,#184169,#184170,
#184171,#184172,#184173,#184174,#184175,#184176,#184177,#184178,#184179,
#184180,#184181,#184182,#184183,#184184,#184185,#184186,#184187,#184188,
#184189,#184190,#184191,#184192,#184193,#184194,#184195,#184196,#184197,
#184198,#184199,#184200,#184201,#184202,#184203,#184204,#184205,#184206),
 .UNSPECIFIED.,.F.,.F.,(6,1,1,1,1,1,1,1,1,1,1,1,1,1,1,1,1,1,1,1,1,1,1,1,
1,1,1,1,1,1,1,1,1,1,1,1,1,1,1,1,1,1,1,1,1,1,1,1,1,1,1,1,1,1,1,1,1,1,1,1,
1,1,1,1,1,1,1,1,1,1,1,1,1,1,1,1,1,1,1,1,1,1,1,1,1,1,1,1,1,1,1,1,1,1,1,1,
1,1,1,1,1,1,1,1,1,1,1,1,1,1,1,1,1,1,1,1,1,1,1,1,1,1,1,1,1,1,1,1,1,1,1,1,
1,1,1,1,1,1,1,1,1,1,1,1,1,1,1,1,1,1,1,1,1,1,1,1,1,1,1,1,1,1,1,1,1,1,1,1,
1,1,1,1,1,1,1,1,1,1,1,1,1,1,1,1,1,1,1,1,1,1,1,1,1,1,1,1,1,1,1,1,1,1,1,1,
1,1,1,1,1,1,1,1,1,1,1,1,1,1,1,1,1,1,1,1,1,1,1,1,1,1,1,1,1,1,1,1,1,1,1,1,
1,1,1,1,1,1,1,1,1,1,1,1,1,1,1,1,1,1,1,1,1,1,1,1,1,1,1,1,1,1,1,1,1,1,1,1,
1,1,1,1,1,1,1,1,1,1,1,1,1,1,1,1,1,1,1,1,1,1,1,1,1,1,1,1,1,1,1,1,1,1,1,1,
1,1,1,1,1,1,1,1,1,1,1,1,1,1,1,1,1,1,1,1,1,1,1,1,1,1,1,1,1,1,1,1,1,1,1,1,
1,1,1,1,1,1,1,1,1,1,1,1,1,1,1,1,1,1,1,1,1,1,1,1,1,1,1,1,1,1,1,1,1,1,1,1,
1,1,1,1,1,1,1,1,1,1,1,1,1,1,1,1,1,1,1,1,1,1,1,1,1,1,1,1,1,1,1,1,1,1,1,1,
1,1,1,1,1,1,1,1,1,1,1,1,1,1,1,1,1,1,1,1,1,1,1,1,1,1,1,1,1,1,1,1,1,1,1,1,
1,1,1,1,1,1,1,1,1,1,1,6),(-1.,-0.998165138,-0.996330275,-0.994495413,-0.99266055,
-0.990825688,-0.988990826,-0.987155963,-0.985321101,-0.983486239,-0.981651376,
-0.979816514,-0.977981651,-0.976146789,-0.974311927,-0.972477064,-0.970642202,
-0.968807339,-0.966972477,-0.965137615,-0.963302752,-0.96146789,-0.959633028,
-0.957798165,-0.955963303,-0.95412844,-0.952293578,-0.950458716,-0.948623853,
-0.946788991,-0.944954128,-0.943119266,-0.941284404,-0.939449541,-0.937614679,
-0.935779817,-0.933944954,-0.932110092,-0.930275229,-0.928440367,-0.926605505,
-0.924770642,-0.92293578,-0.921100917,-0.919266055,-0.917431193,-0.91559633,
-0.913761468,-0.911926606,-0.910091743,-0.908256881,-0.906422018,-0.904587156,
-0.902752294,-0.900917431,-0.899082569,-0.897247706,-0.895412844,-0.893577982,
-0.891743119,-0.889908257,-0.888073394,-0.886238532,-0.88440367,-0.882568807,
-0.880733945,-0.878899083,-0.87706422,-0.875229358,-0.873394495,-0.871559633,
-0.869724771,-0.867889908,-0.866055046,-0.864220183,-0.862385321,-0.860550459,
-0.858715596,-0.856880734,-0.855045872,-0.853211009,-0.851376147,-0.849541284,
-0.847706422,-0.84587156,-0.844036697,-0.842201835,-0.840366972,-0.83853211,
-0.836697248,-0.834862385,-0.833027523,-0.831192661,-0.829357798,-0.827522936,
-0.825688073,-0.823853211,-0.822018349,-0.820183486,-0.818348624,-0.816513761,
-0.814678899,-0.812844037,-0.811009174,-0.809174312,-0.80733945,-0.805504587,
-0.803669725,-0.801834862,-0.8,-0.798165138,-0.796330275,-0.794495413,-0.79266055,
-0.790825688,-0.788990826,-0.787155963,-0.785321101,-0.783486239,-0.781651376,
-0.779816514,-0.777981651,-0.776146789,-0.774311927,-0.772477064,-0.770642202,
-0.768807339,-0.766972477,-0.765137615,-0.763302752,-0.76146789,-0.759633028,
-0.757798165,-0.755963303,-0.75412844,-0.752293578,-0.750458716,-0.748623853,
-0.746788991,-0.744954128,-0.743119266,-0.741284404,-0.739449541,-0.737614679,
-0.735779817,-0.733944954,-0.732110092,-0.730275229,-0.728440367,-0.726605505,
-0.724770642,-0.72293578,-0.721100917,-0.719266055,-0.717431193,-0.71559633,
-0.713761468,-0.711926606,-0.710091743,-0.708256881,-0.706422018,-0.704587156,
-0.702752294,-0.700917431,-0.699082569,-0.697247706,-0.695412844,-0.693577982,
-0.691743119,-0.689908257,-0.688073394,-0.686238532,-0.68440367,-0.682568807,
-0.680733945,-0.678899083,-0.67706422,-0.675229358,-0.673394495,-0.671559633,
-0.669724771,-0.667889908,-0.666055046,-0.664220183,-0.662385321,-0.660550459,
-0.658715596,-0.656880734,-0.655045872,-0.653211009,-0.651376147,-0.649541284,
-0.647706422,-0.64587156,-0.644036697,-0.642201835,-0.640366972,-0.63853211,
-0.636697248,-0.634862385,-0.633027523,-0.631192661,-0.629357798,-0.627522936,
-0.625688073,-0.623853211,-0.622018349,-0.620183486,-0.618348624,-0.616513761,
-0.614678899,-0.612844037,-0.611009174,-0.609174312,-0.60733945,-0.605504587,
-0.603669725,-0.601834862,-0.6,-0.598165138,-0.596330275,-0.594495413,-0.59266055,
-0.590825688,-0.588990826,-0.587155963,-0.585321101,-0.583486239,-0.581651376,
-0.579816514,-0.577981651,-0.576146789,-0.574311927,-0.572477064,-0.570642202,
-0.568807339,-0.566972477,-0.565137615,-0.563302752,-0.56146789,-0.559633028,
-0.557798165,-0.555963303,-0.55412844,-0.552293578,-0.550458716,-0.548623853,
-0.546788991,-0.544954128,-0.543119266,-0.541284404,-0.539449541,-0.537614679,
-0.535779817,-0.533944954,-0.532110092,-0.530275229,-0.528440367,-0.526605505,
-0.524770642,-0.52293578,-0.521100917,-0.519266055,-0.517431193,-0.51559633,
-0.513761468,-0.511926606,-0.510091743,-0.508256881,-0.506422018,-0.504587156,
-0.502752294,-0.500917431,-0.499082569,-0.497247706,-0.495412844,-0.493577982,
-0.491743119,-0.489908257,-0.488073394,-0.486238532,-0.48440367,-0.482568807,
-0.480733945,-0.478899083,-0.47706422,-0.475229358,-0.473394495,-0.471559633,
-0.469724771,-0.467889908,-0.466055046,-0.464220183,-0.462385321,-0.460550459,
-0.458715596,-0.456880734,-0.455045872,-0.453211009,-0.451376147,-0.449541284,
-0.447706422,-0.44587156,-0.444036697,-0.442201835,-0.440366972,-0.43853211,
-0.436697248,-0.434862385,-0.433027523,-0.431192661,-0.429357798,-0.427522936,
-0.425688073,-0.423853211,-0.422018349,-0.420183486,-0.418348624,-0.416513761,
-0.414678899,-0.412844037,-0.411009174,-0.409174312,-0.40733945,-0.405504587,
-0.403669725,-0.401834862,-0.4,-0.398165138,-0.396330275,-0.394495413,-0.39266055,
-0.390825688,-0.388990826,-0.387155963,-0.385321101,-0.383486239,-0.381651376,
-0.379816514,-0.377981651,-0.376146789,-0.374311927,-0.372477064,-0.370642202,
-0.368807339,-0.366972477,-0.365137615,-0.363302752,-0.36146789,-0.359633028,
-0.357798165,-0.355963303,-0.35412844,-0.352293578,-0.350458716,-0.348623853,
-0.346788991,-0.344954128,-0.343119266,-0.341284404,-0.339449541,-0.337614679,
-0.335779817,-0.333944954,-0.332110092,-0.330275229,-0.328440367,-0.326605505,
-0.324770642,-0.32293578,-0.321100917,-0.319266055,-0.317431193,-0.31559633,
-0.313761468,-0.311926606,-0.310091743,-0.308256881,-0.306422018,-0.304587156,
-0.302752294,-0.300917431,-0.299082569,-0.297247706,-0.295412844,-0.293577982,
-0.291743119,-0.289908257,-0.288073394,-0.286238532,-0.28440367,-0.282568807,
-0.280733945,-0.278899083,-0.27706422,-0.275229358,-0.273394495,-0.271559633,
-0.269724771,-0.267889908,-0.266055046,-0.264220183,-0.262385321,-0.260550459,
-0.258715596,-0.256880734,-0.255045872,-0.253211009,-0.251376147,-0.249541284,
-0.247706422,-0.24587156,-0.244036697,-0.242201835,-0.240366972,-0.23853211,
-0.236697248,-0.234862385,-0.233027523,-0.231192661,-0.229357798,-0.227522936,
-0.225688073,-0.223853211,-0.222018349,-0.220183486,-0.218348624,-0.216513761,
-0.214678899,-0.212844037,-0.211009174,-0.209174312,-0.20733945,-0.205504587,
-0.203669725,-0.201834862,-0.2,-0.198165138,-0.196330275,-0.194495413,-0.19266055,
-0.190825688,-0.188990826,-0.187155963,-0.185321101,-0.183486239,-0.181651376,
-0.179816514,-0.177981651,-0.176146789,-0.174311927,-0.172477064,-0.170642202,
-0.168807339,-0.166972477,-0.165137615,-0.163302752,-0.16146789,-0.159633028,
-0.157798165,-0.155963303,-0.15412844,-0.152293578,-0.150458716,-0.148623853,
-0.146788991,-0.144954128,-0.143172102),.UNSPECIFIED.);
#24354=B_SPLINE_CURVE_WITH_KNOTS('',5,(#184207,#184208,#184209,#184210,
#184211,#184212,#184213,#184214,#184215,#184216,#184217,#184218,#184219,
#184220,#184221,#184222,#184223,#184224,#184225,#184226,#184227,#184228,
#184229,#184230,#184231,#184232,#184233,#184234,#184235,#184236,#184237,
#184238,#184239,#184240,#184241,#184242,#184243,#184244,#184245,#184246,
#184247,#184248,#184249,#184250,#184251,#184252,#184253,#184254,#184255,
#184256,#184257,#184258,#184259,#184260,#184261,#184262,#184263,#184264,
#184265,#184266,#184267,#184268,#184269,#184270,#184271,#184272,#184273,
#184274,#184275,#184276,#184277,#184278,#184279,#184280,#184281,#184282,
#184283,#184284,#184285,#184286,#184287,#184288,#184289,#184290,#184291,
#184292,#184293,#184294,#184295,#184296,#184297,#184298,#184299,#184300,
#184301,#184302,#184303,#184304,#184305,#184306,#184307,#184308,#184309,
#184310,#184311,#184312,#184313,#184314,#184315,#184316,#184317,#184318,
#184319,#184320,#184321,#184322,#184323,#184324,#184325,#184326,#184327,
#184328,#184329,#184330,#184331,#184332,#184333,#184334,#184335,#184336,
#184337,#184338,#184339,#184340,#184341,#184342,#184343,#184344,#184345,
#184346,#184347,#184348,#184349,#184350,#184351,#184352,#184353,#184354,
#184355,#184356,#184357,#184358,#184359,#184360,#184361,#184362,#184363,
#184364,#184365,#184366,#184367,#184368,#184369,#184370,#184371,#184372,
#184373,#184374,#184375,#184376,#184377,#184378,#184379,#184380,#184381,
#184382,#184383,#184384,#184385,#184386,#184387,#184388,#184389,#184390,
#184391,#184392,#184393,#184394,#184395,#184396,#184397,#184398,#184399,
#184400,#184401,#184402,#184403,#184404,#184405,#184406,#184407,#184408,
#184409,#184410,#184411,#184412,#184413,#184414,#184415,#184416,#184417,
#184418,#184419,#184420,#184421,#184422,#184423,#184424,#184425,#184426,
#184427,#184428,#184429,#184430,#184431,#184432,#184433,#184434,#184435,
#184436,#184437,#184438,#184439,#184440,#184441,#184442,#184443,#184444,
#184445,#184446,#184447,#184448,#184449,#184450,#184451,#184452,#184453,
#184454,#184455,#184456,#184457,#184458,#184459,#184460,#184461,#184462,
#184463,#184464,#184465,#184466,#184467,#184468,#184469,#184470,#184471,
#184472,#184473,#184474,#184475,#184476,#184477,#184478,#184479,#184480,
#184481,#184482,#184483,#184484,#184485,#184486,#184487,#184488,#184489,
#184490,#184491,#184492,#184493,#184494,#184495,#184496,#184497,#184498,
#184499,#184500,#184501,#184502,#184503,#184504,#184505,#184506,#184507,
#184508,#184509,#184510,#184511,#184512,#184513,#184514,#184515,#184516,
#184517,#184518,#184519,#184520,#184521,#184522,#184523,#184524,#184525,
#184526,#184527,#184528,#184529,#184530,#184531,#184532,#184533,#184534,
#184535,#184536,#184537,#184538,#184539,#184540,#184541,#184542,#184543,
#184544,#184545,#184546,#184547,#184548,#184549,#184550,#184551,#184552,
#184553,#184554,#184555,#184556,#184557,#184558,#184559,#184560,#184561,
#184562,#184563,#184564,#184565,#184566,#184567,#184568,#184569,#184570,
#184571,#184572,#184573,#184574,#184575,#184576,#184577,#184578,#184579,
#184580,#184581,#184582,#184583,#184584,#184585,#184586,#184587,#184588,
#184589,#184590,#184591,#184592,#184593,#184594,#184595,#184596,#184597,
#184598,#184599,#184600,#184601,#184602,#184603,#184604,#184605,#184606,
#184607,#184608,#184609,#184610,#184611,#184612,#184613,#184614,#184615,
#184616,#184617,#184618,#184619,#184620,#184621,#184622,#184623,#184624,
#184625,#184626,#184627,#184628,#184629,#184630,#184631,#184632,#184633,
#184634,#184635,#184636,#184637,#184638,#184639,#184640,#184641,#184642,
#184643,#184644,#184645,#184646,#184647,#184648,#184649,#184650,#184651,
#184652,#184653,#184654,#184655,#184656,#184657,#184658,#184659,#184660,
#184661,#184662,#184663,#184664,#184665,#184666,#184667,#184668,#184669,
#184670,#184671,#184672,#184673,#184674,#184675,#184676,#184677,#184678),
 .UNSPECIFIED.,.F.,.F.,(6,1,1,1,1,1,1,1,1,1,1,1,1,1,1,1,1,1,1,1,1,1,1,1,
1,1,1,1,1,1,1,1,1,1,1,1,1,1,1,1,1,1,1,1,1,1,1,1,1,1,1,1,1,1,1,1,1,1,1,1,
1,1,1,1,1,1,1,1,1,1,1,1,1,1,1,1,1,1,1,1,1,1,1,1,1,1,1,1,1,1,1,1,1,1,1,1,
1,1,1,1,1,1,1,1,1,1,1,1,1,1,1,1,1,1,1,1,1,1,1,1,1,1,1,1,1,1,1,1,1,1,1,1,
1,1,1,1,1,1,1,1,1,1,1,1,1,1,1,1,1,1,1,1,1,1,1,1,1,1,1,1,1,1,1,1,1,1,1,1,
1,1,1,1,1,1,1,1,1,1,1,1,1,1,1,1,1,1,1,1,1,1,1,1,1,1,1,1,1,1,1,1,1,1,1,1,
1,1,1,1,1,1,1,1,1,1,1,1,1,1,1,1,1,1,1,1,1,1,1,1,1,1,1,1,1,1,1,1,1,1,1,1,
1,1,1,1,1,1,1,1,1,1,1,1,1,1,1,1,1,1,1,1,1,1,1,1,1,1,1,1,1,1,1,1,1,1,1,1,
1,1,1,1,1,1,1,1,1,1,1,1,1,1,1,1,1,1,1,1,1,1,1,1,1,1,1,1,1,1,1,1,1,1,1,1,
1,1,1,1,1,1,1,1,1,1,1,1,1,1,1,1,1,1,1,1,1,1,1,1,1,1,1,1,1,1,1,1,1,1,1,1,
1,1,1,1,1,1,1,1,1,1,1,1,1,1,1,1,1,1,1,1,1,1,1,1,1,1,1,1,1,1,1,1,1,1,1,1,
1,1,1,1,1,1,1,1,1,1,1,1,1,1,1,1,1,1,1,1,1,1,1,1,1,1,1,1,1,1,1,1,1,1,1,1,
1,1,1,1,1,1,1,1,1,1,1,1,1,1,1,1,1,1,1,1,1,1,1,1,1,1,1,1,1,1,1,1,1,1,1,1,
1,1,1,1,1,1,1,1,1,1,1,6),(0.143172102,0.144954128,0.146788991,0.148623853,
0.150458716,0.152293578,0.15412844,0.155963303,0.157798165,0.159633028,
0.16146789,0.163302752,0.165137615,0.166972477,0.168807339,0.170642202,
0.172477064,0.174311927,0.176146789,0.177981651,0.179816514,0.181651376,
0.183486239,0.185321101,0.187155963,0.188990826,0.190825688,0.19266055,
0.194495413,0.196330275,0.198165138,0.2,0.201834862,0.203669725,0.205504587,
0.20733945,0.209174312,0.211009174,0.212844037,0.214678899,0.216513761,
0.218348624,0.220183486,0.222018349,0.223853211,0.225688073,0.227522936,
0.229357798,0.231192661,0.233027523,0.234862385,0.236697248,0.23853211,
0.240366972,0.242201835,0.244036697,0.24587156,0.247706422,0.249541284,
0.251376147,0.253211009,0.255045872,0.256880734,0.258715596,0.260550459,
0.262385321,0.264220183,0.266055046,0.267889908,0.269724771,0.271559633,
0.273394495,0.275229358,0.27706422,0.278899083,0.280733945,0.282568807,
0.28440367,0.286238532,0.288073394,0.289908257,0.291743119,0.293577982,
0.295412844,0.297247706,0.299082569,0.300917431,0.302752294,0.304587156,
0.306422018,0.308256881,0.310091743,0.311926606,0.313761468,0.31559633,
0.317431193,0.319266055,0.321100917,0.32293578,0.324770642,0.326605505,
0.328440367,0.330275229,0.332110092,0.333944954,0.335779817,0.337614679,
0.339449541,0.341284404,0.343119266,0.344954128,0.346788991,0.348623853,
0.350458716,0.352293578,0.35412844,0.355963303,0.357798165,0.359633028,
0.36146789,0.363302752,0.365137615,0.366972477,0.368807339,0.370642202,
0.372477064,0.374311927,0.376146789,0.377981651,0.379816514,0.381651376,
0.383486239,0.385321101,0.387155963,0.388990826,0.390825688,0.39266055,
0.394495413,0.396330275,0.398165138,0.4,0.401834862,0.403669725,0.405504587,
0.40733945,0.409174312,0.411009174,0.412844037,0.414678899,0.416513761,
0.418348624,0.420183486,0.422018349,0.423853211,0.425688073,0.427522936,
0.429357798,0.431192661,0.433027523,0.434862385,0.436697248,0.43853211,
0.440366972,0.442201835,0.444036697,0.44587156,0.447706422,0.449541284,
0.451376147,0.453211009,0.455045872,0.456880734,0.458715596,0.460550459,
0.462385321,0.464220183,0.466055046,0.467889908,0.469724771,0.471559633,
0.473394495,0.475229358,0.47706422,0.478899083,0.480733945,0.482568807,
0.48440367,0.486238532,0.488073394,0.489908257,0.491743119,0.493577982,
0.495412844,0.497247706,0.499082569,0.500917431,0.502752294,0.504587156,
0.506422018,0.508256881,0.510091743,0.511926606,0.513761468,0.51559633,
0.517431193,0.519266055,0.521100917,0.52293578,0.524770642,0.526605505,
0.528440367,0.530275229,0.532110092,0.533944954,0.535779817,0.537614679,
0.539449541,0.541284404,0.543119266,0.544954128,0.546788991,0.548623853,
0.550458716,0.552293578,0.55412844,0.555963303,0.557798165,0.559633028,
0.56146789,0.563302752,0.565137615,0.566972477,0.568807339,0.570642202,
0.572477064,0.574311927,0.576146789,0.577981651,0.579816514,0.581651376,
0.583486239,0.585321101,0.587155963,0.588990826,0.590825688,0.59266055,
0.594495413,0.596330275,0.598165138,0.6,0.601834862,0.603669725,0.605504587,
0.60733945,0.609174312,0.611009174,0.612844037,0.614678899,0.616513761,
0.618348624,0.620183486,0.622018349,0.623853211,0.625688073,0.627522936,
0.629357798,0.631192661,0.633027523,0.634862385,0.636697248,0.63853211,
0.640366972,0.642201835,0.644036697,0.64587156,0.647706422,0.649541284,
0.651376147,0.653211009,0.655045872,0.656880734,0.658715596,0.660550459,
0.662385321,0.664220183,0.666055046,0.667889908,0.669724771,0.671559633,
0.673394495,0.675229358,0.67706422,0.678899083,0.680733945,0.682568807,
0.68440367,0.686238532,0.688073394,0.689908257,0.691743119,0.693577982,
0.695412844,0.697247706,0.699082569,0.700917431,0.702752294,0.704587156,
0.706422018,0.708256881,0.710091743,0.711926606,0.713761468,0.71559633,
0.717431193,0.719266055,0.721100917,0.72293578,0.724770642,0.726605505,
0.728440367,0.730275229,0.732110092,0.733944954,0.735779817,0.737614679,
0.739449541,0.741284404,0.743119266,0.744954128,0.746788991,0.748623853,
0.750458716,0.752293578,0.75412844,0.755963303,0.757798165,0.759633028,
0.76146789,0.763302752,0.765137615,0.766972477,0.768807339,0.770642202,
0.772477064,0.774311927,0.776146789,0.777981651,0.779816514,0.781651376,
0.783486239,0.785321101,0.787155963,0.788990826,0.790825688,0.79266055,
0.794495413,0.796330275,0.798165138,0.8,0.801834862,0.803669725,0.805504587,
0.80733945,0.809174312,0.811009174,0.812844037,0.814678899,0.816513761,
0.818348624,0.820183486,0.822018349,0.823853211,0.825688073,0.827522936,
0.829357798,0.831192661,0.833027523,0.834862385,0.836697248,0.83853211,
0.840366972,0.842201835,0.844036697,0.84587156,0.847706422,0.849541284,
0.851376147,0.853211009,0.855045872,0.856880734,0.858715596,0.860550459,
0.862385321,0.864220183,0.866055046,0.867889908,0.869724771,0.871559633,
0.873394495,0.875229358,0.87706422,0.878899083,0.880733945,0.882568807,
0.88440367,0.886238532,0.888073394,0.889908257,0.891743119,0.893577982,
0.895412844,0.897247706,0.899082569,0.900917431,0.902752294,0.904587156,
0.906422018,0.908256881,0.910091743,0.911926606,0.913761468,0.91559633,
0.917431193,0.919266055,0.921100917,0.92293578,0.924770642,0.926605505,
0.928440367,0.930275229,0.932110092,0.933944954,0.935779817,0.937614679,
0.939449541,0.941284404,0.943119266,0.944954128,0.946788991,0.948623853,
0.950458716,0.952293578,0.95412844,0.955963303,0.957798165,0.959633028,
0.96146789,0.963302752,0.965137615,0.966972477,0.968807339,0.970642202,
0.972477064,0.974311927,0.976146789,0.977981651,0.979816514,0.981651376,
0.983486239,0.985321101,0.987155963,0.988990826,0.990825688,0.99266055,
0.994495413,0.996330275,0.998165138,1.),.UNSPECIFIED.);
#24355=B_SPLINE_CURVE_WITH_KNOTS('',3,(#185641,#185642,#185643,#185644,
#185645,#185646,#185647,#185648,#185649,#185650,#185651,#185652,#185653,
#185654,#185655,#185656,#185657,#185658,#185659,#185660,#185661,#185662,
#185663,#185664,#185665,#185666,#185667,#185668,#185669,#185670,#185671,
#185672,#185673,#185674,#185675,#185676,#185677,#185678,#185679,#185680,
#185681,#185682,#185683,#185684,#185685,#185686,#185687,#185688,#185689,
#185690,#185691,#185692,#185693,#185694,#185695,#185696,#185697,#185698,
#185699,#185700,#185701,#185702,#185703,#185704,#185705,#185706,#185707,
#185708,#185709,#185710,#185711,#185712,#185713,#185714,#185715,#185716,
#185717,#185718,#185719,#185720,#185721,#185722,#185723,#185724,#185725,
#185726,#185727,#185728,#185729,#185730,#185731,#185732,#185733,#185734,
#185735,#185736,#185737,#185738,#185739,#185740,#185741,#185742,#185743,
#185744,#185745,#185746,#185747,#185748,#185749,#185750,#185751,#185752,
#185753,#185754,#185755,#185756,#185757,#185758,#185759,#185760,#185761,
#185762,#185763,#185764,#185765,#185766,#185767,#185768,#185769,#185770,
#185771,#185772,#185773,#185774,#185775,#185776,#185777,#185778,#185779,
#185780,#185781,#185782,#185783,#185784,#185785,#185786,#185787,#185788,
#185789,#185790,#185791,#185792,#185793,#185794,#185795,#185796,#185797,
#185798,#185799,#185800,#185801,#185802,#185803,#185804,#185805,#185806,
#185807,#185808,#185809,#185810,#185811,#185812,#185813,#185814,#185815,
#185816,#185817,#185818,#185819,#185820,#185821,#185822,#185823,#185824,
#185825,#185826,#185827,#185828,#185829,#185830,#185831,#185832,#185833,
#185834,#185835,#185836,#185837,#185838,#185839,#185840,#185841,#185842,
#185843,#185844,#185845,#185846,#185847,#185848,#185849,#185850,#185851,
#185852,#185853,#185854,#185855,#185856,#185857,#185858,#185859,#185860,
#185861,#185862,#185863,#185864,#185865,#185866,#185867,#185868,#185869,
#185870,#185871,#185872,#185873,#185874,#185875,#185876,#185877,#185878,
#185879,#185880,#185881,#185882,#185883,#185884,#185885,#185886,#185887,
#185888,#185889,#185890,#185891,#185892,#185893,#185894,#185895,#185896,
#185897,#185898,#185899,#185900,#185901,#185902,#185903,#185904,#185905,
#185906,#185907,#185908,#185909,#185910,#185911,#185912,#185913,#185914,
#185915,#185916,#185917,#185918,#185919,#185920,#185921,#185922,#185923,
#185924,#185925,#185926,#185927,#185928,#185929,#185930,#185931,#185932,
#185933,#185934,#185935,#185936,#185937,#185938,#185939,#185940,#185941,
#185942,#185943,#185944,#185945,#185946,#185947,#185948,#185949,#185950,
#185951,#185952,#185953,#185954,#185955,#185956,#185957,#185958,#185959,
#185960,#185961,#185962,#185963,#185964,#185965,#185966,#185967,#185968),
 .UNSPECIFIED.,.F.,.F.,(4,3,3,3,3,3,3,3,3,3,3,3,3,3,3,3,3,3,3,3,3,3,3,3,
3,3,3,3,3,3,3,3,3,3,3,3,3,3,3,3,3,3,3,3,3,3,3,3,3,3,3,3,3,3,3,3,3,3,3,3,
3,3,3,3,3,3,3,3,3,3,3,3,3,3,3,3,3,3,3,3,3,3,3,3,3,3,3,3,3,3,3,3,3,3,3,3,
3,3,3,3,3,3,3,3,3,3,3,3,3,4),(-1.,-0.994495413,-0.988990826,-0.983486239,
-0.977981651,-0.972477064,-0.966972477,-0.959633028,-0.95412844,-0.948623853,
-0.943119266,-0.937614679,-0.932110092,-0.926605505,-0.921100917,-0.91559633,
-0.910091743,-0.904587156,-0.899082569,-0.893577982,-0.888073394,-0.882568807,
-0.87706422,-0.871559633,-0.866055046,-0.860550459,-0.855045872,-0.849541284,
-0.842201835,-0.836697248,-0.831192661,-0.825688073,-0.818348624,-0.812844037,
-0.80733945,-0.8,-0.79266055,-0.785321101,-0.777981651,-0.770642202,-0.763302752,
-0.755963303,-0.748623853,-0.741284404,-0.733944954,-0.726605505,-0.719266055,
-0.711926606,-0.704587156,-0.697247706,-0.689908257,-0.682568807,-0.675229358,
-0.667889908,-0.660550459,-0.653211009,-0.64587156,-0.63853211,-0.631192661,
-0.623853211,-0.616513761,-0.609174312,-0.601834862,-0.59266055,-0.585321101,
-0.577981651,-0.570642202,-0.563302752,-0.555963303,-0.548623853,-0.541284404,
-0.533944954,-0.526605505,-0.517431193,-0.508256881,-0.499082569,-0.489908257,
-0.480733945,-0.471559633,-0.462385321,-0.453211009,-0.444036697,-0.434862385,
-0.425688073,-0.414678899,-0.405504587,-0.396330275,-0.387155963,-0.374311927,
-0.363302752,-0.352293578,-0.341284404,-0.330275229,-0.319266055,-0.308256881,
-0.297247706,-0.286238532,-0.275229358,-0.264220183,-0.253211009,-0.242201835,
-0.231192661,-0.220183486,-0.209174312,-0.198165138,-0.187155963,-0.176146789,
-0.165137615,-0.15412844,-0.143172102),.UNSPECIFIED.);
#24356=B_SPLINE_CURVE_WITH_KNOTS('',3,(#185969,#185970,#185971,#185972,
#185973,#185974,#185975,#185976,#185977,#185978,#185979,#185980,#185981,
#185982,#185983,#185984,#185985,#185986,#185987,#185988,#185989,#185990,
#185991,#185992,#185993,#185994,#185995,#185996,#185997,#185998,#185999,
#186000,#186001,#186002,#186003,#186004,#186005,#186006,#186007,#186008,
#186009,#186010,#186011,#186012,#186013,#186014,#186015,#186016,#186017,
#186018,#186019,#186020,#186021,#186022,#186023,#186024,#186025,#186026,
#186027,#186028,#186029,#186030,#186031,#186032,#186033,#186034,#186035,
#186036,#186037,#186038,#186039,#186040,#186041,#186042,#186043,#186044,
#186045,#186046,#186047,#186048,#186049,#186050,#186051,#186052,#186053,
#186054,#186055,#186056,#186057,#186058,#186059,#186060,#186061,#186062,
#186063,#186064,#186065,#186066,#186067,#186068,#186069,#186070,#186071,
#186072,#186073,#186074,#186075,#186076,#186077,#186078,#186079,#186080,
#186081,#186082,#186083,#186084,#186085,#186086,#186087,#186088,#186089,
#186090,#186091,#186092,#186093,#186094,#186095,#186096,#186097,#186098,
#186099,#186100,#186101,#186102,#186103,#186104,#186105,#186106,#186107,
#186108,#186109,#186110,#186111,#186112,#186113,#186114,#186115,#186116,
#186117,#186118,#186119,#186120,#186121,#186122,#186123,#186124,#186125,
#186126,#186127,#186128,#186129,#186130,#186131,#186132,#186133,#186134,
#186135,#186136,#186137,#186138,#186139,#186140,#186141,#186142,#186143,
#186144,#186145,#186146,#186147,#186148,#186149,#186150,#186151,#186152,
#186153,#186154,#186155,#186156,#186157,#186158,#186159,#186160,#186161,
#186162,#186163,#186164,#186165,#186166,#186167,#186168,#186169,#186170,
#186171,#186172,#186173,#186174,#186175,#186176,#186177,#186178,#186179,
#186180,#186181,#186182,#186183,#186184,#186185,#186186,#186187,#186188,
#186189,#186190,#186191,#186192,#186193,#186194,#186195,#186196,#186197,
#186198,#186199,#186200,#186201,#186202,#186203,#186204,#186205,#186206,
#186207,#186208,#186209,#186210,#186211,#186212,#186213,#186214,#186215,
#186216,#186217,#186218,#186219,#186220,#186221,#186222,#186223,#186224,
#186225,#186226,#186227,#186228,#186229,#186230,#186231,#186232,#186233,
#186234,#186235,#186236,#186237,#186238,#186239,#186240,#186241,#186242,
#186243,#186244,#186245,#186246,#186247,#186248,#186249,#186250,#186251,
#186252,#186253,#186254,#186255,#186256,#186257,#186258,#186259,#186260,
#186261,#186262,#186263,#186264,#186265,#186266,#186267,#186268,#186269,
#186270,#186271,#186272,#186273,#186274,#186275,#186276,#186277,#186278),
 .UNSPECIFIED.,.F.,.F.,(4,3,3,3,3,3,3,3,3,3,3,3,3,3,3,3,3,3,3,3,3,3,3,3,
3,3,3,3,3,3,3,3,3,3,3,3,3,3,3,3,3,3,3,3,3,3,3,3,3,3,3,3,3,3,3,3,3,3,3,3,
3,3,3,3,3,3,3,3,3,3,3,3,3,3,3,3,3,3,3,3,3,3,3,3,3,3,3,3,3,3,3,3,3,3,3,3,
3,3,3,3,3,3,3,4),(0.143172102,0.15412844,0.165137615,0.176146789,0.187155963,
0.198165138,0.209174312,0.220183486,0.231192661,0.242201835,0.253211009,
0.264220183,0.275229358,0.286238532,0.297247706,0.308256881,0.319266055,
0.330275229,0.341284404,0.352293578,0.363302752,0.374311927,0.388990826,
0.398165138,0.40733945,0.416513761,0.425688073,0.434862385,0.444036697,
0.453211009,0.462385321,0.473394495,0.482568807,0.491743119,0.504587156,
0.51559633,0.524770642,0.533944954,0.541284404,0.548623853,0.555963303,
0.563302752,0.570642202,0.577981651,0.585321101,0.59266055,0.601834862,
0.609174312,0.616513761,0.625688073,0.633027523,0.640366972,0.649541284,
0.658715596,0.666055046,0.673394495,0.680733945,0.688073394,0.695412844,
0.706422018,0.713761468,0.721100917,0.730275229,0.739449541,0.746788991,
0.75412844,0.76146789,0.768807339,0.777981651,0.785321101,0.79266055,0.8,
0.80733945,0.812844037,0.818348624,0.823853211,0.829357798,0.836697248,
0.842201835,0.849541284,0.855045872,0.860550459,0.866055046,0.871559633,
0.878899083,0.888073394,0.893577982,0.899082569,0.904587156,0.910091743,
0.917431193,0.924770642,0.930275229,0.939449541,0.944954128,0.950458716,
0.955963303,0.96146789,0.966972477,0.972477064,0.977981651,0.985321101,
0.99266055,1.),.UNSPECIFIED.);
#24357=B_SPLINE_CURVE_WITH_KNOTS('',3,(#187223,#187224,#187225,#187226,
#187227,#187228,#187229,#187230,#187231,#187232,#187233,#187234,#187235,
#187236,#187237,#187238,#187239,#187240,#187241,#187242,#187243,#187244,
#187245,#187246,#187247,#187248,#187249,#187250,#187251,#187252,#187253,
#187254,#187255,#187256,#187257,#187258,#187259,#187260,#187261,#187262,
#187263,#187264,#187265,#187266,#187267,#187268,#187269,#187270,#187271,
#187272,#187273,#187274,#187275,#187276,#187277,#187278,#187279,#187280,
#187281,#187282,#187283,#187284,#187285,#187286,#187287,#187288,#187289,
#187290,#187291,#187292,#187293,#187294,#187295,#187296,#187297,#187298,
#187299,#187300,#187301,#187302,#187303,#187304,#187305,#187306,#187307,
#187308,#187309,#187310,#187311,#187312,#187313,#187314,#187315,#187316,
#187317,#187318,#187319,#187320,#187321,#187322,#187323,#187324,#187325,
#187326,#187327,#187328,#187329,#187330,#187331,#187332,#187333,#187334,
#187335,#187336,#187337,#187338,#187339,#187340,#187341,#187342,#187343,
#187344,#187345,#187346,#187347,#187348,#187349,#187350,#187351,#187352,
#187353,#187354,#187355,#187356,#187357,#187358,#187359,#187360,#187361,
#187362,#187363,#187364,#187365,#187366,#187367,#187368,#187369,#187370,
#187371,#187372,#187373,#187374,#187375,#187376,#187377,#187378,#187379,
#187380,#187381,#187382,#187383,#187384,#187385,#187386,#187387,#187388,
#187389,#187390,#187391,#187392,#187393,#187394,#187395,#187396,#187397,
#187398,#187399,#187400,#187401,#187402,#187403,#187404,#187405,#187406,
#187407,#187408,#187409,#187410,#187411,#187412,#187413,#187414,#187415,
#187416,#187417,#187418,#187419,#187420,#187421,#187422,#187423,#187424,
#187425,#187426,#187427,#187428,#187429,#187430,#187431,#187432,#187433,
#187434,#187435,#187436,#187437,#187438,#187439,#187440,#187441,#187442,
#187443,#187444,#187445,#187446,#187447,#187448,#187449,#187450,#187451,
#187452,#187453,#187454,#187455,#187456,#187457,#187458,#187459,#187460,
#187461,#187462,#187463,#187464,#187465,#187466,#187467,#187468,#187469,
#187470,#187471,#187472,#187473,#187474,#187475,#187476,#187477,#187478,
#187479,#187480,#187481,#187482,#187483,#187484,#187485,#187486,#187487,
#187488,#187489,#187490,#187491,#187492,#187493,#187494,#187495,#187496,
#187497,#187498,#187499,#187500,#187501,#187502,#187503,#187504,#187505,
#187506,#187507,#187508,#187509,#187510,#187511,#187512,#187513,#187514,
#187515,#187516,#187517,#187518,#187519,#187520,#187521,#187522,#187523,
#187524,#187525,#187526,#187527,#187528,#187529,#187530,#187531,#187532,
#187533,#187534,#187535,#187536,#187537,#187538,#187539,#187540,#187541,
#187542,#187543,#187544),.UNSPECIFIED.,.F.,.F.,(4,3,3,3,3,3,3,3,3,3,3,3,
3,3,3,3,3,3,3,3,3,3,3,3,3,3,3,3,3,3,3,3,3,3,3,3,3,3,3,3,3,3,3,3,3,3,3,3,
3,3,3,3,3,3,3,3,3,3,3,3,3,3,3,3,3,3,3,3,3,3,3,3,3,3,3,3,3,3,3,3,3,3,3,3,
3,3,3,3,3,3,3,3,3,3,3,3,3,3,3,3,3,3,3,3,3,3,3,4),(0.143172102,0.15412844,
0.165137615,0.176146789,0.187155963,0.198165138,0.209174312,0.222018349,
0.233027523,0.244036697,0.255045872,0.266055046,0.27706422,0.288073394,
0.299082569,0.311926606,0.32293578,0.335779817,0.346788991,0.357798165,
0.368807339,0.379816514,0.390825688,0.4,0.409174312,0.418348624,0.427522936,
0.436697248,0.44587156,0.455045872,0.464220183,0.473394495,0.482568807,
0.491743119,0.500917431,0.510091743,0.519266055,0.528440367,0.535779817,
0.543119266,0.550458716,0.557798165,0.565137615,0.572477064,0.579816514,
0.587155963,0.594495413,0.601834862,0.609174312,0.616513761,0.623853211,
0.631192661,0.63853211,0.64587156,0.655045872,0.662385321,0.671559633,0.678899083,
0.686238532,0.693577982,0.700917431,0.708256881,0.71559633,0.72293578,0.730275229,
0.737614679,0.746788991,0.75412844,0.76146789,0.768807339,0.776146789,0.783486239,
0.790825688,0.798165138,0.805504587,0.811009174,0.818348624,0.823853211,
0.831192661,0.836697248,0.842201835,0.847706422,0.855045872,0.860550459,
0.869724771,0.875229358,0.880733945,0.886238532,0.891743119,0.897247706,
0.902752294,0.908256881,0.913761468,0.919266055,0.926605505,0.932110092,
0.937614679,0.943119266,0.948623853,0.95412844,0.959633028,0.966972477,
0.972477064,0.977981651,0.983486239,0.988990826,0.994495413,1.),
 .UNSPECIFIED.);
#24358=B_SPLINE_CURVE_WITH_KNOTS('',3,(#187545,#187546,#187547,#187548,
#187549,#187550,#187551,#187552,#187553,#187554,#187555,#187556,#187557,
#187558,#187559,#187560,#187561,#187562,#187563,#187564,#187565,#187566,
#187567,#187568,#187569,#187570,#187571,#187572,#187573,#187574,#187575,
#187576,#187577,#187578,#187579,#187580,#187581,#187582,#187583,#187584,
#187585,#187586,#187587,#187588,#187589,#187590,#187591,#187592,#187593,
#187594,#187595,#187596,#187597,#187598,#187599,#187600,#187601,#187602,
#187603,#187604,#187605,#187606,#187607,#187608,#187609,#187610,#187611,
#187612,#187613,#187614,#187615,#187616,#187617,#187618,#187619,#187620,
#187621,#187622,#187623,#187624,#187625,#187626,#187627,#187628,#187629,
#187630,#187631,#187632,#187633,#187634,#187635,#187636,#187637,#187638,
#187639,#187640,#187641,#187642,#187643,#187644,#187645,#187646,#187647,
#187648,#187649,#187650,#187651,#187652,#187653,#187654,#187655,#187656,
#187657,#187658,#187659,#187660,#187661,#187662,#187663,#187664,#187665,
#187666,#187667,#187668,#187669,#187670,#187671,#187672,#187673,#187674,
#187675,#187676,#187677,#187678,#187679,#187680,#187681,#187682,#187683,
#187684,#187685,#187686,#187687,#187688,#187689,#187690,#187691,#187692,
#187693,#187694,#187695,#187696,#187697,#187698,#187699,#187700,#187701,
#187702,#187703,#187704,#187705,#187706,#187707,#187708,#187709,#187710,
#187711,#187712,#187713,#187714,#187715,#187716,#187717,#187718,#187719,
#187720,#187721,#187722,#187723,#187724,#187725,#187726,#187727,#187728,
#187729,#187730,#187731,#187732,#187733,#187734,#187735,#187736,#187737,
#187738,#187739,#187740,#187741,#187742,#187743,#187744,#187745,#187746,
#187747,#187748,#187749,#187750,#187751,#187752,#187753,#187754,#187755,
#187756,#187757,#187758,#187759,#187760,#187761,#187762,#187763,#187764,
#187765,#187766,#187767,#187768,#187769,#187770,#187771,#187772,#187773,
#187774,#187775,#187776,#187777,#187778,#187779,#187780,#187781,#187782,
#187783,#187784,#187785,#187786,#187787,#187788,#187789,#187790,#187791,
#187792,#187793,#187794,#187795,#187796,#187797,#187798,#187799,#187800,
#187801,#187802,#187803,#187804,#187805,#187806,#187807,#187808,#187809,
#187810,#187811,#187812,#187813,#187814,#187815,#187816,#187817,#187818,
#187819,#187820,#187821,#187822,#187823,#187824,#187825,#187826,#187827,
#187828,#187829,#187830,#187831,#187832,#187833,#187834,#187835,#187836,
#187837,#187838,#187839,#187840,#187841,#187842,#187843,#187844,#187845,
#187846,#187847,#187848,#187849,#187850,#187851,#187852,#187853,#187854,
#187855,#187856,#187857,#187858,#187859,#187860,#187861,#187862,#187863,
#187864,#187865,#187866),.UNSPECIFIED.,.F.,.F.,(4,3,3,3,3,3,3,3,3,3,3,3,
3,3,3,3,3,3,3,3,3,3,3,3,3,3,3,3,3,3,3,3,3,3,3,3,3,3,3,3,3,3,3,3,3,3,3,3,
3,3,3,3,3,3,3,3,3,3,3,3,3,3,3,3,3,3,3,3,3,3,3,3,3,3,3,3,3,3,3,3,3,3,3,3,
3,3,3,3,3,3,3,3,3,3,3,3,3,3,3,3,3,3,3,3,3,3,3,4),(0.143172102,0.15412844,
0.165137615,0.176146789,0.187155963,0.198165138,0.209174312,0.220183486,
0.231192661,0.242201835,0.253211009,0.264220183,0.275229358,0.286238532,
0.297247706,0.308256881,0.319266055,0.330275229,0.341284404,0.352293578,
0.363302752,0.374311927,0.385321101,0.398165138,0.40733945,0.416513761,
0.425688073,0.434862385,0.444036697,0.453211009,0.464220183,0.473394495,
0.48440367,0.493577982,0.502752294,0.511926606,0.521100917,0.530275229,
0.537614679,0.544954128,0.552293578,0.559633028,0.566972477,0.574311927,
0.581651376,0.588990826,0.596330275,0.603669725,0.612844037,0.620183486,
0.627522936,0.634862385,0.642201835,0.649541284,0.656880734,0.664220183,
0.673394495,0.680733945,0.688073394,0.695412844,0.704587156,0.711926606,
0.719266055,0.726605505,0.733944954,0.741284404,0.748623853,0.755963303,
0.763302752,0.770642202,0.777981651,0.785321101,0.79266055,0.8,0.809174312,
0.814678899,0.820183486,0.825688073,0.831192661,0.836697248,0.842201835,
0.847706422,0.853211009,0.858715596,0.864220183,0.869724771,0.875229358,
0.880733945,0.888073394,0.893577982,0.899082569,0.904587156,0.910091743,
0.91559633,0.921100917,0.930275229,0.935779817,0.941284404,0.946788991,
0.952293578,0.957798165,0.963302752,0.968807339,0.974311927,0.979816514,
0.985321101,0.990825688,1.),.UNSPECIFIED.);
#24359=B_SPLINE_CURVE_WITH_KNOTS('',3,(#188826,#188827,#188828,#188829,
#188830,#188831,#188832,#188833,#188834,#188835,#188836,#188837,#188838,
#188839,#188840,#188841,#188842,#188843,#188844,#188845,#188846,#188847,
#188848,#188849,#188850,#188851,#188852,#188853,#188854,#188855,#188856,
#188857,#188858,#188859,#188860,#188861,#188862,#188863,#188864,#188865,
#188866,#188867,#188868,#188869,#188870,#188871,#188872,#188873,#188874,
#188875,#188876,#188877,#188878,#188879,#188880,#188881,#188882,#188883,
#188884,#188885,#188886,#188887,#188888,#188889,#188890,#188891,#188892,
#188893,#188894,#188895,#188896,#188897,#188898,#188899,#188900,#188901,
#188902,#188903,#188904,#188905,#188906,#188907,#188908,#188909,#188910,
#188911,#188912,#188913,#188914,#188915,#188916,#188917,#188918,#188919,
#188920,#188921,#188922,#188923,#188924,#188925,#188926,#188927,#188928,
#188929,#188930,#188931,#188932,#188933,#188934,#188935,#188936,#188937,
#188938,#188939,#188940,#188941,#188942,#188943,#188944,#188945,#188946,
#188947,#188948,#188949,#188950,#188951,#188952,#188953,#188954,#188955,
#188956,#188957,#188958,#188959,#188960,#188961,#188962,#188963,#188964,
#188965,#188966,#188967,#188968,#188969,#188970,#188971,#188972,#188973,
#188974,#188975,#188976,#188977,#188978,#188979,#188980,#188981,#188982,
#188983,#188984,#188985,#188986,#188987,#188988,#188989,#188990,#188991,
#188992,#188993,#188994,#188995,#188996,#188997,#188998,#188999,#189000,
#189001,#189002,#189003,#189004,#189005,#189006,#189007,#189008,#189009,
#189010,#189011,#189012,#189013,#189014,#189015,#189016,#189017,#189018,
#189019,#189020,#189021,#189022,#189023,#189024,#189025,#189026,#189027,
#189028,#189029,#189030,#189031,#189032,#189033,#189034,#189035,#189036,
#189037,#189038,#189039,#189040,#189041,#189042,#189043,#189044,#189045,
#189046,#189047,#189048,#189049,#189050,#189051,#189052,#189053,#189054,
#189055,#189056,#189057,#189058,#189059,#189060,#189061,#189062,#189063,
#189064,#189065,#189066,#189067,#189068,#189069,#189070,#189071,#189072,
#189073,#189074,#189075,#189076,#189077,#189078,#189079,#189080,#189081,
#189082,#189083,#189084,#189085,#189086,#189087,#189088,#189089,#189090,
#189091,#189092,#189093,#189094,#189095,#189096,#189097,#189098,#189099,
#189100,#189101,#189102,#189103,#189104,#189105,#189106,#189107,#189108,
#189109,#189110,#189111,#189112,#189113,#189114),.UNSPECIFIED.,.F.,.F.,
(4,3,3,3,3,3,3,3,3,3,3,3,3,3,3,3,3,3,3,3,3,3,3,3,3,3,3,3,3,3,3,3,3,3,3,
3,3,3,3,3,3,3,3,3,3,3,3,3,3,3,3,3,3,3,3,3,3,3,3,3,3,3,3,3,3,3,3,3,3,3,3,
3,3,3,3,3,3,3,3,3,3,3,3,3,3,3,3,3,3,3,3,3,3,3,3,3,4),(0.143172102,0.15412844,
0.165137615,0.177981651,0.188990826,0.2,0.212844037,0.223853211,0.234862385,
0.24587156,0.256880734,0.267889908,0.278899083,0.289908257,0.300917431,
0.31559633,0.328440367,0.341284404,0.352293578,0.365137615,0.376146789,
0.39266055,0.403669725,0.416513761,0.427522936,0.43853211,0.449541284,0.460550459,
0.469724771,0.480733945,0.493577982,0.504587156,0.51559633,0.524770642,
0.533944954,0.541284404,0.550458716,0.557798165,0.565137615,0.572477064,
0.583486239,0.590825688,0.598165138,0.60733945,0.614678899,0.622018349,
0.629357798,0.640366972,0.651376147,0.660550459,0.667889908,0.67706422,
0.686238532,0.693577982,0.700917431,0.713761468,0.726605505,0.733944954,
0.743119266,0.750458716,0.757798165,0.765137615,0.772477064,0.779816514,
0.788990826,0.798165138,0.80733945,0.812844037,0.818348624,0.825688073,
0.831192661,0.83853211,0.84587156,0.851376147,0.858715596,0.864220183,0.871559633,
0.87706422,0.88440367,0.893577982,0.900917431,0.910091743,0.91559633,0.92293578,
0.928440367,0.935779817,0.941284404,0.948623853,0.95412844,0.96146789,0.966972477,
0.972477064,0.977981651,0.983486239,0.988990826,0.994495413,1.),
 .UNSPECIFIED.);
#24360=B_SPLINE_CURVE_WITH_KNOTS('',3,(#189115,#189116,#189117,#189118,
#189119,#189120,#189121,#189122,#189123,#189124,#189125,#189126,#189127,
#189128,#189129,#189130,#189131,#189132,#189133,#189134,#189135,#189136,
#189137,#189138,#189139,#189140,#189141,#189142,#189143,#189144,#189145,
#189146,#189147,#189148,#189149,#189150,#189151,#189152,#189153,#189154,
#189155,#189156,#189157,#189158,#189159,#189160,#189161,#189162,#189163,
#189164,#189165,#189166,#189167,#189168,#189169,#189170,#189171,#189172,
#189173,#189174,#189175,#189176,#189177,#189178,#189179,#189180,#189181,
#189182,#189183,#189184,#189185,#189186,#189187,#189188,#189189,#189190,
#189191,#189192,#189193,#189194,#189195,#189196,#189197,#189198,#189199,
#189200,#189201,#189202,#189203,#189204,#189205,#189206,#189207,#189208,
#189209,#189210,#189211,#189212,#189213,#189214,#189215,#189216,#189217,
#189218,#189219,#189220,#189221,#189222,#189223,#189224,#189225,#189226,
#189227,#189228,#189229,#189230,#189231,#189232,#189233,#189234,#189235,
#189236,#189237,#189238,#189239,#189240,#189241,#189242,#189243,#189244,
#189245,#189246,#189247,#189248,#189249,#189250,#189251,#189252,#189253,
#189254,#189255,#189256,#189257,#189258,#189259,#189260,#189261,#189262,
#189263,#189264,#189265,#189266,#189267,#189268,#189269,#189270,#189271,
#189272,#189273,#189274,#189275,#189276,#189277,#189278,#189279,#189280,
#189281,#189282,#189283,#189284,#189285,#189286,#189287,#189288,#189289,
#189290,#189291,#189292,#189293,#189294,#189295,#189296,#189297,#189298,
#189299,#189300,#189301,#189302,#189303,#189304,#189305,#189306,#189307,
#189308,#189309,#189310,#189311,#189312,#189313,#189314,#189315,#189316,
#189317,#189318,#189319,#189320,#189321,#189322,#189323,#189324,#189325,
#189326,#189327,#189328,#189329,#189330,#189331,#189332,#189333,#189334,
#189335,#189336,#189337,#189338,#189339,#189340,#189341,#189342,#189343,
#189344,#189345,#189346,#189347,#189348,#189349,#189350,#189351,#189352,
#189353,#189354,#189355,#189356,#189357,#189358,#189359,#189360,#189361,
#189362,#189363,#189364,#189365,#189366,#189367,#189368,#189369,#189370,
#189371,#189372,#189373,#189374,#189375,#189376,#189377,#189378,#189379,
#189380,#189381,#189382,#189383,#189384,#189385,#189386,#189387,#189388,
#189389,#189390,#189391,#189392,#189393,#189394,#189395,#189396,#189397,
#189398,#189399,#189400,#189401,#189402,#189403,#189404,#189405,#189406,
#189407,#189408,#189409,#189410,#189411,#189412,#189413,#189414,#189415,
#189416,#189417,#189418,#189419,#189420,#189421,#189422,#189423,#189424,
#189425,#189426,#189427,#189428,#189429,#189430,#189431,#189432,#189433),
 .UNSPECIFIED.,.F.,.F.,(4,3,3,3,3,3,3,3,3,3,3,3,3,3,3,3,3,3,3,3,3,3,3,3,
3,3,3,3,3,3,3,3,3,3,3,3,3,3,3,3,3,3,3,3,3,3,3,3,3,3,3,3,3,3,3,3,3,3,3,3,
3,3,3,3,3,3,3,3,3,3,3,3,3,3,3,3,3,3,3,3,3,3,3,3,3,3,3,3,3,3,3,3,3,3,3,3,
3,3,3,3,3,3,3,3,3,3,4),(0.143172102,0.15412844,0.165137615,0.176146789,
0.187155963,0.198165138,0.209174312,0.220183486,0.233027523,0.244036697,
0.262385321,0.275229358,0.288073394,0.300917431,0.311926606,0.32293578,
0.333944954,0.344954128,0.355963303,0.368807339,0.379816514,0.390825688,
0.401834862,0.411009174,0.420183486,0.429357798,0.43853211,0.449541284,
0.458715596,0.467889908,0.478899083,0.488073394,0.499082569,0.508256881,
0.517431193,0.526605505,0.533944954,0.541284404,0.548623853,0.555963303,
0.563302752,0.570642202,0.577981651,0.585321101,0.59266055,0.6,0.60733945,
0.614678899,0.622018349,0.629357798,0.636697248,0.644036697,0.651376147,
0.658715596,0.667889908,0.67706422,0.68440367,0.691743119,0.699082569,0.706422018,
0.713761468,0.721100917,0.728440367,0.735779817,0.743119266,0.750458716,
0.757798165,0.765137615,0.772477064,0.781651376,0.788990826,0.796330275,
0.805504587,0.811009174,0.816513761,0.822018349,0.827522936,0.833027523,
0.83853211,0.844036697,0.849541284,0.855045872,0.860550459,0.866055046,
0.871559633,0.87706422,0.882568807,0.888073394,0.893577982,0.900917431,
0.906422018,0.911926606,0.917431193,0.92293578,0.928440367,0.933944954,
0.939449541,0.944954128,0.950458716,0.957798165,0.963302752,0.968807339,
0.974311927,0.979816514,0.985321101,0.990825688,1.),.UNSPECIFIED.);
#24361=B_SPLINE_CURVE_WITH_KNOTS('',3,(#190381,#190382,#190383,#190384,
#190385,#190386,#190387,#190388,#190389,#190390,#190391,#190392,#190393,
#190394,#190395,#190396,#190397,#190398,#190399,#190400,#190401,#190402,
#190403,#190404,#190405,#190406,#190407,#190408,#190409,#190410,#190411,
#190412,#190413,#190414,#190415,#190416,#190417,#190418,#190419,#190420,
#190421,#190422,#190423,#190424,#190425,#190426,#190427,#190428,#190429,
#190430,#190431,#190432,#190433,#190434,#190435,#190436,#190437,#190438,
#190439,#190440,#190441,#190442,#190443,#190444,#190445,#190446,#190447,
#190448,#190449,#190450,#190451,#190452,#190453,#190454,#190455,#190456,
#190457,#190458,#190459,#190460,#190461,#190462,#190463,#190464,#190465,
#190466,#190467,#190468,#190469,#190470,#190471,#190472,#190473,#190474,
#190475,#190476,#190477,#190478,#190479,#190480,#190481,#190482,#190483,
#190484,#190485,#190486,#190487,#190488,#190489,#190490,#190491,#190492,
#190493,#190494,#190495,#190496,#190497,#190498,#190499,#190500,#190501,
#190502,#190503,#190504,#190505,#190506,#190507,#190508,#190509,#190510,
#190511,#190512,#190513,#190514,#190515,#190516,#190517,#190518,#190519,
#190520,#190521,#190522,#190523,#190524,#190525,#190526,#190527,#190528,
#190529,#190530,#190531,#190532,#190533,#190534,#190535,#190536,#190537,
#190538,#190539,#190540,#190541,#190542,#190543,#190544,#190545,#190546,
#190547,#190548,#190549,#190550,#190551,#190552,#190553,#190554,#190555,
#190556,#190557,#190558,#190559,#190560,#190561,#190562,#190563,#190564,
#190565,#190566,#190567,#190568,#190569,#190570,#190571,#190572,#190573,
#190574,#190575,#190576,#190577,#190578,#190579,#190580,#190581,#190582,
#190583,#190584,#190585,#190586,#190587,#190588,#190589,#190590,#190591,
#190592,#190593,#190594,#190595,#190596,#190597,#190598,#190599,#190600,
#190601,#190602,#190603,#190604,#190605,#190606,#190607,#190608,#190609,
#190610,#190611,#190612,#190613,#190614,#190615,#190616,#190617,#190618,
#190619,#190620,#190621,#190622,#190623,#190624,#190625,#190626,#190627,
#190628,#190629,#190630,#190631,#190632,#190633,#190634,#190635,#190636,
#190637,#190638,#190639,#190640,#190641,#190642,#190643,#190644,#190645,
#190646,#190647,#190648,#190649,#190650,#190651,#190652,#190653,#190654,
#190655,#190656,#190657,#190658,#190659,#190660,#190661,#190662,#190663,
#190664,#190665,#190666,#190667,#190668,#190669,#190670,#190671,#190672,
#190673,#190674,#190675,#190676,#190677,#190678,#190679,#190680,#190681,
#190682,#190683,#190684,#190685,#190686,#190687,#190688,#190689,#190690,
#190691,#190692,#190693,#190694,#190695,#190696,#190697,#190698,#190699,
#190700,#190701,#190702),.UNSPECIFIED.,.F.,.F.,(4,3,3,3,3,3,3,3,3,3,3,3,
3,3,3,3,3,3,3,3,3,3,3,3,3,3,3,3,3,3,3,3,3,3,3,3,3,3,3,3,3,3,3,3,3,3,3,3,
3,3,3,3,3,3,3,3,3,3,3,3,3,3,3,3,3,3,3,3,3,3,3,3,3,3,3,3,3,3,3,3,3,3,3,3,
3,3,3,3,3,3,3,3,3,3,3,3,3,3,3,3,3,3,3,3,3,3,3,4),(-1.,-0.994495413,-0.988990826,
-0.983486239,-0.977981651,-0.972477064,-0.966972477,-0.96146789,-0.955963303,
-0.950458716,-0.944954128,-0.939449541,-0.933944954,-0.928440367,-0.92293578,
-0.917431193,-0.911926606,-0.906422018,-0.900917431,-0.895412844,-0.889908257,
-0.88440367,-0.878899083,-0.873394495,-0.867889908,-0.862385321,-0.855045872,
-0.849541284,-0.842201835,-0.836697248,-0.831192661,-0.825688073,-0.820183486,
-0.814678899,-0.809174312,-0.801834862,-0.794495413,-0.787155963,-0.779816514,
-0.772477064,-0.765137615,-0.757798165,-0.750458716,-0.743119266,-0.735779817,
-0.728440367,-0.721100917,-0.713761468,-0.706422018,-0.697247706,-0.689908257,
-0.682568807,-0.675229358,-0.667889908,-0.660550459,-0.653211009,-0.644036697,
-0.636697248,-0.627522936,-0.620183486,-0.612844037,-0.605504587,-0.598165138,
-0.590825688,-0.583486239,-0.576146789,-0.568807339,-0.56146789,-0.55412844,
-0.546788991,-0.539449541,-0.532110092,-0.52293578,-0.513761468,-0.504587156,
-0.495412844,-0.486238532,-0.475229358,-0.466055046,-0.453211009,-0.444036697,
-0.434862385,-0.425688073,-0.416513761,-0.40733945,-0.398165138,-0.385321101,
-0.374311927,-0.363302752,-0.352293578,-0.341284404,-0.330275229,-0.319266055,
-0.308256881,-0.297247706,-0.286238532,-0.275229358,-0.264220183,-0.253211009,
-0.240366972,-0.229357798,-0.218348624,-0.20733945,-0.196330275,-0.185321101,
-0.172477064,-0.16146789,-0.143172102),.UNSPECIFIED.);
#24362=B_SPLINE_CURVE_WITH_KNOTS('',3,(#190703,#190704,#190705,#190706,
#190707,#190708,#190709,#190710,#190711,#190712,#190713,#190714,#190715,
#190716,#190717,#190718,#190719,#190720,#190721,#190722,#190723,#190724,
#190725,#190726,#190727,#190728,#190729,#190730,#190731,#190732,#190733,
#190734,#190735,#190736,#190737,#190738,#190739,#190740,#190741,#190742,
#190743,#190744,#190745,#190746,#190747,#190748,#190749,#190750,#190751,
#190752,#190753,#190754,#190755,#190756,#190757,#190758,#190759,#190760,
#190761,#190762,#190763,#190764,#190765,#190766,#190767,#190768,#190769,
#190770,#190771,#190772,#190773,#190774,#190775,#190776,#190777,#190778,
#190779,#190780,#190781,#190782,#190783,#190784,#190785,#190786,#190787,
#190788,#190789,#190790,#190791,#190792,#190793,#190794,#190795,#190796,
#190797,#190798,#190799,#190800,#190801,#190802,#190803,#190804,#190805,
#190806,#190807,#190808,#190809,#190810,#190811,#190812,#190813,#190814,
#190815,#190816,#190817,#190818,#190819,#190820,#190821,#190822,#190823,
#190824,#190825,#190826,#190827,#190828,#190829,#190830,#190831,#190832,
#190833,#190834,#190835,#190836,#190837,#190838,#190839,#190840,#190841,
#190842,#190843,#190844,#190845,#190846,#190847,#190848,#190849,#190850,
#190851,#190852,#190853,#190854,#190855,#190856,#190857,#190858,#190859,
#190860,#190861,#190862,#190863,#190864,#190865,#190866,#190867,#190868,
#190869,#190870,#190871,#190872,#190873,#190874,#190875,#190876,#190877,
#190878,#190879,#190880,#190881,#190882,#190883,#190884,#190885,#190886,
#190887,#190888,#190889,#190890,#190891,#190892,#190893,#190894,#190895,
#190896,#190897,#190898,#190899,#190900,#190901,#190902,#190903,#190904,
#190905,#190906,#190907,#190908,#190909,#190910,#190911,#190912,#190913,
#190914,#190915,#190916,#190917,#190918,#190919,#190920,#190921,#190922,
#190923,#190924,#190925,#190926,#190927,#190928,#190929,#190930,#190931,
#190932,#190933,#190934,#190935,#190936,#190937,#190938,#190939,#190940,
#190941,#190942,#190943,#190944,#190945,#190946,#190947,#190948,#190949,
#190950,#190951,#190952,#190953,#190954,#190955,#190956,#190957,#190958,
#190959,#190960,#190961,#190962,#190963,#190964,#190965,#190966,#190967,
#190968,#190969,#190970,#190971,#190972,#190973,#190974,#190975,#190976,
#190977,#190978,#190979,#190980,#190981,#190982,#190983,#190984,#190985,
#190986,#190987,#190988,#190989,#190990,#190991,#190992,#190993,#190994,
#190995,#190996,#190997,#190998,#190999,#191000),.UNSPECIFIED.,.F.,.F.,
(4,3,3,3,3,3,3,3,3,3,3,3,3,3,3,3,3,3,3,3,3,3,3,3,3,3,3,3,3,3,3,3,3,3,3,
3,3,3,3,3,3,3,3,3,3,3,3,3,3,3,3,3,3,3,3,3,3,3,3,3,3,3,3,3,3,3,3,3,3,3,3,
3,3,3,3,3,3,3,3,3,3,3,3,3,3,3,3,3,3,3,3,3,3,3,3,3,3,3,3,4),(0.143172102,
0.15412844,0.165137615,0.179816514,0.190825688,0.201834862,0.212844037,
0.223853211,0.234862385,0.24587156,0.256880734,0.267889908,0.278899083,
0.289908257,0.300917431,0.313761468,0.324770642,0.335779817,0.346788991,
0.363302752,0.374311927,0.385321101,0.396330275,0.405504587,0.416513761,
0.425688073,0.434862385,0.444036697,0.453211009,0.464220183,0.473394495,
0.482568807,0.491743119,0.500917431,0.510091743,0.521100917,0.530275229,
0.539449541,0.550458716,0.557798165,0.568807339,0.576146789,0.583486239,
0.59266055,0.6,0.60733945,0.614678899,0.622018349,0.631192661,0.640366972,
0.649541284,0.656880734,0.664220183,0.673394495,0.680733945,0.688073394,
0.695412844,0.702752294,0.710091743,0.717431193,0.730275229,0.743119266,
0.750458716,0.763302752,0.770642202,0.777981651,0.785321101,0.79266055,
0.8,0.811009174,0.816513761,0.822018349,0.827522936,0.833027523,0.83853211,
0.847706422,0.855045872,0.862385321,0.869724771,0.875229358,0.880733945,
0.886238532,0.893577982,0.899082569,0.904587156,0.910091743,0.917431193,
0.92293578,0.928440367,0.933944954,0.939449541,0.944954128,0.950458716,
0.957798165,0.966972477,0.972477064,0.977981651,0.983486239,0.99266055,
1.),.UNSPECIFIED.);
#24363=B_SPLINE_CURVE_WITH_KNOTS('',5,(#191963,#191964,#191965,#191966,
#191967,#191968,#191969,#191970,#191971,#191972,#191973,#191974,#191975,
#191976,#191977,#191978,#191979,#191980,#191981,#191982,#191983,#191984,
#191985,#191986,#191987,#191988,#191989,#191990,#191991,#191992,#191993,
#191994,#191995,#191996,#191997,#191998,#191999,#192000,#192001,#192002,
#192003,#192004,#192005,#192006,#192007,#192008,#192009,#192010,#192011,
#192012,#192013,#192014,#192015,#192016,#192017,#192018,#192019,#192020,
#192021,#192022,#192023,#192024,#192025,#192026,#192027,#192028,#192029,
#192030,#192031,#192032,#192033,#192034,#192035,#192036,#192037,#192038,
#192039,#192040,#192041,#192042,#192043,#192044,#192045,#192046,#192047,
#192048,#192049,#192050,#192051,#192052,#192053,#192054,#192055,#192056,
#192057,#192058,#192059,#192060,#192061,#192062,#192063,#192064,#192065,
#192066,#192067,#192068,#192069,#192070,#192071,#192072,#192073,#192074,
#192075,#192076,#192077,#192078,#192079,#192080,#192081,#192082,#192083,
#192084,#192085,#192086,#192087,#192088,#192089,#192090,#192091,#192092,
#192093,#192094,#192095,#192096,#192097,#192098,#192099,#192100,#192101,
#192102,#192103,#192104,#192105,#192106,#192107,#192108,#192109,#192110,
#192111,#192112,#192113,#192114,#192115,#192116,#192117,#192118,#192119,
#192120,#192121,#192122,#192123,#192124,#192125,#192126,#192127,#192128,
#192129,#192130,#192131,#192132,#192133,#192134,#192135,#192136,#192137,
#192138,#192139,#192140,#192141,#192142,#192143,#192144,#192145,#192146,
#192147,#192148,#192149,#192150,#192151,#192152,#192153,#192154,#192155,
#192156,#192157,#192158,#192159,#192160,#192161,#192162,#192163,#192164,
#192165,#192166,#192167,#192168,#192169,#192170,#192171,#192172,#192173,
#192174,#192175,#192176,#192177,#192178,#192179,#192180,#192181,#192182,
#192183,#192184,#192185,#192186,#192187,#192188,#192189,#192190,#192191,
#192192,#192193,#192194,#192195,#192196,#192197,#192198,#192199,#192200,
#192201,#192202,#192203,#192204,#192205,#192206,#192207,#192208,#192209,
#192210,#192211,#192212,#192213,#192214,#192215,#192216,#192217,#192218,
#192219,#192220,#192221,#192222,#192223,#192224,#192225,#192226,#192227,
#192228,#192229,#192230,#192231,#192232,#192233,#192234,#192235,#192236,
#192237,#192238,#192239,#192240,#192241,#192242,#192243,#192244,#192245,
#192246,#192247,#192248,#192249,#192250,#192251,#192252,#192253,#192254,
#192255,#192256,#192257,#192258,#192259,#192260,#192261,#192262,#192263,
#192264,#192265,#192266,#192267,#192268,#192269,#192270,#192271,#192272,
#192273,#192274,#192275,#192276,#192277,#192278,#192279,#192280,#192281,
#192282,#192283,#192284,#192285,#192286,#192287,#192288,#192289,#192290,
#192291,#192292,#192293,#192294,#192295,#192296,#192297,#192298,#192299,
#192300,#192301,#192302,#192303,#192304,#192305,#192306,#192307,#192308,
#192309,#192310,#192311,#192312,#192313,#192314,#192315,#192316,#192317,
#192318,#192319,#192320,#192321,#192322,#192323,#192324,#192325,#192326,
#192327,#192328,#192329,#192330,#192331,#192332,#192333,#192334,#192335,
#192336,#192337,#192338,#192339,#192340,#192341,#192342,#192343,#192344,
#192345,#192346,#192347,#192348,#192349,#192350,#192351,#192352,#192353,
#192354,#192355,#192356,#192357,#192358,#192359,#192360,#192361,#192362,
#192363,#192364,#192365,#192366,#192367,#192368,#192369,#192370,#192371,
#192372,#192373,#192374,#192375,#192376,#192377,#192378,#192379,#192380,
#192381,#192382,#192383,#192384,#192385,#192386,#192387,#192388,#192389,
#192390,#192391,#192392,#192393,#192394,#192395,#192396,#192397,#192398,
#192399,#192400,#192401,#192402,#192403,#192404,#192405,#192406,#192407,
#192408,#192409,#192410,#192411,#192412,#192413,#192414,#192415,#192416,
#192417,#192418,#192419,#192420,#192421,#192422,#192423,#192424,#192425,
#192426,#192427,#192428,#192429,#192430,#192431,#192432,#192433),
 .UNSPECIFIED.,.F.,.F.,(6,1,1,1,1,1,1,1,1,1,1,1,1,1,1,1,1,1,1,1,1,1,1,1,
1,1,1,1,1,1,1,1,1,1,1,1,1,1,1,1,1,1,1,1,1,1,1,1,1,1,1,1,1,1,1,1,1,1,1,1,
1,1,1,1,1,1,1,1,1,1,1,1,1,1,1,1,1,1,1,1,1,1,1,1,1,1,1,1,1,1,1,1,1,1,1,1,
1,1,1,1,1,1,1,1,1,1,1,1,1,1,1,1,1,1,1,1,1,1,1,1,1,1,1,1,1,1,1,1,1,1,1,1,
1,1,1,1,1,1,1,1,1,1,1,1,1,1,1,1,1,1,1,1,1,1,1,1,1,1,1,1,1,1,1,1,1,1,1,1,
1,1,1,1,1,1,1,1,1,1,1,1,1,1,1,1,1,1,1,1,1,1,1,1,1,1,1,1,1,1,1,1,1,1,1,1,
1,1,1,1,1,1,1,1,1,1,1,1,1,1,1,1,1,1,1,1,1,1,1,1,1,1,1,1,1,1,1,1,1,1,1,1,
1,1,1,1,1,1,1,1,1,1,1,1,1,1,1,1,1,1,1,1,1,1,1,1,1,1,1,1,1,1,1,1,1,1,1,1,
1,1,1,1,1,1,1,1,1,1,1,1,1,1,1,1,1,1,1,1,1,1,1,1,1,1,1,1,1,1,1,1,1,1,1,1,
1,1,1,1,1,1,1,1,1,1,1,1,1,1,1,1,1,1,1,1,1,1,1,1,1,1,1,1,1,1,1,1,1,1,1,1,
1,1,1,1,1,1,1,1,1,1,1,1,1,1,1,1,1,1,1,1,1,1,1,1,1,1,1,1,1,1,1,1,1,1,1,1,
1,1,1,1,1,1,1,1,1,1,1,1,1,1,1,1,1,1,1,1,1,1,1,1,1,1,1,1,1,1,1,1,1,1,1,1,
1,1,1,1,1,1,1,1,1,1,1,1,1,1,1,1,1,1,1,1,1,1,1,1,1,1,1,1,1,1,1,1,1,1,1,1,
1,1,1,1,1,1,1,1,1,1,6),(-1.,-0.998165138,-0.996330275,-0.994495413,-0.99266055,
-0.990825688,-0.988990826,-0.987155963,-0.985321101,-0.983486239,-0.981651376,
-0.979816514,-0.977981651,-0.976146789,-0.974311927,-0.972477064,-0.970642202,
-0.968807339,-0.966972477,-0.965137615,-0.963302752,-0.96146789,-0.959633028,
-0.957798165,-0.955963303,-0.95412844,-0.952293578,-0.950458716,-0.948623853,
-0.946788991,-0.944954128,-0.943119266,-0.941284404,-0.939449541,-0.937614679,
-0.935779817,-0.933944954,-0.932110092,-0.930275229,-0.928440367,-0.926605505,
-0.924770642,-0.92293578,-0.921100917,-0.919266055,-0.917431193,-0.91559633,
-0.913761468,-0.911926606,-0.910091743,-0.908256881,-0.906422018,-0.904587156,
-0.902752294,-0.900917431,-0.899082569,-0.897247706,-0.895412844,-0.893577982,
-0.891743119,-0.889908257,-0.888073394,-0.886238532,-0.88440367,-0.882568807,
-0.880733945,-0.878899083,-0.87706422,-0.875229358,-0.873394495,-0.871559633,
-0.869724771,-0.867889908,-0.866055046,-0.864220183,-0.862385321,-0.860550459,
-0.858715596,-0.856880734,-0.855045872,-0.853211009,-0.851376147,-0.849541284,
-0.847706422,-0.84587156,-0.844036697,-0.842201835,-0.840366972,-0.83853211,
-0.836697248,-0.834862385,-0.833027523,-0.831192661,-0.829357798,-0.827522936,
-0.825688073,-0.823853211,-0.822018349,-0.820183486,-0.818348624,-0.816513761,
-0.814678899,-0.812844037,-0.811009174,-0.809174312,-0.80733945,-0.805504587,
-0.803669725,-0.801834862,-0.8,-0.798165138,-0.796330275,-0.794495413,-0.79266055,
-0.790825688,-0.788990826,-0.787155963,-0.785321101,-0.783486239,-0.781651376,
-0.779816514,-0.777981651,-0.776146789,-0.774311927,-0.772477064,-0.770642202,
-0.768807339,-0.766972477,-0.765137615,-0.763302752,-0.76146789,-0.759633028,
-0.757798165,-0.755963303,-0.75412844,-0.752293578,-0.750458716,-0.748623853,
-0.746788991,-0.744954128,-0.743119266,-0.741284404,-0.739449541,-0.737614679,
-0.735779817,-0.733944954,-0.732110092,-0.730275229,-0.728440367,-0.726605505,
-0.724770642,-0.72293578,-0.721100917,-0.719266055,-0.717431193,-0.71559633,
-0.713761468,-0.711926606,-0.710091743,-0.708256881,-0.706422018,-0.704587156,
-0.702752294,-0.700917431,-0.699082569,-0.697247706,-0.695412844,-0.693577982,
-0.691743119,-0.689908257,-0.688073394,-0.686238532,-0.68440367,-0.682568807,
-0.680733945,-0.678899083,-0.67706422,-0.675229358,-0.673394495,-0.671559633,
-0.669724771,-0.667889908,-0.666055046,-0.664220183,-0.662385321,-0.660550459,
-0.658715596,-0.656880734,-0.655045872,-0.653211009,-0.651376147,-0.649541284,
-0.647706422,-0.64587156,-0.644036697,-0.642201835,-0.640366972,-0.63853211,
-0.636697248,-0.634862385,-0.633027523,-0.631192661,-0.629357798,-0.627522936,
-0.625688073,-0.623853211,-0.622018349,-0.620183486,-0.618348624,-0.616513761,
-0.614678899,-0.612844037,-0.611009174,-0.609174312,-0.60733945,-0.605504587,
-0.603669725,-0.601834862,-0.6,-0.598165138,-0.596330275,-0.594495413,-0.59266055,
-0.590825688,-0.588990826,-0.587155963,-0.585321101,-0.583486239,-0.581651376,
-0.579816514,-0.577981651,-0.576146789,-0.574311927,-0.572477064,-0.570642202,
-0.568807339,-0.566972477,-0.565137615,-0.563302752,-0.56146789,-0.559633028,
-0.557798165,-0.555963303,-0.55412844,-0.552293578,-0.550458716,-0.548623853,
-0.546788991,-0.544954128,-0.543119266,-0.541284404,-0.539449541,-0.537614679,
-0.535779817,-0.533944954,-0.532110092,-0.530275229,-0.528440367,-0.526605505,
-0.524770642,-0.52293578,-0.521100917,-0.519266055,-0.517431193,-0.51559633,
-0.513761468,-0.511926606,-0.510091743,-0.508256881,-0.506422018,-0.504587156,
-0.502752294,-0.500917431,-0.499082569,-0.497247706,-0.495412844,-0.493577982,
-0.491743119,-0.489908257,-0.488073394,-0.486238532,-0.48440367,-0.482568807,
-0.480733945,-0.478899083,-0.475229358,-0.473394495,-0.471559633,-0.469724771,
-0.467889908,-0.466055046,-0.464220183,-0.462385321,-0.460550459,-0.458715596,
-0.456880734,-0.455045872,-0.453211009,-0.451376147,-0.449541284,-0.447706422,
-0.44587156,-0.444036697,-0.442201835,-0.440366972,-0.43853211,-0.436697248,
-0.434862385,-0.433027523,-0.431192661,-0.429357798,-0.427522936,-0.425688073,
-0.423853211,-0.422018349,-0.420183486,-0.418348624,-0.416513761,-0.414678899,
-0.412844037,-0.411009174,-0.409174312,-0.40733945,-0.405504587,-0.403669725,
-0.401834862,-0.4,-0.398165138,-0.396330275,-0.394495413,-0.39266055,-0.390825688,
-0.388990826,-0.387155963,-0.385321101,-0.383486239,-0.381651376,-0.379816514,
-0.377981651,-0.376146789,-0.374311927,-0.372477064,-0.370642202,-0.368807339,
-0.366972477,-0.365137615,-0.363302752,-0.36146789,-0.359633028,-0.357798165,
-0.355963303,-0.35412844,-0.352293578,-0.350458716,-0.348623853,-0.346788991,
-0.344954128,-0.343119266,-0.341284404,-0.339449541,-0.337614679,-0.335779817,
-0.333944954,-0.332110092,-0.330275229,-0.328440367,-0.326605505,-0.324770642,
-0.32293578,-0.321100917,-0.319266055,-0.317431193,-0.31559633,-0.313761468,
-0.311926606,-0.310091743,-0.308256881,-0.306422018,-0.304587156,-0.302752294,
-0.300917431,-0.299082569,-0.297247706,-0.295412844,-0.293577982,-0.291743119,
-0.289908257,-0.288073394,-0.286238532,-0.28440367,-0.282568807,-0.280733945,
-0.278899083,-0.27706422,-0.275229358,-0.273394495,-0.271559633,-0.269724771,
-0.267889908,-0.266055046,-0.264220183,-0.262385321,-0.260550459,-0.258715596,
-0.256880734,-0.255045872,-0.253211009,-0.251376147,-0.249541284,-0.247706422,
-0.24587156,-0.244036697,-0.242201835,-0.240366972,-0.23853211,-0.236697248,
-0.234862385,-0.233027523,-0.231192661,-0.229357798,-0.227522936,-0.225688073,
-0.223853211,-0.222018349,-0.220183486,-0.218348624,-0.216513761,-0.214678899,
-0.212844037,-0.211009174,-0.209174312,-0.20733945,-0.205504587,-0.203669725,
-0.201834862,-0.2,-0.198165138,-0.196330275,-0.194495413,-0.19266055,-0.190825688,
-0.188990826,-0.187155963,-0.185321101,-0.183486239,-0.181651376,-0.179816514,
-0.177981651,-0.176146789,-0.174311927,-0.172477064,-0.170642202,-0.168807339,
-0.166972477,-0.165137615,-0.163302752,-0.16146789,-0.159633028,-0.157798165,
-0.155963303,-0.15412844,-0.152293578,-0.150458716,-0.148623853,-0.146788991,
-0.144954128,-0.143172102),.UNSPECIFIED.);
#24364=B_SPLINE_CURVE_WITH_KNOTS('',5,(#192434,#192435,#192436,#192437,
#192438,#192439,#192440,#192441,#192442,#192443,#192444,#192445,#192446,
#192447,#192448,#192449,#192450,#192451,#192452,#192453,#192454,#192455,
#192456,#192457,#192458,#192459,#192460,#192461,#192462,#192463,#192464,
#192465,#192466,#192467,#192468,#192469,#192470,#192471,#192472,#192473,
#192474,#192475,#192476,#192477,#192478,#192479,#192480,#192481,#192482,
#192483,#192484,#192485,#192486,#192487,#192488,#192489,#192490,#192491,
#192492,#192493,#192494,#192495,#192496,#192497,#192498,#192499,#192500,
#192501,#192502,#192503,#192504,#192505,#192506,#192507,#192508,#192509,
#192510,#192511,#192512,#192513,#192514,#192515,#192516,#192517,#192518,
#192519,#192520,#192521,#192522,#192523,#192524,#192525,#192526,#192527,
#192528,#192529,#192530,#192531,#192532,#192533,#192534,#192535,#192536,
#192537,#192538,#192539,#192540,#192541,#192542,#192543,#192544,#192545,
#192546,#192547,#192548,#192549,#192550,#192551,#192552,#192553,#192554,
#192555,#192556,#192557,#192558,#192559,#192560,#192561,#192562,#192563,
#192564,#192565,#192566,#192567,#192568,#192569,#192570,#192571,#192572,
#192573,#192574,#192575,#192576,#192577,#192578,#192579,#192580,#192581,
#192582,#192583,#192584,#192585,#192586,#192587,#192588,#192589,#192590,
#192591,#192592,#192593,#192594,#192595,#192596,#192597,#192598,#192599,
#192600,#192601,#192602,#192603,#192604,#192605,#192606,#192607,#192608,
#192609,#192610,#192611,#192612,#192613,#192614,#192615,#192616,#192617,
#192618,#192619,#192620,#192621,#192622,#192623,#192624,#192625,#192626,
#192627,#192628,#192629,#192630,#192631,#192632,#192633,#192634,#192635,
#192636,#192637,#192638,#192639,#192640,#192641,#192642,#192643,#192644,
#192645,#192646,#192647,#192648,#192649,#192650,#192651,#192652,#192653,
#192654,#192655,#192656,#192657,#192658,#192659,#192660,#192661,#192662,
#192663,#192664,#192665,#192666,#192667,#192668,#192669,#192670,#192671,
#192672,#192673,#192674,#192675,#192676,#192677,#192678,#192679,#192680,
#192681,#192682,#192683,#192684,#192685,#192686,#192687,#192688,#192689,
#192690,#192691,#192692,#192693,#192694,#192695,#192696,#192697,#192698,
#192699,#192700,#192701,#192702,#192703,#192704,#192705,#192706,#192707,
#192708,#192709,#192710,#192711,#192712,#192713,#192714,#192715,#192716,
#192717,#192718,#192719,#192720,#192721,#192722,#192723,#192724,#192725,
#192726,#192727,#192728,#192729,#192730,#192731,#192732,#192733,#192734,
#192735,#192736,#192737,#192738,#192739,#192740,#192741,#192742,#192743,
#192744,#192745,#192746,#192747,#192748,#192749,#192750,#192751,#192752,
#192753,#192754,#192755,#192756,#192757,#192758,#192759,#192760,#192761,
#192762,#192763,#192764,#192765,#192766,#192767,#192768,#192769,#192770,
#192771,#192772,#192773,#192774,#192775,#192776,#192777,#192778,#192779,
#192780,#192781,#192782,#192783,#192784,#192785,#192786,#192787,#192788,
#192789,#192790,#192791,#192792,#192793,#192794,#192795,#192796,#192797,
#192798,#192799,#192800,#192801,#192802,#192803,#192804,#192805,#192806,
#192807,#192808,#192809,#192810,#192811,#192812,#192813,#192814,#192815,
#192816,#192817,#192818,#192819,#192820,#192821,#192822,#192823,#192824,
#192825,#192826,#192827,#192828,#192829,#192830,#192831,#192832,#192833,
#192834,#192835,#192836,#192837,#192838,#192839,#192840,#192841,#192842,
#192843,#192844,#192845,#192846,#192847,#192848,#192849,#192850,#192851,
#192852,#192853,#192854,#192855,#192856,#192857,#192858,#192859,#192860,
#192861,#192862,#192863,#192864,#192865,#192866,#192867,#192868,#192869,
#192870,#192871,#192872,#192873,#192874,#192875,#192876,#192877,#192878,
#192879,#192880,#192881,#192882,#192883,#192884,#192885,#192886,#192887,
#192888,#192889,#192890,#192891,#192892,#192893,#192894,#192895,#192896,
#192897,#192898,#192899,#192900,#192901,#192902,#192903,#192904),
 .UNSPECIFIED.,.F.,.F.,(6,1,1,1,1,1,1,1,1,1,1,1,1,1,1,1,1,1,1,1,1,1,1,1,
1,1,1,1,1,1,1,1,1,1,1,1,1,1,1,1,1,1,1,1,1,1,1,1,1,1,1,1,1,1,1,1,1,1,1,1,
1,1,1,1,1,1,1,1,1,1,1,1,1,1,1,1,1,1,1,1,1,1,1,1,1,1,1,1,1,1,1,1,1,1,1,1,
1,1,1,1,1,1,1,1,1,1,1,1,1,1,1,1,1,1,1,1,1,1,1,1,1,1,1,1,1,1,1,1,1,1,1,1,
1,1,1,1,1,1,1,1,1,1,1,1,1,1,1,1,1,1,1,1,1,1,1,1,1,1,1,1,1,1,1,1,1,1,1,1,
1,1,1,1,1,1,1,1,1,1,1,1,1,1,1,1,1,1,1,1,1,1,1,1,1,1,1,1,1,1,1,1,1,1,1,1,
1,1,1,1,1,1,1,1,1,1,1,1,1,1,1,1,1,1,1,1,1,1,1,1,1,1,1,1,1,1,1,1,1,1,1,1,
1,1,1,1,1,1,1,1,1,1,1,1,1,1,1,1,1,1,1,1,1,1,1,1,1,1,1,1,1,1,1,1,1,1,1,1,
1,1,1,1,1,1,1,1,1,1,1,1,1,1,1,1,1,1,1,1,1,1,1,1,1,1,1,1,1,1,1,1,1,1,1,1,
1,1,1,1,1,1,1,1,1,1,1,1,1,1,1,1,1,1,1,1,1,1,1,1,1,1,1,1,1,1,1,1,1,1,1,1,
1,1,1,1,1,1,1,1,1,1,1,1,1,1,1,1,1,1,1,1,1,1,1,1,1,1,1,1,1,1,1,1,1,1,1,1,
1,1,1,1,1,1,1,1,1,1,1,1,1,1,1,1,1,1,1,1,1,1,1,1,1,1,1,1,1,1,1,1,1,1,1,1,
1,1,1,1,1,1,1,1,1,1,1,1,1,1,1,1,1,1,1,1,1,1,1,1,1,1,1,1,1,1,1,1,1,1,1,1,
1,1,1,1,1,1,1,1,1,1,6),(0.143172102,0.144954128,0.146788991,0.148623853,
0.150458716,0.152293578,0.15412844,0.155963303,0.157798165,0.159633028,
0.16146789,0.163302752,0.165137615,0.166972477,0.168807339,0.170642202,
0.172477064,0.174311927,0.176146789,0.177981651,0.179816514,0.181651376,
0.183486239,0.185321101,0.187155963,0.188990826,0.190825688,0.19266055,
0.194495413,0.196330275,0.198165138,0.2,0.201834862,0.203669725,0.205504587,
0.20733945,0.209174312,0.211009174,0.212844037,0.214678899,0.216513761,
0.218348624,0.220183486,0.222018349,0.223853211,0.225688073,0.227522936,
0.229357798,0.231192661,0.233027523,0.234862385,0.236697248,0.23853211,
0.240366972,0.242201835,0.244036697,0.24587156,0.247706422,0.249541284,
0.251376147,0.253211009,0.255045872,0.256880734,0.258715596,0.260550459,
0.262385321,0.264220183,0.266055046,0.267889908,0.269724771,0.271559633,
0.273394495,0.275229358,0.27706422,0.278899083,0.280733945,0.282568807,
0.28440367,0.286238532,0.288073394,0.289908257,0.291743119,0.293577982,
0.295412844,0.297247706,0.299082569,0.300917431,0.302752294,0.304587156,
0.306422018,0.308256881,0.310091743,0.311926606,0.313761468,0.31559633,
0.317431193,0.319266055,0.321100917,0.32293578,0.324770642,0.326605505,
0.328440367,0.330275229,0.332110092,0.333944954,0.335779817,0.337614679,
0.339449541,0.341284404,0.343119266,0.344954128,0.346788991,0.348623853,
0.350458716,0.352293578,0.35412844,0.355963303,0.357798165,0.359633028,
0.36146789,0.363302752,0.365137615,0.366972477,0.368807339,0.370642202,
0.372477064,0.374311927,0.376146789,0.377981651,0.379816514,0.381651376,
0.383486239,0.385321101,0.387155963,0.388990826,0.390825688,0.39266055,
0.394495413,0.396330275,0.398165138,0.4,0.401834862,0.403669725,0.405504587,
0.40733945,0.409174312,0.411009174,0.412844037,0.414678899,0.416513761,
0.418348624,0.420183486,0.422018349,0.423853211,0.425688073,0.427522936,
0.429357798,0.431192661,0.433027523,0.434862385,0.436697248,0.43853211,
0.440366972,0.442201835,0.444036697,0.44587156,0.447706422,0.449541284,
0.451376147,0.453211009,0.455045872,0.456880734,0.458715596,0.460550459,
0.462385321,0.464220183,0.466055046,0.467889908,0.469724771,0.471559633,
0.473394495,0.475229358,0.478899083,0.480733945,0.482568807,0.48440367,
0.486238532,0.488073394,0.489908257,0.491743119,0.493577982,0.495412844,
0.497247706,0.499082569,0.500917431,0.502752294,0.504587156,0.506422018,
0.508256881,0.510091743,0.511926606,0.513761468,0.51559633,0.517431193,
0.519266055,0.521100917,0.52293578,0.524770642,0.526605505,0.528440367,
0.530275229,0.532110092,0.533944954,0.535779817,0.537614679,0.539449541,
0.541284404,0.543119266,0.544954128,0.546788991,0.548623853,0.550458716,
0.552293578,0.55412844,0.555963303,0.557798165,0.559633028,0.56146789,0.563302752,
0.565137615,0.566972477,0.568807339,0.570642202,0.572477064,0.574311927,
0.576146789,0.577981651,0.579816514,0.581651376,0.583486239,0.585321101,
0.587155963,0.588990826,0.590825688,0.59266055,0.594495413,0.596330275,
0.598165138,0.6,0.601834862,0.603669725,0.605504587,0.60733945,0.609174312,
0.611009174,0.612844037,0.614678899,0.616513761,0.618348624,0.620183486,
0.622018349,0.623853211,0.625688073,0.627522936,0.629357798,0.631192661,
0.633027523,0.634862385,0.636697248,0.63853211,0.640366972,0.642201835,
0.644036697,0.64587156,0.647706422,0.649541284,0.651376147,0.653211009,
0.655045872,0.656880734,0.658715596,0.660550459,0.662385321,0.664220183,
0.666055046,0.667889908,0.669724771,0.671559633,0.673394495,0.675229358,
0.67706422,0.678899083,0.680733945,0.682568807,0.68440367,0.686238532,0.688073394,
0.689908257,0.691743119,0.693577982,0.695412844,0.697247706,0.699082569,
0.700917431,0.702752294,0.704587156,0.706422018,0.708256881,0.710091743,
0.711926606,0.713761468,0.71559633,0.717431193,0.719266055,0.721100917,
0.72293578,0.724770642,0.726605505,0.728440367,0.730275229,0.732110092,
0.733944954,0.735779817,0.737614679,0.739449541,0.741284404,0.743119266,
0.744954128,0.746788991,0.748623853,0.750458716,0.752293578,0.75412844,
0.755963303,0.757798165,0.759633028,0.76146789,0.763302752,0.765137615,
0.766972477,0.768807339,0.770642202,0.772477064,0.774311927,0.776146789,
0.777981651,0.779816514,0.781651376,0.783486239,0.785321101,0.787155963,
0.788990826,0.790825688,0.79266055,0.794495413,0.796330275,0.798165138,
0.8,0.801834862,0.803669725,0.805504587,0.80733945,0.809174312,0.811009174,
0.812844037,0.814678899,0.816513761,0.818348624,0.820183486,0.822018349,
0.823853211,0.825688073,0.827522936,0.829357798,0.831192661,0.833027523,
0.834862385,0.836697248,0.83853211,0.840366972,0.842201835,0.844036697,
0.84587156,0.847706422,0.849541284,0.851376147,0.853211009,0.855045872,
0.856880734,0.858715596,0.860550459,0.862385321,0.864220183,0.866055046,
0.867889908,0.869724771,0.871559633,0.873394495,0.875229358,0.87706422,
0.878899083,0.880733945,0.882568807,0.88440367,0.886238532,0.888073394,
0.889908257,0.891743119,0.893577982,0.895412844,0.897247706,0.899082569,
0.900917431,0.902752294,0.904587156,0.906422018,0.908256881,0.910091743,
0.911926606,0.913761468,0.91559633,0.917431193,0.919266055,0.921100917,
0.92293578,0.924770642,0.926605505,0.928440367,0.930275229,0.932110092,
0.933944954,0.935779817,0.937614679,0.939449541,0.941284404,0.943119266,
0.944954128,0.946788991,0.948623853,0.950458716,0.952293578,0.95412844,
0.955963303,0.957798165,0.959633028,0.96146789,0.963302752,0.965137615,
0.966972477,0.968807339,0.970642202,0.972477064,0.974311927,0.976146789,
0.977981651,0.979816514,0.981651376,0.983486239,0.985321101,0.987155963,
0.988990826,0.990825688,0.99266055,0.994495413,0.996330275,0.998165138,
1.),.UNSPECIFIED.);
#24365=B_SPLINE_CURVE_WITH_KNOTS('',3,(#193849,#193850,#193851,#193852,
#193853,#193854,#193855,#193856,#193857,#193858,#193859,#193860,#193861,
#193862,#193863,#193864,#193865,#193866,#193867,#193868,#193869,#193870,
#193871,#193872,#193873,#193874,#193875,#193876,#193877,#193878,#193879,
#193880,#193881,#193882,#193883,#193884,#193885,#193886,#193887,#193888,
#193889,#193890,#193891,#193892,#193893,#193894,#193895,#193896,#193897,
#193898,#193899,#193900,#193901,#193902,#193903,#193904,#193905,#193906,
#193907,#193908,#193909,#193910,#193911,#193912,#193913,#193914,#193915,
#193916,#193917,#193918,#193919,#193920,#193921,#193922,#193923,#193924,
#193925,#193926,#193927,#193928,#193929,#193930,#193931,#193932,#193933,
#193934,#193935,#193936,#193937,#193938,#193939,#193940,#193941,#193942,
#193943,#193944,#193945,#193946,#193947,#193948,#193949,#193950,#193951,
#193952,#193953,#193954,#193955,#193956,#193957,#193958,#193959,#193960,
#193961,#193962,#193963,#193964,#193965,#193966,#193967,#193968,#193969,
#193970,#193971,#193972,#193973,#193974,#193975,#193976,#193977,#193978,
#193979,#193980,#193981,#193982,#193983,#193984,#193985,#193986,#193987,
#193988,#193989,#193990,#193991,#193992,#193993,#193994,#193995,#193996,
#193997,#193998,#193999,#194000,#194001,#194002,#194003,#194004,#194005,
#194006,#194007,#194008,#194009,#194010,#194011,#194012,#194013,#194014,
#194015,#194016,#194017,#194018,#194019,#194020,#194021,#194022,#194023,
#194024,#194025,#194026,#194027,#194028,#194029,#194030,#194031,#194032,
#194033,#194034,#194035,#194036,#194037,#194038,#194039,#194040,#194041,
#194042,#194043,#194044,#194045,#194046,#194047,#194048,#194049,#194050,
#194051,#194052,#194053,#194054,#194055,#194056,#194057,#194058,#194059,
#194060,#194061,#194062,#194063,#194064,#194065,#194066,#194067,#194068,
#194069,#194070,#194071,#194072,#194073,#194074,#194075,#194076,#194077,
#194078,#194079,#194080,#194081,#194082,#194083,#194084,#194085,#194086,
#194087,#194088,#194089,#194090,#194091,#194092,#194093,#194094,#194095,
#194096,#194097,#194098,#194099,#194100,#194101,#194102,#194103,#194104,
#194105,#194106,#194107,#194108,#194109,#194110,#194111,#194112,#194113,
#194114,#194115,#194116,#194117,#194118,#194119,#194120,#194121,#194122,
#194123,#194124,#194125,#194126,#194127,#194128,#194129,#194130,#194131,
#194132,#194133,#194134,#194135,#194136,#194137,#194138,#194139,#194140,
#194141,#194142,#194143,#194144,#194145,#194146),.UNSPECIFIED.,.F.,.F.,
(4,3,3,3,3,3,3,3,3,3,3,3,3,3,3,3,3,3,3,3,3,3,3,3,3,3,3,3,3,3,3,3,3,3,3,
3,3,3,3,3,3,3,3,3,3,3,3,3,3,3,3,3,3,3,3,3,3,3,3,3,3,3,3,3,3,3,3,3,3,3,3,
3,3,3,3,3,3,3,3,3,3,3,3,3,3,3,3,3,3,3,3,3,3,3,3,3,3,3,3,4),(0.143172102,
0.15412844,0.165137615,0.177981651,0.188990826,0.201834862,0.212844037,
0.223853211,0.234862385,0.24587156,0.256880734,0.267889908,0.278899083,
0.289908257,0.300917431,0.311926606,0.32293578,0.339449541,0.350458716,
0.36146789,0.374311927,0.385321101,0.396330275,0.40733945,0.416513761,0.425688073,
0.434862385,0.44587156,0.458715596,0.467889908,0.47706422,0.491743119,0.500917431,
0.511926606,0.521100917,0.530275229,0.537614679,0.548623853,0.555963303,
0.563302752,0.570642202,0.577981651,0.585321101,0.594495413,0.601834862,
0.609174312,0.616513761,0.623853211,0.631192661,0.640366972,0.647706422,
0.655045872,0.664220183,0.671559633,0.678899083,0.688073394,0.695412844,
0.702752294,0.711926606,0.719266055,0.726605505,0.735779817,0.744954128,
0.75412844,0.76146789,0.768807339,0.776146789,0.785321101,0.796330275,0.803669725,
0.812844037,0.820183486,0.827522936,0.836697248,0.842201835,0.849541284,
0.856880734,0.862385321,0.867889908,0.875229358,0.880733945,0.888073394,
0.893577982,0.899082569,0.906422018,0.911926606,0.917431193,0.92293578,
0.930275229,0.935779817,0.944954128,0.950458716,0.959633028,0.965137615,
0.970642202,0.976146789,0.981651376,0.987155963,0.99266055,1.),
 .UNSPECIFIED.);
#24366=B_SPLINE_CURVE_WITH_KNOTS('',3,(#194147,#194148,#194149,#194150,
#194151,#194152,#194153,#194154,#194155,#194156,#194157,#194158,#194159,
#194160,#194161,#194162,#194163,#194164,#194165,#194166,#194167,#194168,
#194169,#194170,#194171,#194172,#194173,#194174,#194175,#194176,#194177,
#194178,#194179,#194180,#194181,#194182,#194183,#194184,#194185,#194186,
#194187,#194188,#194189,#194190,#194191,#194192,#194193,#194194,#194195,
#194196,#194197,#194198,#194199,#194200,#194201,#194202,#194203,#194204,
#194205,#194206,#194207,#194208,#194209,#194210,#194211,#194212,#194213,
#194214,#194215,#194216,#194217,#194218,#194219,#194220,#194221,#194222,
#194223,#194224,#194225,#194226,#194227,#194228,#194229,#194230,#194231,
#194232,#194233,#194234,#194235,#194236,#194237,#194238,#194239,#194240,
#194241,#194242,#194243,#194244,#194245,#194246,#194247,#194248,#194249,
#194250,#194251,#194252,#194253,#194254,#194255,#194256,#194257,#194258,
#194259,#194260,#194261,#194262,#194263,#194264,#194265,#194266,#194267,
#194268,#194269,#194270,#194271,#194272,#194273,#194274,#194275,#194276,
#194277,#194278,#194279,#194280,#194281,#194282,#194283,#194284,#194285,
#194286,#194287,#194288,#194289,#194290,#194291,#194292,#194293,#194294,
#194295,#194296,#194297,#194298,#194299,#194300,#194301,#194302,#194303,
#194304,#194305,#194306,#194307,#194308,#194309,#194310,#194311,#194312,
#194313,#194314,#194315,#194316,#194317,#194318,#194319,#194320,#194321,
#194322,#194323,#194324,#194325,#194326,#194327,#194328,#194329,#194330,
#194331,#194332,#194333,#194334,#194335,#194336,#194337,#194338,#194339,
#194340,#194341,#194342,#194343,#194344,#194345,#194346,#194347,#194348,
#194349,#194350,#194351,#194352,#194353,#194354,#194355,#194356,#194357,
#194358,#194359,#194360,#194361,#194362,#194363,#194364,#194365,#194366,
#194367,#194368,#194369,#194370,#194371,#194372,#194373,#194374,#194375,
#194376,#194377,#194378,#194379,#194380,#194381,#194382,#194383,#194384,
#194385,#194386,#194387,#194388,#194389,#194390,#194391,#194392,#194393,
#194394,#194395,#194396,#194397,#194398,#194399,#194400,#194401,#194402,
#194403,#194404,#194405,#194406,#194407,#194408,#194409,#194410,#194411,
#194412,#194413,#194414,#194415,#194416,#194417,#194418,#194419,#194420,
#194421,#194422,#194423,#194424,#194425,#194426,#194427,#194428,#194429,
#194430,#194431,#194432,#194433,#194434,#194435,#194436,#194437,#194438,
#194439,#194440,#194441,#194442,#194443,#194444,#194445,#194446,#194447,
#194448,#194449,#194450,#194451,#194452,#194453,#194454,#194455,#194456,
#194457,#194458,#194459,#194460,#194461,#194462,#194463,#194464,#194465,
#194466,#194467,#194468),.UNSPECIFIED.,.F.,.F.,(4,3,3,3,3,3,3,3,3,3,3,3,
3,3,3,3,3,3,3,3,3,3,3,3,3,3,3,3,3,3,3,3,3,3,3,3,3,3,3,3,3,3,3,3,3,3,3,3,
3,3,3,3,3,3,3,3,3,3,3,3,3,3,3,3,3,3,3,3,3,3,3,3,3,3,3,3,3,3,3,3,3,3,3,3,
3,3,3,3,3,3,3,3,3,3,3,3,3,3,3,3,3,3,3,3,3,3,3,4),(0.143172102,0.15412844,
0.165137615,0.177981651,0.188990826,0.201834862,0.212844037,0.223853211,
0.234862385,0.247706422,0.258715596,0.269724771,0.280733945,0.291743119,
0.302752294,0.313761468,0.324770642,0.335779817,0.346788991,0.357798165,
0.368807339,0.379816514,0.39266055,0.401834862,0.411009174,0.420183486,
0.429357798,0.43853211,0.447706422,0.456880734,0.466055046,0.47706422,0.489908257,
0.499082569,0.508256881,0.517431193,0.526605505,0.533944954,0.541284404,
0.548623853,0.555963303,0.563302752,0.570642202,0.577981651,0.585321101,
0.59266055,0.6,0.60733945,0.614678899,0.622018349,0.629357798,0.636697248,
0.644036697,0.651376147,0.658715596,0.667889908,0.675229358,0.682568807,
0.689908257,0.697247706,0.704587156,0.711926606,0.719266055,0.726605505,
0.735779817,0.743119266,0.750458716,0.757798165,0.765137615,0.772477064,
0.779816514,0.787155963,0.794495413,0.801834862,0.809174312,0.814678899,
0.820183486,0.825688073,0.831192661,0.836697248,0.842201835,0.849541284,
0.855045872,0.860550459,0.866055046,0.871559633,0.87706422,0.882568807,
0.888073394,0.893577982,0.900917431,0.906422018,0.911926606,0.917431193,
0.92293578,0.928440367,0.933944954,0.939449541,0.944954128,0.950458716,
0.957798165,0.963302752,0.968807339,0.976146789,0.981651376,0.987155963,
0.99266055,1.),.UNSPECIFIED.);
#24367=B_SPLINE_CURVE_WITH_KNOTS('',3,(#195428,#195429,#195430,#195431,
#195432,#195433,#195434,#195435,#195436,#195437,#195438,#195439,#195440,
#195441,#195442,#195443,#195444,#195445,#195446,#195447,#195448,#195449,
#195450,#195451,#195452,#195453,#195454,#195455,#195456,#195457,#195458,
#195459,#195460,#195461,#195462,#195463,#195464,#195465,#195466,#195467,
#195468,#195469,#195470,#195471,#195472,#195473,#195474,#195475,#195476,
#195477,#195478,#195479,#195480,#195481,#195482,#195483,#195484,#195485,
#195486,#195487,#195488,#195489,#195490,#195491,#195492,#195493,#195494,
#195495,#195496,#195497,#195498,#195499,#195500,#195501,#195502,#195503,
#195504,#195505,#195506,#195507,#195508,#195509,#195510,#195511,#195512,
#195513,#195514,#195515,#195516,#195517,#195518,#195519,#195520,#195521,
#195522,#195523,#195524,#195525,#195526,#195527,#195528,#195529,#195530,
#195531,#195532,#195533,#195534,#195535,#195536,#195537,#195538,#195539,
#195540,#195541,#195542,#195543,#195544,#195545,#195546,#195547,#195548,
#195549,#195550,#195551,#195552,#195553,#195554,#195555,#195556,#195557,
#195558,#195559,#195560,#195561,#195562,#195563,#195564,#195565,#195566,
#195567,#195568,#195569,#195570,#195571,#195572,#195573,#195574,#195575,
#195576,#195577,#195578,#195579,#195580,#195581,#195582,#195583,#195584,
#195585,#195586,#195587,#195588,#195589,#195590,#195591,#195592,#195593,
#195594,#195595,#195596,#195597,#195598,#195599,#195600,#195601,#195602,
#195603,#195604,#195605,#195606,#195607,#195608,#195609,#195610,#195611,
#195612,#195613,#195614,#195615,#195616,#195617,#195618,#195619,#195620,
#195621,#195622,#195623,#195624,#195625,#195626,#195627,#195628,#195629,
#195630,#195631,#195632,#195633,#195634,#195635,#195636,#195637,#195638,
#195639,#195640,#195641,#195642,#195643,#195644,#195645,#195646,#195647,
#195648,#195649,#195650,#195651,#195652,#195653,#195654,#195655,#195656,
#195657,#195658,#195659,#195660,#195661,#195662,#195663,#195664,#195665,
#195666,#195667,#195668,#195669,#195670,#195671,#195672,#195673,#195674,
#195675,#195676,#195677,#195678,#195679,#195680,#195681,#195682,#195683,
#195684,#195685,#195686,#195687,#195688,#195689,#195690,#195691,#195692,
#195693,#195694,#195695,#195696,#195697,#195698,#195699,#195700,#195701,
#195702,#195703,#195704,#195705,#195706,#195707,#195708,#195709,#195710,
#195711,#195712,#195713,#195714,#195715,#195716,#195717,#195718,#195719,
#195720,#195721,#195722,#195723,#195724,#195725,#195726,#195727,#195728,
#195729,#195730,#195731,#195732,#195733,#195734),.UNSPECIFIED.,.F.,.F.,
(4,3,3,3,3,3,3,3,3,3,3,3,3,3,3,3,3,3,3,3,3,3,3,3,3,3,3,3,3,3,3,3,3,3,3,
3,3,3,3,3,3,3,3,3,3,3,3,3,3,3,3,3,3,3,3,3,3,3,3,3,3,3,3,3,3,3,3,3,3,3,3,
3,3,3,3,3,3,3,3,3,3,3,3,3,3,3,3,3,3,3,3,3,3,3,3,3,3,3,3,3,3,3,4),(0.143172102,
0.15412844,0.165137615,0.176146789,0.187155963,0.198165138,0.211009174,
0.222018349,0.233027523,0.244036697,0.255045872,0.266055046,0.27706422,
0.288073394,0.299082569,0.310091743,0.321100917,0.332110092,0.343119266,
0.35412844,0.365137615,0.376146789,0.387155963,0.398165138,0.40733945,0.416513761,
0.425688073,0.434862385,0.444036697,0.453211009,0.466055046,0.47706422,
0.486238532,0.497247706,0.506422018,0.51559633,0.524770642,0.533944954,
0.541284404,0.550458716,0.557798165,0.565137615,0.572477064,0.583486239,
0.59266055,0.6,0.60733945,0.616513761,0.623853211,0.631192661,0.640366972,
0.647706422,0.655045872,0.664220183,0.671559633,0.678899083,0.686238532,
0.693577982,0.702752294,0.713761468,0.721100917,0.728440367,0.735779817,
0.744954128,0.752293578,0.759633028,0.770642202,0.777981651,0.788990826,
0.796330275,0.803669725,0.812844037,0.822018349,0.829357798,0.834862385,
0.840366972,0.84587156,0.853211009,0.858715596,0.864220183,0.871559633,
0.87706422,0.882568807,0.888073394,0.893577982,0.902752294,0.908256881,
0.913761468,0.919266055,0.924770642,0.930275229,0.937614679,0.943119266,
0.948623853,0.95412844,0.96146789,0.966972477,0.972477064,0.977981651,0.983486239,
0.988990826,0.994495413,1.),.UNSPECIFIED.);
#24368=B_SPLINE_CURVE_WITH_KNOTS('',3,(#195735,#195736,#195737,#195738,
#195739,#195740,#195741,#195742,#195743,#195744,#195745,#195746,#195747,
#195748,#195749,#195750,#195751,#195752,#195753,#195754,#195755,#195756,
#195757,#195758,#195759,#195760,#195761,#195762,#195763,#195764,#195765,
#195766,#195767,#195768,#195769,#195770,#195771,#195772,#195773,#195774,
#195775,#195776,#195777,#195778,#195779,#195780,#195781,#195782,#195783,
#195784,#195785,#195786,#195787,#195788,#195789,#195790,#195791,#195792,
#195793,#195794,#195795,#195796,#195797,#195798,#195799,#195800,#195801,
#195802,#195803,#195804,#195805,#195806,#195807,#195808,#195809,#195810,
#195811,#195812,#195813,#195814,#195815,#195816,#195817,#195818,#195819,
#195820,#195821,#195822,#195823,#195824,#195825,#195826,#195827,#195828,
#195829,#195830,#195831,#195832,#195833,#195834,#195835,#195836,#195837,
#195838,#195839,#195840,#195841,#195842,#195843,#195844,#195845,#195846,
#195847,#195848,#195849,#195850,#195851,#195852,#195853,#195854,#195855,
#195856,#195857,#195858,#195859,#195860,#195861,#195862,#195863,#195864,
#195865,#195866,#195867,#195868,#195869,#195870,#195871,#195872,#195873,
#195874,#195875,#195876,#195877,#195878,#195879,#195880,#195881,#195882,
#195883,#195884,#195885,#195886,#195887,#195888,#195889,#195890,#195891,
#195892,#195893,#195894,#195895,#195896,#195897,#195898,#195899,#195900,
#195901,#195902,#195903,#195904,#195905,#195906,#195907,#195908,#195909,
#195910,#195911,#195912,#195913,#195914,#195915,#195916,#195917,#195918,
#195919,#195920,#195921,#195922,#195923,#195924,#195925,#195926,#195927,
#195928,#195929,#195930,#195931,#195932,#195933,#195934,#195935,#195936,
#195937,#195938,#195939,#195940,#195941,#195942,#195943,#195944,#195945,
#195946,#195947,#195948,#195949,#195950,#195951,#195952,#195953,#195954,
#195955,#195956,#195957,#195958,#195959,#195960,#195961,#195962,#195963,
#195964,#195965,#195966,#195967,#195968,#195969,#195970,#195971,#195972,
#195973,#195974,#195975,#195976,#195977,#195978,#195979,#195980,#195981,
#195982,#195983,#195984,#195985,#195986,#195987,#195988,#195989,#195990,
#195991,#195992,#195993,#195994,#195995,#195996,#195997,#195998,#195999,
#196000,#196001,#196002,#196003,#196004,#196005,#196006,#196007,#196008,
#196009,#196010,#196011,#196012,#196013,#196014,#196015,#196016,#196017,
#196018,#196019,#196020,#196021,#196022,#196023,#196024,#196025,#196026,
#196027,#196028,#196029,#196030,#196031,#196032,#196033,#196034,#196035,
#196036,#196037,#196038,#196039,#196040,#196041,#196042,#196043,#196044,
#196045,#196046,#196047,#196048,#196049,#196050,#196051,#196052,#196053),
 .UNSPECIFIED.,.F.,.F.,(4,3,3,3,3,3,3,3,3,3,3,3,3,3,3,3,3,3,3,3,3,3,3,3,
3,3,3,3,3,3,3,3,3,3,3,3,3,3,3,3,3,3,3,3,3,3,3,3,3,3,3,3,3,3,3,3,3,3,3,3,
3,3,3,3,3,3,3,3,3,3,3,3,3,3,3,3,3,3,3,3,3,3,3,3,3,3,3,3,3,3,3,3,3,3,3,3,
3,3,3,3,3,3,3,3,3,3,4),(0.143172102,0.15412844,0.165137615,0.176146789,
0.187155963,0.198165138,0.211009174,0.222018349,0.233027523,0.244036697,
0.255045872,0.266055046,0.27706422,0.289908257,0.300917431,0.311926606,
0.32293578,0.333944954,0.344954128,0.355963303,0.366972477,0.377981651,
0.388990826,0.398165138,0.40733945,0.416513761,0.425688073,0.434862385,
0.444036697,0.453211009,0.464220183,0.473394495,0.482568807,0.491743119,
0.500917431,0.510091743,0.519266055,0.528440367,0.535779817,0.544954128,
0.552293578,0.56146789,0.568807339,0.576146789,0.583486239,0.59266055,0.6,
0.60733945,0.614678899,0.622018349,0.629357798,0.636697248,0.644036697,
0.651376147,0.658715596,0.669724771,0.67706422,0.68440367,0.691743119,0.700917431,
0.708256881,0.71559633,0.72293578,0.730275229,0.737614679,0.744954128,0.752293578,
0.759633028,0.770642202,0.777981651,0.785321101,0.79266055,0.8,0.80733945,
0.812844037,0.820183486,0.825688073,0.831192661,0.83853211,0.844036697,
0.849541284,0.855045872,0.860550459,0.866055046,0.871559633,0.87706422,
0.882568807,0.888073394,0.893577982,0.900917431,0.906422018,0.911926606,
0.917431193,0.924770642,0.930275229,0.935779817,0.941284404,0.946788991,
0.952293578,0.957798165,0.963302752,0.968807339,0.974311927,0.979816514,
0.985321101,0.99266055,1.),.UNSPECIFIED.);
#24369=B_SPLINE_CURVE_WITH_KNOTS('',5,(#197001,#197002,#197003,#197004,
#197005,#197006,#197007,#197008,#197009,#197010,#197011,#197012,#197013,
#197014,#197015,#197016,#197017,#197018,#197019,#197020,#197021,#197022,
#197023,#197024,#197025,#197026,#197027,#197028,#197029,#197030,#197031,
#197032,#197033,#197034,#197035,#197036,#197037,#197038,#197039,#197040,
#197041,#197042,#197043,#197044,#197045,#197046,#197047,#197048,#197049,
#197050,#197051,#197052,#197053,#197054,#197055,#197056,#197057,#197058,
#197059,#197060,#197061,#197062,#197063,#197064,#197065,#197066,#197067,
#197068,#197069,#197070,#197071,#197072,#197073,#197074,#197075,#197076,
#197077,#197078,#197079,#197080,#197081,#197082,#197083,#197084,#197085,
#197086,#197087,#197088,#197089,#197090,#197091,#197092,#197093,#197094,
#197095,#197096,#197097,#197098,#197099,#197100,#197101,#197102,#197103,
#197104,#197105,#197106,#197107,#197108,#197109,#197110,#197111,#197112,
#197113,#197114,#197115,#197116,#197117,#197118,#197119,#197120,#197121,
#197122,#197123,#197124,#197125,#197126,#197127,#197128,#197129,#197130,
#197131,#197132,#197133,#197134,#197135,#197136,#197137,#197138,#197139,
#197140,#197141,#197142,#197143,#197144,#197145,#197146,#197147,#197148,
#197149,#197150,#197151,#197152,#197153,#197154,#197155,#197156,#197157,
#197158,#197159,#197160,#197161,#197162,#197163,#197164,#197165,#197166,
#197167,#197168,#197169,#197170,#197171,#197172,#197173,#197174,#197175,
#197176,#197177,#197178,#197179,#197180,#197181,#197182,#197183,#197184,
#197185,#197186,#197187,#197188,#197189,#197190,#197191,#197192,#197193,
#197194,#197195,#197196,#197197,#197198,#197199,#197200,#197201,#197202,
#197203,#197204,#197205,#197206,#197207,#197208,#197209,#197210,#197211,
#197212,#197213,#197214,#197215,#197216,#197217,#197218,#197219,#197220,
#197221,#197222,#197223,#197224,#197225,#197226,#197227,#197228,#197229,
#197230,#197231,#197232,#197233,#197234,#197235,#197236,#197237,#197238,
#197239,#197240,#197241,#197242,#197243,#197244,#197245,#197246,#197247,
#197248,#197249,#197250,#197251,#197252,#197253,#197254,#197255,#197256,
#197257,#197258,#197259,#197260,#197261,#197262,#197263,#197264,#197265,
#197266,#197267,#197268,#197269,#197270,#197271,#197272,#197273,#197274,
#197275,#197276,#197277,#197278,#197279,#197280,#197281,#197282,#197283,
#197284,#197285,#197286,#197287,#197288,#197289,#197290,#197291,#197292,
#197293,#197294,#197295,#197296,#197297,#197298,#197299,#197300,#197301,
#197302,#197303,#197304,#197305,#197306,#197307,#197308,#197309,#197310,
#197311,#197312,#197313,#197314,#197315,#197316,#197317,#197318,#197319,
#197320,#197321,#197322,#197323,#197324,#197325,#197326,#197327,#197328,
#197329,#197330,#197331,#197332,#197333,#197334,#197335,#197336,#197337,
#197338,#197339,#197340,#197341,#197342,#197343,#197344,#197345,#197346,
#197347,#197348,#197349,#197350,#197351,#197352,#197353,#197354,#197355,
#197356,#197357,#197358,#197359,#197360,#197361,#197362,#197363,#197364,
#197365,#197366,#197367,#197368,#197369,#197370,#197371,#197372,#197373,
#197374,#197375,#197376,#197377,#197378,#197379,#197380,#197381,#197382,
#197383,#197384,#197385,#197386,#197387,#197388,#197389,#197390,#197391,
#197392,#197393,#197394,#197395,#197396,#197397,#197398,#197399,#197400,
#197401,#197402,#197403,#197404,#197405,#197406,#197407,#197408,#197409,
#197410,#197411,#197412,#197413,#197414,#197415,#197416,#197417,#197418,
#197419,#197420,#197421,#197422,#197423,#197424,#197425,#197426,#197427,
#197428,#197429,#197430,#197431,#197432,#197433,#197434,#197435,#197436,
#197437,#197438,#197439,#197440,#197441,#197442,#197443,#197444,#197445,
#197446,#197447,#197448,#197449,#197450,#197451,#197452,#197453,#197454,
#197455,#197456,#197457,#197458,#197459,#197460,#197461,#197462,#197463,
#197464,#197465,#197466,#197467,#197468,#197469,#197470,#197471,#197472),
 .UNSPECIFIED.,.F.,.F.,(6,1,1,1,1,1,1,1,1,1,1,1,1,1,1,1,1,1,1,1,1,1,1,1,
1,1,1,1,1,1,1,1,1,1,1,1,1,1,1,1,1,1,1,1,1,1,1,1,1,1,1,1,1,1,1,1,1,1,1,1,
1,1,1,1,1,1,1,1,1,1,1,1,1,1,1,1,1,1,1,1,1,1,1,1,1,1,1,1,1,1,1,1,1,1,1,1,
1,1,1,1,1,1,1,1,1,1,1,1,1,1,1,1,1,1,1,1,1,1,1,1,1,1,1,1,1,1,1,1,1,1,1,1,
1,1,1,1,1,1,1,1,1,1,1,1,1,1,1,1,1,1,1,1,1,1,1,1,1,1,1,1,1,1,1,1,1,1,1,1,
1,1,1,1,1,1,1,1,1,1,1,1,1,1,1,1,1,1,1,1,1,1,1,1,1,1,1,1,1,1,1,1,1,1,1,1,
1,1,1,1,1,1,1,1,1,1,1,1,1,1,1,1,1,1,1,1,1,1,1,1,1,1,1,1,1,1,1,1,1,1,1,1,
1,1,1,1,1,1,1,1,1,1,1,1,1,1,1,1,1,1,1,1,1,1,1,1,1,1,1,1,1,1,1,1,1,1,1,1,
1,1,1,1,1,1,1,1,1,1,1,1,1,1,1,1,1,1,1,1,1,1,1,1,1,1,1,1,1,1,1,1,1,1,1,1,
1,1,1,1,1,1,1,1,1,1,1,1,1,1,1,1,1,1,1,1,1,1,1,1,1,1,1,1,1,1,1,1,1,1,1,1,
1,1,1,1,1,1,1,1,1,1,1,1,1,1,1,1,1,1,1,1,1,1,1,1,1,1,1,1,1,1,1,1,1,1,1,1,
1,1,1,1,1,1,1,1,1,1,1,1,1,1,1,1,1,1,1,1,1,1,1,1,1,1,1,1,1,1,1,1,1,1,1,1,
1,1,1,1,1,1,1,1,1,1,1,1,1,1,1,1,1,1,1,1,1,1,1,1,1,1,1,1,1,1,1,1,1,1,1,1,
1,1,1,1,1,1,1,1,1,1,1,6),(-1.,-0.998165138,-0.996330275,-0.994495413,-0.99266055,
-0.990825688,-0.988990826,-0.987155963,-0.985321101,-0.983486239,-0.981651376,
-0.979816514,-0.977981651,-0.976146789,-0.974311927,-0.972477064,-0.970642202,
-0.968807339,-0.966972477,-0.965137615,-0.963302752,-0.96146789,-0.959633028,
-0.957798165,-0.955963303,-0.95412844,-0.952293578,-0.950458716,-0.948623853,
-0.946788991,-0.944954128,-0.943119266,-0.941284404,-0.939449541,-0.937614679,
-0.935779817,-0.933944954,-0.932110092,-0.930275229,-0.928440367,-0.926605505,
-0.924770642,-0.92293578,-0.921100917,-0.919266055,-0.917431193,-0.91559633,
-0.913761468,-0.911926606,-0.910091743,-0.908256881,-0.906422018,-0.904587156,
-0.902752294,-0.900917431,-0.899082569,-0.897247706,-0.895412844,-0.893577982,
-0.891743119,-0.889908257,-0.888073394,-0.886238532,-0.88440367,-0.882568807,
-0.880733945,-0.878899083,-0.87706422,-0.875229358,-0.873394495,-0.871559633,
-0.869724771,-0.867889908,-0.866055046,-0.864220183,-0.862385321,-0.860550459,
-0.858715596,-0.856880734,-0.855045872,-0.853211009,-0.851376147,-0.849541284,
-0.847706422,-0.84587156,-0.844036697,-0.842201835,-0.840366972,-0.83853211,
-0.836697248,-0.834862385,-0.833027523,-0.831192661,-0.829357798,-0.827522936,
-0.825688073,-0.823853211,-0.822018349,-0.820183486,-0.818348624,-0.816513761,
-0.814678899,-0.812844037,-0.811009174,-0.809174312,-0.80733945,-0.805504587,
-0.803669725,-0.801834862,-0.8,-0.798165138,-0.796330275,-0.794495413,-0.79266055,
-0.790825688,-0.788990826,-0.787155963,-0.785321101,-0.783486239,-0.781651376,
-0.779816514,-0.777981651,-0.776146789,-0.774311927,-0.772477064,-0.770642202,
-0.768807339,-0.766972477,-0.765137615,-0.763302752,-0.76146789,-0.759633028,
-0.757798165,-0.755963303,-0.75412844,-0.752293578,-0.750458716,-0.748623853,
-0.746788991,-0.744954128,-0.743119266,-0.741284404,-0.739449541,-0.737614679,
-0.735779817,-0.733944954,-0.732110092,-0.730275229,-0.728440367,-0.726605505,
-0.724770642,-0.72293578,-0.721100917,-0.719266055,-0.717431193,-0.71559633,
-0.713761468,-0.711926606,-0.710091743,-0.708256881,-0.706422018,-0.704587156,
-0.702752294,-0.700917431,-0.699082569,-0.697247706,-0.695412844,-0.693577982,
-0.691743119,-0.689908257,-0.688073394,-0.686238532,-0.68440367,-0.682568807,
-0.680733945,-0.678899083,-0.67706422,-0.675229358,-0.673394495,-0.671559633,
-0.669724771,-0.667889908,-0.666055046,-0.664220183,-0.662385321,-0.660550459,
-0.658715596,-0.656880734,-0.655045872,-0.653211009,-0.651376147,-0.649541284,
-0.647706422,-0.64587156,-0.644036697,-0.642201835,-0.640366972,-0.63853211,
-0.636697248,-0.634862385,-0.633027523,-0.631192661,-0.629357798,-0.627522936,
-0.625688073,-0.623853211,-0.622018349,-0.620183486,-0.618348624,-0.616513761,
-0.614678899,-0.612844037,-0.611009174,-0.609174312,-0.60733945,-0.605504587,
-0.603669725,-0.601834862,-0.6,-0.598165138,-0.596330275,-0.594495413,-0.59266055,
-0.590825688,-0.588990826,-0.587155963,-0.585321101,-0.583486239,-0.581651376,
-0.579816514,-0.577981651,-0.576146789,-0.574311927,-0.572477064,-0.570642202,
-0.568807339,-0.566972477,-0.565137615,-0.563302752,-0.56146789,-0.559633028,
-0.557798165,-0.555963303,-0.55412844,-0.552293578,-0.550458716,-0.548623853,
-0.546788991,-0.544954128,-0.543119266,-0.541284404,-0.539449541,-0.537614679,
-0.535779817,-0.533944954,-0.532110092,-0.530275229,-0.528440367,-0.526605505,
-0.524770642,-0.52293578,-0.521100917,-0.519266055,-0.517431193,-0.51559633,
-0.513761468,-0.511926606,-0.510091743,-0.508256881,-0.506422018,-0.504587156,
-0.502752294,-0.500917431,-0.499082569,-0.497247706,-0.495412844,-0.493577982,
-0.491743119,-0.489908257,-0.488073394,-0.486238532,-0.48440367,-0.482568807,
-0.480733945,-0.478899083,-0.47706422,-0.475229358,-0.473394495,-0.471559633,
-0.469724771,-0.467889908,-0.466055046,-0.464220183,-0.462385321,-0.460550459,
-0.458715596,-0.456880734,-0.455045872,-0.453211009,-0.451376147,-0.449541284,
-0.447706422,-0.44587156,-0.444036697,-0.442201835,-0.440366972,-0.43853211,
-0.436697248,-0.434862385,-0.433027523,-0.431192661,-0.429357798,-0.427522936,
-0.425688073,-0.423853211,-0.422018349,-0.420183486,-0.418348624,-0.416513761,
-0.414678899,-0.412844037,-0.411009174,-0.409174312,-0.40733945,-0.405504587,
-0.403669725,-0.401834862,-0.4,-0.398165138,-0.396330275,-0.394495413,-0.39266055,
-0.390825688,-0.388990826,-0.387155963,-0.385321101,-0.383486239,-0.381651376,
-0.379816514,-0.377981651,-0.376146789,-0.374311927,-0.372477064,-0.370642202,
-0.368807339,-0.366972477,-0.365137615,-0.363302752,-0.36146789,-0.359633028,
-0.357798165,-0.355963303,-0.35412844,-0.352293578,-0.350458716,-0.348623853,
-0.346788991,-0.344954128,-0.343119266,-0.341284404,-0.339449541,-0.337614679,
-0.335779817,-0.333944954,-0.332110092,-0.330275229,-0.328440367,-0.326605505,
-0.324770642,-0.32293578,-0.321100917,-0.319266055,-0.317431193,-0.31559633,
-0.313761468,-0.311926606,-0.310091743,-0.308256881,-0.306422018,-0.304587156,
-0.302752294,-0.300917431,-0.299082569,-0.297247706,-0.295412844,-0.293577982,
-0.291743119,-0.289908257,-0.288073394,-0.286238532,-0.28440367,-0.282568807,
-0.280733945,-0.278899083,-0.27706422,-0.275229358,-0.273394495,-0.271559633,
-0.269724771,-0.267889908,-0.266055046,-0.264220183,-0.262385321,-0.260550459,
-0.258715596,-0.256880734,-0.255045872,-0.253211009,-0.251376147,-0.249541284,
-0.247706422,-0.24587156,-0.244036697,-0.242201835,-0.240366972,-0.23853211,
-0.236697248,-0.234862385,-0.233027523,-0.231192661,-0.229357798,-0.227522936,
-0.225688073,-0.223853211,-0.222018349,-0.220183486,-0.218348624,-0.216513761,
-0.214678899,-0.212844037,-0.211009174,-0.209174312,-0.20733945,-0.205504587,
-0.203669725,-0.201834862,-0.2,-0.198165138,-0.196330275,-0.194495413,-0.19266055,
-0.190825688,-0.188990826,-0.187155963,-0.185321101,-0.183486239,-0.181651376,
-0.179816514,-0.177981651,-0.176146789,-0.174311927,-0.172477064,-0.170642202,
-0.168807339,-0.166972477,-0.165137615,-0.163302752,-0.16146789,-0.159633028,
-0.157798165,-0.155963303,-0.15412844,-0.152293578,-0.150458716,-0.148623853,
-0.146788991,-0.144954128,-0.143172102),.UNSPECIFIED.);
#24370=B_SPLINE_CURVE_WITH_KNOTS('',5,(#197473,#197474,#197475,#197476,
#197477,#197478,#197479,#197480,#197481,#197482,#197483,#197484,#197485,
#197486,#197487,#197488,#197489,#197490,#197491,#197492,#197493,#197494,
#197495,#197496,#197497,#197498,#197499,#197500,#197501,#197502,#197503,
#197504,#197505,#197506,#197507,#197508,#197509,#197510,#197511,#197512,
#197513,#197514,#197515,#197516,#197517,#197518,#197519,#197520,#197521,
#197522,#197523,#197524,#197525,#197526,#197527,#197528,#197529,#197530,
#197531,#197532,#197533,#197534,#197535,#197536,#197537,#197538,#197539,
#197540,#197541,#197542,#197543,#197544,#197545,#197546,#197547,#197548,
#197549,#197550,#197551,#197552,#197553,#197554,#197555,#197556,#197557,
#197558,#197559,#197560,#197561,#197562,#197563,#197564,#197565,#197566,
#197567,#197568,#197569,#197570,#197571,#197572,#197573,#197574,#197575,
#197576,#197577,#197578,#197579,#197580,#197581,#197582,#197583,#197584,
#197585,#197586,#197587,#197588,#197589,#197590,#197591,#197592,#197593,
#197594,#197595,#197596,#197597,#197598,#197599,#197600,#197601,#197602,
#197603,#197604,#197605,#197606,#197607,#197608,#197609,#197610,#197611,
#197612,#197613,#197614,#197615,#197616,#197617,#197618,#197619,#197620,
#197621,#197622,#197623,#197624,#197625,#197626,#197627,#197628,#197629,
#197630,#197631,#197632,#197633,#197634,#197635,#197636,#197637,#197638,
#197639,#197640,#197641,#197642,#197643,#197644,#197645,#197646,#197647,
#197648,#197649,#197650,#197651,#197652,#197653,#197654,#197655,#197656,
#197657,#197658,#197659,#197660,#197661,#197662,#197663,#197664,#197665,
#197666,#197667,#197668,#197669,#197670,#197671,#197672,#197673,#197674,
#197675,#197676,#197677,#197678,#197679,#197680,#197681,#197682,#197683,
#197684,#197685,#197686,#197687,#197688,#197689,#197690,#197691,#197692,
#197693,#197694,#197695,#197696,#197697,#197698,#197699,#197700,#197701,
#197702,#197703,#197704,#197705,#197706,#197707,#197708,#197709,#197710,
#197711,#197712,#197713,#197714,#197715,#197716,#197717,#197718,#197719,
#197720,#197721,#197722,#197723,#197724,#197725,#197726,#197727,#197728,
#197729,#197730,#197731,#197732,#197733,#197734,#197735,#197736,#197737,
#197738,#197739,#197740,#197741,#197742,#197743,#197744,#197745,#197746,
#197747,#197748,#197749,#197750,#197751,#197752,#197753,#197754,#197755,
#197756,#197757,#197758,#197759,#197760,#197761,#197762,#197763,#197764,
#197765,#197766,#197767,#197768,#197769,#197770,#197771,#197772,#197773,
#197774,#197775,#197776,#197777,#197778,#197779,#197780,#197781,#197782,
#197783,#197784,#197785,#197786,#197787,#197788,#197789,#197790,#197791,
#197792,#197793,#197794,#197795,#197796,#197797,#197798,#197799,#197800,
#197801,#197802,#197803,#197804,#197805,#197806,#197807,#197808,#197809,
#197810,#197811,#197812,#197813,#197814,#197815,#197816,#197817,#197818,
#197819,#197820,#197821,#197822,#197823,#197824,#197825,#197826,#197827,
#197828,#197829,#197830,#197831,#197832,#197833,#197834,#197835,#197836,
#197837,#197838,#197839,#197840,#197841,#197842,#197843,#197844,#197845,
#197846,#197847,#197848,#197849,#197850,#197851,#197852,#197853,#197854,
#197855,#197856,#197857,#197858,#197859,#197860,#197861,#197862,#197863,
#197864,#197865,#197866,#197867,#197868,#197869,#197870,#197871,#197872,
#197873,#197874,#197875,#197876,#197877,#197878,#197879,#197880,#197881,
#197882,#197883,#197884,#197885,#197886,#197887,#197888,#197889,#197890,
#197891,#197892,#197893,#197894,#197895,#197896,#197897,#197898,#197899,
#197900,#197901,#197902,#197903,#197904,#197905,#197906,#197907,#197908,
#197909,#197910,#197911,#197912,#197913,#197914,#197915,#197916,#197917,
#197918,#197919,#197920,#197921,#197922,#197923,#197924,#197925,#197926,
#197927,#197928,#197929,#197930,#197931,#197932,#197933,#197934,#197935,
#197936,#197937,#197938,#197939,#197940,#197941,#197942,#197943,#197944),
 .UNSPECIFIED.,.F.,.F.,(6,1,1,1,1,1,1,1,1,1,1,1,1,1,1,1,1,1,1,1,1,1,1,1,
1,1,1,1,1,1,1,1,1,1,1,1,1,1,1,1,1,1,1,1,1,1,1,1,1,1,1,1,1,1,1,1,1,1,1,1,
1,1,1,1,1,1,1,1,1,1,1,1,1,1,1,1,1,1,1,1,1,1,1,1,1,1,1,1,1,1,1,1,1,1,1,1,
1,1,1,1,1,1,1,1,1,1,1,1,1,1,1,1,1,1,1,1,1,1,1,1,1,1,1,1,1,1,1,1,1,1,1,1,
1,1,1,1,1,1,1,1,1,1,1,1,1,1,1,1,1,1,1,1,1,1,1,1,1,1,1,1,1,1,1,1,1,1,1,1,
1,1,1,1,1,1,1,1,1,1,1,1,1,1,1,1,1,1,1,1,1,1,1,1,1,1,1,1,1,1,1,1,1,1,1,1,
1,1,1,1,1,1,1,1,1,1,1,1,1,1,1,1,1,1,1,1,1,1,1,1,1,1,1,1,1,1,1,1,1,1,1,1,
1,1,1,1,1,1,1,1,1,1,1,1,1,1,1,1,1,1,1,1,1,1,1,1,1,1,1,1,1,1,1,1,1,1,1,1,
1,1,1,1,1,1,1,1,1,1,1,1,1,1,1,1,1,1,1,1,1,1,1,1,1,1,1,1,1,1,1,1,1,1,1,1,
1,1,1,1,1,1,1,1,1,1,1,1,1,1,1,1,1,1,1,1,1,1,1,1,1,1,1,1,1,1,1,1,1,1,1,1,
1,1,1,1,1,1,1,1,1,1,1,1,1,1,1,1,1,1,1,1,1,1,1,1,1,1,1,1,1,1,1,1,1,1,1,1,
1,1,1,1,1,1,1,1,1,1,1,1,1,1,1,1,1,1,1,1,1,1,1,1,1,1,1,1,1,1,1,1,1,1,1,1,
1,1,1,1,1,1,1,1,1,1,1,1,1,1,1,1,1,1,1,1,1,1,1,1,1,1,1,1,1,1,1,1,1,1,1,1,
1,1,1,1,1,1,1,1,1,1,1,6),(0.143172102,0.144954128,0.146788991,0.148623853,
0.150458716,0.152293578,0.15412844,0.155963303,0.157798165,0.159633028,
0.16146789,0.163302752,0.165137615,0.166972477,0.168807339,0.170642202,
0.172477064,0.174311927,0.176146789,0.177981651,0.179816514,0.181651376,
0.183486239,0.185321101,0.187155963,0.188990826,0.190825688,0.19266055,
0.194495413,0.196330275,0.198165138,0.2,0.201834862,0.203669725,0.205504587,
0.20733945,0.209174312,0.211009174,0.212844037,0.214678899,0.216513761,
0.218348624,0.220183486,0.222018349,0.223853211,0.225688073,0.227522936,
0.229357798,0.231192661,0.233027523,0.234862385,0.236697248,0.23853211,
0.240366972,0.242201835,0.244036697,0.24587156,0.247706422,0.249541284,
0.251376147,0.253211009,0.255045872,0.256880734,0.258715596,0.260550459,
0.262385321,0.264220183,0.266055046,0.267889908,0.269724771,0.271559633,
0.273394495,0.275229358,0.27706422,0.278899083,0.280733945,0.282568807,
0.28440367,0.286238532,0.288073394,0.289908257,0.291743119,0.293577982,
0.295412844,0.297247706,0.299082569,0.300917431,0.302752294,0.304587156,
0.306422018,0.308256881,0.310091743,0.311926606,0.313761468,0.31559633,
0.317431193,0.319266055,0.321100917,0.32293578,0.324770642,0.326605505,
0.328440367,0.330275229,0.332110092,0.333944954,0.335779817,0.337614679,
0.339449541,0.341284404,0.343119266,0.344954128,0.346788991,0.348623853,
0.350458716,0.352293578,0.35412844,0.355963303,0.357798165,0.359633028,
0.36146789,0.363302752,0.365137615,0.366972477,0.368807339,0.370642202,
0.372477064,0.374311927,0.376146789,0.377981651,0.379816514,0.381651376,
0.383486239,0.385321101,0.387155963,0.388990826,0.390825688,0.39266055,
0.394495413,0.396330275,0.398165138,0.4,0.401834862,0.403669725,0.405504587,
0.40733945,0.409174312,0.411009174,0.412844037,0.414678899,0.416513761,
0.418348624,0.420183486,0.422018349,0.423853211,0.425688073,0.427522936,
0.429357798,0.431192661,0.433027523,0.434862385,0.436697248,0.43853211,
0.440366972,0.442201835,0.444036697,0.44587156,0.447706422,0.449541284,
0.451376147,0.453211009,0.455045872,0.456880734,0.458715596,0.460550459,
0.462385321,0.464220183,0.466055046,0.467889908,0.469724771,0.471559633,
0.473394495,0.475229358,0.47706422,0.478899083,0.480733945,0.482568807,
0.48440367,0.486238532,0.488073394,0.489908257,0.491743119,0.493577982,
0.495412844,0.497247706,0.499082569,0.500917431,0.502752294,0.504587156,
0.506422018,0.508256881,0.510091743,0.511926606,0.513761468,0.51559633,
0.517431193,0.519266055,0.521100917,0.52293578,0.524770642,0.526605505,
0.528440367,0.530275229,0.532110092,0.533944954,0.535779817,0.537614679,
0.539449541,0.541284404,0.543119266,0.544954128,0.546788991,0.548623853,
0.550458716,0.552293578,0.55412844,0.555963303,0.557798165,0.559633028,
0.56146789,0.563302752,0.565137615,0.566972477,0.568807339,0.570642202,
0.572477064,0.574311927,0.576146789,0.577981651,0.579816514,0.581651376,
0.583486239,0.585321101,0.587155963,0.588990826,0.590825688,0.59266055,
0.594495413,0.596330275,0.598165138,0.6,0.601834862,0.603669725,0.605504587,
0.60733945,0.609174312,0.611009174,0.612844037,0.614678899,0.616513761,
0.618348624,0.620183486,0.622018349,0.623853211,0.625688073,0.627522936,
0.629357798,0.631192661,0.633027523,0.634862385,0.636697248,0.63853211,
0.640366972,0.642201835,0.644036697,0.64587156,0.647706422,0.649541284,
0.651376147,0.653211009,0.655045872,0.656880734,0.658715596,0.660550459,
0.662385321,0.664220183,0.666055046,0.667889908,0.669724771,0.671559633,
0.673394495,0.675229358,0.67706422,0.678899083,0.680733945,0.682568807,
0.68440367,0.686238532,0.688073394,0.689908257,0.691743119,0.693577982,
0.695412844,0.697247706,0.699082569,0.700917431,0.702752294,0.704587156,
0.706422018,0.708256881,0.710091743,0.711926606,0.713761468,0.71559633,
0.717431193,0.719266055,0.721100917,0.72293578,0.724770642,0.726605505,
0.728440367,0.730275229,0.732110092,0.733944954,0.735779817,0.737614679,
0.739449541,0.741284404,0.743119266,0.744954128,0.746788991,0.748623853,
0.750458716,0.752293578,0.75412844,0.755963303,0.757798165,0.759633028,
0.76146789,0.763302752,0.765137615,0.766972477,0.768807339,0.770642202,
0.772477064,0.774311927,0.776146789,0.777981651,0.779816514,0.781651376,
0.783486239,0.785321101,0.787155963,0.788990826,0.790825688,0.79266055,
0.794495413,0.796330275,0.798165138,0.8,0.801834862,0.803669725,0.805504587,
0.80733945,0.809174312,0.811009174,0.812844037,0.814678899,0.816513761,
0.818348624,0.820183486,0.822018349,0.823853211,0.825688073,0.827522936,
0.829357798,0.831192661,0.833027523,0.834862385,0.836697248,0.83853211,
0.840366972,0.842201835,0.844036697,0.84587156,0.847706422,0.849541284,
0.851376147,0.853211009,0.855045872,0.856880734,0.858715596,0.860550459,
0.862385321,0.864220183,0.866055046,0.867889908,0.869724771,0.871559633,
0.873394495,0.875229358,0.87706422,0.878899083,0.880733945,0.882568807,
0.88440367,0.886238532,0.888073394,0.889908257,0.891743119,0.893577982,
0.895412844,0.897247706,0.899082569,0.900917431,0.902752294,0.904587156,
0.906422018,0.908256881,0.910091743,0.911926606,0.913761468,0.91559633,
0.917431193,0.919266055,0.921100917,0.92293578,0.924770642,0.926605505,
0.928440367,0.930275229,0.932110092,0.933944954,0.935779817,0.937614679,
0.939449541,0.941284404,0.943119266,0.944954128,0.946788991,0.948623853,
0.950458716,0.952293578,0.95412844,0.955963303,0.957798165,0.959633028,
0.96146789,0.963302752,0.965137615,0.966972477,0.968807339,0.970642202,
0.972477064,0.974311927,0.976146789,0.977981651,0.979816514,0.981651376,
0.983486239,0.985321101,0.987155963,0.988990826,0.990825688,0.99266055,
0.994495413,0.996330275,0.998165138,1.),.UNSPECIFIED.);
#24371=B_SPLINE_CURVE_WITH_KNOTS('',3,(#198907,#198908,#198909,#198910,
#198911,#198912,#198913,#198914,#198915,#198916,#198917,#198918,#198919,
#198920,#198921,#198922,#198923,#198924,#198925,#198926,#198927,#198928,
#198929,#198930,#198931,#198932,#198933,#198934,#198935,#198936,#198937,
#198938,#198939,#198940,#198941,#198942,#198943,#198944,#198945,#198946,
#198947,#198948,#198949,#198950,#198951,#198952,#198953,#198954,#198955,
#198956,#198957,#198958,#198959,#198960,#198961,#198962,#198963,#198964,
#198965,#198966,#198967,#198968,#198969,#198970,#198971,#198972,#198973,
#198974,#198975,#198976,#198977,#198978,#198979,#198980,#198981,#198982,
#198983,#198984,#198985,#198986,#198987,#198988,#198989,#198990,#198991,
#198992,#198993,#198994,#198995,#198996,#198997,#198998,#198999,#199000,
#199001,#199002,#199003,#199004,#199005,#199006,#199007,#199008,#199009,
#199010,#199011,#199012,#199013,#199014,#199015,#199016,#199017,#199018,
#199019,#199020,#199021,#199022,#199023,#199024,#199025,#199026,#199027,
#199028,#199029,#199030,#199031,#199032,#199033,#199034,#199035,#199036,
#199037,#199038,#199039,#199040,#199041,#199042,#199043,#199044,#199045,
#199046,#199047,#199048,#199049,#199050,#199051,#199052,#199053,#199054,
#199055,#199056,#199057,#199058,#199059,#199060,#199061,#199062,#199063,
#199064,#199065,#199066,#199067,#199068,#199069,#199070,#199071,#199072,
#199073,#199074,#199075,#199076,#199077,#199078,#199079,#199080,#199081,
#199082,#199083,#199084,#199085,#199086,#199087,#199088,#199089,#199090,
#199091,#199092,#199093,#199094,#199095,#199096,#199097,#199098,#199099,
#199100,#199101,#199102,#199103,#199104,#199105,#199106,#199107,#199108,
#199109,#199110,#199111,#199112,#199113,#199114,#199115,#199116,#199117,
#199118,#199119,#199120,#199121,#199122,#199123,#199124,#199125,#199126,
#199127,#199128,#199129,#199130,#199131,#199132,#199133,#199134,#199135,
#199136,#199137,#199138,#199139,#199140,#199141,#199142,#199143,#199144,
#199145,#199146,#199147,#199148,#199149,#199150,#199151,#199152,#199153,
#199154,#199155,#199156,#199157,#199158,#199159,#199160,#199161,#199162,
#199163,#199164,#199165,#199166,#199167,#199168,#199169,#199170,#199171,
#199172,#199173,#199174,#199175,#199176,#199177,#199178,#199179,#199180,
#199181,#199182,#199183,#199184,#199185,#199186,#199187,#199188,#199189,
#199190,#199191,#199192,#199193,#199194,#199195,#199196,#199197,#199198,
#199199,#199200,#199201,#199202,#199203,#199204,#199205,#199206,#199207,
#199208,#199209,#199210,#199211,#199212,#199213,#199214,#199215,#199216,
#199217,#199218,#199219),.UNSPECIFIED.,.F.,.F.,(4,3,3,3,3,3,3,3,3,3,3,3,
3,3,3,3,3,3,3,3,3,3,3,3,3,3,3,3,3,3,3,3,3,3,3,3,3,3,3,3,3,3,3,3,3,3,3,3,
3,3,3,3,3,3,3,3,3,3,3,3,3,3,3,3,3,3,3,3,3,3,3,3,3,3,3,3,3,3,3,3,3,3,3,3,
3,3,3,3,3,3,3,3,3,3,3,3,3,3,3,3,3,3,3,3,4),(-1.,-0.990825688,-0.985321101,
-0.979816514,-0.974311927,-0.966972477,-0.959633028,-0.95412844,-0.948623853,
-0.941284404,-0.932110092,-0.926605505,-0.921100917,-0.913761468,-0.908256881,
-0.900917431,-0.895412844,-0.889908257,-0.88440367,-0.878899083,-0.873394495,
-0.867889908,-0.860550459,-0.855045872,-0.849541284,-0.842201835,-0.836697248,
-0.831192661,-0.825688073,-0.820183486,-0.814678899,-0.809174312,-0.801834862,
-0.794495413,-0.781651376,-0.774311927,-0.766972477,-0.759633028,-0.752293578,
-0.743119266,-0.735779817,-0.728440367,-0.721100917,-0.708256881,-0.700917431,
-0.693577982,-0.686238532,-0.678899083,-0.671559633,-0.664220183,-0.656880734,
-0.649541284,-0.642201835,-0.634862385,-0.627522936,-0.620183486,-0.612844037,
-0.605504587,-0.598165138,-0.590825688,-0.583486239,-0.576146789,-0.568807339,
-0.56146789,-0.55412844,-0.546788991,-0.539449541,-0.532110092,-0.52293578,
-0.513761468,-0.504587156,-0.495412844,-0.486238532,-0.47706422,-0.467889908,
-0.458715596,-0.447706422,-0.43853211,-0.429357798,-0.420183486,-0.411009174,
-0.401834862,-0.39266055,-0.381651376,-0.370642202,-0.359633028,-0.346788991,
-0.335779817,-0.324770642,-0.313761468,-0.302752294,-0.291743119,-0.278899083,
-0.267889908,-0.256880734,-0.244036697,-0.233027523,-0.222018349,-0.211009174,
-0.2,-0.188990826,-0.177981651,-0.166972477,-0.155963303,-0.143172102),
 .UNSPECIFIED.);
#24372=B_SPLINE_CURVE_WITH_KNOTS('',3,(#199220,#199221,#199222,#199223,
#199224,#199225,#199226,#199227,#199228,#199229,#199230,#199231,#199232,
#199233,#199234,#199235,#199236,#199237,#199238,#199239,#199240,#199241,
#199242,#199243,#199244,#199245,#199246,#199247,#199248,#199249,#199250,
#199251,#199252,#199253,#199254,#199255,#199256,#199257,#199258,#199259,
#199260,#199261,#199262,#199263,#199264,#199265,#199266,#199267,#199268,
#199269,#199270,#199271,#199272,#199273,#199274,#199275,#199276,#199277,
#199278,#199279,#199280,#199281,#199282,#199283,#199284,#199285,#199286,
#199287,#199288,#199289,#199290,#199291,#199292,#199293,#199294,#199295,
#199296,#199297,#199298,#199299,#199300,#199301,#199302,#199303,#199304,
#199305,#199306,#199307,#199308,#199309,#199310,#199311,#199312,#199313,
#199314,#199315,#199316,#199317,#199318,#199319,#199320,#199321,#199322,
#199323,#199324,#199325,#199326,#199327,#199328,#199329,#199330,#199331,
#199332,#199333,#199334,#199335,#199336,#199337,#199338,#199339,#199340,
#199341,#199342,#199343,#199344,#199345,#199346,#199347,#199348,#199349,
#199350,#199351,#199352,#199353,#199354,#199355,#199356,#199357,#199358,
#199359,#199360,#199361,#199362,#199363,#199364,#199365,#199366,#199367,
#199368,#199369,#199370,#199371,#199372,#199373,#199374,#199375,#199376,
#199377,#199378,#199379,#199380,#199381,#199382,#199383,#199384,#199385,
#199386,#199387,#199388,#199389,#199390,#199391,#199392,#199393,#199394,
#199395,#199396,#199397,#199398,#199399,#199400,#199401,#199402,#199403,
#199404,#199405,#199406,#199407,#199408,#199409,#199410,#199411,#199412,
#199413,#199414,#199415,#199416,#199417,#199418,#199419,#199420,#199421,
#199422,#199423,#199424,#199425,#199426,#199427,#199428,#199429,#199430,
#199431,#199432,#199433,#199434,#199435,#199436,#199437,#199438,#199439,
#199440,#199441,#199442,#199443,#199444,#199445,#199446,#199447,#199448,
#199449,#199450,#199451,#199452,#199453,#199454,#199455,#199456,#199457,
#199458,#199459,#199460,#199461,#199462,#199463,#199464,#199465,#199466,
#199467,#199468,#199469,#199470,#199471,#199472,#199473,#199474,#199475,
#199476,#199477,#199478,#199479,#199480,#199481,#199482,#199483,#199484,
#199485,#199486,#199487,#199488,#199489,#199490,#199491,#199492,#199493,
#199494,#199495,#199496,#199497,#199498,#199499,#199500,#199501,#199502,
#199503,#199504,#199505,#199506,#199507,#199508,#199509,#199510,#199511,
#199512,#199513,#199514,#199515,#199516,#199517),.UNSPECIFIED.,.F.,.F.,
(4,3,3,3,3,3,3,3,3,3,3,3,3,3,3,3,3,3,3,3,3,3,3,3,3,3,3,3,3,3,3,3,3,3,3,
3,3,3,3,3,3,3,3,3,3,3,3,3,3,3,3,3,3,3,3,3,3,3,3,3,3,3,3,3,3,3,3,3,3,3,3,
3,3,3,3,3,3,3,3,3,3,3,3,3,3,3,3,3,3,3,3,3,3,3,3,3,3,3,3,4),(0.143172102,
0.15412844,0.165137615,0.176146789,0.187155963,0.198165138,0.211009174,
0.222018349,0.233027523,0.244036697,0.255045872,0.271559633,0.282568807,
0.293577982,0.304587156,0.317431193,0.328440367,0.339449541,0.352293578,
0.363302752,0.374311927,0.385321101,0.396330275,0.405504587,0.414678899,
0.425688073,0.434862385,0.44587156,0.455045872,0.466055046,0.475229358,
0.48440367,0.493577982,0.502752294,0.511926606,0.521100917,0.530275229,
0.543119266,0.552293578,0.56146789,0.568807339,0.576146789,0.585321101,
0.59266055,0.6,0.60733945,0.614678899,0.623853211,0.633027523,0.640366972,
0.649541284,0.658715596,0.666055046,0.673394495,0.680733945,0.688073394,
0.695412844,0.704587156,0.713761468,0.721100917,0.728440367,0.739449541,
0.748623853,0.755963303,0.763302752,0.770642202,0.777981651,0.785321101,
0.79266055,0.803669725,0.814678899,0.820183486,0.825688073,0.831192661,
0.836697248,0.842201835,0.847706422,0.853211009,0.858715596,0.864220183,
0.873394495,0.878899083,0.88440367,0.889908257,0.897247706,0.906422018,
0.91559633,0.924770642,0.930275229,0.935779817,0.944954128,0.950458716,
0.955963303,0.963302752,0.968807339,0.974311927,0.979816514,0.987155963,
0.99266055,1.),.UNSPECIFIED.);
#24373=B_SPLINE_CURVE_WITH_KNOTS('',3,(#200462,#200463,#200464,#200465,
#200466,#200467,#200468,#200469,#200470,#200471,#200472,#200473,#200474,
#200475,#200476,#200477,#200478,#200479,#200480,#200481,#200482,#200483,
#200484,#200485,#200486,#200487,#200488,#200489,#200490,#200491,#200492,
#200493,#200494,#200495,#200496,#200497,#200498,#200499,#200500,#200501,
#200502,#200503,#200504,#200505,#200506,#200507,#200508,#200509,#200510,
#200511,#200512,#200513,#200514,#200515,#200516,#200517,#200518,#200519,
#200520,#200521,#200522,#200523,#200524,#200525,#200526,#200527,#200528,
#200529,#200530,#200531,#200532,#200533,#200534,#200535,#200536,#200537,
#200538,#200539,#200540,#200541,#200542,#200543,#200544,#200545,#200546,
#200547,#200548,#200549,#200550,#200551,#200552,#200553,#200554,#200555,
#200556,#200557,#200558,#200559,#200560,#200561,#200562,#200563,#200564,
#200565,#200566,#200567,#200568,#200569,#200570,#200571,#200572,#200573,
#200574,#200575,#200576,#200577,#200578,#200579,#200580,#200581,#200582,
#200583,#200584,#200585,#200586,#200587,#200588,#200589,#200590,#200591,
#200592,#200593,#200594,#200595,#200596,#200597,#200598,#200599,#200600,
#200601,#200602,#200603,#200604,#200605,#200606,#200607,#200608,#200609,
#200610,#200611,#200612,#200613,#200614,#200615,#200616,#200617,#200618,
#200619,#200620,#200621,#200622,#200623,#200624,#200625,#200626,#200627,
#200628,#200629,#200630,#200631,#200632,#200633,#200634,#200635,#200636,
#200637,#200638,#200639,#200640,#200641,#200642,#200643,#200644,#200645,
#200646,#200647,#200648,#200649,#200650,#200651,#200652,#200653,#200654,
#200655,#200656,#200657,#200658,#200659,#200660,#200661,#200662,#200663,
#200664,#200665,#200666,#200667,#200668,#200669,#200670,#200671,#200672,
#200673,#200674,#200675,#200676,#200677,#200678,#200679,#200680,#200681,
#200682,#200683,#200684,#200685,#200686,#200687,#200688,#200689,#200690,
#200691,#200692,#200693,#200694,#200695,#200696,#200697,#200698,#200699,
#200700,#200701,#200702,#200703,#200704,#200705,#200706,#200707,#200708,
#200709,#200710,#200711,#200712,#200713,#200714,#200715,#200716,#200717,
#200718,#200719,#200720,#200721,#200722,#200723,#200724,#200725,#200726,
#200727,#200728,#200729,#200730,#200731,#200732,#200733,#200734,#200735,
#200736,#200737,#200738,#200739,#200740,#200741,#200742,#200743,#200744,
#200745,#200746,#200747,#200748,#200749,#200750,#200751,#200752,#200753,
#200754,#200755,#200756,#200757,#200758,#200759,#200760,#200761,#200762,
#200763,#200764,#200765,#200766,#200767,#200768,#200769,#200770,#200771,
#200772,#200773,#200774,#200775,#200776,#200777),.UNSPECIFIED.,.F.,.F.,
(4,3,3,3,3,3,3,3,3,3,3,3,3,3,3,3,3,3,3,3,3,3,3,3,3,3,3,3,3,3,3,3,3,3,3,
3,3,3,3,3,3,3,3,3,3,3,3,3,3,3,3,3,3,3,3,3,3,3,3,3,3,3,3,3,3,3,3,3,3,3,3,
3,3,3,3,3,3,3,3,3,3,3,3,3,3,3,3,3,3,3,3,3,3,3,3,3,3,3,3,3,3,3,3,3,3,4),
(0.143172102,0.15412844,0.165137615,0.176146789,0.187155963,0.198165138,
0.211009174,0.222018349,0.233027523,0.244036697,0.255045872,0.266055046,
0.27706422,0.288073394,0.299082569,0.310091743,0.321100917,0.332110092,
0.343119266,0.355963303,0.366972477,0.377981651,0.388990826,0.398165138,
0.40733945,0.418348624,0.427522936,0.436697248,0.44587156,0.455045872,0.464220183,
0.473394495,0.482568807,0.491743119,0.500917431,0.510091743,0.519266055,
0.528440367,0.535779817,0.543119266,0.550458716,0.557798165,0.565137615,
0.572477064,0.579816514,0.587155963,0.594495413,0.601834862,0.609174312,
0.616513761,0.625688073,0.633027523,0.640366972,0.649541284,0.656880734,
0.666055046,0.673394495,0.680733945,0.689908257,0.697247706,0.704587156,
0.711926606,0.719266055,0.726605505,0.733944954,0.741284404,0.748623853,
0.755963303,0.763302752,0.772477064,0.779816514,0.787155963,0.794495413,
0.803669725,0.811009174,0.816513761,0.822018349,0.827522936,0.833027523,
0.83853211,0.844036697,0.851376147,0.858715596,0.866055046,0.871559633,
0.878899083,0.886238532,0.891743119,0.897247706,0.902752294,0.910091743,
0.91559633,0.921100917,0.926605505,0.932110092,0.937614679,0.943119266,
0.950458716,0.957798165,0.965137615,0.970642202,0.976146789,0.981651376,
0.988990826,0.994495413,1.),.UNSPECIFIED.);
#24374=B_SPLINE_CURVE_WITH_KNOTS('',3,(#200778,#200779,#200780,#200781,
#200782,#200783,#200784,#200785,#200786,#200787,#200788,#200789,#200790,
#200791,#200792,#200793,#200794,#200795,#200796,#200797,#200798,#200799,
#200800,#200801,#200802,#200803,#200804,#200805,#200806,#200807,#200808,
#200809,#200810,#200811,#200812,#200813,#200814,#200815,#200816,#200817,
#200818,#200819,#200820,#200821,#200822,#200823,#200824,#200825,#200826,
#200827,#200828,#200829,#200830,#200831,#200832,#200833,#200834,#200835,
#200836,#200837,#200838,#200839,#200840,#200841,#200842,#200843,#200844,
#200845,#200846,#200847,#200848,#200849,#200850,#200851,#200852,#200853,
#200854,#200855,#200856,#200857,#200858,#200859,#200860,#200861,#200862,
#200863,#200864,#200865,#200866,#200867,#200868,#200869,#200870,#200871,
#200872,#200873,#200874,#200875,#200876,#200877,#200878,#200879,#200880,
#200881,#200882,#200883,#200884,#200885,#200886,#200887,#200888,#200889,
#200890,#200891,#200892,#200893,#200894,#200895,#200896,#200897,#200898,
#200899,#200900,#200901,#200902,#200903,#200904,#200905,#200906,#200907,
#200908,#200909,#200910,#200911,#200912,#200913,#200914,#200915,#200916,
#200917,#200918,#200919,#200920,#200921,#200922,#200923,#200924,#200925,
#200926,#200927,#200928,#200929,#200930,#200931,#200932,#200933,#200934,
#200935,#200936,#200937,#200938,#200939,#200940,#200941,#200942,#200943,
#200944,#200945,#200946,#200947,#200948,#200949,#200950,#200951,#200952,
#200953,#200954,#200955,#200956,#200957,#200958,#200959,#200960,#200961,
#200962,#200963,#200964,#200965,#200966,#200967,#200968,#200969,#200970,
#200971,#200972,#200973,#200974,#200975,#200976,#200977,#200978,#200979,
#200980,#200981,#200982,#200983,#200984,#200985,#200986,#200987,#200988,
#200989,#200990,#200991,#200992,#200993,#200994,#200995,#200996,#200997,
#200998,#200999,#201000,#201001,#201002,#201003,#201004,#201005,#201006,
#201007,#201008,#201009,#201010,#201011,#201012,#201013,#201014,#201015,
#201016,#201017,#201018,#201019,#201020,#201021,#201022,#201023,#201024,
#201025,#201026,#201027,#201028,#201029,#201030,#201031,#201032,#201033,
#201034,#201035,#201036,#201037,#201038,#201039,#201040,#201041,#201042,
#201043,#201044,#201045,#201046,#201047,#201048,#201049,#201050,#201051,
#201052,#201053,#201054,#201055,#201056,#201057,#201058,#201059,#201060,
#201061,#201062,#201063,#201064,#201065,#201066,#201067,#201068,#201069,
#201070,#201071,#201072,#201073,#201074,#201075,#201076,#201077,#201078,
#201079,#201080,#201081,#201082,#201083,#201084,#201085,#201086,#201087,
#201088,#201089,#201090,#201091,#201092,#201093,#201094,#201095,#201096,
#201097,#201098,#201099,#201100,#201101,#201102),.UNSPECIFIED.,.F.,.F.,
(4,3,3,3,3,3,3,3,3,3,3,3,3,3,3,3,3,3,3,3,3,3,3,3,3,3,3,3,3,3,3,3,3,3,3,
3,3,3,3,3,3,3,3,3,3,3,3,3,3,3,3,3,3,3,3,3,3,3,3,3,3,3,3,3,3,3,3,3,3,3,3,
3,3,3,3,3,3,3,3,3,3,3,3,3,3,3,3,3,3,3,3,3,3,3,3,3,3,3,3,3,3,3,3,3,3,3,3,
3,4),(0.143172102,0.15412844,0.165137615,0.176146789,0.187155963,0.198165138,
0.209174312,0.220183486,0.231192661,0.242201835,0.253211009,0.264220183,
0.275229358,0.286238532,0.297247706,0.308256881,0.319266055,0.330275229,
0.341284404,0.352293578,0.363302752,0.374311927,0.385321101,0.396330275,
0.405504587,0.414678899,0.423853211,0.433027523,0.442201835,0.451376147,
0.460550459,0.469724771,0.478899083,0.488073394,0.497247706,0.506422018,
0.51559633,0.524770642,0.533944954,0.541284404,0.548623853,0.555963303,
0.563302752,0.570642202,0.577981651,0.585321101,0.59266055,0.6,0.60733945,
0.614678899,0.622018349,0.629357798,0.636697248,0.644036697,0.651376147,
0.658715596,0.666055046,0.673394495,0.680733945,0.688073394,0.695412844,
0.704587156,0.711926606,0.719266055,0.726605505,0.733944954,0.741284404,
0.748623853,0.755963303,0.763302752,0.772477064,0.779816514,0.787155963,
0.794495413,0.803669725,0.811009174,0.816513761,0.822018349,0.827522936,
0.833027523,0.840366972,0.84587156,0.853211009,0.858715596,0.864220183,
0.869724771,0.875229358,0.880733945,0.886238532,0.891743119,0.897247706,
0.902752294,0.908256881,0.913761468,0.919266055,0.924770642,0.930275229,
0.935779817,0.941284404,0.946788991,0.95412844,0.959633028,0.965137615,
0.970642202,0.976146789,0.981651376,0.987155963,0.99266055,1.),
 .UNSPECIFIED.);
#24375=B_SPLINE_CURVE_WITH_KNOTS('',3,(#202062,#202063,#202064,#202065,
#202066,#202067,#202068,#202069,#202070,#202071,#202072,#202073,#202074,
#202075,#202076,#202077,#202078,#202079,#202080,#202081,#202082,#202083,
#202084,#202085,#202086,#202087,#202088,#202089,#202090,#202091,#202092,
#202093,#202094,#202095,#202096,#202097,#202098,#202099,#202100,#202101,
#202102,#202103,#202104,#202105,#202106,#202107,#202108,#202109,#202110,
#202111,#202112,#202113,#202114,#202115,#202116,#202117,#202118,#202119,
#202120,#202121,#202122,#202123,#202124,#202125,#202126,#202127,#202128,
#202129,#202130,#202131,#202132,#202133,#202134,#202135,#202136,#202137,
#202138,#202139,#202140,#202141,#202142,#202143,#202144,#202145,#202146,
#202147,#202148,#202149,#202150,#202151,#202152,#202153,#202154,#202155,
#202156,#202157,#202158,#202159,#202160,#202161,#202162,#202163,#202164,
#202165,#202166,#202167,#202168,#202169,#202170,#202171,#202172,#202173,
#202174,#202175,#202176,#202177,#202178,#202179,#202180,#202181,#202182,
#202183,#202184,#202185,#202186,#202187,#202188,#202189,#202190,#202191,
#202192,#202193,#202194,#202195,#202196,#202197,#202198,#202199,#202200,
#202201,#202202,#202203,#202204,#202205,#202206,#202207,#202208,#202209,
#202210,#202211,#202212,#202213,#202214,#202215,#202216,#202217,#202218,
#202219,#202220,#202221,#202222,#202223,#202224,#202225,#202226,#202227,
#202228,#202229,#202230,#202231,#202232,#202233,#202234,#202235,#202236,
#202237,#202238,#202239,#202240,#202241,#202242,#202243,#202244,#202245,
#202246,#202247,#202248,#202249,#202250,#202251,#202252,#202253,#202254,
#202255,#202256,#202257,#202258,#202259,#202260,#202261,#202262,#202263,
#202264,#202265,#202266,#202267,#202268,#202269,#202270,#202271,#202272,
#202273,#202274,#202275,#202276,#202277,#202278,#202279,#202280,#202281,
#202282,#202283,#202284,#202285,#202286,#202287,#202288,#202289,#202290,
#202291,#202292,#202293,#202294,#202295,#202296,#202297,#202298,#202299,
#202300,#202301,#202302,#202303,#202304,#202305,#202306,#202307,#202308,
#202309,#202310,#202311,#202312,#202313,#202314,#202315,#202316,#202317,
#202318,#202319,#202320,#202321,#202322,#202323,#202324,#202325,#202326,
#202327,#202328,#202329,#202330,#202331,#202332,#202333,#202334,#202335,
#202336,#202337,#202338,#202339,#202340,#202341,#202342,#202343,#202344,
#202345,#202346,#202347,#202348,#202349,#202350,#202351,#202352,#202353,
#202354,#202355,#202356,#202357,#202358,#202359,#202360,#202361,#202362,
#202363,#202364,#202365,#202366,#202367,#202368,#202369,#202370,#202371),
 .UNSPECIFIED.,.F.,.F.,(4,3,3,3,3,3,3,3,3,3,3,3,3,3,3,3,3,3,3,3,3,3,3,3,
3,3,3,3,3,3,3,3,3,3,3,3,3,3,3,3,3,3,3,3,3,3,3,3,3,3,3,3,3,3,3,3,3,3,3,3,
3,3,3,3,3,3,3,3,3,3,3,3,3,3,3,3,3,3,3,3,3,3,3,3,3,3,3,3,3,3,3,3,3,3,3,3,
3,3,3,3,3,3,3,4),(0.143172102,0.15412844,0.165137615,0.177981651,0.188990826,
0.201834862,0.212844037,0.225688073,0.236697248,0.249541284,0.260550459,
0.271559633,0.282568807,0.293577982,0.304587156,0.317431193,0.328440367,
0.339449541,0.350458716,0.36146789,0.372477064,0.383486239,0.394495413,
0.403669725,0.412844037,0.423853211,0.433027523,0.442201835,0.451376147,
0.460550459,0.469724771,0.478899083,0.488073394,0.497247706,0.506422018,
0.51559633,0.524770642,0.533944954,0.541284404,0.550458716,0.557798165,
0.566972477,0.574311927,0.583486239,0.59266055,0.6,0.60733945,0.614678899,
0.622018349,0.629357798,0.63853211,0.64587156,0.655045872,0.666055046,0.673394495,
0.680733945,0.689908257,0.700917431,0.708256881,0.71559633,0.72293578,0.732110092,
0.739449541,0.746788991,0.757798165,0.766972477,0.774311927,0.781651376,
0.788990826,0.796330275,0.80733945,0.812844037,0.818348624,0.823853211,
0.829357798,0.834862385,0.840366972,0.84587156,0.855045872,0.860550459,
0.866055046,0.871559633,0.87706422,0.882568807,0.888073394,0.893577982,
0.899082569,0.906422018,0.911926606,0.917431193,0.92293578,0.928440367,
0.933944954,0.941284404,0.946788991,0.952293578,0.957798165,0.963302752,
0.970642202,0.976146789,0.981651376,0.987155963,0.99266055,1.),
 .UNSPECIFIED.);
#24376=B_SPLINE_CURVE_WITH_KNOTS('',3,(#202372,#202373,#202374,#202375,
#202376,#202377,#202378,#202379,#202380,#202381,#202382,#202383,#202384,
#202385,#202386,#202387,#202388,#202389,#202390,#202391,#202392,#202393,
#202394,#202395,#202396,#202397,#202398,#202399,#202400,#202401,#202402,
#202403,#202404,#202405,#202406,#202407,#202408,#202409,#202410,#202411,
#202412,#202413,#202414,#202415,#202416,#202417,#202418,#202419,#202420,
#202421,#202422,#202423,#202424,#202425,#202426,#202427,#202428,#202429,
#202430,#202431,#202432,#202433,#202434,#202435,#202436,#202437,#202438,
#202439,#202440,#202441,#202442,#202443,#202444,#202445,#202446,#202447,
#202448,#202449,#202450,#202451,#202452,#202453,#202454,#202455,#202456,
#202457,#202458,#202459,#202460,#202461,#202462,#202463,#202464,#202465,
#202466,#202467,#202468,#202469,#202470,#202471,#202472,#202473,#202474,
#202475,#202476,#202477,#202478,#202479,#202480,#202481,#202482,#202483,
#202484,#202485,#202486,#202487,#202488,#202489,#202490,#202491,#202492,
#202493,#202494,#202495,#202496,#202497,#202498,#202499,#202500,#202501,
#202502,#202503,#202504,#202505,#202506,#202507,#202508,#202509,#202510,
#202511,#202512,#202513,#202514,#202515,#202516,#202517,#202518,#202519,
#202520,#202521,#202522,#202523,#202524,#202525,#202526,#202527,#202528,
#202529,#202530,#202531,#202532,#202533,#202534,#202535,#202536,#202537,
#202538,#202539,#202540,#202541,#202542,#202543,#202544,#202545,#202546,
#202547,#202548,#202549,#202550,#202551,#202552,#202553,#202554,#202555,
#202556,#202557,#202558,#202559,#202560,#202561,#202562,#202563,#202564,
#202565,#202566,#202567,#202568,#202569,#202570,#202571,#202572,#202573,
#202574,#202575,#202576,#202577,#202578,#202579,#202580,#202581,#202582,
#202583,#202584,#202585,#202586,#202587,#202588,#202589,#202590,#202591,
#202592,#202593,#202594,#202595,#202596,#202597,#202598,#202599,#202600,
#202601,#202602,#202603,#202604,#202605,#202606,#202607,#202608,#202609,
#202610,#202611,#202612,#202613,#202614,#202615,#202616,#202617,#202618,
#202619,#202620,#202621,#202622,#202623,#202624,#202625,#202626,#202627,
#202628,#202629,#202630,#202631,#202632,#202633,#202634,#202635,#202636,
#202637,#202638,#202639,#202640,#202641,#202642,#202643,#202644,#202645,
#202646,#202647,#202648,#202649,#202650,#202651,#202652,#202653,#202654,
#202655,#202656,#202657,#202658,#202659,#202660,#202661,#202662,#202663,
#202664,#202665,#202666,#202667,#202668,#202669,#202670,#202671,#202672,
#202673,#202674,#202675,#202676,#202677,#202678,#202679,#202680,#202681,
#202682,#202683,#202684,#202685,#202686,#202687,#202688,#202689,#202690,
#202691,#202692,#202693,#202694,#202695,#202696,#202697,#202698,#202699),
 .UNSPECIFIED.,.F.,.F.,(4,3,3,3,3,3,3,3,3,3,3,3,3,3,3,3,3,3,3,3,3,3,3,3,
3,3,3,3,3,3,3,3,3,3,3,3,3,3,3,3,3,3,3,3,3,3,3,3,3,3,3,3,3,3,3,3,3,3,3,3,
3,3,3,3,3,3,3,3,3,3,3,3,3,3,3,3,3,3,3,3,3,3,3,3,3,3,3,3,3,3,3,3,3,3,3,3,
3,3,3,3,3,3,3,3,3,3,3,3,3,4),(0.143172102,0.15412844,0.165137615,0.177981651,
0.188990826,0.201834862,0.212844037,0.225688073,0.236697248,0.247706422,
0.258715596,0.269724771,0.280733945,0.291743119,0.302752294,0.313761468,
0.324770642,0.335779817,0.346788991,0.357798165,0.368807339,0.379816514,
0.390825688,0.4,0.409174312,0.418348624,0.427522936,0.436697248,0.44587156,
0.455045872,0.464220183,0.473394495,0.482568807,0.491743119,0.500917431,
0.510091743,0.519266055,0.528440367,0.535779817,0.543119266,0.550458716,
0.557798165,0.565137615,0.572477064,0.579816514,0.587155963,0.594495413,
0.601834862,0.609174312,0.616513761,0.623853211,0.631192661,0.63853211,
0.64587156,0.653211009,0.660550459,0.667889908,0.675229358,0.682568807,
0.689908257,0.697247706,0.704587156,0.711926606,0.719266055,0.726605505,
0.733944954,0.741284404,0.748623853,0.755963303,0.763302752,0.772477064,
0.779816514,0.787155963,0.794495413,0.801834862,0.809174312,0.814678899,
0.820183486,0.825688073,0.831192661,0.836697248,0.842201835,0.849541284,
0.855045872,0.860550459,0.866055046,0.871559633,0.87706422,0.882568807,
0.888073394,0.893577982,0.899082569,0.904587156,0.910091743,0.91559633,
0.921100917,0.926605505,0.932110092,0.937614679,0.943119266,0.948623853,
0.95412844,0.959633028,0.965137615,0.970642202,0.976146789,0.981651376,
0.987155963,0.99266055,1.),.UNSPECIFIED.);
#24377=B_SPLINE_CURVE_WITH_KNOTS('',3,(#203647,#203648,#203649,#203650,
#203651,#203652,#203653,#203654,#203655,#203656,#203657,#203658,#203659,
#203660,#203661,#203662,#203663,#203664,#203665,#203666,#203667,#203668,
#203669,#203670,#203671,#203672,#203673,#203674,#203675,#203676,#203677,
#203678,#203679,#203680,#203681,#203682,#203683,#203684,#203685,#203686,
#203687,#203688,#203689,#203690,#203691,#203692,#203693,#203694,#203695,
#203696,#203697,#203698,#203699,#203700,#203701,#203702,#203703,#203704,
#203705,#203706,#203707,#203708,#203709,#203710,#203711,#203712,#203713,
#203714,#203715,#203716,#203717,#203718,#203719,#203720,#203721,#203722,
#203723,#203724,#203725,#203726,#203727,#203728,#203729,#203730,#203731,
#203732,#203733,#203734,#203735,#203736,#203737,#203738,#203739,#203740,
#203741,#203742,#203743,#203744,#203745,#203746,#203747,#203748,#203749,
#203750,#203751,#203752,#203753,#203754,#203755,#203756,#203757,#203758,
#203759,#203760,#203761,#203762,#203763,#203764,#203765,#203766,#203767,
#203768,#203769,#203770,#203771,#203772,#203773,#203774,#203775,#203776,
#203777,#203778,#203779,#203780,#203781,#203782,#203783,#203784,#203785,
#203786,#203787,#203788,#203789,#203790,#203791,#203792,#203793,#203794,
#203795,#203796,#203797,#203798,#203799,#203800,#203801,#203802,#203803,
#203804,#203805,#203806,#203807,#203808,#203809,#203810,#203811,#203812,
#203813,#203814,#203815,#203816,#203817,#203818,#203819,#203820,#203821,
#203822,#203823,#203824,#203825,#203826,#203827,#203828,#203829,#203830,
#203831,#203832,#203833,#203834,#203835,#203836,#203837,#203838,#203839,
#203840,#203841,#203842,#203843,#203844,#203845,#203846,#203847,#203848,
#203849,#203850,#203851,#203852,#203853,#203854,#203855,#203856,#203857,
#203858,#203859,#203860,#203861,#203862,#203863,#203864,#203865,#203866,
#203867,#203868,#203869,#203870,#203871,#203872,#203873,#203874,#203875,
#203876,#203877,#203878,#203879,#203880,#203881,#203882,#203883,#203884,
#203885,#203886,#203887,#203888,#203889,#203890,#203891,#203892,#203893,
#203894,#203895,#203896,#203897,#203898,#203899,#203900,#203901,#203902,
#203903,#203904,#203905,#203906,#203907,#203908,#203909,#203910,#203911,
#203912,#203913,#203914,#203915,#203916,#203917,#203918,#203919,#203920,
#203921,#203922,#203923,#203924,#203925,#203926,#203927,#203928,#203929,
#203930,#203931,#203932,#203933,#203934,#203935,#203936,#203937,#203938,
#203939,#203940,#203941,#203942,#203943,#203944,#203945,#203946,#203947,
#203948,#203949,#203950,#203951,#203952,#203953,#203954,#203955,#203956,
#203957,#203958,#203959,#203960,#203961,#203962,#203963,#203964,#203965,
#203966,#203967,#203968),.UNSPECIFIED.,.F.,.F.,(4,3,3,3,3,3,3,3,3,3,3,3,
3,3,3,3,3,3,3,3,3,3,3,3,3,3,3,3,3,3,3,3,3,3,3,3,3,3,3,3,3,3,3,3,3,3,3,3,
3,3,3,3,3,3,3,3,3,3,3,3,3,3,3,3,3,3,3,3,3,3,3,3,3,3,3,3,3,3,3,3,3,3,3,3,
3,3,3,3,3,3,3,3,3,3,3,3,3,3,3,3,3,3,3,3,3,3,3,4),(-1.,-0.994495413,-0.988990826,
-0.983486239,-0.977981651,-0.972477064,-0.966972477,-0.96146789,-0.955963303,
-0.950458716,-0.944954128,-0.937614679,-0.932110092,-0.926605505,-0.919266055,
-0.913761468,-0.908256881,-0.900917431,-0.895412844,-0.889908257,-0.88440367,
-0.878899083,-0.873394495,-0.867889908,-0.860550459,-0.855045872,-0.849541284,
-0.844036697,-0.83853211,-0.833027523,-0.827522936,-0.822018349,-0.814678899,
-0.809174312,-0.801834862,-0.794495413,-0.787155963,-0.779816514,-0.770642202,
-0.763302752,-0.755963303,-0.748623853,-0.741284404,-0.733944954,-0.726605505,
-0.719266055,-0.710091743,-0.702752294,-0.695412844,-0.688073394,-0.675229358,
-0.667889908,-0.660550459,-0.653211009,-0.64587156,-0.63853211,-0.631192661,
-0.623853211,-0.616513761,-0.609174312,-0.601834862,-0.594495413,-0.587155963,
-0.579816514,-0.572477064,-0.565137615,-0.557798165,-0.550458716,-0.543119266,
-0.535779817,-0.528440367,-0.519266055,-0.510091743,-0.500917431,-0.491743119,
-0.482568807,-0.473394495,-0.464220183,-0.455045872,-0.44587156,-0.436697248,
-0.427522936,-0.418348624,-0.409174312,-0.4,-0.390825688,-0.379816514,-0.368807339,
-0.357798165,-0.346788991,-0.335779817,-0.324770642,-0.313761468,-0.302752294,
-0.291743119,-0.280733945,-0.269724771,-0.258715596,-0.247706422,-0.236697248,
-0.225688073,-0.212844037,-0.201834862,-0.188990826,-0.177981651,-0.165137615,
-0.15412844,-0.143172102),.UNSPECIFIED.);
#24378=B_SPLINE_CURVE_WITH_KNOTS('',3,(#203969,#203970,#203971,#203972,
#203973,#203974,#203975,#203976,#203977,#203978,#203979,#203980,#203981,
#203982,#203983,#203984,#203985,#203986,#203987,#203988,#203989,#203990,
#203991,#203992,#203993,#203994,#203995,#203996,#203997,#203998,#203999,
#204000,#204001,#204002,#204003,#204004,#204005,#204006,#204007,#204008,
#204009,#204010,#204011,#204012,#204013,#204014,#204015,#204016,#204017,
#204018,#204019,#204020,#204021,#204022,#204023,#204024,#204025,#204026,
#204027,#204028,#204029,#204030,#204031,#204032,#204033,#204034,#204035,
#204036,#204037,#204038,#204039,#204040,#204041,#204042,#204043,#204044,
#204045,#204046,#204047,#204048,#204049,#204050,#204051,#204052,#204053,
#204054,#204055,#204056,#204057,#204058,#204059,#204060,#204061,#204062,
#204063,#204064,#204065,#204066,#204067,#204068,#204069,#204070,#204071,
#204072,#204073,#204074,#204075,#204076,#204077,#204078,#204079,#204080,
#204081,#204082,#204083,#204084,#204085,#204086,#204087,#204088,#204089,
#204090,#204091,#204092,#204093,#204094,#204095,#204096,#204097,#204098,
#204099,#204100,#204101,#204102,#204103,#204104,#204105,#204106,#204107,
#204108,#204109,#204110,#204111,#204112,#204113,#204114,#204115,#204116,
#204117,#204118,#204119,#204120,#204121,#204122,#204123,#204124,#204125,
#204126,#204127,#204128,#204129,#204130,#204131,#204132,#204133,#204134,
#204135,#204136,#204137,#204138,#204139,#204140,#204141,#204142,#204143,
#204144,#204145,#204146,#204147,#204148,#204149,#204150,#204151,#204152,
#204153,#204154,#204155,#204156,#204157,#204158,#204159,#204160,#204161,
#204162,#204163,#204164,#204165,#204166,#204167,#204168,#204169,#204170,
#204171,#204172,#204173,#204174,#204175,#204176,#204177,#204178,#204179,
#204180,#204181,#204182,#204183,#204184,#204185,#204186,#204187,#204188,
#204189,#204190,#204191,#204192,#204193,#204194,#204195,#204196,#204197,
#204198,#204199,#204200,#204201,#204202,#204203,#204204,#204205,#204206,
#204207,#204208,#204209,#204210,#204211,#204212,#204213,#204214,#204215,
#204216,#204217,#204218,#204219,#204220,#204221,#204222,#204223,#204224,
#204225,#204226,#204227,#204228,#204229,#204230,#204231,#204232,#204233,
#204234,#204235,#204236,#204237,#204238,#204239,#204240,#204241,#204242,
#204243,#204244,#204245,#204246,#204247,#204248,#204249,#204250,#204251,
#204252,#204253,#204254,#204255,#204256,#204257,#204258,#204259,#204260,
#204261,#204262,#204263,#204264,#204265,#204266,#204267,#204268,#204269,
#204270,#204271,#204272,#204273,#204274,#204275,#204276,#204277,#204278),
 .UNSPECIFIED.,.F.,.F.,(4,3,3,3,3,3,3,3,3,3,3,3,3,3,3,3,3,3,3,3,3,3,3,3,
3,3,3,3,3,3,3,3,3,3,3,3,3,3,3,3,3,3,3,3,3,3,3,3,3,3,3,3,3,3,3,3,3,3,3,3,
3,3,3,3,3,3,3,3,3,3,3,3,3,3,3,3,3,3,3,3,3,3,3,3,3,3,3,3,3,3,3,3,3,3,3,3,
3,3,3,3,3,3,3,4),(0.143172102,0.15412844,0.165137615,0.176146789,0.187155963,
0.198165138,0.209174312,0.222018349,0.233027523,0.244036697,0.255045872,
0.266055046,0.27706422,0.288073394,0.299082569,0.311926606,0.32293578,0.333944954,
0.344954128,0.355963303,0.368807339,0.379816514,0.390825688,0.4,0.409174312,
0.418348624,0.427522936,0.436697248,0.44587156,0.455045872,0.466055046,
0.475229358,0.48440367,0.493577982,0.502752294,0.513761468,0.52293578,0.532110092,
0.539449541,0.546788991,0.55412844,0.56146789,0.568807339,0.577981651,0.585321101,
0.59266055,0.601834862,0.609174312,0.616513761,0.623853211,0.631192661,
0.63853211,0.64587156,0.653211009,0.660550459,0.667889908,0.675229358,0.682568807,
0.689908257,0.697247706,0.704587156,0.713761468,0.721100917,0.730275229,
0.743119266,0.75412844,0.76146789,0.770642202,0.777981651,0.785321101,0.79266055,
0.801834862,0.811009174,0.818348624,0.825688073,0.834862385,0.840366972,
0.84587156,0.853211009,0.858715596,0.864220183,0.869724771,0.875229358,
0.880733945,0.888073394,0.893577982,0.899082569,0.906422018,0.911926606,
0.917431193,0.924770642,0.930275229,0.937614679,0.943119266,0.948623853,
0.95412844,0.96146789,0.966972477,0.972477064,0.977981651,0.983486239,0.988990826,
0.994495413,1.),.UNSPECIFIED.);
#24379=B_SPLINE_CURVE_WITH_KNOTS('',3,(#205241,#205242,#205243,#205244,
#205245,#205246,#205247,#205248,#205249,#205250,#205251,#205252,#205253,
#205254,#205255,#205256,#205257,#205258,#205259,#205260,#205261,#205262,
#205263,#205264,#205265,#205266,#205267,#205268,#205269,#205270,#205271,
#205272,#205273,#205274,#205275,#205276,#205277,#205278,#205279,#205280,
#205281,#205282,#205283,#205284,#205285,#205286,#205287,#205288,#205289,
#205290,#205291,#205292,#205293,#205294,#205295,#205296,#205297,#205298,
#205299,#205300,#205301,#205302,#205303,#205304,#205305,#205306,#205307,
#205308,#205309,#205310,#205311,#205312,#205313,#205314,#205315,#205316,
#205317,#205318,#205319,#205320,#205321,#205322,#205323,#205324,#205325,
#205326,#205327,#205328,#205329,#205330,#205331,#205332,#205333,#205334,
#205335,#205336,#205337,#205338,#205339,#205340,#205341,#205342,#205343,
#205344,#205345,#205346,#205347,#205348,#205349,#205350,#205351,#205352,
#205353,#205354,#205355,#205356,#205357,#205358,#205359,#205360,#205361,
#205362,#205363,#205364,#205365,#205366,#205367,#205368,#205369,#205370,
#205371,#205372,#205373,#205374,#205375,#205376,#205377,#205378,#205379,
#205380,#205381,#205382,#205383,#205384,#205385,#205386,#205387,#205388,
#205389,#205390,#205391,#205392,#205393,#205394,#205395,#205396,#205397,
#205398,#205399,#205400,#205401,#205402,#205403,#205404,#205405,#205406,
#205407,#205408,#205409,#205410,#205411,#205412,#205413,#205414,#205415,
#205416,#205417,#205418,#205419,#205420,#205421,#205422,#205423,#205424,
#205425,#205426,#205427,#205428,#205429,#205430,#205431,#205432,#205433,
#205434,#205435,#205436,#205437,#205438,#205439,#205440,#205441,#205442,
#205443,#205444,#205445,#205446,#205447,#205448,#205449,#205450,#205451,
#205452,#205453,#205454,#205455,#205456,#205457,#205458,#205459,#205460,
#205461,#205462,#205463,#205464,#205465,#205466,#205467,#205468,#205469,
#205470,#205471,#205472,#205473,#205474,#205475,#205476,#205477,#205478,
#205479,#205480,#205481,#205482,#205483,#205484,#205485,#205486,#205487,
#205488,#205489,#205490,#205491,#205492,#205493,#205494,#205495,#205496,
#205497,#205498,#205499,#205500,#205501,#205502,#205503,#205504,#205505,
#205506,#205507,#205508,#205509,#205510,#205511,#205512,#205513,#205514,
#205515,#205516,#205517,#205518,#205519,#205520,#205521,#205522,#205523,
#205524,#205525,#205526,#205527,#205528,#205529,#205530,#205531,#205532,
#205533,#205534,#205535,#205536,#205537,#205538,#205539,#205540,#205541,
#205542,#205543,#205544,#205545,#205546,#205547,#205548,#205549,#205550,
#205551,#205552,#205553,#205554,#205555,#205556,#205557,#205558,#205559,
#205560,#205561,#205562,#205563,#205564,#205565),.UNSPECIFIED.,.F.,.F.,
(4,3,3,3,3,3,3,3,3,3,3,3,3,3,3,3,3,3,3,3,3,3,3,3,3,3,3,3,3,3,3,3,3,3,3,
3,3,3,3,3,3,3,3,3,3,3,3,3,3,3,3,3,3,3,3,3,3,3,3,3,3,3,3,3,3,3,3,3,3,3,3,
3,3,3,3,3,3,3,3,3,3,3,3,3,3,3,3,3,3,3,3,3,3,3,3,3,3,3,3,3,3,3,3,3,3,3,3,
3,4),(-1.,-0.994495413,-0.988990826,-0.983486239,-0.977981651,-0.970642202,
-0.965137615,-0.959633028,-0.95412844,-0.948623853,-0.943119266,-0.937614679,
-0.932110092,-0.926605505,-0.921100917,-0.91559633,-0.910091743,-0.904587156,
-0.899082569,-0.893577982,-0.888073394,-0.882568807,-0.87706422,-0.871559633,
-0.866055046,-0.860550459,-0.855045872,-0.849541284,-0.844036697,-0.83853211,
-0.833027523,-0.827522936,-0.822018349,-0.814678899,-0.809174312,-0.801834862,
-0.794495413,-0.787155963,-0.779816514,-0.772477064,-0.765137615,-0.757798165,
-0.750458716,-0.743119266,-0.735779817,-0.728440367,-0.721100917,-0.710091743,
-0.702752294,-0.695412844,-0.688073394,-0.678899083,-0.671559633,-0.664220183,
-0.656880734,-0.649541284,-0.642201835,-0.634862385,-0.627522936,-0.620183486,
-0.612844037,-0.605504587,-0.598165138,-0.590825688,-0.583486239,-0.576146789,
-0.568807339,-0.559633028,-0.552293578,-0.544954128,-0.537614679,-0.530275229,
-0.521100917,-0.511926606,-0.502752294,-0.493577982,-0.482568807,-0.473394495,
-0.464220183,-0.455045872,-0.44587156,-0.436697248,-0.427522936,-0.418348624,
-0.409174312,-0.4,-0.390825688,-0.379816514,-0.368807339,-0.357798165,-0.346788991,
-0.335779817,-0.324770642,-0.311926606,-0.300917431,-0.289908257,-0.278899083,
-0.267889908,-0.255045872,-0.244036697,-0.233027523,-0.222018349,-0.211009174,
-0.2,-0.188990826,-0.177981651,-0.166972477,-0.155963303,-0.143172102),
 .UNSPECIFIED.);
#24380=B_SPLINE_CURVE_WITH_KNOTS('',3,(#205566,#205567,#205568,#205569,
#205570,#205571,#205572,#205573,#205574,#205575,#205576,#205577,#205578,
#205579,#205580,#205581,#205582,#205583,#205584,#205585,#205586,#205587,
#205588,#205589,#205590,#205591,#205592,#205593,#205594,#205595,#205596,
#205597,#205598,#205599,#205600,#205601,#205602,#205603,#205604,#205605,
#205606,#205607,#205608,#205609,#205610,#205611,#205612,#205613,#205614,
#205615,#205616,#205617,#205618,#205619,#205620,#205621,#205622,#205623,
#205624,#205625,#205626,#205627,#205628,#205629,#205630,#205631,#205632,
#205633,#205634,#205635,#205636,#205637,#205638,#205639,#205640,#205641,
#205642,#205643,#205644,#205645,#205646,#205647,#205648,#205649,#205650,
#205651,#205652,#205653,#205654,#205655,#205656,#205657,#205658,#205659,
#205660,#205661,#205662,#205663,#205664,#205665,#205666,#205667,#205668,
#205669,#205670,#205671,#205672,#205673,#205674,#205675,#205676,#205677,
#205678,#205679,#205680,#205681,#205682,#205683,#205684,#205685,#205686,
#205687,#205688,#205689,#205690,#205691,#205692,#205693,#205694,#205695,
#205696,#205697,#205698,#205699,#205700,#205701,#205702,#205703,#205704,
#205705,#205706,#205707,#205708,#205709,#205710,#205711,#205712,#205713,
#205714,#205715,#205716,#205717,#205718,#205719,#205720,#205721,#205722,
#205723,#205724,#205725,#205726,#205727,#205728,#205729,#205730,#205731,
#205732,#205733,#205734,#205735,#205736,#205737,#205738,#205739,#205740,
#205741,#205742,#205743,#205744,#205745,#205746,#205747,#205748,#205749,
#205750,#205751,#205752,#205753,#205754,#205755,#205756,#205757,#205758,
#205759,#205760,#205761,#205762,#205763,#205764,#205765,#205766,#205767,
#205768,#205769,#205770,#205771,#205772,#205773,#205774,#205775,#205776,
#205777,#205778,#205779,#205780,#205781,#205782,#205783,#205784,#205785,
#205786,#205787,#205788,#205789,#205790,#205791,#205792,#205793,#205794,
#205795,#205796,#205797,#205798,#205799,#205800,#205801,#205802,#205803,
#205804,#205805,#205806,#205807,#205808,#205809,#205810,#205811,#205812,
#205813,#205814,#205815,#205816,#205817,#205818,#205819,#205820,#205821,
#205822,#205823,#205824,#205825,#205826,#205827,#205828,#205829,#205830,
#205831,#205832,#205833,#205834,#205835,#205836,#205837,#205838,#205839,
#205840,#205841,#205842,#205843,#205844,#205845,#205846,#205847,#205848,
#205849,#205850,#205851,#205852,#205853,#205854,#205855,#205856,#205857,
#205858,#205859,#205860,#205861,#205862,#205863,#205864,#205865,#205866),
 .UNSPECIFIED.,.F.,.F.,(4,3,3,3,3,3,3,3,3,3,3,3,3,3,3,3,3,3,3,3,3,3,3,3,
3,3,3,3,3,3,3,3,3,3,3,3,3,3,3,3,3,3,3,3,3,3,3,3,3,3,3,3,3,3,3,3,3,3,3,3,
3,3,3,3,3,3,3,3,3,3,3,3,3,3,3,3,3,3,3,3,3,3,3,3,3,3,3,3,3,3,3,3,3,3,3,3,
3,3,3,3,4),(0.143172102,0.15412844,0.165137615,0.176146789,0.187155963,
0.198165138,0.209174312,0.220183486,0.231192661,0.242201835,0.253211009,
0.266055046,0.27706422,0.288073394,0.299082569,0.310091743,0.321100917,
0.333944954,0.344954128,0.355963303,0.366972477,0.377981651,0.388990826,
0.398165138,0.409174312,0.420183486,0.433027523,0.442201835,0.451376147,
0.460550459,0.471559633,0.482568807,0.491743119,0.500917431,0.513761468,
0.524770642,0.533944954,0.541284404,0.548623853,0.557798165,0.565137615,
0.572477064,0.579816514,0.590825688,0.6,0.611009174,0.618348624,0.625688073,
0.633027523,0.640366972,0.649541284,0.656880734,0.664220183,0.671559633,
0.678899083,0.686238532,0.693577982,0.700917431,0.708256881,0.71559633,
0.72293578,0.732110092,0.739449541,0.748623853,0.757798165,0.765137615,
0.772477064,0.781651376,0.788990826,0.798165138,0.80733945,0.812844037,
0.822018349,0.829357798,0.836697248,0.844036697,0.849541284,0.855045872,
0.860550459,0.866055046,0.871559633,0.87706422,0.882568807,0.889908257,
0.895412844,0.904587156,0.910091743,0.91559633,0.921100917,0.926605505,
0.932110092,0.937614679,0.944954128,0.950458716,0.957798165,0.966972477,
0.972477064,0.977981651,0.983486239,0.99266055,1.),.UNSPECIFIED.);
#24381=B_SPLINE_CURVE_WITH_KNOTS('',3,(#206811,#206812,#206813,#206814,
#206815,#206816,#206817,#206818,#206819,#206820,#206821,#206822,#206823,
#206824,#206825,#206826,#206827,#206828,#206829,#206830,#206831,#206832,
#206833,#206834,#206835,#206836,#206837,#206838,#206839,#206840,#206841,
#206842,#206843,#206844,#206845,#206846,#206847,#206848,#206849,#206850,
#206851,#206852,#206853,#206854,#206855,#206856,#206857,#206858,#206859,
#206860,#206861,#206862,#206863,#206864,#206865,#206866,#206867,#206868,
#206869,#206870,#206871,#206872,#206873,#206874,#206875,#206876,#206877,
#206878,#206879,#206880,#206881,#206882,#206883,#206884,#206885,#206886,
#206887,#206888,#206889,#206890,#206891,#206892,#206893,#206894,#206895,
#206896,#206897,#206898,#206899,#206900,#206901,#206902,#206903,#206904,
#206905,#206906,#206907,#206908,#206909,#206910,#206911,#206912,#206913,
#206914,#206915,#206916,#206917,#206918,#206919,#206920,#206921,#206922,
#206923,#206924,#206925,#206926,#206927,#206928,#206929,#206930,#206931,
#206932,#206933,#206934,#206935,#206936,#206937,#206938,#206939,#206940,
#206941,#206942,#206943,#206944,#206945,#206946,#206947,#206948,#206949,
#206950,#206951,#206952,#206953,#206954,#206955,#206956,#206957,#206958,
#206959,#206960,#206961,#206962,#206963,#206964,#206965,#206966,#206967,
#206968,#206969,#206970,#206971,#206972,#206973,#206974,#206975,#206976,
#206977,#206978,#206979,#206980,#206981,#206982,#206983,#206984,#206985,
#206986,#206987,#206988,#206989,#206990,#206991,#206992,#206993,#206994,
#206995,#206996,#206997,#206998,#206999,#207000,#207001,#207002,#207003,
#207004,#207005,#207006,#207007,#207008,#207009,#207010,#207011,#207012,
#207013,#207014,#207015,#207016,#207017,#207018,#207019,#207020,#207021,
#207022,#207023,#207024,#207025,#207026,#207027,#207028,#207029,#207030,
#207031,#207032,#207033,#207034,#207035,#207036,#207037,#207038,#207039,
#207040,#207041,#207042,#207043,#207044,#207045,#207046,#207047,#207048,
#207049,#207050,#207051,#207052,#207053,#207054,#207055,#207056,#207057,
#207058,#207059,#207060,#207061,#207062,#207063,#207064,#207065,#207066,
#207067,#207068,#207069,#207070,#207071,#207072,#207073,#207074,#207075,
#207076,#207077,#207078,#207079,#207080,#207081,#207082,#207083,#207084,
#207085,#207086,#207087,#207088,#207089,#207090,#207091,#207092,#207093,
#207094,#207095,#207096,#207097,#207098,#207099,#207100,#207101,#207102,
#207103,#207104,#207105,#207106,#207107,#207108,#207109,#207110,#207111),
 .UNSPECIFIED.,.F.,.F.,(4,3,3,3,3,3,3,3,3,3,3,3,3,3,3,3,3,3,3,3,3,3,3,3,
3,3,3,3,3,3,3,3,3,3,3,3,3,3,3,3,3,3,3,3,3,3,3,3,3,3,3,3,3,3,3,3,3,3,3,3,
3,3,3,3,3,3,3,3,3,3,3,3,3,3,3,3,3,3,3,3,3,3,3,3,3,3,3,3,3,3,3,3,3,3,3,3,
3,3,3,3,4),(0.143172102,0.15412844,0.165137615,0.176146789,0.187155963,
0.198165138,0.211009174,0.222018349,0.233027523,0.244036697,0.255045872,
0.266055046,0.27706422,0.288073394,0.299082569,0.310091743,0.321100917,
0.332110092,0.344954128,0.355963303,0.366972477,0.377981651,0.388990826,
0.398165138,0.40733945,0.418348624,0.427522936,0.436697248,0.44587156,0.455045872,
0.464220183,0.475229358,0.48440367,0.495412844,0.504587156,0.51559633,0.524770642,
0.533944954,0.541284404,0.548623853,0.557798165,0.565137615,0.572477064,
0.579816514,0.587155963,0.594495413,0.601834862,0.609174312,0.616513761,
0.623853211,0.631192661,0.644036697,0.651376147,0.658715596,0.667889908,
0.675229358,0.682568807,0.689908257,0.700917431,0.710091743,0.717431193,
0.724770642,0.735779817,0.743119266,0.750458716,0.757798165,0.766972477,
0.774311927,0.781651376,0.788990826,0.796330275,0.803669725,0.811009174,
0.818348624,0.825688073,0.831192661,0.83853211,0.844036697,0.849541284,
0.858715596,0.864220183,0.871559633,0.87706422,0.88440367,0.889908257,0.895412844,
0.900917431,0.908256881,0.913761468,0.919266055,0.924770642,0.932110092,
0.939449541,0.948623853,0.95412844,0.959633028,0.966972477,0.972477064,
0.981651376,0.990825688,1.),.UNSPECIFIED.);
#24382=B_SPLINE_CURVE_WITH_KNOTS('',3,(#207112,#207113,#207114,#207115,
#207116,#207117,#207118,#207119,#207120,#207121,#207122,#207123,#207124,
#207125,#207126,#207127,#207128,#207129,#207130,#207131,#207132,#207133,
#207134,#207135,#207136,#207137,#207138,#207139,#207140,#207141,#207142,
#207143,#207144,#207145,#207146,#207147,#207148,#207149,#207150,#207151,
#207152,#207153,#207154,#207155,#207156,#207157,#207158,#207159,#207160,
#207161,#207162,#207163,#207164,#207165,#207166,#207167,#207168,#207169,
#207170,#207171,#207172,#207173,#207174,#207175,#207176,#207177,#207178,
#207179,#207180,#207181,#207182,#207183,#207184,#207185,#207186,#207187,
#207188,#207189,#207190,#207191,#207192,#207193,#207194,#207195,#207196,
#207197,#207198,#207199,#207200,#207201,#207202,#207203,#207204,#207205,
#207206,#207207,#207208,#207209,#207210,#207211,#207212,#207213,#207214,
#207215,#207216,#207217,#207218,#207219,#207220,#207221,#207222,#207223,
#207224,#207225,#207226,#207227,#207228,#207229,#207230,#207231,#207232,
#207233,#207234,#207235,#207236,#207237,#207238,#207239,#207240,#207241,
#207242,#207243,#207244,#207245,#207246,#207247,#207248,#207249,#207250,
#207251,#207252,#207253,#207254,#207255,#207256,#207257,#207258,#207259,
#207260,#207261,#207262,#207263,#207264,#207265,#207266,#207267,#207268,
#207269,#207270,#207271,#207272,#207273,#207274,#207275,#207276,#207277,
#207278,#207279,#207280,#207281,#207282,#207283,#207284,#207285,#207286,
#207287,#207288,#207289,#207290,#207291,#207292,#207293,#207294,#207295,
#207296,#207297,#207298,#207299,#207300,#207301,#207302,#207303,#207304,
#207305,#207306,#207307,#207308,#207309,#207310,#207311,#207312,#207313,
#207314,#207315,#207316,#207317,#207318,#207319,#207320,#207321,#207322,
#207323,#207324,#207325,#207326,#207327,#207328,#207329,#207330,#207331,
#207332,#207333,#207334,#207335,#207336,#207337,#207338,#207339,#207340,
#207341,#207342,#207343,#207344,#207345,#207346,#207347,#207348,#207349,
#207350,#207351,#207352,#207353,#207354,#207355,#207356,#207357,#207358,
#207359,#207360,#207361,#207362,#207363,#207364,#207365,#207366,#207367,
#207368,#207369,#207370,#207371,#207372,#207373,#207374,#207375,#207376,
#207377,#207378,#207379,#207380,#207381,#207382,#207383,#207384,#207385,
#207386,#207387,#207388,#207389,#207390,#207391,#207392,#207393,#207394,
#207395,#207396,#207397,#207398,#207399,#207400,#207401,#207402,#207403,
#207404,#207405,#207406,#207407,#207408,#207409,#207410,#207411,#207412,
#207413,#207414,#207415,#207416,#207417,#207418,#207419,#207420,#207421,
#207422,#207423,#207424,#207425,#207426,#207427,#207428,#207429,#207430),
 .UNSPECIFIED.,.F.,.F.,(4,3,3,3,3,3,3,3,3,3,3,3,3,3,3,3,3,3,3,3,3,3,3,3,
3,3,3,3,3,3,3,3,3,3,3,3,3,3,3,3,3,3,3,3,3,3,3,3,3,3,3,3,3,3,3,3,3,3,3,3,
3,3,3,3,3,3,3,3,3,3,3,3,3,3,3,3,3,3,3,3,3,3,3,3,3,3,3,3,3,3,3,3,3,3,3,3,
3,3,3,3,3,3,3,3,3,3,4),(0.143172102,0.15412844,0.165137615,0.176146789,
0.187155963,0.198165138,0.211009174,0.222018349,0.233027523,0.244036697,
0.255045872,0.266055046,0.27706422,0.288073394,0.299082569,0.310091743,
0.321100917,0.332110092,0.344954128,0.355963303,0.366972477,0.377981651,
0.388990826,0.398165138,0.40733945,0.418348624,0.427522936,0.436697248,
0.44587156,0.455045872,0.464220183,0.473394495,0.48440367,0.493577982,0.502752294,
0.511926606,0.521100917,0.530275229,0.537614679,0.544954128,0.552293578,
0.559633028,0.566972477,0.574311927,0.581651376,0.588990826,0.596330275,
0.603669725,0.611009174,0.618348624,0.625688073,0.633027523,0.640366972,
0.647706422,0.655045872,0.664220183,0.671559633,0.678899083,0.686238532,
0.693577982,0.700917431,0.710091743,0.717431193,0.724770642,0.733944954,
0.741284404,0.748623853,0.755963303,0.763302752,0.772477064,0.779816514,
0.787155963,0.794495413,0.803669725,0.811009174,0.816513761,0.822018349,
0.827522936,0.834862385,0.840366972,0.84587156,0.851376147,0.856880734,
0.862385321,0.867889908,0.873394495,0.878899083,0.88440367,0.889908257,
0.895412844,0.900917431,0.906422018,0.911926606,0.917431193,0.924770642,
0.930275229,0.937614679,0.943119266,0.948623853,0.95412844,0.959633028,
0.966972477,0.972477064,0.977981651,0.983486239,0.990825688,1.),
 .UNSPECIFIED.);
#24383=B_SPLINE_CURVE_WITH_KNOTS('',3,(#208390,#208391,#208392,#208393,
#208394,#208395,#208396,#208397,#208398,#208399,#208400,#208401,#208402,
#208403,#208404,#208405,#208406,#208407,#208408,#208409,#208410,#208411,
#208412,#208413,#208414,#208415,#208416,#208417,#208418,#208419,#208420,
#208421,#208422,#208423,#208424,#208425,#208426,#208427,#208428,#208429,
#208430,#208431,#208432,#208433,#208434,#208435,#208436,#208437,#208438,
#208439,#208440,#208441,#208442,#208443,#208444,#208445,#208446,#208447,
#208448,#208449,#208450,#208451,#208452,#208453,#208454,#208455,#208456,
#208457,#208458,#208459,#208460,#208461,#208462,#208463,#208464,#208465,
#208466,#208467,#208468,#208469,#208470,#208471,#208472,#208473,#208474,
#208475,#208476,#208477,#208478,#208479,#208480,#208481,#208482,#208483,
#208484,#208485,#208486,#208487,#208488,#208489,#208490,#208491,#208492,
#208493,#208494,#208495,#208496,#208497,#208498,#208499,#208500,#208501,
#208502,#208503,#208504,#208505,#208506,#208507,#208508,#208509,#208510,
#208511,#208512,#208513,#208514,#208515,#208516,#208517,#208518,#208519,
#208520,#208521,#208522,#208523,#208524,#208525,#208526,#208527,#208528,
#208529,#208530,#208531,#208532,#208533,#208534,#208535,#208536,#208537,
#208538,#208539,#208540,#208541,#208542,#208543,#208544,#208545,#208546,
#208547,#208548,#208549,#208550,#208551,#208552,#208553,#208554,#208555,
#208556,#208557,#208558,#208559,#208560,#208561,#208562,#208563,#208564,
#208565,#208566,#208567,#208568,#208569,#208570,#208571,#208572,#208573,
#208574,#208575,#208576,#208577,#208578,#208579,#208580,#208581,#208582,
#208583,#208584,#208585,#208586,#208587,#208588,#208589,#208590,#208591,
#208592,#208593,#208594,#208595,#208596,#208597,#208598,#208599,#208600,
#208601,#208602,#208603,#208604,#208605,#208606,#208607,#208608,#208609,
#208610,#208611,#208612,#208613,#208614,#208615,#208616,#208617,#208618,
#208619,#208620,#208621,#208622,#208623,#208624,#208625,#208626,#208627,
#208628,#208629,#208630,#208631,#208632,#208633,#208634,#208635,#208636,
#208637,#208638,#208639,#208640,#208641,#208642,#208643,#208644,#208645,
#208646,#208647,#208648,#208649,#208650,#208651,#208652,#208653,#208654,
#208655,#208656,#208657,#208658,#208659,#208660,#208661,#208662,#208663,
#208664,#208665,#208666,#208667,#208668,#208669,#208670,#208671,#208672,
#208673,#208674,#208675,#208676,#208677,#208678,#208679,#208680,#208681,
#208682,#208683,#208684,#208685,#208686,#208687,#208688,#208689,#208690,
#208691,#208692,#208693,#208694,#208695,#208696,#208697,#208698,#208699,
#208700,#208701,#208702),.UNSPECIFIED.,.F.,.F.,(4,3,3,3,3,3,3,3,3,3,3,3,
3,3,3,3,3,3,3,3,3,3,3,3,3,3,3,3,3,3,3,3,3,3,3,3,3,3,3,3,3,3,3,3,3,3,3,3,
3,3,3,3,3,3,3,3,3,3,3,3,3,3,3,3,3,3,3,3,3,3,3,3,3,3,3,3,3,3,3,3,3,3,3,3,
3,3,3,3,3,3,3,3,3,3,3,3,3,3,3,3,3,3,3,3,4),(0.143172102,0.15412844,0.165137615,
0.176146789,0.187155963,0.198165138,0.211009174,0.222018349,0.233027523,
0.244036697,0.255045872,0.266055046,0.27706422,0.288073394,0.299082569,
0.310091743,0.321100917,0.332110092,0.343119266,0.35412844,0.365137615,
0.376146789,0.387155963,0.396330275,0.405504587,0.414678899,0.425688073,
0.434862385,0.44587156,0.455045872,0.464220183,0.473394495,0.482568807,
0.491743119,0.500917431,0.511926606,0.521100917,0.530275229,0.537614679,
0.548623853,0.557798165,0.565137615,0.572477064,0.579816514,0.587155963,
0.596330275,0.603669725,0.611009174,0.620183486,0.627522936,0.634862385,
0.642201835,0.649541284,0.656880734,0.664220183,0.673394495,0.680733945,
0.688073394,0.697247706,0.704587156,0.713761468,0.721100917,0.728440367,
0.735779817,0.746788991,0.755963303,0.765137615,0.772477064,0.779816514,
0.790825688,0.798165138,0.805504587,0.811009174,0.818348624,0.823853211,
0.829357798,0.836697248,0.842201835,0.847706422,0.856880734,0.862385321,
0.867889908,0.873394495,0.878899083,0.88440367,0.889908257,0.895412844,
0.902752294,0.908256881,0.913761468,0.921100917,0.926605505,0.932110092,
0.937614679,0.943119266,0.948623853,0.95412844,0.959633028,0.965137615,
0.970642202,0.976146789,0.981651376,0.987155963,0.99266055,1.),
 .UNSPECIFIED.);
#24384=B_SPLINE_CURVE_WITH_KNOTS('',3,(#208703,#208704,#208705,#208706,
#208707,#208708,#208709,#208710,#208711,#208712,#208713,#208714,#208715,
#208716,#208717,#208718,#208719,#208720,#208721,#208722,#208723,#208724,
#208725,#208726,#208727,#208728,#208729,#208730,#208731,#208732,#208733,
#208734,#208735,#208736,#208737,#208738,#208739,#208740,#208741,#208742,
#208743,#208744,#208745,#208746,#208747,#208748,#208749,#208750,#208751,
#208752,#208753,#208754,#208755,#208756,#208757,#208758,#208759,#208760,
#208761,#208762,#208763,#208764,#208765,#208766,#208767,#208768,#208769,
#208770,#208771,#208772,#208773,#208774,#208775,#208776,#208777,#208778,
#208779,#208780,#208781,#208782,#208783,#208784,#208785,#208786,#208787,
#208788,#208789,#208790,#208791,#208792,#208793,#208794,#208795,#208796,
#208797,#208798,#208799,#208800,#208801,#208802,#208803,#208804,#208805,
#208806,#208807,#208808,#208809,#208810,#208811,#208812,#208813,#208814,
#208815,#208816,#208817,#208818,#208819,#208820,#208821,#208822,#208823,
#208824,#208825,#208826,#208827,#208828,#208829,#208830,#208831,#208832,
#208833,#208834,#208835,#208836,#208837,#208838,#208839,#208840,#208841,
#208842,#208843,#208844,#208845,#208846,#208847,#208848,#208849,#208850,
#208851,#208852,#208853,#208854,#208855,#208856,#208857,#208858,#208859,
#208860,#208861,#208862,#208863,#208864,#208865,#208866,#208867,#208868,
#208869,#208870,#208871,#208872,#208873,#208874,#208875,#208876,#208877,
#208878,#208879,#208880,#208881,#208882,#208883,#208884,#208885,#208886,
#208887,#208888,#208889,#208890,#208891,#208892,#208893,#208894,#208895,
#208896,#208897,#208898,#208899,#208900,#208901,#208902,#208903,#208904,
#208905,#208906,#208907,#208908,#208909,#208910,#208911,#208912,#208913,
#208914,#208915,#208916,#208917,#208918,#208919,#208920,#208921,#208922,
#208923,#208924,#208925,#208926,#208927,#208928,#208929,#208930,#208931,
#208932,#208933,#208934,#208935,#208936,#208937,#208938,#208939,#208940,
#208941,#208942,#208943,#208944,#208945,#208946,#208947,#208948,#208949,
#208950,#208951,#208952,#208953,#208954,#208955,#208956,#208957,#208958,
#208959,#208960,#208961,#208962,#208963,#208964,#208965,#208966,#208967,
#208968,#208969,#208970,#208971,#208972,#208973,#208974,#208975,#208976,
#208977,#208978,#208979,#208980,#208981,#208982,#208983,#208984,#208985,
#208986,#208987,#208988,#208989,#208990,#208991,#208992,#208993,#208994,
#208995,#208996,#208997,#208998,#208999,#209000,#209001,#209002,#209003,
#209004,#209005,#209006,#209007,#209008,#209009,#209010,#209011,#209012,
#209013,#209014,#209015,#209016,#209017,#209018,#209019,#209020,#209021,
#209022,#209023,#209024,#209025,#209026,#209027),.UNSPECIFIED.,.F.,.F.,
(4,3,3,3,3,3,3,3,3,3,3,3,3,3,3,3,3,3,3,3,3,3,3,3,3,3,3,3,3,3,3,3,3,3,3,
3,3,3,3,3,3,3,3,3,3,3,3,3,3,3,3,3,3,3,3,3,3,3,3,3,3,3,3,3,3,3,3,3,3,3,3,
3,3,3,3,3,3,3,3,3,3,3,3,3,3,3,3,3,3,3,3,3,3,3,3,3,3,3,3,3,3,3,3,3,3,3,3,
3,4),(0.143172102,0.15412844,0.165137615,0.176146789,0.187155963,0.198165138,
0.211009174,0.222018349,0.233027523,0.244036697,0.255045872,0.266055046,
0.27706422,0.288073394,0.299082569,0.310091743,0.321100917,0.332110092,
0.343119266,0.35412844,0.365137615,0.376146789,0.387155963,0.396330275,
0.405504587,0.414678899,0.423853211,0.433027523,0.442201835,0.451376147,
0.460550459,0.469724771,0.478899083,0.488073394,0.497247706,0.506422018,
0.51559633,0.524770642,0.533944954,0.541284404,0.548623853,0.557798165,
0.565137615,0.572477064,0.579816514,0.587155963,0.596330275,0.603669725,
0.611009174,0.618348624,0.625688073,0.633027523,0.640366972,0.647706422,
0.655045872,0.664220183,0.671559633,0.678899083,0.686238532,0.693577982,
0.700917431,0.708256881,0.71559633,0.72293578,0.730275229,0.737614679,0.744954128,
0.752293578,0.759633028,0.766972477,0.774311927,0.781651376,0.788990826,
0.796330275,0.805504587,0.811009174,0.816513761,0.822018349,0.827522936,
0.833027523,0.83853211,0.844036697,0.849541284,0.855045872,0.860550459,
0.866055046,0.871559633,0.87706422,0.882568807,0.888073394,0.893577982,
0.899082569,0.904587156,0.910091743,0.91559633,0.921100917,0.926605505,
0.933944954,0.939449541,0.944954128,0.950458716,0.955963303,0.96146789,
0.968807339,0.974311927,0.979816514,0.985321101,0.99266055,1.),
 .UNSPECIFIED.);
#24385=B_SPLINE_CURVE_WITH_KNOTS('',3,(#209975,#209976,#209977,#209978,
#209979,#209980,#209981,#209982,#209983,#209984,#209985,#209986,#209987,
#209988,#209989,#209990,#209991,#209992,#209993,#209994,#209995,#209996,
#209997,#209998,#209999,#210000,#210001,#210002,#210003,#210004,#210005,
#210006,#210007,#210008,#210009,#210010,#210011,#210012,#210013,#210014,
#210015,#210016,#210017,#210018,#210019,#210020,#210021,#210022,#210023,
#210024,#210025,#210026,#210027,#210028,#210029,#210030,#210031,#210032,
#210033,#210034,#210035,#210036,#210037,#210038,#210039,#210040,#210041,
#210042,#210043,#210044,#210045,#210046,#210047,#210048,#210049,#210050,
#210051,#210052,#210053,#210054,#210055,#210056,#210057,#210058,#210059,
#210060,#210061,#210062,#210063,#210064,#210065,#210066,#210067,#210068,
#210069,#210070,#210071,#210072,#210073,#210074,#210075,#210076,#210077,
#210078,#210079,#210080,#210081,#210082,#210083,#210084,#210085,#210086,
#210087,#210088,#210089,#210090,#210091,#210092,#210093,#210094,#210095,
#210096,#210097,#210098,#210099,#210100,#210101,#210102,#210103,#210104,
#210105,#210106,#210107,#210108,#210109,#210110,#210111,#210112,#210113,
#210114,#210115,#210116,#210117,#210118,#210119,#210120,#210121,#210122,
#210123,#210124,#210125,#210126,#210127,#210128,#210129,#210130,#210131,
#210132,#210133,#210134,#210135,#210136,#210137,#210138,#210139,#210140,
#210141,#210142,#210143,#210144,#210145,#210146,#210147,#210148,#210149,
#210150,#210151,#210152,#210153,#210154,#210155,#210156,#210157,#210158,
#210159,#210160,#210161,#210162,#210163,#210164,#210165,#210166,#210167,
#210168,#210169,#210170,#210171,#210172,#210173,#210174,#210175,#210176,
#210177,#210178,#210179,#210180,#210181,#210182,#210183,#210184,#210185,
#210186,#210187,#210188,#210189,#210190,#210191,#210192,#210193,#210194,
#210195,#210196,#210197,#210198,#210199,#210200,#210201,#210202,#210203,
#210204,#210205,#210206,#210207,#210208,#210209,#210210,#210211,#210212,
#210213,#210214,#210215,#210216,#210217,#210218,#210219,#210220,#210221,
#210222,#210223,#210224,#210225,#210226,#210227,#210228,#210229,#210230,
#210231,#210232,#210233,#210234,#210235,#210236,#210237,#210238,#210239,
#210240,#210241,#210242,#210243,#210244,#210245,#210246,#210247,#210248,
#210249,#210250,#210251,#210252,#210253,#210254,#210255,#210256,#210257,
#210258,#210259,#210260,#210261,#210262,#210263,#210264,#210265,#210266,
#210267,#210268,#210269,#210270,#210271,#210272,#210273,#210274,#210275,
#210276,#210277,#210278,#210279,#210280,#210281,#210282,#210283,#210284,
#210285,#210286,#210287,#210288,#210289,#210290,#210291,#210292,#210293,
#210294,#210295,#210296,#210297,#210298,#210299),.UNSPECIFIED.,.F.,.F.,
(4,3,3,3,3,3,3,3,3,3,3,3,3,3,3,3,3,3,3,3,3,3,3,3,3,3,3,3,3,3,3,3,3,3,3,
3,3,3,3,3,3,3,3,3,3,3,3,3,3,3,3,3,3,3,3,3,3,3,3,3,3,3,3,3,3,3,3,3,3,3,3,
3,3,3,3,3,3,3,3,3,3,3,3,3,3,3,3,3,3,3,3,3,3,3,3,3,3,3,3,3,3,3,3,3,3,3,3,
3,4),(-1.,-0.994495413,-0.988990826,-0.983486239,-0.977981651,-0.972477064,
-0.966972477,-0.96146789,-0.955963303,-0.950458716,-0.944954128,-0.937614679,
-0.932110092,-0.926605505,-0.919266055,-0.913761468,-0.908256881,-0.902752294,
-0.897247706,-0.889908257,-0.88440367,-0.878899083,-0.873394495,-0.867889908,
-0.862385321,-0.856880734,-0.851376147,-0.84587156,-0.840366972,-0.834862385,
-0.829357798,-0.823853211,-0.818348624,-0.812844037,-0.80733945,-0.8,-0.79266055,
-0.785321101,-0.776146789,-0.768807339,-0.76146789,-0.75412844,-0.746788991,
-0.739449541,-0.732110092,-0.724770642,-0.717431193,-0.708256881,-0.699082569,
-0.691743119,-0.68440367,-0.67706422,-0.669724771,-0.662385321,-0.655045872,
-0.647706422,-0.640366972,-0.633027523,-0.625688073,-0.618348624,-0.611009174,
-0.603669725,-0.594495413,-0.587155963,-0.579816514,-0.572477064,-0.565137615,
-0.557798165,-0.550458716,-0.543119266,-0.535779817,-0.528440367,-0.519266055,
-0.510091743,-0.500917431,-0.491743119,-0.482568807,-0.473394495,-0.464220183,
-0.455045872,-0.44587156,-0.436697248,-0.427522936,-0.418348624,-0.409174312,
-0.398165138,-0.388990826,-0.377981651,-0.366972477,-0.355963303,-0.344954128,
-0.333944954,-0.32293578,-0.311926606,-0.300917431,-0.289908257,-0.278899083,
-0.267889908,-0.256880734,-0.24587156,-0.234862385,-0.223853211,-0.212844037,
-0.201834862,-0.190825688,-0.179816514,-0.168807339,-0.157798165,-0.143172102),
 .UNSPECIFIED.);
#24386=B_SPLINE_CURVE_WITH_KNOTS('',3,(#210300,#210301,#210302,#210303,
#210304,#210305,#210306,#210307,#210308,#210309,#210310,#210311,#210312,
#210313,#210314,#210315,#210316,#210317,#210318,#210319,#210320,#210321,
#210322,#210323,#210324,#210325,#210326,#210327,#210328,#210329,#210330,
#210331,#210332,#210333,#210334,#210335,#210336,#210337,#210338,#210339,
#210340,#210341,#210342,#210343,#210344,#210345,#210346,#210347,#210348,
#210349,#210350,#210351,#210352,#210353,#210354,#210355,#210356,#210357,
#210358,#210359,#210360,#210361,#210362,#210363,#210364,#210365,#210366,
#210367,#210368,#210369,#210370,#210371,#210372,#210373,#210374,#210375,
#210376,#210377,#210378,#210379,#210380,#210381,#210382,#210383,#210384,
#210385,#210386,#210387,#210388,#210389,#210390,#210391,#210392,#210393,
#210394,#210395,#210396,#210397,#210398,#210399,#210400,#210401,#210402,
#210403,#210404,#210405,#210406,#210407,#210408,#210409,#210410,#210411,
#210412,#210413,#210414,#210415,#210416,#210417,#210418,#210419,#210420,
#210421,#210422,#210423,#210424,#210425,#210426,#210427,#210428,#210429,
#210430,#210431,#210432,#210433,#210434,#210435,#210436,#210437,#210438,
#210439,#210440,#210441,#210442,#210443,#210444,#210445,#210446,#210447,
#210448,#210449,#210450,#210451,#210452,#210453,#210454,#210455,#210456,
#210457,#210458,#210459,#210460,#210461,#210462,#210463,#210464,#210465,
#210466,#210467,#210468,#210469,#210470,#210471,#210472,#210473,#210474,
#210475,#210476,#210477,#210478,#210479,#210480,#210481,#210482,#210483,
#210484,#210485,#210486,#210487,#210488,#210489,#210490,#210491,#210492,
#210493,#210494,#210495,#210496,#210497,#210498,#210499,#210500,#210501,
#210502,#210503,#210504,#210505,#210506,#210507,#210508,#210509,#210510,
#210511,#210512,#210513,#210514,#210515,#210516,#210517,#210518,#210519,
#210520,#210521,#210522,#210523,#210524,#210525,#210526,#210527,#210528,
#210529,#210530,#210531,#210532,#210533,#210534,#210535,#210536,#210537,
#210538,#210539,#210540,#210541,#210542,#210543,#210544,#210545,#210546,
#210547,#210548,#210549,#210550,#210551,#210552,#210553,#210554,#210555,
#210556,#210557,#210558,#210559,#210560,#210561,#210562,#210563,#210564,
#210565,#210566,#210567,#210568,#210569,#210570,#210571,#210572,#210573,
#210574,#210575,#210576,#210577,#210578,#210579,#210580,#210581,#210582,
#210583,#210584,#210585,#210586,#210587,#210588,#210589,#210590,#210591,
#210592,#210593,#210594,#210595,#210596,#210597,#210598,#210599,#210600,
#210601,#210602,#210603,#210604,#210605,#210606,#210607,#210608,#210609),
 .UNSPECIFIED.,.F.,.F.,(4,3,3,3,3,3,3,3,3,3,3,3,3,3,3,3,3,3,3,3,3,3,3,3,
3,3,3,3,3,3,3,3,3,3,3,3,3,3,3,3,3,3,3,3,3,3,3,3,3,3,3,3,3,3,3,3,3,3,3,3,
3,3,3,3,3,3,3,3,3,3,3,3,3,3,3,3,3,3,3,3,3,3,3,3,3,3,3,3,3,3,3,3,3,3,3,3,
3,3,3,3,3,3,3,4),(0.143172102,0.15412844,0.165137615,0.176146789,0.187155963,
0.198165138,0.209174312,0.220183486,0.231192661,0.242201835,0.253211009,
0.264220183,0.275229358,0.288073394,0.299082569,0.311926606,0.32293578,
0.333944954,0.344954128,0.355963303,0.366972477,0.377981651,0.388990826,
0.398165138,0.40733945,0.416513761,0.425688073,0.434862385,0.444036697,
0.455045872,0.464220183,0.473394495,0.482568807,0.491743119,0.500917431,
0.510091743,0.519266055,0.528440367,0.535779817,0.543119266,0.550458716,
0.557798165,0.565137615,0.574311927,0.581651376,0.588990826,0.598165138,
0.605504587,0.612844037,0.620183486,0.627522936,0.63853211,0.64587156,0.655045872,
0.662385321,0.671559633,0.678899083,0.686238532,0.693577982,0.706422018,
0.713761468,0.721100917,0.728440367,0.735779817,0.743119266,0.750458716,
0.757798165,0.765137615,0.772477064,0.781651376,0.79266055,0.801834862,
0.809174312,0.814678899,0.820183486,0.825688073,0.831192661,0.840366972,
0.847706422,0.853211009,0.860550459,0.867889908,0.873394495,0.878899083,
0.88440367,0.893577982,0.899082569,0.904587156,0.910091743,0.91559633,0.921100917,
0.930275229,0.935779817,0.943119266,0.948623853,0.955963303,0.96146789,
0.966972477,0.972477064,0.977981651,0.983486239,0.988990826,0.994495413,
1.),.UNSPECIFIED.);
#24387=B_SPLINE_CURVE_WITH_KNOTS('',3,(#211572,#211573,#211574,#211575,
#211576,#211577,#211578,#211579,#211580,#211581,#211582,#211583,#211584,
#211585,#211586,#211587,#211588,#211589,#211590,#211591,#211592,#211593,
#211594,#211595,#211596,#211597,#211598,#211599,#211600,#211601,#211602,
#211603,#211604,#211605,#211606,#211607,#211608,#211609,#211610,#211611,
#211612,#211613,#211614,#211615,#211616,#211617,#211618,#211619,#211620,
#211621,#211622,#211623,#211624,#211625,#211626,#211627,#211628,#211629,
#211630,#211631,#211632,#211633,#211634,#211635,#211636,#211637,#211638,
#211639,#211640,#211641,#211642,#211643,#211644,#211645,#211646,#211647,
#211648,#211649,#211650,#211651,#211652,#211653,#211654,#211655,#211656,
#211657,#211658,#211659,#211660,#211661,#211662,#211663,#211664,#211665,
#211666,#211667,#211668,#211669,#211670,#211671,#211672,#211673,#211674,
#211675,#211676,#211677,#211678,#211679,#211680,#211681,#211682,#211683,
#211684,#211685,#211686,#211687,#211688,#211689,#211690,#211691,#211692,
#211693,#211694,#211695,#211696,#211697,#211698,#211699,#211700,#211701,
#211702,#211703,#211704,#211705,#211706,#211707,#211708,#211709,#211710,
#211711,#211712,#211713,#211714,#211715,#211716,#211717,#211718,#211719,
#211720,#211721,#211722,#211723,#211724,#211725,#211726,#211727,#211728,
#211729,#211730,#211731,#211732,#211733,#211734,#211735,#211736,#211737,
#211738,#211739,#211740,#211741,#211742,#211743,#211744,#211745,#211746,
#211747,#211748,#211749,#211750,#211751,#211752,#211753,#211754,#211755,
#211756,#211757,#211758,#211759,#211760,#211761,#211762,#211763,#211764,
#211765,#211766,#211767,#211768,#211769,#211770,#211771,#211772,#211773,
#211774,#211775,#211776,#211777,#211778,#211779,#211780,#211781,#211782,
#211783,#211784,#211785,#211786,#211787,#211788,#211789,#211790,#211791,
#211792,#211793,#211794,#211795,#211796,#211797,#211798,#211799,#211800,
#211801,#211802,#211803,#211804,#211805,#211806,#211807,#211808,#211809,
#211810,#211811,#211812,#211813,#211814,#211815,#211816,#211817,#211818,
#211819,#211820,#211821,#211822,#211823,#211824,#211825,#211826,#211827,
#211828,#211829,#211830,#211831,#211832,#211833,#211834,#211835,#211836,
#211837,#211838,#211839,#211840,#211841,#211842,#211843,#211844,#211845,
#211846,#211847,#211848,#211849,#211850,#211851,#211852,#211853,#211854,
#211855,#211856,#211857,#211858,#211859,#211860,#211861,#211862,#211863,
#211864,#211865,#211866,#211867,#211868,#211869,#211870,#211871,#211872,
#211873,#211874,#211875,#211876,#211877,#211878,#211879,#211880,#211881,
#211882,#211883,#211884,#211885,#211886,#211887,#211888,#211889,#211890,
#211891,#211892,#211893),.UNSPECIFIED.,.F.,.F.,(4,3,3,3,3,3,3,3,3,3,3,3,
3,3,3,3,3,3,3,3,3,3,3,3,3,3,3,3,3,3,3,3,3,3,3,3,3,3,3,3,3,3,3,3,3,3,3,3,
3,3,3,3,3,3,3,3,3,3,3,3,3,3,3,3,3,3,3,3,3,3,3,3,3,3,3,3,3,3,3,3,3,3,3,3,
3,3,3,3,3,3,3,3,3,3,3,3,3,3,3,3,3,3,3,3,3,3,3,4),(-1.,-0.994495413,-0.988990826,
-0.981651376,-0.976146789,-0.970642202,-0.965137615,-0.959633028,-0.95412844,
-0.948623853,-0.941284404,-0.932110092,-0.926605505,-0.921100917,-0.91559633,
-0.910091743,-0.904587156,-0.899082569,-0.893577982,-0.888073394,-0.882568807,
-0.87706422,-0.871559633,-0.866055046,-0.860550459,-0.855045872,-0.849541284,
-0.842201835,-0.836697248,-0.831192661,-0.825688073,-0.820183486,-0.814678899,
-0.809174312,-0.801834862,-0.794495413,-0.787155963,-0.777981651,-0.770642202,
-0.763302752,-0.755963303,-0.748623853,-0.741284404,-0.732110092,-0.724770642,
-0.717431193,-0.710091743,-0.702752294,-0.695412844,-0.688073394,-0.680733945,
-0.671559633,-0.664220183,-0.656880734,-0.649541284,-0.642201835,-0.634862385,
-0.627522936,-0.620183486,-0.612844037,-0.605504587,-0.598165138,-0.590825688,
-0.583486239,-0.576146789,-0.568807339,-0.56146789,-0.55412844,-0.546788991,
-0.539449541,-0.532110092,-0.52293578,-0.513761468,-0.504587156,-0.495412844,
-0.486238532,-0.47706422,-0.467889908,-0.458715596,-0.449541284,-0.440366972,
-0.431192661,-0.422018349,-0.412844037,-0.403669725,-0.394495413,-0.383486239,
-0.372477064,-0.359633028,-0.348623853,-0.337614679,-0.326605505,-0.31559633,
-0.304587156,-0.293577982,-0.282568807,-0.271559633,-0.260550459,-0.249541284,
-0.23853211,-0.227522936,-0.216513761,-0.205504587,-0.194495413,-0.183486239,
-0.172477064,-0.16146789,-0.143172102),.UNSPECIFIED.);
#24388=B_SPLINE_CURVE_WITH_KNOTS('',3,(#211894,#211895,#211896,#211897,
#211898,#211899,#211900,#211901,#211902,#211903,#211904,#211905,#211906,
#211907,#211908,#211909,#211910,#211911,#211912,#211913,#211914,#211915,
#211916,#211917,#211918,#211919,#211920,#211921,#211922,#211923,#211924,
#211925,#211926,#211927,#211928,#211929,#211930,#211931,#211932,#211933,
#211934,#211935,#211936,#211937,#211938,#211939,#211940,#211941,#211942,
#211943,#211944,#211945,#211946,#211947,#211948,#211949,#211950,#211951,
#211952,#211953,#211954,#211955,#211956,#211957,#211958,#211959,#211960,
#211961,#211962,#211963,#211964,#211965,#211966,#211967,#211968,#211969,
#211970,#211971,#211972,#211973,#211974,#211975,#211976,#211977,#211978,
#211979,#211980,#211981,#211982,#211983,#211984,#211985,#211986,#211987,
#211988,#211989,#211990,#211991,#211992,#211993,#211994,#211995,#211996,
#211997,#211998,#211999,#212000,#212001,#212002,#212003,#212004,#212005,
#212006,#212007,#212008,#212009,#212010,#212011,#212012,#212013,#212014,
#212015,#212016,#212017,#212018,#212019,#212020,#212021,#212022,#212023,
#212024,#212025,#212026,#212027,#212028,#212029,#212030,#212031,#212032,
#212033,#212034,#212035,#212036,#212037,#212038,#212039,#212040,#212041,
#212042,#212043,#212044,#212045,#212046,#212047,#212048,#212049,#212050,
#212051,#212052,#212053,#212054,#212055,#212056,#212057,#212058,#212059,
#212060,#212061,#212062,#212063,#212064,#212065,#212066,#212067,#212068,
#212069,#212070,#212071,#212072,#212073,#212074,#212075,#212076,#212077,
#212078,#212079,#212080,#212081,#212082,#212083,#212084,#212085,#212086,
#212087,#212088,#212089,#212090,#212091,#212092,#212093,#212094,#212095,
#212096,#212097,#212098,#212099,#212100,#212101,#212102,#212103,#212104,
#212105,#212106,#212107,#212108,#212109,#212110,#212111,#212112,#212113,
#212114,#212115,#212116,#212117,#212118,#212119,#212120,#212121,#212122,
#212123,#212124,#212125,#212126,#212127,#212128,#212129,#212130,#212131,
#212132,#212133,#212134,#212135,#212136,#212137,#212138,#212139,#212140,
#212141,#212142,#212143,#212144,#212145,#212146,#212147,#212148,#212149,
#212150,#212151,#212152,#212153,#212154,#212155,#212156,#212157,#212158,
#212159,#212160,#212161,#212162,#212163,#212164,#212165,#212166,#212167,
#212168,#212169,#212170,#212171,#212172,#212173,#212174,#212175,#212176,
#212177,#212178,#212179,#212180,#212181,#212182,#212183,#212184,#212185,
#212186,#212187,#212188,#212189,#212190,#212191,#212192,#212193,#212194),
 .UNSPECIFIED.,.F.,.F.,(4,3,3,3,3,3,3,3,3,3,3,3,3,3,3,3,3,3,3,3,3,3,3,3,
3,3,3,3,3,3,3,3,3,3,3,3,3,3,3,3,3,3,3,3,3,3,3,3,3,3,3,3,3,3,3,3,3,3,3,3,
3,3,3,3,3,3,3,3,3,3,3,3,3,3,3,3,3,3,3,3,3,3,3,3,3,3,3,3,3,3,3,3,3,3,3,3,
3,3,3,3,4),(0.143172102,0.15412844,0.165137615,0.176146789,0.187155963,
0.198165138,0.209174312,0.220183486,0.231192661,0.242201835,0.253211009,
0.264220183,0.275229358,0.288073394,0.299082569,0.310091743,0.326605505,
0.337614679,0.348623853,0.359633028,0.370642202,0.381651376,0.39266055,
0.401834862,0.411009174,0.420183486,0.429357798,0.43853211,0.449541284,
0.458715596,0.467889908,0.47706422,0.488073394,0.499082569,0.508256881,
0.517431193,0.526605505,0.533944954,0.541284404,0.548623853,0.555963303,
0.563302752,0.572477064,0.579816514,0.590825688,0.598165138,0.60733945,
0.614678899,0.622018349,0.631192661,0.640366972,0.647706422,0.656880734,
0.669724771,0.67706422,0.686238532,0.693577982,0.704587156,0.713761468,
0.721100917,0.728440367,0.737614679,0.744954128,0.752293578,0.76146789,
0.768807339,0.776146789,0.785321101,0.79266055,0.8,0.80733945,0.814678899,
0.820183486,0.825688073,0.833027523,0.83853211,0.844036697,0.853211009,
0.858715596,0.864220183,0.873394495,0.878899083,0.886238532,0.891743119,
0.897247706,0.902752294,0.908256881,0.917431193,0.92293578,0.930275229,
0.937614679,0.944954128,0.952293578,0.957798165,0.963302752,0.968807339,
0.974311927,0.979816514,0.988990826,0.994495413,1.),.UNSPECIFIED.);
#24389=B_SPLINE_CURVE_WITH_KNOTS('',3,(#213139,#213140,#213141,#213142,
#213143,#213144,#213145,#213146,#213147,#213148,#213149,#213150,#213151,
#213152,#213153,#213154,#213155,#213156,#213157,#213158,#213159,#213160,
#213161,#213162,#213163,#213164,#213165,#213166,#213167,#213168,#213169,
#213170,#213171,#213172,#213173,#213174,#213175,#213176,#213177,#213178,
#213179,#213180,#213181,#213182,#213183,#213184,#213185,#213186,#213187,
#213188,#213189,#213190,#213191,#213192,#213193,#213194,#213195,#213196,
#213197,#213198,#213199,#213200,#213201,#213202,#213203,#213204,#213205,
#213206,#213207,#213208,#213209,#213210,#213211,#213212,#213213,#213214,
#213215,#213216,#213217,#213218,#213219,#213220,#213221,#213222,#213223,
#213224,#213225,#213226,#213227,#213228,#213229,#213230,#213231,#213232,
#213233,#213234,#213235,#213236,#213237,#213238,#213239,#213240,#213241,
#213242,#213243,#213244,#213245,#213246,#213247,#213248,#213249,#213250,
#213251,#213252,#213253,#213254,#213255,#213256,#213257,#213258,#213259,
#213260,#213261,#213262,#213263,#213264,#213265,#213266,#213267,#213268,
#213269,#213270,#213271,#213272,#213273,#213274,#213275,#213276,#213277,
#213278,#213279,#213280,#213281,#213282,#213283,#213284,#213285,#213286,
#213287,#213288,#213289,#213290,#213291,#213292,#213293,#213294,#213295,
#213296,#213297,#213298,#213299,#213300,#213301,#213302,#213303,#213304,
#213305,#213306,#213307,#213308,#213309,#213310,#213311,#213312,#213313,
#213314,#213315,#213316,#213317,#213318,#213319,#213320,#213321,#213322,
#213323,#213324,#213325,#213326,#213327,#213328,#213329,#213330,#213331,
#213332,#213333,#213334,#213335,#213336,#213337,#213338,#213339,#213340,
#213341,#213342,#213343,#213344,#213345,#213346,#213347,#213348,#213349,
#213350,#213351,#213352,#213353,#213354,#213355,#213356,#213357,#213358,
#213359,#213360,#213361,#213362,#213363,#213364,#213365,#213366,#213367,
#213368,#213369,#213370,#213371,#213372,#213373,#213374,#213375,#213376,
#213377,#213378,#213379,#213380,#213381,#213382,#213383,#213384,#213385,
#213386,#213387,#213388,#213389,#213390,#213391,#213392,#213393,#213394,
#213395,#213396,#213397,#213398,#213399,#213400,#213401,#213402,#213403,
#213404,#213405,#213406,#213407,#213408,#213409,#213410,#213411,#213412,
#213413,#213414,#213415,#213416,#213417,#213418,#213419,#213420,#213421,
#213422,#213423,#213424,#213425,#213426,#213427,#213428,#213429,#213430,
#213431,#213432,#213433,#213434,#213435,#213436,#213437,#213438,#213439,
#213440,#213441,#213442,#213443,#213444,#213445,#213446,#213447,#213448),
 .UNSPECIFIED.,.F.,.F.,(4,3,3,3,3,3,3,3,3,3,3,3,3,3,3,3,3,3,3,3,3,3,3,3,
3,3,3,3,3,3,3,3,3,3,3,3,3,3,3,3,3,3,3,3,3,3,3,3,3,3,3,3,3,3,3,3,3,3,3,3,
3,3,3,3,3,3,3,3,3,3,3,3,3,3,3,3,3,3,3,3,3,3,3,3,3,3,3,3,3,3,3,3,3,3,3,3,
3,3,3,3,3,3,3,4),(0.143172102,0.15412844,0.165137615,0.177981651,0.188990826,
0.2,0.211009174,0.222018349,0.233027523,0.244036697,0.255045872,0.266055046,
0.27706422,0.288073394,0.302752294,0.313761468,0.324770642,0.335779817,
0.346788991,0.357798165,0.368807339,0.379816514,0.390825688,0.4,0.409174312,
0.418348624,0.429357798,0.43853211,0.447706422,0.456880734,0.467889908,
0.47706422,0.486238532,0.495412844,0.504587156,0.513761468,0.52293578,0.532110092,
0.539449541,0.546788991,0.55412844,0.56146789,0.568807339,0.576146789,0.583486239,
0.590825688,0.601834862,0.611009174,0.618348624,0.625688073,0.634862385,
0.644036697,0.653211009,0.660550459,0.667889908,0.675229358,0.68440367,
0.691743119,0.699082569,0.706422018,0.713761468,0.721100917,0.730275229,
0.739449541,0.746788991,0.755963303,0.763302752,0.772477064,0.779816514,
0.787155963,0.794495413,0.801834862,0.809174312,0.814678899,0.823853211,
0.829357798,0.834862385,0.840366972,0.84587156,0.851376147,0.856880734,
0.864220183,0.869724771,0.875229358,0.88440367,0.889908257,0.895412844,
0.900917431,0.906422018,0.911926606,0.917431193,0.92293578,0.928440367,
0.933944954,0.941284404,0.946788991,0.955963303,0.96146789,0.966972477,
0.974311927,0.981651376,0.987155963,0.99266055,1.),.UNSPECIFIED.);
#24390=B_SPLINE_CURVE_WITH_KNOTS('',3,(#213449,#213450,#213451,#213452,
#213453,#213454,#213455,#213456,#213457,#213458,#213459,#213460,#213461,
#213462,#213463,#213464,#213465,#213466,#213467,#213468,#213469,#213470,
#213471,#213472,#213473,#213474,#213475,#213476,#213477,#213478,#213479,
#213480,#213481,#213482,#213483,#213484,#213485,#213486,#213487,#213488,
#213489,#213490,#213491,#213492,#213493,#213494,#213495,#213496,#213497,
#213498,#213499,#213500,#213501,#213502,#213503,#213504,#213505,#213506,
#213507,#213508,#213509,#213510,#213511,#213512,#213513,#213514,#213515,
#213516,#213517,#213518,#213519,#213520,#213521,#213522,#213523,#213524,
#213525,#213526,#213527,#213528,#213529,#213530,#213531,#213532,#213533,
#213534,#213535,#213536,#213537,#213538,#213539,#213540,#213541,#213542,
#213543,#213544,#213545,#213546,#213547,#213548,#213549,#213550,#213551,
#213552,#213553,#213554,#213555,#213556,#213557,#213558,#213559,#213560,
#213561,#213562,#213563,#213564,#213565,#213566,#213567,#213568,#213569,
#213570,#213571,#213572,#213573,#213574,#213575,#213576,#213577,#213578,
#213579,#213580,#213581,#213582,#213583,#213584,#213585,#213586,#213587,
#213588,#213589,#213590,#213591,#213592,#213593,#213594,#213595,#213596,
#213597,#213598,#213599,#213600,#213601,#213602,#213603,#213604,#213605,
#213606,#213607,#213608,#213609,#213610,#213611,#213612,#213613,#213614,
#213615,#213616,#213617,#213618,#213619,#213620,#213621,#213622,#213623,
#213624,#213625,#213626,#213627,#213628,#213629,#213630,#213631,#213632,
#213633,#213634,#213635,#213636,#213637,#213638,#213639,#213640,#213641,
#213642,#213643,#213644,#213645,#213646,#213647,#213648,#213649,#213650,
#213651,#213652,#213653,#213654,#213655,#213656,#213657,#213658,#213659,
#213660,#213661,#213662,#213663,#213664,#213665,#213666,#213667,#213668,
#213669,#213670,#213671,#213672,#213673,#213674,#213675,#213676,#213677,
#213678,#213679,#213680,#213681,#213682,#213683,#213684,#213685,#213686,
#213687,#213688,#213689,#213690,#213691,#213692,#213693,#213694,#213695,
#213696,#213697,#213698,#213699,#213700,#213701,#213702,#213703,#213704,
#213705,#213706,#213707,#213708,#213709,#213710,#213711,#213712,#213713,
#213714,#213715,#213716,#213717,#213718,#213719,#213720,#213721,#213722,
#213723,#213724,#213725,#213726,#213727,#213728,#213729,#213730,#213731,
#213732,#213733,#213734,#213735,#213736,#213737,#213738,#213739,#213740,
#213741,#213742,#213743,#213744,#213745,#213746,#213747,#213748,#213749,
#213750,#213751,#213752,#213753,#213754,#213755,#213756,#213757,#213758,
#213759,#213760,#213761,#213762,#213763,#213764,#213765,#213766,#213767,
#213768,#213769,#213770,#213771,#213772,#213773),.UNSPECIFIED.,.F.,.F.,
(4,3,3,3,3,3,3,3,3,3,3,3,3,3,3,3,3,3,3,3,3,3,3,3,3,3,3,3,3,3,3,3,3,3,3,
3,3,3,3,3,3,3,3,3,3,3,3,3,3,3,3,3,3,3,3,3,3,3,3,3,3,3,3,3,3,3,3,3,3,3,3,
3,3,3,3,3,3,3,3,3,3,3,3,3,3,3,3,3,3,3,3,3,3,3,3,3,3,3,3,3,3,3,3,3,3,3,3,
3,4),(0.143172102,0.15412844,0.165137615,0.177981651,0.188990826,0.2,0.211009174,
0.222018349,0.233027523,0.244036697,0.255045872,0.266055046,0.27706422,
0.288073394,0.300917431,0.311926606,0.32293578,0.333944954,0.344954128,
0.355963303,0.366972477,0.377981651,0.388990826,0.398165138,0.40733945,
0.416513761,0.429357798,0.43853211,0.447706422,0.456880734,0.466055046,
0.475229358,0.486238532,0.495412844,0.504587156,0.513761468,0.52293578,
0.532110092,0.539449541,0.546788991,0.55412844,0.56146789,0.568807339,0.576146789,
0.583486239,0.590825688,0.598165138,0.605504587,0.612844037,0.620183486,
0.627522936,0.634862385,0.644036697,0.651376147,0.658715596,0.666055046,
0.673394495,0.680733945,0.688073394,0.695412844,0.702752294,0.710091743,
0.717431193,0.724770642,0.732110092,0.739449541,0.746788991,0.75412844,
0.76146789,0.768807339,0.776146789,0.783486239,0.790825688,0.798165138,
0.805504587,0.811009174,0.816513761,0.822018349,0.827522936,0.833027523,
0.83853211,0.844036697,0.849541284,0.855045872,0.860550459,0.866055046,
0.871559633,0.87706422,0.882568807,0.888073394,0.893577982,0.899082569,
0.904587156,0.910091743,0.91559633,0.921100917,0.928440367,0.933944954,
0.939449541,0.944954128,0.950458716,0.955963303,0.96146789,0.966972477,
0.974311927,0.979816514,0.987155963,0.99266055,1.),.UNSPECIFIED.);
#24391=B_SPLINE_CURVE_WITH_KNOTS('',3,(#214733,#214734,#214735,#214736,
#214737,#214738,#214739,#214740,#214741,#214742,#214743,#214744,#214745,
#214746,#214747,#214748,#214749,#214750,#214751,#214752,#214753,#214754,
#214755,#214756,#214757,#214758,#214759,#214760,#214761,#214762,#214763,
#214764,#214765,#214766,#214767,#214768,#214769,#214770,#214771,#214772,
#214773,#214774,#214775,#214776,#214777,#214778,#214779,#214780,#214781,
#214782,#214783,#214784,#214785,#214786,#214787,#214788,#214789,#214790,
#214791,#214792,#214793,#214794,#214795,#214796,#214797,#214798,#214799,
#214800,#214801,#214802,#214803,#214804,#214805,#214806,#214807,#214808,
#214809,#214810,#214811,#214812,#214813,#214814,#214815,#214816,#214817,
#214818,#214819,#214820,#214821,#214822,#214823,#214824,#214825,#214826,
#214827,#214828,#214829,#214830,#214831,#214832,#214833,#214834,#214835,
#214836,#214837,#214838,#214839,#214840,#214841,#214842,#214843,#214844,
#214845,#214846,#214847,#214848,#214849,#214850,#214851,#214852,#214853,
#214854,#214855,#214856,#214857,#214858,#214859,#214860,#214861,#214862,
#214863,#214864,#214865,#214866,#214867,#214868,#214869,#214870,#214871,
#214872,#214873,#214874,#214875,#214876,#214877,#214878,#214879,#214880,
#214881,#214882,#214883,#214884,#214885,#214886,#214887,#214888,#214889,
#214890,#214891,#214892,#214893,#214894,#214895,#214896,#214897,#214898,
#214899,#214900,#214901,#214902,#214903,#214904,#214905,#214906,#214907,
#214908,#214909,#214910,#214911,#214912,#214913,#214914,#214915,#214916,
#214917,#214918,#214919,#214920,#214921,#214922,#214923,#214924,#214925,
#214926,#214927,#214928,#214929,#214930,#214931,#214932,#214933,#214934,
#214935,#214936,#214937,#214938,#214939,#214940,#214941,#214942,#214943,
#214944,#214945,#214946,#214947,#214948,#214949,#214950,#214951,#214952,
#214953,#214954,#214955,#214956,#214957,#214958,#214959,#214960,#214961,
#214962,#214963,#214964,#214965,#214966,#214967,#214968,#214969,#214970,
#214971,#214972,#214973,#214974,#214975,#214976,#214977,#214978,#214979,
#214980,#214981,#214982,#214983,#214984,#214985,#214986,#214987,#214988,
#214989,#214990,#214991,#214992,#214993,#214994,#214995,#214996,#214997,
#214998,#214999,#215000,#215001,#215002,#215003,#215004,#215005,#215006,
#215007,#215008,#215009,#215010,#215011,#215012,#215013,#215014,#215015,
#215016,#215017,#215018,#215019,#215020,#215021,#215022,#215023,#215024,
#215025,#215026,#215027,#215028,#215029,#215030,#215031,#215032,#215033,
#215034,#215035,#215036,#215037,#215038,#215039),.UNSPECIFIED.,.F.,.F.,
(4,3,3,3,3,3,3,3,3,3,3,3,3,3,3,3,3,3,3,3,3,3,3,3,3,3,3,3,3,3,3,3,3,3,3,
3,3,3,3,3,3,3,3,3,3,3,3,3,3,3,3,3,3,3,3,3,3,3,3,3,3,3,3,3,3,3,3,3,3,3,3,
3,3,3,3,3,3,3,3,3,3,3,3,3,3,3,3,3,3,3,3,3,3,3,3,3,3,3,3,3,3,3,4),(0.143172102,
0.15412844,0.165137615,0.176146789,0.187155963,0.198165138,0.211009174,
0.222018349,0.233027523,0.244036697,0.255045872,0.266055046,0.27706422,
0.288073394,0.299082569,0.310091743,0.321100917,0.332110092,0.343119266,
0.35412844,0.365137615,0.376146789,0.387155963,0.396330275,0.405504587,
0.414678899,0.423853211,0.434862385,0.444036697,0.455045872,0.464220183,
0.473394495,0.482568807,0.491743119,0.500917431,0.510091743,0.519266055,
0.530275229,0.537614679,0.544954128,0.552293578,0.559633028,0.566972477,
0.574311927,0.581651376,0.59266055,0.6,0.60733945,0.614678899,0.622018349,
0.629357798,0.636697248,0.644036697,0.651376147,0.658715596,0.666055046,
0.673394495,0.680733945,0.693577982,0.704587156,0.711926606,0.719266055,
0.726605505,0.733944954,0.741284404,0.748623853,0.755963303,0.763302752,
0.772477064,0.781651376,0.790825688,0.798165138,0.80733945,0.814678899,
0.822018349,0.831192661,0.836697248,0.84587156,0.853211009,0.858715596,
0.864220183,0.869724771,0.875229358,0.88440367,0.893577982,0.899082569,
0.904587156,0.910091743,0.919266055,0.924770642,0.930275229,0.935779817,
0.943119266,0.948623853,0.95412844,0.959633028,0.966972477,0.972477064,
0.977981651,0.983486239,0.988990826,0.994495413,1.),.UNSPECIFIED.);
#24392=B_SPLINE_CURVE_WITH_KNOTS('',3,(#215040,#215041,#215042,#215043,
#215044,#215045,#215046,#215047,#215048,#215049,#215050,#215051,#215052,
#215053,#215054,#215055,#215056,#215057,#215058,#215059,#215060,#215061,
#215062,#215063,#215064,#215065,#215066,#215067,#215068,#215069,#215070,
#215071,#215072,#215073,#215074,#215075,#215076,#215077,#215078,#215079,
#215080,#215081,#215082,#215083,#215084,#215085,#215086,#215087,#215088,
#215089,#215090,#215091,#215092,#215093,#215094,#215095,#215096,#215097,
#215098,#215099,#215100,#215101,#215102,#215103,#215104,#215105,#215106,
#215107,#215108,#215109,#215110,#215111,#215112,#215113,#215114,#215115,
#215116,#215117,#215118,#215119,#215120,#215121,#215122,#215123,#215124,
#215125,#215126,#215127,#215128,#215129,#215130,#215131,#215132,#215133,
#215134,#215135,#215136,#215137,#215138,#215139,#215140,#215141,#215142,
#215143,#215144,#215145,#215146,#215147,#215148,#215149,#215150,#215151,
#215152,#215153,#215154,#215155,#215156,#215157,#215158,#215159,#215160,
#215161,#215162,#215163,#215164,#215165,#215166,#215167,#215168,#215169,
#215170,#215171,#215172,#215173,#215174,#215175,#215176,#215177,#215178,
#215179,#215180,#215181,#215182,#215183,#215184,#215185,#215186,#215187,
#215188,#215189,#215190,#215191,#215192,#215193,#215194,#215195,#215196,
#215197,#215198,#215199,#215200,#215201,#215202,#215203,#215204,#215205,
#215206,#215207,#215208,#215209,#215210,#215211,#215212,#215213,#215214,
#215215,#215216,#215217,#215218,#215219,#215220,#215221,#215222,#215223,
#215224,#215225,#215226,#215227,#215228,#215229,#215230,#215231,#215232,
#215233,#215234,#215235,#215236,#215237,#215238,#215239,#215240,#215241,
#215242,#215243,#215244,#215245,#215246,#215247,#215248,#215249,#215250,
#215251,#215252,#215253,#215254,#215255,#215256,#215257,#215258,#215259,
#215260,#215261,#215262,#215263,#215264,#215265,#215266,#215267,#215268,
#215269,#215270,#215271,#215272,#215273,#215274,#215275,#215276,#215277,
#215278,#215279,#215280,#215281,#215282,#215283,#215284,#215285,#215286,
#215287,#215288,#215289,#215290,#215291,#215292,#215293,#215294,#215295,
#215296,#215297,#215298,#215299,#215300,#215301,#215302,#215303,#215304,
#215305,#215306,#215307,#215308,#215309,#215310,#215311,#215312,#215313,
#215314,#215315,#215316,#215317,#215318,#215319,#215320,#215321,#215322,
#215323,#215324,#215325,#215326,#215327,#215328,#215329,#215330,#215331,
#215332,#215333,#215334,#215335,#215336,#215337,#215338,#215339,#215340,
#215341,#215342,#215343,#215344,#215345,#215346,#215347,#215348,#215349,
#215350,#215351,#215352,#215353,#215354,#215355,#215356,#215357,#215358,
#215359,#215360,#215361,#215362,#215363,#215364),.UNSPECIFIED.,.F.,.F.,
(4,3,3,3,3,3,3,3,3,3,3,3,3,3,3,3,3,3,3,3,3,3,3,3,3,3,3,3,3,3,3,3,3,3,3,
3,3,3,3,3,3,3,3,3,3,3,3,3,3,3,3,3,3,3,3,3,3,3,3,3,3,3,3,3,3,3,3,3,3,3,3,
3,3,3,3,3,3,3,3,3,3,3,3,3,3,3,3,3,3,3,3,3,3,3,3,3,3,3,3,3,3,3,3,3,3,3,3,
3,4),(0.143172102,0.15412844,0.165137615,0.176146789,0.187155963,0.198165138,
0.211009174,0.222018349,0.233027523,0.244036697,0.255045872,0.266055046,
0.27706422,0.288073394,0.299082569,0.310091743,0.321100917,0.332110092,
0.343119266,0.35412844,0.365137615,0.376146789,0.387155963,0.396330275,
0.405504587,0.414678899,0.423853211,0.433027523,0.442201835,0.451376147,
0.460550459,0.469724771,0.478899083,0.488073394,0.497247706,0.506422018,
0.51559633,0.524770642,0.533944954,0.541284404,0.548623853,0.555963303,
0.563302752,0.570642202,0.577981651,0.585321101,0.59266055,0.6,0.60733945,
0.614678899,0.622018349,0.629357798,0.636697248,0.644036697,0.651376147,
0.658715596,0.666055046,0.673394495,0.680733945,0.688073394,0.695412844,
0.704587156,0.711926606,0.719266055,0.726605505,0.733944954,0.741284404,
0.748623853,0.755963303,0.763302752,0.772477064,0.779816514,0.787155963,
0.794495413,0.801834862,0.809174312,0.814678899,0.820183486,0.825688073,
0.831192661,0.836697248,0.842201835,0.847706422,0.853211009,0.858715596,
0.864220183,0.869724771,0.875229358,0.882568807,0.888073394,0.893577982,
0.899082569,0.904587156,0.910091743,0.91559633,0.921100917,0.928440367,
0.933944954,0.939449541,0.944954128,0.950458716,0.957798165,0.963302752,
0.968807339,0.974311927,0.979816514,0.985321101,0.990825688,1.),
 .UNSPECIFIED.);
#24393=B_SPLINE_CURVE_WITH_KNOTS('',3,(#216312,#216313,#216314,#216315,
#216316,#216317,#216318,#216319,#216320,#216321,#216322,#216323,#216324,
#216325,#216326,#216327,#216328,#216329,#216330,#216331,#216332,#216333,
#216334,#216335,#216336,#216337,#216338,#216339,#216340,#216341,#216342,
#216343,#216344,#216345,#216346,#216347,#216348,#216349,#216350,#216351,
#216352,#216353,#216354,#216355,#216356,#216357,#216358,#216359,#216360,
#216361,#216362,#216363,#216364,#216365,#216366,#216367,#216368,#216369,
#216370,#216371,#216372,#216373,#216374,#216375,#216376,#216377,#216378,
#216379,#216380,#216381,#216382,#216383,#216384,#216385,#216386,#216387,
#216388,#216389,#216390,#216391,#216392,#216393,#216394,#216395,#216396,
#216397,#216398,#216399,#216400,#216401,#216402,#216403,#216404,#216405,
#216406,#216407,#216408,#216409,#216410,#216411,#216412,#216413,#216414,
#216415,#216416,#216417,#216418,#216419,#216420,#216421,#216422,#216423,
#216424,#216425,#216426,#216427,#216428,#216429,#216430,#216431,#216432,
#216433,#216434,#216435,#216436,#216437,#216438,#216439,#216440,#216441,
#216442,#216443,#216444,#216445,#216446,#216447,#216448,#216449,#216450,
#216451,#216452,#216453,#216454,#216455,#216456,#216457,#216458,#216459,
#216460,#216461,#216462,#216463,#216464,#216465,#216466,#216467,#216468,
#216469,#216470,#216471,#216472,#216473,#216474,#216475,#216476,#216477,
#216478,#216479,#216480,#216481,#216482,#216483,#216484,#216485,#216486,
#216487,#216488,#216489,#216490,#216491,#216492,#216493,#216494,#216495,
#216496,#216497,#216498,#216499,#216500,#216501,#216502,#216503,#216504,
#216505,#216506,#216507,#216508,#216509,#216510,#216511,#216512,#216513,
#216514,#216515,#216516,#216517,#216518,#216519,#216520,#216521,#216522,
#216523,#216524,#216525,#216526,#216527,#216528,#216529,#216530,#216531,
#216532,#216533,#216534,#216535,#216536,#216537,#216538,#216539,#216540,
#216541,#216542,#216543,#216544,#216545,#216546,#216547,#216548,#216549,
#216550,#216551,#216552,#216553,#216554,#216555,#216556,#216557,#216558,
#216559,#216560,#216561,#216562,#216563,#216564,#216565,#216566,#216567,
#216568,#216569,#216570,#216571,#216572,#216573,#216574,#216575,#216576,
#216577,#216578,#216579,#216580,#216581,#216582,#216583,#216584,#216585,
#216586,#216587,#216588,#216589,#216590,#216591,#216592,#216593,#216594,
#216595,#216596,#216597,#216598,#216599,#216600,#216601,#216602,#216603,
#216604,#216605,#216606,#216607,#216608,#216609,#216610,#216611,#216612,
#216613,#216614,#216615,#216616,#216617,#216618,#216619,#216620,#216621,
#216622,#216623,#216624,#216625,#216626,#216627,#216628,#216629,#216630,
#216631,#216632,#216633),.UNSPECIFIED.,.F.,.F.,(4,3,3,3,3,3,3,3,3,3,3,3,
3,3,3,3,3,3,3,3,3,3,3,3,3,3,3,3,3,3,3,3,3,3,3,3,3,3,3,3,3,3,3,3,3,3,3,3,
3,3,3,3,3,3,3,3,3,3,3,3,3,3,3,3,3,3,3,3,3,3,3,3,3,3,3,3,3,3,3,3,3,3,3,3,
3,3,3,3,3,3,3,3,3,3,3,3,3,3,3,3,3,3,3,3,3,3,3,4),(-1.,-0.99266055,-0.985321101,
-0.979816514,-0.974311927,-0.968807339,-0.963302752,-0.957798165,-0.952293578,
-0.946788991,-0.941284404,-0.933944954,-0.928440367,-0.92293578,-0.917431193,
-0.911926606,-0.906422018,-0.900917431,-0.895412844,-0.889908257,-0.88440367,
-0.878899083,-0.873394495,-0.867889908,-0.862385321,-0.856880734,-0.851376147,
-0.84587156,-0.840366972,-0.833027523,-0.827522936,-0.822018349,-0.816513761,
-0.809174312,-0.801834862,-0.794495413,-0.787155963,-0.779816514,-0.772477064,
-0.765137615,-0.757798165,-0.750458716,-0.743119266,-0.735779817,-0.728440367,
-0.721100917,-0.710091743,-0.702752294,-0.695412844,-0.688073394,-0.680733945,
-0.673394495,-0.666055046,-0.658715596,-0.651376147,-0.644036697,-0.636697248,
-0.627522936,-0.620183486,-0.612844037,-0.605504587,-0.598165138,-0.590825688,
-0.583486239,-0.576146789,-0.568807339,-0.56146789,-0.55412844,-0.546788991,
-0.539449541,-0.532110092,-0.52293578,-0.513761468,-0.504587156,-0.495412844,
-0.486238532,-0.47706422,-0.467889908,-0.458715596,-0.447706422,-0.43853211,
-0.429357798,-0.420183486,-0.411009174,-0.401834862,-0.39266055,-0.381651376,
-0.370642202,-0.359633028,-0.346788991,-0.335779817,-0.324770642,-0.313761468,
-0.302752294,-0.291743119,-0.280733945,-0.269724771,-0.258715596,-0.247706422,
-0.236697248,-0.225688073,-0.214678899,-0.203669725,-0.19266055,-0.181651376,
-0.170642202,-0.159633028,-0.143172102),.UNSPECIFIED.);
#24394=B_SPLINE_CURVE_WITH_KNOTS('',3,(#216634,#216635,#216636,#216637,
#216638,#216639,#216640,#216641,#216642,#216643,#216644,#216645,#216646,
#216647,#216648,#216649,#216650,#216651,#216652,#216653,#216654,#216655,
#216656,#216657,#216658,#216659,#216660,#216661,#216662,#216663,#216664,
#216665,#216666,#216667,#216668,#216669,#216670,#216671,#216672,#216673,
#216674,#216675,#216676,#216677,#216678,#216679,#216680,#216681,#216682,
#216683,#216684,#216685,#216686,#216687,#216688,#216689,#216690,#216691,
#216692,#216693,#216694,#216695,#216696,#216697,#216698,#216699,#216700,
#216701,#216702,#216703,#216704,#216705,#216706,#216707,#216708,#216709,
#216710,#216711,#216712,#216713,#216714,#216715,#216716,#216717,#216718,
#216719,#216720,#216721,#216722,#216723,#216724,#216725,#216726,#216727,
#216728,#216729,#216730,#216731,#216732,#216733,#216734,#216735,#216736,
#216737,#216738,#216739,#216740,#216741,#216742,#216743,#216744,#216745,
#216746,#216747,#216748,#216749,#216750,#216751,#216752,#216753,#216754,
#216755,#216756,#216757,#216758,#216759,#216760,#216761,#216762,#216763,
#216764,#216765,#216766,#216767,#216768,#216769,#216770,#216771,#216772,
#216773,#216774,#216775,#216776,#216777,#216778,#216779,#216780,#216781,
#216782,#216783,#216784,#216785,#216786,#216787,#216788,#216789,#216790,
#216791,#216792,#216793,#216794,#216795,#216796,#216797,#216798,#216799,
#216800,#216801,#216802,#216803,#216804,#216805,#216806,#216807,#216808,
#216809,#216810,#216811,#216812,#216813,#216814,#216815,#216816,#216817,
#216818,#216819,#216820,#216821,#216822,#216823,#216824,#216825,#216826,
#216827,#216828,#216829,#216830,#216831,#216832,#216833,#216834,#216835,
#216836,#216837,#216838,#216839,#216840,#216841,#216842,#216843,#216844,
#216845,#216846,#216847,#216848,#216849,#216850,#216851,#216852,#216853,
#216854,#216855,#216856,#216857,#216858,#216859,#216860,#216861,#216862,
#216863,#216864,#216865,#216866,#216867,#216868,#216869,#216870,#216871,
#216872,#216873,#216874,#216875,#216876,#216877,#216878,#216879,#216880,
#216881,#216882,#216883,#216884,#216885,#216886,#216887,#216888,#216889,
#216890,#216891,#216892,#216893,#216894,#216895,#216896,#216897,#216898,
#216899,#216900,#216901,#216902,#216903,#216904,#216905,#216906,#216907,
#216908,#216909,#216910,#216911,#216912,#216913,#216914,#216915,#216916,
#216917,#216918,#216919,#216920,#216921,#216922,#216923,#216924,#216925,
#216926,#216927,#216928,#216929,#216930,#216931,#216932,#216933,#216934,
#216935,#216936,#216937,#216938,#216939,#216940),.UNSPECIFIED.,.F.,.F.,
(4,3,3,3,3,3,3,3,3,3,3,3,3,3,3,3,3,3,3,3,3,3,3,3,3,3,3,3,3,3,3,3,3,3,3,
3,3,3,3,3,3,3,3,3,3,3,3,3,3,3,3,3,3,3,3,3,3,3,3,3,3,3,3,3,3,3,3,3,3,3,3,
3,3,3,3,3,3,3,3,3,3,3,3,3,3,3,3,3,3,3,3,3,3,3,3,3,3,3,3,3,3,3,4),(0.143172102,
0.15412844,0.165137615,0.176146789,0.187155963,0.198165138,0.209174312,
0.220183486,0.231192661,0.242201835,0.253211009,0.264220183,0.275229358,
0.286238532,0.297247706,0.308256881,0.319266055,0.330275229,0.341284404,
0.352293578,0.363302752,0.376146789,0.387155963,0.396330275,0.405504587,
0.416513761,0.425688073,0.434862385,0.444036697,0.453211009,0.462385321,
0.471559633,0.48440367,0.493577982,0.502752294,0.511926606,0.521100917,
0.530275229,0.537614679,0.544954128,0.552293578,0.56146789,0.568807339,
0.576146789,0.585321101,0.594495413,0.601834862,0.609174312,0.616513761,
0.623853211,0.631192661,0.63853211,0.64587156,0.653211009,0.662385321,0.669724771,
0.678899083,0.688073394,0.695412844,0.702752294,0.710091743,0.721100917,
0.730275229,0.739449541,0.746788991,0.75412844,0.763302752,0.770642202,
0.777981651,0.785321101,0.79266055,0.801834862,0.809174312,0.816513761,
0.822018349,0.827522936,0.836697248,0.844036697,0.851376147,0.856880734,
0.862385321,0.867889908,0.873394495,0.882568807,0.888073394,0.893577982,
0.900917431,0.906422018,0.913761468,0.919266055,0.924770642,0.930275229,
0.937614679,0.944954128,0.952293578,0.957798165,0.963302752,0.968807339,
0.974311927,0.979816514,0.988990826,0.994495413,1.),.UNSPECIFIED.);
#24395=B_SPLINE_CURVE_WITH_KNOTS('',5,(#217903,#217904,#217905,#217906,
#217907,#217908,#217909,#217910,#217911,#217912,#217913,#217914,#217915,
#217916,#217917,#217918,#217919,#217920,#217921,#217922,#217923,#217924,
#217925,#217926,#217927,#217928,#217929,#217930,#217931,#217932,#217933,
#217934,#217935,#217936,#217937,#217938,#217939,#217940,#217941,#217942,
#217943,#217944,#217945,#217946,#217947,#217948,#217949,#217950,#217951,
#217952,#217953,#217954,#217955,#217956,#217957,#217958,#217959,#217960,
#217961,#217962,#217963,#217964,#217965,#217966,#217967,#217968,#217969,
#217970,#217971,#217972,#217973,#217974,#217975,#217976,#217977,#217978,
#217979,#217980,#217981,#217982,#217983,#217984,#217985,#217986,#217987,
#217988,#217989,#217990,#217991,#217992,#217993,#217994,#217995,#217996,
#217997,#217998,#217999,#218000,#218001,#218002,#218003,#218004,#218005,
#218006,#218007,#218008,#218009,#218010,#218011,#218012,#218013,#218014,
#218015,#218016,#218017,#218018,#218019,#218020,#218021,#218022,#218023,
#218024,#218025,#218026,#218027,#218028,#218029,#218030,#218031,#218032,
#218033,#218034,#218035,#218036,#218037,#218038,#218039,#218040,#218041,
#218042,#218043,#218044,#218045,#218046,#218047,#218048,#218049,#218050,
#218051,#218052,#218053,#218054,#218055,#218056,#218057,#218058,#218059,
#218060,#218061,#218062,#218063,#218064,#218065,#218066,#218067,#218068,
#218069,#218070,#218071,#218072,#218073,#218074,#218075,#218076,#218077,
#218078,#218079,#218080,#218081,#218082,#218083,#218084,#218085,#218086,
#218087,#218088,#218089,#218090,#218091,#218092,#218093,#218094,#218095,
#218096,#218097,#218098,#218099,#218100,#218101,#218102,#218103,#218104,
#218105,#218106,#218107,#218108,#218109,#218110,#218111,#218112,#218113,
#218114,#218115,#218116,#218117,#218118,#218119,#218120,#218121,#218122,
#218123,#218124,#218125,#218126,#218127,#218128,#218129,#218130,#218131,
#218132,#218133,#218134,#218135,#218136,#218137,#218138,#218139,#218140,
#218141,#218142,#218143,#218144,#218145,#218146,#218147,#218148,#218149,
#218150,#218151,#218152,#218153,#218154,#218155,#218156,#218157,#218158,
#218159,#218160,#218161,#218162,#218163,#218164,#218165,#218166,#218167,
#218168,#218169,#218170,#218171,#218172,#218173,#218174,#218175,#218176,
#218177,#218178,#218179,#218180,#218181,#218182,#218183,#218184,#218185,
#218186,#218187,#218188,#218189,#218190,#218191,#218192,#218193,#218194,
#218195,#218196,#218197,#218198,#218199,#218200,#218201,#218202,#218203,
#218204,#218205,#218206,#218207,#218208,#218209,#218210,#218211,#218212,
#218213,#218214,#218215,#218216,#218217,#218218,#218219,#218220,#218221,
#218222,#218223,#218224,#218225,#218226,#218227,#218228,#218229,#218230,
#218231,#218232,#218233,#218234,#218235,#218236,#218237,#218238,#218239,
#218240,#218241,#218242,#218243,#218244,#218245,#218246,#218247,#218248,
#218249,#218250,#218251,#218252,#218253,#218254,#218255,#218256,#218257,
#218258,#218259,#218260,#218261,#218262,#218263,#218264,#218265,#218266,
#218267,#218268,#218269,#218270,#218271,#218272,#218273,#218274,#218275,
#218276,#218277,#218278,#218279,#218280,#218281,#218282,#218283,#218284,
#218285,#218286,#218287,#218288,#218289,#218290,#218291,#218292,#218293,
#218294,#218295,#218296,#218297,#218298,#218299,#218300,#218301,#218302,
#218303,#218304,#218305,#218306,#218307,#218308,#218309,#218310,#218311,
#218312,#218313,#218314,#218315,#218316,#218317,#218318,#218319,#218320,
#218321,#218322,#218323,#218324,#218325,#218326,#218327,#218328,#218329,
#218330,#218331,#218332,#218333,#218334,#218335,#218336,#218337,#218338,
#218339,#218340,#218341,#218342,#218343,#218344,#218345,#218346,#218347,
#218348,#218349,#218350,#218351,#218352,#218353,#218354,#218355,#218356,
#218357,#218358,#218359,#218360,#218361,#218362,#218363,#218364,#218365,
#218366,#218367,#218368,#218369,#218370,#218371,#218372,#218373),
 .UNSPECIFIED.,.F.,.F.,(6,1,1,1,1,1,1,1,1,1,1,1,1,1,1,1,1,1,1,1,1,1,1,1,
1,1,1,1,1,1,1,1,1,1,1,1,1,1,1,1,1,1,1,1,1,1,1,1,1,1,1,1,1,1,1,1,1,1,1,1,
1,1,1,1,1,1,1,1,1,1,1,1,1,1,1,1,1,1,1,1,1,1,1,1,1,1,1,1,1,1,1,1,1,1,1,1,
1,1,1,1,1,1,1,1,1,1,1,1,1,1,1,1,1,1,1,1,1,1,1,1,1,1,1,1,1,1,1,1,1,1,1,1,
1,1,1,1,1,1,1,1,1,1,1,1,1,1,1,1,1,1,1,1,1,1,1,1,1,1,1,1,1,1,1,1,1,1,1,1,
1,1,1,1,1,1,1,1,1,1,1,1,1,1,1,1,1,1,1,1,1,1,1,1,1,1,1,1,1,1,1,1,1,1,1,1,
1,1,1,1,1,1,1,1,1,1,1,1,1,1,1,1,1,1,1,1,1,1,1,1,1,1,1,1,1,1,1,1,1,1,1,1,
1,1,1,1,1,1,1,1,1,1,1,1,1,1,1,1,1,1,1,1,1,1,1,1,1,1,1,1,1,1,1,1,1,1,1,1,
1,1,1,1,1,1,1,1,1,1,1,1,1,1,1,1,1,1,1,1,1,1,1,1,1,1,1,1,1,1,1,1,1,1,1,1,
1,1,1,1,1,1,1,1,1,1,1,1,1,1,1,1,1,1,1,1,1,1,1,1,1,1,1,1,1,1,1,1,1,1,1,1,
1,1,1,1,1,1,1,1,1,1,1,1,1,1,1,1,1,1,1,1,1,1,1,1,1,1,1,1,1,1,1,1,1,1,1,1,
1,1,1,1,1,1,1,1,1,1,1,1,1,1,1,1,1,1,1,1,1,1,1,1,1,1,1,1,1,1,1,1,1,1,1,1,
1,1,1,1,1,1,1,1,1,1,1,1,1,1,1,1,1,1,1,1,1,1,1,1,1,1,1,1,1,1,1,1,1,1,1,1,
1,1,1,1,1,1,1,1,1,1,6),(-1.,-0.998165138,-0.996330275,-0.994495413,-0.99266055,
-0.990825688,-0.988990826,-0.987155963,-0.985321101,-0.983486239,-0.981651376,
-0.979816514,-0.977981651,-0.976146789,-0.974311927,-0.972477064,-0.970642202,
-0.968807339,-0.966972477,-0.965137615,-0.963302752,-0.96146789,-0.959633028,
-0.957798165,-0.955963303,-0.95412844,-0.952293578,-0.950458716,-0.948623853,
-0.946788991,-0.944954128,-0.943119266,-0.941284404,-0.939449541,-0.937614679,
-0.935779817,-0.933944954,-0.932110092,-0.930275229,-0.928440367,-0.926605505,
-0.924770642,-0.92293578,-0.921100917,-0.919266055,-0.917431193,-0.91559633,
-0.913761468,-0.911926606,-0.910091743,-0.908256881,-0.906422018,-0.904587156,
-0.902752294,-0.900917431,-0.899082569,-0.897247706,-0.895412844,-0.893577982,
-0.891743119,-0.889908257,-0.888073394,-0.886238532,-0.88440367,-0.882568807,
-0.880733945,-0.878899083,-0.87706422,-0.875229358,-0.873394495,-0.871559633,
-0.869724771,-0.867889908,-0.866055046,-0.864220183,-0.862385321,-0.860550459,
-0.858715596,-0.856880734,-0.855045872,-0.853211009,-0.851376147,-0.849541284,
-0.847706422,-0.84587156,-0.844036697,-0.842201835,-0.840366972,-0.83853211,
-0.836697248,-0.834862385,-0.833027523,-0.831192661,-0.829357798,-0.827522936,
-0.825688073,-0.823853211,-0.822018349,-0.820183486,-0.818348624,-0.816513761,
-0.814678899,-0.812844037,-0.811009174,-0.809174312,-0.80733945,-0.805504587,
-0.803669725,-0.801834862,-0.8,-0.798165138,-0.796330275,-0.794495413,-0.79266055,
-0.790825688,-0.788990826,-0.787155963,-0.785321101,-0.783486239,-0.781651376,
-0.779816514,-0.777981651,-0.776146789,-0.774311927,-0.772477064,-0.770642202,
-0.768807339,-0.766972477,-0.765137615,-0.763302752,-0.76146789,-0.759633028,
-0.757798165,-0.755963303,-0.75412844,-0.752293578,-0.750458716,-0.748623853,
-0.746788991,-0.744954128,-0.743119266,-0.741284404,-0.739449541,-0.737614679,
-0.735779817,-0.733944954,-0.732110092,-0.730275229,-0.728440367,-0.726605505,
-0.724770642,-0.72293578,-0.721100917,-0.719266055,-0.717431193,-0.71559633,
-0.713761468,-0.711926606,-0.710091743,-0.708256881,-0.706422018,-0.704587156,
-0.702752294,-0.700917431,-0.699082569,-0.697247706,-0.695412844,-0.693577982,
-0.691743119,-0.689908257,-0.688073394,-0.686238532,-0.68440367,-0.682568807,
-0.680733945,-0.678899083,-0.67706422,-0.675229358,-0.673394495,-0.671559633,
-0.669724771,-0.667889908,-0.666055046,-0.664220183,-0.662385321,-0.660550459,
-0.658715596,-0.656880734,-0.655045872,-0.653211009,-0.651376147,-0.649541284,
-0.647706422,-0.64587156,-0.644036697,-0.642201835,-0.640366972,-0.63853211,
-0.636697248,-0.634862385,-0.633027523,-0.631192661,-0.629357798,-0.627522936,
-0.625688073,-0.623853211,-0.622018349,-0.618348624,-0.616513761,-0.614678899,
-0.612844037,-0.611009174,-0.609174312,-0.60733945,-0.605504587,-0.603669725,
-0.601834862,-0.6,-0.598165138,-0.596330275,-0.594495413,-0.59266055,-0.590825688,
-0.588990826,-0.587155963,-0.585321101,-0.583486239,-0.581651376,-0.579816514,
-0.577981651,-0.576146789,-0.574311927,-0.572477064,-0.570642202,-0.568807339,
-0.566972477,-0.565137615,-0.563302752,-0.56146789,-0.559633028,-0.557798165,
-0.555963303,-0.55412844,-0.552293578,-0.550458716,-0.548623853,-0.546788991,
-0.544954128,-0.543119266,-0.541284404,-0.539449541,-0.537614679,-0.535779817,
-0.533944954,-0.532110092,-0.530275229,-0.528440367,-0.526605505,-0.524770642,
-0.52293578,-0.521100917,-0.519266055,-0.517431193,-0.51559633,-0.513761468,
-0.511926606,-0.510091743,-0.508256881,-0.506422018,-0.504587156,-0.502752294,
-0.500917431,-0.499082569,-0.497247706,-0.495412844,-0.493577982,-0.491743119,
-0.489908257,-0.488073394,-0.486238532,-0.48440367,-0.482568807,-0.480733945,
-0.478899083,-0.47706422,-0.475229358,-0.473394495,-0.471559633,-0.469724771,
-0.467889908,-0.466055046,-0.464220183,-0.462385321,-0.460550459,-0.458715596,
-0.456880734,-0.455045872,-0.453211009,-0.451376147,-0.449541284,-0.447706422,
-0.44587156,-0.444036697,-0.442201835,-0.440366972,-0.43853211,-0.436697248,
-0.434862385,-0.433027523,-0.431192661,-0.429357798,-0.427522936,-0.425688073,
-0.423853211,-0.422018349,-0.420183486,-0.418348624,-0.416513761,-0.414678899,
-0.412844037,-0.411009174,-0.409174312,-0.40733945,-0.405504587,-0.403669725,
-0.401834862,-0.4,-0.398165138,-0.396330275,-0.394495413,-0.39266055,-0.390825688,
-0.388990826,-0.387155963,-0.385321101,-0.383486239,-0.381651376,-0.379816514,
-0.377981651,-0.376146789,-0.374311927,-0.372477064,-0.370642202,-0.368807339,
-0.366972477,-0.365137615,-0.363302752,-0.36146789,-0.359633028,-0.357798165,
-0.355963303,-0.35412844,-0.352293578,-0.350458716,-0.348623853,-0.346788991,
-0.344954128,-0.343119266,-0.341284404,-0.339449541,-0.337614679,-0.335779817,
-0.333944954,-0.332110092,-0.330275229,-0.328440367,-0.326605505,-0.324770642,
-0.32293578,-0.321100917,-0.319266055,-0.317431193,-0.31559633,-0.313761468,
-0.311926606,-0.310091743,-0.308256881,-0.306422018,-0.304587156,-0.302752294,
-0.300917431,-0.299082569,-0.297247706,-0.295412844,-0.293577982,-0.291743119,
-0.289908257,-0.288073394,-0.286238532,-0.28440367,-0.282568807,-0.280733945,
-0.278899083,-0.27706422,-0.275229358,-0.273394495,-0.271559633,-0.269724771,
-0.267889908,-0.266055046,-0.264220183,-0.262385321,-0.260550459,-0.258715596,
-0.256880734,-0.255045872,-0.253211009,-0.251376147,-0.249541284,-0.247706422,
-0.24587156,-0.244036697,-0.242201835,-0.240366972,-0.23853211,-0.236697248,
-0.234862385,-0.233027523,-0.231192661,-0.229357798,-0.227522936,-0.225688073,
-0.223853211,-0.222018349,-0.220183486,-0.218348624,-0.216513761,-0.214678899,
-0.212844037,-0.211009174,-0.209174312,-0.20733945,-0.205504587,-0.203669725,
-0.201834862,-0.2,-0.198165138,-0.196330275,-0.194495413,-0.19266055,-0.190825688,
-0.188990826,-0.187155963,-0.185321101,-0.183486239,-0.181651376,-0.179816514,
-0.177981651,-0.176146789,-0.174311927,-0.172477064,-0.170642202,-0.168807339,
-0.166972477,-0.165137615,-0.163302752,-0.16146789,-0.159633028,-0.157798165,
-0.155963303,-0.15412844,-0.152293578,-0.150458716,-0.148623853,-0.146788991,
-0.144954128,-0.143172102),.UNSPECIFIED.);
#24396=B_SPLINE_CURVE_WITH_KNOTS('',5,(#218374,#218375,#218376,#218377,
#218378,#218379,#218380,#218381,#218382,#218383,#218384,#218385,#218386,
#218387,#218388,#218389,#218390,#218391,#218392,#218393,#218394,#218395,
#218396,#218397,#218398,#218399,#218400,#218401,#218402,#218403,#218404,
#218405,#218406,#218407,#218408,#218409,#218410,#218411,#218412,#218413,
#218414,#218415,#218416,#218417,#218418,#218419,#218420,#218421,#218422,
#218423,#218424,#218425,#218426,#218427,#218428,#218429,#218430,#218431,
#218432,#218433,#218434,#218435,#218436,#218437,#218438,#218439,#218440,
#218441,#218442,#218443,#218444,#218445,#218446,#218447,#218448,#218449,
#218450,#218451,#218452,#218453,#218454,#218455,#218456,#218457,#218458,
#218459,#218460,#218461,#218462,#218463,#218464,#218465,#218466,#218467,
#218468,#218469,#218470,#218471,#218472,#218473,#218474,#218475,#218476,
#218477,#218478,#218479,#218480,#218481,#218482,#218483,#218484,#218485,
#218486,#218487,#218488,#218489,#218490,#218491,#218492,#218493,#218494,
#218495,#218496,#218497,#218498,#218499,#218500,#218501,#218502,#218503,
#218504,#218505,#218506,#218507,#218508,#218509,#218510,#218511,#218512,
#218513,#218514,#218515,#218516,#218517,#218518,#218519,#218520,#218521,
#218522,#218523,#218524,#218525,#218526,#218527,#218528,#218529,#218530,
#218531,#218532,#218533,#218534,#218535,#218536,#218537,#218538,#218539,
#218540,#218541,#218542,#218543,#218544,#218545,#218546,#218547,#218548,
#218549,#218550,#218551,#218552,#218553,#218554,#218555,#218556,#218557,
#218558,#218559,#218560,#218561,#218562,#218563,#218564,#218565,#218566,
#218567,#218568,#218569,#218570,#218571,#218572,#218573,#218574,#218575,
#218576,#218577,#218578,#218579,#218580,#218581,#218582,#218583,#218584,
#218585,#218586,#218587,#218588,#218589,#218590,#218591,#218592,#218593,
#218594,#218595,#218596,#218597,#218598,#218599,#218600,#218601,#218602,
#218603,#218604,#218605,#218606,#218607,#218608,#218609,#218610,#218611,
#218612,#218613,#218614,#218615,#218616,#218617,#218618,#218619,#218620,
#218621,#218622,#218623,#218624,#218625,#218626,#218627,#218628,#218629,
#218630,#218631,#218632,#218633,#218634,#218635,#218636,#218637,#218638,
#218639,#218640,#218641,#218642,#218643,#218644,#218645,#218646,#218647,
#218648,#218649,#218650,#218651,#218652,#218653,#218654,#218655,#218656,
#218657,#218658,#218659,#218660,#218661,#218662,#218663,#218664,#218665,
#218666,#218667,#218668,#218669,#218670,#218671,#218672,#218673,#218674,
#218675,#218676,#218677,#218678,#218679,#218680,#218681,#218682,#218683,
#218684,#218685,#218686,#218687,#218688,#218689,#218690,#218691,#218692,
#218693,#218694,#218695,#218696,#218697,#218698,#218699,#218700,#218701,
#218702,#218703,#218704,#218705,#218706,#218707,#218708,#218709,#218710,
#218711,#218712,#218713,#218714,#218715,#218716,#218717,#218718,#218719,
#218720,#218721,#218722,#218723,#218724,#218725,#218726,#218727,#218728,
#218729,#218730,#218731,#218732,#218733,#218734,#218735,#218736,#218737,
#218738,#218739,#218740,#218741,#218742,#218743,#218744,#218745,#218746,
#218747,#218748,#218749,#218750,#218751,#218752,#218753,#218754,#218755,
#218756,#218757,#218758,#218759,#218760,#218761,#218762,#218763,#218764,
#218765,#218766,#218767,#218768,#218769,#218770,#218771,#218772,#218773,
#218774,#218775,#218776,#218777,#218778,#218779,#218780,#218781,#218782,
#218783,#218784,#218785,#218786,#218787,#218788,#218789,#218790,#218791,
#218792,#218793,#218794,#218795,#218796,#218797,#218798,#218799,#218800,
#218801,#218802,#218803,#218804,#218805,#218806,#218807,#218808,#218809,
#218810,#218811,#218812,#218813,#218814,#218815,#218816,#218817,#218818,
#218819,#218820,#218821,#218822,#218823,#218824,#218825,#218826,#218827,
#218828,#218829,#218830,#218831,#218832,#218833,#218834,#218835,#218836,
#218837,#218838,#218839,#218840,#218841,#218842,#218843,#218844),
 .UNSPECIFIED.,.F.,.F.,(6,1,1,1,1,1,1,1,1,1,1,1,1,1,1,1,1,1,1,1,1,1,1,1,
1,1,1,1,1,1,1,1,1,1,1,1,1,1,1,1,1,1,1,1,1,1,1,1,1,1,1,1,1,1,1,1,1,1,1,1,
1,1,1,1,1,1,1,1,1,1,1,1,1,1,1,1,1,1,1,1,1,1,1,1,1,1,1,1,1,1,1,1,1,1,1,1,
1,1,1,1,1,1,1,1,1,1,1,1,1,1,1,1,1,1,1,1,1,1,1,1,1,1,1,1,1,1,1,1,1,1,1,1,
1,1,1,1,1,1,1,1,1,1,1,1,1,1,1,1,1,1,1,1,1,1,1,1,1,1,1,1,1,1,1,1,1,1,1,1,
1,1,1,1,1,1,1,1,1,1,1,1,1,1,1,1,1,1,1,1,1,1,1,1,1,1,1,1,1,1,1,1,1,1,1,1,
1,1,1,1,1,1,1,1,1,1,1,1,1,1,1,1,1,1,1,1,1,1,1,1,1,1,1,1,1,1,1,1,1,1,1,1,
1,1,1,1,1,1,1,1,1,1,1,1,1,1,1,1,1,1,1,1,1,1,1,1,1,1,1,1,1,1,1,1,1,1,1,1,
1,1,1,1,1,1,1,1,1,1,1,1,1,1,1,1,1,1,1,1,1,1,1,1,1,1,1,1,1,1,1,1,1,1,1,1,
1,1,1,1,1,1,1,1,1,1,1,1,1,1,1,1,1,1,1,1,1,1,1,1,1,1,1,1,1,1,1,1,1,1,1,1,
1,1,1,1,1,1,1,1,1,1,1,1,1,1,1,1,1,1,1,1,1,1,1,1,1,1,1,1,1,1,1,1,1,1,1,1,
1,1,1,1,1,1,1,1,1,1,1,1,1,1,1,1,1,1,1,1,1,1,1,1,1,1,1,1,1,1,1,1,1,1,1,1,
1,1,1,1,1,1,1,1,1,1,1,1,1,1,1,1,1,1,1,1,1,1,1,1,1,1,1,1,1,1,1,1,1,1,1,1,
1,1,1,1,1,1,1,1,1,1,6),(0.143172102,0.144954128,0.146788991,0.148623853,
0.150458716,0.152293578,0.15412844,0.155963303,0.157798165,0.159633028,
0.16146789,0.163302752,0.165137615,0.166972477,0.168807339,0.170642202,
0.172477064,0.174311927,0.176146789,0.177981651,0.179816514,0.181651376,
0.183486239,0.185321101,0.187155963,0.188990826,0.190825688,0.19266055,
0.194495413,0.196330275,0.198165138,0.2,0.201834862,0.203669725,0.205504587,
0.20733945,0.209174312,0.211009174,0.212844037,0.214678899,0.216513761,
0.218348624,0.220183486,0.222018349,0.223853211,0.225688073,0.227522936,
0.229357798,0.231192661,0.233027523,0.234862385,0.236697248,0.23853211,
0.240366972,0.242201835,0.244036697,0.24587156,0.247706422,0.249541284,
0.251376147,0.253211009,0.255045872,0.256880734,0.258715596,0.260550459,
0.262385321,0.264220183,0.266055046,0.267889908,0.269724771,0.271559633,
0.273394495,0.275229358,0.27706422,0.278899083,0.280733945,0.282568807,
0.28440367,0.286238532,0.288073394,0.289908257,0.291743119,0.293577982,
0.295412844,0.297247706,0.299082569,0.300917431,0.302752294,0.304587156,
0.306422018,0.308256881,0.310091743,0.311926606,0.313761468,0.31559633,
0.317431193,0.319266055,0.321100917,0.32293578,0.324770642,0.326605505,
0.328440367,0.330275229,0.332110092,0.333944954,0.335779817,0.337614679,
0.339449541,0.341284404,0.343119266,0.344954128,0.346788991,0.348623853,
0.350458716,0.352293578,0.35412844,0.355963303,0.357798165,0.359633028,
0.36146789,0.363302752,0.365137615,0.366972477,0.368807339,0.370642202,
0.372477064,0.374311927,0.376146789,0.377981651,0.379816514,0.381651376,
0.383486239,0.385321101,0.387155963,0.388990826,0.390825688,0.39266055,
0.394495413,0.396330275,0.398165138,0.4,0.401834862,0.403669725,0.405504587,
0.40733945,0.409174312,0.411009174,0.412844037,0.414678899,0.416513761,
0.418348624,0.420183486,0.422018349,0.423853211,0.425688073,0.427522936,
0.429357798,0.431192661,0.433027523,0.434862385,0.436697248,0.43853211,
0.440366972,0.442201835,0.444036697,0.44587156,0.447706422,0.449541284,
0.451376147,0.453211009,0.455045872,0.456880734,0.458715596,0.460550459,
0.462385321,0.464220183,0.466055046,0.467889908,0.469724771,0.471559633,
0.473394495,0.475229358,0.47706422,0.478899083,0.480733945,0.482568807,
0.48440367,0.486238532,0.488073394,0.489908257,0.491743119,0.493577982,
0.495412844,0.497247706,0.499082569,0.500917431,0.502752294,0.504587156,
0.506422018,0.508256881,0.510091743,0.511926606,0.513761468,0.51559633,
0.517431193,0.519266055,0.521100917,0.52293578,0.524770642,0.526605505,
0.528440367,0.530275229,0.532110092,0.533944954,0.535779817,0.537614679,
0.539449541,0.541284404,0.543119266,0.544954128,0.546788991,0.548623853,
0.550458716,0.552293578,0.55412844,0.555963303,0.557798165,0.559633028,
0.56146789,0.563302752,0.565137615,0.566972477,0.568807339,0.570642202,
0.572477064,0.574311927,0.576146789,0.577981651,0.579816514,0.581651376,
0.583486239,0.585321101,0.587155963,0.588990826,0.590825688,0.59266055,
0.594495413,0.596330275,0.598165138,0.6,0.601834862,0.603669725,0.605504587,
0.60733945,0.609174312,0.611009174,0.612844037,0.614678899,0.616513761,
0.618348624,0.622018349,0.623853211,0.625688073,0.627522936,0.629357798,
0.631192661,0.633027523,0.634862385,0.636697248,0.63853211,0.640366972,
0.642201835,0.644036697,0.64587156,0.647706422,0.649541284,0.651376147,
0.653211009,0.655045872,0.656880734,0.658715596,0.660550459,0.662385321,
0.664220183,0.666055046,0.667889908,0.669724771,0.671559633,0.673394495,
0.675229358,0.67706422,0.678899083,0.680733945,0.682568807,0.68440367,0.686238532,
0.688073394,0.689908257,0.691743119,0.693577982,0.695412844,0.697247706,
0.699082569,0.700917431,0.702752294,0.704587156,0.706422018,0.708256881,
0.710091743,0.711926606,0.713761468,0.71559633,0.717431193,0.719266055,
0.721100917,0.72293578,0.724770642,0.726605505,0.728440367,0.730275229,
0.732110092,0.733944954,0.735779817,0.737614679,0.739449541,0.741284404,
0.743119266,0.744954128,0.746788991,0.748623853,0.750458716,0.752293578,
0.75412844,0.755963303,0.757798165,0.759633028,0.76146789,0.763302752,0.765137615,
0.766972477,0.768807339,0.770642202,0.772477064,0.774311927,0.776146789,
0.777981651,0.779816514,0.781651376,0.783486239,0.785321101,0.787155963,
0.788990826,0.790825688,0.79266055,0.794495413,0.796330275,0.798165138,
0.8,0.801834862,0.803669725,0.805504587,0.80733945,0.809174312,0.811009174,
0.812844037,0.814678899,0.816513761,0.818348624,0.820183486,0.822018349,
0.823853211,0.825688073,0.827522936,0.829357798,0.831192661,0.833027523,
0.834862385,0.836697248,0.83853211,0.840366972,0.842201835,0.844036697,
0.84587156,0.847706422,0.849541284,0.851376147,0.853211009,0.855045872,
0.856880734,0.858715596,0.860550459,0.862385321,0.864220183,0.866055046,
0.867889908,0.869724771,0.871559633,0.873394495,0.875229358,0.87706422,
0.878899083,0.880733945,0.882568807,0.88440367,0.886238532,0.888073394,
0.889908257,0.891743119,0.893577982,0.895412844,0.897247706,0.899082569,
0.900917431,0.902752294,0.904587156,0.906422018,0.908256881,0.910091743,
0.911926606,0.913761468,0.91559633,0.917431193,0.919266055,0.921100917,
0.92293578,0.924770642,0.926605505,0.928440367,0.930275229,0.932110092,
0.933944954,0.935779817,0.937614679,0.939449541,0.941284404,0.943119266,
0.944954128,0.946788991,0.948623853,0.950458716,0.952293578,0.95412844,
0.955963303,0.957798165,0.959633028,0.96146789,0.963302752,0.965137615,
0.966972477,0.968807339,0.970642202,0.972477064,0.974311927,0.976146789,
0.977981651,0.979816514,0.981651376,0.983486239,0.985321101,0.987155963,
0.988990826,0.990825688,0.99266055,0.994495413,0.996330275,0.998165138,
1.),.UNSPECIFIED.);
#24397=B_SPLINE_CURVE_WITH_KNOTS('',3,(#219789,#219790,#219791,#219792,
#219793,#219794,#219795,#219796,#219797,#219798,#219799,#219800,#219801,
#219802,#219803,#219804,#219805,#219806,#219807,#219808,#219809,#219810,
#219811,#219812,#219813,#219814,#219815,#219816,#219817,#219818,#219819,
#219820,#219821,#219822,#219823,#219824,#219825,#219826,#219827,#219828,
#219829,#219830,#219831,#219832,#219833,#219834,#219835,#219836,#219837,
#219838,#219839,#219840,#219841,#219842,#219843,#219844,#219845,#219846,
#219847,#219848,#219849,#219850,#219851,#219852,#219853,#219854,#219855,
#219856,#219857,#219858,#219859,#219860,#219861,#219862,#219863,#219864,
#219865,#219866,#219867,#219868,#219869,#219870,#219871,#219872,#219873,
#219874,#219875,#219876,#219877,#219878,#219879,#219880,#219881,#219882,
#219883,#219884,#219885,#219886,#219887,#219888,#219889,#219890,#219891,
#219892,#219893,#219894,#219895,#219896,#219897,#219898,#219899,#219900,
#219901,#219902,#219903,#219904,#219905,#219906,#219907,#219908,#219909,
#219910,#219911,#219912,#219913,#219914,#219915,#219916,#219917,#219918,
#219919,#219920,#219921,#219922,#219923,#219924,#219925,#219926,#219927,
#219928,#219929,#219930,#219931,#219932,#219933,#219934,#219935,#219936,
#219937,#219938,#219939,#219940,#219941,#219942,#219943,#219944,#219945,
#219946,#219947,#219948,#219949,#219950,#219951,#219952,#219953,#219954,
#219955,#219956,#219957,#219958,#219959,#219960,#219961,#219962,#219963,
#219964,#219965,#219966,#219967,#219968,#219969,#219970,#219971,#219972,
#219973,#219974,#219975,#219976,#219977,#219978,#219979,#219980,#219981,
#219982,#219983,#219984,#219985,#219986,#219987,#219988,#219989,#219990,
#219991,#219992,#219993,#219994,#219995,#219996,#219997,#219998,#219999,
#220000,#220001,#220002,#220003,#220004,#220005,#220006,#220007,#220008,
#220009,#220010,#220011,#220012,#220013,#220014,#220015,#220016,#220017,
#220018,#220019,#220020,#220021,#220022,#220023,#220024,#220025,#220026,
#220027,#220028,#220029,#220030,#220031,#220032,#220033,#220034,#220035,
#220036,#220037,#220038,#220039,#220040,#220041,#220042,#220043,#220044,
#220045,#220046,#220047,#220048,#220049,#220050,#220051,#220052,#220053,
#220054,#220055,#220056,#220057,#220058,#220059,#220060,#220061,#220062,
#220063,#220064,#220065,#220066,#220067,#220068,#220069,#220070,#220071,
#220072,#220073,#220074,#220075,#220076,#220077,#220078,#220079,#220080,
#220081,#220082,#220083,#220084,#220085,#220086,#220087,#220088,#220089),
 .UNSPECIFIED.,.F.,.F.,(4,3,3,3,3,3,3,3,3,3,3,3,3,3,3,3,3,3,3,3,3,3,3,3,
3,3,3,3,3,3,3,3,3,3,3,3,3,3,3,3,3,3,3,3,3,3,3,3,3,3,3,3,3,3,3,3,3,3,3,3,
3,3,3,3,3,3,3,3,3,3,3,3,3,3,3,3,3,3,3,3,3,3,3,3,3,3,3,3,3,3,3,3,3,3,3,3,
3,3,3,3,4),(0.143172102,0.15412844,0.165137615,0.176146789,0.187155963,
0.198165138,0.209174312,0.220183486,0.231192661,0.242201835,0.253211009,
0.264220183,0.275229358,0.286238532,0.297247706,0.308256881,0.319266055,
0.330275229,0.343119266,0.35412844,0.365137615,0.376146789,0.387155963,
0.396330275,0.405504587,0.416513761,0.425688073,0.436697248,0.44587156,
0.455045872,0.464220183,0.473394495,0.48440367,0.499082569,0.511926606,
0.521100917,0.530275229,0.539449541,0.548623853,0.555963303,0.565137615,
0.572477064,0.581651376,0.590825688,0.598165138,0.605504587,0.614678899,
0.622018349,0.629357798,0.63853211,0.647706422,0.655045872,0.667889908,
0.678899083,0.686238532,0.693577982,0.700917431,0.710091743,0.717431193,
0.726605505,0.733944954,0.741284404,0.748623853,0.757798165,0.770642202,
0.779816514,0.79266055,0.8,0.80733945,0.812844037,0.818348624,0.823853211,
0.831192661,0.836697248,0.844036697,0.849541284,0.855045872,0.862385321,
0.867889908,0.873394495,0.878899083,0.88440367,0.889908257,0.895412844,
0.900917431,0.906422018,0.911926606,0.917431193,0.924770642,0.930275229,
0.935779817,0.941284404,0.950458716,0.955963303,0.96146789,0.966972477,
0.972477064,0.979816514,0.985321101,0.994495413,1.),.UNSPECIFIED.);
#24398=B_SPLINE_CURVE_WITH_KNOTS('',3,(#220090,#220091,#220092,#220093,
#220094,#220095,#220096,#220097,#220098,#220099,#220100,#220101,#220102,
#220103,#220104,#220105,#220106,#220107,#220108,#220109,#220110,#220111,
#220112,#220113,#220114,#220115,#220116,#220117,#220118,#220119,#220120,
#220121,#220122,#220123,#220124,#220125,#220126,#220127,#220128,#220129,
#220130,#220131,#220132,#220133,#220134,#220135,#220136,#220137,#220138,
#220139,#220140,#220141,#220142,#220143,#220144,#220145,#220146,#220147,
#220148,#220149,#220150,#220151,#220152,#220153,#220154,#220155,#220156,
#220157,#220158,#220159,#220160,#220161,#220162,#220163,#220164,#220165,
#220166,#220167,#220168,#220169,#220170,#220171,#220172,#220173,#220174,
#220175,#220176,#220177,#220178,#220179,#220180,#220181,#220182,#220183,
#220184,#220185,#220186,#220187,#220188,#220189,#220190,#220191,#220192,
#220193,#220194,#220195,#220196,#220197,#220198,#220199,#220200,#220201,
#220202,#220203,#220204,#220205,#220206,#220207,#220208,#220209,#220210,
#220211,#220212,#220213,#220214,#220215,#220216,#220217,#220218,#220219,
#220220,#220221,#220222,#220223,#220224,#220225,#220226,#220227,#220228,
#220229,#220230,#220231,#220232,#220233,#220234,#220235,#220236,#220237,
#220238,#220239,#220240,#220241,#220242,#220243,#220244,#220245,#220246,
#220247,#220248,#220249,#220250,#220251,#220252,#220253,#220254,#220255,
#220256,#220257,#220258,#220259,#220260,#220261,#220262,#220263,#220264,
#220265,#220266,#220267,#220268,#220269,#220270,#220271,#220272,#220273,
#220274,#220275,#220276,#220277,#220278,#220279,#220280,#220281,#220282,
#220283,#220284,#220285,#220286,#220287,#220288,#220289,#220290,#220291,
#220292,#220293,#220294,#220295,#220296,#220297,#220298,#220299,#220300,
#220301,#220302,#220303,#220304,#220305,#220306,#220307,#220308,#220309,
#220310,#220311,#220312,#220313,#220314,#220315,#220316,#220317,#220318,
#220319,#220320,#220321,#220322,#220323,#220324,#220325,#220326,#220327,
#220328,#220329,#220330,#220331,#220332,#220333,#220334,#220335,#220336,
#220337,#220338,#220339,#220340,#220341,#220342,#220343,#220344,#220345,
#220346,#220347,#220348,#220349,#220350,#220351,#220352,#220353,#220354,
#220355,#220356,#220357,#220358,#220359,#220360,#220361,#220362,#220363,
#220364,#220365,#220366,#220367,#220368,#220369,#220370,#220371,#220372,
#220373,#220374,#220375,#220376,#220377,#220378,#220379,#220380,#220381,
#220382,#220383,#220384,#220385,#220386,#220387,#220388,#220389,#220390,
#220391,#220392,#220393,#220394,#220395,#220396,#220397,#220398,#220399,
#220400,#220401,#220402,#220403,#220404,#220405),.UNSPECIFIED.,.F.,.F.,
(4,3,3,3,3,3,3,3,3,3,3,3,3,3,3,3,3,3,3,3,3,3,3,3,3,3,3,3,3,3,3,3,3,3,3,
3,3,3,3,3,3,3,3,3,3,3,3,3,3,3,3,3,3,3,3,3,3,3,3,3,3,3,3,3,3,3,3,3,3,3,3,
3,3,3,3,3,3,3,3,3,3,3,3,3,3,3,3,3,3,3,3,3,3,3,3,3,3,3,3,3,3,3,3,3,3,4),
(0.143172102,0.15412844,0.165137615,0.176146789,0.187155963,0.198165138,
0.209174312,0.220183486,0.231192661,0.242201835,0.253211009,0.264220183,
0.275229358,0.286238532,0.297247706,0.308256881,0.319266055,0.330275229,
0.341284404,0.352293578,0.363302752,0.374311927,0.385321101,0.396330275,
0.405504587,0.416513761,0.425688073,0.434862385,0.444036697,0.453211009,
0.462385321,0.471559633,0.480733945,0.489908257,0.499082569,0.510091743,
0.519266055,0.528440367,0.535779817,0.543119266,0.550458716,0.557798165,
0.565137615,0.572477064,0.581651376,0.588990826,0.596330275,0.603669725,
0.611009174,0.618348624,0.625688073,0.633027523,0.640366972,0.647706422,
0.655045872,0.662385321,0.669724771,0.67706422,0.68440367,0.691743119,0.700917431,
0.710091743,0.717431193,0.724770642,0.733944954,0.741284404,0.748623853,
0.755963303,0.763302752,0.770642202,0.777981651,0.785321101,0.79266055,
0.8,0.809174312,0.816513761,0.822018349,0.827522936,0.834862385,0.842201835,
0.847706422,0.853211009,0.858715596,0.864220183,0.869724771,0.875229358,
0.880733945,0.888073394,0.893577982,0.900917431,0.906422018,0.911926606,
0.917431193,0.924770642,0.930275229,0.937614679,0.943119266,0.948623853,
0.95412844,0.96146789,0.968807339,0.974311927,0.979816514,0.987155963,0.994495413,
1.),.UNSPECIFIED.);
#24399=B_SPLINE_CURVE_WITH_KNOTS('',3,(#221365,#221366,#221367,#221368,
#221369,#221370,#221371,#221372,#221373,#221374,#221375,#221376,#221377,
#221378,#221379,#221380,#221381,#221382,#221383,#221384,#221385,#221386,
#221387,#221388,#221389,#221390,#221391,#221392,#221393,#221394,#221395,
#221396,#221397,#221398,#221399,#221400,#221401,#221402,#221403,#221404,
#221405,#221406,#221407,#221408,#221409,#221410,#221411,#221412,#221413,
#221414,#221415,#221416,#221417,#221418,#221419,#221420,#221421,#221422,
#221423,#221424,#221425,#221426,#221427,#221428,#221429,#221430,#221431,
#221432,#221433,#221434,#221435,#221436,#221437,#221438,#221439,#221440,
#221441,#221442,#221443,#221444,#221445,#221446,#221447,#221448,#221449,
#221450,#221451,#221452,#221453,#221454,#221455,#221456,#221457,#221458,
#221459,#221460,#221461,#221462,#221463,#221464,#221465,#221466,#221467,
#221468,#221469,#221470,#221471,#221472,#221473,#221474,#221475,#221476,
#221477,#221478,#221479,#221480,#221481,#221482,#221483,#221484,#221485,
#221486,#221487,#221488,#221489,#221490,#221491,#221492,#221493,#221494,
#221495,#221496,#221497,#221498,#221499,#221500,#221501,#221502,#221503,
#221504,#221505,#221506,#221507,#221508,#221509,#221510,#221511,#221512,
#221513,#221514,#221515,#221516,#221517,#221518,#221519,#221520,#221521,
#221522,#221523,#221524,#221525,#221526,#221527,#221528,#221529,#221530,
#221531,#221532,#221533,#221534,#221535,#221536,#221537,#221538,#221539,
#221540,#221541,#221542,#221543,#221544,#221545,#221546,#221547,#221548,
#221549,#221550,#221551,#221552,#221553,#221554,#221555,#221556,#221557,
#221558,#221559,#221560,#221561,#221562,#221563,#221564,#221565,#221566,
#221567,#221568,#221569,#221570,#221571,#221572,#221573,#221574,#221575,
#221576,#221577,#221578,#221579,#221580,#221581,#221582,#221583,#221584,
#221585,#221586,#221587,#221588,#221589,#221590,#221591,#221592,#221593,
#221594,#221595,#221596,#221597,#221598,#221599,#221600,#221601,#221602,
#221603,#221604,#221605,#221606,#221607,#221608,#221609,#221610,#221611,
#221612,#221613,#221614,#221615,#221616,#221617,#221618,#221619,#221620,
#221621,#221622,#221623,#221624,#221625,#221626,#221627,#221628,#221629,
#221630,#221631,#221632,#221633,#221634,#221635,#221636,#221637,#221638,
#221639,#221640,#221641,#221642,#221643,#221644,#221645,#221646,#221647,
#221648,#221649,#221650,#221651,#221652,#221653,#221654,#221655,#221656),
 .UNSPECIFIED.,.F.,.F.,(4,3,3,3,3,3,3,3,3,3,3,3,3,3,3,3,3,3,3,3,3,3,3,3,
3,3,3,3,3,3,3,3,3,3,3,3,3,3,3,3,3,3,3,3,3,3,3,3,3,3,3,3,3,3,3,3,3,3,3,3,
3,3,3,3,3,3,3,3,3,3,3,3,3,3,3,3,3,3,3,3,3,3,3,3,3,3,3,3,3,3,3,3,3,3,3,3,
3,4),(0.143172102,0.15412844,0.165137615,0.176146789,0.187155963,0.198165138,
0.209174312,0.220183486,0.231192661,0.242201835,0.253211009,0.264220183,
0.275229358,0.288073394,0.300917431,0.311926606,0.32293578,0.333944954,
0.344954128,0.357798165,0.368807339,0.379816514,0.39266055,0.401834862,
0.412844037,0.422018349,0.431192661,0.440366972,0.449541284,0.458715596,
0.469724771,0.478899083,0.488073394,0.497247706,0.508256881,0.519266055,
0.530275229,0.537614679,0.550458716,0.56146789,0.572477064,0.581651376,
0.588990826,0.598165138,0.605504587,0.612844037,0.622018349,0.629357798,
0.636697248,0.644036697,0.653211009,0.660550459,0.669724771,0.67706422,
0.68440367,0.691743119,0.699082569,0.706422018,0.71559633,0.72293578,0.730275229,
0.743119266,0.755963303,0.768807339,0.781651376,0.79266055,0.803669725,
0.811009174,0.816513761,0.822018349,0.831192661,0.836697248,0.842201835,
0.847706422,0.855045872,0.860550459,0.866055046,0.873394495,0.878899083,
0.88440367,0.889908257,0.897247706,0.904587156,0.910091743,0.917431193,
0.92293578,0.928440367,0.933944954,0.939449541,0.946788991,0.952293578,
0.96146789,0.966972477,0.972477064,0.979816514,0.985321101,0.990825688,
1.),.UNSPECIFIED.);
#24400=B_SPLINE_CURVE_WITH_KNOTS('',3,(#221657,#221658,#221659,#221660,
#221661,#221662,#221663,#221664,#221665,#221666,#221667,#221668,#221669,
#221670,#221671,#221672,#221673,#221674,#221675,#221676,#221677,#221678,
#221679,#221680,#221681,#221682,#221683,#221684,#221685,#221686,#221687,
#221688,#221689,#221690,#221691,#221692,#221693,#221694,#221695,#221696,
#221697,#221698,#221699,#221700,#221701,#221702,#221703,#221704,#221705,
#221706,#221707,#221708,#221709,#221710,#221711,#221712,#221713,#221714,
#221715,#221716,#221717,#221718,#221719,#221720,#221721,#221722,#221723,
#221724,#221725,#221726,#221727,#221728,#221729,#221730,#221731,#221732,
#221733,#221734,#221735,#221736,#221737,#221738,#221739,#221740,#221741,
#221742,#221743,#221744,#221745,#221746,#221747,#221748,#221749,#221750,
#221751,#221752,#221753,#221754,#221755,#221756,#221757,#221758,#221759,
#221760,#221761,#221762,#221763,#221764,#221765,#221766,#221767,#221768,
#221769,#221770,#221771,#221772,#221773,#221774,#221775,#221776,#221777,
#221778,#221779,#221780,#221781,#221782,#221783,#221784,#221785,#221786,
#221787,#221788,#221789,#221790,#221791,#221792,#221793,#221794,#221795,
#221796,#221797,#221798,#221799,#221800,#221801,#221802,#221803,#221804,
#221805,#221806,#221807,#221808,#221809,#221810,#221811,#221812,#221813,
#221814,#221815,#221816,#221817,#221818,#221819,#221820,#221821,#221822,
#221823,#221824,#221825,#221826,#221827,#221828,#221829,#221830,#221831,
#221832,#221833,#221834,#221835,#221836,#221837,#221838,#221839,#221840,
#221841,#221842,#221843,#221844,#221845,#221846,#221847,#221848,#221849,
#221850,#221851,#221852,#221853,#221854,#221855,#221856,#221857,#221858,
#221859,#221860,#221861,#221862,#221863,#221864,#221865,#221866,#221867,
#221868,#221869,#221870,#221871,#221872,#221873,#221874,#221875,#221876,
#221877,#221878,#221879,#221880,#221881,#221882,#221883,#221884,#221885,
#221886,#221887,#221888,#221889,#221890,#221891,#221892,#221893,#221894,
#221895,#221896,#221897,#221898,#221899,#221900,#221901,#221902,#221903,
#221904,#221905,#221906,#221907,#221908,#221909,#221910,#221911,#221912,
#221913,#221914,#221915,#221916,#221917,#221918,#221919,#221920,#221921,
#221922,#221923,#221924,#221925,#221926,#221927,#221928,#221929,#221930,
#221931,#221932,#221933,#221934,#221935,#221936,#221937,#221938,#221939,
#221940,#221941,#221942,#221943,#221944,#221945,#221946,#221947,#221948,
#221949,#221950,#221951,#221952,#221953,#221954,#221955,#221956,#221957,
#221958,#221959,#221960,#221961,#221962,#221963,#221964,#221965,#221966,
#221967,#221968,#221969,#221970,#221971,#221972,#221973,#221974,#221975),
 .UNSPECIFIED.,.F.,.F.,(4,3,3,3,3,3,3,3,3,3,3,3,3,3,3,3,3,3,3,3,3,3,3,3,
3,3,3,3,3,3,3,3,3,3,3,3,3,3,3,3,3,3,3,3,3,3,3,3,3,3,3,3,3,3,3,3,3,3,3,3,
3,3,3,3,3,3,3,3,3,3,3,3,3,3,3,3,3,3,3,3,3,3,3,3,3,3,3,3,3,3,3,3,3,3,3,3,
3,3,3,3,3,3,3,3,3,3,4),(0.143172102,0.15412844,0.165137615,0.176146789,
0.187155963,0.198165138,0.209174312,0.220183486,0.231192661,0.242201835,
0.253211009,0.264220183,0.275229358,0.288073394,0.300917431,0.311926606,
0.32293578,0.333944954,0.344954128,0.355963303,0.366972477,0.377981651,
0.388990826,0.398165138,0.40733945,0.418348624,0.427522936,0.436697248,
0.44587156,0.456880734,0.466055046,0.475229358,0.488073394,0.497247706,
0.508256881,0.519266055,0.528440367,0.535779817,0.543119266,0.550458716,
0.557798165,0.566972477,0.574311927,0.581651376,0.588990826,0.596330275,
0.603669725,0.611009174,0.618348624,0.625688073,0.633027523,0.640366972,
0.647706422,0.655045872,0.664220183,0.671559633,0.678899083,0.686238532,
0.693577982,0.700917431,0.708256881,0.71559633,0.72293578,0.730275229,0.737614679,
0.744954128,0.752293578,0.759633028,0.768807339,0.776146789,0.783486239,
0.790825688,0.798165138,0.805504587,0.811009174,0.816513761,0.822018349,
0.827522936,0.833027523,0.840366972,0.84587156,0.853211009,0.858715596,
0.864220183,0.869724771,0.875229358,0.882568807,0.888073394,0.893577982,
0.900917431,0.906422018,0.911926606,0.917431193,0.924770642,0.930275229,
0.935779817,0.943119266,0.948623853,0.95412844,0.96146789,0.966972477,0.972477064,
0.977981651,0.983486239,0.988990826,0.994495413,1.),.UNSPECIFIED.);
#24401=B_SPLINE_CURVE_WITH_KNOTS('',3,(#222923,#222924,#222925,#222926,
#222927,#222928,#222929,#222930,#222931,#222932,#222933,#222934,#222935,
#222936,#222937,#222938,#222939,#222940,#222941,#222942,#222943,#222944,
#222945,#222946,#222947,#222948,#222949,#222950,#222951,#222952,#222953,
#222954,#222955,#222956,#222957,#222958,#222959,#222960,#222961,#222962,
#222963,#222964,#222965,#222966,#222967,#222968,#222969,#222970,#222971,
#222972,#222973,#222974,#222975,#222976,#222977,#222978,#222979,#222980,
#222981,#222982,#222983,#222984,#222985,#222986,#222987,#222988,#222989,
#222990,#222991,#222992,#222993,#222994,#222995,#222996,#222997,#222998,
#222999,#223000,#223001,#223002,#223003,#223004,#223005,#223006,#223007,
#223008,#223009,#223010,#223011,#223012,#223013,#223014,#223015,#223016,
#223017,#223018,#223019,#223020,#223021,#223022,#223023,#223024,#223025,
#223026,#223027,#223028,#223029,#223030,#223031,#223032,#223033,#223034,
#223035,#223036,#223037,#223038,#223039,#223040,#223041,#223042,#223043,
#223044,#223045,#223046,#223047,#223048,#223049,#223050,#223051,#223052,
#223053,#223054,#223055,#223056,#223057,#223058,#223059,#223060,#223061,
#223062,#223063,#223064,#223065,#223066,#223067,#223068,#223069,#223070,
#223071,#223072,#223073,#223074,#223075,#223076,#223077,#223078,#223079,
#223080,#223081,#223082,#223083,#223084,#223085,#223086,#223087,#223088,
#223089,#223090,#223091,#223092,#223093,#223094,#223095,#223096,#223097,
#223098,#223099,#223100,#223101,#223102,#223103,#223104,#223105,#223106,
#223107,#223108,#223109,#223110,#223111,#223112,#223113,#223114,#223115,
#223116,#223117,#223118,#223119,#223120,#223121,#223122,#223123,#223124,
#223125,#223126,#223127,#223128,#223129,#223130,#223131,#223132,#223133,
#223134,#223135,#223136,#223137,#223138,#223139,#223140,#223141,#223142,
#223143,#223144,#223145,#223146,#223147,#223148,#223149,#223150,#223151,
#223152,#223153,#223154,#223155,#223156,#223157,#223158,#223159,#223160,
#223161,#223162,#223163,#223164,#223165,#223166,#223167,#223168,#223169,
#223170,#223171,#223172,#223173,#223174,#223175,#223176,#223177,#223178,
#223179,#223180,#223181,#223182,#223183,#223184,#223185,#223186,#223187,
#223188,#223189,#223190,#223191,#223192,#223193,#223194,#223195,#223196,
#223197,#223198,#223199,#223200,#223201,#223202,#223203,#223204,#223205,
#223206,#223207,#223208,#223209,#223210,#223211,#223212,#223213,#223214,
#223215,#223216,#223217,#223218,#223219,#223220,#223221,#223222,#223223,
#223224,#223225,#223226,#223227,#223228,#223229,#223230,#223231,#223232,
#223233,#223234,#223235,#223236,#223237,#223238,#223239,#223240,#223241,
#223242,#223243,#223244,#223245,#223246,#223247),.UNSPECIFIED.,.F.,.F.,
(4,3,3,3,3,3,3,3,3,3,3,3,3,3,3,3,3,3,3,3,3,3,3,3,3,3,3,3,3,3,3,3,3,3,3,
3,3,3,3,3,3,3,3,3,3,3,3,3,3,3,3,3,3,3,3,3,3,3,3,3,3,3,3,3,3,3,3,3,3,3,3,
3,3,3,3,3,3,3,3,3,3,3,3,3,3,3,3,3,3,3,3,3,3,3,3,3,3,3,3,3,3,3,3,3,3,3,3,
3,4),(-1.,-0.99266055,-0.987155963,-0.981651376,-0.976146789,-0.970642202,
-0.965137615,-0.959633028,-0.95412844,-0.948623853,-0.943119266,-0.937614679,
-0.932110092,-0.926605505,-0.921100917,-0.91559633,-0.910091743,-0.904587156,
-0.899082569,-0.893577982,-0.888073394,-0.882568807,-0.87706422,-0.871559633,
-0.866055046,-0.860550459,-0.855045872,-0.849541284,-0.842201835,-0.836697248,
-0.831192661,-0.825688073,-0.818348624,-0.812844037,-0.80733945,-0.8,-0.79266055,
-0.781651376,-0.774311927,-0.766972477,-0.759633028,-0.752293578,-0.744954128,
-0.737614679,-0.730275229,-0.72293578,-0.71559633,-0.708256881,-0.700917431,
-0.693577982,-0.686238532,-0.678899083,-0.671559633,-0.664220183,-0.656880734,
-0.649541284,-0.642201835,-0.634862385,-0.627522936,-0.620183486,-0.612844037,
-0.605504587,-0.598165138,-0.590825688,-0.583486239,-0.576146789,-0.568807339,
-0.56146789,-0.55412844,-0.546788991,-0.539449541,-0.532110092,-0.52293578,
-0.513761468,-0.504587156,-0.495412844,-0.486238532,-0.47706422,-0.467889908,
-0.458715596,-0.449541284,-0.440366972,-0.431192661,-0.422018349,-0.412844037,
-0.403669725,-0.394495413,-0.383486239,-0.372477064,-0.36146789,-0.350458716,
-0.339449541,-0.328440367,-0.317431193,-0.306422018,-0.295412844,-0.28440367,
-0.273394495,-0.262385321,-0.251376147,-0.240366972,-0.229357798,-0.218348624,
-0.20733945,-0.196330275,-0.183486239,-0.172477064,-0.16146789,-0.143172102),
 .UNSPECIFIED.);
#24402=B_SPLINE_CURVE_WITH_KNOTS('',3,(#223248,#223249,#223250,#223251,
#223252,#223253,#223254,#223255,#223256,#223257,#223258,#223259,#223260,
#223261,#223262,#223263,#223264,#223265,#223266,#223267,#223268,#223269,
#223270,#223271,#223272,#223273,#223274,#223275,#223276,#223277,#223278,
#223279,#223280,#223281,#223282,#223283,#223284,#223285,#223286,#223287,
#223288,#223289,#223290,#223291,#223292,#223293,#223294,#223295,#223296,
#223297,#223298,#223299,#223300,#223301,#223302,#223303,#223304,#223305,
#223306,#223307,#223308,#223309,#223310,#223311,#223312,#223313,#223314,
#223315,#223316,#223317,#223318,#223319,#223320,#223321,#223322,#223323,
#223324,#223325,#223326,#223327,#223328,#223329,#223330,#223331,#223332,
#223333,#223334,#223335,#223336,#223337,#223338,#223339,#223340,#223341,
#223342,#223343,#223344,#223345,#223346,#223347,#223348,#223349,#223350,
#223351,#223352,#223353,#223354,#223355,#223356,#223357,#223358,#223359,
#223360,#223361,#223362,#223363,#223364,#223365,#223366,#223367,#223368,
#223369,#223370,#223371,#223372,#223373,#223374,#223375,#223376,#223377,
#223378,#223379,#223380,#223381,#223382,#223383,#223384,#223385,#223386,
#223387,#223388,#223389,#223390,#223391,#223392,#223393,#223394,#223395,
#223396,#223397,#223398,#223399,#223400,#223401,#223402,#223403,#223404,
#223405,#223406,#223407,#223408,#223409,#223410,#223411,#223412,#223413,
#223414,#223415,#223416,#223417,#223418,#223419,#223420,#223421,#223422,
#223423,#223424,#223425,#223426,#223427,#223428,#223429,#223430,#223431,
#223432,#223433,#223434,#223435,#223436,#223437,#223438,#223439,#223440,
#223441,#223442,#223443,#223444,#223445,#223446,#223447,#223448,#223449,
#223450,#223451,#223452,#223453,#223454,#223455,#223456,#223457,#223458,
#223459,#223460,#223461,#223462,#223463,#223464,#223465,#223466,#223467,
#223468,#223469,#223470,#223471,#223472,#223473,#223474,#223475,#223476,
#223477,#223478,#223479,#223480,#223481,#223482,#223483,#223484,#223485,
#223486,#223487,#223488,#223489,#223490,#223491,#223492,#223493,#223494,
#223495,#223496,#223497,#223498,#223499,#223500,#223501,#223502,#223503,
#223504,#223505,#223506,#223507,#223508,#223509,#223510,#223511,#223512,
#223513,#223514,#223515,#223516,#223517,#223518,#223519,#223520,#223521,
#223522,#223523,#223524,#223525,#223526,#223527,#223528,#223529,#223530,
#223531,#223532,#223533,#223534,#223535,#223536,#223537,#223538,#223539,
#223540,#223541,#223542,#223543,#223544,#223545,#223546,#223547,#223548),
 .UNSPECIFIED.,.F.,.F.,(4,3,3,3,3,3,3,3,3,3,3,3,3,3,3,3,3,3,3,3,3,3,3,3,
3,3,3,3,3,3,3,3,3,3,3,3,3,3,3,3,3,3,3,3,3,3,3,3,3,3,3,3,3,3,3,3,3,3,3,3,
3,3,3,3,3,3,3,3,3,3,3,3,3,3,3,3,3,3,3,3,3,3,3,3,3,3,3,3,3,3,3,3,3,3,3,3,
3,3,3,3,4),(0.143172102,0.15412844,0.165137615,0.176146789,0.187155963,
0.198165138,0.209174312,0.220183486,0.231192661,0.242201835,0.255045872,
0.266055046,0.280733945,0.291743119,0.302752294,0.313761468,0.326605505,
0.337614679,0.348623853,0.359633028,0.370642202,0.381651376,0.39266055,
0.401834862,0.411009174,0.420183486,0.429357798,0.440366972,0.449541284,
0.458715596,0.467889908,0.47706422,0.488073394,0.497247706,0.506422018,
0.51559633,0.526605505,0.533944954,0.541284404,0.548623853,0.555963303,
0.565137615,0.572477064,0.579816514,0.588990826,0.596330275,0.603669725,
0.616513761,0.625688073,0.633027523,0.640366972,0.649541284,0.658715596,
0.667889908,0.67706422,0.68440367,0.691743119,0.702752294,0.710091743,0.719266055,
0.726605505,0.735779817,0.743119266,0.750458716,0.757798165,0.766972477,
0.776146789,0.787155963,0.794495413,0.803669725,0.811009174,0.816513761,
0.823853211,0.829357798,0.834862385,0.840366972,0.847706422,0.853211009,
0.858715596,0.864220183,0.869724771,0.875229358,0.880733945,0.888073394,
0.893577982,0.902752294,0.908256881,0.913761468,0.921100917,0.928440367,
0.933944954,0.941284404,0.950458716,0.955963303,0.96146789,0.968807339,
0.974311927,0.979816514,0.985321101,0.990825688,1.),.UNSPECIFIED.);
#24403=B_SPLINE_CURVE_WITH_KNOTS('',5,(#224511,#224512,#224513,#224514,
#224515,#224516,#224517,#224518,#224519,#224520,#224521,#224522,#224523,
#224524,#224525,#224526,#224527,#224528,#224529,#224530,#224531,#224532,
#224533,#224534,#224535,#224536,#224537,#224538,#224539,#224540,#224541,
#224542,#224543,#224544,#224545,#224546,#224547,#224548,#224549,#224550,
#224551,#224552,#224553,#224554,#224555,#224556,#224557,#224558,#224559,
#224560,#224561,#224562,#224563,#224564,#224565,#224566,#224567,#224568,
#224569,#224570,#224571,#224572,#224573,#224574,#224575,#224576,#224577,
#224578,#224579,#224580,#224581,#224582,#224583,#224584,#224585,#224586,
#224587,#224588,#224589,#224590,#224591,#224592,#224593,#224594,#224595,
#224596,#224597,#224598,#224599,#224600,#224601,#224602,#224603,#224604,
#224605,#224606,#224607,#224608,#224609,#224610,#224611,#224612,#224613,
#224614,#224615,#224616,#224617,#224618,#224619,#224620,#224621,#224622,
#224623,#224624,#224625,#224626,#224627,#224628,#224629,#224630,#224631,
#224632,#224633,#224634,#224635,#224636,#224637,#224638,#224639,#224640,
#224641,#224642,#224643,#224644,#224645,#224646,#224647,#224648,#224649,
#224650,#224651,#224652,#224653,#224654,#224655,#224656,#224657,#224658,
#224659,#224660,#224661,#224662,#224663,#224664,#224665,#224666,#224667,
#224668,#224669,#224670,#224671,#224672,#224673,#224674,#224675,#224676,
#224677,#224678,#224679,#224680,#224681,#224682,#224683,#224684,#224685,
#224686,#224687,#224688,#224689,#224690,#224691,#224692,#224693,#224694,
#224695,#224696,#224697,#224698,#224699,#224700,#224701,#224702,#224703,
#224704,#224705,#224706,#224707,#224708,#224709,#224710,#224711,#224712,
#224713,#224714,#224715,#224716,#224717,#224718,#224719,#224720,#224721,
#224722,#224723,#224724,#224725,#224726,#224727,#224728,#224729,#224730,
#224731,#224732,#224733,#224734,#224735,#224736,#224737,#224738,#224739,
#224740,#224741,#224742,#224743,#224744,#224745,#224746,#224747,#224748,
#224749,#224750,#224751,#224752,#224753,#224754,#224755,#224756,#224757,
#224758,#224759,#224760,#224761,#224762,#224763,#224764,#224765,#224766,
#224767,#224768,#224769,#224770,#224771,#224772,#224773,#224774,#224775,
#224776,#224777,#224778,#224779,#224780,#224781,#224782,#224783,#224784,
#224785,#224786,#224787,#224788,#224789,#224790,#224791,#224792,#224793,
#224794,#224795,#224796,#224797,#224798,#224799,#224800,#224801,#224802,
#224803,#224804,#224805,#224806,#224807,#224808,#224809,#224810,#224811,
#224812,#224813,#224814,#224815,#224816,#224817,#224818,#224819,#224820,
#224821,#224822,#224823,#224824,#224825,#224826,#224827,#224828,#224829,
#224830,#224831,#224832,#224833,#224834,#224835,#224836,#224837,#224838,
#224839,#224840,#224841,#224842,#224843,#224844,#224845,#224846,#224847,
#224848,#224849,#224850,#224851,#224852,#224853,#224854,#224855,#224856,
#224857,#224858,#224859,#224860,#224861,#224862,#224863,#224864,#224865,
#224866,#224867,#224868,#224869,#224870,#224871,#224872,#224873,#224874,
#224875,#224876,#224877,#224878,#224879,#224880,#224881,#224882,#224883,
#224884,#224885,#224886,#224887,#224888,#224889,#224890,#224891,#224892,
#224893,#224894,#224895,#224896,#224897,#224898,#224899,#224900,#224901,
#224902,#224903,#224904,#224905,#224906,#224907,#224908,#224909,#224910,
#224911,#224912,#224913,#224914,#224915,#224916,#224917,#224918,#224919,
#224920,#224921,#224922,#224923,#224924,#224925,#224926,#224927,#224928,
#224929,#224930,#224931,#224932,#224933,#224934,#224935,#224936,#224937,
#224938,#224939,#224940,#224941,#224942,#224943,#224944,#224945,#224946,
#224947,#224948,#224949,#224950,#224951,#224952,#224953,#224954,#224955,
#224956,#224957,#224958,#224959,#224960,#224961,#224962,#224963,#224964,
#224965,#224966,#224967,#224968,#224969,#224970,#224971,#224972,#224973,
#224974,#224975,#224976,#224977,#224978,#224979,#224980,#224981),
 .UNSPECIFIED.,.F.,.F.,(6,1,1,1,1,1,1,1,1,1,1,1,1,1,1,1,1,1,1,1,1,1,1,1,
1,1,1,1,1,1,1,1,1,1,1,1,1,1,1,1,1,1,1,1,1,1,1,1,1,1,1,1,1,1,1,1,1,1,1,1,
1,1,1,1,1,1,1,1,1,1,1,1,1,1,1,1,1,1,1,1,1,1,1,1,1,1,1,1,1,1,1,1,1,1,1,1,
1,1,1,1,1,1,1,1,1,1,1,1,1,1,1,1,1,1,1,1,1,1,1,1,1,1,1,1,1,1,1,1,1,1,1,1,
1,1,1,1,1,1,1,1,1,1,1,1,1,1,1,1,1,1,1,1,1,1,1,1,1,1,1,1,1,1,1,1,1,1,1,1,
1,1,1,1,1,1,1,1,1,1,1,1,1,1,1,1,1,1,1,1,1,1,1,1,1,1,1,1,1,1,1,1,1,1,1,1,
1,1,1,1,1,1,1,1,1,1,1,1,1,1,1,1,1,1,1,1,1,1,1,1,1,1,1,1,1,1,1,1,1,1,1,1,
1,1,1,1,1,1,1,1,1,1,1,1,1,1,1,1,1,1,1,1,1,1,1,1,1,1,1,1,1,1,1,1,1,1,1,1,
1,1,1,1,1,1,1,1,1,1,1,1,1,1,1,1,1,1,1,1,1,1,1,1,1,1,1,1,1,1,1,1,1,1,1,1,
1,1,1,1,1,1,1,1,1,1,1,1,1,1,1,1,1,1,1,1,1,1,1,1,1,1,1,1,1,1,1,1,1,1,1,1,
1,1,1,1,1,1,1,1,1,1,1,1,1,1,1,1,1,1,1,1,1,1,1,1,1,1,1,1,1,1,1,1,1,1,1,1,
1,1,1,1,1,1,1,1,1,1,1,1,1,1,1,1,1,1,1,1,1,1,1,1,1,1,1,1,1,1,1,1,1,1,1,1,
1,1,1,1,1,1,1,1,1,1,1,1,1,1,1,1,1,1,1,1,1,1,1,1,1,1,1,1,1,1,1,1,1,1,1,1,
1,1,1,1,1,1,1,1,1,1,6),(-1.,-0.998165138,-0.996330275,-0.994495413,-0.99266055,
-0.990825688,-0.988990826,-0.987155963,-0.985321101,-0.983486239,-0.981651376,
-0.979816514,-0.977981651,-0.976146789,-0.974311927,-0.972477064,-0.970642202,
-0.968807339,-0.966972477,-0.965137615,-0.963302752,-0.96146789,-0.959633028,
-0.957798165,-0.955963303,-0.95412844,-0.952293578,-0.950458716,-0.948623853,
-0.946788991,-0.944954128,-0.943119266,-0.941284404,-0.939449541,-0.937614679,
-0.935779817,-0.933944954,-0.932110092,-0.930275229,-0.928440367,-0.926605505,
-0.924770642,-0.92293578,-0.921100917,-0.919266055,-0.917431193,-0.91559633,
-0.913761468,-0.911926606,-0.910091743,-0.908256881,-0.906422018,-0.904587156,
-0.902752294,-0.900917431,-0.899082569,-0.897247706,-0.895412844,-0.893577982,
-0.891743119,-0.889908257,-0.888073394,-0.886238532,-0.88440367,-0.882568807,
-0.880733945,-0.878899083,-0.87706422,-0.875229358,-0.873394495,-0.869724771,
-0.867889908,-0.866055046,-0.864220183,-0.862385321,-0.860550459,-0.858715596,
-0.856880734,-0.855045872,-0.853211009,-0.851376147,-0.849541284,-0.847706422,
-0.84587156,-0.844036697,-0.842201835,-0.840366972,-0.83853211,-0.836697248,
-0.834862385,-0.833027523,-0.831192661,-0.829357798,-0.827522936,-0.825688073,
-0.823853211,-0.822018349,-0.820183486,-0.818348624,-0.816513761,-0.814678899,
-0.812844037,-0.811009174,-0.809174312,-0.80733945,-0.805504587,-0.803669725,
-0.801834862,-0.8,-0.798165138,-0.796330275,-0.794495413,-0.79266055,-0.790825688,
-0.788990826,-0.787155963,-0.785321101,-0.783486239,-0.781651376,-0.779816514,
-0.777981651,-0.776146789,-0.774311927,-0.772477064,-0.770642202,-0.768807339,
-0.766972477,-0.765137615,-0.763302752,-0.76146789,-0.759633028,-0.757798165,
-0.755963303,-0.75412844,-0.752293578,-0.750458716,-0.748623853,-0.746788991,
-0.744954128,-0.743119266,-0.741284404,-0.739449541,-0.737614679,-0.735779817,
-0.733944954,-0.732110092,-0.730275229,-0.728440367,-0.726605505,-0.724770642,
-0.72293578,-0.721100917,-0.719266055,-0.717431193,-0.71559633,-0.713761468,
-0.711926606,-0.710091743,-0.708256881,-0.706422018,-0.704587156,-0.702752294,
-0.700917431,-0.699082569,-0.697247706,-0.695412844,-0.693577982,-0.691743119,
-0.689908257,-0.688073394,-0.686238532,-0.68440367,-0.682568807,-0.680733945,
-0.678899083,-0.67706422,-0.675229358,-0.673394495,-0.671559633,-0.669724771,
-0.667889908,-0.666055046,-0.664220183,-0.662385321,-0.660550459,-0.658715596,
-0.656880734,-0.655045872,-0.653211009,-0.651376147,-0.649541284,-0.647706422,
-0.64587156,-0.644036697,-0.642201835,-0.640366972,-0.63853211,-0.636697248,
-0.634862385,-0.633027523,-0.631192661,-0.629357798,-0.627522936,-0.625688073,
-0.623853211,-0.622018349,-0.620183486,-0.618348624,-0.616513761,-0.614678899,
-0.612844037,-0.611009174,-0.609174312,-0.60733945,-0.605504587,-0.603669725,
-0.601834862,-0.6,-0.598165138,-0.596330275,-0.594495413,-0.59266055,-0.590825688,
-0.588990826,-0.587155963,-0.585321101,-0.583486239,-0.581651376,-0.579816514,
-0.577981651,-0.576146789,-0.574311927,-0.572477064,-0.570642202,-0.568807339,
-0.566972477,-0.565137615,-0.563302752,-0.56146789,-0.559633028,-0.557798165,
-0.555963303,-0.55412844,-0.552293578,-0.550458716,-0.548623853,-0.546788991,
-0.544954128,-0.543119266,-0.541284404,-0.539449541,-0.537614679,-0.535779817,
-0.533944954,-0.532110092,-0.530275229,-0.528440367,-0.526605505,-0.524770642,
-0.52293578,-0.521100917,-0.519266055,-0.517431193,-0.51559633,-0.513761468,
-0.511926606,-0.510091743,-0.508256881,-0.506422018,-0.504587156,-0.502752294,
-0.500917431,-0.499082569,-0.497247706,-0.495412844,-0.493577982,-0.491743119,
-0.489908257,-0.488073394,-0.486238532,-0.48440367,-0.482568807,-0.480733945,
-0.478899083,-0.47706422,-0.475229358,-0.473394495,-0.471559633,-0.469724771,
-0.467889908,-0.466055046,-0.464220183,-0.462385321,-0.460550459,-0.458715596,
-0.456880734,-0.455045872,-0.453211009,-0.451376147,-0.449541284,-0.447706422,
-0.44587156,-0.444036697,-0.442201835,-0.440366972,-0.43853211,-0.436697248,
-0.434862385,-0.433027523,-0.431192661,-0.429357798,-0.427522936,-0.425688073,
-0.423853211,-0.422018349,-0.420183486,-0.418348624,-0.416513761,-0.414678899,
-0.412844037,-0.411009174,-0.409174312,-0.40733945,-0.405504587,-0.403669725,
-0.401834862,-0.4,-0.398165138,-0.396330275,-0.394495413,-0.39266055,-0.390825688,
-0.388990826,-0.387155963,-0.385321101,-0.383486239,-0.381651376,-0.379816514,
-0.377981651,-0.376146789,-0.374311927,-0.372477064,-0.370642202,-0.368807339,
-0.366972477,-0.365137615,-0.363302752,-0.36146789,-0.359633028,-0.357798165,
-0.355963303,-0.35412844,-0.352293578,-0.350458716,-0.348623853,-0.346788991,
-0.344954128,-0.343119266,-0.341284404,-0.339449541,-0.337614679,-0.335779817,
-0.333944954,-0.332110092,-0.330275229,-0.328440367,-0.326605505,-0.324770642,
-0.32293578,-0.321100917,-0.319266055,-0.317431193,-0.31559633,-0.313761468,
-0.311926606,-0.310091743,-0.308256881,-0.306422018,-0.304587156,-0.302752294,
-0.300917431,-0.299082569,-0.297247706,-0.295412844,-0.293577982,-0.291743119,
-0.289908257,-0.288073394,-0.286238532,-0.28440367,-0.282568807,-0.280733945,
-0.278899083,-0.27706422,-0.275229358,-0.273394495,-0.271559633,-0.269724771,
-0.267889908,-0.266055046,-0.264220183,-0.262385321,-0.260550459,-0.258715596,
-0.256880734,-0.255045872,-0.253211009,-0.251376147,-0.249541284,-0.247706422,
-0.24587156,-0.244036697,-0.242201835,-0.240366972,-0.23853211,-0.236697248,
-0.234862385,-0.233027523,-0.231192661,-0.229357798,-0.227522936,-0.225688073,
-0.223853211,-0.222018349,-0.220183486,-0.218348624,-0.216513761,-0.214678899,
-0.212844037,-0.211009174,-0.209174312,-0.20733945,-0.205504587,-0.203669725,
-0.201834862,-0.2,-0.198165138,-0.196330275,-0.194495413,-0.19266055,-0.190825688,
-0.188990826,-0.187155963,-0.185321101,-0.183486239,-0.181651376,-0.179816514,
-0.177981651,-0.176146789,-0.174311927,-0.172477064,-0.170642202,-0.168807339,
-0.166972477,-0.165137615,-0.163302752,-0.16146789,-0.159633028,-0.157798165,
-0.155963303,-0.15412844,-0.152293578,-0.150458716,-0.148623853,-0.146788991,
-0.144954128,-0.143172102),.UNSPECIFIED.);
#24404=B_SPLINE_CURVE_WITH_KNOTS('',5,(#224982,#224983,#224984,#224985,
#224986,#224987,#224988,#224989,#224990,#224991,#224992,#224993,#224994,
#224995,#224996,#224997,#224998,#224999,#225000,#225001,#225002,#225003,
#225004,#225005,#225006,#225007,#225008,#225009,#225010,#225011,#225012,
#225013,#225014,#225015,#225016,#225017,#225018,#225019,#225020,#225021,
#225022,#225023,#225024,#225025,#225026,#225027,#225028,#225029,#225030,
#225031,#225032,#225033,#225034,#225035,#225036,#225037,#225038,#225039,
#225040,#225041,#225042,#225043,#225044,#225045,#225046,#225047,#225048,
#225049,#225050,#225051,#225052,#225053,#225054,#225055,#225056,#225057,
#225058,#225059,#225060,#225061,#225062,#225063,#225064,#225065,#225066,
#225067,#225068,#225069,#225070,#225071,#225072,#225073,#225074,#225075,
#225076,#225077,#225078,#225079,#225080,#225081,#225082,#225083,#225084,
#225085,#225086,#225087,#225088,#225089,#225090,#225091,#225092,#225093,
#225094,#225095,#225096,#225097,#225098,#225099,#225100,#225101,#225102,
#225103,#225104,#225105,#225106,#225107,#225108,#225109,#225110,#225111,
#225112,#225113,#225114,#225115,#225116,#225117,#225118,#225119,#225120,
#225121,#225122,#225123,#225124,#225125,#225126,#225127,#225128,#225129,
#225130,#225131,#225132,#225133,#225134,#225135,#225136,#225137,#225138,
#225139,#225140,#225141,#225142,#225143,#225144,#225145,#225146,#225147,
#225148,#225149,#225150,#225151,#225152,#225153,#225154,#225155,#225156,
#225157,#225158,#225159,#225160,#225161,#225162,#225163,#225164,#225165,
#225166,#225167,#225168,#225169,#225170,#225171,#225172,#225173,#225174,
#225175,#225176,#225177,#225178,#225179,#225180,#225181,#225182,#225183,
#225184,#225185,#225186,#225187,#225188,#225189,#225190,#225191,#225192,
#225193,#225194,#225195,#225196,#225197,#225198,#225199,#225200,#225201,
#225202,#225203,#225204,#225205,#225206,#225207,#225208,#225209,#225210,
#225211,#225212,#225213,#225214,#225215,#225216,#225217,#225218,#225219,
#225220,#225221,#225222,#225223,#225224,#225225,#225226,#225227,#225228,
#225229,#225230,#225231,#225232,#225233,#225234,#225235,#225236,#225237,
#225238,#225239,#225240,#225241,#225242,#225243,#225244,#225245,#225246,
#225247,#225248,#225249,#225250,#225251,#225252,#225253,#225254,#225255,
#225256,#225257,#225258,#225259,#225260,#225261,#225262,#225263,#225264,
#225265,#225266,#225267,#225268,#225269,#225270,#225271,#225272,#225273,
#225274,#225275,#225276,#225277,#225278,#225279,#225280,#225281,#225282,
#225283,#225284,#225285,#225286,#225287,#225288,#225289,#225290,#225291,
#225292,#225293,#225294,#225295,#225296,#225297,#225298,#225299,#225300,
#225301,#225302,#225303,#225304,#225305,#225306,#225307,#225308,#225309,
#225310,#225311,#225312,#225313,#225314,#225315,#225316,#225317,#225318,
#225319,#225320,#225321,#225322,#225323,#225324,#225325,#225326,#225327,
#225328,#225329,#225330,#225331,#225332,#225333,#225334,#225335,#225336,
#225337,#225338,#225339,#225340,#225341,#225342,#225343,#225344,#225345,
#225346,#225347,#225348,#225349,#225350,#225351,#225352,#225353,#225354,
#225355,#225356,#225357,#225358,#225359,#225360,#225361,#225362,#225363,
#225364,#225365,#225366,#225367,#225368,#225369,#225370,#225371,#225372,
#225373,#225374,#225375,#225376,#225377,#225378,#225379,#225380,#225381,
#225382,#225383,#225384,#225385,#225386,#225387,#225388,#225389,#225390,
#225391,#225392,#225393,#225394,#225395,#225396,#225397,#225398,#225399,
#225400,#225401,#225402,#225403,#225404,#225405,#225406,#225407,#225408,
#225409,#225410,#225411,#225412,#225413,#225414,#225415,#225416,#225417,
#225418,#225419,#225420,#225421,#225422,#225423,#225424,#225425,#225426,
#225427,#225428,#225429,#225430,#225431,#225432,#225433,#225434,#225435,
#225436,#225437,#225438,#225439,#225440,#225441,#225442,#225443,#225444,
#225445,#225446,#225447,#225448,#225449,#225450,#225451,#225452),
 .UNSPECIFIED.,.F.,.F.,(6,1,1,1,1,1,1,1,1,1,1,1,1,1,1,1,1,1,1,1,1,1,1,1,
1,1,1,1,1,1,1,1,1,1,1,1,1,1,1,1,1,1,1,1,1,1,1,1,1,1,1,1,1,1,1,1,1,1,1,1,
1,1,1,1,1,1,1,1,1,1,1,1,1,1,1,1,1,1,1,1,1,1,1,1,1,1,1,1,1,1,1,1,1,1,1,1,
1,1,1,1,1,1,1,1,1,1,1,1,1,1,1,1,1,1,1,1,1,1,1,1,1,1,1,1,1,1,1,1,1,1,1,1,
1,1,1,1,1,1,1,1,1,1,1,1,1,1,1,1,1,1,1,1,1,1,1,1,1,1,1,1,1,1,1,1,1,1,1,1,
1,1,1,1,1,1,1,1,1,1,1,1,1,1,1,1,1,1,1,1,1,1,1,1,1,1,1,1,1,1,1,1,1,1,1,1,
1,1,1,1,1,1,1,1,1,1,1,1,1,1,1,1,1,1,1,1,1,1,1,1,1,1,1,1,1,1,1,1,1,1,1,1,
1,1,1,1,1,1,1,1,1,1,1,1,1,1,1,1,1,1,1,1,1,1,1,1,1,1,1,1,1,1,1,1,1,1,1,1,
1,1,1,1,1,1,1,1,1,1,1,1,1,1,1,1,1,1,1,1,1,1,1,1,1,1,1,1,1,1,1,1,1,1,1,1,
1,1,1,1,1,1,1,1,1,1,1,1,1,1,1,1,1,1,1,1,1,1,1,1,1,1,1,1,1,1,1,1,1,1,1,1,
1,1,1,1,1,1,1,1,1,1,1,1,1,1,1,1,1,1,1,1,1,1,1,1,1,1,1,1,1,1,1,1,1,1,1,1,
1,1,1,1,1,1,1,1,1,1,1,1,1,1,1,1,1,1,1,1,1,1,1,1,1,1,1,1,1,1,1,1,1,1,1,1,
1,1,1,1,1,1,1,1,1,1,1,1,1,1,1,1,1,1,1,1,1,1,1,1,1,1,1,1,1,1,1,1,1,1,1,1,
1,1,1,1,1,1,1,1,1,1,6),(0.143172102,0.144954128,0.146788991,0.148623853,
0.150458716,0.152293578,0.15412844,0.155963303,0.157798165,0.159633028,
0.16146789,0.163302752,0.165137615,0.166972477,0.168807339,0.170642202,
0.172477064,0.174311927,0.176146789,0.177981651,0.179816514,0.181651376,
0.183486239,0.185321101,0.187155963,0.188990826,0.190825688,0.19266055,
0.194495413,0.196330275,0.198165138,0.2,0.201834862,0.203669725,0.205504587,
0.20733945,0.209174312,0.211009174,0.212844037,0.214678899,0.216513761,
0.218348624,0.220183486,0.222018349,0.223853211,0.225688073,0.227522936,
0.229357798,0.231192661,0.233027523,0.234862385,0.236697248,0.23853211,
0.240366972,0.242201835,0.244036697,0.24587156,0.247706422,0.249541284,
0.251376147,0.253211009,0.255045872,0.256880734,0.258715596,0.260550459,
0.262385321,0.264220183,0.266055046,0.267889908,0.269724771,0.271559633,
0.273394495,0.275229358,0.27706422,0.278899083,0.280733945,0.282568807,
0.28440367,0.286238532,0.288073394,0.289908257,0.291743119,0.293577982,
0.295412844,0.297247706,0.299082569,0.300917431,0.302752294,0.304587156,
0.306422018,0.308256881,0.310091743,0.311926606,0.313761468,0.31559633,
0.317431193,0.319266055,0.321100917,0.32293578,0.324770642,0.326605505,
0.328440367,0.330275229,0.332110092,0.333944954,0.335779817,0.337614679,
0.339449541,0.341284404,0.343119266,0.344954128,0.346788991,0.348623853,
0.350458716,0.352293578,0.35412844,0.355963303,0.357798165,0.359633028,
0.36146789,0.363302752,0.365137615,0.366972477,0.368807339,0.370642202,
0.372477064,0.374311927,0.376146789,0.377981651,0.379816514,0.381651376,
0.383486239,0.385321101,0.387155963,0.388990826,0.390825688,0.39266055,
0.394495413,0.396330275,0.398165138,0.4,0.401834862,0.403669725,0.405504587,
0.40733945,0.409174312,0.411009174,0.412844037,0.414678899,0.416513761,
0.418348624,0.420183486,0.422018349,0.423853211,0.425688073,0.427522936,
0.429357798,0.431192661,0.433027523,0.434862385,0.436697248,0.43853211,
0.440366972,0.442201835,0.444036697,0.44587156,0.447706422,0.449541284,
0.451376147,0.453211009,0.455045872,0.456880734,0.458715596,0.460550459,
0.462385321,0.464220183,0.466055046,0.467889908,0.469724771,0.471559633,
0.473394495,0.475229358,0.47706422,0.478899083,0.480733945,0.482568807,
0.48440367,0.486238532,0.488073394,0.489908257,0.491743119,0.493577982,
0.495412844,0.497247706,0.499082569,0.500917431,0.502752294,0.504587156,
0.506422018,0.508256881,0.510091743,0.511926606,0.513761468,0.51559633,
0.517431193,0.519266055,0.521100917,0.52293578,0.524770642,0.526605505,
0.528440367,0.530275229,0.532110092,0.533944954,0.535779817,0.537614679,
0.539449541,0.541284404,0.543119266,0.544954128,0.546788991,0.548623853,
0.550458716,0.552293578,0.55412844,0.555963303,0.557798165,0.559633028,
0.56146789,0.563302752,0.565137615,0.566972477,0.568807339,0.570642202,
0.572477064,0.574311927,0.576146789,0.577981651,0.579816514,0.581651376,
0.583486239,0.585321101,0.587155963,0.588990826,0.590825688,0.59266055,
0.594495413,0.596330275,0.598165138,0.6,0.601834862,0.603669725,0.605504587,
0.60733945,0.609174312,0.611009174,0.612844037,0.614678899,0.616513761,
0.618348624,0.620183486,0.622018349,0.623853211,0.625688073,0.627522936,
0.629357798,0.631192661,0.633027523,0.634862385,0.636697248,0.63853211,
0.640366972,0.642201835,0.644036697,0.64587156,0.647706422,0.649541284,
0.651376147,0.653211009,0.655045872,0.656880734,0.658715596,0.660550459,
0.662385321,0.664220183,0.666055046,0.667889908,0.669724771,0.671559633,
0.673394495,0.675229358,0.67706422,0.678899083,0.680733945,0.682568807,
0.68440367,0.686238532,0.688073394,0.689908257,0.691743119,0.693577982,
0.695412844,0.697247706,0.699082569,0.700917431,0.702752294,0.704587156,
0.706422018,0.708256881,0.710091743,0.711926606,0.713761468,0.71559633,
0.717431193,0.719266055,0.721100917,0.72293578,0.724770642,0.726605505,
0.728440367,0.730275229,0.732110092,0.733944954,0.735779817,0.737614679,
0.739449541,0.741284404,0.743119266,0.744954128,0.746788991,0.748623853,
0.750458716,0.752293578,0.75412844,0.755963303,0.757798165,0.759633028,
0.76146789,0.763302752,0.765137615,0.766972477,0.768807339,0.770642202,
0.772477064,0.774311927,0.776146789,0.777981651,0.779816514,0.781651376,
0.783486239,0.785321101,0.787155963,0.788990826,0.790825688,0.79266055,
0.794495413,0.796330275,0.798165138,0.8,0.801834862,0.803669725,0.805504587,
0.80733945,0.809174312,0.811009174,0.812844037,0.814678899,0.816513761,
0.818348624,0.820183486,0.822018349,0.823853211,0.825688073,0.827522936,
0.829357798,0.831192661,0.833027523,0.834862385,0.836697248,0.83853211,
0.840366972,0.842201835,0.844036697,0.84587156,0.847706422,0.849541284,
0.851376147,0.853211009,0.855045872,0.856880734,0.858715596,0.860550459,
0.862385321,0.864220183,0.866055046,0.867889908,0.869724771,0.873394495,
0.875229358,0.87706422,0.878899083,0.880733945,0.882568807,0.88440367,0.886238532,
0.888073394,0.889908257,0.891743119,0.893577982,0.895412844,0.897247706,
0.899082569,0.900917431,0.902752294,0.904587156,0.906422018,0.908256881,
0.910091743,0.911926606,0.913761468,0.91559633,0.917431193,0.919266055,
0.921100917,0.92293578,0.924770642,0.926605505,0.928440367,0.930275229,
0.932110092,0.933944954,0.935779817,0.937614679,0.939449541,0.941284404,
0.943119266,0.944954128,0.946788991,0.948623853,0.950458716,0.952293578,
0.95412844,0.955963303,0.957798165,0.959633028,0.96146789,0.963302752,0.965137615,
0.966972477,0.968807339,0.970642202,0.972477064,0.974311927,0.976146789,
0.977981651,0.979816514,0.981651376,0.983486239,0.985321101,0.987155963,
0.988990826,0.990825688,0.99266055,0.994495413,0.996330275,0.998165138,
1.),.UNSPECIFIED.);
#24405=B_SPLINE_CURVE_WITH_KNOTS('',3,(#226397,#226398,#226399,#226400,
#226401,#226402,#226403,#226404,#226405,#226406,#226407,#226408,#226409,
#226410,#226411,#226412,#226413,#226414,#226415,#226416,#226417,#226418,
#226419,#226420,#226421,#226422,#226423,#226424,#226425,#226426,#226427,
#226428,#226429,#226430,#226431,#226432,#226433,#226434,#226435,#226436,
#226437,#226438,#226439,#226440,#226441,#226442,#226443,#226444,#226445,
#226446,#226447,#226448,#226449,#226450,#226451,#226452,#226453,#226454,
#226455,#226456,#226457,#226458,#226459,#226460,#226461,#226462,#226463,
#226464,#226465,#226466,#226467,#226468,#226469,#226470,#226471,#226472,
#226473,#226474,#226475,#226476,#226477,#226478,#226479,#226480,#226481,
#226482,#226483,#226484,#226485,#226486,#226487,#226488,#226489,#226490,
#226491,#226492,#226493,#226494,#226495,#226496,#226497,#226498,#226499,
#226500,#226501,#226502,#226503,#226504,#226505,#226506,#226507,#226508,
#226509,#226510,#226511,#226512,#226513,#226514,#226515,#226516,#226517,
#226518,#226519,#226520,#226521,#226522,#226523,#226524,#226525,#226526,
#226527,#226528,#226529,#226530,#226531,#226532,#226533,#226534,#226535,
#226536,#226537,#226538,#226539,#226540,#226541,#226542,#226543,#226544,
#226545,#226546,#226547,#226548,#226549,#226550,#226551,#226552,#226553,
#226554,#226555,#226556,#226557,#226558,#226559,#226560,#226561,#226562,
#226563,#226564,#226565,#226566,#226567,#226568,#226569,#226570,#226571,
#226572,#226573,#226574,#226575,#226576,#226577,#226578,#226579,#226580,
#226581,#226582,#226583,#226584,#226585,#226586,#226587,#226588,#226589,
#226590,#226591,#226592,#226593,#226594,#226595,#226596,#226597,#226598,
#226599,#226600,#226601,#226602,#226603,#226604,#226605,#226606,#226607,
#226608,#226609,#226610,#226611,#226612,#226613,#226614,#226615,#226616,
#226617,#226618,#226619,#226620,#226621,#226622,#226623,#226624,#226625,
#226626,#226627,#226628,#226629,#226630,#226631,#226632,#226633,#226634,
#226635,#226636,#226637,#226638,#226639,#226640,#226641,#226642,#226643,
#226644,#226645,#226646,#226647,#226648,#226649,#226650,#226651,#226652,
#226653,#226654,#226655,#226656,#226657,#226658,#226659,#226660,#226661,
#226662,#226663,#226664,#226665,#226666,#226667,#226668,#226669,#226670,
#226671,#226672,#226673,#226674,#226675,#226676),.UNSPECIFIED.,.F.,.F.,
(4,3,3,3,3,3,3,3,3,3,3,3,3,3,3,3,3,3,3,3,3,3,3,3,3,3,3,3,3,3,3,3,3,3,3,
3,3,3,3,3,3,3,3,3,3,3,3,3,3,3,3,3,3,3,3,3,3,3,3,3,3,3,3,3,3,3,3,3,3,3,3,
3,3,3,3,3,3,3,3,3,3,3,3,3,3,3,3,3,3,3,3,3,3,4),(0.143172102,0.15412844,
0.165137615,0.181651376,0.19266055,0.203669725,0.214678899,0.231192661,
0.242201835,0.253211009,0.266055046,0.27706422,0.291743119,0.302752294,
0.32293578,0.335779817,0.346788991,0.359633028,0.370642202,0.383486239,
0.394495413,0.405504587,0.414678899,0.423853211,0.433027523,0.444036697,
0.455045872,0.464220183,0.47706422,0.486238532,0.497247706,0.508256881,
0.517431193,0.526605505,0.533944954,0.541284404,0.550458716,0.56146789,
0.568807339,0.581651376,0.588990826,0.6,0.60733945,0.616513761,0.623853211,
0.634862385,0.64587156,0.655045872,0.664220183,0.671559633,0.682568807,
0.691743119,0.700917431,0.713761468,0.724770642,0.732110092,0.739449541,
0.752293578,0.759633028,0.766972477,0.774311927,0.781651376,0.790825688,
0.798165138,0.80733945,0.814678899,0.823853211,0.829357798,0.836697248,
0.844036697,0.853211009,0.862385321,0.867889908,0.873394495,0.878899083,
0.886238532,0.891743119,0.899082569,0.904587156,0.910091743,0.91559633,
0.921100917,0.926605505,0.932110092,0.941284404,0.950458716,0.955963303,
0.96146789,0.966972477,0.976146789,0.983486239,0.988990826,0.994495413,
1.),.UNSPECIFIED.);
#24406=B_SPLINE_CURVE_WITH_KNOTS('',3,(#226677,#226678,#226679,#226680,
#226681,#226682,#226683,#226684,#226685,#226686,#226687,#226688,#226689,
#226690,#226691,#226692,#226693,#226694,#226695,#226696,#226697,#226698,
#226699,#226700,#226701,#226702,#226703,#226704,#226705,#226706,#226707,
#226708,#226709,#226710,#226711,#226712,#226713,#226714,#226715,#226716,
#226717,#226718,#226719,#226720,#226721,#226722,#226723,#226724,#226725,
#226726,#226727,#226728,#226729,#226730,#226731,#226732,#226733,#226734,
#226735,#226736,#226737,#226738,#226739,#226740,#226741,#226742,#226743,
#226744,#226745,#226746,#226747,#226748,#226749,#226750,#226751,#226752,
#226753,#226754,#226755,#226756,#226757,#226758,#226759,#226760,#226761,
#226762,#226763,#226764,#226765,#226766,#226767,#226768,#226769,#226770,
#226771,#226772,#226773,#226774,#226775,#226776,#226777,#226778,#226779,
#226780,#226781,#226782,#226783,#226784,#226785,#226786,#226787,#226788,
#226789,#226790,#226791,#226792,#226793,#226794,#226795,#226796,#226797,
#226798,#226799,#226800,#226801,#226802,#226803,#226804,#226805,#226806,
#226807,#226808,#226809,#226810,#226811,#226812,#226813,#226814,#226815,
#226816,#226817,#226818,#226819,#226820,#226821,#226822,#226823,#226824,
#226825,#226826,#226827,#226828,#226829,#226830,#226831,#226832,#226833,
#226834,#226835,#226836,#226837,#226838,#226839,#226840,#226841,#226842,
#226843,#226844,#226845,#226846,#226847,#226848,#226849,#226850,#226851,
#226852,#226853,#226854,#226855,#226856,#226857,#226858,#226859,#226860,
#226861,#226862,#226863,#226864,#226865,#226866,#226867,#226868,#226869,
#226870,#226871,#226872,#226873,#226874,#226875,#226876,#226877,#226878,
#226879,#226880,#226881,#226882,#226883,#226884,#226885,#226886,#226887,
#226888,#226889,#226890,#226891,#226892,#226893,#226894,#226895,#226896,
#226897,#226898,#226899,#226900,#226901,#226902,#226903,#226904,#226905,
#226906,#226907,#226908,#226909,#226910,#226911,#226912,#226913,#226914,
#226915,#226916,#226917,#226918,#226919,#226920,#226921,#226922,#226923,
#226924,#226925,#226926,#226927,#226928,#226929,#226930,#226931,#226932,
#226933,#226934,#226935,#226936,#226937,#226938,#226939,#226940,#226941,
#226942,#226943,#226944,#226945,#226946,#226947,#226948,#226949,#226950,
#226951,#226952,#226953,#226954,#226955,#226956,#226957,#226958,#226959,
#226960,#226961,#226962,#226963,#226964,#226965,#226966,#226967,#226968,
#226969,#226970,#226971,#226972,#226973,#226974,#226975,#226976,#226977,
#226978,#226979,#226980,#226981,#226982,#226983,#226984,#226985,#226986,
#226987,#226988,#226989,#226990,#226991,#226992),.UNSPECIFIED.,.F.,.F.,
(4,3,3,3,3,3,3,3,3,3,3,3,3,3,3,3,3,3,3,3,3,3,3,3,3,3,3,3,3,3,3,3,3,3,3,
3,3,3,3,3,3,3,3,3,3,3,3,3,3,3,3,3,3,3,3,3,3,3,3,3,3,3,3,3,3,3,3,3,3,3,3,
3,3,3,3,3,3,3,3,3,3,3,3,3,3,3,3,3,3,3,3,3,3,3,3,3,3,3,3,3,3,3,3,3,3,4),
(0.143172102,0.15412844,0.165137615,0.177981651,0.188990826,0.2,0.211009174,
0.222018349,0.234862385,0.24587156,0.256880734,0.267889908,0.278899083,
0.289908257,0.300917431,0.311926606,0.32293578,0.333944954,0.344954128,
0.355963303,0.368807339,0.379816514,0.39266055,0.401834862,0.411009174,
0.420183486,0.429357798,0.43853211,0.447706422,0.456880734,0.466055046,
0.47706422,0.489908257,0.500917431,0.510091743,0.519266055,0.528440367,
0.535779817,0.543119266,0.550458716,0.557798165,0.565137615,0.572477064,
0.581651376,0.588990826,0.596330275,0.603669725,0.611009174,0.618348624,
0.625688073,0.633027523,0.640366972,0.647706422,0.655045872,0.664220183,
0.671559633,0.678899083,0.686238532,0.693577982,0.700917431,0.710091743,
0.717431193,0.724770642,0.732110092,0.739449541,0.748623853,0.755963303,
0.763302752,0.774311927,0.781651376,0.788990826,0.796330275,0.803669725,
0.811009174,0.816513761,0.822018349,0.827522936,0.833027523,0.83853211,
0.844036697,0.849541284,0.855045872,0.860550459,0.867889908,0.873394495,
0.878899083,0.88440367,0.891743119,0.897247706,0.902752294,0.908256881,
0.913761468,0.921100917,0.926605505,0.933944954,0.939449541,0.944954128,
0.950458716,0.957798165,0.963302752,0.968807339,0.974311927,0.979816514,
0.985321101,0.994495413,1.),.UNSPECIFIED.);
#24407=B_SPLINE_CURVE_WITH_KNOTS('',3,(#227952,#227953,#227954,#227955,
#227956,#227957,#227958,#227959,#227960,#227961,#227962,#227963,#227964,
#227965,#227966,#227967,#227968,#227969,#227970,#227971,#227972,#227973,
#227974,#227975,#227976,#227977,#227978,#227979,#227980,#227981,#227982,
#227983,#227984,#227985,#227986,#227987,#227988,#227989,#227990,#227991,
#227992,#227993,#227994,#227995,#227996,#227997,#227998,#227999,#228000,
#228001,#228002,#228003,#228004,#228005,#228006,#228007,#228008,#228009,
#228010,#228011,#228012,#228013,#228014,#228015,#228016,#228017,#228018,
#228019,#228020,#228021,#228022,#228023,#228024,#228025,#228026,#228027,
#228028,#228029,#228030,#228031,#228032,#228033,#228034,#228035,#228036,
#228037,#228038,#228039,#228040,#228041,#228042,#228043,#228044,#228045,
#228046,#228047,#228048,#228049,#228050,#228051,#228052,#228053,#228054,
#228055,#228056,#228057,#228058,#228059,#228060,#228061,#228062,#228063,
#228064,#228065,#228066,#228067,#228068,#228069,#228070,#228071,#228072,
#228073,#228074,#228075,#228076,#228077,#228078,#228079,#228080,#228081,
#228082,#228083,#228084,#228085,#228086,#228087,#228088,#228089,#228090,
#228091,#228092,#228093,#228094,#228095,#228096,#228097,#228098,#228099,
#228100,#228101,#228102,#228103,#228104,#228105,#228106,#228107,#228108,
#228109,#228110,#228111,#228112,#228113,#228114,#228115,#228116,#228117,
#228118,#228119,#228120,#228121,#228122,#228123,#228124,#228125,#228126,
#228127,#228128,#228129,#228130,#228131,#228132,#228133,#228134,#228135,
#228136,#228137,#228138,#228139,#228140,#228141,#228142,#228143,#228144,
#228145,#228146,#228147,#228148,#228149,#228150,#228151,#228152,#228153,
#228154,#228155,#228156,#228157,#228158,#228159,#228160,#228161,#228162,
#228163,#228164,#228165,#228166,#228167,#228168,#228169,#228170,#228171,
#228172,#228173,#228174,#228175,#228176,#228177,#228178,#228179,#228180,
#228181,#228182,#228183,#228184,#228185,#228186,#228187,#228188,#228189,
#228190,#228191,#228192,#228193,#228194,#228195,#228196,#228197,#228198,
#228199,#228200,#228201,#228202,#228203,#228204,#228205,#228206,#228207,
#228208,#228209,#228210,#228211,#228212,#228213,#228214,#228215,#228216,
#228217,#228218,#228219,#228220,#228221,#228222,#228223,#228224,#228225,
#228226,#228227,#228228,#228229,#228230,#228231,#228232,#228233,#228234,
#228235,#228236,#228237,#228238,#228239,#228240,#228241,#228242,#228243,
#228244,#228245,#228246,#228247,#228248,#228249,#228250,#228251,#228252),
 .UNSPECIFIED.,.F.,.F.,(4,3,3,3,3,3,3,3,3,3,3,3,3,3,3,3,3,3,3,3,3,3,3,3,
3,3,3,3,3,3,3,3,3,3,3,3,3,3,3,3,3,3,3,3,3,3,3,3,3,3,3,3,3,3,3,3,3,3,3,3,
3,3,3,3,3,3,3,3,3,3,3,3,3,3,3,3,3,3,3,3,3,3,3,3,3,3,3,3,3,3,3,3,3,3,3,3,
3,3,3,3,4),(0.143172102,0.15412844,0.165137615,0.179816514,0.190825688,
0.201834862,0.212844037,0.225688073,0.236697248,0.247706422,0.258715596,
0.269724771,0.282568807,0.293577982,0.304587156,0.31559633,0.326605505,
0.344954128,0.355963303,0.366972477,0.377981651,0.388990826,0.398165138,
0.40733945,0.416513761,0.427522936,0.43853211,0.449541284,0.460550459,0.473394495,
0.48440367,0.493577982,0.502752294,0.511926606,0.521100917,0.530275229,
0.537614679,0.544954128,0.552293578,0.559633028,0.568807339,0.576146789,
0.583486239,0.590825688,0.598165138,0.605504587,0.616513761,0.623853211,
0.633027523,0.640366972,0.647706422,0.655045872,0.664220183,0.671559633,
0.682568807,0.689908257,0.700917431,0.711926606,0.719266055,0.726605505,
0.733944954,0.741284404,0.750458716,0.757798165,0.766972477,0.774311927,
0.781651376,0.790825688,0.798165138,0.80733945,0.812844037,0.822018349,
0.827522936,0.833027523,0.83853211,0.844036697,0.851376147,0.856880734,
0.862385321,0.867889908,0.875229358,0.880733945,0.886238532,0.895412844,
0.900917431,0.906422018,0.911926606,0.919266055,0.924770642,0.930275229,
0.935779817,0.943119266,0.950458716,0.955963303,0.963302752,0.968807339,
0.974311927,0.981651376,0.987155963,0.99266055,1.),.UNSPECIFIED.);
#24408=B_SPLINE_CURVE_WITH_KNOTS('',3,(#228253,#228254,#228255,#228256,
#228257,#228258,#228259,#228260,#228261,#228262,#228263,#228264,#228265,
#228266,#228267,#228268,#228269,#228270,#228271,#228272,#228273,#228274,
#228275,#228276,#228277,#228278,#228279,#228280,#228281,#228282,#228283,
#228284,#228285,#228286,#228287,#228288,#228289,#228290,#228291,#228292,
#228293,#228294,#228295,#228296,#228297,#228298,#228299,#228300,#228301,
#228302,#228303,#228304,#228305,#228306,#228307,#228308,#228309,#228310,
#228311,#228312,#228313,#228314,#228315,#228316,#228317,#228318,#228319,
#228320,#228321,#228322,#228323,#228324,#228325,#228326,#228327,#228328,
#228329,#228330,#228331,#228332,#228333,#228334,#228335,#228336,#228337,
#228338,#228339,#228340,#228341,#228342,#228343,#228344,#228345,#228346,
#228347,#228348,#228349,#228350,#228351,#228352,#228353,#228354,#228355,
#228356,#228357,#228358,#228359,#228360,#228361,#228362,#228363,#228364,
#228365,#228366,#228367,#228368,#228369,#228370,#228371,#228372,#228373,
#228374,#228375,#228376,#228377,#228378,#228379,#228380,#228381,#228382,
#228383,#228384,#228385,#228386,#228387,#228388,#228389,#228390,#228391,
#228392,#228393,#228394,#228395,#228396,#228397,#228398,#228399,#228400,
#228401,#228402,#228403,#228404,#228405,#228406,#228407,#228408,#228409,
#228410,#228411,#228412,#228413,#228414,#228415,#228416,#228417,#228418,
#228419,#228420,#228421,#228422,#228423,#228424,#228425,#228426,#228427,
#228428,#228429,#228430,#228431,#228432,#228433,#228434,#228435,#228436,
#228437,#228438,#228439,#228440,#228441,#228442,#228443,#228444,#228445,
#228446,#228447,#228448,#228449,#228450,#228451,#228452,#228453,#228454,
#228455,#228456,#228457,#228458,#228459,#228460,#228461,#228462,#228463,
#228464,#228465,#228466,#228467,#228468,#228469,#228470,#228471,#228472,
#228473,#228474,#228475,#228476,#228477,#228478,#228479,#228480,#228481,
#228482,#228483,#228484,#228485,#228486,#228487,#228488,#228489,#228490,
#228491,#228492,#228493,#228494,#228495,#228496,#228497,#228498,#228499,
#228500,#228501,#228502,#228503,#228504,#228505,#228506,#228507,#228508,
#228509,#228510,#228511,#228512,#228513,#228514,#228515,#228516,#228517,
#228518,#228519,#228520,#228521,#228522,#228523,#228524,#228525,#228526,
#228527,#228528,#228529,#228530,#228531,#228532,#228533,#228534,#228535,
#228536,#228537,#228538,#228539,#228540,#228541,#228542,#228543,#228544,
#228545,#228546,#228547,#228548,#228549,#228550,#228551,#228552,#228553,
#228554,#228555,#228556,#228557,#228558,#228559,#228560,#228561,#228562,
#228563,#228564,#228565,#228566,#228567,#228568,#228569,#228570,#228571,
#228572,#228573,#228574),.UNSPECIFIED.,.F.,.F.,(4,3,3,3,3,3,3,3,3,3,3,3,
3,3,3,3,3,3,3,3,3,3,3,3,3,3,3,3,3,3,3,3,3,3,3,3,3,3,3,3,3,3,3,3,3,3,3,3,
3,3,3,3,3,3,3,3,3,3,3,3,3,3,3,3,3,3,3,3,3,3,3,3,3,3,3,3,3,3,3,3,3,3,3,3,
3,3,3,3,3,3,3,3,3,3,3,3,3,3,3,3,3,3,3,3,3,3,3,4),(0.143172102,0.15412844,
0.165137615,0.176146789,0.187155963,0.198165138,0.211009174,0.222018349,
0.233027523,0.244036697,0.255045872,0.267889908,0.278899083,0.289908257,
0.300917431,0.311926606,0.32293578,0.333944954,0.344954128,0.355963303,
0.366972477,0.377981651,0.388990826,0.398165138,0.40733945,0.416513761,
0.427522936,0.436697248,0.44587156,0.455045872,0.464220183,0.473394495,
0.48440367,0.493577982,0.502752294,0.511926606,0.521100917,0.530275229,
0.537614679,0.544954128,0.552293578,0.559633028,0.566972477,0.574311927,
0.581651376,0.588990826,0.596330275,0.603669725,0.611009174,0.618348624,
0.625688073,0.633027523,0.640366972,0.647706422,0.655045872,0.664220183,
0.671559633,0.678899083,0.686238532,0.693577982,0.700917431,0.710091743,
0.717431193,0.724770642,0.733944954,0.741284404,0.748623853,0.755963303,
0.763302752,0.772477064,0.779816514,0.787155963,0.794495413,0.803669725,
0.811009174,0.816513761,0.822018349,0.827522936,0.833027523,0.83853211,
0.844036697,0.849541284,0.855045872,0.860550459,0.867889908,0.873394495,
0.878899083,0.88440367,0.889908257,0.895412844,0.900917431,0.906422018,
0.911926606,0.917431193,0.924770642,0.930275229,0.935779817,0.941284404,
0.946788991,0.95412844,0.96146789,0.966972477,0.972477064,0.977981651,0.983486239,
0.988990826,0.994495413,1.),.UNSPECIFIED.);
#24409=B_SPLINE_CURVE_WITH_KNOTS('',3,(#229522,#229523,#229524,#229525,
#229526,#229527,#229528,#229529,#229530,#229531,#229532,#229533,#229534,
#229535,#229536,#229537,#229538,#229539,#229540,#229541,#229542,#229543,
#229544,#229545,#229546,#229547,#229548,#229549,#229550,#229551,#229552,
#229553,#229554,#229555,#229556,#229557,#229558,#229559,#229560,#229561,
#229562,#229563,#229564,#229565,#229566,#229567,#229568,#229569,#229570,
#229571,#229572,#229573,#229574,#229575,#229576,#229577,#229578,#229579,
#229580,#229581,#229582,#229583,#229584,#229585,#229586,#229587,#229588,
#229589,#229590,#229591,#229592,#229593,#229594,#229595,#229596,#229597,
#229598,#229599,#229600,#229601,#229602,#229603,#229604,#229605,#229606,
#229607,#229608,#229609,#229610,#229611,#229612,#229613,#229614,#229615,
#229616,#229617,#229618,#229619,#229620,#229621,#229622,#229623,#229624,
#229625,#229626,#229627,#229628,#229629,#229630,#229631,#229632,#229633,
#229634,#229635,#229636,#229637,#229638,#229639,#229640,#229641,#229642,
#229643,#229644,#229645,#229646,#229647,#229648,#229649,#229650,#229651,
#229652,#229653,#229654,#229655,#229656,#229657,#229658,#229659,#229660,
#229661,#229662,#229663,#229664,#229665,#229666,#229667,#229668,#229669,
#229670,#229671,#229672,#229673,#229674,#229675,#229676,#229677,#229678,
#229679,#229680,#229681,#229682,#229683,#229684,#229685,#229686,#229687,
#229688,#229689,#229690,#229691,#229692,#229693,#229694,#229695,#229696,
#229697,#229698,#229699,#229700,#229701,#229702,#229703,#229704,#229705,
#229706,#229707,#229708,#229709,#229710,#229711,#229712,#229713,#229714,
#229715,#229716,#229717,#229718,#229719,#229720,#229721,#229722,#229723,
#229724,#229725,#229726,#229727,#229728,#229729,#229730,#229731,#229732,
#229733,#229734,#229735,#229736,#229737,#229738,#229739,#229740,#229741,
#229742,#229743,#229744,#229745,#229746,#229747,#229748,#229749,#229750,
#229751,#229752,#229753,#229754,#229755,#229756,#229757,#229758,#229759,
#229760,#229761,#229762,#229763,#229764,#229765,#229766,#229767,#229768,
#229769,#229770,#229771,#229772,#229773,#229774,#229775,#229776,#229777,
#229778,#229779,#229780,#229781,#229782,#229783,#229784,#229785,#229786,
#229787,#229788,#229789,#229790,#229791,#229792,#229793,#229794,#229795,
#229796,#229797,#229798,#229799,#229800,#229801,#229802,#229803,#229804,
#229805,#229806,#229807,#229808,#229809,#229810,#229811,#229812,#229813,
#229814,#229815,#229816,#229817,#229818,#229819,#229820,#229821,#229822,
#229823,#229824,#229825,#229826,#229827,#229828,#229829,#229830,#229831,
#229832,#229833,#229834,#229835,#229836,#229837,#229838,#229839,#229840,
#229841,#229842,#229843),.UNSPECIFIED.,.F.,.F.,(4,3,3,3,3,3,3,3,3,3,3,3,
3,3,3,3,3,3,3,3,3,3,3,3,3,3,3,3,3,3,3,3,3,3,3,3,3,3,3,3,3,3,3,3,3,3,3,3,
3,3,3,3,3,3,3,3,3,3,3,3,3,3,3,3,3,3,3,3,3,3,3,3,3,3,3,3,3,3,3,3,3,3,3,3,
3,3,3,3,3,3,3,3,3,3,3,3,3,3,3,3,3,3,3,3,3,3,3,4),(-1.,-0.994495413,-0.988990826,
-0.983486239,-0.977981651,-0.970642202,-0.965137615,-0.959633028,-0.95412844,
-0.948623853,-0.943119266,-0.937614679,-0.932110092,-0.926605505,-0.921100917,
-0.91559633,-0.910091743,-0.904587156,-0.899082569,-0.893577982,-0.888073394,
-0.882568807,-0.87706422,-0.871559633,-0.866055046,-0.860550459,-0.855045872,
-0.849541284,-0.842201835,-0.836697248,-0.831192661,-0.825688073,-0.820183486,
-0.814678899,-0.809174312,-0.801834862,-0.794495413,-0.787155963,-0.779816514,
-0.770642202,-0.763302752,-0.755963303,-0.746788991,-0.737614679,-0.730275229,
-0.72293578,-0.71559633,-0.706422018,-0.699082569,-0.691743119,-0.68440367,
-0.675229358,-0.666055046,-0.658715596,-0.651376147,-0.644036697,-0.636697248,
-0.629357798,-0.622018349,-0.614678899,-0.60733945,-0.6,-0.59266055,-0.585321101,
-0.577981651,-0.570642202,-0.563302752,-0.555963303,-0.546788991,-0.537614679,
-0.530275229,-0.521100917,-0.511926606,-0.502752294,-0.493577982,-0.48440367,
-0.475229358,-0.466055046,-0.453211009,-0.444036697,-0.434862385,-0.425688073,
-0.414678899,-0.405504587,-0.396330275,-0.387155963,-0.376146789,-0.365137615,
-0.35412844,-0.343119266,-0.332110092,-0.321100917,-0.308256881,-0.297247706,
-0.286238532,-0.275229358,-0.264220183,-0.253211009,-0.242201835,-0.231192661,
-0.220183486,-0.209174312,-0.198165138,-0.187155963,-0.176146789,-0.165137615,
-0.15412844,-0.143172102),.UNSPECIFIED.);
#24410=B_SPLINE_CURVE_WITH_KNOTS('',3,(#229844,#229845,#229846,#229847,
#229848,#229849,#229850,#229851,#229852,#229853,#229854,#229855,#229856,
#229857,#229858,#229859,#229860,#229861,#229862,#229863,#229864,#229865,
#229866,#229867,#229868,#229869,#229870,#229871,#229872,#229873,#229874,
#229875,#229876,#229877,#229878,#229879,#229880,#229881,#229882,#229883,
#229884,#229885,#229886,#229887,#229888,#229889,#229890,#229891,#229892,
#229893,#229894,#229895,#229896,#229897,#229898,#229899,#229900,#229901,
#229902,#229903,#229904,#229905,#229906,#229907,#229908,#229909,#229910,
#229911,#229912,#229913,#229914,#229915,#229916,#229917,#229918,#229919,
#229920,#229921,#229922,#229923,#229924,#229925,#229926,#229927,#229928,
#229929,#229930,#229931,#229932,#229933,#229934,#229935,#229936,#229937,
#229938,#229939,#229940,#229941,#229942,#229943,#229944,#229945,#229946,
#229947,#229948,#229949,#229950,#229951,#229952,#229953,#229954,#229955,
#229956,#229957,#229958,#229959,#229960,#229961,#229962,#229963,#229964,
#229965,#229966,#229967,#229968,#229969,#229970,#229971,#229972,#229973,
#229974,#229975,#229976,#229977,#229978,#229979,#229980,#229981,#229982,
#229983,#229984,#229985,#229986,#229987,#229988,#229989,#229990,#229991,
#229992,#229993,#229994,#229995,#229996,#229997,#229998,#229999,#230000,
#230001,#230002,#230003,#230004,#230005,#230006,#230007,#230008,#230009,
#230010,#230011,#230012,#230013,#230014,#230015,#230016,#230017,#230018,
#230019,#230020,#230021,#230022,#230023,#230024,#230025,#230026,#230027,
#230028,#230029,#230030,#230031,#230032,#230033,#230034,#230035,#230036,
#230037,#230038,#230039,#230040,#230041,#230042,#230043,#230044,#230045,
#230046,#230047,#230048,#230049,#230050,#230051,#230052,#230053,#230054,
#230055,#230056,#230057,#230058,#230059,#230060,#230061,#230062,#230063,
#230064,#230065,#230066,#230067,#230068,#230069,#230070,#230071,#230072,
#230073,#230074,#230075,#230076,#230077,#230078,#230079,#230080,#230081,
#230082,#230083,#230084,#230085,#230086,#230087,#230088,#230089,#230090,
#230091,#230092,#230093,#230094,#230095,#230096,#230097,#230098,#230099,
#230100,#230101,#230102,#230103,#230104,#230105,#230106,#230107,#230108,
#230109,#230110,#230111,#230112,#230113,#230114,#230115,#230116,#230117,
#230118,#230119,#230120,#230121,#230122,#230123,#230124,#230125,#230126,
#230127,#230128,#230129,#230130,#230131,#230132),.UNSPECIFIED.,.F.,.F.,
(4,3,3,3,3,3,3,3,3,3,3,3,3,3,3,3,3,3,3,3,3,3,3,3,3,3,3,3,3,3,3,3,3,3,3,
3,3,3,3,3,3,3,3,3,3,3,3,3,3,3,3,3,3,3,3,3,3,3,3,3,3,3,3,3,3,3,3,3,3,3,3,
3,3,3,3,3,3,3,3,3,3,3,3,3,3,3,3,3,3,3,3,3,3,3,3,3,4),(0.143172102,0.15412844,
0.165137615,0.176146789,0.187155963,0.198165138,0.209174312,0.220183486,
0.231192661,0.242201835,0.253211009,0.264220183,0.278899083,0.291743119,
0.302752294,0.31559633,0.326605505,0.337614679,0.350458716,0.363302752,
0.374311927,0.385321101,0.403669725,0.412844037,0.425688073,0.434862385,
0.444036697,0.453211009,0.466055046,0.475229358,0.48440367,0.493577982,
0.506422018,0.517431193,0.526605505,0.533944954,0.541284404,0.55412844,
0.565137615,0.572477064,0.585321101,0.594495413,0.601834862,0.611009174,
0.618348624,0.629357798,0.636697248,0.649541284,0.656880734,0.664220183,
0.671559633,0.678899083,0.688073394,0.697247706,0.704587156,0.711926606,
0.719266055,0.728440367,0.735779817,0.744954128,0.75412844,0.763302752,
0.770642202,0.777981651,0.785321101,0.79266055,0.803669725,0.811009174,
0.816513761,0.825688073,0.833027523,0.83853211,0.84587156,0.851376147,0.858715596,
0.864220183,0.871559633,0.87706422,0.882568807,0.888073394,0.893577982,
0.899082569,0.906422018,0.911926606,0.917431193,0.926605505,0.932110092,
0.939449541,0.944954128,0.95412844,0.959633028,0.968807339,0.974311927,
0.979816514,0.985321101,0.994495413,1.),.UNSPECIFIED.);
#24411=B_SPLINE_CURVE_WITH_KNOTS('',3,(#231095,#231096,#231097,#231098,
#231099,#231100,#231101,#231102,#231103,#231104,#231105,#231106,#231107,
#231108,#231109,#231110,#231111,#231112,#231113,#231114,#231115,#231116,
#231117,#231118,#231119,#231120,#231121,#231122,#231123,#231124,#231125,
#231126,#231127,#231128,#231129,#231130,#231131,#231132,#231133,#231134,
#231135,#231136,#231137,#231138,#231139,#231140,#231141,#231142,#231143,
#231144,#231145,#231146,#231147,#231148,#231149,#231150,#231151,#231152,
#231153,#231154,#231155,#231156,#231157,#231158,#231159,#231160,#231161,
#231162,#231163,#231164,#231165,#231166,#231167,#231168,#231169,#231170,
#231171,#231172,#231173,#231174,#231175,#231176,#231177,#231178,#231179,
#231180,#231181,#231182,#231183,#231184,#231185,#231186,#231187,#231188,
#231189,#231190,#231191,#231192,#231193,#231194,#231195,#231196,#231197,
#231198,#231199,#231200,#231201,#231202,#231203,#231204,#231205,#231206,
#231207,#231208,#231209,#231210,#231211,#231212,#231213,#231214,#231215,
#231216,#231217,#231218,#231219,#231220,#231221,#231222,#231223,#231224,
#231225,#231226,#231227,#231228,#231229,#231230,#231231,#231232,#231233,
#231234,#231235,#231236,#231237,#231238,#231239,#231240,#231241,#231242,
#231243,#231244,#231245,#231246,#231247,#231248,#231249,#231250,#231251,
#231252,#231253,#231254,#231255,#231256,#231257,#231258,#231259,#231260,
#231261,#231262,#231263,#231264,#231265,#231266,#231267,#231268,#231269,
#231270,#231271,#231272,#231273,#231274,#231275,#231276,#231277,#231278,
#231279,#231280,#231281,#231282,#231283,#231284,#231285,#231286,#231287,
#231288,#231289,#231290,#231291,#231292,#231293,#231294,#231295,#231296,
#231297,#231298,#231299,#231300,#231301,#231302,#231303,#231304,#231305,
#231306,#231307,#231308,#231309,#231310,#231311,#231312,#231313,#231314,
#231315,#231316,#231317,#231318,#231319,#231320,#231321,#231322,#231323,
#231324,#231325,#231326,#231327,#231328,#231329,#231330,#231331,#231332,
#231333,#231334,#231335,#231336,#231337,#231338,#231339,#231340,#231341,
#231342,#231343,#231344,#231345,#231346,#231347,#231348,#231349,#231350,
#231351,#231352,#231353,#231354,#231355,#231356,#231357,#231358,#231359,
#231360,#231361,#231362,#231363,#231364,#231365,#231366,#231367,#231368,
#231369,#231370,#231371,#231372,#231373,#231374,#231375,#231376,#231377,
#231378,#231379,#231380,#231381,#231382,#231383,#231384,#231385,#231386,
#231387,#231388,#231389,#231390,#231391,#231392,#231393,#231394,#231395,
#231396,#231397,#231398,#231399,#231400,#231401,#231402,#231403,#231404,
#231405,#231406,#231407,#231408,#231409,#231410,#231411,#231412,#231413),
 .UNSPECIFIED.,.F.,.F.,(4,3,3,3,3,3,3,3,3,3,3,3,3,3,3,3,3,3,3,3,3,3,3,3,
3,3,3,3,3,3,3,3,3,3,3,3,3,3,3,3,3,3,3,3,3,3,3,3,3,3,3,3,3,3,3,3,3,3,3,3,
3,3,3,3,3,3,3,3,3,3,3,3,3,3,3,3,3,3,3,3,3,3,3,3,3,3,3,3,3,3,3,3,3,3,3,3,
3,3,3,3,3,3,3,3,3,3,4),(-1.,-0.990825688,-0.985321101,-0.979816514,-0.974311927,
-0.965137615,-0.959633028,-0.95412844,-0.948623853,-0.943119266,-0.937614679,
-0.932110092,-0.926605505,-0.921100917,-0.91559633,-0.910091743,-0.904587156,
-0.899082569,-0.893577982,-0.888073394,-0.882568807,-0.87706422,-0.871559633,
-0.866055046,-0.860550459,-0.855045872,-0.849541284,-0.844036697,-0.83853211,
-0.833027523,-0.827522936,-0.822018349,-0.814678899,-0.809174312,-0.801834862,
-0.794495413,-0.787155963,-0.779816514,-0.772477064,-0.765137615,-0.757798165,
-0.750458716,-0.743119266,-0.735779817,-0.728440367,-0.721100917,-0.711926606,
-0.704587156,-0.697247706,-0.689908257,-0.682568807,-0.675229358,-0.666055046,
-0.658715596,-0.651376147,-0.644036697,-0.636697248,-0.627522936,-0.620183486,
-0.612844037,-0.605504587,-0.598165138,-0.590825688,-0.583486239,-0.576146789,
-0.568807339,-0.559633028,-0.550458716,-0.543119266,-0.535779817,-0.528440367,
-0.519266055,-0.508256881,-0.499082569,-0.489908257,-0.480733945,-0.471559633,
-0.462385321,-0.453211009,-0.444036697,-0.434862385,-0.425688073,-0.414678899,
-0.405504587,-0.396330275,-0.383486239,-0.372477064,-0.36146789,-0.350458716,
-0.339449541,-0.328440367,-0.317431193,-0.306422018,-0.293577982,-0.282568807,
-0.271559633,-0.260550459,-0.249541284,-0.23853211,-0.227522936,-0.216513761,
-0.205504587,-0.194495413,-0.183486239,-0.172477064,-0.16146789,-0.143172102),
 .UNSPECIFIED.);
#24412=B_SPLINE_CURVE_WITH_KNOTS('',3,(#231414,#231415,#231416,#231417,
#231418,#231419,#231420,#231421,#231422,#231423,#231424,#231425,#231426,
#231427,#231428,#231429,#231430,#231431,#231432,#231433,#231434,#231435,
#231436,#231437,#231438,#231439,#231440,#231441,#231442,#231443,#231444,
#231445,#231446,#231447,#231448,#231449,#231450,#231451,#231452,#231453,
#231454,#231455,#231456,#231457,#231458,#231459,#231460,#231461,#231462,
#231463,#231464,#231465,#231466,#231467,#231468,#231469,#231470,#231471,
#231472,#231473,#231474,#231475,#231476,#231477,#231478,#231479,#231480,
#231481,#231482,#231483,#231484,#231485,#231486,#231487,#231488,#231489,
#231490,#231491,#231492,#231493,#231494,#231495,#231496,#231497,#231498,
#231499,#231500,#231501,#231502,#231503,#231504,#231505,#231506,#231507,
#231508,#231509,#231510,#231511,#231512,#231513,#231514,#231515,#231516,
#231517,#231518,#231519,#231520,#231521,#231522,#231523,#231524,#231525,
#231526,#231527,#231528,#231529,#231530,#231531,#231532,#231533,#231534,
#231535,#231536,#231537,#231538,#231539,#231540,#231541,#231542,#231543,
#231544,#231545,#231546,#231547,#231548,#231549,#231550,#231551,#231552,
#231553,#231554,#231555,#231556,#231557,#231558,#231559,#231560,#231561,
#231562,#231563,#231564,#231565,#231566,#231567,#231568,#231569,#231570,
#231571,#231572,#231573,#231574,#231575,#231576,#231577,#231578,#231579,
#231580,#231581,#231582,#231583,#231584,#231585,#231586,#231587,#231588,
#231589,#231590,#231591,#231592,#231593,#231594,#231595,#231596,#231597,
#231598,#231599,#231600,#231601,#231602,#231603,#231604,#231605,#231606,
#231607,#231608,#231609,#231610,#231611,#231612,#231613,#231614,#231615,
#231616,#231617,#231618,#231619,#231620,#231621,#231622,#231623,#231624,
#231625,#231626,#231627,#231628,#231629,#231630,#231631,#231632,#231633,
#231634,#231635,#231636,#231637,#231638,#231639,#231640,#231641,#231642,
#231643,#231644,#231645,#231646,#231647,#231648,#231649,#231650,#231651,
#231652,#231653,#231654,#231655,#231656,#231657,#231658,#231659,#231660,
#231661,#231662,#231663,#231664,#231665,#231666,#231667,#231668,#231669,
#231670,#231671,#231672,#231673,#231674,#231675,#231676,#231677,#231678,
#231679,#231680,#231681,#231682,#231683,#231684,#231685,#231686,#231687,
#231688,#231689,#231690,#231691,#231692,#231693,#231694,#231695,#231696,
#231697,#231698,#231699,#231700,#231701,#231702,#231703,#231704,#231705),
 .UNSPECIFIED.,.F.,.F.,(4,3,3,3,3,3,3,3,3,3,3,3,3,3,3,3,3,3,3,3,3,3,3,3,
3,3,3,3,3,3,3,3,3,3,3,3,3,3,3,3,3,3,3,3,3,3,3,3,3,3,3,3,3,3,3,3,3,3,3,3,
3,3,3,3,3,3,3,3,3,3,3,3,3,3,3,3,3,3,3,3,3,3,3,3,3,3,3,3,3,3,3,3,3,3,3,3,
3,4),(0.143172102,0.15412844,0.165137615,0.176146789,0.187155963,0.198165138,
0.209174312,0.220183486,0.231192661,0.242201835,0.253211009,0.264220183,
0.275229358,0.286238532,0.299082569,0.310091743,0.321100917,0.332110092,
0.343119266,0.35412844,0.366972477,0.379816514,0.39266055,0.401834862,0.412844037,
0.422018349,0.431192661,0.440366972,0.453211009,0.462385321,0.471559633,
0.480733945,0.489908257,0.500917431,0.513761468,0.52293578,0.532110092,
0.539449541,0.546788991,0.55412844,0.563302752,0.570642202,0.579816514,
0.587155963,0.596330275,0.603669725,0.611009174,0.620183486,0.631192661,
0.640366972,0.649541284,0.658715596,0.666055046,0.673394495,0.680733945,
0.688073394,0.695412844,0.706422018,0.71559633,0.72293578,0.733944954,0.743119266,
0.750458716,0.76146789,0.768807339,0.776146789,0.783486239,0.79266055,0.801834862,
0.809174312,0.818348624,0.825688073,0.831192661,0.836697248,0.842201835,
0.849541284,0.858715596,0.864220183,0.869724771,0.87706422,0.886238532,
0.893577982,0.899082569,0.906422018,0.913761468,0.919266055,0.924770642,
0.930275229,0.935779817,0.944954128,0.95412844,0.959633028,0.968807339,
0.974311927,0.979816514,0.985321101,0.990825688,1.),.UNSPECIFIED.);
#24413=B_SPLINE_CURVE_WITH_KNOTS('',3,(#232650,#232651,#232652,#232653,
#232654,#232655,#232656,#232657,#232658,#232659,#232660,#232661,#232662,
#232663,#232664,#232665,#232666,#232667,#232668,#232669,#232670,#232671,
#232672,#232673,#232674,#232675,#232676,#232677,#232678,#232679,#232680,
#232681,#232682,#232683,#232684,#232685,#232686,#232687,#232688,#232689,
#232690,#232691,#232692,#232693,#232694,#232695,#232696,#232697,#232698,
#232699,#232700,#232701,#232702,#232703,#232704,#232705,#232706,#232707,
#232708,#232709,#232710,#232711,#232712,#232713,#232714,#232715,#232716,
#232717,#232718,#232719,#232720,#232721,#232722,#232723,#232724,#232725,
#232726,#232727,#232728,#232729,#232730,#232731,#232732,#232733,#232734,
#232735,#232736,#232737,#232738,#232739,#232740,#232741,#232742,#232743,
#232744,#232745,#232746,#232747,#232748,#232749,#232750,#232751,#232752,
#232753,#232754,#232755,#232756,#232757,#232758,#232759,#232760,#232761,
#232762,#232763,#232764,#232765,#232766,#232767,#232768,#232769,#232770,
#232771,#232772,#232773,#232774,#232775,#232776,#232777,#232778,#232779,
#232780,#232781,#232782,#232783,#232784,#232785,#232786,#232787,#232788,
#232789,#232790,#232791,#232792,#232793,#232794,#232795,#232796,#232797,
#232798,#232799,#232800,#232801,#232802,#232803,#232804,#232805,#232806,
#232807,#232808,#232809,#232810,#232811,#232812,#232813,#232814,#232815,
#232816,#232817,#232818,#232819,#232820,#232821,#232822,#232823,#232824,
#232825,#232826,#232827,#232828,#232829,#232830,#232831,#232832,#232833,
#232834,#232835,#232836,#232837,#232838,#232839,#232840,#232841,#232842,
#232843,#232844,#232845,#232846,#232847,#232848,#232849,#232850,#232851,
#232852,#232853,#232854,#232855,#232856,#232857,#232858,#232859,#232860,
#232861,#232862,#232863,#232864,#232865,#232866,#232867,#232868,#232869,
#232870,#232871,#232872,#232873,#232874,#232875,#232876,#232877,#232878,
#232879,#232880,#232881,#232882,#232883,#232884,#232885,#232886,#232887,
#232888,#232889,#232890,#232891,#232892,#232893,#232894,#232895,#232896,
#232897,#232898,#232899,#232900,#232901,#232902,#232903,#232904,#232905,
#232906,#232907,#232908,#232909,#232910,#232911,#232912,#232913,#232914,
#232915,#232916,#232917,#232918,#232919,#232920,#232921,#232922,#232923,
#232924,#232925,#232926,#232927,#232928,#232929,#232930,#232931,#232932,
#232933,#232934,#232935,#232936,#232937,#232938,#232939,#232940,#232941,
#232942,#232943,#232944,#232945,#232946,#232947,#232948,#232949,#232950,
#232951,#232952,#232953),.UNSPECIFIED.,.F.,.F.,(4,3,3,3,3,3,3,3,3,3,3,3,
3,3,3,3,3,3,3,3,3,3,3,3,3,3,3,3,3,3,3,3,3,3,3,3,3,3,3,3,3,3,3,3,3,3,3,3,
3,3,3,3,3,3,3,3,3,3,3,3,3,3,3,3,3,3,3,3,3,3,3,3,3,3,3,3,3,3,3,3,3,3,3,3,
3,3,3,3,3,3,3,3,3,3,3,3,3,3,3,3,3,4),(0.143172102,0.15412844,0.165137615,
0.176146789,0.187155963,0.198165138,0.209174312,0.220183486,0.231192661,
0.242201835,0.253211009,0.264220183,0.27706422,0.289908257,0.300917431,
0.313761468,0.324770642,0.335779817,0.348623853,0.359633028,0.370642202,
0.383486239,0.394495413,0.403669725,0.412844037,0.423853211,0.433027523,
0.442201835,0.451376147,0.460550459,0.473394495,0.482568807,0.491743119,
0.500917431,0.510091743,0.519266055,0.528440367,0.535779817,0.543119266,
0.550458716,0.557798165,0.565137615,0.574311927,0.583486239,0.590825688,
0.598165138,0.605504587,0.612844037,0.622018349,0.629357798,0.636697248,
0.644036697,0.651376147,0.664220183,0.673394495,0.680733945,0.689908257,
0.699082569,0.710091743,0.719266055,0.726605505,0.735779817,0.743119266,
0.750458716,0.757798165,0.765137615,0.774311927,0.781651376,0.788990826,
0.796330275,0.803669725,0.812844037,0.820183486,0.825688073,0.831192661,
0.83853211,0.844036697,0.851376147,0.856880734,0.862385321,0.867889908,
0.873394495,0.878899083,0.88440367,0.891743119,0.897247706,0.904587156,
0.910091743,0.91559633,0.921100917,0.928440367,0.933944954,0.939449541,
0.948623853,0.955963303,0.96146789,0.966972477,0.974311927,0.979816514,
0.985321101,0.990825688,1.),.UNSPECIFIED.);
#24414=B_SPLINE_CURVE_WITH_KNOTS('',3,(#232954,#232955,#232956,#232957,
#232958,#232959,#232960,#232961,#232962,#232963,#232964,#232965,#232966,
#232967,#232968,#232969,#232970,#232971,#232972,#232973,#232974,#232975,
#232976,#232977,#232978,#232979,#232980,#232981,#232982,#232983,#232984,
#232985,#232986,#232987,#232988,#232989,#232990,#232991,#232992,#232993,
#232994,#232995,#232996,#232997,#232998,#232999,#233000,#233001,#233002,
#233003,#233004,#233005,#233006,#233007,#233008,#233009,#233010,#233011,
#233012,#233013,#233014,#233015,#233016,#233017,#233018,#233019,#233020,
#233021,#233022,#233023,#233024,#233025,#233026,#233027,#233028,#233029,
#233030,#233031,#233032,#233033,#233034,#233035,#233036,#233037,#233038,
#233039,#233040,#233041,#233042,#233043,#233044,#233045,#233046,#233047,
#233048,#233049,#233050,#233051,#233052,#233053,#233054,#233055,#233056,
#233057,#233058,#233059,#233060,#233061,#233062,#233063,#233064,#233065,
#233066,#233067,#233068,#233069,#233070,#233071,#233072,#233073,#233074,
#233075,#233076,#233077,#233078,#233079,#233080,#233081,#233082,#233083,
#233084,#233085,#233086,#233087,#233088,#233089,#233090,#233091,#233092,
#233093,#233094,#233095,#233096,#233097,#233098,#233099,#233100,#233101,
#233102,#233103,#233104,#233105,#233106,#233107,#233108,#233109,#233110,
#233111,#233112,#233113,#233114,#233115,#233116,#233117,#233118,#233119,
#233120,#233121,#233122,#233123,#233124,#233125,#233126,#233127,#233128,
#233129,#233130,#233131,#233132,#233133,#233134,#233135,#233136,#233137,
#233138,#233139,#233140,#233141,#233142,#233143,#233144,#233145,#233146,
#233147,#233148,#233149,#233150,#233151,#233152,#233153,#233154,#233155,
#233156,#233157,#233158,#233159,#233160,#233161,#233162,#233163,#233164,
#233165,#233166,#233167,#233168,#233169,#233170,#233171,#233172,#233173,
#233174,#233175,#233176,#233177,#233178,#233179,#233180,#233181,#233182,
#233183,#233184,#233185,#233186,#233187,#233188,#233189,#233190,#233191,
#233192,#233193,#233194,#233195,#233196,#233197,#233198,#233199,#233200,
#233201,#233202,#233203,#233204,#233205,#233206,#233207,#233208,#233209,
#233210,#233211,#233212,#233213,#233214,#233215,#233216,#233217,#233218,
#233219,#233220,#233221,#233222,#233223,#233224,#233225,#233226,#233227,
#233228,#233229,#233230,#233231,#233232,#233233,#233234,#233235,#233236,
#233237,#233238,#233239,#233240,#233241,#233242,#233243,#233244,#233245,
#233246,#233247,#233248,#233249,#233250,#233251,#233252,#233253,#233254,
#233255,#233256,#233257,#233258,#233259,#233260,#233261,#233262,#233263,
#233264,#233265,#233266,#233267,#233268,#233269,#233270,#233271,#233272),
 .UNSPECIFIED.,.F.,.F.,(4,3,3,3,3,3,3,3,3,3,3,3,3,3,3,3,3,3,3,3,3,3,3,3,
3,3,3,3,3,3,3,3,3,3,3,3,3,3,3,3,3,3,3,3,3,3,3,3,3,3,3,3,3,3,3,3,3,3,3,3,
3,3,3,3,3,3,3,3,3,3,3,3,3,3,3,3,3,3,3,3,3,3,3,3,3,3,3,3,3,3,3,3,3,3,3,3,
3,3,3,3,3,3,3,3,3,3,4),(0.143172102,0.15412844,0.165137615,0.176146789,
0.187155963,0.198165138,0.209174312,0.220183486,0.231192661,0.242201835,
0.253211009,0.264220183,0.27706422,0.289908257,0.300917431,0.311926606,
0.32293578,0.333944954,0.344954128,0.355963303,0.366972477,0.377981651,
0.388990826,0.398165138,0.40733945,0.416513761,0.425688073,0.434862385,
0.44587156,0.455045872,0.464220183,0.473394495,0.482568807,0.491743119,
0.500917431,0.510091743,0.519266055,0.528440367,0.535779817,0.543119266,
0.550458716,0.557798165,0.565137615,0.572477064,0.579816514,0.587155963,
0.598165138,0.605504587,0.612844037,0.620183486,0.629357798,0.636697248,
0.644036697,0.651376147,0.658715596,0.666055046,0.673394495,0.680733945,
0.688073394,0.695412844,0.702752294,0.710091743,0.717431193,0.724770642,
0.732110092,0.739449541,0.746788991,0.75412844,0.76146789,0.770642202,0.777981651,
0.785321101,0.79266055,0.8,0.80733945,0.812844037,0.820183486,0.825688073,
0.831192661,0.83853211,0.844036697,0.849541284,0.855045872,0.860550459,
0.867889908,0.873394495,0.878899083,0.88440367,0.891743119,0.897247706,
0.902752294,0.908256881,0.913761468,0.921100917,0.926605505,0.933944954,
0.939449541,0.944954128,0.950458716,0.955963303,0.96146789,0.966972477,
0.972477064,0.977981651,0.983486239,0.990825688,1.),.UNSPECIFIED.);
#24415=B_SPLINE_CURVE_WITH_KNOTS('',3,(#234232,#234233,#234234,#234235,
#234236,#234237,#234238,#234239,#234240,#234241,#234242,#234243,#234244,
#234245,#234246,#234247,#234248,#234249,#234250,#234251,#234252,#234253,
#234254,#234255,#234256,#234257,#234258,#234259,#234260,#234261,#234262,
#234263,#234264,#234265,#234266,#234267,#234268,#234269,#234270,#234271,
#234272,#234273,#234274,#234275,#234276,#234277,#234278,#234279,#234280,
#234281,#234282,#234283,#234284,#234285,#234286,#234287,#234288,#234289,
#234290,#234291,#234292,#234293,#234294,#234295,#234296,#234297,#234298,
#234299,#234300,#234301,#234302,#234303,#234304,#234305,#234306,#234307,
#234308,#234309,#234310,#234311,#234312,#234313,#234314,#234315,#234316,
#234317,#234318,#234319,#234320,#234321,#234322,#234323,#234324,#234325,
#234326,#234327,#234328,#234329,#234330,#234331,#234332,#234333,#234334,
#234335,#234336,#234337,#234338,#234339,#234340,#234341,#234342,#234343,
#234344,#234345,#234346,#234347,#234348,#234349,#234350,#234351,#234352,
#234353,#234354,#234355,#234356,#234357,#234358,#234359,#234360,#234361,
#234362,#234363,#234364,#234365,#234366,#234367,#234368,#234369,#234370,
#234371,#234372,#234373,#234374,#234375,#234376,#234377,#234378,#234379,
#234380,#234381,#234382,#234383,#234384,#234385,#234386,#234387,#234388,
#234389,#234390,#234391,#234392,#234393,#234394,#234395,#234396,#234397,
#234398,#234399,#234400,#234401,#234402,#234403,#234404,#234405,#234406,
#234407,#234408,#234409,#234410,#234411,#234412,#234413,#234414,#234415,
#234416,#234417,#234418,#234419,#234420,#234421,#234422,#234423,#234424,
#234425,#234426,#234427,#234428,#234429,#234430,#234431,#234432,#234433,
#234434,#234435,#234436,#234437,#234438,#234439,#234440,#234441,#234442,
#234443,#234444,#234445,#234446,#234447,#234448,#234449,#234450,#234451,
#234452,#234453,#234454,#234455,#234456,#234457,#234458,#234459,#234460,
#234461,#234462,#234463,#234464,#234465,#234466,#234467,#234468,#234469,
#234470,#234471,#234472,#234473,#234474,#234475,#234476,#234477,#234478,
#234479,#234480,#234481,#234482,#234483,#234484,#234485,#234486,#234487,
#234488,#234489,#234490,#234491,#234492,#234493,#234494,#234495,#234496,
#234497,#234498,#234499,#234500,#234501,#234502,#234503,#234504,#234505,
#234506,#234507,#234508,#234509,#234510,#234511,#234512,#234513,#234514,
#234515,#234516,#234517,#234518,#234519,#234520,#234521,#234522,#234523,
#234524,#234525,#234526,#234527,#234528,#234529,#234530,#234531,#234532,
#234533,#234534,#234535,#234536,#234537,#234538,#234539,#234540,#234541),
 .UNSPECIFIED.,.F.,.F.,(4,3,3,3,3,3,3,3,3,3,3,3,3,3,3,3,3,3,3,3,3,3,3,3,
3,3,3,3,3,3,3,3,3,3,3,3,3,3,3,3,3,3,3,3,3,3,3,3,3,3,3,3,3,3,3,3,3,3,3,3,
3,3,3,3,3,3,3,3,3,3,3,3,3,3,3,3,3,3,3,3,3,3,3,3,3,3,3,3,3,3,3,3,3,3,3,3,
3,3,3,3,3,3,3,4),(0.143172102,0.15412844,0.165137615,0.176146789,0.187155963,
0.198165138,0.209174312,0.220183486,0.231192661,0.242201835,0.253211009,
0.264220183,0.275229358,0.286238532,0.297247706,0.308256881,0.319266055,
0.332110092,0.343119266,0.35412844,0.365137615,0.376146789,0.387155963,
0.396330275,0.405504587,0.414678899,0.423853211,0.433027523,0.442201835,
0.451376147,0.460550459,0.469724771,0.478899083,0.488073394,0.497247706,
0.506422018,0.51559633,0.524770642,0.533944954,0.541284404,0.550458716,
0.557798165,0.565137615,0.572477064,0.579816514,0.587155963,0.594495413,
0.601834862,0.609174312,0.622018349,0.629357798,0.642201835,0.649541284,
0.656880734,0.666055046,0.673394495,0.680733945,0.688073394,0.697247706,
0.706422018,0.71559633,0.724770642,0.732110092,0.739449541,0.746788991,
0.75412844,0.76146789,0.768807339,0.777981651,0.785321101,0.794495413,0.801834862,
0.812844037,0.818348624,0.823853211,0.829357798,0.834862385,0.840366972,
0.84587156,0.851376147,0.856880734,0.866055046,0.871559633,0.87706422,0.882568807,
0.888073394,0.895412844,0.900917431,0.908256881,0.913761468,0.92293578,
0.928440367,0.933944954,0.939449541,0.944954128,0.950458716,0.955963303,
0.96146789,0.968807339,0.974311927,0.979816514,0.988990826,0.994495413,
1.),.UNSPECIFIED.);
#24416=B_SPLINE_CURVE_WITH_KNOTS('',3,(#234542,#234543,#234544,#234545,
#234546,#234547,#234548,#234549,#234550,#234551,#234552,#234553,#234554,
#234555,#234556,#234557,#234558,#234559,#234560,#234561,#234562,#234563,
#234564,#234565,#234566,#234567,#234568,#234569,#234570,#234571,#234572,
#234573,#234574,#234575,#234576,#234577,#234578,#234579,#234580,#234581,
#234582,#234583,#234584,#234585,#234586,#234587,#234588,#234589,#234590,
#234591,#234592,#234593,#234594,#234595,#234596,#234597,#234598,#234599,
#234600,#234601,#234602,#234603,#234604,#234605,#234606,#234607,#234608,
#234609,#234610,#234611,#234612,#234613,#234614,#234615,#234616,#234617,
#234618,#234619,#234620,#234621,#234622,#234623,#234624,#234625,#234626,
#234627,#234628,#234629,#234630,#234631,#234632,#234633,#234634,#234635,
#234636,#234637,#234638,#234639,#234640,#234641,#234642,#234643,#234644,
#234645,#234646,#234647,#234648,#234649,#234650,#234651,#234652,#234653,
#234654,#234655,#234656,#234657,#234658,#234659,#234660,#234661,#234662,
#234663,#234664,#234665,#234666,#234667,#234668,#234669,#234670,#234671,
#234672,#234673,#234674,#234675,#234676,#234677,#234678,#234679,#234680,
#234681,#234682,#234683,#234684,#234685,#234686,#234687,#234688,#234689,
#234690,#234691,#234692,#234693,#234694,#234695,#234696,#234697,#234698,
#234699,#234700,#234701,#234702,#234703,#234704,#234705,#234706,#234707,
#234708,#234709,#234710,#234711,#234712,#234713,#234714,#234715,#234716,
#234717,#234718,#234719,#234720,#234721,#234722,#234723,#234724,#234725,
#234726,#234727,#234728,#234729,#234730,#234731,#234732,#234733,#234734,
#234735,#234736,#234737,#234738,#234739,#234740,#234741,#234742,#234743,
#234744,#234745,#234746,#234747,#234748,#234749,#234750,#234751,#234752,
#234753,#234754,#234755,#234756,#234757,#234758,#234759,#234760,#234761,
#234762,#234763,#234764,#234765,#234766,#234767,#234768,#234769,#234770,
#234771,#234772,#234773,#234774,#234775,#234776,#234777,#234778,#234779,
#234780,#234781,#234782,#234783,#234784,#234785,#234786,#234787,#234788,
#234789,#234790,#234791,#234792,#234793,#234794,#234795,#234796,#234797,
#234798,#234799,#234800,#234801,#234802,#234803,#234804,#234805,#234806,
#234807,#234808,#234809,#234810,#234811,#234812,#234813,#234814,#234815,
#234816,#234817,#234818,#234819,#234820,#234821,#234822,#234823,#234824,
#234825,#234826,#234827,#234828,#234829,#234830,#234831,#234832,#234833,
#234834,#234835,#234836,#234837,#234838,#234839,#234840,#234841,#234842,
#234843,#234844,#234845,#234846,#234847,#234848,#234849,#234850,#234851,
#234852,#234853,#234854,#234855,#234856,#234857,#234858,#234859,#234860,
#234861,#234862,#234863,#234864,#234865,#234866,#234867,#234868,#234869),
 .UNSPECIFIED.,.F.,.F.,(4,3,3,3,3,3,3,3,3,3,3,3,3,3,3,3,3,3,3,3,3,3,3,3,
3,3,3,3,3,3,3,3,3,3,3,3,3,3,3,3,3,3,3,3,3,3,3,3,3,3,3,3,3,3,3,3,3,3,3,3,
3,3,3,3,3,3,3,3,3,3,3,3,3,3,3,3,3,3,3,3,3,3,3,3,3,3,3,3,3,3,3,3,3,3,3,3,
3,3,3,3,3,3,3,3,3,3,3,3,3,4),(0.143172102,0.15412844,0.165137615,0.176146789,
0.187155963,0.198165138,0.209174312,0.220183486,0.231192661,0.242201835,
0.253211009,0.264220183,0.275229358,0.286238532,0.297247706,0.308256881,
0.319266055,0.332110092,0.343119266,0.35412844,0.365137615,0.376146789,
0.387155963,0.396330275,0.405504587,0.414678899,0.423853211,0.433027523,
0.442201835,0.451376147,0.460550459,0.469724771,0.478899083,0.488073394,
0.497247706,0.506422018,0.51559633,0.524770642,0.533944954,0.541284404,
0.548623853,0.555963303,0.563302752,0.570642202,0.577981651,0.585321101,
0.59266055,0.6,0.60733945,0.614678899,0.622018349,0.629357798,0.636697248,
0.644036697,0.651376147,0.658715596,0.666055046,0.673394495,0.680733945,
0.688073394,0.695412844,0.702752294,0.710091743,0.717431193,0.724770642,
0.732110092,0.739449541,0.746788991,0.75412844,0.76146789,0.768807339,0.776146789,
0.785321101,0.79266055,0.8,0.80733945,0.812844037,0.818348624,0.823853211,
0.829357798,0.834862385,0.840366972,0.84587156,0.851376147,0.856880734,
0.862385321,0.867889908,0.873394495,0.878899083,0.88440367,0.889908257,
0.895412844,0.900917431,0.906422018,0.911926606,0.917431193,0.92293578,
0.928440367,0.933944954,0.939449541,0.944954128,0.950458716,0.955963303,
0.96146789,0.968807339,0.974311927,0.979816514,0.987155963,0.994495413,
1.),.UNSPECIFIED.);
#24417=B_SPLINE_CURVE_WITH_KNOTS('',3,(#235817,#235818,#235819,#235820,
#235821,#235822,#235823,#235824,#235825,#235826,#235827,#235828,#235829,
#235830,#235831,#235832,#235833,#235834,#235835,#235836,#235837,#235838,
#235839,#235840,#235841,#235842,#235843,#235844,#235845,#235846,#235847,
#235848,#235849,#235850,#235851,#235852,#235853,#235854,#235855,#235856,
#235857,#235858,#235859,#235860,#235861,#235862,#235863,#235864,#235865,
#235866,#235867,#235868,#235869,#235870,#235871,#235872,#235873,#235874,
#235875,#235876,#235877,#235878,#235879,#235880,#235881,#235882,#235883,
#235884,#235885,#235886,#235887,#235888,#235889,#235890,#235891,#235892,
#235893,#235894,#235895,#235896,#235897,#235898,#235899,#235900,#235901,
#235902,#235903,#235904,#235905,#235906,#235907,#235908,#235909,#235910,
#235911,#235912,#235913,#235914,#235915,#235916,#235917,#235918,#235919,
#235920,#235921,#235922,#235923,#235924,#235925,#235926,#235927,#235928,
#235929,#235930,#235931,#235932,#235933,#235934,#235935,#235936,#235937,
#235938,#235939,#235940,#235941,#235942,#235943,#235944,#235945,#235946,
#235947,#235948,#235949,#235950,#235951,#235952,#235953,#235954,#235955,
#235956,#235957,#235958,#235959,#235960,#235961,#235962,#235963,#235964,
#235965,#235966,#235967,#235968,#235969,#235970,#235971,#235972,#235973,
#235974,#235975,#235976,#235977,#235978,#235979,#235980,#235981,#235982,
#235983,#235984,#235985,#235986,#235987,#235988,#235989,#235990,#235991,
#235992,#235993,#235994,#235995,#235996,#235997,#235998,#235999,#236000,
#236001,#236002,#236003,#236004,#236005,#236006,#236007,#236008,#236009,
#236010,#236011,#236012,#236013,#236014,#236015,#236016,#236017,#236018,
#236019,#236020,#236021,#236022,#236023,#236024,#236025,#236026,#236027,
#236028,#236029,#236030,#236031,#236032,#236033,#236034,#236035,#236036,
#236037,#236038,#236039,#236040,#236041,#236042,#236043,#236044,#236045,
#236046,#236047,#236048,#236049,#236050,#236051,#236052,#236053,#236054,
#236055,#236056,#236057,#236058,#236059,#236060,#236061,#236062,#236063,
#236064,#236065,#236066,#236067,#236068,#236069,#236070,#236071,#236072,
#236073,#236074,#236075,#236076,#236077,#236078,#236079,#236080,#236081,
#236082,#236083,#236084,#236085,#236086,#236087,#236088,#236089,#236090,
#236091,#236092,#236093,#236094,#236095,#236096,#236097,#236098,#236099,
#236100,#236101,#236102,#236103,#236104,#236105,#236106,#236107,#236108,
#236109,#236110,#236111,#236112,#236113,#236114,#236115,#236116,#236117,
#236118,#236119,#236120,#236121,#236122,#236123,#236124,#236125,#236126,
#236127,#236128,#236129,#236130,#236131,#236132,#236133,#236134,#236135,
#236136,#236137,#236138),.UNSPECIFIED.,.F.,.F.,(4,3,3,3,3,3,3,3,3,3,3,3,
3,3,3,3,3,3,3,3,3,3,3,3,3,3,3,3,3,3,3,3,3,3,3,3,3,3,3,3,3,3,3,3,3,3,3,3,
3,3,3,3,3,3,3,3,3,3,3,3,3,3,3,3,3,3,3,3,3,3,3,3,3,3,3,3,3,3,3,3,3,3,3,3,
3,3,3,3,3,3,3,3,3,3,3,3,3,3,3,3,3,3,3,3,3,3,3,4),(-1.,-0.99266055,-0.987155963,
-0.981651376,-0.972477064,-0.966972477,-0.96146789,-0.955963303,-0.950458716,
-0.944954128,-0.937614679,-0.932110092,-0.926605505,-0.921100917,-0.91559633,
-0.910091743,-0.904587156,-0.899082569,-0.893577982,-0.888073394,-0.882568807,
-0.87706422,-0.871559633,-0.866055046,-0.860550459,-0.855045872,-0.849541284,
-0.842201835,-0.836697248,-0.831192661,-0.825688073,-0.820183486,-0.814678899,
-0.809174312,-0.801834862,-0.794495413,-0.787155963,-0.779816514,-0.772477064,
-0.765137615,-0.757798165,-0.748623853,-0.741284404,-0.733944954,-0.726605505,
-0.719266055,-0.708256881,-0.700917431,-0.693577982,-0.686238532,-0.678899083,
-0.671559633,-0.664220183,-0.656880734,-0.649541284,-0.642201835,-0.634862385,
-0.627522936,-0.620183486,-0.612844037,-0.605504587,-0.598165138,-0.590825688,
-0.583486239,-0.576146789,-0.568807339,-0.56146789,-0.55412844,-0.546788991,
-0.539449541,-0.532110092,-0.52293578,-0.513761468,-0.504587156,-0.495412844,
-0.486238532,-0.475229358,-0.466055046,-0.453211009,-0.444036697,-0.434862385,
-0.425688073,-0.416513761,-0.40733945,-0.398165138,-0.388990826,-0.377981651,
-0.366972477,-0.355963303,-0.344954128,-0.333944954,-0.32293578,-0.311926606,
-0.300917431,-0.289908257,-0.278899083,-0.267889908,-0.255045872,-0.244036697,
-0.233027523,-0.222018349,-0.211009174,-0.2,-0.188990826,-0.177981651,-0.166972477,
-0.155963303,-0.143172102),.UNSPECIFIED.);
#24418=B_SPLINE_CURVE_WITH_KNOTS('',3,(#236139,#236140,#236141,#236142,
#236143,#236144,#236145,#236146,#236147,#236148,#236149,#236150,#236151,
#236152,#236153,#236154,#236155,#236156,#236157,#236158,#236159,#236160,
#236161,#236162,#236163,#236164,#236165,#236166,#236167,#236168,#236169,
#236170,#236171,#236172,#236173,#236174,#236175,#236176,#236177,#236178,
#236179,#236180,#236181,#236182,#236183,#236184,#236185,#236186,#236187,
#236188,#236189,#236190,#236191,#236192,#236193,#236194,#236195,#236196,
#236197,#236198,#236199,#236200,#236201,#236202,#236203,#236204,#236205,
#236206,#236207,#236208,#236209,#236210,#236211,#236212,#236213,#236214,
#236215,#236216,#236217,#236218,#236219,#236220,#236221,#236222,#236223,
#236224,#236225,#236226,#236227,#236228,#236229,#236230,#236231,#236232,
#236233,#236234,#236235,#236236,#236237,#236238,#236239,#236240,#236241,
#236242,#236243,#236244,#236245,#236246,#236247,#236248,#236249,#236250,
#236251,#236252,#236253,#236254,#236255,#236256,#236257,#236258,#236259,
#236260,#236261,#236262,#236263,#236264,#236265,#236266,#236267,#236268,
#236269,#236270,#236271,#236272,#236273,#236274,#236275,#236276,#236277,
#236278,#236279,#236280,#236281,#236282,#236283,#236284,#236285,#236286,
#236287,#236288,#236289,#236290,#236291,#236292,#236293,#236294,#236295,
#236296,#236297,#236298,#236299,#236300,#236301,#236302,#236303,#236304,
#236305,#236306,#236307,#236308,#236309,#236310,#236311,#236312,#236313,
#236314,#236315,#236316,#236317,#236318,#236319,#236320,#236321,#236322,
#236323,#236324,#236325,#236326,#236327,#236328,#236329,#236330,#236331,
#236332,#236333,#236334,#236335,#236336,#236337,#236338,#236339,#236340,
#236341,#236342,#236343,#236344,#236345,#236346,#236347,#236348,#236349,
#236350,#236351,#236352,#236353,#236354,#236355,#236356,#236357,#236358,
#236359,#236360,#236361,#236362,#236363,#236364,#236365,#236366,#236367,
#236368,#236369,#236370,#236371,#236372,#236373,#236374,#236375,#236376,
#236377,#236378,#236379,#236380,#236381,#236382,#236383,#236384,#236385,
#236386,#236387,#236388,#236389,#236390,#236391,#236392,#236393,#236394,
#236395,#236396,#236397,#236398,#236399,#236400,#236401,#236402,#236403,
#236404,#236405,#236406,#236407,#236408,#236409,#236410,#236411,#236412,
#236413,#236414,#236415,#236416,#236417,#236418,#236419,#236420,#236421,
#236422,#236423,#236424,#236425,#236426,#236427,#236428,#236429,#236430),
 .UNSPECIFIED.,.F.,.F.,(4,3,3,3,3,3,3,3,3,3,3,3,3,3,3,3,3,3,3,3,3,3,3,3,
3,3,3,3,3,3,3,3,3,3,3,3,3,3,3,3,3,3,3,3,3,3,3,3,3,3,3,3,3,3,3,3,3,3,3,3,
3,3,3,3,3,3,3,3,3,3,3,3,3,3,3,3,3,3,3,3,3,3,3,3,3,3,3,3,3,3,3,3,3,3,3,3,
3,4),(0.143172102,0.15412844,0.165137615,0.176146789,0.187155963,0.198165138,
0.209174312,0.220183486,0.231192661,0.242201835,0.255045872,0.267889908,
0.278899083,0.291743119,0.306422018,0.317431193,0.330275229,0.343119266,
0.35412844,0.365137615,0.376146789,0.387155963,0.396330275,0.40733945,0.416513761,
0.425688073,0.43853211,0.449541284,0.458715596,0.469724771,0.482568807,
0.491743119,0.506422018,0.517431193,0.530275229,0.537614679,0.544954128,
0.55412844,0.56146789,0.568807339,0.576146789,0.585321101,0.59266055,0.6,
0.60733945,0.614678899,0.622018349,0.634862385,0.642201835,0.649541284,
0.656880734,0.666055046,0.673394495,0.682568807,0.689908257,0.700917431,
0.708256881,0.717431193,0.726605505,0.733944954,0.741284404,0.748623853,
0.755963303,0.763302752,0.770642202,0.777981651,0.787155963,0.798165138,
0.805504587,0.812844037,0.823853211,0.829357798,0.834862385,0.842201835,
0.849541284,0.855045872,0.860550459,0.867889908,0.873394495,0.878899083,
0.88440367,0.889908257,0.897247706,0.904587156,0.910091743,0.917431193,
0.92293578,0.928440367,0.937614679,0.944954128,0.95412844,0.963302752,0.968807339,
0.977981651,0.983486239,0.988990826,0.994495413,1.),.UNSPECIFIED.);
#24419=B_SPLINE_CURVE_WITH_KNOTS('',3,(#237393,#237394,#237395,#237396,
#237397,#237398,#237399,#237400,#237401,#237402,#237403,#237404,#237405,
#237406,#237407,#237408,#237409,#237410,#237411,#237412,#237413,#237414,
#237415,#237416,#237417,#237418,#237419,#237420,#237421,#237422,#237423,
#237424,#237425,#237426,#237427,#237428,#237429,#237430,#237431,#237432,
#237433,#237434,#237435,#237436,#237437,#237438,#237439,#237440,#237441,
#237442,#237443,#237444,#237445,#237446,#237447,#237448,#237449,#237450,
#237451,#237452,#237453,#237454,#237455,#237456,#237457,#237458,#237459,
#237460,#237461,#237462,#237463,#237464,#237465,#237466,#237467,#237468,
#237469,#237470,#237471,#237472,#237473,#237474,#237475,#237476,#237477,
#237478,#237479,#237480,#237481,#237482,#237483,#237484,#237485,#237486,
#237487,#237488,#237489,#237490,#237491,#237492,#237493,#237494,#237495,
#237496,#237497,#237498,#237499,#237500,#237501,#237502,#237503,#237504,
#237505,#237506,#237507,#237508,#237509,#237510,#237511,#237512,#237513,
#237514,#237515,#237516,#237517,#237518,#237519,#237520,#237521,#237522,
#237523,#237524,#237525,#237526,#237527,#237528,#237529,#237530,#237531,
#237532,#237533,#237534,#237535,#237536,#237537,#237538,#237539,#237540,
#237541,#237542,#237543,#237544,#237545,#237546,#237547,#237548,#237549,
#237550,#237551,#237552,#237553,#237554,#237555,#237556,#237557,#237558,
#237559,#237560,#237561,#237562,#237563,#237564,#237565,#237566,#237567,
#237568,#237569,#237570,#237571,#237572,#237573,#237574,#237575,#237576,
#237577,#237578,#237579,#237580,#237581,#237582,#237583,#237584,#237585,
#237586,#237587,#237588,#237589,#237590,#237591,#237592,#237593,#237594,
#237595,#237596,#237597,#237598,#237599,#237600,#237601,#237602,#237603,
#237604,#237605,#237606,#237607,#237608,#237609,#237610,#237611,#237612,
#237613,#237614,#237615,#237616,#237617,#237618,#237619,#237620,#237621,
#237622,#237623,#237624,#237625,#237626,#237627,#237628,#237629,#237630,
#237631,#237632,#237633,#237634,#237635,#237636,#237637,#237638,#237639,
#237640,#237641,#237642,#237643,#237644,#237645,#237646,#237647,#237648,
#237649,#237650,#237651,#237652,#237653,#237654,#237655,#237656,#237657,
#237658,#237659,#237660,#237661,#237662,#237663,#237664,#237665,#237666,
#237667,#237668,#237669,#237670,#237671,#237672,#237673,#237674,#237675,
#237676,#237677,#237678,#237679,#237680,#237681,#237682,#237683,#237684,
#237685,#237686,#237687,#237688,#237689,#237690,#237691,#237692,#237693,
#237694,#237695,#237696,#237697,#237698,#237699,#237700,#237701,#237702,
#237703,#237704,#237705,#237706,#237707,#237708,#237709,#237710,#237711),
 .UNSPECIFIED.,.F.,.F.,(4,3,3,3,3,3,3,3,3,3,3,3,3,3,3,3,3,3,3,3,3,3,3,3,
3,3,3,3,3,3,3,3,3,3,3,3,3,3,3,3,3,3,3,3,3,3,3,3,3,3,3,3,3,3,3,3,3,3,3,3,
3,3,3,3,3,3,3,3,3,3,3,3,3,3,3,3,3,3,3,3,3,3,3,3,3,3,3,3,3,3,3,3,3,3,3,3,
3,3,3,3,3,3,3,3,3,3,4),(-1.,-0.994495413,-0.988990826,-0.983486239,-0.977981651,
-0.970642202,-0.965137615,-0.959633028,-0.95412844,-0.948623853,-0.943119266,
-0.935779817,-0.928440367,-0.92293578,-0.917431193,-0.911926606,-0.906422018,
-0.900917431,-0.895412844,-0.889908257,-0.88440367,-0.878899083,-0.873394495,
-0.867889908,-0.860550459,-0.855045872,-0.849541284,-0.844036697,-0.83853211,
-0.833027523,-0.827522936,-0.822018349,-0.814678899,-0.80733945,-0.8,-0.79266055,
-0.783486239,-0.776146789,-0.768807339,-0.76146789,-0.75412844,-0.746788991,
-0.739449541,-0.732110092,-0.724770642,-0.717431193,-0.708256881,-0.700917431,
-0.693577982,-0.686238532,-0.678899083,-0.671559633,-0.664220183,-0.656880734,
-0.649541284,-0.642201835,-0.634862385,-0.627522936,-0.620183486,-0.612844037,
-0.605504587,-0.598165138,-0.590825688,-0.583486239,-0.576146789,-0.568807339,
-0.559633028,-0.552293578,-0.543119266,-0.535779817,-0.528440367,-0.519266055,
-0.508256881,-0.499082569,-0.489908257,-0.480733945,-0.471559633,-0.462385321,
-0.453211009,-0.442201835,-0.433027523,-0.423853211,-0.414678899,-0.405504587,
-0.394495413,-0.381651376,-0.370642202,-0.359633028,-0.348623853,-0.337614679,
-0.324770642,-0.311926606,-0.300917431,-0.289908257,-0.278899083,-0.267889908,
-0.255045872,-0.244036697,-0.233027523,-0.222018349,-0.211009174,-0.2,-0.188990826,
-0.177981651,-0.165137615,-0.15412844,-0.143172102),.UNSPECIFIED.);
#24420=B_SPLINE_CURVE_WITH_KNOTS('',3,(#237712,#237713,#237714,#237715,
#237716,#237717,#237718,#237719,#237720,#237721,#237722,#237723,#237724,
#237725,#237726,#237727,#237728,#237729,#237730,#237731,#237732,#237733,
#237734,#237735,#237736,#237737,#237738,#237739,#237740,#237741,#237742,
#237743,#237744,#237745,#237746,#237747,#237748,#237749,#237750,#237751,
#237752,#237753,#237754,#237755,#237756,#237757,#237758,#237759,#237760,
#237761,#237762,#237763,#237764,#237765,#237766,#237767,#237768,#237769,
#237770,#237771,#237772,#237773,#237774,#237775,#237776,#237777,#237778,
#237779,#237780,#237781,#237782,#237783,#237784,#237785,#237786,#237787,
#237788,#237789,#237790,#237791,#237792,#237793,#237794,#237795,#237796,
#237797,#237798,#237799,#237800,#237801,#237802,#237803,#237804,#237805,
#237806,#237807,#237808,#237809,#237810,#237811,#237812,#237813,#237814,
#237815,#237816,#237817,#237818,#237819,#237820,#237821,#237822,#237823,
#237824,#237825,#237826,#237827,#237828,#237829,#237830,#237831,#237832,
#237833,#237834,#237835,#237836,#237837,#237838,#237839,#237840,#237841,
#237842,#237843,#237844,#237845,#237846,#237847,#237848,#237849,#237850,
#237851,#237852,#237853,#237854,#237855,#237856,#237857,#237858,#237859,
#237860,#237861,#237862,#237863,#237864,#237865,#237866,#237867,#237868,
#237869,#237870,#237871,#237872,#237873,#237874,#237875,#237876,#237877,
#237878,#237879,#237880,#237881,#237882,#237883,#237884,#237885,#237886,
#237887,#237888,#237889,#237890,#237891,#237892,#237893,#237894,#237895,
#237896,#237897,#237898,#237899,#237900,#237901,#237902,#237903,#237904,
#237905,#237906,#237907,#237908,#237909,#237910,#237911,#237912,#237913,
#237914,#237915,#237916,#237917,#237918,#237919,#237920,#237921,#237922,
#237923,#237924,#237925,#237926,#237927,#237928,#237929,#237930,#237931,
#237932,#237933,#237934,#237935,#237936,#237937,#237938,#237939,#237940,
#237941,#237942,#237943,#237944,#237945,#237946,#237947,#237948,#237949,
#237950,#237951,#237952,#237953,#237954,#237955,#237956,#237957,#237958,
#237959,#237960,#237961,#237962,#237963,#237964,#237965,#237966,#237967,
#237968,#237969,#237970,#237971,#237972,#237973,#237974,#237975,#237976,
#237977,#237978,#237979,#237980,#237981,#237982,#237983,#237984,#237985,
#237986,#237987,#237988,#237989,#237990,#237991,#237992,#237993,#237994,
#237995,#237996,#237997,#237998,#237999,#238000,#238001,#238002,#238003,
#238004,#238005,#238006,#238007,#238008,#238009,#238010,#238011,#238012,
#238013,#238014,#238015,#238016,#238017,#238018,#238019,#238020,#238021),
 .UNSPECIFIED.,.F.,.F.,(4,3,3,3,3,3,3,3,3,3,3,3,3,3,3,3,3,3,3,3,3,3,3,3,
3,3,3,3,3,3,3,3,3,3,3,3,3,3,3,3,3,3,3,3,3,3,3,3,3,3,3,3,3,3,3,3,3,3,3,3,
3,3,3,3,3,3,3,3,3,3,3,3,3,3,3,3,3,3,3,3,3,3,3,3,3,3,3,3,3,3,3,3,3,3,3,3,
3,3,3,3,3,3,3,4),(0.143172102,0.15412844,0.165137615,0.176146789,0.187155963,
0.198165138,0.209174312,0.220183486,0.231192661,0.242201835,0.253211009,
0.264220183,0.275229358,0.286238532,0.297247706,0.308256881,0.32293578,
0.333944954,0.344954128,0.355963303,0.368807339,0.379816514,0.390825688,
0.4,0.409174312,0.418348624,0.427522936,0.436697248,0.44587156,0.455045872,
0.464220183,0.473394495,0.48440367,0.495412844,0.504587156,0.513761468,
0.52293578,0.532110092,0.539449541,0.550458716,0.559633028,0.566972477,
0.574311927,0.581651376,0.588990826,0.596330275,0.603669725,0.611009174,
0.618348624,0.625688073,0.633027523,0.640366972,0.647706422,0.656880734,
0.664220183,0.673394495,0.682568807,0.689908257,0.697247706,0.706422018,
0.71559633,0.72293578,0.730275229,0.737614679,0.744954128,0.75412844,0.76146789,
0.768807339,0.776146789,0.783486239,0.79266055,0.8,0.80733945,0.812844037,
0.818348624,0.823853211,0.829357798,0.836697248,0.84587156,0.851376147,
0.856880734,0.864220183,0.871559633,0.87706422,0.882568807,0.888073394,
0.893577982,0.900917431,0.906422018,0.913761468,0.919266055,0.924770642,
0.930275229,0.935779817,0.941284404,0.950458716,0.955963303,0.96146789,
0.968807339,0.974311927,0.979816514,0.985321101,0.99266055,1.),
 .UNSPECIFIED.);
#24421=B_SPLINE_CURVE_WITH_KNOTS('',3,(#238966,#238967,#238968,#238969,
#238970,#238971,#238972,#238973,#238974,#238975,#238976,#238977,#238978,
#238979,#238980,#238981,#238982,#238983,#238984,#238985,#238986,#238987,
#238988,#238989,#238990,#238991,#238992,#238993,#238994,#238995,#238996,
#238997,#238998,#238999,#239000,#239001,#239002,#239003,#239004,#239005,
#239006,#239007,#239008,#239009,#239010,#239011,#239012,#239013,#239014,
#239015,#239016,#239017,#239018,#239019,#239020,#239021,#239022,#239023,
#239024,#239025,#239026,#239027,#239028,#239029,#239030,#239031,#239032,
#239033,#239034,#239035,#239036,#239037,#239038,#239039,#239040,#239041,
#239042,#239043,#239044,#239045,#239046,#239047,#239048,#239049,#239050,
#239051,#239052,#239053,#239054,#239055,#239056,#239057,#239058,#239059,
#239060,#239061,#239062,#239063,#239064,#239065,#239066,#239067,#239068,
#239069,#239070,#239071,#239072,#239073,#239074,#239075,#239076,#239077,
#239078,#239079,#239080,#239081,#239082,#239083,#239084,#239085,#239086,
#239087,#239088,#239089,#239090,#239091,#239092,#239093,#239094,#239095,
#239096,#239097,#239098,#239099,#239100,#239101,#239102,#239103,#239104,
#239105,#239106,#239107,#239108,#239109,#239110,#239111,#239112,#239113,
#239114,#239115,#239116,#239117,#239118,#239119,#239120,#239121,#239122,
#239123,#239124,#239125,#239126,#239127,#239128,#239129,#239130,#239131,
#239132,#239133,#239134,#239135,#239136,#239137,#239138,#239139,#239140,
#239141,#239142,#239143,#239144,#239145,#239146,#239147,#239148,#239149,
#239150,#239151,#239152,#239153,#239154,#239155,#239156,#239157,#239158,
#239159,#239160,#239161,#239162,#239163,#239164,#239165,#239166,#239167,
#239168,#239169,#239170,#239171,#239172,#239173,#239174,#239175,#239176,
#239177,#239178,#239179,#239180,#239181,#239182,#239183,#239184,#239185,
#239186,#239187,#239188,#239189,#239190,#239191,#239192,#239193,#239194,
#239195,#239196,#239197,#239198,#239199,#239200,#239201,#239202,#239203,
#239204,#239205,#239206,#239207,#239208,#239209,#239210,#239211,#239212,
#239213,#239214,#239215,#239216,#239217,#239218,#239219,#239220,#239221,
#239222,#239223,#239224,#239225,#239226,#239227,#239228,#239229,#239230,
#239231,#239232,#239233,#239234,#239235,#239236,#239237,#239238,#239239,
#239240,#239241,#239242,#239243,#239244,#239245,#239246,#239247,#239248,
#239249,#239250,#239251,#239252,#239253,#239254,#239255,#239256,#239257,
#239258,#239259,#239260,#239261,#239262,#239263,#239264,#239265,#239266,
#239267,#239268,#239269,#239270,#239271,#239272,#239273,#239274,#239275),
 .UNSPECIFIED.,.F.,.F.,(4,3,3,3,3,3,3,3,3,3,3,3,3,3,3,3,3,3,3,3,3,3,3,3,
3,3,3,3,3,3,3,3,3,3,3,3,3,3,3,3,3,3,3,3,3,3,3,3,3,3,3,3,3,3,3,3,3,3,3,3,
3,3,3,3,3,3,3,3,3,3,3,3,3,3,3,3,3,3,3,3,3,3,3,3,3,3,3,3,3,3,3,3,3,3,3,3,
3,3,3,3,3,3,3,4),(0.143172102,0.15412844,0.165137615,0.176146789,0.187155963,
0.198165138,0.209174312,0.220183486,0.231192661,0.242201835,0.253211009,
0.264220183,0.275229358,0.286238532,0.297247706,0.308256881,0.319266055,
0.330275229,0.343119266,0.35412844,0.365137615,0.376146789,0.387155963,
0.396330275,0.405504587,0.414678899,0.427522936,0.436697248,0.44587156,
0.456880734,0.466055046,0.47706422,0.486238532,0.495412844,0.504587156,
0.513761468,0.52293578,0.532110092,0.539449541,0.546788991,0.55412844,0.56146789,
0.570642202,0.577981651,0.585321101,0.59266055,0.6,0.60733945,0.616513761,
0.625688073,0.633027523,0.640366972,0.647706422,0.655045872,0.664220183,
0.671559633,0.680733945,0.688073394,0.695412844,0.702752294,0.710091743,
0.717431193,0.724770642,0.733944954,0.741284404,0.748623853,0.755963303,
0.763302752,0.770642202,0.777981651,0.785321101,0.794495413,0.801834862,
0.811009174,0.820183486,0.827522936,0.833027523,0.840366972,0.84587156,
0.851376147,0.856880734,0.862385321,0.871559633,0.87706422,0.886238532,
0.891743119,0.897247706,0.902752294,0.911926606,0.917431193,0.92293578,
0.928440367,0.933944954,0.939449541,0.944954128,0.950458716,0.955963303,
0.96146789,0.966972477,0.972477064,0.977981651,0.983486239,0.990825688,
1.),.UNSPECIFIED.);
#24422=B_SPLINE_CURVE_WITH_KNOTS('',3,(#239276,#239277,#239278,#239279,
#239280,#239281,#239282,#239283,#239284,#239285,#239286,#239287,#239288,
#239289,#239290,#239291,#239292,#239293,#239294,#239295,#239296,#239297,
#239298,#239299,#239300,#239301,#239302,#239303,#239304,#239305,#239306,
#239307,#239308,#239309,#239310,#239311,#239312,#239313,#239314,#239315,
#239316,#239317,#239318,#239319,#239320,#239321,#239322,#239323,#239324,
#239325,#239326,#239327,#239328,#239329,#239330,#239331,#239332,#239333,
#239334,#239335,#239336,#239337,#239338,#239339,#239340,#239341,#239342,
#239343,#239344,#239345,#239346,#239347,#239348,#239349,#239350,#239351,
#239352,#239353,#239354,#239355,#239356,#239357,#239358,#239359,#239360,
#239361,#239362,#239363,#239364,#239365,#239366,#239367,#239368,#239369,
#239370,#239371,#239372,#239373,#239374,#239375,#239376,#239377,#239378,
#239379,#239380,#239381,#239382,#239383,#239384,#239385,#239386,#239387,
#239388,#239389,#239390,#239391,#239392,#239393,#239394,#239395,#239396,
#239397,#239398,#239399,#239400,#239401,#239402,#239403,#239404,#239405,
#239406,#239407,#239408,#239409,#239410,#239411,#239412,#239413,#239414,
#239415,#239416,#239417,#239418,#239419,#239420,#239421,#239422,#239423,
#239424,#239425,#239426,#239427,#239428,#239429,#239430,#239431,#239432,
#239433,#239434,#239435,#239436,#239437,#239438,#239439,#239440,#239441,
#239442,#239443,#239444,#239445,#239446,#239447,#239448,#239449,#239450,
#239451,#239452,#239453,#239454,#239455,#239456,#239457,#239458,#239459,
#239460,#239461,#239462,#239463,#239464,#239465,#239466,#239467,#239468,
#239469,#239470,#239471,#239472,#239473,#239474,#239475,#239476,#239477,
#239478,#239479,#239480,#239481,#239482,#239483,#239484,#239485,#239486,
#239487,#239488,#239489,#239490,#239491,#239492,#239493,#239494,#239495,
#239496,#239497,#239498,#239499,#239500,#239501,#239502,#239503,#239504,
#239505,#239506,#239507,#239508,#239509,#239510,#239511,#239512,#239513,
#239514,#239515,#239516,#239517,#239518,#239519,#239520,#239521,#239522,
#239523,#239524,#239525,#239526,#239527,#239528,#239529,#239530,#239531,
#239532,#239533,#239534,#239535,#239536,#239537,#239538,#239539,#239540,
#239541,#239542,#239543,#239544,#239545,#239546,#239547,#239548,#239549,
#239550,#239551,#239552,#239553,#239554,#239555,#239556,#239557,#239558,
#239559,#239560,#239561,#239562,#239563,#239564,#239565,#239566,#239567,
#239568,#239569,#239570,#239571,#239572,#239573,#239574,#239575,#239576,
#239577,#239578,#239579,#239580,#239581,#239582,#239583,#239584,#239585,
#239586,#239587,#239588,#239589,#239590,#239591,#239592,#239593,#239594,
#239595,#239596,#239597,#239598,#239599,#239600),.UNSPECIFIED.,.F.,.F.,
(4,3,3,3,3,3,3,3,3,3,3,3,3,3,3,3,3,3,3,3,3,3,3,3,3,3,3,3,3,3,3,3,3,3,3,
3,3,3,3,3,3,3,3,3,3,3,3,3,3,3,3,3,3,3,3,3,3,3,3,3,3,3,3,3,3,3,3,3,3,3,3,
3,3,3,3,3,3,3,3,3,3,3,3,3,3,3,3,3,3,3,3,3,3,3,3,3,3,3,3,3,3,3,3,3,3,3,3,
3,4),(0.143172102,0.15412844,0.165137615,0.176146789,0.187155963,0.198165138,
0.209174312,0.220183486,0.231192661,0.244036697,0.255045872,0.266055046,
0.27706422,0.288073394,0.299082569,0.310091743,0.321100917,0.332110092,
0.343119266,0.35412844,0.365137615,0.376146789,0.387155963,0.396330275,
0.405504587,0.414678899,0.423853211,0.433027523,0.444036697,0.453211009,
0.462385321,0.475229358,0.48440367,0.493577982,0.502752294,0.511926606,
0.521100917,0.530275229,0.537614679,0.544954128,0.552293578,0.559633028,
0.566972477,0.574311927,0.581651376,0.588990826,0.596330275,0.603669725,
0.611009174,0.618348624,0.625688073,0.633027523,0.640366972,0.647706422,
0.655045872,0.664220183,0.671559633,0.678899083,0.686238532,0.693577982,
0.700917431,0.708256881,0.71559633,0.72293578,0.730275229,0.739449541,0.746788991,
0.75412844,0.76146789,0.768807339,0.776146789,0.783486239,0.790825688,0.798165138,
0.805504587,0.811009174,0.816513761,0.823853211,0.829357798,0.834862385,
0.840366972,0.84587156,0.851376147,0.856880734,0.862385321,0.867889908,
0.873394495,0.878899083,0.886238532,0.891743119,0.897247706,0.902752294,
0.908256881,0.913761468,0.921100917,0.926605505,0.932110092,0.937614679,
0.943119266,0.948623853,0.95412844,0.959633028,0.965137615,0.970642202,
0.976146789,0.981651376,0.987155963,0.994495413,1.),.UNSPECIFIED.);
#24423=B_SPLINE_CURVE_WITH_KNOTS('',3,(#240560,#240561,#240562,#240563,
#240564,#240565,#240566,#240567,#240568,#240569,#240570,#240571,#240572,
#240573,#240574,#240575,#240576,#240577,#240578,#240579,#240580,#240581,
#240582,#240583,#240584,#240585,#240586,#240587,#240588,#240589,#240590,
#240591,#240592,#240593,#240594,#240595,#240596,#240597,#240598,#240599,
#240600,#240601,#240602,#240603,#240604,#240605,#240606,#240607,#240608,
#240609,#240610,#240611,#240612,#240613,#240614,#240615,#240616,#240617,
#240618,#240619,#240620,#240621,#240622,#240623,#240624,#240625,#240626,
#240627,#240628,#240629,#240630,#240631,#240632,#240633,#240634,#240635,
#240636,#240637,#240638,#240639,#240640,#240641,#240642,#240643,#240644,
#240645,#240646,#240647,#240648,#240649,#240650,#240651,#240652,#240653,
#240654,#240655,#240656,#240657,#240658,#240659,#240660,#240661,#240662,
#240663,#240664,#240665,#240666,#240667,#240668,#240669,#240670,#240671,
#240672,#240673,#240674,#240675,#240676,#240677,#240678,#240679,#240680,
#240681,#240682,#240683,#240684,#240685,#240686,#240687,#240688,#240689,
#240690,#240691,#240692,#240693,#240694,#240695,#240696,#240697,#240698,
#240699,#240700,#240701,#240702,#240703,#240704,#240705,#240706,#240707,
#240708,#240709,#240710,#240711,#240712,#240713,#240714,#240715,#240716,
#240717,#240718,#240719,#240720,#240721,#240722,#240723,#240724,#240725,
#240726,#240727,#240728,#240729,#240730,#240731,#240732,#240733,#240734,
#240735,#240736,#240737,#240738,#240739,#240740,#240741,#240742,#240743,
#240744,#240745,#240746,#240747,#240748,#240749,#240750,#240751,#240752,
#240753,#240754,#240755,#240756,#240757,#240758,#240759,#240760,#240761,
#240762,#240763,#240764,#240765,#240766,#240767,#240768,#240769,#240770,
#240771,#240772,#240773,#240774,#240775,#240776,#240777,#240778,#240779,
#240780,#240781,#240782,#240783,#240784,#240785,#240786,#240787,#240788,
#240789,#240790,#240791,#240792,#240793,#240794,#240795,#240796,#240797,
#240798,#240799,#240800,#240801,#240802,#240803,#240804,#240805,#240806,
#240807,#240808,#240809,#240810,#240811,#240812,#240813,#240814,#240815,
#240816,#240817,#240818,#240819,#240820,#240821,#240822,#240823,#240824,
#240825,#240826,#240827,#240828,#240829,#240830,#240831,#240832,#240833,
#240834,#240835,#240836,#240837,#240838,#240839,#240840,#240841,#240842,
#240843,#240844,#240845,#240846,#240847,#240848,#240849,#240850,#240851,
#240852,#240853,#240854,#240855,#240856,#240857,#240858,#240859,#240860,
#240861,#240862,#240863,#240864,#240865,#240866,#240867,#240868,#240869),
 .UNSPECIFIED.,.F.,.F.,(4,3,3,3,3,3,3,3,3,3,3,3,3,3,3,3,3,3,3,3,3,3,3,3,
3,3,3,3,3,3,3,3,3,3,3,3,3,3,3,3,3,3,3,3,3,3,3,3,3,3,3,3,3,3,3,3,3,3,3,3,
3,3,3,3,3,3,3,3,3,3,3,3,3,3,3,3,3,3,3,3,3,3,3,3,3,3,3,3,3,3,3,3,3,3,3,3,
3,3,3,3,3,3,3,4),(0.143172102,0.15412844,0.165137615,0.176146789,0.187155963,
0.198165138,0.209174312,0.222018349,0.233027523,0.244036697,0.255045872,
0.266055046,0.27706422,0.288073394,0.299082569,0.310091743,0.321100917,
0.332110092,0.343119266,0.35412844,0.365137615,0.377981651,0.388990826,
0.398165138,0.409174312,0.418348624,0.427522936,0.436697248,0.44587156,
0.455045872,0.464220183,0.473394495,0.482568807,0.491743119,0.500917431,
0.510091743,0.519266055,0.528440367,0.535779817,0.546788991,0.55412844,
0.56146789,0.568807339,0.576146789,0.583486239,0.590825688,0.598165138,
0.605504587,0.612844037,0.620183486,0.627522936,0.634862385,0.642201835,
0.649541284,0.656880734,0.664220183,0.671559633,0.680733945,0.688073394,
0.699082569,0.710091743,0.717431193,0.724770642,0.732110092,0.739449541,
0.748623853,0.755963303,0.763302752,0.774311927,0.781651376,0.79266055,
0.8,0.80733945,0.812844037,0.818348624,0.825688073,0.831192661,0.836697248,
0.844036697,0.849541284,0.856880734,0.862385321,0.869724771,0.87706422,
0.88440367,0.889908257,0.895412844,0.900917431,0.910091743,0.91559633,0.921100917,
0.926605505,0.932110092,0.937614679,0.944954128,0.950458716,0.957798165,
0.963302752,0.968807339,0.974311927,0.979816514,0.985321101,0.990825688,
1.),.UNSPECIFIED.);
#24424=B_SPLINE_CURVE_WITH_KNOTS('',3,(#240870,#240871,#240872,#240873,
#240874,#240875,#240876,#240877,#240878,#240879,#240880,#240881,#240882,
#240883,#240884,#240885,#240886,#240887,#240888,#240889,#240890,#240891,
#240892,#240893,#240894,#240895,#240896,#240897,#240898,#240899,#240900,
#240901,#240902,#240903,#240904,#240905,#240906,#240907,#240908,#240909,
#240910,#240911,#240912,#240913,#240914,#240915,#240916,#240917,#240918,
#240919,#240920,#240921,#240922,#240923,#240924,#240925,#240926,#240927,
#240928,#240929,#240930,#240931,#240932,#240933,#240934,#240935,#240936,
#240937,#240938,#240939,#240940,#240941,#240942,#240943,#240944,#240945,
#240946,#240947,#240948,#240949,#240950,#240951,#240952,#240953,#240954,
#240955,#240956,#240957,#240958,#240959,#240960,#240961,#240962,#240963,
#240964,#240965,#240966,#240967,#240968,#240969,#240970,#240971,#240972,
#240973,#240974,#240975,#240976,#240977,#240978,#240979,#240980,#240981,
#240982,#240983,#240984,#240985,#240986,#240987,#240988,#240989,#240990,
#240991,#240992,#240993,#240994,#240995,#240996,#240997,#240998,#240999,
#241000,#241001,#241002,#241003,#241004,#241005,#241006,#241007,#241008,
#241009,#241010,#241011,#241012,#241013,#241014,#241015,#241016,#241017,
#241018,#241019,#241020,#241021,#241022,#241023,#241024,#241025,#241026,
#241027,#241028,#241029,#241030,#241031,#241032,#241033,#241034,#241035,
#241036,#241037,#241038,#241039,#241040,#241041,#241042,#241043,#241044,
#241045,#241046,#241047,#241048,#241049,#241050,#241051,#241052,#241053,
#241054,#241055,#241056,#241057,#241058,#241059,#241060,#241061,#241062,
#241063,#241064,#241065,#241066,#241067,#241068,#241069,#241070,#241071,
#241072,#241073,#241074,#241075,#241076,#241077,#241078,#241079,#241080,
#241081,#241082,#241083,#241084,#241085,#241086,#241087,#241088,#241089,
#241090,#241091,#241092,#241093,#241094,#241095,#241096,#241097,#241098,
#241099,#241100,#241101,#241102,#241103,#241104,#241105,#241106,#241107,
#241108,#241109,#241110,#241111,#241112,#241113,#241114,#241115,#241116,
#241117,#241118,#241119,#241120,#241121,#241122,#241123,#241124,#241125,
#241126,#241127,#241128,#241129,#241130,#241131,#241132,#241133,#241134,
#241135,#241136,#241137,#241138,#241139,#241140,#241141,#241142,#241143,
#241144,#241145,#241146,#241147,#241148,#241149,#241150,#241151,#241152,
#241153,#241154,#241155,#241156,#241157,#241158,#241159,#241160,#241161,
#241162,#241163,#241164,#241165,#241166,#241167,#241168,#241169,#241170,
#241171,#241172,#241173,#241174,#241175,#241176,#241177,#241178,#241179,
#241180,#241181,#241182,#241183,#241184,#241185,#241186,#241187,#241188,
#241189,#241190,#241191),.UNSPECIFIED.,.F.,.F.,(4,3,3,3,3,3,3,3,3,3,3,3,
3,3,3,3,3,3,3,3,3,3,3,3,3,3,3,3,3,3,3,3,3,3,3,3,3,3,3,3,3,3,3,3,3,3,3,3,
3,3,3,3,3,3,3,3,3,3,3,3,3,3,3,3,3,3,3,3,3,3,3,3,3,3,3,3,3,3,3,3,3,3,3,3,
3,3,3,3,3,3,3,3,3,3,3,3,3,3,3,3,3,3,3,3,3,3,3,4),(0.143172102,0.15412844,
0.165137615,0.176146789,0.187155963,0.198165138,0.209174312,0.220183486,
0.231192661,0.242201835,0.253211009,0.264220183,0.275229358,0.286238532,
0.297247706,0.308256881,0.319266055,0.330275229,0.341284404,0.352293578,
0.363302752,0.374311927,0.385321101,0.396330275,0.405504587,0.414678899,
0.423853211,0.433027523,0.442201835,0.451376147,0.460550459,0.469724771,
0.478899083,0.488073394,0.497247706,0.506422018,0.51559633,0.524770642,
0.533944954,0.541284404,0.548623853,0.557798165,0.565137615,0.572477064,
0.579816514,0.587155963,0.596330275,0.603669725,0.611009174,0.618348624,
0.625688073,0.633027523,0.640366972,0.647706422,0.655045872,0.662385321,
0.671559633,0.678899083,0.686238532,0.693577982,0.700917431,0.710091743,
0.717431193,0.724770642,0.732110092,0.739449541,0.748623853,0.755963303,
0.763302752,0.772477064,0.779816514,0.787155963,0.794495413,0.801834862,
0.809174312,0.814678899,0.820183486,0.825688073,0.831192661,0.836697248,
0.842201835,0.847706422,0.853211009,0.858715596,0.864220183,0.869724771,
0.875229358,0.880733945,0.888073394,0.893577982,0.899082569,0.904587156,
0.910091743,0.91559633,0.921100917,0.926605505,0.932110092,0.937614679,
0.943119266,0.948623853,0.95412844,0.96146789,0.966972477,0.972477064,0.977981651,
0.983486239,0.990825688,1.),.UNSPECIFIED.);
#24425=B_SPLINE_CURVE_WITH_KNOTS('',3,(#242139,#242140,#242141,#242142,
#242143,#242144,#242145,#242146,#242147,#242148,#242149,#242150,#242151,
#242152,#242153,#242154,#242155,#242156,#242157,#242158,#242159,#242160,
#242161,#242162,#242163,#242164,#242165,#242166,#242167,#242168,#242169,
#242170,#242171,#242172,#242173,#242174,#242175,#242176,#242177,#242178,
#242179,#242180,#242181,#242182,#242183,#242184,#242185,#242186,#242187,
#242188,#242189,#242190,#242191,#242192,#242193,#242194,#242195,#242196,
#242197,#242198,#242199,#242200,#242201,#242202,#242203,#242204,#242205,
#242206,#242207,#242208,#242209,#242210,#242211,#242212,#242213,#242214,
#242215,#242216,#242217,#242218,#242219,#242220,#242221,#242222,#242223,
#242224,#242225,#242226,#242227,#242228,#242229,#242230,#242231,#242232,
#242233,#242234,#242235,#242236,#242237,#242238,#242239,#242240,#242241,
#242242,#242243,#242244,#242245,#242246,#242247,#242248,#242249,#242250,
#242251,#242252,#242253,#242254,#242255,#242256,#242257,#242258,#242259,
#242260,#242261,#242262,#242263,#242264,#242265,#242266,#242267,#242268,
#242269,#242270,#242271,#242272,#242273,#242274,#242275,#242276,#242277,
#242278,#242279,#242280,#242281,#242282,#242283,#242284,#242285,#242286,
#242287,#242288,#242289,#242290,#242291,#242292,#242293,#242294,#242295,
#242296,#242297,#242298,#242299,#242300,#242301,#242302,#242303,#242304,
#242305,#242306,#242307,#242308,#242309,#242310,#242311,#242312,#242313,
#242314,#242315,#242316,#242317,#242318,#242319,#242320,#242321,#242322,
#242323,#242324,#242325,#242326,#242327,#242328,#242329,#242330,#242331,
#242332,#242333,#242334,#242335,#242336,#242337,#242338,#242339,#242340,
#242341,#242342,#242343,#242344,#242345,#242346,#242347,#242348,#242349,
#242350,#242351,#242352,#242353,#242354,#242355,#242356,#242357,#242358,
#242359,#242360,#242361,#242362,#242363,#242364,#242365,#242366,#242367,
#242368,#242369,#242370,#242371,#242372,#242373,#242374,#242375,#242376,
#242377,#242378,#242379,#242380,#242381,#242382,#242383,#242384,#242385,
#242386,#242387,#242388,#242389,#242390,#242391,#242392,#242393,#242394,
#242395,#242396,#242397,#242398,#242399,#242400,#242401,#242402,#242403,
#242404,#242405,#242406,#242407,#242408,#242409,#242410,#242411,#242412,
#242413,#242414,#242415,#242416,#242417,#242418,#242419,#242420,#242421,
#242422,#242423,#242424,#242425,#242426,#242427,#242428,#242429,#242430,
#242431,#242432,#242433,#242434,#242435,#242436,#242437,#242438,#242439,
#242440,#242441,#242442,#242443,#242444,#242445,#242446,#242447,#242448,
#242449,#242450,#242451,#242452,#242453,#242454,#242455,#242456,#242457,
#242458,#242459,#242460),.UNSPECIFIED.,.F.,.F.,(4,3,3,3,3,3,3,3,3,3,3,3,
3,3,3,3,3,3,3,3,3,3,3,3,3,3,3,3,3,3,3,3,3,3,3,3,3,3,3,3,3,3,3,3,3,3,3,3,
3,3,3,3,3,3,3,3,3,3,3,3,3,3,3,3,3,3,3,3,3,3,3,3,3,3,3,3,3,3,3,3,3,3,3,3,
3,3,3,3,3,3,3,3,3,3,3,3,3,3,3,3,3,3,3,3,3,3,3,4),(-1.,-0.994495413,-0.988990826,
-0.983486239,-0.977981651,-0.968807339,-0.959633028,-0.95412844,-0.948623853,
-0.941284404,-0.935779817,-0.930275229,-0.924770642,-0.919266055,-0.913761468,
-0.908256881,-0.902752294,-0.897247706,-0.891743119,-0.886238532,-0.880733945,
-0.875229358,-0.867889908,-0.862385321,-0.855045872,-0.849541284,-0.844036697,
-0.83853211,-0.833027523,-0.827522936,-0.822018349,-0.816513761,-0.811009174,
-0.803669725,-0.796330275,-0.788990826,-0.781651376,-0.774311927,-0.766972477,
-0.759633028,-0.752293578,-0.743119266,-0.735779817,-0.728440367,-0.721100917,
-0.713761468,-0.706422018,-0.699082569,-0.691743119,-0.68440367,-0.67706422,
-0.669724771,-0.662385321,-0.655045872,-0.647706422,-0.640366972,-0.633027523,
-0.625688073,-0.618348624,-0.611009174,-0.603669725,-0.594495413,-0.587155963,
-0.579816514,-0.572477064,-0.565137615,-0.557798165,-0.550458716,-0.543119266,
-0.535779817,-0.528440367,-0.519266055,-0.510091743,-0.500917431,-0.491743119,
-0.480733945,-0.471559633,-0.462385321,-0.453211009,-0.444036697,-0.434862385,
-0.425688073,-0.416513761,-0.40733945,-0.398165138,-0.388990826,-0.377981651,
-0.366972477,-0.355963303,-0.344954128,-0.333944954,-0.32293578,-0.310091743,
-0.299082569,-0.288073394,-0.27706422,-0.266055046,-0.255045872,-0.244036697,
-0.233027523,-0.222018349,-0.211009174,-0.198165138,-0.187155963,-0.176146789,
-0.165137615,-0.15412844,-0.143172102),.UNSPECIFIED.);
#24426=B_SPLINE_CURVE_WITH_KNOTS('',3,(#242461,#242462,#242463,#242464,
#242465,#242466,#242467,#242468,#242469,#242470,#242471,#242472,#242473,
#242474,#242475,#242476,#242477,#242478,#242479,#242480,#242481,#242482,
#242483,#242484,#242485,#242486,#242487,#242488,#242489,#242490,#242491,
#242492,#242493,#242494,#242495,#242496,#242497,#242498,#242499,#242500,
#242501,#242502,#242503,#242504,#242505,#242506,#242507,#242508,#242509,
#242510,#242511,#242512,#242513,#242514,#242515,#242516,#242517,#242518,
#242519,#242520,#242521,#242522,#242523,#242524,#242525,#242526,#242527,
#242528,#242529,#242530,#242531,#242532,#242533,#242534,#242535,#242536,
#242537,#242538,#242539,#242540,#242541,#242542,#242543,#242544,#242545,
#242546,#242547,#242548,#242549,#242550,#242551,#242552,#242553,#242554,
#242555,#242556,#242557,#242558,#242559,#242560,#242561,#242562,#242563,
#242564,#242565,#242566,#242567,#242568,#242569,#242570,#242571,#242572,
#242573,#242574,#242575,#242576,#242577,#242578,#242579,#242580,#242581,
#242582,#242583,#242584,#242585,#242586,#242587,#242588,#242589,#242590,
#242591,#242592,#242593,#242594,#242595,#242596,#242597,#242598,#242599,
#242600,#242601,#242602,#242603,#242604,#242605,#242606,#242607,#242608,
#242609,#242610,#242611,#242612,#242613,#242614,#242615,#242616,#242617,
#242618,#242619,#242620,#242621,#242622,#242623,#242624,#242625,#242626,
#242627,#242628,#242629,#242630,#242631,#242632,#242633,#242634,#242635,
#242636,#242637,#242638,#242639,#242640,#242641,#242642,#242643,#242644,
#242645,#242646,#242647,#242648,#242649,#242650,#242651,#242652,#242653,
#242654,#242655,#242656,#242657,#242658,#242659,#242660,#242661,#242662,
#242663,#242664,#242665,#242666,#242667,#242668,#242669,#242670,#242671,
#242672,#242673,#242674,#242675,#242676,#242677,#242678,#242679,#242680,
#242681,#242682,#242683,#242684,#242685,#242686,#242687,#242688,#242689,
#242690,#242691,#242692,#242693,#242694,#242695,#242696,#242697,#242698,
#242699,#242700,#242701,#242702,#242703,#242704,#242705,#242706,#242707,
#242708,#242709,#242710,#242711,#242712,#242713,#242714,#242715,#242716,
#242717,#242718,#242719,#242720,#242721,#242722,#242723,#242724,#242725,
#242726,#242727,#242728,#242729,#242730,#242731,#242732,#242733,#242734,
#242735,#242736,#242737,#242738,#242739,#242740,#242741,#242742,#242743,
#242744,#242745,#242746,#242747,#242748,#242749,#242750,#242751,#242752,
#242753,#242754,#242755,#242756,#242757,#242758,#242759,#242760,#242761,
#242762,#242763,#242764,#242765,#242766,#242767),.UNSPECIFIED.,.F.,.F.,
(4,3,3,3,3,3,3,3,3,3,3,3,3,3,3,3,3,3,3,3,3,3,3,3,3,3,3,3,3,3,3,3,3,3,3,
3,3,3,3,3,3,3,3,3,3,3,3,3,3,3,3,3,3,3,3,3,3,3,3,3,3,3,3,3,3,3,3,3,3,3,3,
3,3,3,3,3,3,3,3,3,3,3,3,3,3,3,3,3,3,3,3,3,3,3,3,3,3,3,3,3,3,3,4),(0.143172102,
0.15412844,0.165137615,0.176146789,0.187155963,0.198165138,0.209174312,
0.220183486,0.231192661,0.242201835,0.253211009,0.264220183,0.275229358,
0.286238532,0.297247706,0.308256881,0.319266055,0.330275229,0.341284404,
0.352293578,0.363302752,0.374311927,0.385321101,0.396330275,0.405504587,
0.414678899,0.425688073,0.434862385,0.444036697,0.455045872,0.464220183,
0.473394495,0.48440367,0.495412844,0.506422018,0.51559633,0.524770642,0.533944954,
0.541284404,0.548623853,0.555963303,0.563302752,0.572477064,0.579816514,
0.587155963,0.594495413,0.601834862,0.609174312,0.616513761,0.623853211,
0.631192661,0.640366972,0.647706422,0.658715596,0.669724771,0.67706422,
0.68440367,0.693577982,0.700917431,0.708256881,0.71559633,0.72293578,0.730275229,
0.737614679,0.744954128,0.752293578,0.759633028,0.766972477,0.774311927,
0.781651376,0.788990826,0.796330275,0.80733945,0.814678899,0.820183486,
0.825688073,0.831192661,0.840366972,0.84587156,0.851376147,0.858715596,
0.864220183,0.871559633,0.87706422,0.882568807,0.891743119,0.897247706,
0.902752294,0.908256881,0.91559633,0.921100917,0.928440367,0.933944954,
0.939449541,0.944954128,0.952293578,0.957798165,0.963302752,0.968807339,
0.974311927,0.981651376,0.990825688,1.),.UNSPECIFIED.);
#24427=B_SPLINE_CURVE_WITH_KNOTS('',3,(#243730,#243731,#243732,#243733,
#243734,#243735,#243736,#243737,#243738,#243739,#243740,#243741,#243742,
#243743,#243744,#243745,#243746,#243747,#243748,#243749,#243750,#243751,
#243752,#243753,#243754,#243755,#243756,#243757,#243758,#243759,#243760,
#243761,#243762,#243763,#243764,#243765,#243766,#243767,#243768,#243769,
#243770,#243771,#243772,#243773,#243774,#243775,#243776,#243777,#243778,
#243779,#243780,#243781,#243782,#243783,#243784,#243785,#243786,#243787,
#243788,#243789,#243790,#243791,#243792,#243793,#243794,#243795,#243796,
#243797,#243798,#243799,#243800,#243801,#243802,#243803,#243804,#243805,
#243806,#243807,#243808,#243809,#243810,#243811,#243812,#243813,#243814,
#243815,#243816,#243817,#243818,#243819,#243820,#243821,#243822,#243823,
#243824,#243825,#243826,#243827,#243828,#243829,#243830,#243831,#243832,
#243833,#243834,#243835,#243836,#243837,#243838,#243839,#243840,#243841,
#243842,#243843,#243844,#243845,#243846,#243847,#243848,#243849,#243850,
#243851,#243852,#243853,#243854,#243855,#243856,#243857,#243858,#243859,
#243860,#243861,#243862,#243863,#243864,#243865,#243866,#243867,#243868,
#243869,#243870,#243871,#243872,#243873,#243874,#243875,#243876,#243877,
#243878,#243879,#243880,#243881,#243882,#243883,#243884,#243885,#243886,
#243887,#243888,#243889,#243890,#243891,#243892,#243893,#243894,#243895,
#243896,#243897,#243898,#243899,#243900,#243901,#243902,#243903,#243904,
#243905,#243906,#243907,#243908,#243909,#243910,#243911,#243912,#243913,
#243914,#243915,#243916,#243917,#243918,#243919,#243920,#243921,#243922,
#243923,#243924,#243925,#243926,#243927,#243928,#243929,#243930,#243931,
#243932,#243933,#243934,#243935,#243936,#243937,#243938,#243939,#243940,
#243941,#243942,#243943,#243944,#243945,#243946,#243947,#243948,#243949,
#243950,#243951,#243952,#243953,#243954,#243955,#243956,#243957,#243958,
#243959,#243960,#243961,#243962,#243963,#243964,#243965,#243966,#243967,
#243968,#243969,#243970,#243971,#243972,#243973,#243974,#243975,#243976,
#243977,#243978,#243979,#243980,#243981,#243982,#243983,#243984,#243985,
#243986,#243987,#243988,#243989,#243990,#243991,#243992,#243993,#243994,
#243995,#243996,#243997,#243998,#243999,#244000,#244001,#244002,#244003,
#244004,#244005,#244006,#244007,#244008,#244009,#244010,#244011,#244012,
#244013,#244014,#244015,#244016,#244017,#244018,#244019,#244020,#244021,
#244022,#244023,#244024,#244025,#244026,#244027,#244028,#244029,#244030,
#244031,#244032,#244033,#244034,#244035,#244036,#244037,#244038,#244039,
#244040,#244041,#244042,#244043,#244044,#244045,#244046,#244047,#244048,
#244049,#244050,#244051,#244052,#244053,#244054),.UNSPECIFIED.,.F.,.F.,
(4,3,3,3,3,3,3,3,3,3,3,3,3,3,3,3,3,3,3,3,3,3,3,3,3,3,3,3,3,3,3,3,3,3,3,
3,3,3,3,3,3,3,3,3,3,3,3,3,3,3,3,3,3,3,3,3,3,3,3,3,3,3,3,3,3,3,3,3,3,3,3,
3,3,3,3,3,3,3,3,3,3,3,3,3,3,3,3,3,3,3,3,3,3,3,3,3,3,3,3,3,3,3,3,3,3,3,3,
3,4),(-1.,-0.994495413,-0.988990826,-0.983486239,-0.977981651,-0.972477064,
-0.966972477,-0.96146789,-0.955963303,-0.950458716,-0.944954128,-0.939449541,
-0.933944954,-0.926605505,-0.919266055,-0.913761468,-0.908256881,-0.902752294,
-0.897247706,-0.891743119,-0.886238532,-0.880733945,-0.875229358,-0.869724771,
-0.864220183,-0.858715596,-0.851376147,-0.84587156,-0.840366972,-0.834862385,
-0.829357798,-0.823853211,-0.818348624,-0.812844037,-0.80733945,-0.8,-0.79266055,
-0.785321101,-0.777981651,-0.770642202,-0.763302752,-0.755963303,-0.748623853,
-0.741284404,-0.732110092,-0.724770642,-0.717431193,-0.708256881,-0.700917431,
-0.693577982,-0.686238532,-0.67706422,-0.669724771,-0.662385321,-0.655045872,
-0.647706422,-0.640366972,-0.633027523,-0.625688073,-0.618348624,-0.611009174,
-0.603669725,-0.596330275,-0.588990826,-0.581651376,-0.574311927,-0.566972477,
-0.559633028,-0.552293578,-0.544954128,-0.537614679,-0.530275229,-0.521100917,
-0.511926606,-0.502752294,-0.493577982,-0.478899083,-0.469724771,-0.460550459,
-0.451376147,-0.442201835,-0.433027523,-0.423853211,-0.414678899,-0.405504587,
-0.396330275,-0.387155963,-0.376146789,-0.365137615,-0.35412844,-0.343119266,
-0.332110092,-0.321100917,-0.310091743,-0.299082569,-0.288073394,-0.27706422,
-0.266055046,-0.255045872,-0.244036697,-0.233027523,-0.222018349,-0.211009174,
-0.2,-0.188990826,-0.177981651,-0.166972477,-0.155963303,-0.143172102),
 .UNSPECIFIED.);
#24428=B_SPLINE_CURVE_WITH_KNOTS('',3,(#244055,#244056,#244057,#244058,
#244059,#244060,#244061,#244062,#244063,#244064,#244065,#244066,#244067,
#244068,#244069,#244070,#244071,#244072,#244073,#244074,#244075,#244076,
#244077,#244078,#244079,#244080,#244081,#244082,#244083,#244084,#244085,
#244086,#244087,#244088,#244089,#244090,#244091,#244092,#244093,#244094,
#244095,#244096,#244097,#244098,#244099,#244100,#244101,#244102,#244103,
#244104,#244105,#244106,#244107,#244108,#244109,#244110,#244111,#244112,
#244113,#244114,#244115,#244116,#244117,#244118,#244119,#244120,#244121,
#244122,#244123,#244124,#244125,#244126,#244127,#244128,#244129,#244130,
#244131,#244132,#244133,#244134,#244135,#244136,#244137,#244138,#244139,
#244140,#244141,#244142,#244143,#244144,#244145,#244146,#244147,#244148,
#244149,#244150,#244151,#244152,#244153,#244154,#244155,#244156,#244157,
#244158,#244159,#244160,#244161,#244162,#244163,#244164,#244165,#244166,
#244167,#244168,#244169,#244170,#244171,#244172,#244173,#244174,#244175,
#244176,#244177,#244178,#244179,#244180,#244181,#244182,#244183,#244184,
#244185,#244186,#244187,#244188,#244189,#244190,#244191,#244192,#244193,
#244194,#244195,#244196,#244197,#244198,#244199,#244200,#244201,#244202,
#244203,#244204,#244205,#244206,#244207,#244208,#244209,#244210,#244211,
#244212,#244213,#244214,#244215,#244216,#244217,#244218,#244219,#244220,
#244221,#244222,#244223,#244224,#244225,#244226,#244227,#244228,#244229,
#244230,#244231,#244232,#244233,#244234,#244235,#244236,#244237,#244238,
#244239,#244240,#244241,#244242,#244243,#244244,#244245,#244246,#244247,
#244248,#244249,#244250,#244251,#244252,#244253,#244254,#244255,#244256,
#244257,#244258,#244259,#244260,#244261,#244262,#244263,#244264,#244265,
#244266,#244267,#244268,#244269,#244270,#244271,#244272,#244273,#244274,
#244275,#244276,#244277,#244278,#244279,#244280,#244281,#244282,#244283,
#244284,#244285,#244286,#244287,#244288,#244289,#244290,#244291,#244292,
#244293,#244294,#244295,#244296,#244297,#244298,#244299,#244300,#244301,
#244302,#244303,#244304,#244305,#244306,#244307,#244308,#244309,#244310,
#244311,#244312,#244313,#244314,#244315,#244316,#244317,#244318,#244319,
#244320,#244321,#244322,#244323,#244324,#244325,#244326,#244327,#244328,
#244329,#244330,#244331,#244332,#244333,#244334,#244335,#244336,#244337,
#244338,#244339,#244340,#244341,#244342,#244343,#244344,#244345,#244346,
#244347,#244348,#244349,#244350,#244351,#244352,#244353,#244354,#244355,
#244356,#244357,#244358,#244359,#244360,#244361),.UNSPECIFIED.,.F.,.F.,
(4,3,3,3,3,3,3,3,3,3,3,3,3,3,3,3,3,3,3,3,3,3,3,3,3,3,3,3,3,3,3,3,3,3,3,
3,3,3,3,3,3,3,3,3,3,3,3,3,3,3,3,3,3,3,3,3,3,3,3,3,3,3,3,3,3,3,3,3,3,3,3,
3,3,3,3,3,3,3,3,3,3,3,3,3,3,3,3,3,3,3,3,3,3,3,3,3,3,3,3,3,3,3,4),(0.143172102,
0.15412844,0.165137615,0.177981651,0.188990826,0.2,0.211009174,0.222018349,
0.233027523,0.244036697,0.255045872,0.266055046,0.27706422,0.288073394,
0.299082569,0.310091743,0.321100917,0.332110092,0.343119266,0.35412844,
0.365137615,0.376146789,0.387155963,0.396330275,0.405504587,0.418348624,
0.429357798,0.43853211,0.449541284,0.460550459,0.473394495,0.486238532,
0.495412844,0.506422018,0.51559633,0.524770642,0.535779817,0.543119266,
0.550458716,0.557798165,0.565137615,0.572477064,0.581651376,0.588990826,
0.596330275,0.603669725,0.611009174,0.618348624,0.625688073,0.633027523,
0.640366972,0.647706422,0.655045872,0.662385321,0.669724771,0.67706422,
0.68440367,0.693577982,0.700917431,0.708256881,0.71559633,0.72293578,0.730275229,
0.737614679,0.744954128,0.752293578,0.763302752,0.770642202,0.777981651,
0.785321101,0.79266055,0.8,0.80733945,0.812844037,0.820183486,0.825688073,
0.831192661,0.836697248,0.842201835,0.851376147,0.856880734,0.864220183,
0.869724771,0.875229358,0.882568807,0.888073394,0.897247706,0.902752294,
0.908256881,0.91559633,0.92293578,0.930275229,0.937614679,0.943119266,0.950458716,
0.955963303,0.96146789,0.966972477,0.972477064,0.977981651,0.983486239,
0.99266055,1.),.UNSPECIFIED.);
#24429=B_SPLINE_CURVE_WITH_KNOTS('',5,(#245306,#245307,#245308,#245309,
#245310,#245311,#245312,#245313,#245314,#245315,#245316,#245317,#245318,
#245319,#245320,#245321,#245322,#245323,#245324,#245325,#245326,#245327,
#245328,#245329,#245330,#245331,#245332,#245333,#245334,#245335,#245336,
#245337,#245338,#245339,#245340,#245341,#245342,#245343,#245344,#245345,
#245346,#245347,#245348,#245349,#245350,#245351,#245352,#245353,#245354,
#245355,#245356,#245357,#245358,#245359,#245360,#245361,#245362,#245363,
#245364,#245365,#245366,#245367,#245368,#245369,#245370,#245371,#245372,
#245373,#245374,#245375,#245376,#245377,#245378,#245379,#245380,#245381,
#245382,#245383,#245384,#245385,#245386,#245387,#245388,#245389,#245390,
#245391,#245392,#245393,#245394,#245395,#245396,#245397,#245398,#245399,
#245400,#245401,#245402,#245403,#245404,#245405,#245406,#245407,#245408,
#245409,#245410,#245411,#245412,#245413,#245414,#245415,#245416,#245417,
#245418,#245419,#245420,#245421,#245422,#245423,#245424,#245425,#245426,
#245427,#245428,#245429,#245430,#245431,#245432,#245433,#245434,#245435,
#245436,#245437,#245438,#245439,#245440,#245441,#245442,#245443,#245444,
#245445,#245446,#245447,#245448,#245449,#245450,#245451,#245452,#245453,
#245454,#245455,#245456,#245457,#245458,#245459,#245460,#245461,#245462,
#245463,#245464,#245465,#245466,#245467,#245468,#245469,#245470,#245471,
#245472,#245473,#245474,#245475,#245476,#245477,#245478,#245479,#245480,
#245481,#245482,#245483,#245484,#245485,#245486,#245487,#245488,#245489,
#245490,#245491,#245492,#245493,#245494,#245495,#245496,#245497,#245498,
#245499,#245500,#245501,#245502,#245503,#245504,#245505,#245506,#245507,
#245508,#245509,#245510,#245511,#245512,#245513,#245514,#245515,#245516,
#245517,#245518,#245519,#245520,#245521,#245522,#245523,#245524,#245525,
#245526,#245527,#245528,#245529,#245530,#245531,#245532,#245533,#245534,
#245535,#245536,#245537,#245538,#245539,#245540,#245541,#245542,#245543,
#245544,#245545,#245546,#245547,#245548,#245549,#245550,#245551,#245552,
#245553,#245554,#245555,#245556,#245557,#245558,#245559,#245560,#245561,
#245562,#245563,#245564,#245565,#245566,#245567,#245568,#245569,#245570,
#245571,#245572,#245573,#245574,#245575,#245576,#245577,#245578,#245579,
#245580,#245581,#245582,#245583,#245584,#245585,#245586,#245587,#245588,
#245589,#245590,#245591,#245592,#245593,#245594,#245595,#245596,#245597,
#245598,#245599,#245600,#245601,#245602,#245603,#245604,#245605,#245606,
#245607,#245608,#245609,#245610,#245611,#245612,#245613,#245614,#245615,
#245616,#245617,#245618,#245619,#245620,#245621,#245622,#245623,#245624,
#245625,#245626,#245627,#245628,#245629,#245630,#245631,#245632,#245633,
#245634,#245635,#245636,#245637,#245638,#245639,#245640,#245641,#245642,
#245643,#245644,#245645,#245646,#245647,#245648,#245649,#245650,#245651,
#245652,#245653,#245654,#245655,#245656,#245657,#245658,#245659,#245660,
#245661,#245662,#245663,#245664,#245665,#245666,#245667,#245668,#245669,
#245670,#245671,#245672,#245673,#245674,#245675,#245676,#245677,#245678,
#245679,#245680,#245681,#245682,#245683,#245684,#245685,#245686,#245687,
#245688,#245689,#245690,#245691,#245692,#245693,#245694,#245695,#245696,
#245697,#245698,#245699,#245700,#245701,#245702,#245703,#245704,#245705,
#245706,#245707,#245708,#245709,#245710,#245711,#245712,#245713,#245714,
#245715,#245716,#245717,#245718,#245719,#245720,#245721,#245722,#245723,
#245724,#245725,#245726,#245727,#245728,#245729,#245730,#245731,#245732,
#245733,#245734,#245735,#245736,#245737,#245738,#245739,#245740,#245741,
#245742,#245743,#245744,#245745,#245746,#245747,#245748,#245749,#245750,
#245751,#245752,#245753,#245754,#245755,#245756,#245757,#245758,#245759,
#245760,#245761,#245762,#245763,#245764,#245765,#245766,#245767,#245768,
#245769,#245770,#245771,#245772,#245773,#245774,#245775,#245776,#245777),
 .UNSPECIFIED.,.F.,.F.,(6,1,1,1,1,1,1,1,1,1,1,1,1,1,1,1,1,1,1,1,1,1,1,1,
1,1,1,1,1,1,1,1,1,1,1,1,1,1,1,1,1,1,1,1,1,1,1,1,1,1,1,1,1,1,1,1,1,1,1,1,
1,1,1,1,1,1,1,1,1,1,1,1,1,1,1,1,1,1,1,1,1,1,1,1,1,1,1,1,1,1,1,1,1,1,1,1,
1,1,1,1,1,1,1,1,1,1,1,1,1,1,1,1,1,1,1,1,1,1,1,1,1,1,1,1,1,1,1,1,1,1,1,1,
1,1,1,1,1,1,1,1,1,1,1,1,1,1,1,1,1,1,1,1,1,1,1,1,1,1,1,1,1,1,1,1,1,1,1,1,
1,1,1,1,1,1,1,1,1,1,1,1,1,1,1,1,1,1,1,1,1,1,1,1,1,1,1,1,1,1,1,1,1,1,1,1,
1,1,1,1,1,1,1,1,1,1,1,1,1,1,1,1,1,1,1,1,1,1,1,1,1,1,1,1,1,1,1,1,1,1,1,1,
1,1,1,1,1,1,1,1,1,1,1,1,1,1,1,1,1,1,1,1,1,1,1,1,1,1,1,1,1,1,1,1,1,1,1,1,
1,1,1,1,1,1,1,1,1,1,1,1,1,1,1,1,1,1,1,1,1,1,1,1,1,1,1,1,1,1,1,1,1,1,1,1,
1,1,1,1,1,1,1,1,1,1,1,1,1,1,1,1,1,1,1,1,1,1,1,1,1,1,1,1,1,1,1,1,1,1,1,1,
1,1,1,1,1,1,1,1,1,1,1,1,1,1,1,1,1,1,1,1,1,1,1,1,1,1,1,1,1,1,1,1,1,1,1,1,
1,1,1,1,1,1,1,1,1,1,1,1,1,1,1,1,1,1,1,1,1,1,1,1,1,1,1,1,1,1,1,1,1,1,1,1,
1,1,1,1,1,1,1,1,1,1,1,1,1,1,1,1,1,1,1,1,1,1,1,1,1,1,1,1,1,1,1,1,1,1,1,1,
1,1,1,1,1,1,1,1,1,1,1,6),(0.143172102,0.144954128,0.146788991,0.148623853,
0.150458716,0.152293578,0.15412844,0.155963303,0.157798165,0.159633028,
0.16146789,0.163302752,0.165137615,0.166972477,0.168807339,0.170642202,
0.172477064,0.174311927,0.176146789,0.177981651,0.179816514,0.181651376,
0.183486239,0.185321101,0.187155963,0.188990826,0.190825688,0.19266055,
0.194495413,0.196330275,0.198165138,0.2,0.201834862,0.203669725,0.205504587,
0.20733945,0.209174312,0.211009174,0.212844037,0.214678899,0.216513761,
0.218348624,0.220183486,0.222018349,0.223853211,0.225688073,0.227522936,
0.229357798,0.231192661,0.233027523,0.234862385,0.236697248,0.23853211,
0.240366972,0.242201835,0.244036697,0.24587156,0.247706422,0.249541284,
0.251376147,0.253211009,0.255045872,0.256880734,0.258715596,0.260550459,
0.262385321,0.264220183,0.266055046,0.267889908,0.269724771,0.271559633,
0.273394495,0.275229358,0.27706422,0.278899083,0.280733945,0.282568807,
0.28440367,0.286238532,0.288073394,0.289908257,0.291743119,0.293577982,
0.295412844,0.297247706,0.299082569,0.300917431,0.302752294,0.304587156,
0.306422018,0.308256881,0.310091743,0.311926606,0.313761468,0.31559633,
0.317431193,0.319266055,0.321100917,0.32293578,0.324770642,0.326605505,
0.328440367,0.330275229,0.332110092,0.333944954,0.335779817,0.337614679,
0.339449541,0.341284404,0.343119266,0.344954128,0.346788991,0.348623853,
0.350458716,0.352293578,0.35412844,0.355963303,0.357798165,0.359633028,
0.36146789,0.363302752,0.365137615,0.366972477,0.368807339,0.370642202,
0.372477064,0.374311927,0.376146789,0.377981651,0.379816514,0.381651376,
0.383486239,0.385321101,0.387155963,0.388990826,0.390825688,0.39266055,
0.394495413,0.396330275,0.398165138,0.4,0.401834862,0.403669725,0.405504587,
0.40733945,0.409174312,0.411009174,0.412844037,0.414678899,0.416513761,
0.418348624,0.420183486,0.422018349,0.423853211,0.425688073,0.427522936,
0.429357798,0.431192661,0.433027523,0.434862385,0.436697248,0.43853211,
0.440366972,0.442201835,0.444036697,0.44587156,0.447706422,0.449541284,
0.451376147,0.453211009,0.455045872,0.456880734,0.458715596,0.460550459,
0.462385321,0.464220183,0.466055046,0.467889908,0.469724771,0.471559633,
0.473394495,0.475229358,0.47706422,0.478899083,0.480733945,0.482568807,
0.48440367,0.486238532,0.488073394,0.489908257,0.491743119,0.493577982,
0.495412844,0.497247706,0.499082569,0.500917431,0.502752294,0.504587156,
0.506422018,0.508256881,0.510091743,0.511926606,0.513761468,0.51559633,
0.517431193,0.519266055,0.521100917,0.52293578,0.524770642,0.526605505,
0.528440367,0.530275229,0.532110092,0.533944954,0.535779817,0.537614679,
0.539449541,0.541284404,0.543119266,0.544954128,0.546788991,0.548623853,
0.550458716,0.552293578,0.55412844,0.555963303,0.557798165,0.559633028,
0.56146789,0.563302752,0.565137615,0.566972477,0.568807339,0.570642202,
0.572477064,0.574311927,0.576146789,0.577981651,0.579816514,0.581651376,
0.583486239,0.585321101,0.587155963,0.588990826,0.590825688,0.59266055,
0.594495413,0.596330275,0.598165138,0.6,0.601834862,0.603669725,0.605504587,
0.60733945,0.609174312,0.611009174,0.612844037,0.614678899,0.616513761,
0.618348624,0.620183486,0.622018349,0.623853211,0.625688073,0.627522936,
0.629357798,0.631192661,0.633027523,0.634862385,0.636697248,0.63853211,
0.640366972,0.642201835,0.644036697,0.64587156,0.647706422,0.649541284,
0.651376147,0.653211009,0.655045872,0.656880734,0.658715596,0.660550459,
0.662385321,0.664220183,0.666055046,0.667889908,0.669724771,0.671559633,
0.673394495,0.675229358,0.67706422,0.678899083,0.680733945,0.682568807,
0.68440367,0.686238532,0.688073394,0.689908257,0.691743119,0.693577982,
0.695412844,0.697247706,0.699082569,0.700917431,0.702752294,0.704587156,
0.706422018,0.708256881,0.710091743,0.711926606,0.713761468,0.71559633,
0.717431193,0.719266055,0.721100917,0.72293578,0.724770642,0.726605505,
0.728440367,0.730275229,0.732110092,0.733944954,0.735779817,0.737614679,
0.739449541,0.741284404,0.743119266,0.744954128,0.746788991,0.748623853,
0.750458716,0.752293578,0.75412844,0.755963303,0.757798165,0.759633028,
0.76146789,0.763302752,0.765137615,0.766972477,0.768807339,0.770642202,
0.772477064,0.774311927,0.776146789,0.777981651,0.779816514,0.781651376,
0.783486239,0.785321101,0.787155963,0.788990826,0.790825688,0.79266055,
0.794495413,0.796330275,0.798165138,0.8,0.801834862,0.803669725,0.805504587,
0.80733945,0.809174312,0.811009174,0.812844037,0.814678899,0.816513761,
0.818348624,0.820183486,0.822018349,0.823853211,0.825688073,0.827522936,
0.829357798,0.831192661,0.833027523,0.834862385,0.836697248,0.83853211,
0.840366972,0.842201835,0.844036697,0.84587156,0.847706422,0.849541284,
0.851376147,0.853211009,0.855045872,0.856880734,0.858715596,0.860550459,
0.862385321,0.864220183,0.866055046,0.867889908,0.869724771,0.871559633,
0.873394495,0.875229358,0.87706422,0.878899083,0.880733945,0.882568807,
0.88440367,0.886238532,0.888073394,0.889908257,0.891743119,0.893577982,
0.895412844,0.897247706,0.899082569,0.900917431,0.902752294,0.904587156,
0.906422018,0.908256881,0.910091743,0.911926606,0.913761468,0.91559633,
0.917431193,0.919266055,0.921100917,0.92293578,0.924770642,0.926605505,
0.928440367,0.930275229,0.932110092,0.933944954,0.935779817,0.937614679,
0.939449541,0.941284404,0.943119266,0.944954128,0.946788991,0.948623853,
0.950458716,0.952293578,0.95412844,0.955963303,0.957798165,0.959633028,
0.96146789,0.963302752,0.965137615,0.966972477,0.968807339,0.970642202,
0.972477064,0.974311927,0.976146789,0.977981651,0.979816514,0.981651376,
0.983486239,0.985321101,0.987155963,0.988990826,0.990825688,0.99266055,
0.994495413,0.996330275,0.998165138,1.),.UNSPECIFIED.);
#24430=B_SPLINE_CURVE_WITH_KNOTS('',5,(#245778,#245779,#245780,#245781,
#245782,#245783,#245784,#245785,#245786,#245787,#245788,#245789,#245790,
#245791,#245792,#245793,#245794,#245795,#245796,#245797,#245798,#245799,
#245800,#245801,#245802,#245803,#245804,#245805,#245806,#245807,#245808,
#245809,#245810,#245811,#245812,#245813,#245814,#245815,#245816,#245817,
#245818,#245819,#245820,#245821,#245822,#245823,#245824,#245825,#245826,
#245827,#245828,#245829,#245830,#245831,#245832,#245833,#245834,#245835,
#245836,#245837,#245838,#245839,#245840,#245841,#245842,#245843,#245844,
#245845,#245846,#245847,#245848,#245849,#245850,#245851,#245852,#245853,
#245854,#245855,#245856,#245857,#245858,#245859,#245860,#245861,#245862,
#245863,#245864,#245865,#245866,#245867,#245868,#245869,#245870,#245871,
#245872,#245873,#245874,#245875,#245876,#245877,#245878,#245879,#245880,
#245881,#245882,#245883,#245884,#245885,#245886,#245887,#245888,#245889,
#245890,#245891,#245892,#245893,#245894,#245895,#245896,#245897,#245898,
#245899,#245900,#245901,#245902,#245903,#245904,#245905,#245906,#245907,
#245908,#245909,#245910,#245911,#245912,#245913,#245914,#245915,#245916,
#245917,#245918,#245919,#245920,#245921,#245922,#245923,#245924,#245925,
#245926,#245927,#245928,#245929,#245930,#245931,#245932,#245933,#245934,
#245935,#245936,#245937,#245938,#245939,#245940,#245941,#245942,#245943,
#245944,#245945,#245946,#245947,#245948,#245949,#245950,#245951,#245952,
#245953,#245954,#245955,#245956,#245957,#245958,#245959,#245960,#245961,
#245962,#245963,#245964,#245965,#245966,#245967,#245968,#245969,#245970,
#245971,#245972,#245973,#245974,#245975,#245976,#245977,#245978,#245979,
#245980,#245981,#245982,#245983,#245984,#245985,#245986,#245987,#245988,
#245989,#245990,#245991,#245992,#245993,#245994,#245995,#245996,#245997,
#245998,#245999,#246000,#246001,#246002,#246003,#246004,#246005,#246006,
#246007,#246008,#246009,#246010,#246011,#246012,#246013,#246014,#246015,
#246016,#246017,#246018,#246019,#246020,#246021,#246022,#246023,#246024,
#246025,#246026,#246027,#246028,#246029,#246030,#246031,#246032,#246033,
#246034,#246035,#246036,#246037,#246038,#246039,#246040,#246041,#246042,
#246043,#246044,#246045,#246046,#246047,#246048,#246049,#246050,#246051,
#246052,#246053,#246054,#246055,#246056,#246057,#246058,#246059,#246060,
#246061,#246062,#246063,#246064,#246065,#246066,#246067,#246068,#246069,
#246070,#246071,#246072,#246073,#246074,#246075,#246076,#246077,#246078,
#246079,#246080,#246081,#246082,#246083,#246084,#246085,#246086,#246087,
#246088,#246089,#246090,#246091,#246092,#246093,#246094,#246095,#246096,
#246097,#246098,#246099,#246100,#246101,#246102,#246103,#246104,#246105,
#246106,#246107,#246108,#246109,#246110,#246111,#246112,#246113,#246114,
#246115,#246116,#246117,#246118,#246119,#246120,#246121,#246122,#246123,
#246124,#246125,#246126,#246127,#246128,#246129,#246130,#246131,#246132,
#246133,#246134,#246135,#246136,#246137,#246138,#246139,#246140,#246141,
#246142,#246143,#246144,#246145,#246146,#246147,#246148,#246149,#246150,
#246151,#246152,#246153,#246154,#246155,#246156,#246157,#246158,#246159,
#246160,#246161,#246162,#246163,#246164,#246165,#246166,#246167,#246168,
#246169,#246170,#246171,#246172,#246173,#246174,#246175,#246176,#246177,
#246178,#246179,#246180,#246181,#246182,#246183,#246184,#246185,#246186,
#246187,#246188,#246189,#246190,#246191,#246192,#246193,#246194,#246195,
#246196,#246197,#246198,#246199,#246200,#246201,#246202,#246203,#246204,
#246205,#246206,#246207,#246208,#246209,#246210,#246211,#246212,#246213,
#246214,#246215,#246216,#246217,#246218,#246219,#246220,#246221,#246222,
#246223,#246224,#246225,#246226,#246227,#246228,#246229,#246230,#246231,
#246232,#246233,#246234,#246235,#246236,#246237,#246238,#246239,#246240,
#246241,#246242,#246243,#246244,#246245,#246246,#246247,#246248,#246249),
 .UNSPECIFIED.,.F.,.F.,(6,1,1,1,1,1,1,1,1,1,1,1,1,1,1,1,1,1,1,1,1,1,1,1,
1,1,1,1,1,1,1,1,1,1,1,1,1,1,1,1,1,1,1,1,1,1,1,1,1,1,1,1,1,1,1,1,1,1,1,1,
1,1,1,1,1,1,1,1,1,1,1,1,1,1,1,1,1,1,1,1,1,1,1,1,1,1,1,1,1,1,1,1,1,1,1,1,
1,1,1,1,1,1,1,1,1,1,1,1,1,1,1,1,1,1,1,1,1,1,1,1,1,1,1,1,1,1,1,1,1,1,1,1,
1,1,1,1,1,1,1,1,1,1,1,1,1,1,1,1,1,1,1,1,1,1,1,1,1,1,1,1,1,1,1,1,1,1,1,1,
1,1,1,1,1,1,1,1,1,1,1,1,1,1,1,1,1,1,1,1,1,1,1,1,1,1,1,1,1,1,1,1,1,1,1,1,
1,1,1,1,1,1,1,1,1,1,1,1,1,1,1,1,1,1,1,1,1,1,1,1,1,1,1,1,1,1,1,1,1,1,1,1,
1,1,1,1,1,1,1,1,1,1,1,1,1,1,1,1,1,1,1,1,1,1,1,1,1,1,1,1,1,1,1,1,1,1,1,1,
1,1,1,1,1,1,1,1,1,1,1,1,1,1,1,1,1,1,1,1,1,1,1,1,1,1,1,1,1,1,1,1,1,1,1,1,
1,1,1,1,1,1,1,1,1,1,1,1,1,1,1,1,1,1,1,1,1,1,1,1,1,1,1,1,1,1,1,1,1,1,1,1,
1,1,1,1,1,1,1,1,1,1,1,1,1,1,1,1,1,1,1,1,1,1,1,1,1,1,1,1,1,1,1,1,1,1,1,1,
1,1,1,1,1,1,1,1,1,1,1,1,1,1,1,1,1,1,1,1,1,1,1,1,1,1,1,1,1,1,1,1,1,1,1,1,
1,1,1,1,1,1,1,1,1,1,1,1,1,1,1,1,1,1,1,1,1,1,1,1,1,1,1,1,1,1,1,1,1,1,1,1,
1,1,1,1,1,1,1,1,1,1,1,6),(0.143172102,0.144954128,0.146788991,0.148623853,
0.150458716,0.152293578,0.15412844,0.155963303,0.157798165,0.159633028,
0.16146789,0.163302752,0.165137615,0.166972477,0.168807339,0.170642202,
0.172477064,0.174311927,0.176146789,0.177981651,0.179816514,0.181651376,
0.183486239,0.185321101,0.187155963,0.188990826,0.190825688,0.19266055,
0.194495413,0.196330275,0.198165138,0.2,0.201834862,0.203669725,0.205504587,
0.20733945,0.209174312,0.211009174,0.212844037,0.214678899,0.216513761,
0.218348624,0.220183486,0.222018349,0.223853211,0.225688073,0.227522936,
0.229357798,0.231192661,0.233027523,0.234862385,0.236697248,0.23853211,
0.240366972,0.242201835,0.244036697,0.24587156,0.247706422,0.249541284,
0.251376147,0.253211009,0.255045872,0.256880734,0.258715596,0.260550459,
0.262385321,0.264220183,0.266055046,0.267889908,0.269724771,0.271559633,
0.273394495,0.275229358,0.27706422,0.278899083,0.280733945,0.282568807,
0.28440367,0.286238532,0.288073394,0.289908257,0.291743119,0.293577982,
0.295412844,0.297247706,0.299082569,0.300917431,0.302752294,0.304587156,
0.306422018,0.308256881,0.310091743,0.311926606,0.313761468,0.31559633,
0.317431193,0.319266055,0.321100917,0.32293578,0.324770642,0.326605505,
0.328440367,0.330275229,0.332110092,0.333944954,0.335779817,0.337614679,
0.339449541,0.341284404,0.343119266,0.344954128,0.346788991,0.348623853,
0.350458716,0.352293578,0.35412844,0.355963303,0.357798165,0.359633028,
0.36146789,0.363302752,0.365137615,0.366972477,0.368807339,0.370642202,
0.372477064,0.374311927,0.376146789,0.377981651,0.379816514,0.381651376,
0.383486239,0.385321101,0.387155963,0.388990826,0.390825688,0.39266055,
0.394495413,0.396330275,0.398165138,0.4,0.401834862,0.403669725,0.405504587,
0.40733945,0.409174312,0.411009174,0.412844037,0.414678899,0.416513761,
0.418348624,0.420183486,0.422018349,0.423853211,0.425688073,0.427522936,
0.429357798,0.431192661,0.433027523,0.434862385,0.436697248,0.43853211,
0.440366972,0.442201835,0.444036697,0.44587156,0.447706422,0.449541284,
0.451376147,0.453211009,0.455045872,0.456880734,0.458715596,0.460550459,
0.462385321,0.464220183,0.466055046,0.467889908,0.469724771,0.471559633,
0.473394495,0.475229358,0.47706422,0.478899083,0.480733945,0.482568807,
0.48440367,0.486238532,0.488073394,0.489908257,0.491743119,0.493577982,
0.495412844,0.497247706,0.499082569,0.500917431,0.502752294,0.504587156,
0.506422018,0.508256881,0.510091743,0.511926606,0.513761468,0.51559633,
0.517431193,0.519266055,0.521100917,0.52293578,0.524770642,0.526605505,
0.528440367,0.530275229,0.532110092,0.533944954,0.535779817,0.537614679,
0.539449541,0.541284404,0.543119266,0.544954128,0.546788991,0.548623853,
0.550458716,0.552293578,0.55412844,0.555963303,0.557798165,0.559633028,
0.56146789,0.563302752,0.565137615,0.566972477,0.568807339,0.570642202,
0.572477064,0.574311927,0.576146789,0.577981651,0.579816514,0.581651376,
0.583486239,0.585321101,0.587155963,0.588990826,0.590825688,0.59266055,
0.594495413,0.596330275,0.598165138,0.6,0.601834862,0.603669725,0.605504587,
0.60733945,0.609174312,0.611009174,0.612844037,0.614678899,0.616513761,
0.618348624,0.620183486,0.622018349,0.623853211,0.625688073,0.627522936,
0.629357798,0.631192661,0.633027523,0.634862385,0.636697248,0.63853211,
0.640366972,0.642201835,0.644036697,0.64587156,0.647706422,0.649541284,
0.651376147,0.653211009,0.655045872,0.656880734,0.658715596,0.660550459,
0.662385321,0.664220183,0.666055046,0.667889908,0.669724771,0.671559633,
0.673394495,0.675229358,0.67706422,0.678899083,0.680733945,0.682568807,
0.68440367,0.686238532,0.688073394,0.689908257,0.691743119,0.693577982,
0.695412844,0.697247706,0.699082569,0.700917431,0.702752294,0.704587156,
0.706422018,0.708256881,0.710091743,0.711926606,0.713761468,0.71559633,
0.717431193,0.719266055,0.721100917,0.72293578,0.724770642,0.726605505,
0.728440367,0.730275229,0.732110092,0.733944954,0.735779817,0.737614679,
0.739449541,0.741284404,0.743119266,0.744954128,0.746788991,0.748623853,
0.750458716,0.752293578,0.75412844,0.755963303,0.757798165,0.759633028,
0.76146789,0.763302752,0.765137615,0.766972477,0.768807339,0.770642202,
0.772477064,0.774311927,0.776146789,0.777981651,0.779816514,0.781651376,
0.783486239,0.785321101,0.787155963,0.788990826,0.790825688,0.79266055,
0.794495413,0.796330275,0.798165138,0.8,0.801834862,0.803669725,0.805504587,
0.80733945,0.809174312,0.811009174,0.812844037,0.814678899,0.816513761,
0.818348624,0.820183486,0.822018349,0.823853211,0.825688073,0.827522936,
0.829357798,0.831192661,0.833027523,0.834862385,0.836697248,0.83853211,
0.840366972,0.842201835,0.844036697,0.84587156,0.847706422,0.849541284,
0.851376147,0.853211009,0.855045872,0.856880734,0.858715596,0.860550459,
0.862385321,0.864220183,0.866055046,0.867889908,0.869724771,0.871559633,
0.873394495,0.875229358,0.87706422,0.878899083,0.880733945,0.882568807,
0.88440367,0.886238532,0.888073394,0.889908257,0.891743119,0.893577982,
0.895412844,0.897247706,0.899082569,0.900917431,0.902752294,0.904587156,
0.906422018,0.908256881,0.910091743,0.911926606,0.913761468,0.91559633,
0.917431193,0.919266055,0.921100917,0.92293578,0.924770642,0.926605505,
0.928440367,0.930275229,0.932110092,0.933944954,0.935779817,0.937614679,
0.939449541,0.941284404,0.943119266,0.944954128,0.946788991,0.948623853,
0.950458716,0.952293578,0.95412844,0.955963303,0.957798165,0.959633028,
0.96146789,0.963302752,0.965137615,0.966972477,0.968807339,0.970642202,
0.972477064,0.974311927,0.976146789,0.977981651,0.979816514,0.981651376,
0.983486239,0.985321101,0.987155963,0.988990826,0.990825688,0.99266055,
0.994495413,0.996330275,0.998165138,1.),.UNSPECIFIED.);
#24431=B_SPLINE_CURVE_WITH_KNOTS('',3,(#247209,#247210,#247211,#247212,
#247213,#247214,#247215,#247216,#247217,#247218,#247219,#247220,#247221,
#247222,#247223,#247224,#247225,#247226,#247227,#247228,#247229,#247230,
#247231,#247232,#247233,#247234,#247235,#247236,#247237,#247238,#247239,
#247240,#247241,#247242,#247243,#247244,#247245,#247246,#247247,#247248,
#247249,#247250,#247251,#247252,#247253,#247254,#247255,#247256,#247257,
#247258,#247259,#247260,#247261,#247262,#247263,#247264,#247265,#247266,
#247267,#247268,#247269,#247270,#247271,#247272,#247273,#247274,#247275,
#247276,#247277,#247278,#247279,#247280,#247281,#247282,#247283,#247284,
#247285,#247286,#247287,#247288,#247289,#247290,#247291,#247292,#247293,
#247294,#247295,#247296,#247297,#247298,#247299,#247300,#247301,#247302,
#247303,#247304,#247305,#247306,#247307,#247308,#247309,#247310,#247311,
#247312,#247313,#247314,#247315,#247316,#247317,#247318,#247319,#247320,
#247321,#247322,#247323,#247324,#247325,#247326,#247327,#247328,#247329,
#247330,#247331,#247332,#247333,#247334,#247335,#247336,#247337,#247338,
#247339,#247340,#247341,#247342,#247343,#247344,#247345,#247346,#247347,
#247348,#247349,#247350,#247351,#247352,#247353,#247354,#247355,#247356,
#247357,#247358,#247359,#247360,#247361,#247362,#247363,#247364,#247365,
#247366,#247367,#247368,#247369,#247370,#247371,#247372,#247373,#247374,
#247375,#247376,#247377,#247378,#247379,#247380,#247381,#247382,#247383,
#247384,#247385,#247386,#247387,#247388,#247389,#247390,#247391,#247392,
#247393,#247394,#247395,#247396,#247397,#247398,#247399,#247400,#247401,
#247402,#247403,#247404,#247405,#247406,#247407,#247408,#247409,#247410,
#247411,#247412,#247413,#247414,#247415,#247416,#247417,#247418,#247419,
#247420,#247421,#247422,#247423,#247424,#247425,#247426,#247427,#247428,
#247429,#247430,#247431,#247432,#247433,#247434,#247435,#247436,#247437,
#247438,#247439,#247440,#247441,#247442,#247443,#247444,#247445,#247446,
#247447,#247448,#247449,#247450,#247451,#247452,#247453,#247454,#247455,
#247456,#247457,#247458,#247459,#247460,#247461,#247462,#247463,#247464,
#247465,#247466,#247467,#247468,#247469,#247470,#247471,#247472,#247473,
#247474,#247475,#247476,#247477,#247478,#247479,#247480,#247481,#247482,
#247483,#247484,#247485,#247486,#247487,#247488,#247489,#247490,#247491,
#247492,#247493,#247494,#247495,#247496,#247497,#247498,#247499,#247500,
#247501,#247502,#247503,#247504,#247505,#247506,#247507,#247508,#247509,
#247510,#247511,#247512,#247513,#247514,#247515,#247516,#247517,#247518,
#247519,#247520,#247521),.UNSPECIFIED.,.F.,.F.,(4,3,3,3,3,3,3,3,3,3,3,3,
3,3,3,3,3,3,3,3,3,3,3,3,3,3,3,3,3,3,3,3,3,3,3,3,3,3,3,3,3,3,3,3,3,3,3,3,
3,3,3,3,3,3,3,3,3,3,3,3,3,3,3,3,3,3,3,3,3,3,3,3,3,3,3,3,3,3,3,3,3,3,3,3,
3,3,3,3,3,3,3,3,3,3,3,3,3,3,3,3,3,3,3,3,4),(0.143172102,0.15412844,0.165137615,
0.176146789,0.187155963,0.198165138,0.209174312,0.220183486,0.231192661,
0.242201835,0.253211009,0.264220183,0.275229358,0.286238532,0.297247706,
0.308256881,0.319266055,0.330275229,0.341284404,0.352293578,0.363302752,
0.374311927,0.385321101,0.396330275,0.405504587,0.414678899,0.423853211,
0.434862385,0.444036697,0.453211009,0.462385321,0.471559633,0.480733945,
0.489908257,0.499082569,0.508256881,0.517431193,0.526605505,0.535779817,
0.543119266,0.550458716,0.557798165,0.565137615,0.572477064,0.579816514,
0.587155963,0.594495413,0.603669725,0.611009174,0.618348624,0.625688073,
0.634862385,0.644036697,0.653211009,0.662385321,0.669724771,0.67706422,
0.68440367,0.691743119,0.702752294,0.710091743,0.717431193,0.726605505,
0.733944954,0.741284404,0.752293578,0.759633028,0.768807339,0.779816514,
0.787155963,0.794495413,0.801834862,0.809174312,0.814678899,0.820183486,
0.827522936,0.833027523,0.840366972,0.84587156,0.851376147,0.856880734,
0.862385321,0.867889908,0.873394495,0.878899083,0.888073394,0.895412844,
0.900917431,0.908256881,0.91559633,0.921100917,0.926605505,0.933944954,
0.939449541,0.944954128,0.950458716,0.955963303,0.96146789,0.966972477,
0.972477064,0.977981651,0.983486239,0.988990826,0.994495413,1.),
 .UNSPECIFIED.);
#24432=B_SPLINE_CURVE_WITH_KNOTS('',3,(#247522,#247523,#247524,#247525,
#247526,#247527,#247528,#247529,#247530,#247531,#247532,#247533,#247534,
#247535,#247536,#247537,#247538,#247539,#247540,#247541,#247542,#247543,
#247544,#247545,#247546,#247547,#247548,#247549,#247550,#247551,#247552,
#247553,#247554,#247555,#247556,#247557,#247558,#247559,#247560,#247561,
#247562,#247563,#247564,#247565,#247566,#247567,#247568,#247569,#247570,
#247571,#247572,#247573,#247574,#247575,#247576,#247577,#247578,#247579,
#247580,#247581,#247582,#247583,#247584,#247585,#247586,#247587,#247588,
#247589,#247590,#247591,#247592,#247593,#247594,#247595,#247596,#247597,
#247598,#247599,#247600,#247601,#247602,#247603,#247604,#247605,#247606,
#247607,#247608,#247609,#247610,#247611,#247612,#247613,#247614,#247615,
#247616,#247617,#247618,#247619,#247620,#247621,#247622,#247623,#247624,
#247625,#247626,#247627,#247628,#247629,#247630,#247631,#247632,#247633,
#247634,#247635,#247636,#247637,#247638,#247639,#247640,#247641,#247642,
#247643,#247644,#247645,#247646,#247647,#247648,#247649,#247650,#247651,
#247652,#247653,#247654,#247655,#247656,#247657,#247658,#247659,#247660,
#247661,#247662,#247663,#247664,#247665,#247666,#247667,#247668,#247669,
#247670,#247671,#247672,#247673,#247674,#247675,#247676,#247677,#247678,
#247679,#247680,#247681,#247682,#247683,#247684,#247685,#247686,#247687,
#247688,#247689,#247690,#247691,#247692,#247693,#247694,#247695,#247696,
#247697,#247698,#247699,#247700,#247701,#247702,#247703,#247704,#247705,
#247706,#247707,#247708,#247709,#247710,#247711,#247712,#247713,#247714,
#247715,#247716,#247717,#247718,#247719,#247720,#247721,#247722,#247723,
#247724,#247725,#247726,#247727,#247728,#247729,#247730,#247731,#247732,
#247733,#247734,#247735,#247736,#247737,#247738,#247739,#247740,#247741,
#247742,#247743,#247744,#247745,#247746,#247747,#247748,#247749,#247750,
#247751,#247752,#247753,#247754,#247755,#247756,#247757,#247758,#247759,
#247760,#247761,#247762,#247763,#247764,#247765,#247766,#247767,#247768,
#247769,#247770,#247771,#247772,#247773,#247774,#247775,#247776,#247777,
#247778,#247779,#247780,#247781,#247782,#247783,#247784,#247785,#247786,
#247787,#247788,#247789,#247790,#247791,#247792,#247793,#247794,#247795,
#247796,#247797,#247798,#247799,#247800,#247801,#247802,#247803,#247804,
#247805,#247806,#247807,#247808,#247809,#247810,#247811,#247812,#247813,
#247814,#247815,#247816,#247817,#247818,#247819,#247820,#247821,#247822,
#247823,#247824,#247825,#247826,#247827,#247828,#247829,#247830,#247831,
#247832,#247833,#247834,#247835,#247836,#247837,#247838,#247839,#247840,
#247841,#247842,#247843),.UNSPECIFIED.,.F.,.F.,(4,3,3,3,3,3,3,3,3,3,3,3,
3,3,3,3,3,3,3,3,3,3,3,3,3,3,3,3,3,3,3,3,3,3,3,3,3,3,3,3,3,3,3,3,3,3,3,3,
3,3,3,3,3,3,3,3,3,3,3,3,3,3,3,3,3,3,3,3,3,3,3,3,3,3,3,3,3,3,3,3,3,3,3,3,
3,3,3,3,3,3,3,3,3,3,3,3,3,3,3,3,3,3,3,3,3,3,3,4),(0.143172102,0.15412844,
0.165137615,0.176146789,0.187155963,0.198165138,0.209174312,0.220183486,
0.231192661,0.242201835,0.253211009,0.264220183,0.275229358,0.286238532,
0.297247706,0.308256881,0.319266055,0.330275229,0.341284404,0.352293578,
0.363302752,0.374311927,0.385321101,0.396330275,0.405504587,0.414678899,
0.423853211,0.433027523,0.442201835,0.451376147,0.460550459,0.469724771,
0.478899083,0.488073394,0.497247706,0.508256881,0.517431193,0.526605505,
0.533944954,0.541284404,0.548623853,0.555963303,0.563302752,0.570642202,
0.577981651,0.585321101,0.59266055,0.6,0.60733945,0.614678899,0.622018349,
0.629357798,0.636697248,0.644036697,0.651376147,0.658715596,0.667889908,
0.675229358,0.682568807,0.689908257,0.697247706,0.704587156,0.711926606,
0.719266055,0.726605505,0.733944954,0.744954128,0.752293578,0.759633028,
0.768807339,0.776146789,0.783486239,0.790825688,0.798165138,0.805504587,
0.811009174,0.816513761,0.822018349,0.827522936,0.834862385,0.840366972,
0.84587156,0.851376147,0.856880734,0.862385321,0.867889908,0.873394495,
0.878899083,0.888073394,0.895412844,0.900917431,0.906422018,0.911926606,
0.917431193,0.924770642,0.930275229,0.935779817,0.941284404,0.946788991,
0.952293578,0.957798165,0.963302752,0.968807339,0.974311927,0.979816514,
0.985321101,0.994495413,1.),.UNSPECIFIED.);
#24433=B_SPLINE_CURVE_WITH_KNOTS('',3,(#248791,#248792,#248793,#248794,
#248795,#248796,#248797,#248798,#248799,#248800,#248801,#248802,#248803,
#248804,#248805,#248806,#248807,#248808,#248809,#248810,#248811,#248812,
#248813,#248814,#248815,#248816,#248817,#248818,#248819,#248820,#248821,
#248822,#248823,#248824,#248825,#248826,#248827,#248828,#248829,#248830,
#248831,#248832,#248833,#248834,#248835,#248836,#248837,#248838,#248839,
#248840,#248841,#248842,#248843,#248844,#248845,#248846,#248847,#248848,
#248849,#248850,#248851,#248852,#248853,#248854,#248855,#248856,#248857,
#248858,#248859,#248860,#248861,#248862,#248863,#248864,#248865,#248866,
#248867,#248868,#248869,#248870,#248871,#248872,#248873,#248874,#248875,
#248876,#248877,#248878,#248879,#248880,#248881,#248882,#248883,#248884,
#248885,#248886,#248887,#248888,#248889,#248890,#248891,#248892,#248893,
#248894,#248895,#248896,#248897,#248898,#248899,#248900,#248901,#248902,
#248903,#248904,#248905,#248906,#248907,#248908,#248909,#248910,#248911,
#248912,#248913,#248914,#248915,#248916,#248917,#248918,#248919,#248920,
#248921,#248922,#248923,#248924,#248925,#248926,#248927,#248928,#248929,
#248930,#248931,#248932,#248933,#248934,#248935,#248936,#248937,#248938,
#248939,#248940,#248941,#248942,#248943,#248944,#248945,#248946,#248947,
#248948,#248949,#248950,#248951,#248952,#248953,#248954,#248955,#248956,
#248957,#248958,#248959,#248960,#248961,#248962,#248963,#248964,#248965,
#248966,#248967,#248968,#248969,#248970,#248971,#248972,#248973,#248974,
#248975,#248976,#248977,#248978,#248979,#248980,#248981,#248982,#248983,
#248984,#248985,#248986,#248987,#248988,#248989,#248990,#248991,#248992,
#248993,#248994,#248995,#248996,#248997,#248998,#248999,#249000,#249001,
#249002,#249003,#249004,#249005,#249006,#249007,#249008,#249009,#249010,
#249011,#249012,#249013,#249014,#249015,#249016,#249017,#249018,#249019,
#249020,#249021,#249022,#249023,#249024,#249025,#249026,#249027,#249028,
#249029,#249030,#249031,#249032,#249033,#249034,#249035,#249036,#249037,
#249038,#249039,#249040,#249041,#249042,#249043,#249044,#249045,#249046,
#249047,#249048,#249049,#249050,#249051,#249052,#249053,#249054,#249055,
#249056,#249057,#249058,#249059,#249060,#249061,#249062,#249063,#249064,
#249065,#249066,#249067,#249068,#249069,#249070,#249071,#249072,#249073,
#249074,#249075,#249076,#249077,#249078,#249079,#249080,#249081,#249082,
#249083,#249084,#249085,#249086,#249087,#249088,#249089,#249090,#249091,
#249092,#249093,#249094,#249095,#249096,#249097,#249098,#249099,#249100,
#249101,#249102,#249103,#249104,#249105,#249106,#249107,#249108,#249109,
#249110,#249111,#249112,#249113,#249114,#249115),.UNSPECIFIED.,.F.,.F.,
(4,3,3,3,3,3,3,3,3,3,3,3,3,3,3,3,3,3,3,3,3,3,3,3,3,3,3,3,3,3,3,3,3,3,3,
3,3,3,3,3,3,3,3,3,3,3,3,3,3,3,3,3,3,3,3,3,3,3,3,3,3,3,3,3,3,3,3,3,3,3,3,
3,3,3,3,3,3,3,3,3,3,3,3,3,3,3,3,3,3,3,3,3,3,3,3,3,3,3,3,3,3,3,3,3,3,3,3,
3,4),(-1.,-0.994495413,-0.988990826,-0.983486239,-0.977981651,-0.970642202,
-0.965137615,-0.959633028,-0.95412844,-0.948623853,-0.943119266,-0.937614679,
-0.932110092,-0.926605505,-0.921100917,-0.91559633,-0.910091743,-0.904587156,
-0.899082569,-0.893577982,-0.886238532,-0.880733945,-0.875229358,-0.869724771,
-0.864220183,-0.858715596,-0.853211009,-0.847706422,-0.842201835,-0.836697248,
-0.831192661,-0.825688073,-0.818348624,-0.812844037,-0.80733945,-0.8,-0.79266055,
-0.785321101,-0.777981651,-0.770642202,-0.763302752,-0.755963303,-0.748623853,
-0.741284404,-0.733944954,-0.726605505,-0.719266055,-0.710091743,-0.702752294,
-0.695412844,-0.688073394,-0.678899083,-0.671559633,-0.664220183,-0.656880734,
-0.649541284,-0.642201835,-0.634862385,-0.627522936,-0.620183486,-0.612844037,
-0.605504587,-0.598165138,-0.590825688,-0.583486239,-0.576146789,-0.568807339,
-0.559633028,-0.552293578,-0.544954128,-0.537614679,-0.530275229,-0.521100917,
-0.511926606,-0.502752294,-0.493577982,-0.478899083,-0.469724771,-0.460550459,
-0.451376147,-0.442201835,-0.433027523,-0.423853211,-0.414678899,-0.405504587,
-0.396330275,-0.387155963,-0.374311927,-0.363302752,-0.352293578,-0.341284404,
-0.330275229,-0.319266055,-0.308256881,-0.297247706,-0.286238532,-0.275229358,
-0.264220183,-0.253211009,-0.242201835,-0.231192661,-0.220183486,-0.209174312,
-0.198165138,-0.187155963,-0.176146789,-0.165137615,-0.15412844,-0.143172102),
 .UNSPECIFIED.);
#24434=B_SPLINE_CURVE_WITH_KNOTS('',3,(#249116,#249117,#249118,#249119,
#249120,#249121,#249122,#249123,#249124,#249125,#249126,#249127,#249128,
#249129,#249130,#249131,#249132,#249133,#249134,#249135,#249136,#249137,
#249138,#249139,#249140,#249141,#249142,#249143,#249144,#249145,#249146,
#249147,#249148,#249149,#249150,#249151,#249152,#249153,#249154,#249155,
#249156,#249157,#249158,#249159,#249160,#249161,#249162,#249163,#249164,
#249165,#249166,#249167,#249168,#249169,#249170,#249171,#249172,#249173,
#249174,#249175,#249176,#249177,#249178,#249179,#249180,#249181,#249182,
#249183,#249184,#249185,#249186,#249187,#249188,#249189,#249190,#249191,
#249192,#249193,#249194,#249195,#249196,#249197,#249198,#249199,#249200,
#249201,#249202,#249203,#249204,#249205,#249206,#249207,#249208,#249209,
#249210,#249211,#249212,#249213,#249214,#249215,#249216,#249217,#249218,
#249219,#249220,#249221,#249222,#249223,#249224,#249225,#249226,#249227,
#249228,#249229,#249230,#249231,#249232,#249233,#249234,#249235,#249236,
#249237,#249238,#249239,#249240,#249241,#249242,#249243,#249244,#249245,
#249246,#249247,#249248,#249249,#249250,#249251,#249252,#249253,#249254,
#249255,#249256,#249257,#249258,#249259,#249260,#249261,#249262,#249263,
#249264,#249265,#249266,#249267,#249268,#249269,#249270,#249271,#249272,
#249273,#249274,#249275,#249276,#249277,#249278,#249279,#249280,#249281,
#249282,#249283,#249284,#249285,#249286,#249287,#249288,#249289,#249290,
#249291,#249292,#249293,#249294,#249295,#249296,#249297,#249298,#249299,
#249300,#249301,#249302,#249303,#249304,#249305,#249306,#249307,#249308,
#249309,#249310,#249311,#249312,#249313,#249314,#249315,#249316,#249317,
#249318,#249319,#249320,#249321,#249322,#249323,#249324,#249325,#249326,
#249327,#249328,#249329,#249330,#249331,#249332,#249333,#249334,#249335,
#249336,#249337,#249338,#249339,#249340,#249341,#249342,#249343,#249344,
#249345,#249346,#249347,#249348,#249349,#249350,#249351,#249352,#249353,
#249354,#249355,#249356,#249357,#249358,#249359,#249360,#249361,#249362,
#249363,#249364,#249365,#249366,#249367,#249368,#249369,#249370,#249371,
#249372,#249373,#249374,#249375,#249376,#249377,#249378,#249379,#249380,
#249381,#249382,#249383,#249384,#249385,#249386,#249387,#249388,#249389,
#249390,#249391,#249392,#249393,#249394,#249395,#249396,#249397,#249398,
#249399,#249400,#249401,#249402,#249403,#249404,#249405,#249406,#249407,
#249408,#249409,#249410,#249411,#249412,#249413,#249414,#249415,#249416,
#249417,#249418,#249419,#249420,#249421,#249422),.UNSPECIFIED.,.F.,.F.,
(4,3,3,3,3,3,3,3,3,3,3,3,3,3,3,3,3,3,3,3,3,3,3,3,3,3,3,3,3,3,3,3,3,3,3,
3,3,3,3,3,3,3,3,3,3,3,3,3,3,3,3,3,3,3,3,3,3,3,3,3,3,3,3,3,3,3,3,3,3,3,3,
3,3,3,3,3,3,3,3,3,3,3,3,3,3,3,3,3,3,3,3,3,3,3,3,3,3,3,3,3,3,3,4),(0.143172102,
0.15412844,0.165137615,0.176146789,0.187155963,0.198165138,0.209174312,
0.220183486,0.231192661,0.242201835,0.253211009,0.264220183,0.275229358,
0.288073394,0.299082569,0.310091743,0.32293578,0.333944954,0.344954128,
0.355963303,0.368807339,0.379816514,0.394495413,0.403669725,0.412844037,
0.422018349,0.433027523,0.442201835,0.451376147,0.462385321,0.471559633,
0.486238532,0.495412844,0.506422018,0.51559633,0.524770642,0.533944954,
0.544954128,0.55412844,0.563302752,0.570642202,0.577981651,0.585321101,
0.59266055,0.6,0.609174312,0.616513761,0.625688073,0.634862385,0.644036697,
0.651376147,0.658715596,0.667889908,0.67706422,0.68440367,0.691743119,0.699082569,
0.706422018,0.71559633,0.724770642,0.733944954,0.741284404,0.748623853,
0.755963303,0.763302752,0.770642202,0.777981651,0.785321101,0.79266055,
0.8,0.80733945,0.812844037,0.818348624,0.823853211,0.831192661,0.836697248,
0.842201835,0.847706422,0.853211009,0.858715596,0.864220183,0.869724771,
0.875229358,0.880733945,0.886238532,0.893577982,0.899082569,0.906422018,
0.911926606,0.919266055,0.924770642,0.930275229,0.935779817,0.943119266,
0.948623853,0.955963303,0.963302752,0.968807339,0.976146789,0.981651376,
0.988990826,0.994495413,1.),.UNSPECIFIED.);
#24435=B_SPLINE_CURVE_WITH_KNOTS('',3,(#250385,#250386,#250387,#250388,
#250389,#250390,#250391,#250392,#250393,#250394,#250395,#250396,#250397,
#250398,#250399,#250400,#250401,#250402,#250403,#250404,#250405,#250406,
#250407,#250408,#250409,#250410,#250411,#250412,#250413,#250414,#250415,
#250416,#250417,#250418,#250419,#250420,#250421,#250422,#250423,#250424,
#250425,#250426,#250427,#250428,#250429,#250430,#250431,#250432,#250433,
#250434,#250435,#250436,#250437,#250438,#250439,#250440,#250441,#250442,
#250443,#250444,#250445,#250446,#250447,#250448,#250449,#250450,#250451,
#250452,#250453,#250454,#250455,#250456,#250457,#250458,#250459,#250460,
#250461,#250462,#250463,#250464,#250465,#250466,#250467,#250468,#250469,
#250470,#250471,#250472,#250473,#250474,#250475,#250476,#250477,#250478,
#250479,#250480,#250481,#250482,#250483,#250484,#250485,#250486,#250487,
#250488,#250489,#250490,#250491,#250492,#250493,#250494,#250495,#250496,
#250497,#250498,#250499,#250500,#250501,#250502,#250503,#250504,#250505,
#250506,#250507,#250508,#250509,#250510,#250511,#250512,#250513,#250514,
#250515,#250516,#250517,#250518,#250519,#250520,#250521,#250522,#250523,
#250524,#250525,#250526,#250527,#250528,#250529,#250530,#250531,#250532,
#250533,#250534,#250535,#250536,#250537,#250538,#250539,#250540,#250541,
#250542,#250543,#250544,#250545,#250546,#250547,#250548,#250549,#250550,
#250551,#250552,#250553,#250554,#250555,#250556,#250557,#250558,#250559,
#250560,#250561,#250562,#250563,#250564,#250565,#250566,#250567,#250568,
#250569,#250570,#250571,#250572,#250573,#250574,#250575,#250576,#250577,
#250578,#250579,#250580,#250581,#250582,#250583,#250584,#250585,#250586,
#250587,#250588,#250589,#250590,#250591,#250592,#250593,#250594,#250595,
#250596,#250597,#250598,#250599,#250600,#250601,#250602,#250603,#250604,
#250605,#250606,#250607,#250608,#250609,#250610,#250611,#250612,#250613,
#250614,#250615,#250616,#250617,#250618,#250619,#250620,#250621,#250622,
#250623,#250624,#250625,#250626,#250627,#250628,#250629,#250630,#250631,
#250632,#250633,#250634,#250635,#250636,#250637,#250638,#250639,#250640,
#250641,#250642,#250643,#250644,#250645,#250646,#250647,#250648,#250649,
#250650,#250651,#250652,#250653,#250654,#250655,#250656,#250657,#250658,
#250659,#250660,#250661,#250662,#250663,#250664,#250665,#250666,#250667,
#250668,#250669,#250670,#250671,#250672,#250673,#250674,#250675,#250676,
#250677,#250678,#250679,#250680,#250681,#250682,#250683,#250684,#250685,
#250686,#250687,#250688,#250689,#250690,#250691,#250692,#250693,#250694,
#250695,#250696,#250697,#250698,#250699,#250700,#250701,#250702,#250703,
#250704,#250705,#250706,#250707,#250708,#250709,#250710,#250711,#250712),
 .UNSPECIFIED.,.F.,.F.,(4,3,3,3,3,3,3,3,3,3,3,3,3,3,3,3,3,3,3,3,3,3,3,3,
3,3,3,3,3,3,3,3,3,3,3,3,3,3,3,3,3,3,3,3,3,3,3,3,3,3,3,3,3,3,3,3,3,3,3,3,
3,3,3,3,3,3,3,3,3,3,3,3,3,3,3,3,3,3,3,3,3,3,3,3,3,3,3,3,3,3,3,3,3,3,3,3,
3,3,3,3,3,3,3,3,3,3,3,3,3,4),(-1.,-0.994495413,-0.988990826,-0.983486239,
-0.977981651,-0.972477064,-0.966972477,-0.96146789,-0.955963303,-0.950458716,
-0.944954128,-0.939449541,-0.932110092,-0.926605505,-0.921100917,-0.91559633,
-0.910091743,-0.904587156,-0.899082569,-0.893577982,-0.888073394,-0.882568807,
-0.87706422,-0.871559633,-0.866055046,-0.860550459,-0.855045872,-0.849541284,
-0.844036697,-0.83853211,-0.833027523,-0.827522936,-0.822018349,-0.814678899,
-0.809174312,-0.801834862,-0.794495413,-0.787155963,-0.779816514,-0.772477064,
-0.765137615,-0.757798165,-0.748623853,-0.741284404,-0.733944954,-0.726605505,
-0.719266055,-0.711926606,-0.704587156,-0.697247706,-0.689908257,-0.682568807,
-0.675229358,-0.667889908,-0.660550459,-0.653211009,-0.64587156,-0.63853211,
-0.631192661,-0.623853211,-0.616513761,-0.609174312,-0.601834862,-0.594495413,
-0.587155963,-0.579816514,-0.572477064,-0.565137615,-0.555963303,-0.548623853,
-0.541284404,-0.533944954,-0.526605505,-0.517431193,-0.508256881,-0.499082569,
-0.489908257,-0.480733945,-0.471559633,-0.462385321,-0.453211009,-0.442201835,
-0.433027523,-0.423853211,-0.414678899,-0.405504587,-0.396330275,-0.387155963,
-0.376146789,-0.365137615,-0.35412844,-0.343119266,-0.332110092,-0.321100917,
-0.308256881,-0.297247706,-0.286238532,-0.275229358,-0.264220183,-0.253211009,
-0.242201835,-0.231192661,-0.220183486,-0.209174312,-0.198165138,-0.187155963,
-0.176146789,-0.165137615,-0.15412844,-0.143172102),.UNSPECIFIED.);
#24436=B_SPLINE_CURVE_WITH_KNOTS('',3,(#250713,#250714,#250715,#250716,
#250717,#250718,#250719,#250720,#250721,#250722,#250723,#250724,#250725,
#250726,#250727,#250728,#250729,#250730,#250731,#250732,#250733,#250734,
#250735,#250736,#250737,#250738,#250739,#250740,#250741,#250742,#250743,
#250744,#250745,#250746,#250747,#250748,#250749,#250750,#250751,#250752,
#250753,#250754,#250755,#250756,#250757,#250758,#250759,#250760,#250761,
#250762,#250763,#250764,#250765,#250766,#250767,#250768,#250769,#250770,
#250771,#250772,#250773,#250774,#250775,#250776,#250777,#250778,#250779,
#250780,#250781,#250782,#250783,#250784,#250785,#250786,#250787,#250788,
#250789,#250790,#250791,#250792,#250793,#250794,#250795,#250796,#250797,
#250798,#250799,#250800,#250801,#250802,#250803,#250804,#250805,#250806,
#250807,#250808,#250809,#250810,#250811,#250812,#250813,#250814,#250815,
#250816,#250817,#250818,#250819,#250820,#250821,#250822,#250823,#250824,
#250825,#250826,#250827,#250828,#250829,#250830,#250831,#250832,#250833,
#250834,#250835,#250836,#250837,#250838,#250839,#250840,#250841,#250842,
#250843,#250844,#250845,#250846,#250847,#250848,#250849,#250850,#250851,
#250852,#250853,#250854,#250855,#250856,#250857,#250858,#250859,#250860,
#250861,#250862,#250863,#250864,#250865,#250866,#250867,#250868,#250869,
#250870,#250871,#250872,#250873,#250874,#250875,#250876,#250877,#250878,
#250879,#250880,#250881,#250882,#250883,#250884,#250885,#250886,#250887,
#250888,#250889,#250890,#250891,#250892,#250893,#250894,#250895,#250896,
#250897,#250898,#250899,#250900,#250901,#250902,#250903,#250904,#250905,
#250906,#250907,#250908,#250909,#250910,#250911,#250912,#250913,#250914,
#250915,#250916,#250917,#250918,#250919,#250920,#250921,#250922,#250923,
#250924,#250925,#250926,#250927,#250928,#250929,#250930,#250931,#250932,
#250933,#250934,#250935,#250936,#250937,#250938,#250939,#250940,#250941,
#250942,#250943,#250944,#250945,#250946,#250947,#250948,#250949,#250950,
#250951,#250952,#250953,#250954,#250955,#250956,#250957,#250958,#250959,
#250960,#250961,#250962,#250963,#250964,#250965,#250966,#250967,#250968,
#250969,#250970,#250971,#250972,#250973,#250974,#250975,#250976,#250977,
#250978,#250979,#250980,#250981,#250982,#250983,#250984,#250985,#250986,
#250987,#250988,#250989,#250990,#250991,#250992,#250993,#250994,#250995,
#250996,#250997,#250998,#250999,#251000,#251001,#251002,#251003,#251004,
#251005,#251006,#251007,#251008,#251009,#251010,#251011,#251012,#251013,
#251014,#251015,#251016,#251017,#251018,#251019,#251020,#251021,#251022),
 .UNSPECIFIED.,.F.,.F.,(4,3,3,3,3,3,3,3,3,3,3,3,3,3,3,3,3,3,3,3,3,3,3,3,
3,3,3,3,3,3,3,3,3,3,3,3,3,3,3,3,3,3,3,3,3,3,3,3,3,3,3,3,3,3,3,3,3,3,3,3,
3,3,3,3,3,3,3,3,3,3,3,3,3,3,3,3,3,3,3,3,3,3,3,3,3,3,3,3,3,3,3,3,3,3,3,3,
3,3,3,3,3,3,3,4),(0.143172102,0.15412844,0.165137615,0.176146789,0.187155963,
0.198165138,0.211009174,0.222018349,0.233027523,0.244036697,0.255045872,
0.266055046,0.27706422,0.288073394,0.299082569,0.310091743,0.321100917,
0.332110092,0.343119266,0.35412844,0.365137615,0.376146789,0.387155963,
0.396330275,0.405504587,0.414678899,0.423853211,0.433027523,0.44587156,
0.455045872,0.464220183,0.473394495,0.482568807,0.491743119,0.500917431,
0.510091743,0.519266055,0.528440367,0.535779817,0.543119266,0.550458716,
0.557798165,0.568807339,0.576146789,0.583486239,0.594495413,0.601834862,
0.611009174,0.618348624,0.625688073,0.633027523,0.640366972,0.647706422,
0.656880734,0.666055046,0.673394495,0.686238532,0.697247706,0.706422018,
0.713761468,0.721100917,0.732110092,0.739449541,0.748623853,0.755963303,
0.763302752,0.770642202,0.777981651,0.787155963,0.794495413,0.801834862,
0.812844037,0.818348624,0.823853211,0.829357798,0.836697248,0.842201835,
0.847706422,0.853211009,0.858715596,0.864220183,0.869724771,0.875229358,
0.880733945,0.888073394,0.893577982,0.899082569,0.904587156,0.910091743,
0.91559633,0.921100917,0.926605505,0.932110092,0.937614679,0.943119266,
0.952293578,0.957798165,0.963302752,0.968807339,0.974311927,0.979816514,
0.985321101,0.99266055,1.),.UNSPECIFIED.);
#24437=B_SPLINE_CURVE_WITH_KNOTS('',3,(#251967,#251968,#251969,#251970,
#251971,#251972,#251973,#251974,#251975,#251976,#251977,#251978,#251979,
#251980,#251981,#251982,#251983,#251984,#251985,#251986,#251987,#251988,
#251989,#251990,#251991,#251992,#251993,#251994,#251995,#251996,#251997,
#251998,#251999,#252000,#252001,#252002,#252003,#252004,#252005,#252006,
#252007,#252008,#252009,#252010,#252011,#252012,#252013,#252014,#252015,
#252016,#252017,#252018,#252019,#252020,#252021,#252022,#252023,#252024,
#252025,#252026,#252027,#252028,#252029,#252030,#252031,#252032,#252033,
#252034,#252035,#252036,#252037,#252038,#252039,#252040,#252041,#252042,
#252043,#252044,#252045,#252046,#252047,#252048,#252049,#252050,#252051,
#252052,#252053,#252054,#252055,#252056,#252057,#252058,#252059,#252060,
#252061,#252062,#252063,#252064,#252065,#252066,#252067,#252068,#252069,
#252070,#252071,#252072,#252073,#252074,#252075,#252076,#252077,#252078,
#252079,#252080,#252081,#252082,#252083,#252084,#252085,#252086,#252087,
#252088,#252089,#252090,#252091,#252092,#252093,#252094,#252095,#252096,
#252097,#252098,#252099,#252100,#252101,#252102,#252103,#252104,#252105,
#252106,#252107,#252108,#252109,#252110,#252111,#252112,#252113,#252114,
#252115,#252116,#252117,#252118,#252119,#252120,#252121,#252122,#252123,
#252124,#252125,#252126,#252127,#252128,#252129,#252130,#252131,#252132,
#252133,#252134,#252135,#252136,#252137,#252138,#252139,#252140,#252141,
#252142,#252143,#252144,#252145,#252146,#252147,#252148,#252149,#252150,
#252151,#252152,#252153,#252154,#252155,#252156,#252157,#252158,#252159,
#252160,#252161,#252162,#252163,#252164,#252165,#252166,#252167,#252168,
#252169,#252170,#252171,#252172,#252173,#252174,#252175,#252176,#252177,
#252178,#252179,#252180,#252181,#252182,#252183,#252184,#252185,#252186,
#252187,#252188,#252189,#252190,#252191,#252192,#252193,#252194,#252195,
#252196,#252197,#252198,#252199,#252200,#252201,#252202,#252203,#252204,
#252205,#252206,#252207,#252208,#252209,#252210,#252211,#252212,#252213,
#252214,#252215,#252216,#252217,#252218,#252219,#252220,#252221,#252222,
#252223,#252224,#252225,#252226,#252227,#252228,#252229,#252230,#252231,
#252232,#252233,#252234,#252235,#252236,#252237,#252238,#252239,#252240,
#252241,#252242,#252243,#252244,#252245,#252246,#252247,#252248,#252249,
#252250,#252251,#252252,#252253,#252254,#252255,#252256,#252257,#252258,
#252259,#252260,#252261,#252262,#252263,#252264,#252265,#252266,#252267,
#252268,#252269,#252270,#252271,#252272,#252273),.UNSPECIFIED.,.F.,.F.,
(4,3,3,3,3,3,3,3,3,3,3,3,3,3,3,3,3,3,3,3,3,3,3,3,3,3,3,3,3,3,3,3,3,3,3,
3,3,3,3,3,3,3,3,3,3,3,3,3,3,3,3,3,3,3,3,3,3,3,3,3,3,3,3,3,3,3,3,3,3,3,3,
3,3,3,3,3,3,3,3,3,3,3,3,3,3,3,3,3,3,3,3,3,3,3,3,3,3,3,3,3,3,3,4),(0.143172102,
0.15412844,0.165137615,0.176146789,0.187155963,0.198165138,0.209174312,
0.220183486,0.231192661,0.242201835,0.253211009,0.264220183,0.27706422,
0.288073394,0.299082569,0.310091743,0.321100917,0.332110092,0.343119266,
0.35412844,0.366972477,0.377981651,0.388990826,0.398165138,0.40733945,0.416513761,
0.425688073,0.434862385,0.444036697,0.456880734,0.466055046,0.475229358,
0.48440367,0.493577982,0.502752294,0.511926606,0.521100917,0.530275229,
0.537614679,0.544954128,0.55412844,0.56146789,0.570642202,0.577981651,0.585321101,
0.594495413,0.601834862,0.612844037,0.620183486,0.629357798,0.63853211,
0.649541284,0.656880734,0.664220183,0.671559633,0.678899083,0.686238532,
0.693577982,0.700917431,0.708256881,0.71559633,0.72293578,0.732110092,0.739449541,
0.746788991,0.75412844,0.76146789,0.768807339,0.776146789,0.785321101,0.79266055,
0.801834862,0.811009174,0.816513761,0.822018349,0.831192661,0.836697248,
0.844036697,0.849541284,0.855045872,0.862385321,0.871559633,0.87706422,
0.882568807,0.891743119,0.897247706,0.902752294,0.908256881,0.913761468,
0.921100917,0.926605505,0.932110092,0.937614679,0.943119266,0.950458716,
0.955963303,0.96146789,0.966972477,0.974311927,0.979816514,0.985321101,
0.994495413,1.),.UNSPECIFIED.);
#24438=B_SPLINE_CURVE_WITH_KNOTS('',3,(#252274,#252275,#252276,#252277,
#252278,#252279,#252280,#252281,#252282,#252283,#252284,#252285,#252286,
#252287,#252288,#252289,#252290,#252291,#252292,#252293,#252294,#252295,
#252296,#252297,#252298,#252299,#252300,#252301,#252302,#252303,#252304,
#252305,#252306,#252307,#252308,#252309,#252310,#252311,#252312,#252313,
#252314,#252315,#252316,#252317,#252318,#252319,#252320,#252321,#252322,
#252323,#252324,#252325,#252326,#252327,#252328,#252329,#252330,#252331,
#252332,#252333,#252334,#252335,#252336,#252337,#252338,#252339,#252340,
#252341,#252342,#252343,#252344,#252345,#252346,#252347,#252348,#252349,
#252350,#252351,#252352,#252353,#252354,#252355,#252356,#252357,#252358,
#252359,#252360,#252361,#252362,#252363,#252364,#252365,#252366,#252367,
#252368,#252369,#252370,#252371,#252372,#252373,#252374,#252375,#252376,
#252377,#252378,#252379,#252380,#252381,#252382,#252383,#252384,#252385,
#252386,#252387,#252388,#252389,#252390,#252391,#252392,#252393,#252394,
#252395,#252396,#252397,#252398,#252399,#252400,#252401,#252402,#252403,
#252404,#252405,#252406,#252407,#252408,#252409,#252410,#252411,#252412,
#252413,#252414,#252415,#252416,#252417,#252418,#252419,#252420,#252421,
#252422,#252423,#252424,#252425,#252426,#252427,#252428,#252429,#252430,
#252431,#252432,#252433,#252434,#252435,#252436,#252437,#252438,#252439,
#252440,#252441,#252442,#252443,#252444,#252445,#252446,#252447,#252448,
#252449,#252450,#252451,#252452,#252453,#252454,#252455,#252456,#252457,
#252458,#252459,#252460,#252461,#252462,#252463,#252464,#252465,#252466,
#252467,#252468,#252469,#252470,#252471,#252472,#252473,#252474,#252475,
#252476,#252477,#252478,#252479,#252480,#252481,#252482,#252483,#252484,
#252485,#252486,#252487,#252488,#252489,#252490,#252491,#252492,#252493,
#252494,#252495,#252496,#252497,#252498,#252499,#252500,#252501,#252502,
#252503,#252504,#252505,#252506,#252507,#252508,#252509,#252510,#252511,
#252512,#252513,#252514,#252515,#252516,#252517,#252518,#252519,#252520,
#252521,#252522,#252523,#252524,#252525,#252526,#252527,#252528,#252529,
#252530,#252531,#252532,#252533,#252534,#252535,#252536,#252537,#252538,
#252539,#252540,#252541,#252542,#252543,#252544,#252545,#252546,#252547,
#252548,#252549,#252550,#252551,#252552,#252553,#252554,#252555,#252556,
#252557,#252558,#252559,#252560,#252561,#252562,#252563,#252564,#252565,
#252566,#252567,#252568,#252569,#252570,#252571,#252572,#252573,#252574,
#252575,#252576,#252577,#252578,#252579,#252580,#252581,#252582,#252583,
#252584,#252585,#252586,#252587,#252588,#252589,#252590,#252591,#252592,
#252593,#252594,#252595),.UNSPECIFIED.,.F.,.F.,(4,3,3,3,3,3,3,3,3,3,3,3,
3,3,3,3,3,3,3,3,3,3,3,3,3,3,3,3,3,3,3,3,3,3,3,3,3,3,3,3,3,3,3,3,3,3,3,3,
3,3,3,3,3,3,3,3,3,3,3,3,3,3,3,3,3,3,3,3,3,3,3,3,3,3,3,3,3,3,3,3,3,3,3,3,
3,3,3,3,3,3,3,3,3,3,3,3,3,3,3,3,3,3,3,3,3,3,3,4),(0.143172102,0.15412844,
0.165137615,0.176146789,0.187155963,0.198165138,0.209174312,0.220183486,
0.231192661,0.242201835,0.253211009,0.264220183,0.27706422,0.288073394,
0.299082569,0.310091743,0.321100917,0.332110092,0.343119266,0.35412844,
0.365137615,0.376146789,0.387155963,0.396330275,0.405504587,0.414678899,
0.423853211,0.433027523,0.442201835,0.451376147,0.460550459,0.469724771,
0.478899083,0.489908257,0.499082569,0.510091743,0.519266055,0.528440367,
0.535779817,0.544954128,0.552293578,0.559633028,0.566972477,0.574311927,
0.581651376,0.588990826,0.596330275,0.603669725,0.611009174,0.618348624,
0.625688073,0.633027523,0.640366972,0.647706422,0.655045872,0.664220183,
0.671559633,0.678899083,0.686238532,0.693577982,0.700917431,0.708256881,
0.71559633,0.72293578,0.732110092,0.739449541,0.746788991,0.75412844,0.76146789,
0.768807339,0.776146789,0.783486239,0.790825688,0.798165138,0.805504587,
0.811009174,0.816513761,0.822018349,0.827522936,0.833027523,0.842201835,
0.849541284,0.855045872,0.860550459,0.866055046,0.871559633,0.87706422,
0.882568807,0.888073394,0.893577982,0.900917431,0.906422018,0.911926606,
0.917431193,0.924770642,0.930275229,0.935779817,0.941284404,0.946788991,
0.95412844,0.959633028,0.965137615,0.972477064,0.977981651,0.983486239,
0.988990826,0.994495413,1.),.UNSPECIFIED.);
#24439=B_SPLINE_CURVE_WITH_KNOTS('',3,(#253555,#253556,#253557,#253558,
#253559,#253560,#253561,#253562,#253563,#253564,#253565,#253566,#253567,
#253568,#253569,#253570,#253571,#253572,#253573,#253574,#253575,#253576,
#253577,#253578,#253579,#253580,#253581,#253582,#253583,#253584,#253585,
#253586,#253587,#253588,#253589,#253590,#253591,#253592,#253593,#253594,
#253595,#253596,#253597,#253598,#253599,#253600,#253601,#253602,#253603,
#253604,#253605,#253606,#253607,#253608,#253609,#253610,#253611,#253612,
#253613,#253614,#253615,#253616,#253617,#253618,#253619,#253620,#253621,
#253622,#253623,#253624,#253625,#253626,#253627,#253628,#253629,#253630,
#253631,#253632,#253633,#253634,#253635,#253636,#253637,#253638,#253639,
#253640,#253641,#253642,#253643,#253644,#253645,#253646,#253647,#253648,
#253649,#253650,#253651,#253652,#253653,#253654,#253655,#253656,#253657,
#253658,#253659,#253660,#253661,#253662,#253663,#253664,#253665,#253666,
#253667,#253668,#253669,#253670,#253671,#253672,#253673,#253674,#253675,
#253676,#253677,#253678,#253679,#253680,#253681,#253682,#253683,#253684,
#253685,#253686,#253687,#253688,#253689,#253690,#253691,#253692,#253693,
#253694,#253695,#253696,#253697,#253698,#253699,#253700,#253701,#253702,
#253703,#253704,#253705,#253706,#253707,#253708,#253709,#253710,#253711,
#253712,#253713,#253714,#253715,#253716,#253717,#253718,#253719,#253720,
#253721,#253722,#253723,#253724,#253725,#253726,#253727,#253728,#253729,
#253730,#253731,#253732,#253733,#253734,#253735,#253736,#253737,#253738,
#253739,#253740,#253741,#253742,#253743,#253744,#253745,#253746,#253747,
#253748,#253749,#253750,#253751,#253752,#253753,#253754,#253755,#253756,
#253757,#253758,#253759,#253760,#253761,#253762,#253763,#253764,#253765,
#253766,#253767,#253768,#253769,#253770,#253771,#253772,#253773,#253774,
#253775,#253776,#253777,#253778,#253779,#253780,#253781,#253782,#253783,
#253784,#253785,#253786,#253787,#253788,#253789,#253790,#253791,#253792,
#253793,#253794,#253795,#253796,#253797,#253798,#253799,#253800,#253801,
#253802,#253803,#253804,#253805,#253806,#253807,#253808,#253809,#253810,
#253811,#253812,#253813,#253814,#253815,#253816,#253817,#253818,#253819,
#253820,#253821,#253822,#253823,#253824,#253825,#253826,#253827,#253828,
#253829,#253830,#253831,#253832,#253833,#253834,#253835,#253836,#253837,
#253838,#253839,#253840,#253841,#253842,#253843,#253844,#253845,#253846),
 .UNSPECIFIED.,.F.,.F.,(4,3,3,3,3,3,3,3,3,3,3,3,3,3,3,3,3,3,3,3,3,3,3,3,
3,3,3,3,3,3,3,3,3,3,3,3,3,3,3,3,3,3,3,3,3,3,3,3,3,3,3,3,3,3,3,3,3,3,3,3,
3,3,3,3,3,3,3,3,3,3,3,3,3,3,3,3,3,3,3,3,3,3,3,3,3,3,3,3,3,3,3,3,3,3,3,3,
3,4),(0.143172102,0.15412844,0.165137615,0.176146789,0.187155963,0.198165138,
0.209174312,0.220183486,0.231192661,0.242201835,0.253211009,0.264220183,
0.275229358,0.286238532,0.297247706,0.308256881,0.319266055,0.330275229,
0.341284404,0.352293578,0.363302752,0.376146789,0.388990826,0.398165138,
0.40733945,0.416513761,0.425688073,0.434862385,0.444036697,0.453211009,
0.462385321,0.475229358,0.48440367,0.495412844,0.506422018,0.51559633,0.524770642,
0.533944954,0.541284404,0.548623853,0.555963303,0.563302752,0.570642202,
0.577981651,0.590825688,0.598165138,0.605504587,0.618348624,0.625688073,
0.634862385,0.642201835,0.651376147,0.664220183,0.675229358,0.682568807,
0.691743119,0.699082569,0.706422018,0.717431193,0.724770642,0.735779817,
0.743119266,0.752293578,0.759633028,0.768807339,0.781651376,0.788990826,
0.796330275,0.80733945,0.812844037,0.818348624,0.823853211,0.829357798,
0.83853211,0.84587156,0.851376147,0.860550459,0.867889908,0.87706422,0.882568807,
0.889908257,0.895412844,0.900917431,0.910091743,0.919266055,0.926605505,
0.933944954,0.939449541,0.944954128,0.950458716,0.955963303,0.963302752,
0.968807339,0.974311927,0.981651376,0.987155963,0.994495413,1.),
 .UNSPECIFIED.);
#24440=B_SPLINE_CURVE_WITH_KNOTS('',3,(#253847,#253848,#253849,#253850,
#253851,#253852,#253853,#253854,#253855,#253856,#253857,#253858,#253859,
#253860,#253861,#253862,#253863,#253864,#253865,#253866,#253867,#253868,
#253869,#253870,#253871,#253872,#253873,#253874,#253875,#253876,#253877,
#253878,#253879,#253880,#253881,#253882,#253883,#253884,#253885,#253886,
#253887,#253888,#253889,#253890,#253891,#253892,#253893,#253894,#253895,
#253896,#253897,#253898,#253899,#253900,#253901,#253902,#253903,#253904,
#253905,#253906,#253907,#253908,#253909,#253910,#253911,#253912,#253913,
#253914,#253915,#253916,#253917,#253918,#253919,#253920,#253921,#253922,
#253923,#253924,#253925,#253926,#253927,#253928,#253929,#253930,#253931,
#253932,#253933,#253934,#253935,#253936,#253937,#253938,#253939,#253940,
#253941,#253942,#253943,#253944,#253945,#253946,#253947,#253948,#253949,
#253950,#253951,#253952,#253953,#253954,#253955,#253956,#253957,#253958,
#253959,#253960,#253961,#253962,#253963,#253964,#253965,#253966,#253967,
#253968,#253969,#253970,#253971,#253972,#253973,#253974,#253975,#253976,
#253977,#253978,#253979,#253980,#253981,#253982,#253983,#253984,#253985,
#253986,#253987,#253988,#253989,#253990,#253991,#253992,#253993,#253994,
#253995,#253996,#253997,#253998,#253999,#254000,#254001,#254002,#254003,
#254004,#254005,#254006,#254007,#254008,#254009,#254010,#254011,#254012,
#254013,#254014,#254015,#254016,#254017,#254018,#254019,#254020,#254021,
#254022,#254023,#254024,#254025,#254026,#254027,#254028,#254029,#254030,
#254031,#254032,#254033,#254034,#254035,#254036,#254037,#254038,#254039,
#254040,#254041,#254042,#254043,#254044,#254045,#254046,#254047,#254048,
#254049,#254050,#254051,#254052,#254053,#254054,#254055,#254056,#254057,
#254058,#254059,#254060,#254061,#254062,#254063,#254064,#254065,#254066,
#254067,#254068,#254069,#254070,#254071,#254072,#254073,#254074,#254075,
#254076,#254077,#254078,#254079,#254080,#254081,#254082,#254083,#254084,
#254085,#254086,#254087,#254088,#254089,#254090,#254091,#254092,#254093,
#254094,#254095,#254096,#254097,#254098,#254099,#254100,#254101,#254102,
#254103,#254104,#254105,#254106,#254107,#254108,#254109,#254110,#254111,
#254112,#254113,#254114,#254115,#254116,#254117,#254118,#254119,#254120,
#254121,#254122,#254123,#254124,#254125,#254126,#254127,#254128,#254129,
#254130,#254131,#254132,#254133,#254134,#254135,#254136,#254137,#254138,
#254139,#254140,#254141,#254142,#254143,#254144,#254145,#254146,#254147,
#254148,#254149,#254150,#254151,#254152,#254153,#254154,#254155,#254156,
#254157,#254158,#254159,#254160,#254161,#254162,#254163,#254164,#254165),
 .UNSPECIFIED.,.F.,.F.,(4,3,3,3,3,3,3,3,3,3,3,3,3,3,3,3,3,3,3,3,3,3,3,3,
3,3,3,3,3,3,3,3,3,3,3,3,3,3,3,3,3,3,3,3,3,3,3,3,3,3,3,3,3,3,3,3,3,3,3,3,
3,3,3,3,3,3,3,3,3,3,3,3,3,3,3,3,3,3,3,3,3,3,3,3,3,3,3,3,3,3,3,3,3,3,3,3,
3,3,3,3,3,3,3,3,3,3,4),(0.143172102,0.15412844,0.165137615,0.176146789,
0.187155963,0.198165138,0.209174312,0.220183486,0.231192661,0.242201835,
0.253211009,0.266055046,0.27706422,0.288073394,0.300917431,0.311926606,
0.32293578,0.333944954,0.344954128,0.355963303,0.366972477,0.377981651,
0.390825688,0.4,0.409174312,0.418348624,0.429357798,0.43853211,0.447706422,
0.456880734,0.466055046,0.475229358,0.48440367,0.493577982,0.502752294,
0.511926606,0.521100917,0.530275229,0.537614679,0.544954128,0.552293578,
0.559633028,0.566972477,0.574311927,0.581651376,0.588990826,0.596330275,
0.603669725,0.611009174,0.618348624,0.625688073,0.633027523,0.640366972,
0.647706422,0.655045872,0.662385321,0.671559633,0.678899083,0.686238532,
0.693577982,0.700917431,0.708256881,0.71559633,0.72293578,0.730275229,0.737614679,
0.744954128,0.752293578,0.759633028,0.766972477,0.774311927,0.781651376,
0.788990826,0.796330275,0.805504587,0.811009174,0.816513761,0.822018349,
0.827522936,0.834862385,0.840366972,0.84587156,0.853211009,0.858715596,
0.864220183,0.869724771,0.875229358,0.882568807,0.888073394,0.893577982,
0.900917431,0.906422018,0.911926606,0.917431193,0.924770642,0.930275229,
0.935779817,0.941284404,0.946788991,0.95412844,0.959633028,0.968807339,
0.976146789,0.981651376,0.987155963,0.99266055,1.),.UNSPECIFIED.);
#24441=B_SPLINE_CURVE_WITH_KNOTS('',3,(#255113,#255114,#255115,#255116,
#255117,#255118,#255119,#255120,#255121,#255122,#255123,#255124,#255125,
#255126,#255127,#255128,#255129,#255130,#255131,#255132,#255133,#255134,
#255135,#255136,#255137,#255138,#255139,#255140,#255141,#255142,#255143,
#255144,#255145,#255146,#255147,#255148,#255149,#255150,#255151,#255152,
#255153,#255154,#255155,#255156,#255157,#255158,#255159,#255160,#255161,
#255162,#255163,#255164,#255165,#255166,#255167,#255168,#255169,#255170,
#255171,#255172,#255173,#255174,#255175,#255176,#255177,#255178,#255179,
#255180,#255181,#255182,#255183,#255184,#255185,#255186,#255187,#255188,
#255189,#255190,#255191,#255192,#255193,#255194,#255195,#255196,#255197,
#255198,#255199,#255200,#255201,#255202,#255203,#255204,#255205,#255206,
#255207,#255208,#255209,#255210,#255211,#255212,#255213,#255214,#255215,
#255216,#255217,#255218,#255219,#255220,#255221,#255222,#255223,#255224,
#255225,#255226,#255227,#255228,#255229,#255230,#255231,#255232,#255233,
#255234,#255235,#255236,#255237,#255238,#255239,#255240,#255241,#255242,
#255243,#255244,#255245,#255246,#255247,#255248,#255249,#255250,#255251,
#255252,#255253,#255254,#255255,#255256,#255257,#255258,#255259,#255260,
#255261,#255262,#255263,#255264,#255265,#255266,#255267,#255268,#255269,
#255270,#255271,#255272,#255273,#255274,#255275,#255276,#255277,#255278,
#255279,#255280,#255281,#255282,#255283,#255284,#255285,#255286,#255287,
#255288,#255289,#255290,#255291,#255292,#255293,#255294,#255295,#255296,
#255297,#255298,#255299,#255300,#255301,#255302,#255303,#255304,#255305,
#255306,#255307,#255308,#255309,#255310,#255311,#255312,#255313,#255314,
#255315,#255316,#255317,#255318,#255319,#255320,#255321,#255322,#255323,
#255324,#255325,#255326,#255327,#255328,#255329,#255330,#255331,#255332,
#255333,#255334,#255335,#255336,#255337,#255338,#255339,#255340,#255341,
#255342,#255343,#255344,#255345,#255346,#255347,#255348,#255349,#255350,
#255351,#255352,#255353,#255354,#255355,#255356,#255357,#255358,#255359,
#255360,#255361,#255362,#255363,#255364,#255365,#255366,#255367,#255368,
#255369,#255370,#255371,#255372,#255373,#255374,#255375,#255376,#255377,
#255378,#255379,#255380,#255381,#255382,#255383,#255384,#255385,#255386,
#255387,#255388,#255389,#255390,#255391,#255392,#255393,#255394,#255395,
#255396,#255397,#255398,#255399,#255400,#255401,#255402,#255403,#255404,
#255405,#255406,#255407,#255408,#255409,#255410,#255411,#255412,#255413,
#255414,#255415,#255416,#255417,#255418,#255419,#255420,#255421,#255422,
#255423,#255424,#255425,#255426,#255427,#255428,#255429,#255430,#255431,
#255432,#255433,#255434),.UNSPECIFIED.,.F.,.F.,(4,3,3,3,3,3,3,3,3,3,3,3,
3,3,3,3,3,3,3,3,3,3,3,3,3,3,3,3,3,3,3,3,3,3,3,3,3,3,3,3,3,3,3,3,3,3,3,3,
3,3,3,3,3,3,3,3,3,3,3,3,3,3,3,3,3,3,3,3,3,3,3,3,3,3,3,3,3,3,3,3,3,3,3,3,
3,3,3,3,3,3,3,3,3,3,3,3,3,3,3,3,3,3,3,3,3,3,3,4),(-1.,-0.994495413,-0.988990826,
-0.983486239,-0.977981651,-0.972477064,-0.966972477,-0.959633028,-0.95412844,
-0.948623853,-0.943119266,-0.937614679,-0.932110092,-0.926605505,-0.919266055,
-0.913761468,-0.908256881,-0.902752294,-0.897247706,-0.891743119,-0.886238532,
-0.880733945,-0.875229358,-0.867889908,-0.860550459,-0.855045872,-0.849541284,
-0.844036697,-0.83853211,-0.833027523,-0.827522936,-0.822018349,-0.814678899,
-0.809174312,-0.801834862,-0.794495413,-0.787155963,-0.779816514,-0.772477064,
-0.765137615,-0.757798165,-0.750458716,-0.743119266,-0.735779817,-0.728440367,
-0.721100917,-0.711926606,-0.704587156,-0.697247706,-0.689908257,-0.682568807,
-0.675229358,-0.667889908,-0.660550459,-0.653211009,-0.644036697,-0.636697248,
-0.629357798,-0.622018349,-0.614678899,-0.60733945,-0.6,-0.59266055,-0.585321101,
-0.577981651,-0.570642202,-0.563302752,-0.555963303,-0.548623853,-0.541284404,
-0.533944954,-0.524770642,-0.513761468,-0.504587156,-0.495412844,-0.486238532,
-0.47706422,-0.467889908,-0.458715596,-0.449541284,-0.440366972,-0.431192661,
-0.422018349,-0.412844037,-0.403669725,-0.39266055,-0.381651376,-0.370642202,
-0.359633028,-0.348623853,-0.337614679,-0.326605505,-0.31559633,-0.304587156,
-0.291743119,-0.278899083,-0.267889908,-0.256880734,-0.24587156,-0.234862385,
-0.223853211,-0.212844037,-0.201834862,-0.190825688,-0.179816514,-0.168807339,
-0.157798165,-0.143172102),.UNSPECIFIED.);
#24442=B_SPLINE_CURVE_WITH_KNOTS('',3,(#255435,#255436,#255437,#255438,
#255439,#255440,#255441,#255442,#255443,#255444,#255445,#255446,#255447,
#255448,#255449,#255450,#255451,#255452,#255453,#255454,#255455,#255456,
#255457,#255458,#255459,#255460,#255461,#255462,#255463,#255464,#255465,
#255466,#255467,#255468,#255469,#255470,#255471,#255472,#255473,#255474,
#255475,#255476,#255477,#255478,#255479,#255480,#255481,#255482,#255483,
#255484,#255485,#255486,#255487,#255488,#255489,#255490,#255491,#255492,
#255493,#255494,#255495,#255496,#255497,#255498,#255499,#255500,#255501,
#255502,#255503,#255504,#255505,#255506,#255507,#255508,#255509,#255510,
#255511,#255512,#255513,#255514,#255515,#255516,#255517,#255518,#255519,
#255520,#255521,#255522,#255523,#255524,#255525,#255526,#255527,#255528,
#255529,#255530,#255531,#255532,#255533,#255534,#255535,#255536,#255537,
#255538,#255539,#255540,#255541,#255542,#255543,#255544,#255545,#255546,
#255547,#255548,#255549,#255550,#255551,#255552,#255553,#255554,#255555,
#255556,#255557,#255558,#255559,#255560,#255561,#255562,#255563,#255564,
#255565,#255566,#255567,#255568,#255569,#255570,#255571,#255572,#255573,
#255574,#255575,#255576,#255577,#255578,#255579,#255580,#255581,#255582,
#255583,#255584,#255585,#255586,#255587,#255588,#255589,#255590,#255591,
#255592,#255593,#255594,#255595,#255596,#255597,#255598,#255599,#255600,
#255601,#255602,#255603,#255604,#255605,#255606,#255607,#255608,#255609,
#255610,#255611,#255612,#255613,#255614,#255615,#255616,#255617,#255618,
#255619,#255620,#255621,#255622,#255623,#255624,#255625,#255626,#255627,
#255628,#255629,#255630,#255631,#255632,#255633,#255634,#255635,#255636,
#255637,#255638,#255639,#255640,#255641,#255642,#255643,#255644,#255645,
#255646,#255647,#255648,#255649,#255650,#255651,#255652,#255653,#255654,
#255655,#255656,#255657,#255658,#255659,#255660,#255661,#255662,#255663,
#255664,#255665,#255666,#255667,#255668,#255669,#255670,#255671,#255672,
#255673,#255674,#255675,#255676,#255677,#255678,#255679,#255680,#255681,
#255682,#255683,#255684,#255685,#255686,#255687,#255688,#255689,#255690,
#255691,#255692,#255693,#255694,#255695,#255696,#255697,#255698,#255699,
#255700,#255701,#255702,#255703,#255704,#255705,#255706,#255707,#255708,
#255709,#255710,#255711,#255712,#255713,#255714,#255715,#255716,#255717,
#255718,#255719,#255720,#255721,#255722,#255723,#255724,#255725,#255726,
#255727,#255728,#255729,#255730,#255731,#255732,#255733,#255734,#255735,
#255736,#255737,#255738,#255739,#255740,#255741,#255742,#255743,#255744,
#255745,#255746,#255747),.UNSPECIFIED.,.F.,.F.,(4,3,3,3,3,3,3,3,3,3,3,3,
3,3,3,3,3,3,3,3,3,3,3,3,3,3,3,3,3,3,3,3,3,3,3,3,3,3,3,3,3,3,3,3,3,3,3,3,
3,3,3,3,3,3,3,3,3,3,3,3,3,3,3,3,3,3,3,3,3,3,3,3,3,3,3,3,3,3,3,3,3,3,3,3,
3,3,3,3,3,3,3,3,3,3,3,3,3,3,3,3,3,3,3,3,4),(0.143172102,0.15412844,0.165137615,
0.176146789,0.187155963,0.198165138,0.211009174,0.222018349,0.233027523,
0.244036697,0.255045872,0.266055046,0.27706422,0.288073394,0.299082569,
0.310091743,0.321100917,0.332110092,0.343119266,0.35412844,0.365137615,
0.376146789,0.387155963,0.396330275,0.405504587,0.414678899,0.423853211,
0.433027523,0.442201835,0.451376147,0.460550459,0.469724771,0.478899083,
0.488073394,0.497247706,0.506422018,0.519266055,0.528440367,0.537614679,
0.544954128,0.55412844,0.56146789,0.568807339,0.576146789,0.583486239,0.590825688,
0.598165138,0.605504587,0.612844037,0.620183486,0.627522936,0.63853211,
0.647706422,0.655045872,0.666055046,0.673394495,0.680733945,0.688073394,
0.695412844,0.702752294,0.710091743,0.719266055,0.726605505,0.733944954,
0.741284404,0.748623853,0.755963303,0.763302752,0.770642202,0.777981651,
0.787155963,0.794495413,0.801834862,0.809174312,0.818348624,0.823853211,
0.829357798,0.834862385,0.840366972,0.847706422,0.853211009,0.858715596,
0.864220183,0.873394495,0.878899083,0.888073394,0.893577982,0.899082569,
0.906422018,0.911926606,0.917431193,0.92293578,0.928440367,0.937614679,
0.943119266,0.948623853,0.95412844,0.959633028,0.966972477,0.972477064,
0.977981651,0.983486239,0.988990826,0.994495413,1.),.UNSPECIFIED.);
#24443=B_SPLINE_CURVE_WITH_KNOTS('',3,(#256710,#256711,#256712,#256713,
#256714,#256715,#256716,#256717,#256718,#256719,#256720,#256721,#256722,
#256723,#256724,#256725,#256726,#256727,#256728,#256729,#256730,#256731,
#256732,#256733,#256734,#256735,#256736,#256737,#256738,#256739,#256740,
#256741,#256742,#256743,#256744,#256745,#256746,#256747,#256748,#256749,
#256750,#256751,#256752,#256753,#256754,#256755,#256756,#256757,#256758,
#256759,#256760,#256761,#256762,#256763,#256764,#256765,#256766,#256767,
#256768,#256769,#256770,#256771,#256772,#256773,#256774,#256775,#256776,
#256777,#256778,#256779,#256780,#256781,#256782,#256783,#256784,#256785,
#256786,#256787,#256788,#256789,#256790,#256791,#256792,#256793,#256794,
#256795,#256796,#256797,#256798,#256799,#256800,#256801,#256802,#256803,
#256804,#256805,#256806,#256807,#256808,#256809,#256810,#256811,#256812,
#256813,#256814,#256815,#256816,#256817,#256818,#256819,#256820,#256821,
#256822,#256823,#256824,#256825,#256826,#256827,#256828,#256829,#256830,
#256831,#256832,#256833,#256834,#256835,#256836,#256837,#256838,#256839,
#256840,#256841,#256842,#256843,#256844,#256845,#256846,#256847,#256848,
#256849,#256850,#256851,#256852,#256853,#256854,#256855,#256856,#256857,
#256858,#256859,#256860,#256861,#256862,#256863,#256864,#256865,#256866,
#256867,#256868,#256869,#256870,#256871,#256872,#256873,#256874,#256875,
#256876,#256877,#256878,#256879,#256880,#256881,#256882,#256883,#256884,
#256885,#256886,#256887,#256888,#256889,#256890,#256891,#256892,#256893,
#256894,#256895,#256896,#256897,#256898,#256899,#256900,#256901,#256902,
#256903,#256904,#256905,#256906,#256907,#256908,#256909,#256910,#256911,
#256912,#256913,#256914,#256915,#256916,#256917,#256918,#256919,#256920,
#256921,#256922,#256923,#256924,#256925,#256926,#256927,#256928,#256929,
#256930,#256931,#256932,#256933,#256934,#256935,#256936,#256937,#256938,
#256939,#256940,#256941,#256942,#256943,#256944,#256945,#256946,#256947,
#256948,#256949,#256950,#256951,#256952,#256953,#256954,#256955,#256956,
#256957,#256958,#256959,#256960,#256961,#256962,#256963,#256964,#256965,
#256966,#256967,#256968,#256969,#256970,#256971,#256972,#256973,#256974,
#256975,#256976,#256977,#256978,#256979,#256980,#256981,#256982,#256983,
#256984,#256985,#256986,#256987,#256988,#256989,#256990,#256991,#256992,
#256993,#256994,#256995,#256996,#256997,#256998,#256999,#257000,#257001,
#257002,#257003,#257004,#257005,#257006,#257007,#257008,#257009,#257010,
#257011,#257012,#257013,#257014,#257015,#257016,#257017,#257018,#257019,
#257020,#257021,#257022,#257023,#257024,#257025,#257026,#257027,#257028,
#257029,#257030,#257031),.UNSPECIFIED.,.F.,.F.,(4,3,3,3,3,3,3,3,3,3,3,3,
3,3,3,3,3,3,3,3,3,3,3,3,3,3,3,3,3,3,3,3,3,3,3,3,3,3,3,3,3,3,3,3,3,3,3,3,
3,3,3,3,3,3,3,3,3,3,3,3,3,3,3,3,3,3,3,3,3,3,3,3,3,3,3,3,3,3,3,3,3,3,3,3,
3,3,3,3,3,3,3,3,3,3,3,3,3,3,3,3,3,3,3,3,3,3,3,4),(-1.,-0.99266055,-0.987155963,
-0.981651376,-0.976146789,-0.970642202,-0.965137615,-0.959633028,-0.95412844,
-0.948623853,-0.941284404,-0.935779817,-0.930275229,-0.924770642,-0.919266055,
-0.913761468,-0.908256881,-0.902752294,-0.897247706,-0.889908257,-0.88440367,
-0.878899083,-0.873394495,-0.867889908,-0.862385321,-0.855045872,-0.849541284,
-0.844036697,-0.83853211,-0.833027523,-0.827522936,-0.822018349,-0.814678899,
-0.809174312,-0.8,-0.79266055,-0.785321101,-0.777981651,-0.770642202,-0.763302752,
-0.755963303,-0.748623853,-0.741284404,-0.733944954,-0.726605505,-0.719266055,
-0.710091743,-0.702752294,-0.695412844,-0.688073394,-0.680733945,-0.671559633,
-0.664220183,-0.656880734,-0.649541284,-0.642201835,-0.634862385,-0.627522936,
-0.620183486,-0.612844037,-0.605504587,-0.598165138,-0.590825688,-0.583486239,
-0.576146789,-0.568807339,-0.56146789,-0.55412844,-0.546788991,-0.539449541,
-0.532110092,-0.521100917,-0.511926606,-0.502752294,-0.493577982,-0.48440367,
-0.475229358,-0.466055046,-0.456880734,-0.447706422,-0.43853211,-0.429357798,
-0.420183486,-0.411009174,-0.401834862,-0.39266055,-0.381651376,-0.370642202,
-0.359633028,-0.348623853,-0.337614679,-0.326605505,-0.31559633,-0.304587156,
-0.293577982,-0.282568807,-0.271559633,-0.260550459,-0.249541284,-0.23853211,
-0.227522936,-0.216513761,-0.205504587,-0.194495413,-0.183486239,-0.172477064,
-0.16146789,-0.143172102),.UNSPECIFIED.);
#24444=B_SPLINE_CURVE_WITH_KNOTS('',3,(#257032,#257033,#257034,#257035,
#257036,#257037,#257038,#257039,#257040,#257041,#257042,#257043,#257044,
#257045,#257046,#257047,#257048,#257049,#257050,#257051,#257052,#257053,
#257054,#257055,#257056,#257057,#257058,#257059,#257060,#257061,#257062,
#257063,#257064,#257065,#257066,#257067,#257068,#257069,#257070,#257071,
#257072,#257073,#257074,#257075,#257076,#257077,#257078,#257079,#257080,
#257081,#257082,#257083,#257084,#257085,#257086,#257087,#257088,#257089,
#257090,#257091,#257092,#257093,#257094,#257095,#257096,#257097,#257098,
#257099,#257100,#257101,#257102,#257103,#257104,#257105,#257106,#257107,
#257108,#257109,#257110,#257111,#257112,#257113,#257114,#257115,#257116,
#257117,#257118,#257119,#257120,#257121,#257122,#257123,#257124,#257125,
#257126,#257127,#257128,#257129,#257130,#257131,#257132,#257133,#257134,
#257135,#257136,#257137,#257138,#257139,#257140,#257141,#257142,#257143,
#257144,#257145,#257146,#257147,#257148,#257149,#257150,#257151,#257152,
#257153,#257154,#257155,#257156,#257157,#257158,#257159,#257160,#257161,
#257162,#257163,#257164,#257165,#257166,#257167,#257168,#257169,#257170,
#257171,#257172,#257173,#257174,#257175,#257176,#257177,#257178,#257179,
#257180,#257181,#257182,#257183,#257184,#257185,#257186,#257187,#257188,
#257189,#257190,#257191,#257192,#257193,#257194,#257195,#257196,#257197,
#257198,#257199,#257200,#257201,#257202,#257203,#257204,#257205,#257206,
#257207,#257208,#257209,#257210,#257211,#257212,#257213,#257214,#257215,
#257216,#257217,#257218,#257219,#257220,#257221,#257222,#257223,#257224,
#257225,#257226,#257227,#257228,#257229,#257230,#257231,#257232,#257233,
#257234,#257235,#257236,#257237,#257238,#257239,#257240,#257241,#257242,
#257243,#257244,#257245,#257246,#257247,#257248,#257249,#257250,#257251,
#257252,#257253,#257254,#257255,#257256,#257257,#257258,#257259,#257260,
#257261,#257262,#257263,#257264,#257265,#257266,#257267,#257268,#257269,
#257270,#257271,#257272,#257273,#257274,#257275,#257276,#257277,#257278,
#257279,#257280,#257281,#257282,#257283,#257284,#257285,#257286,#257287,
#257288,#257289,#257290,#257291,#257292,#257293,#257294,#257295,#257296,
#257297,#257298,#257299,#257300,#257301,#257302,#257303,#257304,#257305,
#257306,#257307,#257308,#257309,#257310,#257311,#257312,#257313,#257314,
#257315,#257316,#257317,#257318,#257319,#257320,#257321,#257322,#257323,
#257324,#257325,#257326,#257327,#257328,#257329,#257330,#257331,#257332,
#257333,#257334,#257335,#257336,#257337,#257338),.UNSPECIFIED.,.F.,.F.,
(4,3,3,3,3,3,3,3,3,3,3,3,3,3,3,3,3,3,3,3,3,3,3,3,3,3,3,3,3,3,3,3,3,3,3,
3,3,3,3,3,3,3,3,3,3,3,3,3,3,3,3,3,3,3,3,3,3,3,3,3,3,3,3,3,3,3,3,3,3,3,3,
3,3,3,3,3,3,3,3,3,3,3,3,3,3,3,3,3,3,3,3,3,3,3,3,3,3,3,3,3,3,3,4),(0.143172102,
0.15412844,0.165137615,0.176146789,0.187155963,0.198165138,0.211009174,
0.222018349,0.233027523,0.244036697,0.255045872,0.266055046,0.27706422,
0.288073394,0.299082569,0.310091743,0.321100917,0.332110092,0.344954128,
0.355963303,0.366972477,0.377981651,0.388990826,0.398165138,0.40733945,
0.416513761,0.427522936,0.436697248,0.44587156,0.456880734,0.467889908,
0.47706422,0.488073394,0.497247706,0.506422018,0.519266055,0.528440367,
0.537614679,0.544954128,0.55412844,0.56146789,0.568807339,0.576146789,0.587155963,
0.598165138,0.60733945,0.616513761,0.623853211,0.631192661,0.640366972,
0.649541284,0.656880734,0.667889908,0.675229358,0.682568807,0.689908257,
0.697247706,0.704587156,0.713761468,0.721100917,0.730275229,0.741284404,
0.748623853,0.755963303,0.763302752,0.770642202,0.777981651,0.785321101,
0.79266055,0.803669725,0.811009174,0.818348624,0.823853211,0.829357798,
0.834862385,0.840366972,0.84587156,0.851376147,0.856880734,0.862385321,
0.867889908,0.873394495,0.878899083,0.88440367,0.893577982,0.899082569,
0.904587156,0.910091743,0.91559633,0.921100917,0.928440367,0.935779817,
0.941284404,0.946788991,0.952293578,0.957798165,0.963302752,0.968807339,
0.974311927,0.979816514,0.985321101,0.99266055,1.),.UNSPECIFIED.);
#24445=B_SPLINE_CURVE_WITH_KNOTS('',3,(#258283,#258284,#258285,#258286,
#258287,#258288,#258289,#258290,#258291,#258292,#258293,#258294,#258295,
#258296,#258297,#258298,#258299,#258300,#258301,#258302,#258303,#258304,
#258305,#258306,#258307,#258308,#258309,#258310,#258311,#258312,#258313,
#258314,#258315,#258316,#258317,#258318,#258319,#258320,#258321,#258322,
#258323,#258324,#258325,#258326,#258327,#258328,#258329,#258330,#258331,
#258332,#258333,#258334,#258335,#258336,#258337,#258338,#258339,#258340,
#258341,#258342,#258343,#258344,#258345,#258346,#258347,#258348,#258349,
#258350,#258351,#258352,#258353,#258354,#258355,#258356,#258357,#258358,
#258359,#258360,#258361,#258362,#258363,#258364,#258365,#258366,#258367,
#258368,#258369,#258370,#258371,#258372,#258373,#258374,#258375,#258376,
#258377,#258378,#258379,#258380,#258381,#258382,#258383,#258384,#258385,
#258386,#258387,#258388,#258389,#258390,#258391,#258392,#258393,#258394,
#258395,#258396,#258397,#258398,#258399,#258400,#258401,#258402,#258403,
#258404,#258405,#258406,#258407,#258408,#258409,#258410,#258411,#258412,
#258413,#258414,#258415,#258416,#258417,#258418,#258419,#258420,#258421,
#258422,#258423,#258424,#258425,#258426,#258427,#258428,#258429,#258430,
#258431,#258432,#258433,#258434,#258435,#258436,#258437,#258438,#258439,
#258440,#258441,#258442,#258443,#258444,#258445,#258446,#258447,#258448,
#258449,#258450,#258451,#258452,#258453,#258454,#258455,#258456,#258457,
#258458,#258459,#258460,#258461,#258462,#258463,#258464,#258465,#258466,
#258467,#258468,#258469,#258470,#258471,#258472,#258473,#258474,#258475,
#258476,#258477,#258478,#258479,#258480,#258481,#258482,#258483,#258484,
#258485,#258486,#258487,#258488,#258489,#258490,#258491,#258492,#258493,
#258494,#258495,#258496,#258497,#258498,#258499,#258500,#258501,#258502,
#258503,#258504,#258505,#258506,#258507,#258508,#258509,#258510,#258511,
#258512,#258513,#258514,#258515,#258516,#258517,#258518,#258519,#258520,
#258521,#258522,#258523,#258524,#258525,#258526,#258527,#258528,#258529,
#258530,#258531,#258532,#258533,#258534,#258535,#258536,#258537,#258538,
#258539,#258540,#258541,#258542,#258543,#258544,#258545,#258546,#258547,
#258548,#258549,#258550,#258551,#258552,#258553,#258554,#258555,#258556,
#258557,#258558,#258559,#258560,#258561,#258562,#258563,#258564,#258565,
#258566,#258567,#258568,#258569,#258570,#258571,#258572,#258573,#258574),
 .UNSPECIFIED.,.F.,.F.,(4,3,3,3,3,3,3,3,3,3,3,3,3,3,3,3,3,3,3,3,3,3,3,3,
3,3,3,3,3,3,3,3,3,3,3,3,3,3,3,3,3,3,3,3,3,3,3,3,3,3,3,3,3,3,3,3,3,3,3,3,
3,3,3,3,3,3,3,3,3,3,3,3,3,3,3,3,3,3,3,3,3,3,3,3,3,3,3,3,3,3,3,3,3,3,3,3,
3,4),(0.143172102,0.15412844,0.165137615,0.176146789,0.187155963,0.198165138,
0.211009174,0.222018349,0.234862385,0.24587156,0.256880734,0.267889908,
0.278899083,0.289908257,0.300917431,0.311926606,0.32293578,0.333944954,
0.346788991,0.357798165,0.368807339,0.379816514,0.39266055,0.403669725,
0.412844037,0.423853211,0.433027523,0.444036697,0.453211009,0.466055046,
0.482568807,0.491743119,0.500917431,0.510091743,0.519266055,0.533944954,
0.541284404,0.548623853,0.555963303,0.565137615,0.572477064,0.579816514,
0.587155963,0.596330275,0.605504587,0.614678899,0.622018349,0.629357798,
0.636697248,0.64587156,0.655045872,0.664220183,0.67706422,0.686238532,0.693577982,
0.700917431,0.710091743,0.721100917,0.728440367,0.735779817,0.743119266,
0.750458716,0.757798165,0.766972477,0.774311927,0.781651376,0.790825688,
0.798165138,0.80733945,0.812844037,0.818348624,0.825688073,0.831192661,
0.836697248,0.842201835,0.851376147,0.856880734,0.864220183,0.873394495,
0.878899083,0.888073394,0.893577982,0.900917431,0.908256881,0.91559633,
0.92293578,0.930275229,0.939449541,0.944954128,0.950458716,0.955963303,
0.96146789,0.966972477,0.974311927,0.981651376,0.988990826,0.994495413,
1.),.UNSPECIFIED.);
#24446=B_SPLINE_CURVE_WITH_KNOTS('',3,(#258575,#258576,#258577,#258578,
#258579,#258580,#258581,#258582,#258583,#258584,#258585,#258586,#258587,
#258588,#258589,#258590,#258591,#258592,#258593,#258594,#258595,#258596,
#258597,#258598,#258599,#258600,#258601,#258602,#258603,#258604,#258605,
#258606,#258607,#258608,#258609,#258610,#258611,#258612,#258613,#258614,
#258615,#258616,#258617,#258618,#258619,#258620,#258621,#258622,#258623,
#258624,#258625,#258626,#258627,#258628,#258629,#258630,#258631,#258632,
#258633,#258634,#258635,#258636,#258637,#258638,#258639,#258640,#258641,
#258642,#258643,#258644,#258645,#258646,#258647,#258648,#258649,#258650,
#258651,#258652,#258653,#258654,#258655,#258656,#258657,#258658,#258659,
#258660,#258661,#258662,#258663,#258664,#258665,#258666,#258667,#258668,
#258669,#258670,#258671,#258672,#258673,#258674,#258675,#258676,#258677,
#258678,#258679,#258680,#258681,#258682,#258683,#258684,#258685,#258686,
#258687,#258688,#258689,#258690,#258691,#258692,#258693,#258694,#258695,
#258696,#258697,#258698,#258699,#258700,#258701,#258702,#258703,#258704,
#258705,#258706,#258707,#258708,#258709,#258710,#258711,#258712,#258713,
#258714,#258715,#258716,#258717,#258718,#258719,#258720,#258721,#258722,
#258723,#258724,#258725,#258726,#258727,#258728,#258729,#258730,#258731,
#258732,#258733,#258734,#258735,#258736,#258737,#258738,#258739,#258740,
#258741,#258742,#258743,#258744,#258745,#258746,#258747,#258748,#258749,
#258750,#258751,#258752,#258753,#258754,#258755,#258756,#258757,#258758,
#258759,#258760,#258761,#258762,#258763,#258764,#258765,#258766,#258767,
#258768,#258769,#258770,#258771,#258772,#258773,#258774,#258775,#258776,
#258777,#258778,#258779,#258780,#258781,#258782,#258783,#258784,#258785,
#258786,#258787,#258788,#258789,#258790,#258791,#258792,#258793,#258794,
#258795,#258796,#258797,#258798,#258799,#258800,#258801,#258802,#258803,
#258804,#258805,#258806,#258807,#258808,#258809,#258810,#258811,#258812,
#258813,#258814,#258815,#258816,#258817,#258818,#258819,#258820,#258821,
#258822,#258823,#258824,#258825,#258826,#258827,#258828,#258829,#258830,
#258831,#258832,#258833,#258834,#258835,#258836,#258837,#258838,#258839,
#258840,#258841,#258842,#258843,#258844,#258845,#258846,#258847,#258848,
#258849,#258850,#258851,#258852,#258853,#258854,#258855,#258856,#258857,
#258858,#258859,#258860,#258861,#258862,#258863,#258864,#258865,#258866,
#258867,#258868,#258869,#258870,#258871,#258872,#258873,#258874,#258875,
#258876,#258877,#258878,#258879,#258880,#258881,#258882,#258883,#258884,
#258885,#258886,#258887,#258888,#258889,#258890,#258891,#258892,#258893,
#258894,#258895,#258896),.UNSPECIFIED.,.F.,.F.,(4,3,3,3,3,3,3,3,3,3,3,3,
3,3,3,3,3,3,3,3,3,3,3,3,3,3,3,3,3,3,3,3,3,3,3,3,3,3,3,3,3,3,3,3,3,3,3,3,
3,3,3,3,3,3,3,3,3,3,3,3,3,3,3,3,3,3,3,3,3,3,3,3,3,3,3,3,3,3,3,3,3,3,3,3,
3,3,3,3,3,3,3,3,3,3,3,3,3,3,3,3,3,3,3,3,3,3,3,4),(0.143172102,0.15412844,
0.165137615,0.176146789,0.187155963,0.198165138,0.209174312,0.220183486,
0.231192661,0.244036697,0.255045872,0.266055046,0.27706422,0.288073394,
0.299082569,0.310091743,0.321100917,0.332110092,0.343119266,0.355963303,
0.368807339,0.379816514,0.39266055,0.401834862,0.411009174,0.420183486,
0.429357798,0.43853211,0.447706422,0.456880734,0.466055046,0.475229358,
0.48440367,0.493577982,0.502752294,0.511926606,0.521100917,0.530275229,
0.537614679,0.546788991,0.55412844,0.56146789,0.568807339,0.576146789,0.583486239,
0.590825688,0.6,0.60733945,0.614678899,0.622018349,0.629357798,0.636697248,
0.644036697,0.651376147,0.658715596,0.667889908,0.675229358,0.682568807,
0.689908257,0.697247706,0.704587156,0.711926606,0.719266055,0.726605505,
0.733944954,0.743119266,0.750458716,0.757798165,0.765137615,0.772477064,
0.779816514,0.787155963,0.794495413,0.801834862,0.809174312,0.816513761,
0.822018349,0.827522936,0.833027523,0.83853211,0.844036697,0.849541284,
0.855045872,0.860550459,0.866055046,0.871559633,0.87706422,0.882568807,
0.888073394,0.893577982,0.899082569,0.904587156,0.910091743,0.91559633,
0.921100917,0.928440367,0.933944954,0.939449541,0.944954128,0.950458716,
0.955963303,0.96146789,0.966972477,0.972477064,0.979816514,0.987155963,
0.99266055,1.),.UNSPECIFIED.);
#24447=B_SPLINE_CURVE_WITH_KNOTS('',5,(#259856,#259857,#259858,#259859,
#259860,#259861,#259862,#259863,#259864,#259865,#259866,#259867,#259868,
#259869,#259870,#259871,#259872,#259873,#259874,#259875,#259876,#259877,
#259878,#259879,#259880,#259881,#259882,#259883,#259884,#259885,#259886,
#259887,#259888,#259889,#259890,#259891,#259892,#259893,#259894,#259895,
#259896,#259897,#259898,#259899,#259900,#259901,#259902,#259903,#259904,
#259905,#259906,#259907,#259908,#259909,#259910,#259911,#259912,#259913,
#259914,#259915,#259916,#259917,#259918,#259919,#259920,#259921,#259922,
#259923,#259924,#259925,#259926,#259927,#259928,#259929,#259930,#259931,
#259932,#259933,#259934,#259935,#259936,#259937,#259938,#259939,#259940,
#259941,#259942,#259943,#259944,#259945,#259946,#259947,#259948,#259949,
#259950,#259951,#259952,#259953,#259954,#259955,#259956,#259957,#259958,
#259959,#259960,#259961,#259962,#259963,#259964,#259965,#259966,#259967,
#259968,#259969,#259970,#259971,#259972,#259973,#259974,#259975,#259976,
#259977,#259978,#259979,#259980,#259981,#259982,#259983,#259984,#259985,
#259986,#259987,#259988,#259989,#259990,#259991,#259992,#259993,#259994,
#259995,#259996,#259997,#259998,#259999,#260000,#260001,#260002,#260003,
#260004,#260005,#260006,#260007,#260008,#260009,#260010,#260011,#260012,
#260013,#260014,#260015,#260016,#260017,#260018,#260019,#260020,#260021,
#260022,#260023,#260024,#260025,#260026,#260027,#260028,#260029,#260030,
#260031,#260032,#260033,#260034,#260035,#260036,#260037,#260038,#260039,
#260040,#260041,#260042,#260043,#260044,#260045,#260046,#260047,#260048,
#260049,#260050,#260051,#260052,#260053,#260054,#260055,#260056,#260057,
#260058,#260059,#260060,#260061,#260062,#260063,#260064,#260065,#260066,
#260067,#260068,#260069,#260070,#260071,#260072,#260073,#260074,#260075,
#260076,#260077,#260078,#260079,#260080,#260081,#260082,#260083,#260084,
#260085,#260086,#260087,#260088,#260089,#260090,#260091,#260092,#260093,
#260094,#260095,#260096,#260097,#260098,#260099,#260100,#260101,#260102,
#260103,#260104,#260105,#260106,#260107,#260108,#260109,#260110,#260111,
#260112,#260113,#260114,#260115,#260116,#260117,#260118,#260119,#260120,
#260121,#260122,#260123,#260124,#260125,#260126,#260127,#260128,#260129,
#260130,#260131,#260132,#260133,#260134,#260135,#260136,#260137,#260138,
#260139,#260140,#260141,#260142,#260143,#260144,#260145,#260146,#260147,
#260148,#260149,#260150,#260151,#260152,#260153,#260154,#260155,#260156,
#260157,#260158,#260159,#260160,#260161,#260162,#260163,#260164,#260165,
#260166,#260167,#260168,#260169,#260170,#260171,#260172,#260173,#260174,
#260175,#260176,#260177,#260178,#260179,#260180,#260181,#260182,#260183,
#260184,#260185,#260186,#260187,#260188,#260189,#260190,#260191,#260192,
#260193,#260194,#260195,#260196,#260197,#260198,#260199,#260200,#260201,
#260202,#260203,#260204,#260205,#260206,#260207,#260208,#260209,#260210,
#260211,#260212,#260213,#260214,#260215,#260216,#260217,#260218,#260219,
#260220,#260221,#260222,#260223,#260224,#260225,#260226,#260227,#260228,
#260229,#260230,#260231,#260232,#260233,#260234,#260235,#260236,#260237,
#260238,#260239,#260240,#260241,#260242,#260243,#260244,#260245,#260246,
#260247,#260248,#260249,#260250,#260251,#260252,#260253,#260254,#260255,
#260256,#260257,#260258,#260259,#260260,#260261,#260262,#260263,#260264,
#260265,#260266,#260267,#260268,#260269,#260270,#260271,#260272,#260273,
#260274,#260275,#260276,#260277,#260278,#260279,#260280,#260281,#260282,
#260283,#260284,#260285,#260286,#260287,#260288,#260289,#260290,#260291,
#260292,#260293,#260294,#260295,#260296,#260297,#260298,#260299,#260300,
#260301,#260302,#260303,#260304,#260305,#260306,#260307,#260308,#260309,
#260310,#260311,#260312,#260313,#260314,#260315,#260316,#260317,#260318,
#260319,#260320,#260321,#260322,#260323,#260324,#260325,#260326),
 .UNSPECIFIED.,.F.,.F.,(6,1,1,1,1,1,1,1,1,1,1,1,1,1,1,1,1,1,1,1,1,1,1,1,
1,1,1,1,1,1,1,1,1,1,1,1,1,1,1,1,1,1,1,1,1,1,1,1,1,1,1,1,1,1,1,1,1,1,1,1,
1,1,1,1,1,1,1,1,1,1,1,1,1,1,1,1,1,1,1,1,1,1,1,1,1,1,1,1,1,1,1,1,1,1,1,1,
1,1,1,1,1,1,1,1,1,1,1,1,1,1,1,1,1,1,1,1,1,1,1,1,1,1,1,1,1,1,1,1,1,1,1,1,
1,1,1,1,1,1,1,1,1,1,1,1,1,1,1,1,1,1,1,1,1,1,1,1,1,1,1,1,1,1,1,1,1,1,1,1,
1,1,1,1,1,1,1,1,1,1,1,1,1,1,1,1,1,1,1,1,1,1,1,1,1,1,1,1,1,1,1,1,1,1,1,1,
1,1,1,1,1,1,1,1,1,1,1,1,1,1,1,1,1,1,1,1,1,1,1,1,1,1,1,1,1,1,1,1,1,1,1,1,
1,1,1,1,1,1,1,1,1,1,1,1,1,1,1,1,1,1,1,1,1,1,1,1,1,1,1,1,1,1,1,1,1,1,1,1,
1,1,1,1,1,1,1,1,1,1,1,1,1,1,1,1,1,1,1,1,1,1,1,1,1,1,1,1,1,1,1,1,1,1,1,1,
1,1,1,1,1,1,1,1,1,1,1,1,1,1,1,1,1,1,1,1,1,1,1,1,1,1,1,1,1,1,1,1,1,1,1,1,
1,1,1,1,1,1,1,1,1,1,1,1,1,1,1,1,1,1,1,1,1,1,1,1,1,1,1,1,1,1,1,1,1,1,1,1,
1,1,1,1,1,1,1,1,1,1,1,1,1,1,1,1,1,1,1,1,1,1,1,1,1,1,1,1,1,1,1,1,1,1,1,1,
1,1,1,1,1,1,1,1,1,1,1,1,1,1,1,1,1,1,1,1,1,1,1,1,1,1,1,1,1,1,1,1,1,1,1,1,
1,1,1,1,1,1,1,1,1,1,6),(0.143172102,0.144954128,0.146788991,0.148623853,
0.150458716,0.152293578,0.15412844,0.155963303,0.157798165,0.159633028,
0.16146789,0.163302752,0.165137615,0.166972477,0.168807339,0.170642202,
0.172477064,0.174311927,0.176146789,0.177981651,0.179816514,0.181651376,
0.183486239,0.185321101,0.187155963,0.188990826,0.190825688,0.19266055,
0.194495413,0.196330275,0.198165138,0.2,0.201834862,0.203669725,0.205504587,
0.20733945,0.209174312,0.211009174,0.212844037,0.214678899,0.216513761,
0.218348624,0.220183486,0.222018349,0.223853211,0.225688073,0.227522936,
0.229357798,0.231192661,0.233027523,0.234862385,0.236697248,0.23853211,
0.240366972,0.242201835,0.244036697,0.24587156,0.247706422,0.249541284,
0.251376147,0.253211009,0.255045872,0.256880734,0.258715596,0.260550459,
0.262385321,0.264220183,0.266055046,0.267889908,0.269724771,0.271559633,
0.273394495,0.275229358,0.27706422,0.278899083,0.280733945,0.282568807,
0.28440367,0.286238532,0.288073394,0.289908257,0.291743119,0.293577982,
0.295412844,0.297247706,0.299082569,0.300917431,0.302752294,0.304587156,
0.306422018,0.308256881,0.310091743,0.311926606,0.313761468,0.31559633,
0.317431193,0.319266055,0.321100917,0.32293578,0.324770642,0.326605505,
0.328440367,0.330275229,0.332110092,0.333944954,0.335779817,0.337614679,
0.339449541,0.341284404,0.343119266,0.344954128,0.346788991,0.348623853,
0.350458716,0.352293578,0.35412844,0.355963303,0.357798165,0.359633028,
0.36146789,0.363302752,0.365137615,0.366972477,0.368807339,0.370642202,
0.372477064,0.374311927,0.376146789,0.377981651,0.379816514,0.381651376,
0.383486239,0.385321101,0.387155963,0.388990826,0.390825688,0.39266055,
0.394495413,0.396330275,0.398165138,0.4,0.401834862,0.403669725,0.405504587,
0.40733945,0.409174312,0.411009174,0.412844037,0.414678899,0.416513761,
0.418348624,0.420183486,0.422018349,0.423853211,0.425688073,0.427522936,
0.429357798,0.431192661,0.433027523,0.434862385,0.436697248,0.43853211,
0.440366972,0.442201835,0.444036697,0.44587156,0.447706422,0.449541284,
0.451376147,0.453211009,0.455045872,0.456880734,0.458715596,0.460550459,
0.462385321,0.464220183,0.466055046,0.467889908,0.469724771,0.471559633,
0.473394495,0.475229358,0.47706422,0.478899083,0.480733945,0.482568807,
0.48440367,0.486238532,0.488073394,0.489908257,0.491743119,0.493577982,
0.495412844,0.497247706,0.499082569,0.500917431,0.502752294,0.504587156,
0.506422018,0.508256881,0.510091743,0.511926606,0.513761468,0.51559633,
0.517431193,0.519266055,0.521100917,0.52293578,0.524770642,0.526605505,
0.528440367,0.530275229,0.532110092,0.533944954,0.535779817,0.537614679,
0.539449541,0.541284404,0.543119266,0.544954128,0.546788991,0.548623853,
0.550458716,0.552293578,0.55412844,0.555963303,0.557798165,0.559633028,
0.56146789,0.563302752,0.565137615,0.566972477,0.568807339,0.570642202,
0.572477064,0.574311927,0.577981651,0.579816514,0.581651376,0.583486239,
0.585321101,0.587155963,0.588990826,0.590825688,0.59266055,0.594495413,
0.596330275,0.598165138,0.6,0.601834862,0.603669725,0.605504587,0.60733945,
0.609174312,0.611009174,0.612844037,0.614678899,0.616513761,0.618348624,
0.620183486,0.622018349,0.623853211,0.625688073,0.627522936,0.629357798,
0.631192661,0.633027523,0.634862385,0.636697248,0.63853211,0.640366972,
0.642201835,0.644036697,0.64587156,0.647706422,0.649541284,0.651376147,
0.653211009,0.655045872,0.656880734,0.658715596,0.660550459,0.662385321,
0.664220183,0.666055046,0.667889908,0.669724771,0.671559633,0.673394495,
0.675229358,0.67706422,0.678899083,0.680733945,0.682568807,0.68440367,0.686238532,
0.688073394,0.689908257,0.691743119,0.693577982,0.695412844,0.697247706,
0.699082569,0.700917431,0.702752294,0.704587156,0.706422018,0.708256881,
0.710091743,0.711926606,0.713761468,0.71559633,0.717431193,0.719266055,
0.721100917,0.72293578,0.724770642,0.726605505,0.728440367,0.730275229,
0.732110092,0.733944954,0.735779817,0.737614679,0.739449541,0.741284404,
0.743119266,0.744954128,0.746788991,0.748623853,0.750458716,0.752293578,
0.75412844,0.755963303,0.757798165,0.759633028,0.76146789,0.763302752,0.765137615,
0.766972477,0.768807339,0.770642202,0.772477064,0.774311927,0.776146789,
0.777981651,0.779816514,0.781651376,0.783486239,0.785321101,0.787155963,
0.788990826,0.790825688,0.79266055,0.794495413,0.796330275,0.798165138,
0.8,0.801834862,0.803669725,0.805504587,0.80733945,0.809174312,0.811009174,
0.812844037,0.814678899,0.816513761,0.818348624,0.820183486,0.822018349,
0.823853211,0.825688073,0.827522936,0.829357798,0.831192661,0.833027523,
0.834862385,0.836697248,0.83853211,0.840366972,0.842201835,0.844036697,
0.84587156,0.847706422,0.849541284,0.851376147,0.853211009,0.855045872,
0.856880734,0.858715596,0.860550459,0.862385321,0.864220183,0.866055046,
0.867889908,0.869724771,0.871559633,0.873394495,0.875229358,0.87706422,
0.878899083,0.880733945,0.882568807,0.88440367,0.886238532,0.888073394,
0.889908257,0.891743119,0.893577982,0.895412844,0.897247706,0.899082569,
0.900917431,0.902752294,0.904587156,0.906422018,0.908256881,0.910091743,
0.911926606,0.913761468,0.91559633,0.917431193,0.919266055,0.921100917,
0.92293578,0.924770642,0.926605505,0.928440367,0.930275229,0.932110092,
0.933944954,0.935779817,0.937614679,0.939449541,0.941284404,0.943119266,
0.944954128,0.946788991,0.948623853,0.950458716,0.952293578,0.95412844,
0.955963303,0.957798165,0.959633028,0.96146789,0.963302752,0.965137615,
0.966972477,0.968807339,0.970642202,0.972477064,0.974311927,0.976146789,
0.977981651,0.979816514,0.981651376,0.983486239,0.985321101,0.987155963,
0.988990826,0.990825688,0.99266055,0.994495413,0.996330275,0.998165138,
1.),.UNSPECIFIED.);
#24448=B_SPLINE_CURVE_WITH_KNOTS('',5,(#260327,#260328,#260329,#260330,
#260331,#260332,#260333,#260334,#260335,#260336,#260337,#260338,#260339,
#260340,#260341,#260342,#260343,#260344,#260345,#260346,#260347,#260348,
#260349,#260350,#260351,#260352,#260353,#260354,#260355,#260356,#260357,
#260358,#260359,#260360,#260361,#260362,#260363,#260364,#260365,#260366,
#260367,#260368,#260369,#260370,#260371,#260372,#260373,#260374,#260375,
#260376,#260377,#260378,#260379,#260380,#260381,#260382,#260383,#260384,
#260385,#260386,#260387,#260388,#260389,#260390,#260391,#260392,#260393,
#260394,#260395,#260396,#260397,#260398,#260399,#260400,#260401,#260402,
#260403,#260404,#260405,#260406,#260407,#260408,#260409,#260410,#260411,
#260412,#260413,#260414,#260415,#260416,#260417,#260418,#260419,#260420,
#260421,#260422,#260423,#260424,#260425,#260426,#260427,#260428,#260429,
#260430,#260431,#260432,#260433,#260434,#260435,#260436,#260437,#260438,
#260439,#260440,#260441,#260442,#260443,#260444,#260445,#260446,#260447,
#260448,#260449,#260450,#260451,#260452,#260453,#260454,#260455,#260456,
#260457,#260458,#260459,#260460,#260461,#260462,#260463,#260464,#260465,
#260466,#260467,#260468,#260469,#260470,#260471,#260472,#260473,#260474,
#260475,#260476,#260477,#260478,#260479,#260480,#260481,#260482,#260483,
#260484,#260485,#260486,#260487,#260488,#260489,#260490,#260491,#260492,
#260493,#260494,#260495,#260496,#260497,#260498,#260499,#260500,#260501,
#260502,#260503,#260504,#260505,#260506,#260507,#260508,#260509,#260510,
#260511,#260512,#260513,#260514,#260515,#260516,#260517,#260518,#260519,
#260520,#260521,#260522,#260523,#260524,#260525,#260526,#260527,#260528,
#260529,#260530,#260531,#260532,#260533,#260534,#260535,#260536,#260537,
#260538,#260539,#260540,#260541,#260542,#260543,#260544,#260545,#260546,
#260547,#260548,#260549,#260550,#260551,#260552,#260553,#260554,#260555,
#260556,#260557,#260558,#260559,#260560,#260561,#260562,#260563,#260564,
#260565,#260566,#260567,#260568,#260569,#260570,#260571,#260572,#260573,
#260574,#260575,#260576,#260577,#260578,#260579,#260580,#260581,#260582,
#260583,#260584,#260585,#260586,#260587,#260588,#260589,#260590,#260591,
#260592,#260593,#260594,#260595,#260596,#260597,#260598,#260599,#260600,
#260601,#260602,#260603,#260604,#260605,#260606,#260607,#260608,#260609,
#260610,#260611,#260612,#260613,#260614,#260615,#260616,#260617,#260618,
#260619,#260620,#260621,#260622,#260623,#260624,#260625,#260626,#260627,
#260628,#260629,#260630,#260631,#260632,#260633,#260634,#260635,#260636,
#260637,#260638,#260639,#260640,#260641,#260642,#260643,#260644,#260645,
#260646,#260647,#260648,#260649,#260650,#260651,#260652,#260653,#260654,
#260655,#260656,#260657,#260658,#260659,#260660,#260661,#260662,#260663,
#260664,#260665,#260666,#260667,#260668,#260669,#260670,#260671,#260672,
#260673,#260674,#260675,#260676,#260677,#260678,#260679,#260680,#260681,
#260682,#260683,#260684,#260685,#260686,#260687,#260688,#260689,#260690,
#260691,#260692,#260693,#260694,#260695,#260696,#260697,#260698,#260699,
#260700,#260701,#260702,#260703,#260704,#260705,#260706,#260707,#260708,
#260709,#260710,#260711,#260712,#260713,#260714,#260715,#260716,#260717,
#260718,#260719,#260720,#260721,#260722,#260723,#260724,#260725,#260726,
#260727,#260728,#260729,#260730,#260731,#260732,#260733,#260734,#260735,
#260736,#260737,#260738,#260739,#260740,#260741,#260742,#260743,#260744,
#260745,#260746,#260747,#260748,#260749,#260750,#260751,#260752,#260753,
#260754,#260755,#260756,#260757,#260758,#260759,#260760,#260761,#260762,
#260763,#260764,#260765,#260766,#260767,#260768,#260769,#260770,#260771,
#260772,#260773,#260774,#260775,#260776,#260777,#260778,#260779,#260780,
#260781,#260782,#260783,#260784,#260785,#260786,#260787,#260788,#260789,
#260790,#260791,#260792,#260793,#260794,#260795,#260796,#260797),
 .UNSPECIFIED.,.F.,.F.,(6,1,1,1,1,1,1,1,1,1,1,1,1,1,1,1,1,1,1,1,1,1,1,1,
1,1,1,1,1,1,1,1,1,1,1,1,1,1,1,1,1,1,1,1,1,1,1,1,1,1,1,1,1,1,1,1,1,1,1,1,
1,1,1,1,1,1,1,1,1,1,1,1,1,1,1,1,1,1,1,1,1,1,1,1,1,1,1,1,1,1,1,1,1,1,1,1,
1,1,1,1,1,1,1,1,1,1,1,1,1,1,1,1,1,1,1,1,1,1,1,1,1,1,1,1,1,1,1,1,1,1,1,1,
1,1,1,1,1,1,1,1,1,1,1,1,1,1,1,1,1,1,1,1,1,1,1,1,1,1,1,1,1,1,1,1,1,1,1,1,
1,1,1,1,1,1,1,1,1,1,1,1,1,1,1,1,1,1,1,1,1,1,1,1,1,1,1,1,1,1,1,1,1,1,1,1,
1,1,1,1,1,1,1,1,1,1,1,1,1,1,1,1,1,1,1,1,1,1,1,1,1,1,1,1,1,1,1,1,1,1,1,1,
1,1,1,1,1,1,1,1,1,1,1,1,1,1,1,1,1,1,1,1,1,1,1,1,1,1,1,1,1,1,1,1,1,1,1,1,
1,1,1,1,1,1,1,1,1,1,1,1,1,1,1,1,1,1,1,1,1,1,1,1,1,1,1,1,1,1,1,1,1,1,1,1,
1,1,1,1,1,1,1,1,1,1,1,1,1,1,1,1,1,1,1,1,1,1,1,1,1,1,1,1,1,1,1,1,1,1,1,1,
1,1,1,1,1,1,1,1,1,1,1,1,1,1,1,1,1,1,1,1,1,1,1,1,1,1,1,1,1,1,1,1,1,1,1,1,
1,1,1,1,1,1,1,1,1,1,1,1,1,1,1,1,1,1,1,1,1,1,1,1,1,1,1,1,1,1,1,1,1,1,1,1,
1,1,1,1,1,1,1,1,1,1,1,1,1,1,1,1,1,1,1,1,1,1,1,1,1,1,1,1,1,1,1,1,1,1,1,1,
1,1,1,1,1,1,1,1,1,1,6),(0.143172102,0.144954128,0.146788991,0.148623853,
0.150458716,0.152293578,0.15412844,0.155963303,0.157798165,0.159633028,
0.16146789,0.163302752,0.165137615,0.166972477,0.168807339,0.170642202,
0.172477064,0.174311927,0.176146789,0.177981651,0.179816514,0.181651376,
0.183486239,0.185321101,0.187155963,0.188990826,0.190825688,0.19266055,
0.194495413,0.196330275,0.198165138,0.2,0.201834862,0.203669725,0.205504587,
0.20733945,0.209174312,0.211009174,0.212844037,0.214678899,0.216513761,
0.218348624,0.220183486,0.222018349,0.223853211,0.225688073,0.227522936,
0.229357798,0.231192661,0.233027523,0.234862385,0.236697248,0.23853211,
0.240366972,0.242201835,0.244036697,0.24587156,0.247706422,0.249541284,
0.251376147,0.253211009,0.255045872,0.256880734,0.258715596,0.260550459,
0.262385321,0.264220183,0.266055046,0.267889908,0.269724771,0.271559633,
0.273394495,0.275229358,0.27706422,0.278899083,0.280733945,0.282568807,
0.28440367,0.286238532,0.288073394,0.289908257,0.291743119,0.293577982,
0.295412844,0.297247706,0.299082569,0.300917431,0.302752294,0.304587156,
0.306422018,0.308256881,0.310091743,0.311926606,0.313761468,0.31559633,
0.317431193,0.319266055,0.321100917,0.32293578,0.324770642,0.326605505,
0.328440367,0.330275229,0.332110092,0.333944954,0.335779817,0.337614679,
0.339449541,0.341284404,0.343119266,0.344954128,0.346788991,0.348623853,
0.350458716,0.352293578,0.35412844,0.355963303,0.357798165,0.359633028,
0.36146789,0.363302752,0.365137615,0.366972477,0.368807339,0.370642202,
0.372477064,0.374311927,0.376146789,0.377981651,0.379816514,0.381651376,
0.383486239,0.385321101,0.387155963,0.388990826,0.390825688,0.39266055,
0.394495413,0.396330275,0.398165138,0.4,0.401834862,0.403669725,0.405504587,
0.40733945,0.409174312,0.411009174,0.412844037,0.414678899,0.416513761,
0.418348624,0.420183486,0.422018349,0.423853211,0.425688073,0.427522936,
0.429357798,0.431192661,0.433027523,0.434862385,0.436697248,0.43853211,
0.440366972,0.442201835,0.444036697,0.44587156,0.447706422,0.449541284,
0.451376147,0.453211009,0.455045872,0.456880734,0.458715596,0.460550459,
0.462385321,0.464220183,0.466055046,0.467889908,0.469724771,0.471559633,
0.473394495,0.475229358,0.47706422,0.478899083,0.480733945,0.482568807,
0.48440367,0.486238532,0.488073394,0.489908257,0.491743119,0.493577982,
0.495412844,0.497247706,0.499082569,0.500917431,0.502752294,0.504587156,
0.506422018,0.508256881,0.510091743,0.511926606,0.513761468,0.51559633,
0.517431193,0.519266055,0.521100917,0.52293578,0.524770642,0.526605505,
0.528440367,0.530275229,0.532110092,0.533944954,0.535779817,0.537614679,
0.539449541,0.541284404,0.543119266,0.544954128,0.546788991,0.548623853,
0.550458716,0.552293578,0.55412844,0.555963303,0.557798165,0.559633028,
0.56146789,0.563302752,0.565137615,0.566972477,0.568807339,0.570642202,
0.572477064,0.574311927,0.577981651,0.579816514,0.581651376,0.583486239,
0.585321101,0.587155963,0.588990826,0.590825688,0.59266055,0.594495413,
0.596330275,0.598165138,0.6,0.601834862,0.603669725,0.605504587,0.60733945,
0.609174312,0.611009174,0.612844037,0.614678899,0.616513761,0.618348624,
0.620183486,0.622018349,0.623853211,0.625688073,0.627522936,0.629357798,
0.631192661,0.633027523,0.634862385,0.636697248,0.63853211,0.640366972,
0.642201835,0.644036697,0.64587156,0.647706422,0.649541284,0.651376147,
0.653211009,0.655045872,0.656880734,0.658715596,0.660550459,0.662385321,
0.664220183,0.666055046,0.667889908,0.669724771,0.671559633,0.673394495,
0.675229358,0.67706422,0.678899083,0.680733945,0.682568807,0.68440367,0.686238532,
0.688073394,0.689908257,0.691743119,0.693577982,0.695412844,0.697247706,
0.699082569,0.700917431,0.702752294,0.704587156,0.706422018,0.708256881,
0.710091743,0.711926606,0.713761468,0.71559633,0.717431193,0.719266055,
0.721100917,0.72293578,0.724770642,0.726605505,0.728440367,0.730275229,
0.732110092,0.733944954,0.735779817,0.737614679,0.739449541,0.741284404,
0.743119266,0.744954128,0.746788991,0.748623853,0.750458716,0.752293578,
0.75412844,0.755963303,0.757798165,0.759633028,0.76146789,0.763302752,0.765137615,
0.766972477,0.768807339,0.770642202,0.772477064,0.774311927,0.776146789,
0.777981651,0.779816514,0.781651376,0.783486239,0.785321101,0.787155963,
0.788990826,0.790825688,0.79266055,0.794495413,0.796330275,0.798165138,
0.8,0.801834862,0.803669725,0.805504587,0.80733945,0.809174312,0.811009174,
0.812844037,0.814678899,0.816513761,0.818348624,0.820183486,0.822018349,
0.823853211,0.825688073,0.827522936,0.829357798,0.831192661,0.833027523,
0.834862385,0.836697248,0.83853211,0.840366972,0.842201835,0.844036697,
0.84587156,0.847706422,0.849541284,0.851376147,0.853211009,0.855045872,
0.856880734,0.858715596,0.860550459,0.862385321,0.864220183,0.866055046,
0.867889908,0.869724771,0.871559633,0.873394495,0.875229358,0.87706422,
0.878899083,0.880733945,0.882568807,0.88440367,0.886238532,0.888073394,
0.889908257,0.891743119,0.893577982,0.895412844,0.897247706,0.899082569,
0.900917431,0.902752294,0.904587156,0.906422018,0.908256881,0.910091743,
0.911926606,0.913761468,0.91559633,0.917431193,0.919266055,0.921100917,
0.92293578,0.924770642,0.926605505,0.928440367,0.930275229,0.932110092,
0.933944954,0.935779817,0.937614679,0.939449541,0.941284404,0.943119266,
0.944954128,0.946788991,0.948623853,0.950458716,0.952293578,0.95412844,
0.955963303,0.957798165,0.959633028,0.96146789,0.963302752,0.965137615,
0.966972477,0.968807339,0.970642202,0.972477064,0.974311927,0.976146789,
0.977981651,0.979816514,0.981651376,0.983486239,0.985321101,0.987155963,
0.988990826,0.990825688,0.99266055,0.994495413,0.996330275,0.998165138,
1.),.UNSPECIFIED.);
#24449=B_SPLINE_CURVE_WITH_KNOTS('',5,(#261745,#261746,#261747,#261748,
#261749,#261750,#261751,#261752,#261753,#261754,#261755,#261756,#261757,
#261758,#261759,#261760,#261761,#261762,#261763,#261764,#261765,#261766,
#261767,#261768,#261769,#261770,#261771,#261772,#261773,#261774,#261775,
#261776,#261777,#261778,#261779,#261780,#261781,#261782,#261783,#261784,
#261785,#261786,#261787,#261788,#261789,#261790,#261791,#261792,#261793,
#261794,#261795,#261796,#261797,#261798,#261799,#261800,#261801,#261802,
#261803,#261804,#261805,#261806,#261807,#261808,#261809,#261810,#261811,
#261812,#261813,#261814,#261815,#261816,#261817,#261818,#261819,#261820,
#261821,#261822,#261823,#261824,#261825,#261826,#261827,#261828,#261829,
#261830,#261831,#261832,#261833,#261834,#261835,#261836,#261837,#261838,
#261839,#261840,#261841,#261842,#261843,#261844,#261845,#261846,#261847,
#261848,#261849,#261850,#261851,#261852,#261853,#261854,#261855,#261856,
#261857,#261858,#261859,#261860,#261861,#261862,#261863,#261864,#261865,
#261866,#261867,#261868,#261869,#261870,#261871,#261872,#261873,#261874,
#261875,#261876,#261877,#261878,#261879,#261880,#261881,#261882,#261883,
#261884,#261885,#261886,#261887,#261888,#261889,#261890,#261891,#261892,
#261893,#261894,#261895,#261896,#261897,#261898,#261899,#261900,#261901,
#261902,#261903,#261904,#261905,#261906,#261907,#261908,#261909,#261910,
#261911,#261912,#261913,#261914,#261915,#261916,#261917,#261918,#261919,
#261920,#261921,#261922,#261923,#261924,#261925,#261926,#261927,#261928,
#261929,#261930,#261931,#261932,#261933,#261934,#261935,#261936,#261937,
#261938,#261939,#261940,#261941,#261942,#261943,#261944,#261945,#261946,
#261947,#261948,#261949,#261950,#261951,#261952,#261953,#261954,#261955,
#261956,#261957,#261958,#261959,#261960,#261961,#261962,#261963,#261964,
#261965,#261966,#261967,#261968,#261969,#261970,#261971,#261972,#261973,
#261974,#261975,#261976,#261977,#261978,#261979,#261980,#261981,#261982,
#261983,#261984,#261985,#261986,#261987,#261988,#261989,#261990,#261991,
#261992,#261993,#261994,#261995,#261996,#261997,#261998,#261999,#262000,
#262001,#262002,#262003,#262004,#262005,#262006,#262007,#262008,#262009,
#262010,#262011,#262012,#262013,#262014,#262015,#262016,#262017,#262018,
#262019,#262020,#262021,#262022,#262023,#262024,#262025,#262026,#262027,
#262028,#262029,#262030,#262031,#262032,#262033,#262034,#262035,#262036,
#262037,#262038,#262039,#262040,#262041,#262042,#262043,#262044,#262045,
#262046,#262047,#262048,#262049,#262050,#262051,#262052,#262053,#262054,
#262055,#262056,#262057,#262058,#262059,#262060,#262061,#262062,#262063,
#262064,#262065,#262066,#262067,#262068,#262069,#262070,#262071,#262072,
#262073,#262074,#262075,#262076,#262077,#262078,#262079,#262080,#262081,
#262082,#262083,#262084,#262085,#262086,#262087,#262088,#262089,#262090,
#262091,#262092,#262093,#262094,#262095,#262096,#262097,#262098,#262099,
#262100,#262101,#262102,#262103,#262104,#262105,#262106,#262107,#262108,
#262109,#262110,#262111,#262112,#262113,#262114,#262115,#262116,#262117,
#262118,#262119,#262120,#262121,#262122,#262123,#262124,#262125,#262126,
#262127,#262128,#262129,#262130,#262131,#262132,#262133,#262134,#262135,
#262136,#262137,#262138,#262139,#262140,#262141,#262142,#262143,#262144,
#262145,#262146,#262147,#262148,#262149,#262150,#262151,#262152,#262153,
#262154,#262155,#262156,#262157,#262158,#262159,#262160,#262161,#262162,
#262163,#262164,#262165,#262166,#262167,#262168,#262169,#262170,#262171,
#262172,#262173,#262174,#262175,#262176,#262177,#262178,#262179,#262180,
#262181,#262182,#262183,#262184,#262185,#262186,#262187,#262188,#262189,
#262190,#262191,#262192,#262193,#262194,#262195,#262196,#262197,#262198,
#262199,#262200,#262201,#262202,#262203,#262204,#262205,#262206,#262207,
#262208,#262209,#262210,#262211,#262212,#262213,#262214,#262215,#262216),
 .UNSPECIFIED.,.F.,.F.,(6,1,1,1,1,1,1,1,1,1,1,1,1,1,1,1,1,1,1,1,1,1,1,1,
1,1,1,1,1,1,1,1,1,1,1,1,1,1,1,1,1,1,1,1,1,1,1,1,1,1,1,1,1,1,1,1,1,1,1,1,
1,1,1,1,1,1,1,1,1,1,1,1,1,1,1,1,1,1,1,1,1,1,1,1,1,1,1,1,1,1,1,1,1,1,1,1,
1,1,1,1,1,1,1,1,1,1,1,1,1,1,1,1,1,1,1,1,1,1,1,1,1,1,1,1,1,1,1,1,1,1,1,1,
1,1,1,1,1,1,1,1,1,1,1,1,1,1,1,1,1,1,1,1,1,1,1,1,1,1,1,1,1,1,1,1,1,1,1,1,
1,1,1,1,1,1,1,1,1,1,1,1,1,1,1,1,1,1,1,1,1,1,1,1,1,1,1,1,1,1,1,1,1,1,1,1,
1,1,1,1,1,1,1,1,1,1,1,1,1,1,1,1,1,1,1,1,1,1,1,1,1,1,1,1,1,1,1,1,1,1,1,1,
1,1,1,1,1,1,1,1,1,1,1,1,1,1,1,1,1,1,1,1,1,1,1,1,1,1,1,1,1,1,1,1,1,1,1,1,
1,1,1,1,1,1,1,1,1,1,1,1,1,1,1,1,1,1,1,1,1,1,1,1,1,1,1,1,1,1,1,1,1,1,1,1,
1,1,1,1,1,1,1,1,1,1,1,1,1,1,1,1,1,1,1,1,1,1,1,1,1,1,1,1,1,1,1,1,1,1,1,1,
1,1,1,1,1,1,1,1,1,1,1,1,1,1,1,1,1,1,1,1,1,1,1,1,1,1,1,1,1,1,1,1,1,1,1,1,
1,1,1,1,1,1,1,1,1,1,1,1,1,1,1,1,1,1,1,1,1,1,1,1,1,1,1,1,1,1,1,1,1,1,1,1,
1,1,1,1,1,1,1,1,1,1,1,1,1,1,1,1,1,1,1,1,1,1,1,1,1,1,1,1,1,1,1,1,1,1,1,1,
1,1,1,1,1,1,1,1,1,1,1,6),(-1.,-0.998165138,-0.996330275,-0.994495413,-0.99266055,
-0.990825688,-0.988990826,-0.987155963,-0.985321101,-0.983486239,-0.981651376,
-0.979816514,-0.977981651,-0.976146789,-0.974311927,-0.972477064,-0.970642202,
-0.968807339,-0.966972477,-0.965137615,-0.963302752,-0.96146789,-0.959633028,
-0.957798165,-0.955963303,-0.95412844,-0.952293578,-0.950458716,-0.948623853,
-0.946788991,-0.944954128,-0.943119266,-0.941284404,-0.939449541,-0.937614679,
-0.935779817,-0.933944954,-0.932110092,-0.930275229,-0.928440367,-0.926605505,
-0.924770642,-0.92293578,-0.921100917,-0.919266055,-0.917431193,-0.91559633,
-0.913761468,-0.911926606,-0.910091743,-0.908256881,-0.906422018,-0.904587156,
-0.902752294,-0.900917431,-0.899082569,-0.897247706,-0.895412844,-0.893577982,
-0.891743119,-0.889908257,-0.888073394,-0.886238532,-0.88440367,-0.882568807,
-0.880733945,-0.878899083,-0.87706422,-0.875229358,-0.873394495,-0.871559633,
-0.869724771,-0.867889908,-0.866055046,-0.864220183,-0.862385321,-0.860550459,
-0.858715596,-0.856880734,-0.855045872,-0.853211009,-0.851376147,-0.849541284,
-0.847706422,-0.84587156,-0.844036697,-0.842201835,-0.840366972,-0.83853211,
-0.836697248,-0.834862385,-0.833027523,-0.831192661,-0.829357798,-0.827522936,
-0.825688073,-0.823853211,-0.822018349,-0.820183486,-0.818348624,-0.816513761,
-0.814678899,-0.812844037,-0.811009174,-0.809174312,-0.80733945,-0.805504587,
-0.803669725,-0.801834862,-0.8,-0.798165138,-0.796330275,-0.794495413,-0.79266055,
-0.790825688,-0.788990826,-0.787155963,-0.785321101,-0.783486239,-0.781651376,
-0.779816514,-0.777981651,-0.776146789,-0.774311927,-0.772477064,-0.770642202,
-0.768807339,-0.766972477,-0.765137615,-0.763302752,-0.76146789,-0.759633028,
-0.757798165,-0.755963303,-0.75412844,-0.752293578,-0.750458716,-0.748623853,
-0.746788991,-0.744954128,-0.743119266,-0.741284404,-0.739449541,-0.737614679,
-0.735779817,-0.733944954,-0.732110092,-0.730275229,-0.728440367,-0.726605505,
-0.724770642,-0.72293578,-0.721100917,-0.719266055,-0.717431193,-0.71559633,
-0.713761468,-0.711926606,-0.710091743,-0.708256881,-0.706422018,-0.704587156,
-0.702752294,-0.700917431,-0.699082569,-0.697247706,-0.695412844,-0.693577982,
-0.691743119,-0.689908257,-0.688073394,-0.686238532,-0.68440367,-0.682568807,
-0.680733945,-0.678899083,-0.67706422,-0.675229358,-0.673394495,-0.671559633,
-0.669724771,-0.667889908,-0.666055046,-0.664220183,-0.662385321,-0.660550459,
-0.658715596,-0.656880734,-0.655045872,-0.653211009,-0.651376147,-0.649541284,
-0.647706422,-0.64587156,-0.644036697,-0.642201835,-0.640366972,-0.63853211,
-0.636697248,-0.634862385,-0.633027523,-0.631192661,-0.629357798,-0.627522936,
-0.625688073,-0.623853211,-0.622018349,-0.620183486,-0.618348624,-0.616513761,
-0.614678899,-0.612844037,-0.611009174,-0.609174312,-0.60733945,-0.605504587,
-0.603669725,-0.601834862,-0.6,-0.598165138,-0.596330275,-0.594495413,-0.59266055,
-0.590825688,-0.588990826,-0.587155963,-0.585321101,-0.583486239,-0.581651376,
-0.579816514,-0.577981651,-0.576146789,-0.574311927,-0.572477064,-0.570642202,
-0.568807339,-0.566972477,-0.565137615,-0.563302752,-0.56146789,-0.559633028,
-0.557798165,-0.555963303,-0.55412844,-0.552293578,-0.550458716,-0.548623853,
-0.546788991,-0.544954128,-0.543119266,-0.541284404,-0.539449541,-0.537614679,
-0.535779817,-0.533944954,-0.532110092,-0.530275229,-0.528440367,-0.526605505,
-0.524770642,-0.52293578,-0.521100917,-0.519266055,-0.517431193,-0.51559633,
-0.513761468,-0.511926606,-0.510091743,-0.508256881,-0.506422018,-0.504587156,
-0.502752294,-0.500917431,-0.499082569,-0.497247706,-0.495412844,-0.493577982,
-0.491743119,-0.489908257,-0.488073394,-0.486238532,-0.48440367,-0.482568807,
-0.480733945,-0.478899083,-0.47706422,-0.475229358,-0.473394495,-0.471559633,
-0.469724771,-0.467889908,-0.466055046,-0.464220183,-0.462385321,-0.460550459,
-0.458715596,-0.456880734,-0.455045872,-0.453211009,-0.451376147,-0.449541284,
-0.447706422,-0.44587156,-0.444036697,-0.442201835,-0.440366972,-0.43853211,
-0.436697248,-0.434862385,-0.433027523,-0.431192661,-0.429357798,-0.427522936,
-0.425688073,-0.423853211,-0.422018349,-0.420183486,-0.418348624,-0.416513761,
-0.414678899,-0.412844037,-0.411009174,-0.409174312,-0.40733945,-0.405504587,
-0.403669725,-0.401834862,-0.4,-0.398165138,-0.396330275,-0.394495413,-0.39266055,
-0.390825688,-0.388990826,-0.387155963,-0.385321101,-0.383486239,-0.381651376,
-0.379816514,-0.377981651,-0.376146789,-0.374311927,-0.372477064,-0.370642202,
-0.368807339,-0.366972477,-0.365137615,-0.363302752,-0.36146789,-0.359633028,
-0.357798165,-0.355963303,-0.35412844,-0.352293578,-0.350458716,-0.348623853,
-0.346788991,-0.344954128,-0.343119266,-0.341284404,-0.339449541,-0.337614679,
-0.335779817,-0.333944954,-0.332110092,-0.330275229,-0.328440367,-0.326605505,
-0.324770642,-0.32293578,-0.321100917,-0.319266055,-0.317431193,-0.31559633,
-0.313761468,-0.311926606,-0.310091743,-0.308256881,-0.306422018,-0.304587156,
-0.302752294,-0.300917431,-0.299082569,-0.297247706,-0.295412844,-0.293577982,
-0.291743119,-0.289908257,-0.288073394,-0.286238532,-0.28440367,-0.282568807,
-0.280733945,-0.278899083,-0.27706422,-0.275229358,-0.273394495,-0.271559633,
-0.269724771,-0.267889908,-0.266055046,-0.264220183,-0.262385321,-0.260550459,
-0.258715596,-0.256880734,-0.255045872,-0.253211009,-0.251376147,-0.249541284,
-0.247706422,-0.24587156,-0.244036697,-0.242201835,-0.240366972,-0.23853211,
-0.236697248,-0.234862385,-0.233027523,-0.231192661,-0.229357798,-0.227522936,
-0.225688073,-0.223853211,-0.222018349,-0.220183486,-0.218348624,-0.216513761,
-0.214678899,-0.212844037,-0.211009174,-0.209174312,-0.20733945,-0.205504587,
-0.203669725,-0.201834862,-0.2,-0.198165138,-0.196330275,-0.194495413,-0.19266055,
-0.190825688,-0.188990826,-0.187155963,-0.185321101,-0.183486239,-0.181651376,
-0.179816514,-0.177981651,-0.176146789,-0.174311927,-0.172477064,-0.170642202,
-0.168807339,-0.166972477,-0.165137615,-0.163302752,-0.16146789,-0.159633028,
-0.157798165,-0.155963303,-0.15412844,-0.152293578,-0.150458716,-0.148623853,
-0.146788991,-0.144954128,-0.143172102),.UNSPECIFIED.);
#24450=B_SPLINE_CURVE_WITH_KNOTS('',5,(#262217,#262218,#262219,#262220,
#262221,#262222,#262223,#262224,#262225,#262226,#262227,#262228,#262229,
#262230,#262231,#262232,#262233,#262234,#262235,#262236,#262237,#262238,
#262239,#262240,#262241,#262242,#262243,#262244,#262245,#262246,#262247,
#262248,#262249,#262250,#262251,#262252,#262253,#262254,#262255,#262256,
#262257,#262258,#262259,#262260,#262261,#262262,#262263,#262264,#262265,
#262266,#262267,#262268,#262269,#262270,#262271,#262272,#262273,#262274,
#262275,#262276,#262277,#262278,#262279,#262280,#262281,#262282,#262283,
#262284,#262285,#262286,#262287,#262288,#262289,#262290,#262291,#262292,
#262293,#262294,#262295,#262296,#262297,#262298,#262299,#262300,#262301,
#262302,#262303,#262304,#262305,#262306,#262307,#262308,#262309,#262310,
#262311,#262312,#262313,#262314,#262315,#262316,#262317,#262318,#262319,
#262320,#262321,#262322,#262323,#262324,#262325,#262326,#262327,#262328,
#262329,#262330,#262331,#262332,#262333,#262334,#262335,#262336,#262337,
#262338,#262339,#262340,#262341,#262342,#262343,#262344,#262345,#262346,
#262347,#262348,#262349,#262350,#262351,#262352,#262353,#262354,#262355,
#262356,#262357,#262358,#262359,#262360,#262361,#262362,#262363,#262364,
#262365,#262366,#262367,#262368,#262369,#262370,#262371,#262372,#262373,
#262374,#262375,#262376,#262377,#262378,#262379,#262380,#262381,#262382,
#262383,#262384,#262385,#262386,#262387,#262388,#262389,#262390,#262391,
#262392,#262393,#262394,#262395,#262396,#262397,#262398,#262399,#262400,
#262401,#262402,#262403,#262404,#262405,#262406,#262407,#262408,#262409,
#262410,#262411,#262412,#262413,#262414,#262415,#262416,#262417,#262418,
#262419,#262420,#262421,#262422,#262423,#262424,#262425,#262426,#262427,
#262428,#262429,#262430,#262431,#262432,#262433,#262434,#262435,#262436,
#262437,#262438,#262439,#262440,#262441,#262442,#262443,#262444,#262445,
#262446,#262447,#262448,#262449,#262450,#262451,#262452,#262453,#262454,
#262455,#262456,#262457,#262458,#262459,#262460,#262461,#262462,#262463,
#262464,#262465,#262466,#262467,#262468,#262469,#262470,#262471,#262472,
#262473,#262474,#262475,#262476,#262477,#262478,#262479,#262480,#262481,
#262482,#262483,#262484,#262485,#262486,#262487,#262488,#262489,#262490,
#262491,#262492,#262493,#262494,#262495,#262496,#262497,#262498,#262499,
#262500,#262501,#262502,#262503,#262504,#262505,#262506,#262507,#262508,
#262509,#262510,#262511,#262512,#262513,#262514,#262515,#262516,#262517,
#262518,#262519,#262520,#262521,#262522,#262523,#262524,#262525,#262526,
#262527,#262528,#262529,#262530,#262531,#262532,#262533,#262534,#262535,
#262536,#262537,#262538,#262539,#262540,#262541,#262542,#262543,#262544,
#262545,#262546,#262547,#262548,#262549,#262550,#262551,#262552,#262553,
#262554,#262555,#262556,#262557,#262558,#262559,#262560,#262561,#262562,
#262563,#262564,#262565,#262566,#262567,#262568,#262569,#262570,#262571,
#262572,#262573,#262574,#262575,#262576,#262577,#262578,#262579,#262580,
#262581,#262582,#262583,#262584,#262585,#262586,#262587,#262588,#262589,
#262590,#262591,#262592,#262593,#262594,#262595,#262596,#262597,#262598,
#262599,#262600,#262601,#262602,#262603,#262604,#262605,#262606,#262607,
#262608,#262609,#262610,#262611,#262612,#262613,#262614,#262615,#262616,
#262617,#262618,#262619,#262620,#262621,#262622,#262623,#262624,#262625,
#262626,#262627,#262628,#262629,#262630,#262631,#262632,#262633,#262634,
#262635,#262636,#262637,#262638,#262639,#262640,#262641,#262642,#262643,
#262644,#262645,#262646,#262647,#262648,#262649,#262650,#262651,#262652,
#262653,#262654,#262655,#262656,#262657,#262658,#262659,#262660,#262661,
#262662,#262663,#262664,#262665,#262666,#262667,#262668,#262669,#262670,
#262671,#262672,#262673,#262674,#262675,#262676,#262677,#262678,#262679,
#262680,#262681,#262682,#262683,#262684,#262685,#262686,#262687,#262688),
 .UNSPECIFIED.,.F.,.F.,(6,1,1,1,1,1,1,1,1,1,1,1,1,1,1,1,1,1,1,1,1,1,1,1,
1,1,1,1,1,1,1,1,1,1,1,1,1,1,1,1,1,1,1,1,1,1,1,1,1,1,1,1,1,1,1,1,1,1,1,1,
1,1,1,1,1,1,1,1,1,1,1,1,1,1,1,1,1,1,1,1,1,1,1,1,1,1,1,1,1,1,1,1,1,1,1,1,
1,1,1,1,1,1,1,1,1,1,1,1,1,1,1,1,1,1,1,1,1,1,1,1,1,1,1,1,1,1,1,1,1,1,1,1,
1,1,1,1,1,1,1,1,1,1,1,1,1,1,1,1,1,1,1,1,1,1,1,1,1,1,1,1,1,1,1,1,1,1,1,1,
1,1,1,1,1,1,1,1,1,1,1,1,1,1,1,1,1,1,1,1,1,1,1,1,1,1,1,1,1,1,1,1,1,1,1,1,
1,1,1,1,1,1,1,1,1,1,1,1,1,1,1,1,1,1,1,1,1,1,1,1,1,1,1,1,1,1,1,1,1,1,1,1,
1,1,1,1,1,1,1,1,1,1,1,1,1,1,1,1,1,1,1,1,1,1,1,1,1,1,1,1,1,1,1,1,1,1,1,1,
1,1,1,1,1,1,1,1,1,1,1,1,1,1,1,1,1,1,1,1,1,1,1,1,1,1,1,1,1,1,1,1,1,1,1,1,
1,1,1,1,1,1,1,1,1,1,1,1,1,1,1,1,1,1,1,1,1,1,1,1,1,1,1,1,1,1,1,1,1,1,1,1,
1,1,1,1,1,1,1,1,1,1,1,1,1,1,1,1,1,1,1,1,1,1,1,1,1,1,1,1,1,1,1,1,1,1,1,1,
1,1,1,1,1,1,1,1,1,1,1,1,1,1,1,1,1,1,1,1,1,1,1,1,1,1,1,1,1,1,1,1,1,1,1,1,
1,1,1,1,1,1,1,1,1,1,1,1,1,1,1,1,1,1,1,1,1,1,1,1,1,1,1,1,1,1,1,1,1,1,1,1,
1,1,1,1,1,1,1,1,1,1,1,6),(0.143172102,0.144954128,0.146788991,0.148623853,
0.150458716,0.152293578,0.15412844,0.155963303,0.157798165,0.159633028,
0.16146789,0.163302752,0.165137615,0.166972477,0.168807339,0.170642202,
0.172477064,0.174311927,0.176146789,0.177981651,0.179816514,0.181651376,
0.183486239,0.185321101,0.187155963,0.188990826,0.190825688,0.19266055,
0.194495413,0.196330275,0.198165138,0.2,0.201834862,0.203669725,0.205504587,
0.20733945,0.209174312,0.211009174,0.212844037,0.214678899,0.216513761,
0.218348624,0.220183486,0.222018349,0.223853211,0.225688073,0.227522936,
0.229357798,0.231192661,0.233027523,0.234862385,0.236697248,0.23853211,
0.240366972,0.242201835,0.244036697,0.24587156,0.247706422,0.249541284,
0.251376147,0.253211009,0.255045872,0.256880734,0.258715596,0.260550459,
0.262385321,0.264220183,0.266055046,0.267889908,0.269724771,0.271559633,
0.273394495,0.275229358,0.27706422,0.278899083,0.280733945,0.282568807,
0.28440367,0.286238532,0.288073394,0.289908257,0.291743119,0.293577982,
0.295412844,0.297247706,0.299082569,0.300917431,0.302752294,0.304587156,
0.306422018,0.308256881,0.310091743,0.311926606,0.313761468,0.31559633,
0.317431193,0.319266055,0.321100917,0.32293578,0.324770642,0.326605505,
0.328440367,0.330275229,0.332110092,0.333944954,0.335779817,0.337614679,
0.339449541,0.341284404,0.343119266,0.344954128,0.346788991,0.348623853,
0.350458716,0.352293578,0.35412844,0.355963303,0.357798165,0.359633028,
0.36146789,0.363302752,0.365137615,0.366972477,0.368807339,0.370642202,
0.372477064,0.374311927,0.376146789,0.377981651,0.379816514,0.381651376,
0.383486239,0.385321101,0.387155963,0.388990826,0.390825688,0.39266055,
0.394495413,0.396330275,0.398165138,0.4,0.401834862,0.403669725,0.405504587,
0.40733945,0.409174312,0.411009174,0.412844037,0.414678899,0.416513761,
0.418348624,0.420183486,0.422018349,0.423853211,0.425688073,0.427522936,
0.429357798,0.431192661,0.433027523,0.434862385,0.436697248,0.43853211,
0.440366972,0.442201835,0.444036697,0.44587156,0.447706422,0.449541284,
0.451376147,0.453211009,0.455045872,0.456880734,0.458715596,0.460550459,
0.462385321,0.464220183,0.466055046,0.467889908,0.469724771,0.471559633,
0.473394495,0.475229358,0.47706422,0.478899083,0.480733945,0.482568807,
0.48440367,0.486238532,0.488073394,0.489908257,0.491743119,0.493577982,
0.495412844,0.497247706,0.499082569,0.500917431,0.502752294,0.504587156,
0.506422018,0.508256881,0.510091743,0.511926606,0.513761468,0.51559633,
0.517431193,0.519266055,0.521100917,0.52293578,0.524770642,0.526605505,
0.528440367,0.530275229,0.532110092,0.533944954,0.535779817,0.537614679,
0.539449541,0.541284404,0.543119266,0.544954128,0.546788991,0.548623853,
0.550458716,0.552293578,0.55412844,0.555963303,0.557798165,0.559633028,
0.56146789,0.563302752,0.565137615,0.566972477,0.568807339,0.570642202,
0.572477064,0.574311927,0.576146789,0.577981651,0.579816514,0.581651376,
0.583486239,0.585321101,0.587155963,0.588990826,0.590825688,0.59266055,
0.594495413,0.596330275,0.598165138,0.6,0.601834862,0.603669725,0.605504587,
0.60733945,0.609174312,0.611009174,0.612844037,0.614678899,0.616513761,
0.618348624,0.620183486,0.622018349,0.623853211,0.625688073,0.627522936,
0.629357798,0.631192661,0.633027523,0.634862385,0.636697248,0.63853211,
0.640366972,0.642201835,0.644036697,0.64587156,0.647706422,0.649541284,
0.651376147,0.653211009,0.655045872,0.656880734,0.658715596,0.660550459,
0.662385321,0.664220183,0.666055046,0.667889908,0.669724771,0.671559633,
0.673394495,0.675229358,0.67706422,0.678899083,0.680733945,0.682568807,
0.68440367,0.686238532,0.688073394,0.689908257,0.691743119,0.693577982,
0.695412844,0.697247706,0.699082569,0.700917431,0.702752294,0.704587156,
0.706422018,0.708256881,0.710091743,0.711926606,0.713761468,0.71559633,
0.717431193,0.719266055,0.721100917,0.72293578,0.724770642,0.726605505,
0.728440367,0.730275229,0.732110092,0.733944954,0.735779817,0.737614679,
0.739449541,0.741284404,0.743119266,0.744954128,0.746788991,0.748623853,
0.750458716,0.752293578,0.75412844,0.755963303,0.757798165,0.759633028,
0.76146789,0.763302752,0.765137615,0.766972477,0.768807339,0.770642202,
0.772477064,0.774311927,0.776146789,0.777981651,0.779816514,0.781651376,
0.783486239,0.785321101,0.787155963,0.788990826,0.790825688,0.79266055,
0.794495413,0.796330275,0.798165138,0.8,0.801834862,0.803669725,0.805504587,
0.80733945,0.809174312,0.811009174,0.812844037,0.814678899,0.816513761,
0.818348624,0.820183486,0.822018349,0.823853211,0.825688073,0.827522936,
0.829357798,0.831192661,0.833027523,0.834862385,0.836697248,0.83853211,
0.840366972,0.842201835,0.844036697,0.84587156,0.847706422,0.849541284,
0.851376147,0.853211009,0.855045872,0.856880734,0.858715596,0.860550459,
0.862385321,0.864220183,0.866055046,0.867889908,0.869724771,0.871559633,
0.873394495,0.875229358,0.87706422,0.878899083,0.880733945,0.882568807,
0.88440367,0.886238532,0.888073394,0.889908257,0.891743119,0.893577982,
0.895412844,0.897247706,0.899082569,0.900917431,0.902752294,0.904587156,
0.906422018,0.908256881,0.910091743,0.911926606,0.913761468,0.91559633,
0.917431193,0.919266055,0.921100917,0.92293578,0.924770642,0.926605505,
0.928440367,0.930275229,0.932110092,0.933944954,0.935779817,0.937614679,
0.939449541,0.941284404,0.943119266,0.944954128,0.946788991,0.948623853,
0.950458716,0.952293578,0.95412844,0.955963303,0.957798165,0.959633028,
0.96146789,0.963302752,0.965137615,0.966972477,0.968807339,0.970642202,
0.972477064,0.974311927,0.976146789,0.977981651,0.979816514,0.981651376,
0.983486239,0.985321101,0.987155963,0.988990826,0.990825688,0.99266055,
0.994495413,0.996330275,0.998165138,1.),.UNSPECIFIED.);
#24451=B_SPLINE_CURVE_WITH_KNOTS('',3,(#263651,#263652,#263653,#263654,
#263655,#263656,#263657,#263658,#263659,#263660,#263661,#263662,#263663,
#263664,#263665,#263666,#263667,#263668,#263669,#263670,#263671,#263672,
#263673,#263674,#263675,#263676,#263677,#263678,#263679,#263680,#263681,
#263682,#263683,#263684,#263685,#263686,#263687,#263688,#263689,#263690,
#263691,#263692,#263693,#263694,#263695,#263696,#263697,#263698,#263699,
#263700,#263701,#263702,#263703,#263704,#263705,#263706,#263707,#263708,
#263709,#263710,#263711,#263712,#263713,#263714,#263715,#263716,#263717,
#263718,#263719,#263720,#263721,#263722,#263723,#263724,#263725,#263726,
#263727,#263728,#263729,#263730,#263731,#263732,#263733,#263734,#263735,
#263736,#263737,#263738,#263739,#263740,#263741,#263742,#263743,#263744,
#263745,#263746,#263747,#263748,#263749,#263750,#263751,#263752,#263753,
#263754,#263755,#263756,#263757,#263758,#263759,#263760,#263761,#263762,
#263763,#263764,#263765,#263766,#263767,#263768,#263769,#263770,#263771,
#263772,#263773,#263774,#263775,#263776,#263777,#263778,#263779,#263780,
#263781,#263782,#263783,#263784,#263785,#263786,#263787,#263788,#263789,
#263790,#263791,#263792,#263793,#263794,#263795,#263796,#263797,#263798,
#263799,#263800,#263801,#263802,#263803,#263804,#263805,#263806,#263807,
#263808,#263809,#263810,#263811,#263812,#263813,#263814,#263815,#263816,
#263817,#263818,#263819,#263820,#263821,#263822,#263823,#263824,#263825,
#263826,#263827,#263828,#263829,#263830,#263831,#263832,#263833,#263834,
#263835,#263836,#263837,#263838,#263839,#263840,#263841,#263842,#263843,
#263844,#263845,#263846,#263847,#263848,#263849,#263850,#263851,#263852,
#263853,#263854,#263855,#263856,#263857,#263858,#263859,#263860,#263861,
#263862,#263863,#263864,#263865,#263866,#263867,#263868,#263869,#263870,
#263871,#263872,#263873,#263874,#263875,#263876,#263877,#263878,#263879,
#263880,#263881,#263882,#263883,#263884,#263885,#263886,#263887,#263888,
#263889,#263890,#263891,#263892,#263893,#263894,#263895,#263896,#263897,
#263898,#263899,#263900,#263901,#263902,#263903,#263904,#263905,#263906,
#263907,#263908,#263909,#263910,#263911,#263912,#263913,#263914,#263915,
#263916,#263917,#263918,#263919,#263920,#263921,#263922,#263923,#263924,
#263925,#263926,#263927,#263928,#263929,#263930,#263931,#263932,#263933,
#263934,#263935,#263936,#263937,#263938,#263939,#263940,#263941,#263942,
#263943,#263944,#263945,#263946,#263947,#263948,#263949,#263950,#263951,
#263952,#263953,#263954,#263955,#263956,#263957,#263958,#263959,#263960,
#263961,#263962,#263963),.UNSPECIFIED.,.F.,.F.,(4,3,3,3,3,3,3,3,3,3,3,3,
3,3,3,3,3,3,3,3,3,3,3,3,3,3,3,3,3,3,3,3,3,3,3,3,3,3,3,3,3,3,3,3,3,3,3,3,
3,3,3,3,3,3,3,3,3,3,3,3,3,3,3,3,3,3,3,3,3,3,3,3,3,3,3,3,3,3,3,3,3,3,3,3,
3,3,3,3,3,3,3,3,3,3,3,3,3,3,3,3,3,3,3,3,4),(-1.,-0.994495413,-0.988990826,
-0.981651376,-0.976146789,-0.970642202,-0.965137615,-0.959633028,-0.95412844,
-0.948623853,-0.943119266,-0.937614679,-0.932110092,-0.926605505,-0.921100917,
-0.913761468,-0.908256881,-0.900917431,-0.895412844,-0.889908257,-0.88440367,
-0.878899083,-0.873394495,-0.867889908,-0.860550459,-0.855045872,-0.849541284,
-0.844036697,-0.83853211,-0.833027523,-0.827522936,-0.822018349,-0.816513761,
-0.809174312,-0.8,-0.79266055,-0.783486239,-0.774311927,-0.766972477,-0.759633028,
-0.752293578,-0.744954128,-0.737614679,-0.728440367,-0.721100917,-0.711926606,
-0.704587156,-0.697247706,-0.689908257,-0.682568807,-0.675229358,-0.667889908,
-0.660550459,-0.653211009,-0.644036697,-0.636697248,-0.627522936,-0.620183486,
-0.612844037,-0.605504587,-0.598165138,-0.590825688,-0.583486239,-0.576146789,
-0.568807339,-0.56146789,-0.55412844,-0.546788991,-0.539449541,-0.532110092,
-0.52293578,-0.513761468,-0.504587156,-0.495412844,-0.486238532,-0.47706422,
-0.466055046,-0.455045872,-0.442201835,-0.433027523,-0.420183486,-0.411009174,
-0.401834862,-0.39266055,-0.381651376,-0.370642202,-0.359633028,-0.348623853,
-0.337614679,-0.324770642,-0.313761468,-0.302752294,-0.291743119,-0.280733945,
-0.269724771,-0.256880734,-0.242201835,-0.231192661,-0.220183486,-0.209174312,
-0.196330275,-0.183486239,-0.172477064,-0.16146789,-0.143172102),
 .UNSPECIFIED.);
#24452=B_SPLINE_CURVE_WITH_KNOTS('',3,(#263964,#263965,#263966,#263967,
#263968,#263969,#263970,#263971,#263972,#263973,#263974,#263975,#263976,
#263977,#263978,#263979,#263980,#263981,#263982,#263983,#263984,#263985,
#263986,#263987,#263988,#263989,#263990,#263991,#263992,#263993,#263994,
#263995,#263996,#263997,#263998,#263999,#264000,#264001,#264002,#264003,
#264004,#264005,#264006,#264007,#264008,#264009,#264010,#264011,#264012,
#264013,#264014,#264015,#264016,#264017,#264018,#264019,#264020,#264021,
#264022,#264023,#264024,#264025,#264026,#264027,#264028,#264029,#264030,
#264031,#264032,#264033,#264034,#264035,#264036,#264037,#264038,#264039,
#264040,#264041,#264042,#264043,#264044,#264045,#264046,#264047,#264048,
#264049,#264050,#264051,#264052,#264053,#264054,#264055,#264056,#264057,
#264058,#264059,#264060,#264061,#264062,#264063,#264064,#264065,#264066,
#264067,#264068,#264069,#264070,#264071,#264072,#264073,#264074,#264075,
#264076,#264077,#264078,#264079,#264080,#264081,#264082,#264083,#264084,
#264085,#264086,#264087,#264088,#264089,#264090,#264091,#264092,#264093,
#264094,#264095,#264096,#264097,#264098,#264099,#264100,#264101,#264102,
#264103,#264104,#264105,#264106,#264107,#264108,#264109,#264110,#264111,
#264112,#264113,#264114,#264115,#264116,#264117,#264118,#264119,#264120,
#264121,#264122,#264123,#264124,#264125,#264126,#264127,#264128,#264129,
#264130,#264131,#264132,#264133,#264134,#264135,#264136,#264137,#264138,
#264139,#264140,#264141,#264142,#264143,#264144,#264145,#264146,#264147,
#264148,#264149,#264150,#264151,#264152,#264153,#264154,#264155,#264156,
#264157,#264158,#264159,#264160,#264161,#264162,#264163,#264164,#264165,
#264166,#264167,#264168,#264169,#264170,#264171,#264172,#264173,#264174,
#264175,#264176,#264177,#264178,#264179,#264180,#264181,#264182,#264183,
#264184,#264185,#264186,#264187,#264188,#264189,#264190,#264191,#264192,
#264193,#264194,#264195,#264196,#264197,#264198,#264199,#264200,#264201,
#264202,#264203,#264204,#264205,#264206,#264207,#264208,#264209,#264210,
#264211,#264212,#264213,#264214,#264215,#264216,#264217,#264218,#264219,
#264220,#264221,#264222,#264223,#264224,#264225,#264226,#264227,#264228,
#264229,#264230,#264231,#264232,#264233,#264234,#264235,#264236,#264237,
#264238,#264239,#264240,#264241,#264242,#264243,#264244,#264245,#264246,
#264247,#264248,#264249,#264250,#264251,#264252,#264253,#264254,#264255,
#264256,#264257,#264258),.UNSPECIFIED.,.F.,.F.,(4,3,3,3,3,3,3,3,3,3,3,3,
3,3,3,3,3,3,3,3,3,3,3,3,3,3,3,3,3,3,3,3,3,3,3,3,3,3,3,3,3,3,3,3,3,3,3,3,
3,3,3,3,3,3,3,3,3,3,3,3,3,3,3,3,3,3,3,3,3,3,3,3,3,3,3,3,3,3,3,3,3,3,3,3,
3,3,3,3,3,3,3,3,3,3,3,3,3,3,4),(0.143172102,0.15412844,0.165137615,0.177981651,
0.188990826,0.201834862,0.212844037,0.223853211,0.234862385,0.24587156,
0.256880734,0.267889908,0.278899083,0.289908257,0.300917431,0.311926606,
0.32293578,0.335779817,0.346788991,0.363302752,0.374311927,0.388990826,
0.4,0.409174312,0.418348624,0.427522936,0.436697248,0.44587156,0.455045872,
0.464220183,0.473394495,0.48440367,0.493577982,0.506422018,0.51559633,0.524770642,
0.533944954,0.543119266,0.552293578,0.559633028,0.566972477,0.577981651,
0.587155963,0.594495413,0.601834862,0.609174312,0.616513761,0.625688073,
0.633027523,0.640366972,0.649541284,0.656880734,0.669724771,0.67706422,
0.686238532,0.693577982,0.700917431,0.708256881,0.717431193,0.724770642,
0.733944954,0.743119266,0.750458716,0.759633028,0.766972477,0.777981651,
0.785321101,0.79266055,0.8,0.80733945,0.812844037,0.822018349,0.827522936,
0.834862385,0.840366972,0.84587156,0.851376147,0.858715596,0.864220183,
0.869724771,0.875229358,0.88440367,0.889908257,0.895412844,0.904587156,
0.913761468,0.921100917,0.930275229,0.935779817,0.943119266,0.948623853,
0.95412844,0.959633028,0.965137615,0.970642202,0.977981651,0.987155963,
0.99266055,1.),.UNSPECIFIED.);
#24453=B_SPLINE_CURVE_WITH_KNOTS('',5,(#265203,#265204,#265205,#265206,
#265207,#265208,#265209,#265210,#265211,#265212,#265213,#265214,#265215,
#265216,#265217,#265218,#265219,#265220,#265221,#265222,#265223,#265224,
#265225,#265226,#265227,#265228,#265229,#265230,#265231,#265232,#265233,
#265234,#265235,#265236,#265237,#265238,#265239,#265240,#265241,#265242,
#265243,#265244,#265245,#265246,#265247,#265248,#265249,#265250,#265251,
#265252,#265253,#265254,#265255,#265256,#265257,#265258,#265259,#265260,
#265261,#265262,#265263,#265264,#265265,#265266,#265267,#265268,#265269,
#265270,#265271,#265272,#265273,#265274,#265275,#265276,#265277,#265278,
#265279,#265280,#265281,#265282,#265283,#265284,#265285,#265286,#265287,
#265288,#265289,#265290,#265291,#265292,#265293,#265294,#265295,#265296,
#265297,#265298,#265299,#265300,#265301,#265302,#265303,#265304,#265305,
#265306,#265307,#265308,#265309,#265310,#265311,#265312,#265313,#265314,
#265315,#265316,#265317,#265318,#265319,#265320,#265321,#265322,#265323,
#265324,#265325,#265326,#265327,#265328,#265329,#265330,#265331,#265332,
#265333,#265334,#265335,#265336,#265337,#265338,#265339,#265340,#265341,
#265342,#265343,#265344,#265345,#265346,#265347,#265348,#265349,#265350,
#265351,#265352,#265353,#265354,#265355,#265356,#265357,#265358,#265359,
#265360,#265361,#265362,#265363,#265364,#265365,#265366,#265367,#265368,
#265369,#265370,#265371,#265372,#265373,#265374,#265375,#265376,#265377,
#265378,#265379,#265380,#265381,#265382,#265383,#265384,#265385,#265386,
#265387,#265388,#265389,#265390,#265391,#265392,#265393,#265394,#265395,
#265396,#265397,#265398,#265399,#265400,#265401,#265402,#265403,#265404,
#265405,#265406,#265407,#265408,#265409,#265410,#265411,#265412,#265413,
#265414,#265415,#265416,#265417,#265418,#265419,#265420,#265421,#265422,
#265423,#265424,#265425,#265426,#265427,#265428,#265429,#265430,#265431,
#265432,#265433,#265434,#265435,#265436,#265437,#265438,#265439,#265440,
#265441,#265442,#265443,#265444,#265445,#265446,#265447,#265448,#265449,
#265450,#265451,#265452,#265453,#265454,#265455,#265456,#265457,#265458,
#265459,#265460,#265461,#265462,#265463,#265464,#265465,#265466,#265467,
#265468,#265469,#265470,#265471,#265472,#265473,#265474,#265475,#265476,
#265477,#265478,#265479,#265480,#265481,#265482,#265483,#265484,#265485,
#265486,#265487,#265488,#265489,#265490,#265491,#265492,#265493,#265494,
#265495,#265496,#265497,#265498,#265499,#265500,#265501,#265502,#265503,
#265504,#265505,#265506,#265507,#265508,#265509,#265510,#265511,#265512,
#265513,#265514,#265515,#265516,#265517,#265518,#265519,#265520,#265521,
#265522,#265523,#265524,#265525,#265526,#265527,#265528,#265529,#265530,
#265531,#265532,#265533,#265534,#265535,#265536,#265537,#265538,#265539,
#265540,#265541,#265542,#265543,#265544,#265545,#265546,#265547,#265548,
#265549,#265550,#265551,#265552,#265553,#265554,#265555,#265556,#265557,
#265558,#265559,#265560,#265561,#265562,#265563,#265564,#265565,#265566,
#265567,#265568,#265569,#265570,#265571,#265572,#265573,#265574,#265575,
#265576,#265577,#265578,#265579,#265580,#265581,#265582,#265583,#265584,
#265585,#265586,#265587,#265588,#265589,#265590,#265591,#265592,#265593,
#265594,#265595,#265596,#265597,#265598,#265599,#265600,#265601,#265602,
#265603,#265604,#265605,#265606,#265607,#265608,#265609,#265610,#265611,
#265612,#265613,#265614,#265615,#265616,#265617,#265618,#265619,#265620,
#265621,#265622,#265623,#265624,#265625,#265626,#265627,#265628,#265629,
#265630,#265631,#265632,#265633,#265634,#265635,#265636,#265637,#265638,
#265639,#265640,#265641,#265642,#265643,#265644,#265645,#265646,#265647,
#265648,#265649,#265650,#265651,#265652,#265653,#265654,#265655,#265656,
#265657,#265658,#265659,#265660,#265661,#265662,#265663,#265664,#265665,
#265666,#265667,#265668,#265669,#265670,#265671,#265672),.UNSPECIFIED.,
 .F.,.F.,(6,1,1,1,1,1,1,1,1,1,1,1,1,1,1,1,1,1,1,1,1,1,1,1,1,1,1,1,1,1,1,
1,1,1,1,1,1,1,1,1,1,1,1,1,1,1,1,1,1,1,1,1,1,1,1,1,1,1,1,1,1,1,1,1,1,1,1,
1,1,1,1,1,1,1,1,1,1,1,1,1,1,1,1,1,1,1,1,1,1,1,1,1,1,1,1,1,1,1,1,1,1,1,1,
1,1,1,1,1,1,1,1,1,1,1,1,1,1,1,1,1,1,1,1,1,1,1,1,1,1,1,1,1,1,1,1,1,1,1,1,
1,1,1,1,1,1,1,1,1,1,1,1,1,1,1,1,1,1,1,1,1,1,1,1,1,1,1,1,1,1,1,1,1,1,1,1,
1,1,1,1,1,1,1,1,1,1,1,1,1,1,1,1,1,1,1,1,1,1,1,1,1,1,1,1,1,1,1,1,1,1,1,1,
1,1,1,1,1,1,1,1,1,1,1,1,1,1,1,1,1,1,1,1,1,1,1,1,1,1,1,1,1,1,1,1,1,1,1,1,
1,1,1,1,1,1,1,1,1,1,1,1,1,1,1,1,1,1,1,1,1,1,1,1,1,1,1,1,1,1,1,1,1,1,1,1,
1,1,1,1,1,1,1,1,1,1,1,1,1,1,1,1,1,1,1,1,1,1,1,1,1,1,1,1,1,1,1,1,1,1,1,1,
1,1,1,1,1,1,1,1,1,1,1,1,1,1,1,1,1,1,1,1,1,1,1,1,1,1,1,1,1,1,1,1,1,1,1,1,
1,1,1,1,1,1,1,1,1,1,1,1,1,1,1,1,1,1,1,1,1,1,1,1,1,1,1,1,1,1,1,1,1,1,1,1,
1,1,1,1,1,1,1,1,1,1,1,1,1,1,1,1,1,1,1,1,1,1,1,1,1,1,1,1,1,1,1,1,1,1,1,1,
1,1,1,1,1,1,1,1,1,1,1,1,1,1,1,1,1,1,1,1,1,1,1,1,1,1,1,1,1,1,1,1,1,1,1,1,
1,1,6),(0.143172102,0.144954128,0.146788991,0.148623853,0.150458716,0.152293578,
0.15412844,0.155963303,0.157798165,0.159633028,0.16146789,0.163302752,0.165137615,
0.166972477,0.168807339,0.170642202,0.172477064,0.174311927,0.176146789,
0.177981651,0.179816514,0.181651376,0.183486239,0.185321101,0.187155963,
0.188990826,0.190825688,0.19266055,0.194495413,0.196330275,0.198165138,
0.2,0.201834862,0.203669725,0.205504587,0.20733945,0.209174312,0.211009174,
0.212844037,0.214678899,0.216513761,0.218348624,0.220183486,0.222018349,
0.223853211,0.225688073,0.227522936,0.229357798,0.231192661,0.233027523,
0.234862385,0.236697248,0.23853211,0.240366972,0.242201835,0.244036697,
0.24587156,0.247706422,0.249541284,0.251376147,0.253211009,0.255045872,
0.256880734,0.258715596,0.260550459,0.262385321,0.264220183,0.266055046,
0.267889908,0.269724771,0.271559633,0.273394495,0.275229358,0.27706422,
0.278899083,0.280733945,0.282568807,0.28440367,0.286238532,0.288073394,
0.289908257,0.291743119,0.293577982,0.295412844,0.297247706,0.299082569,
0.300917431,0.302752294,0.304587156,0.306422018,0.308256881,0.310091743,
0.311926606,0.313761468,0.31559633,0.317431193,0.319266055,0.321100917,
0.32293578,0.324770642,0.326605505,0.328440367,0.330275229,0.333944954,
0.335779817,0.337614679,0.339449541,0.341284404,0.343119266,0.344954128,
0.346788991,0.348623853,0.350458716,0.352293578,0.35412844,0.355963303,
0.357798165,0.359633028,0.36146789,0.363302752,0.365137615,0.366972477,
0.368807339,0.370642202,0.372477064,0.374311927,0.376146789,0.377981651,
0.379816514,0.381651376,0.383486239,0.385321101,0.387155963,0.388990826,
0.390825688,0.39266055,0.394495413,0.396330275,0.398165138,0.4,0.401834862,
0.403669725,0.405504587,0.40733945,0.409174312,0.411009174,0.412844037,
0.414678899,0.416513761,0.418348624,0.420183486,0.422018349,0.423853211,
0.425688073,0.427522936,0.429357798,0.431192661,0.433027523,0.434862385,
0.436697248,0.43853211,0.440366972,0.442201835,0.444036697,0.44587156,0.447706422,
0.449541284,0.451376147,0.453211009,0.455045872,0.456880734,0.458715596,
0.460550459,0.462385321,0.464220183,0.466055046,0.467889908,0.469724771,
0.471559633,0.473394495,0.475229358,0.47706422,0.478899083,0.480733945,
0.482568807,0.48440367,0.486238532,0.488073394,0.489908257,0.491743119,
0.493577982,0.495412844,0.497247706,0.499082569,0.500917431,0.502752294,
0.504587156,0.506422018,0.508256881,0.511926606,0.513761468,0.51559633,
0.517431193,0.519266055,0.521100917,0.52293578,0.524770642,0.526605505,
0.528440367,0.530275229,0.532110092,0.533944954,0.535779817,0.537614679,
0.539449541,0.541284404,0.543119266,0.544954128,0.546788991,0.548623853,
0.550458716,0.552293578,0.55412844,0.555963303,0.557798165,0.559633028,
0.56146789,0.563302752,0.565137615,0.566972477,0.568807339,0.570642202,
0.572477064,0.574311927,0.576146789,0.577981651,0.579816514,0.581651376,
0.583486239,0.585321101,0.587155963,0.588990826,0.590825688,0.59266055,
0.594495413,0.596330275,0.598165138,0.6,0.601834862,0.603669725,0.605504587,
0.60733945,0.609174312,0.611009174,0.612844037,0.614678899,0.616513761,
0.618348624,0.620183486,0.622018349,0.623853211,0.625688073,0.627522936,
0.629357798,0.631192661,0.633027523,0.634862385,0.636697248,0.63853211,
0.640366972,0.642201835,0.644036697,0.64587156,0.647706422,0.649541284,
0.651376147,0.653211009,0.655045872,0.656880734,0.658715596,0.660550459,
0.662385321,0.664220183,0.666055046,0.667889908,0.669724771,0.671559633,
0.673394495,0.675229358,0.67706422,0.678899083,0.680733945,0.682568807,
0.68440367,0.686238532,0.688073394,0.689908257,0.691743119,0.693577982,
0.695412844,0.697247706,0.699082569,0.700917431,0.702752294,0.704587156,
0.706422018,0.708256881,0.710091743,0.711926606,0.713761468,0.71559633,
0.717431193,0.719266055,0.721100917,0.72293578,0.724770642,0.726605505,
0.728440367,0.730275229,0.732110092,0.733944954,0.735779817,0.737614679,
0.739449541,0.741284404,0.743119266,0.744954128,0.746788991,0.748623853,
0.750458716,0.752293578,0.75412844,0.755963303,0.757798165,0.759633028,
0.76146789,0.763302752,0.765137615,0.766972477,0.768807339,0.770642202,
0.772477064,0.774311927,0.776146789,0.777981651,0.779816514,0.781651376,
0.783486239,0.785321101,0.787155963,0.788990826,0.790825688,0.79266055,
0.794495413,0.796330275,0.798165138,0.8,0.801834862,0.803669725,0.805504587,
0.80733945,0.809174312,0.811009174,0.812844037,0.814678899,0.816513761,
0.818348624,0.820183486,0.822018349,0.823853211,0.825688073,0.827522936,
0.829357798,0.831192661,0.833027523,0.834862385,0.836697248,0.83853211,
0.840366972,0.842201835,0.844036697,0.84587156,0.847706422,0.849541284,
0.851376147,0.853211009,0.855045872,0.856880734,0.858715596,0.860550459,
0.862385321,0.864220183,0.866055046,0.867889908,0.869724771,0.871559633,
0.873394495,0.875229358,0.87706422,0.878899083,0.880733945,0.882568807,
0.88440367,0.886238532,0.888073394,0.889908257,0.891743119,0.893577982,
0.895412844,0.897247706,0.899082569,0.900917431,0.902752294,0.904587156,
0.906422018,0.908256881,0.910091743,0.911926606,0.913761468,0.91559633,
0.917431193,0.919266055,0.921100917,0.92293578,0.924770642,0.926605505,
0.928440367,0.930275229,0.932110092,0.933944954,0.935779817,0.937614679,
0.939449541,0.941284404,0.943119266,0.944954128,0.946788991,0.948623853,
0.950458716,0.952293578,0.95412844,0.955963303,0.957798165,0.959633028,
0.96146789,0.963302752,0.965137615,0.966972477,0.968807339,0.970642202,
0.972477064,0.974311927,0.976146789,0.977981651,0.979816514,0.981651376,
0.983486239,0.985321101,0.987155963,0.988990826,0.990825688,0.99266055,
0.994495413,0.996330275,0.998165138,1.),.UNSPECIFIED.);
#24454=B_SPLINE_CURVE_WITH_KNOTS('',5,(#265673,#265674,#265675,#265676,
#265677,#265678,#265679,#265680,#265681,#265682,#265683,#265684,#265685,
#265686,#265687,#265688,#265689,#265690,#265691,#265692,#265693,#265694,
#265695,#265696,#265697,#265698,#265699,#265700,#265701,#265702,#265703,
#265704,#265705,#265706,#265707,#265708,#265709,#265710,#265711,#265712,
#265713,#265714,#265715,#265716,#265717,#265718,#265719,#265720,#265721,
#265722,#265723,#265724,#265725,#265726,#265727,#265728,#265729,#265730,
#265731,#265732,#265733,#265734,#265735,#265736,#265737,#265738,#265739,
#265740,#265741,#265742,#265743,#265744,#265745,#265746,#265747,#265748,
#265749,#265750,#265751,#265752,#265753,#265754,#265755,#265756,#265757,
#265758,#265759,#265760,#265761,#265762,#265763,#265764,#265765,#265766,
#265767,#265768,#265769,#265770,#265771,#265772,#265773,#265774,#265775,
#265776,#265777,#265778,#265779,#265780,#265781,#265782,#265783,#265784,
#265785,#265786,#265787,#265788,#265789,#265790,#265791,#265792,#265793,
#265794,#265795,#265796,#265797,#265798,#265799,#265800,#265801,#265802,
#265803,#265804,#265805,#265806,#265807,#265808,#265809,#265810,#265811,
#265812,#265813,#265814,#265815,#265816,#265817,#265818,#265819,#265820,
#265821,#265822,#265823,#265824,#265825,#265826,#265827,#265828,#265829,
#265830,#265831,#265832,#265833,#265834,#265835,#265836,#265837,#265838,
#265839,#265840,#265841,#265842,#265843,#265844,#265845,#265846,#265847,
#265848,#265849,#265850,#265851,#265852,#265853,#265854,#265855,#265856,
#265857,#265858,#265859,#265860,#265861,#265862,#265863,#265864,#265865,
#265866,#265867,#265868,#265869,#265870,#265871,#265872,#265873,#265874,
#265875,#265876,#265877,#265878,#265879,#265880,#265881,#265882,#265883,
#265884,#265885,#265886,#265887,#265888,#265889,#265890,#265891,#265892,
#265893,#265894,#265895,#265896,#265897,#265898,#265899,#265900,#265901,
#265902,#265903,#265904,#265905,#265906,#265907,#265908,#265909,#265910,
#265911,#265912,#265913,#265914,#265915,#265916,#265917,#265918,#265919,
#265920,#265921,#265922,#265923,#265924,#265925,#265926,#265927,#265928,
#265929,#265930,#265931,#265932,#265933,#265934,#265935,#265936,#265937,
#265938,#265939,#265940,#265941,#265942,#265943,#265944,#265945,#265946,
#265947,#265948,#265949,#265950,#265951,#265952,#265953,#265954,#265955,
#265956,#265957,#265958,#265959,#265960,#265961,#265962,#265963,#265964,
#265965,#265966,#265967,#265968,#265969,#265970,#265971,#265972,#265973,
#265974,#265975,#265976,#265977,#265978,#265979,#265980,#265981,#265982,
#265983,#265984,#265985,#265986,#265987,#265988,#265989,#265990,#265991,
#265992,#265993,#265994,#265995,#265996,#265997,#265998,#265999,#266000,
#266001,#266002,#266003,#266004,#266005,#266006,#266007,#266008,#266009,
#266010,#266011,#266012,#266013,#266014,#266015,#266016,#266017,#266018,
#266019,#266020,#266021,#266022,#266023,#266024,#266025,#266026,#266027,
#266028,#266029,#266030,#266031,#266032,#266033,#266034,#266035,#266036,
#266037,#266038,#266039,#266040,#266041,#266042,#266043,#266044,#266045,
#266046,#266047,#266048,#266049,#266050,#266051,#266052,#266053,#266054,
#266055,#266056,#266057,#266058,#266059,#266060,#266061,#266062,#266063,
#266064,#266065,#266066,#266067,#266068,#266069,#266070,#266071,#266072,
#266073,#266074,#266075,#266076,#266077,#266078,#266079,#266080,#266081,
#266082,#266083,#266084,#266085,#266086,#266087,#266088,#266089,#266090,
#266091,#266092,#266093,#266094,#266095,#266096,#266097,#266098,#266099,
#266100,#266101,#266102,#266103,#266104,#266105,#266106,#266107,#266108,
#266109,#266110,#266111,#266112,#266113,#266114,#266115,#266116,#266117,
#266118,#266119,#266120,#266121,#266122,#266123,#266124,#266125,#266126,
#266127,#266128,#266129,#266130,#266131,#266132,#266133,#266134,#266135,
#266136,#266137,#266138,#266139,#266140,#266141,#266142),.UNSPECIFIED.,
 .F.,.F.,(6,1,1,1,1,1,1,1,1,1,1,1,1,1,1,1,1,1,1,1,1,1,1,1,1,1,1,1,1,1,1,
1,1,1,1,1,1,1,1,1,1,1,1,1,1,1,1,1,1,1,1,1,1,1,1,1,1,1,1,1,1,1,1,1,1,1,1,
1,1,1,1,1,1,1,1,1,1,1,1,1,1,1,1,1,1,1,1,1,1,1,1,1,1,1,1,1,1,1,1,1,1,1,1,
1,1,1,1,1,1,1,1,1,1,1,1,1,1,1,1,1,1,1,1,1,1,1,1,1,1,1,1,1,1,1,1,1,1,1,1,
1,1,1,1,1,1,1,1,1,1,1,1,1,1,1,1,1,1,1,1,1,1,1,1,1,1,1,1,1,1,1,1,1,1,1,1,
1,1,1,1,1,1,1,1,1,1,1,1,1,1,1,1,1,1,1,1,1,1,1,1,1,1,1,1,1,1,1,1,1,1,1,1,
1,1,1,1,1,1,1,1,1,1,1,1,1,1,1,1,1,1,1,1,1,1,1,1,1,1,1,1,1,1,1,1,1,1,1,1,
1,1,1,1,1,1,1,1,1,1,1,1,1,1,1,1,1,1,1,1,1,1,1,1,1,1,1,1,1,1,1,1,1,1,1,1,
1,1,1,1,1,1,1,1,1,1,1,1,1,1,1,1,1,1,1,1,1,1,1,1,1,1,1,1,1,1,1,1,1,1,1,1,
1,1,1,1,1,1,1,1,1,1,1,1,1,1,1,1,1,1,1,1,1,1,1,1,1,1,1,1,1,1,1,1,1,1,1,1,
1,1,1,1,1,1,1,1,1,1,1,1,1,1,1,1,1,1,1,1,1,1,1,1,1,1,1,1,1,1,1,1,1,1,1,1,
1,1,1,1,1,1,1,1,1,1,1,1,1,1,1,1,1,1,1,1,1,1,1,1,1,1,1,1,1,1,1,1,1,1,1,1,
1,1,1,1,1,1,1,1,1,1,1,1,1,1,1,1,1,1,1,1,1,1,1,1,1,1,1,1,1,1,1,1,1,1,1,1,
1,1,6),(0.143172102,0.144954128,0.146788991,0.148623853,0.150458716,0.152293578,
0.15412844,0.155963303,0.157798165,0.159633028,0.16146789,0.163302752,0.165137615,
0.166972477,0.168807339,0.170642202,0.172477064,0.174311927,0.176146789,
0.177981651,0.179816514,0.181651376,0.183486239,0.185321101,0.187155963,
0.188990826,0.190825688,0.19266055,0.194495413,0.196330275,0.198165138,
0.2,0.201834862,0.203669725,0.205504587,0.20733945,0.209174312,0.211009174,
0.212844037,0.214678899,0.216513761,0.218348624,0.220183486,0.222018349,
0.223853211,0.225688073,0.227522936,0.229357798,0.231192661,0.233027523,
0.234862385,0.236697248,0.23853211,0.240366972,0.242201835,0.244036697,
0.24587156,0.247706422,0.249541284,0.251376147,0.253211009,0.255045872,
0.256880734,0.258715596,0.260550459,0.262385321,0.264220183,0.266055046,
0.267889908,0.269724771,0.271559633,0.273394495,0.275229358,0.27706422,
0.278899083,0.280733945,0.282568807,0.28440367,0.286238532,0.288073394,
0.289908257,0.291743119,0.293577982,0.295412844,0.297247706,0.299082569,
0.300917431,0.302752294,0.304587156,0.306422018,0.308256881,0.310091743,
0.311926606,0.313761468,0.31559633,0.317431193,0.319266055,0.321100917,
0.32293578,0.324770642,0.326605505,0.328440367,0.330275229,0.333944954,
0.335779817,0.337614679,0.339449541,0.341284404,0.343119266,0.344954128,
0.346788991,0.348623853,0.350458716,0.352293578,0.35412844,0.355963303,
0.357798165,0.359633028,0.36146789,0.363302752,0.365137615,0.366972477,
0.368807339,0.370642202,0.372477064,0.374311927,0.376146789,0.377981651,
0.379816514,0.381651376,0.383486239,0.385321101,0.387155963,0.388990826,
0.390825688,0.39266055,0.394495413,0.396330275,0.398165138,0.4,0.401834862,
0.403669725,0.405504587,0.40733945,0.409174312,0.411009174,0.412844037,
0.414678899,0.416513761,0.418348624,0.420183486,0.422018349,0.423853211,
0.425688073,0.427522936,0.429357798,0.431192661,0.433027523,0.434862385,
0.436697248,0.43853211,0.440366972,0.442201835,0.444036697,0.44587156,0.447706422,
0.449541284,0.451376147,0.453211009,0.455045872,0.456880734,0.458715596,
0.460550459,0.462385321,0.464220183,0.466055046,0.467889908,0.469724771,
0.471559633,0.473394495,0.475229358,0.47706422,0.478899083,0.480733945,
0.482568807,0.48440367,0.486238532,0.488073394,0.489908257,0.491743119,
0.493577982,0.495412844,0.497247706,0.499082569,0.500917431,0.502752294,
0.504587156,0.506422018,0.508256881,0.511926606,0.513761468,0.51559633,
0.517431193,0.519266055,0.521100917,0.52293578,0.524770642,0.526605505,
0.528440367,0.530275229,0.532110092,0.533944954,0.535779817,0.537614679,
0.539449541,0.541284404,0.543119266,0.544954128,0.546788991,0.548623853,
0.550458716,0.552293578,0.55412844,0.555963303,0.557798165,0.559633028,
0.56146789,0.563302752,0.565137615,0.566972477,0.568807339,0.570642202,
0.572477064,0.574311927,0.576146789,0.577981651,0.579816514,0.581651376,
0.583486239,0.585321101,0.587155963,0.588990826,0.590825688,0.59266055,
0.594495413,0.596330275,0.598165138,0.6,0.601834862,0.603669725,0.605504587,
0.60733945,0.609174312,0.611009174,0.612844037,0.614678899,0.616513761,
0.618348624,0.620183486,0.622018349,0.623853211,0.625688073,0.627522936,
0.629357798,0.631192661,0.633027523,0.634862385,0.636697248,0.63853211,
0.640366972,0.642201835,0.644036697,0.64587156,0.647706422,0.649541284,
0.651376147,0.653211009,0.655045872,0.656880734,0.658715596,0.660550459,
0.662385321,0.664220183,0.666055046,0.667889908,0.669724771,0.671559633,
0.673394495,0.675229358,0.67706422,0.678899083,0.680733945,0.682568807,
0.68440367,0.686238532,0.688073394,0.689908257,0.691743119,0.693577982,
0.695412844,0.697247706,0.699082569,0.700917431,0.702752294,0.704587156,
0.706422018,0.708256881,0.710091743,0.711926606,0.713761468,0.71559633,
0.717431193,0.719266055,0.721100917,0.72293578,0.724770642,0.726605505,
0.728440367,0.730275229,0.732110092,0.733944954,0.735779817,0.737614679,
0.739449541,0.741284404,0.743119266,0.744954128,0.746788991,0.748623853,
0.750458716,0.752293578,0.75412844,0.755963303,0.757798165,0.759633028,
0.76146789,0.763302752,0.765137615,0.766972477,0.768807339,0.770642202,
0.772477064,0.774311927,0.776146789,0.777981651,0.779816514,0.781651376,
0.783486239,0.785321101,0.787155963,0.788990826,0.790825688,0.79266055,
0.794495413,0.796330275,0.798165138,0.8,0.801834862,0.803669725,0.805504587,
0.80733945,0.809174312,0.811009174,0.812844037,0.814678899,0.816513761,
0.818348624,0.820183486,0.822018349,0.823853211,0.825688073,0.827522936,
0.829357798,0.831192661,0.833027523,0.834862385,0.836697248,0.83853211,
0.840366972,0.842201835,0.844036697,0.84587156,0.847706422,0.849541284,
0.851376147,0.853211009,0.855045872,0.856880734,0.858715596,0.860550459,
0.862385321,0.864220183,0.866055046,0.867889908,0.869724771,0.871559633,
0.873394495,0.875229358,0.87706422,0.878899083,0.880733945,0.882568807,
0.88440367,0.886238532,0.888073394,0.889908257,0.891743119,0.893577982,
0.895412844,0.897247706,0.899082569,0.900917431,0.902752294,0.904587156,
0.906422018,0.908256881,0.910091743,0.911926606,0.913761468,0.91559633,
0.917431193,0.919266055,0.921100917,0.92293578,0.924770642,0.926605505,
0.928440367,0.930275229,0.932110092,0.933944954,0.935779817,0.937614679,
0.939449541,0.941284404,0.943119266,0.944954128,0.946788991,0.948623853,
0.950458716,0.952293578,0.95412844,0.955963303,0.957798165,0.959633028,
0.96146789,0.963302752,0.965137615,0.966972477,0.968807339,0.970642202,
0.972477064,0.974311927,0.976146789,0.977981651,0.979816514,0.981651376,
0.983486239,0.985321101,0.987155963,0.988990826,0.990825688,0.99266055,
0.994495413,0.996330275,0.998165138,1.),.UNSPECIFIED.);
#24455=B_SPLINE_CURVE_WITH_KNOTS('',3,(#267102,#267103,#267104,#267105,
#267106,#267107,#267108,#267109,#267110,#267111,#267112,#267113,#267114,
#267115,#267116,#267117,#267118,#267119,#267120,#267121,#267122,#267123,
#267124,#267125,#267126,#267127,#267128,#267129,#267130,#267131,#267132,
#267133,#267134,#267135,#267136,#267137,#267138,#267139,#267140,#267141,
#267142,#267143,#267144,#267145,#267146,#267147,#267148,#267149,#267150,
#267151,#267152,#267153,#267154,#267155,#267156,#267157,#267158,#267159,
#267160,#267161,#267162,#267163,#267164,#267165,#267166,#267167,#267168,
#267169,#267170,#267171,#267172,#267173,#267174,#267175,#267176,#267177,
#267178,#267179,#267180,#267181,#267182,#267183,#267184,#267185,#267186,
#267187,#267188,#267189,#267190,#267191,#267192,#267193,#267194,#267195,
#267196,#267197,#267198,#267199,#267200,#267201,#267202,#267203,#267204,
#267205,#267206,#267207,#267208,#267209,#267210,#267211,#267212,#267213,
#267214,#267215,#267216,#267217,#267218,#267219,#267220,#267221,#267222,
#267223,#267224,#267225,#267226,#267227,#267228,#267229,#267230,#267231,
#267232,#267233,#267234,#267235,#267236,#267237,#267238,#267239,#267240,
#267241,#267242,#267243,#267244,#267245,#267246,#267247,#267248,#267249,
#267250,#267251,#267252,#267253,#267254,#267255,#267256,#267257,#267258,
#267259,#267260,#267261,#267262,#267263,#267264,#267265,#267266,#267267,
#267268,#267269,#267270,#267271,#267272,#267273,#267274,#267275,#267276,
#267277,#267278,#267279,#267280,#267281,#267282,#267283,#267284,#267285,
#267286,#267287,#267288,#267289,#267290,#267291,#267292,#267293,#267294,
#267295,#267296,#267297,#267298,#267299,#267300,#267301,#267302,#267303,
#267304,#267305,#267306,#267307,#267308,#267309,#267310,#267311,#267312,
#267313,#267314,#267315,#267316,#267317,#267318,#267319,#267320,#267321,
#267322,#267323,#267324,#267325,#267326,#267327,#267328,#267329,#267330,
#267331,#267332,#267333,#267334,#267335,#267336,#267337,#267338,#267339,
#267340,#267341,#267342,#267343,#267344,#267345,#267346,#267347,#267348,
#267349,#267350,#267351,#267352,#267353,#267354,#267355,#267356,#267357,
#267358,#267359,#267360,#267361,#267362,#267363,#267364,#267365,#267366,
#267367,#267368,#267369,#267370,#267371,#267372,#267373,#267374,#267375,
#267376,#267377,#267378,#267379,#267380,#267381,#267382,#267383,#267384,
#267385,#267386,#267387,#267388,#267389,#267390,#267391,#267392,#267393,
#267394,#267395,#267396,#267397,#267398,#267399,#267400,#267401,#267402,
#267403,#267404,#267405,#267406,#267407,#267408,#267409,#267410,#267411,
#267412,#267413,#267414),.UNSPECIFIED.,.F.,.F.,(4,3,3,3,3,3,3,3,3,3,3,3,
3,3,3,3,3,3,3,3,3,3,3,3,3,3,3,3,3,3,3,3,3,3,3,3,3,3,3,3,3,3,3,3,3,3,3,3,
3,3,3,3,3,3,3,3,3,3,3,3,3,3,3,3,3,3,3,3,3,3,3,3,3,3,3,3,3,3,3,3,3,3,3,3,
3,3,3,3,3,3,3,3,3,3,3,3,3,3,3,3,3,3,3,3,4),(0.143172102,0.15412844,0.165137615,
0.176146789,0.187155963,0.198165138,0.209174312,0.222018349,0.233027523,
0.244036697,0.255045872,0.266055046,0.27706422,0.288073394,0.299082569,
0.310091743,0.32293578,0.333944954,0.344954128,0.355963303,0.368807339,
0.379816514,0.390825688,0.4,0.409174312,0.418348624,0.429357798,0.43853211,
0.447706422,0.458715596,0.467889908,0.478899083,0.488073394,0.497247706,
0.506422018,0.517431193,0.526605505,0.535779817,0.544954128,0.552293578,
0.559633028,0.566972477,0.574311927,0.581651376,0.588990826,0.596330275,
0.603669725,0.611009174,0.618348624,0.627522936,0.634862385,0.642201835,
0.649541284,0.658715596,0.666055046,0.675229358,0.68440367,0.693577982,
0.700917431,0.711926606,0.719266055,0.726605505,0.735779817,0.743119266,
0.750458716,0.759633028,0.766972477,0.774311927,0.781651376,0.788990826,
0.798165138,0.80733945,0.812844037,0.818348624,0.823853211,0.829357798,
0.834862385,0.840366972,0.84587156,0.851376147,0.856880734,0.862385321,
0.869724771,0.875229358,0.880733945,0.886238532,0.891743119,0.897247706,
0.902752294,0.908256881,0.913761468,0.919266055,0.926605505,0.932110092,
0.937614679,0.943119266,0.948623853,0.95412844,0.963302752,0.968807339,
0.976146789,0.983486239,0.988990826,0.994495413,1.),.UNSPECIFIED.);
#24456=B_SPLINE_CURVE_WITH_KNOTS('',3,(#267415,#267416,#267417,#267418,
#267419,#267420,#267421,#267422,#267423,#267424,#267425,#267426,#267427,
#267428,#267429,#267430,#267431,#267432,#267433,#267434,#267435,#267436,
#267437,#267438,#267439,#267440,#267441,#267442,#267443,#267444,#267445,
#267446,#267447,#267448,#267449,#267450,#267451,#267452,#267453,#267454,
#267455,#267456,#267457,#267458,#267459,#267460,#267461,#267462,#267463,
#267464,#267465,#267466,#267467,#267468,#267469,#267470,#267471,#267472,
#267473,#267474,#267475,#267476,#267477,#267478,#267479,#267480,#267481,
#267482,#267483,#267484,#267485,#267486,#267487,#267488,#267489,#267490,
#267491,#267492,#267493,#267494,#267495,#267496,#267497,#267498,#267499,
#267500,#267501,#267502,#267503,#267504,#267505,#267506,#267507,#267508,
#267509,#267510,#267511,#267512,#267513,#267514,#267515,#267516,#267517,
#267518,#267519,#267520,#267521,#267522,#267523,#267524,#267525,#267526,
#267527,#267528,#267529,#267530,#267531,#267532,#267533,#267534,#267535,
#267536,#267537,#267538,#267539,#267540,#267541,#267542,#267543,#267544,
#267545,#267546,#267547,#267548,#267549,#267550,#267551,#267552,#267553,
#267554,#267555,#267556,#267557,#267558,#267559,#267560,#267561,#267562,
#267563,#267564,#267565,#267566,#267567,#267568,#267569,#267570,#267571,
#267572,#267573,#267574,#267575,#267576,#267577,#267578,#267579,#267580,
#267581,#267582,#267583,#267584,#267585,#267586,#267587,#267588,#267589,
#267590,#267591,#267592,#267593,#267594,#267595,#267596,#267597,#267598,
#267599,#267600,#267601,#267602,#267603,#267604,#267605,#267606,#267607,
#267608,#267609,#267610,#267611,#267612,#267613,#267614,#267615,#267616,
#267617,#267618,#267619,#267620,#267621,#267622,#267623,#267624,#267625,
#267626,#267627,#267628,#267629,#267630,#267631,#267632,#267633,#267634,
#267635,#267636,#267637,#267638,#267639,#267640,#267641,#267642,#267643,
#267644,#267645,#267646,#267647,#267648,#267649,#267650,#267651,#267652,
#267653,#267654,#267655,#267656,#267657,#267658,#267659,#267660,#267661,
#267662,#267663,#267664,#267665,#267666,#267667,#267668,#267669,#267670,
#267671,#267672,#267673,#267674,#267675,#267676,#267677,#267678,#267679,
#267680,#267681,#267682,#267683,#267684,#267685,#267686,#267687,#267688,
#267689,#267690,#267691,#267692,#267693,#267694,#267695,#267696,#267697,
#267698,#267699,#267700,#267701,#267702,#267703,#267704,#267705,#267706,
#267707,#267708,#267709,#267710,#267711,#267712,#267713,#267714,#267715,
#267716,#267717,#267718,#267719,#267720,#267721,#267722,#267723,#267724,
#267725,#267726,#267727,#267728,#267729,#267730,#267731,#267732,#267733,
#267734,#267735,#267736,#267737,#267738,#267739,#267740,#267741,#267742),
 .UNSPECIFIED.,.F.,.F.,(4,3,3,3,3,3,3,3,3,3,3,3,3,3,3,3,3,3,3,3,3,3,3,3,
3,3,3,3,3,3,3,3,3,3,3,3,3,3,3,3,3,3,3,3,3,3,3,3,3,3,3,3,3,3,3,3,3,3,3,3,
3,3,3,3,3,3,3,3,3,3,3,3,3,3,3,3,3,3,3,3,3,3,3,3,3,3,3,3,3,3,3,3,3,3,3,3,
3,3,3,3,3,3,3,3,3,3,3,3,3,4),(0.143172102,0.15412844,0.165137615,0.176146789,
0.187155963,0.198165138,0.209174312,0.220183486,0.231192661,0.242201835,
0.253211009,0.266055046,0.27706422,0.288073394,0.299082569,0.310091743,
0.321100917,0.332110092,0.343119266,0.355963303,0.366972477,0.377981651,
0.388990826,0.398165138,0.40733945,0.416513761,0.425688073,0.434862385,
0.444036697,0.453211009,0.462385321,0.471559633,0.480733945,0.489908257,
0.499082569,0.508256881,0.517431193,0.526605505,0.533944954,0.541284404,
0.548623853,0.555963303,0.563302752,0.570642202,0.579816514,0.587155963,
0.594495413,0.601834862,0.609174312,0.616513761,0.623853211,0.631192661,
0.63853211,0.64587156,0.653211009,0.660550459,0.667889908,0.675229358,0.682568807,
0.689908257,0.697247706,0.704587156,0.711926606,0.719266055,0.726605505,
0.733944954,0.743119266,0.750458716,0.757798165,0.765137615,0.772477064,
0.779816514,0.787155963,0.794495413,0.801834862,0.809174312,0.814678899,
0.820183486,0.825688073,0.831192661,0.836697248,0.842201835,0.849541284,
0.855045872,0.860550459,0.866055046,0.871559633,0.87706422,0.882568807,
0.888073394,0.893577982,0.899082569,0.904587156,0.910091743,0.91559633,
0.921100917,0.926605505,0.932110092,0.937614679,0.943119266,0.948623853,
0.95412844,0.959633028,0.965137615,0.972477064,0.977981651,0.983486239,
0.988990826,0.994495413,1.),.UNSPECIFIED.);
#24457=B_SPLINE_CURVE_WITH_KNOTS('',5,(#268690,#268691,#268692,#268693,
#268694,#268695,#268696,#268697,#268698,#268699,#268700,#268701,#268702,
#268703,#268704,#268705,#268706,#268707,#268708,#268709,#268710,#268711,
#268712,#268713,#268714,#268715,#268716,#268717,#268718,#268719,#268720,
#268721,#268722,#268723,#268724,#268725,#268726,#268727,#268728,#268729,
#268730,#268731,#268732,#268733,#268734,#268735,#268736,#268737,#268738,
#268739,#268740,#268741,#268742,#268743,#268744,#268745,#268746,#268747,
#268748,#268749,#268750,#268751,#268752,#268753,#268754,#268755,#268756,
#268757,#268758,#268759,#268760,#268761,#268762,#268763,#268764,#268765,
#268766,#268767,#268768,#268769,#268770,#268771,#268772,#268773,#268774,
#268775,#268776,#268777,#268778,#268779,#268780,#268781,#268782,#268783,
#268784,#268785,#268786,#268787,#268788,#268789,#268790,#268791,#268792,
#268793,#268794,#268795,#268796,#268797,#268798,#268799,#268800,#268801,
#268802,#268803,#268804,#268805,#268806,#268807,#268808,#268809,#268810,
#268811,#268812,#268813,#268814,#268815,#268816,#268817,#268818,#268819,
#268820,#268821,#268822,#268823,#268824,#268825,#268826,#268827,#268828,
#268829,#268830,#268831,#268832,#268833,#268834,#268835,#268836,#268837,
#268838,#268839,#268840,#268841,#268842,#268843,#268844,#268845,#268846,
#268847,#268848,#268849,#268850,#268851,#268852,#268853,#268854,#268855,
#268856,#268857,#268858,#268859,#268860,#268861,#268862,#268863,#268864,
#268865,#268866,#268867,#268868,#268869,#268870,#268871,#268872,#268873,
#268874,#268875,#268876,#268877,#268878,#268879,#268880,#268881,#268882,
#268883,#268884,#268885,#268886,#268887,#268888,#268889,#268890,#268891,
#268892,#268893,#268894,#268895,#268896,#268897,#268898,#268899,#268900,
#268901,#268902,#268903,#268904,#268905,#268906,#268907,#268908,#268909,
#268910,#268911,#268912,#268913,#268914,#268915,#268916,#268917,#268918,
#268919,#268920,#268921,#268922,#268923,#268924,#268925,#268926,#268927,
#268928,#268929,#268930,#268931,#268932,#268933,#268934,#268935,#268936,
#268937,#268938,#268939,#268940,#268941,#268942,#268943,#268944,#268945,
#268946,#268947,#268948,#268949,#268950,#268951,#268952,#268953,#268954,
#268955,#268956,#268957,#268958,#268959,#268960,#268961,#268962,#268963,
#268964,#268965,#268966,#268967,#268968,#268969,#268970,#268971,#268972,
#268973,#268974,#268975,#268976,#268977,#268978,#268979,#268980,#268981,
#268982,#268983,#268984,#268985,#268986,#268987,#268988,#268989,#268990,
#268991,#268992,#268993,#268994,#268995,#268996,#268997,#268998,#268999,
#269000,#269001,#269002,#269003,#269004,#269005,#269006,#269007,#269008,
#269009,#269010,#269011,#269012,#269013,#269014,#269015,#269016,#269017,
#269018,#269019,#269020,#269021,#269022,#269023,#269024,#269025,#269026,
#269027,#269028,#269029,#269030,#269031,#269032,#269033,#269034,#269035,
#269036,#269037,#269038,#269039,#269040,#269041,#269042,#269043,#269044,
#269045,#269046,#269047,#269048,#269049,#269050,#269051,#269052,#269053,
#269054,#269055,#269056,#269057,#269058,#269059,#269060,#269061,#269062,
#269063,#269064,#269065,#269066,#269067,#269068,#269069,#269070,#269071,
#269072,#269073,#269074,#269075,#269076,#269077,#269078,#269079,#269080,
#269081,#269082,#269083,#269084,#269085,#269086,#269087,#269088,#269089,
#269090,#269091,#269092,#269093,#269094,#269095,#269096,#269097,#269098,
#269099,#269100,#269101,#269102,#269103,#269104,#269105,#269106,#269107,
#269108,#269109,#269110,#269111,#269112,#269113,#269114,#269115,#269116,
#269117,#269118,#269119,#269120,#269121,#269122,#269123,#269124,#269125,
#269126,#269127,#269128,#269129,#269130,#269131,#269132,#269133,#269134,
#269135,#269136,#269137,#269138,#269139,#269140,#269141,#269142,#269143,
#269144,#269145,#269146,#269147,#269148,#269149,#269150,#269151,#269152,
#269153,#269154,#269155,#269156,#269157,#269158,#269159,#269160),
 .UNSPECIFIED.,.F.,.F.,(6,1,1,1,1,1,1,1,1,1,1,1,1,1,1,1,1,1,1,1,1,1,1,1,
1,1,1,1,1,1,1,1,1,1,1,1,1,1,1,1,1,1,1,1,1,1,1,1,1,1,1,1,1,1,1,1,1,1,1,1,
1,1,1,1,1,1,1,1,1,1,1,1,1,1,1,1,1,1,1,1,1,1,1,1,1,1,1,1,1,1,1,1,1,1,1,1,
1,1,1,1,1,1,1,1,1,1,1,1,1,1,1,1,1,1,1,1,1,1,1,1,1,1,1,1,1,1,1,1,1,1,1,1,
1,1,1,1,1,1,1,1,1,1,1,1,1,1,1,1,1,1,1,1,1,1,1,1,1,1,1,1,1,1,1,1,1,1,1,1,
1,1,1,1,1,1,1,1,1,1,1,1,1,1,1,1,1,1,1,1,1,1,1,1,1,1,1,1,1,1,1,1,1,1,1,1,
1,1,1,1,1,1,1,1,1,1,1,1,1,1,1,1,1,1,1,1,1,1,1,1,1,1,1,1,1,1,1,1,1,1,1,1,
1,1,1,1,1,1,1,1,1,1,1,1,1,1,1,1,1,1,1,1,1,1,1,1,1,1,1,1,1,1,1,1,1,1,1,1,
1,1,1,1,1,1,1,1,1,1,1,1,1,1,1,1,1,1,1,1,1,1,1,1,1,1,1,1,1,1,1,1,1,1,1,1,
1,1,1,1,1,1,1,1,1,1,1,1,1,1,1,1,1,1,1,1,1,1,1,1,1,1,1,1,1,1,1,1,1,1,1,1,
1,1,1,1,1,1,1,1,1,1,1,1,1,1,1,1,1,1,1,1,1,1,1,1,1,1,1,1,1,1,1,1,1,1,1,1,
1,1,1,1,1,1,1,1,1,1,1,1,1,1,1,1,1,1,1,1,1,1,1,1,1,1,1,1,1,1,1,1,1,1,1,1,
1,1,1,1,1,1,1,1,1,1,1,1,1,1,1,1,1,1,1,1,1,1,1,1,1,1,1,1,1,1,1,1,1,1,1,1,
1,1,1,1,1,1,1,1,1,1,6),(-1.,-0.998165138,-0.996330275,-0.994495413,-0.99266055,
-0.990825688,-0.988990826,-0.987155963,-0.985321101,-0.983486239,-0.981651376,
-0.979816514,-0.977981651,-0.976146789,-0.974311927,-0.972477064,-0.970642202,
-0.968807339,-0.966972477,-0.965137615,-0.963302752,-0.96146789,-0.959633028,
-0.957798165,-0.955963303,-0.95412844,-0.952293578,-0.950458716,-0.948623853,
-0.946788991,-0.944954128,-0.943119266,-0.941284404,-0.939449541,-0.937614679,
-0.935779817,-0.933944954,-0.932110092,-0.930275229,-0.928440367,-0.926605505,
-0.924770642,-0.92293578,-0.921100917,-0.919266055,-0.917431193,-0.91559633,
-0.913761468,-0.911926606,-0.910091743,-0.908256881,-0.906422018,-0.904587156,
-0.902752294,-0.900917431,-0.899082569,-0.897247706,-0.895412844,-0.893577982,
-0.891743119,-0.889908257,-0.888073394,-0.886238532,-0.88440367,-0.882568807,
-0.880733945,-0.878899083,-0.87706422,-0.875229358,-0.873394495,-0.871559633,
-0.869724771,-0.867889908,-0.866055046,-0.864220183,-0.862385321,-0.860550459,
-0.858715596,-0.856880734,-0.855045872,-0.853211009,-0.851376147,-0.849541284,
-0.847706422,-0.84587156,-0.844036697,-0.842201835,-0.840366972,-0.83853211,
-0.836697248,-0.834862385,-0.833027523,-0.831192661,-0.829357798,-0.827522936,
-0.825688073,-0.823853211,-0.822018349,-0.820183486,-0.818348624,-0.816513761,
-0.814678899,-0.812844037,-0.811009174,-0.809174312,-0.80733945,-0.805504587,
-0.803669725,-0.801834862,-0.8,-0.798165138,-0.796330275,-0.794495413,-0.79266055,
-0.790825688,-0.788990826,-0.787155963,-0.785321101,-0.783486239,-0.781651376,
-0.779816514,-0.777981651,-0.776146789,-0.774311927,-0.772477064,-0.770642202,
-0.768807339,-0.766972477,-0.765137615,-0.763302752,-0.76146789,-0.759633028,
-0.757798165,-0.755963303,-0.75412844,-0.752293578,-0.750458716,-0.748623853,
-0.746788991,-0.744954128,-0.743119266,-0.741284404,-0.739449541,-0.737614679,
-0.735779817,-0.733944954,-0.732110092,-0.730275229,-0.728440367,-0.726605505,
-0.724770642,-0.72293578,-0.721100917,-0.719266055,-0.717431193,-0.71559633,
-0.713761468,-0.711926606,-0.710091743,-0.708256881,-0.706422018,-0.704587156,
-0.702752294,-0.700917431,-0.699082569,-0.697247706,-0.695412844,-0.693577982,
-0.691743119,-0.689908257,-0.688073394,-0.686238532,-0.68440367,-0.682568807,
-0.680733945,-0.678899083,-0.67706422,-0.675229358,-0.673394495,-0.671559633,
-0.669724771,-0.667889908,-0.666055046,-0.664220183,-0.662385321,-0.660550459,
-0.658715596,-0.656880734,-0.655045872,-0.653211009,-0.651376147,-0.649541284,
-0.647706422,-0.64587156,-0.644036697,-0.640366972,-0.63853211,-0.636697248,
-0.634862385,-0.633027523,-0.631192661,-0.629357798,-0.627522936,-0.625688073,
-0.623853211,-0.622018349,-0.620183486,-0.618348624,-0.616513761,-0.614678899,
-0.612844037,-0.611009174,-0.609174312,-0.60733945,-0.605504587,-0.603669725,
-0.601834862,-0.6,-0.598165138,-0.596330275,-0.594495413,-0.59266055,-0.590825688,
-0.588990826,-0.587155963,-0.585321101,-0.583486239,-0.581651376,-0.579816514,
-0.577981651,-0.576146789,-0.574311927,-0.572477064,-0.570642202,-0.568807339,
-0.566972477,-0.565137615,-0.563302752,-0.56146789,-0.559633028,-0.557798165,
-0.555963303,-0.55412844,-0.552293578,-0.550458716,-0.548623853,-0.546788991,
-0.544954128,-0.543119266,-0.541284404,-0.539449541,-0.537614679,-0.535779817,
-0.533944954,-0.532110092,-0.530275229,-0.528440367,-0.526605505,-0.524770642,
-0.52293578,-0.521100917,-0.519266055,-0.517431193,-0.51559633,-0.513761468,
-0.511926606,-0.510091743,-0.508256881,-0.506422018,-0.504587156,-0.502752294,
-0.500917431,-0.499082569,-0.497247706,-0.495412844,-0.493577982,-0.491743119,
-0.489908257,-0.488073394,-0.486238532,-0.48440367,-0.482568807,-0.480733945,
-0.478899083,-0.47706422,-0.475229358,-0.473394495,-0.471559633,-0.469724771,
-0.467889908,-0.466055046,-0.464220183,-0.462385321,-0.460550459,-0.458715596,
-0.456880734,-0.455045872,-0.453211009,-0.451376147,-0.449541284,-0.447706422,
-0.44587156,-0.444036697,-0.442201835,-0.440366972,-0.43853211,-0.436697248,
-0.434862385,-0.433027523,-0.431192661,-0.429357798,-0.427522936,-0.425688073,
-0.423853211,-0.422018349,-0.420183486,-0.418348624,-0.416513761,-0.414678899,
-0.412844037,-0.411009174,-0.409174312,-0.40733945,-0.405504587,-0.403669725,
-0.401834862,-0.4,-0.398165138,-0.396330275,-0.394495413,-0.39266055,-0.390825688,
-0.388990826,-0.387155963,-0.385321101,-0.383486239,-0.381651376,-0.379816514,
-0.377981651,-0.376146789,-0.374311927,-0.372477064,-0.370642202,-0.368807339,
-0.366972477,-0.365137615,-0.363302752,-0.36146789,-0.359633028,-0.357798165,
-0.355963303,-0.35412844,-0.352293578,-0.350458716,-0.348623853,-0.346788991,
-0.344954128,-0.343119266,-0.341284404,-0.339449541,-0.337614679,-0.335779817,
-0.333944954,-0.332110092,-0.330275229,-0.328440367,-0.326605505,-0.324770642,
-0.32293578,-0.321100917,-0.319266055,-0.317431193,-0.31559633,-0.313761468,
-0.311926606,-0.310091743,-0.308256881,-0.306422018,-0.304587156,-0.302752294,
-0.300917431,-0.299082569,-0.297247706,-0.295412844,-0.293577982,-0.291743119,
-0.289908257,-0.288073394,-0.286238532,-0.28440367,-0.282568807,-0.280733945,
-0.278899083,-0.27706422,-0.275229358,-0.273394495,-0.271559633,-0.269724771,
-0.267889908,-0.266055046,-0.264220183,-0.262385321,-0.260550459,-0.258715596,
-0.256880734,-0.255045872,-0.253211009,-0.251376147,-0.249541284,-0.247706422,
-0.24587156,-0.244036697,-0.242201835,-0.240366972,-0.23853211,-0.236697248,
-0.234862385,-0.233027523,-0.231192661,-0.229357798,-0.227522936,-0.225688073,
-0.223853211,-0.222018349,-0.220183486,-0.218348624,-0.216513761,-0.214678899,
-0.212844037,-0.211009174,-0.209174312,-0.20733945,-0.205504587,-0.203669725,
-0.201834862,-0.2,-0.198165138,-0.196330275,-0.194495413,-0.19266055,-0.190825688,
-0.188990826,-0.187155963,-0.185321101,-0.183486239,-0.181651376,-0.179816514,
-0.177981651,-0.176146789,-0.174311927,-0.172477064,-0.170642202,-0.168807339,
-0.166972477,-0.165137615,-0.163302752,-0.16146789,-0.159633028,-0.157798165,
-0.155963303,-0.15412844,-0.152293578,-0.150458716,-0.148623853,-0.146788991,
-0.144954128,-0.143172102),.UNSPECIFIED.);
#24458=B_SPLINE_CURVE_WITH_KNOTS('',5,(#269161,#269162,#269163,#269164,
#269165,#269166,#269167,#269168,#269169,#269170,#269171,#269172,#269173,
#269174,#269175,#269176,#269177,#269178,#269179,#269180,#269181,#269182,
#269183,#269184,#269185,#269186,#269187,#269188,#269189,#269190,#269191,
#269192,#269193,#269194,#269195,#269196,#269197,#269198,#269199,#269200,
#269201,#269202,#269203,#269204,#269205,#269206,#269207,#269208,#269209,
#269210,#269211,#269212,#269213,#269214,#269215,#269216,#269217,#269218,
#269219,#269220,#269221,#269222,#269223,#269224,#269225,#269226,#269227,
#269228,#269229,#269230,#269231,#269232,#269233,#269234,#269235,#269236,
#269237,#269238,#269239,#269240,#269241,#269242,#269243,#269244,#269245,
#269246,#269247,#269248,#269249,#269250,#269251,#269252,#269253,#269254,
#269255,#269256,#269257,#269258,#269259,#269260,#269261,#269262,#269263,
#269264,#269265,#269266,#269267,#269268,#269269,#269270,#269271,#269272,
#269273,#269274,#269275,#269276,#269277,#269278,#269279,#269280,#269281,
#269282,#269283,#269284,#269285,#269286,#269287,#269288,#269289,#269290,
#269291,#269292,#269293,#269294,#269295,#269296,#269297,#269298,#269299,
#269300,#269301,#269302,#269303,#269304,#269305,#269306,#269307,#269308,
#269309,#269310,#269311,#269312,#269313,#269314,#269315,#269316,#269317,
#269318,#269319,#269320,#269321,#269322,#269323,#269324,#269325,#269326,
#269327,#269328,#269329,#269330,#269331,#269332,#269333,#269334,#269335,
#269336,#269337,#269338,#269339,#269340,#269341,#269342,#269343,#269344,
#269345,#269346,#269347,#269348,#269349,#269350,#269351,#269352,#269353,
#269354,#269355,#269356,#269357,#269358,#269359,#269360,#269361,#269362,
#269363,#269364,#269365,#269366,#269367,#269368,#269369,#269370,#269371,
#269372,#269373,#269374,#269375,#269376,#269377,#269378,#269379,#269380,
#269381,#269382,#269383,#269384,#269385,#269386,#269387,#269388,#269389,
#269390,#269391,#269392,#269393,#269394,#269395,#269396,#269397,#269398,
#269399,#269400,#269401,#269402,#269403,#269404,#269405,#269406,#269407,
#269408,#269409,#269410,#269411,#269412,#269413,#269414,#269415,#269416,
#269417,#269418,#269419,#269420,#269421,#269422,#269423,#269424,#269425,
#269426,#269427,#269428,#269429,#269430,#269431,#269432,#269433,#269434,
#269435,#269436,#269437,#269438,#269439,#269440,#269441,#269442,#269443,
#269444,#269445,#269446,#269447,#269448,#269449,#269450,#269451,#269452,
#269453,#269454,#269455,#269456,#269457,#269458,#269459,#269460,#269461,
#269462,#269463,#269464,#269465,#269466,#269467,#269468,#269469,#269470,
#269471,#269472,#269473,#269474,#269475,#269476,#269477,#269478,#269479,
#269480,#269481,#269482,#269483,#269484,#269485,#269486,#269487,#269488,
#269489,#269490,#269491,#269492,#269493,#269494,#269495,#269496,#269497,
#269498,#269499,#269500,#269501,#269502,#269503,#269504,#269505,#269506,
#269507,#269508,#269509,#269510,#269511,#269512,#269513,#269514,#269515,
#269516,#269517,#269518,#269519,#269520,#269521,#269522,#269523,#269524,
#269525,#269526,#269527,#269528,#269529,#269530,#269531,#269532,#269533,
#269534,#269535,#269536,#269537,#269538,#269539,#269540,#269541,#269542,
#269543,#269544,#269545,#269546,#269547,#269548,#269549,#269550,#269551,
#269552,#269553,#269554,#269555,#269556,#269557,#269558,#269559,#269560,
#269561,#269562,#269563,#269564,#269565,#269566,#269567,#269568,#269569,
#269570,#269571,#269572,#269573,#269574,#269575,#269576,#269577,#269578,
#269579,#269580,#269581,#269582,#269583,#269584,#269585,#269586,#269587,
#269588,#269589,#269590,#269591,#269592,#269593,#269594,#269595,#269596,
#269597,#269598,#269599,#269600,#269601,#269602,#269603,#269604,#269605,
#269606,#269607,#269608,#269609,#269610,#269611,#269612,#269613,#269614,
#269615,#269616,#269617,#269618,#269619,#269620,#269621,#269622,#269623,
#269624,#269625,#269626,#269627,#269628,#269629,#269630,#269631),
 .UNSPECIFIED.,.F.,.F.,(6,1,1,1,1,1,1,1,1,1,1,1,1,1,1,1,1,1,1,1,1,1,1,1,
1,1,1,1,1,1,1,1,1,1,1,1,1,1,1,1,1,1,1,1,1,1,1,1,1,1,1,1,1,1,1,1,1,1,1,1,
1,1,1,1,1,1,1,1,1,1,1,1,1,1,1,1,1,1,1,1,1,1,1,1,1,1,1,1,1,1,1,1,1,1,1,1,
1,1,1,1,1,1,1,1,1,1,1,1,1,1,1,1,1,1,1,1,1,1,1,1,1,1,1,1,1,1,1,1,1,1,1,1,
1,1,1,1,1,1,1,1,1,1,1,1,1,1,1,1,1,1,1,1,1,1,1,1,1,1,1,1,1,1,1,1,1,1,1,1,
1,1,1,1,1,1,1,1,1,1,1,1,1,1,1,1,1,1,1,1,1,1,1,1,1,1,1,1,1,1,1,1,1,1,1,1,
1,1,1,1,1,1,1,1,1,1,1,1,1,1,1,1,1,1,1,1,1,1,1,1,1,1,1,1,1,1,1,1,1,1,1,1,
1,1,1,1,1,1,1,1,1,1,1,1,1,1,1,1,1,1,1,1,1,1,1,1,1,1,1,1,1,1,1,1,1,1,1,1,
1,1,1,1,1,1,1,1,1,1,1,1,1,1,1,1,1,1,1,1,1,1,1,1,1,1,1,1,1,1,1,1,1,1,1,1,
1,1,1,1,1,1,1,1,1,1,1,1,1,1,1,1,1,1,1,1,1,1,1,1,1,1,1,1,1,1,1,1,1,1,1,1,
1,1,1,1,1,1,1,1,1,1,1,1,1,1,1,1,1,1,1,1,1,1,1,1,1,1,1,1,1,1,1,1,1,1,1,1,
1,1,1,1,1,1,1,1,1,1,1,1,1,1,1,1,1,1,1,1,1,1,1,1,1,1,1,1,1,1,1,1,1,1,1,1,
1,1,1,1,1,1,1,1,1,1,1,1,1,1,1,1,1,1,1,1,1,1,1,1,1,1,1,1,1,1,1,1,1,1,1,1,
1,1,1,1,1,1,1,1,1,1,6),(0.143172102,0.144954128,0.146788991,0.148623853,
0.150458716,0.152293578,0.15412844,0.155963303,0.157798165,0.159633028,
0.16146789,0.163302752,0.165137615,0.166972477,0.168807339,0.170642202,
0.172477064,0.174311927,0.176146789,0.177981651,0.179816514,0.181651376,
0.183486239,0.185321101,0.187155963,0.188990826,0.190825688,0.19266055,
0.194495413,0.196330275,0.198165138,0.2,0.201834862,0.203669725,0.205504587,
0.20733945,0.209174312,0.211009174,0.212844037,0.214678899,0.216513761,
0.218348624,0.220183486,0.222018349,0.223853211,0.225688073,0.227522936,
0.229357798,0.231192661,0.233027523,0.234862385,0.236697248,0.23853211,
0.240366972,0.242201835,0.244036697,0.24587156,0.247706422,0.249541284,
0.251376147,0.253211009,0.255045872,0.256880734,0.258715596,0.260550459,
0.262385321,0.264220183,0.266055046,0.267889908,0.269724771,0.271559633,
0.273394495,0.275229358,0.27706422,0.278899083,0.280733945,0.282568807,
0.28440367,0.286238532,0.288073394,0.289908257,0.291743119,0.293577982,
0.295412844,0.297247706,0.299082569,0.300917431,0.302752294,0.304587156,
0.306422018,0.308256881,0.310091743,0.311926606,0.313761468,0.31559633,
0.317431193,0.319266055,0.321100917,0.32293578,0.324770642,0.326605505,
0.328440367,0.330275229,0.332110092,0.333944954,0.335779817,0.337614679,
0.339449541,0.341284404,0.343119266,0.344954128,0.346788991,0.348623853,
0.350458716,0.352293578,0.35412844,0.355963303,0.357798165,0.359633028,
0.36146789,0.363302752,0.365137615,0.366972477,0.368807339,0.370642202,
0.372477064,0.374311927,0.376146789,0.377981651,0.379816514,0.381651376,
0.383486239,0.385321101,0.387155963,0.388990826,0.390825688,0.39266055,
0.394495413,0.396330275,0.398165138,0.4,0.401834862,0.403669725,0.405504587,
0.40733945,0.409174312,0.411009174,0.412844037,0.414678899,0.416513761,
0.418348624,0.420183486,0.422018349,0.423853211,0.425688073,0.427522936,
0.429357798,0.431192661,0.433027523,0.434862385,0.436697248,0.43853211,
0.440366972,0.442201835,0.444036697,0.44587156,0.447706422,0.449541284,
0.451376147,0.453211009,0.455045872,0.456880734,0.458715596,0.460550459,
0.462385321,0.464220183,0.466055046,0.467889908,0.469724771,0.471559633,
0.473394495,0.475229358,0.47706422,0.478899083,0.480733945,0.482568807,
0.48440367,0.486238532,0.488073394,0.489908257,0.491743119,0.493577982,
0.495412844,0.497247706,0.499082569,0.500917431,0.502752294,0.504587156,
0.506422018,0.508256881,0.510091743,0.511926606,0.513761468,0.51559633,
0.517431193,0.519266055,0.521100917,0.52293578,0.524770642,0.526605505,
0.528440367,0.530275229,0.532110092,0.533944954,0.535779817,0.537614679,
0.539449541,0.541284404,0.543119266,0.544954128,0.546788991,0.548623853,
0.550458716,0.552293578,0.55412844,0.555963303,0.557798165,0.559633028,
0.56146789,0.563302752,0.565137615,0.566972477,0.568807339,0.570642202,
0.572477064,0.574311927,0.576146789,0.577981651,0.579816514,0.581651376,
0.583486239,0.585321101,0.587155963,0.588990826,0.590825688,0.59266055,
0.594495413,0.596330275,0.598165138,0.6,0.601834862,0.603669725,0.605504587,
0.60733945,0.609174312,0.611009174,0.612844037,0.614678899,0.616513761,
0.618348624,0.620183486,0.622018349,0.623853211,0.625688073,0.627522936,
0.629357798,0.631192661,0.633027523,0.634862385,0.636697248,0.63853211,
0.640366972,0.644036697,0.64587156,0.647706422,0.649541284,0.651376147,
0.653211009,0.655045872,0.656880734,0.658715596,0.660550459,0.662385321,
0.664220183,0.666055046,0.667889908,0.669724771,0.671559633,0.673394495,
0.675229358,0.67706422,0.678899083,0.680733945,0.682568807,0.68440367,0.686238532,
0.688073394,0.689908257,0.691743119,0.693577982,0.695412844,0.697247706,
0.699082569,0.700917431,0.702752294,0.704587156,0.706422018,0.708256881,
0.710091743,0.711926606,0.713761468,0.71559633,0.717431193,0.719266055,
0.721100917,0.72293578,0.724770642,0.726605505,0.728440367,0.730275229,
0.732110092,0.733944954,0.735779817,0.737614679,0.739449541,0.741284404,
0.743119266,0.744954128,0.746788991,0.748623853,0.750458716,0.752293578,
0.75412844,0.755963303,0.757798165,0.759633028,0.76146789,0.763302752,0.765137615,
0.766972477,0.768807339,0.770642202,0.772477064,0.774311927,0.776146789,
0.777981651,0.779816514,0.781651376,0.783486239,0.785321101,0.787155963,
0.788990826,0.790825688,0.79266055,0.794495413,0.796330275,0.798165138,
0.8,0.801834862,0.803669725,0.805504587,0.80733945,0.809174312,0.811009174,
0.812844037,0.814678899,0.816513761,0.818348624,0.820183486,0.822018349,
0.823853211,0.825688073,0.827522936,0.829357798,0.831192661,0.833027523,
0.834862385,0.836697248,0.83853211,0.840366972,0.842201835,0.844036697,
0.84587156,0.847706422,0.849541284,0.851376147,0.853211009,0.855045872,
0.856880734,0.858715596,0.860550459,0.862385321,0.864220183,0.866055046,
0.867889908,0.869724771,0.871559633,0.873394495,0.875229358,0.87706422,
0.878899083,0.880733945,0.882568807,0.88440367,0.886238532,0.888073394,
0.889908257,0.891743119,0.893577982,0.895412844,0.897247706,0.899082569,
0.900917431,0.902752294,0.904587156,0.906422018,0.908256881,0.910091743,
0.911926606,0.913761468,0.91559633,0.917431193,0.919266055,0.921100917,
0.92293578,0.924770642,0.926605505,0.928440367,0.930275229,0.932110092,
0.933944954,0.935779817,0.937614679,0.939449541,0.941284404,0.943119266,
0.944954128,0.946788991,0.948623853,0.950458716,0.952293578,0.95412844,
0.955963303,0.957798165,0.959633028,0.96146789,0.963302752,0.965137615,
0.966972477,0.968807339,0.970642202,0.972477064,0.974311927,0.976146789,
0.977981651,0.979816514,0.981651376,0.983486239,0.985321101,0.987155963,
0.988990826,0.990825688,0.99266055,0.994495413,0.996330275,0.998165138,
1.),.UNSPECIFIED.);
#24459=B_SPLINE_CURVE_WITH_KNOTS('',3,(#270594,#270595,#270596,#270597,
#270598,#270599,#270600,#270601,#270602,#270603,#270604,#270605,#270606,
#270607,#270608,#270609,#270610,#270611,#270612,#270613,#270614,#270615,
#270616,#270617,#270618,#270619,#270620,#270621,#270622,#270623,#270624,
#270625,#270626,#270627,#270628,#270629,#270630,#270631,#270632,#270633,
#270634,#270635,#270636,#270637,#270638,#270639,#270640,#270641,#270642,
#270643,#270644,#270645,#270646,#270647,#270648,#270649,#270650,#270651,
#270652,#270653,#270654,#270655,#270656,#270657,#270658,#270659,#270660,
#270661,#270662,#270663,#270664,#270665,#270666,#270667,#270668,#270669,
#270670,#270671,#270672,#270673,#270674,#270675,#270676,#270677,#270678,
#270679,#270680,#270681,#270682,#270683,#270684,#270685,#270686,#270687,
#270688,#270689,#270690,#270691,#270692,#270693,#270694,#270695,#270696,
#270697,#270698,#270699,#270700,#270701,#270702,#270703,#270704,#270705,
#270706,#270707,#270708,#270709,#270710,#270711,#270712,#270713,#270714,
#270715,#270716,#270717,#270718,#270719,#270720,#270721,#270722,#270723,
#270724,#270725,#270726,#270727,#270728,#270729,#270730,#270731,#270732,
#270733,#270734,#270735,#270736,#270737,#270738,#270739,#270740,#270741,
#270742,#270743,#270744,#270745,#270746,#270747,#270748,#270749,#270750,
#270751,#270752,#270753,#270754,#270755,#270756,#270757,#270758,#270759,
#270760,#270761,#270762,#270763,#270764,#270765,#270766,#270767,#270768,
#270769,#270770,#270771,#270772,#270773,#270774,#270775,#270776,#270777,
#270778,#270779,#270780,#270781,#270782,#270783,#270784,#270785,#270786,
#270787,#270788,#270789,#270790,#270791,#270792,#270793,#270794,#270795,
#270796,#270797,#270798,#270799,#270800,#270801,#270802,#270803,#270804,
#270805,#270806,#270807,#270808,#270809,#270810,#270811,#270812,#270813,
#270814,#270815,#270816,#270817,#270818,#270819,#270820,#270821,#270822,
#270823,#270824,#270825,#270826,#270827,#270828,#270829,#270830,#270831,
#270832,#270833,#270834,#270835,#270836,#270837,#270838,#270839,#270840,
#270841,#270842,#270843,#270844,#270845,#270846,#270847,#270848,#270849,
#270850,#270851,#270852,#270853,#270854,#270855,#270856,#270857,#270858,
#270859,#270860,#270861,#270862,#270863,#270864,#270865,#270866,#270867,
#270868,#270869,#270870,#270871,#270872,#270873,#270874,#270875,#270876,
#270877,#270878,#270879,#270880,#270881,#270882,#270883,#270884,#270885,
#270886,#270887,#270888,#270889,#270890,#270891,#270892,#270893,#270894,
#270895,#270896,#270897,#270898,#270899,#270900,#270901,#270902,#270903,
#270904,#270905,#270906,#270907,#270908,#270909,#270910,#270911,#270912,
#270913,#270914,#270915),.UNSPECIFIED.,.F.,.F.,(4,3,3,3,3,3,3,3,3,3,3,3,
3,3,3,3,3,3,3,3,3,3,3,3,3,3,3,3,3,3,3,3,3,3,3,3,3,3,3,3,3,3,3,3,3,3,3,3,
3,3,3,3,3,3,3,3,3,3,3,3,3,3,3,3,3,3,3,3,3,3,3,3,3,3,3,3,3,3,3,3,3,3,3,3,
3,3,3,3,3,3,3,3,3,3,3,3,3,3,3,3,3,3,3,3,3,3,3,4),(-1.,-0.994495413,-0.988990826,
-0.983486239,-0.977981651,-0.972477064,-0.966972477,-0.957798165,-0.952293578,
-0.946788991,-0.941284404,-0.935779817,-0.930275229,-0.92293578,-0.917431193,
-0.910091743,-0.904587156,-0.899082569,-0.893577982,-0.888073394,-0.882568807,
-0.87706422,-0.871559633,-0.866055046,-0.860550459,-0.855045872,-0.849541284,
-0.844036697,-0.83853211,-0.833027523,-0.827522936,-0.822018349,-0.816513761,
-0.811009174,-0.803669725,-0.796330275,-0.788990826,-0.779816514,-0.772477064,
-0.765137615,-0.757798165,-0.746788991,-0.739449541,-0.732110092,-0.724770642,
-0.717431193,-0.710091743,-0.702752294,-0.695412844,-0.688073394,-0.678899083,
-0.671559633,-0.664220183,-0.656880734,-0.649541284,-0.642201835,-0.633027523,
-0.625688073,-0.618348624,-0.611009174,-0.603669725,-0.596330275,-0.588990826,
-0.579816514,-0.572477064,-0.565137615,-0.557798165,-0.550458716,-0.543119266,
-0.535779817,-0.528440367,-0.519266055,-0.510091743,-0.500917431,-0.491743119,
-0.482568807,-0.473394495,-0.464220183,-0.455045872,-0.44587156,-0.436697248,
-0.427522936,-0.418348624,-0.409174312,-0.4,-0.390825688,-0.379816514,-0.368807339,
-0.357798165,-0.346788991,-0.335779817,-0.324770642,-0.313761468,-0.302752294,
-0.291743119,-0.278899083,-0.267889908,-0.256880734,-0.24587156,-0.234862385,
-0.223853211,-0.212844037,-0.201834862,-0.190825688,-0.179816514,-0.168807339,
-0.157798165,-0.143172102),.UNSPECIFIED.);
#24460=B_SPLINE_CURVE_WITH_KNOTS('',3,(#270916,#270917,#270918,#270919,
#270920,#270921,#270922,#270923,#270924,#270925,#270926,#270927,#270928,
#270929,#270930,#270931,#270932,#270933,#270934,#270935,#270936,#270937,
#270938,#270939,#270940,#270941,#270942,#270943,#270944,#270945,#270946,
#270947,#270948,#270949,#270950,#270951,#270952,#270953,#270954,#270955,
#270956,#270957,#270958,#270959,#270960,#270961,#270962,#270963,#270964,
#270965,#270966,#270967,#270968,#270969,#270970,#270971,#270972,#270973,
#270974,#270975,#270976,#270977,#270978,#270979,#270980,#270981,#270982,
#270983,#270984,#270985,#270986,#270987,#270988,#270989,#270990,#270991,
#270992,#270993,#270994,#270995,#270996,#270997,#270998,#270999,#271000,
#271001,#271002,#271003,#271004,#271005,#271006,#271007,#271008,#271009,
#271010,#271011,#271012,#271013,#271014,#271015,#271016,#271017,#271018,
#271019,#271020,#271021,#271022,#271023,#271024,#271025,#271026,#271027,
#271028,#271029,#271030,#271031,#271032,#271033,#271034,#271035,#271036,
#271037,#271038,#271039,#271040,#271041,#271042,#271043,#271044,#271045,
#271046,#271047,#271048,#271049,#271050,#271051,#271052,#271053,#271054,
#271055,#271056,#271057,#271058,#271059,#271060,#271061,#271062,#271063,
#271064,#271065,#271066,#271067,#271068,#271069,#271070,#271071,#271072,
#271073,#271074,#271075,#271076,#271077,#271078,#271079,#271080,#271081,
#271082,#271083,#271084,#271085,#271086,#271087,#271088,#271089,#271090,
#271091,#271092,#271093,#271094,#271095,#271096,#271097,#271098,#271099,
#271100,#271101,#271102,#271103,#271104,#271105,#271106,#271107,#271108,
#271109,#271110,#271111,#271112,#271113,#271114,#271115,#271116,#271117,
#271118,#271119,#271120,#271121,#271122,#271123,#271124,#271125,#271126,
#271127,#271128,#271129,#271130,#271131,#271132,#271133,#271134,#271135,
#271136,#271137,#271138,#271139,#271140,#271141,#271142,#271143,#271144,
#271145,#271146,#271147,#271148,#271149,#271150,#271151,#271152,#271153,
#271154,#271155,#271156,#271157,#271158,#271159,#271160,#271161,#271162,
#271163,#271164,#271165,#271166,#271167,#271168,#271169,#271170,#271171,
#271172,#271173,#271174,#271175,#271176,#271177,#271178,#271179,#271180,
#271181,#271182,#271183,#271184,#271185,#271186,#271187,#271188,#271189,
#271190,#271191,#271192,#271193,#271194,#271195,#271196,#271197,#271198,
#271199,#271200,#271201,#271202,#271203,#271204,#271205,#271206,#271207,
#271208,#271209,#271210,#271211,#271212,#271213,#271214,#271215,#271216,
#271217,#271218,#271219,#271220,#271221,#271222,#271223,#271224,#271225,
#271226,#271227,#271228,#271229,#271230,#271231,#271232,#271233,#271234),
 .UNSPECIFIED.,.F.,.F.,(4,3,3,3,3,3,3,3,3,3,3,3,3,3,3,3,3,3,3,3,3,3,3,3,
3,3,3,3,3,3,3,3,3,3,3,3,3,3,3,3,3,3,3,3,3,3,3,3,3,3,3,3,3,3,3,3,3,3,3,3,
3,3,3,3,3,3,3,3,3,3,3,3,3,3,3,3,3,3,3,3,3,3,3,3,3,3,3,3,3,3,3,3,3,3,3,3,
3,3,3,3,3,3,3,3,3,3,4),(0.143172102,0.15412844,0.165137615,0.176146789,
0.187155963,0.198165138,0.209174312,0.220183486,0.231192661,0.242201835,
0.255045872,0.266055046,0.27706422,0.288073394,0.299082569,0.310091743,
0.321100917,0.332110092,0.343119266,0.35412844,0.366972477,0.377981651,
0.388990826,0.398165138,0.40733945,0.416513761,0.425688073,0.434862385,
0.44587156,0.455045872,0.464220183,0.473394495,0.482568807,0.491743119,
0.502752294,0.511926606,0.521100917,0.530275229,0.537614679,0.544954128,
0.552293578,0.559633028,0.566972477,0.574311927,0.581651376,0.588990826,
0.596330275,0.603669725,0.611009174,0.618348624,0.625688073,0.633027523,
0.640366972,0.647706422,0.655045872,0.662385321,0.669724771,0.67706422,
0.68440367,0.691743119,0.700917431,0.708256881,0.71559633,0.724770642,0.732110092,
0.739449541,0.748623853,0.755963303,0.763302752,0.772477064,0.779816514,
0.787155963,0.796330275,0.805504587,0.812844037,0.818348624,0.823853211,
0.829357798,0.834862385,0.840366972,0.84587156,0.853211009,0.858715596,
0.864220183,0.869724771,0.87706422,0.882568807,0.888073394,0.893577982,
0.899082569,0.906422018,0.911926606,0.919266055,0.924770642,0.930275229,
0.935779817,0.941284404,0.946788991,0.952293578,0.957798165,0.963302752,
0.968807339,0.974311927,0.979816514,0.985321101,0.990825688,1.),
 .UNSPECIFIED.);
#24461=B_SPLINE_CURVE_WITH_KNOTS('',3,(#272179,#272180,#272181,#272182,
#272183,#272184,#272185,#272186,#272187,#272188,#272189,#272190,#272191,
#272192,#272193,#272194,#272195,#272196,#272197,#272198,#272199,#272200,
#272201,#272202,#272203,#272204,#272205,#272206,#272207,#272208,#272209,
#272210,#272211,#272212,#272213,#272214,#272215,#272216,#272217,#272218,
#272219,#272220,#272221,#272222,#272223,#272224,#272225,#272226,#272227,
#272228,#272229,#272230,#272231,#272232,#272233,#272234,#272235,#272236,
#272237,#272238,#272239,#272240,#272241,#272242,#272243,#272244,#272245,
#272246,#272247,#272248,#272249,#272250,#272251,#272252,#272253,#272254,
#272255,#272256,#272257,#272258,#272259,#272260,#272261,#272262,#272263,
#272264,#272265,#272266,#272267,#272268,#272269,#272270,#272271,#272272,
#272273,#272274,#272275,#272276,#272277,#272278,#272279,#272280,#272281,
#272282,#272283,#272284,#272285,#272286,#272287,#272288,#272289,#272290,
#272291,#272292,#272293,#272294,#272295,#272296,#272297,#272298,#272299,
#272300,#272301,#272302,#272303,#272304,#272305,#272306,#272307,#272308,
#272309,#272310,#272311,#272312,#272313,#272314,#272315,#272316,#272317,
#272318,#272319,#272320,#272321,#272322,#272323,#272324,#272325,#272326,
#272327,#272328,#272329,#272330,#272331,#272332,#272333,#272334,#272335,
#272336,#272337,#272338,#272339,#272340,#272341,#272342,#272343,#272344,
#272345,#272346,#272347,#272348,#272349,#272350,#272351,#272352,#272353,
#272354,#272355,#272356,#272357,#272358,#272359,#272360,#272361,#272362,
#272363,#272364,#272365,#272366,#272367,#272368,#272369,#272370,#272371,
#272372,#272373,#272374,#272375,#272376,#272377,#272378,#272379,#272380,
#272381,#272382,#272383,#272384,#272385,#272386,#272387,#272388,#272389,
#272390,#272391,#272392,#272393,#272394,#272395,#272396,#272397,#272398,
#272399,#272400,#272401,#272402,#272403,#272404,#272405,#272406,#272407,
#272408,#272409,#272410,#272411,#272412,#272413,#272414,#272415,#272416,
#272417,#272418,#272419,#272420,#272421,#272422,#272423,#272424,#272425,
#272426,#272427,#272428,#272429,#272430,#272431,#272432,#272433,#272434,
#272435,#272436,#272437,#272438,#272439,#272440,#272441,#272442,#272443,
#272444,#272445,#272446,#272447,#272448,#272449,#272450,#272451,#272452,
#272453,#272454,#272455,#272456,#272457,#272458,#272459,#272460,#272461,
#272462,#272463,#272464,#272465,#272466,#272467,#272468,#272469,#272470,
#272471,#272472,#272473,#272474,#272475,#272476,#272477,#272478,#272479,
#272480,#272481,#272482,#272483,#272484,#272485,#272486,#272487,#272488,
#272489,#272490,#272491,#272492,#272493,#272494,#272495,#272496,#272497,
#272498,#272499,#272500,#272501,#272502,#272503),.UNSPECIFIED.,.F.,.F.,
(4,3,3,3,3,3,3,3,3,3,3,3,3,3,3,3,3,3,3,3,3,3,3,3,3,3,3,3,3,3,3,3,3,3,3,
3,3,3,3,3,3,3,3,3,3,3,3,3,3,3,3,3,3,3,3,3,3,3,3,3,3,3,3,3,3,3,3,3,3,3,3,
3,3,3,3,3,3,3,3,3,3,3,3,3,3,3,3,3,3,3,3,3,3,3,3,3,3,3,3,3,3,3,3,3,3,3,3,
3,4),(0.143172102,0.15412844,0.165137615,0.176146789,0.187155963,0.198165138,
0.209174312,0.220183486,0.231192661,0.242201835,0.253211009,0.264220183,
0.275229358,0.286238532,0.297247706,0.308256881,0.319266055,0.330275229,
0.341284404,0.352293578,0.363302752,0.374311927,0.385321101,0.396330275,
0.405504587,0.414678899,0.423853211,0.433027523,0.442201835,0.451376147,
0.460550459,0.469724771,0.478899083,0.488073394,0.497247706,0.506422018,
0.51559633,0.524770642,0.535779817,0.543119266,0.550458716,0.557798165,
0.565137615,0.572477064,0.579816514,0.587155963,0.594495413,0.601834862,
0.611009174,0.618348624,0.625688073,0.633027523,0.640366972,0.647706422,
0.655045872,0.662385321,0.669724771,0.67706422,0.68440367,0.691743119,0.699082569,
0.706422018,0.713761468,0.721100917,0.728440367,0.735779817,0.743119266,
0.750458716,0.757798165,0.765137615,0.772477064,0.779816514,0.787155963,
0.794495413,0.801834862,0.809174312,0.816513761,0.822018349,0.827522936,
0.833027523,0.83853211,0.84587156,0.851376147,0.856880734,0.862385321,0.867889908,
0.873394495,0.878899083,0.88440367,0.889908257,0.895412844,0.900917431,
0.906422018,0.911926606,0.917431193,0.92293578,0.928440367,0.933944954,
0.941284404,0.946788991,0.952293578,0.959633028,0.966972477,0.972477064,
0.977981651,0.983486239,0.988990826,0.994495413,1.),.UNSPECIFIED.);
#24462=B_SPLINE_CURVE_WITH_KNOTS('',3,(#272504,#272505,#272506,#272507,
#272508,#272509,#272510,#272511,#272512,#272513,#272514,#272515,#272516,
#272517,#272518,#272519,#272520,#272521,#272522,#272523,#272524,#272525,
#272526,#272527,#272528,#272529,#272530,#272531,#272532,#272533,#272534,
#272535,#272536,#272537,#272538,#272539,#272540,#272541,#272542,#272543,
#272544,#272545,#272546,#272547,#272548,#272549,#272550,#272551,#272552,
#272553,#272554,#272555,#272556,#272557,#272558,#272559,#272560,#272561,
#272562,#272563,#272564,#272565,#272566,#272567,#272568,#272569,#272570,
#272571,#272572,#272573,#272574,#272575,#272576,#272577,#272578,#272579,
#272580,#272581,#272582,#272583,#272584,#272585,#272586,#272587,#272588,
#272589,#272590,#272591,#272592,#272593,#272594,#272595,#272596,#272597,
#272598,#272599,#272600,#272601,#272602,#272603,#272604,#272605,#272606,
#272607,#272608,#272609,#272610,#272611,#272612,#272613,#272614,#272615,
#272616,#272617,#272618,#272619,#272620,#272621,#272622,#272623,#272624,
#272625,#272626,#272627,#272628,#272629,#272630,#272631,#272632,#272633,
#272634,#272635,#272636,#272637,#272638,#272639,#272640,#272641,#272642,
#272643,#272644,#272645,#272646,#272647,#272648,#272649,#272650,#272651,
#272652,#272653,#272654,#272655,#272656,#272657,#272658,#272659,#272660,
#272661,#272662,#272663,#272664,#272665,#272666,#272667,#272668,#272669,
#272670,#272671,#272672,#272673,#272674,#272675,#272676,#272677,#272678,
#272679,#272680,#272681,#272682,#272683,#272684,#272685,#272686,#272687,
#272688,#272689,#272690,#272691,#272692,#272693,#272694,#272695,#272696,
#272697,#272698,#272699,#272700,#272701,#272702,#272703,#272704,#272705,
#272706,#272707,#272708,#272709,#272710,#272711,#272712,#272713,#272714,
#272715,#272716,#272717,#272718,#272719,#272720,#272721,#272722,#272723,
#272724,#272725,#272726,#272727,#272728,#272729,#272730,#272731,#272732,
#272733,#272734,#272735,#272736,#272737,#272738,#272739,#272740,#272741,
#272742,#272743,#272744,#272745,#272746,#272747,#272748,#272749,#272750,
#272751,#272752,#272753,#272754,#272755,#272756,#272757,#272758,#272759,
#272760,#272761,#272762,#272763,#272764,#272765,#272766,#272767,#272768,
#272769,#272770,#272771,#272772,#272773,#272774,#272775,#272776,#272777,
#272778,#272779,#272780,#272781,#272782,#272783,#272784,#272785,#272786,
#272787,#272788,#272789,#272790,#272791,#272792,#272793,#272794,#272795,
#272796,#272797,#272798,#272799,#272800,#272801,#272802,#272803,#272804,
#272805,#272806,#272807,#272808,#272809,#272810,#272811,#272812,#272813,
#272814,#272815,#272816,#272817,#272818,#272819,#272820,#272821,#272822,
#272823,#272824,#272825,#272826,#272827,#272828),.UNSPECIFIED.,.F.,.F.,
(4,3,3,3,3,3,3,3,3,3,3,3,3,3,3,3,3,3,3,3,3,3,3,3,3,3,3,3,3,3,3,3,3,3,3,
3,3,3,3,3,3,3,3,3,3,3,3,3,3,3,3,3,3,3,3,3,3,3,3,3,3,3,3,3,3,3,3,3,3,3,3,
3,3,3,3,3,3,3,3,3,3,3,3,3,3,3,3,3,3,3,3,3,3,3,3,3,3,3,3,3,3,3,3,3,3,3,3,
3,4),(0.143172102,0.15412844,0.165137615,0.176146789,0.187155963,0.198165138,
0.209174312,0.220183486,0.231192661,0.242201835,0.253211009,0.264220183,
0.275229358,0.286238532,0.297247706,0.308256881,0.319266055,0.330275229,
0.341284404,0.352293578,0.363302752,0.374311927,0.385321101,0.396330275,
0.405504587,0.414678899,0.423853211,0.433027523,0.442201835,0.451376147,
0.460550459,0.469724771,0.478899083,0.488073394,0.499082569,0.508256881,
0.517431193,0.526605505,0.533944954,0.543119266,0.550458716,0.557798165,
0.565137615,0.572477064,0.579816514,0.587155963,0.594495413,0.601834862,
0.609174312,0.616513761,0.623853211,0.631192661,0.63853211,0.64587156,0.653211009,
0.660550459,0.667889908,0.675229358,0.682568807,0.689908257,0.697247706,
0.704587156,0.711926606,0.719266055,0.726605505,0.733944954,0.743119266,
0.750458716,0.757798165,0.765137615,0.772477064,0.779816514,0.787155963,
0.794495413,0.801834862,0.809174312,0.816513761,0.822018349,0.827522936,
0.833027523,0.83853211,0.844036697,0.849541284,0.855045872,0.860550459,
0.866055046,0.871559633,0.87706422,0.882568807,0.888073394,0.893577982,
0.900917431,0.906422018,0.911926606,0.921100917,0.926605505,0.932110092,
0.937614679,0.943119266,0.948623853,0.95412844,0.959633028,0.966972477,
0.972477064,0.977981651,0.983486239,0.988990826,0.994495413,1.),
 .UNSPECIFIED.);
#24463=B_SPLINE_CURVE_WITH_KNOTS('',3,(#273788,#273789,#273790,#273791,
#273792,#273793,#273794,#273795,#273796,#273797,#273798,#273799,#273800,
#273801,#273802,#273803,#273804,#273805,#273806,#273807,#273808,#273809,
#273810,#273811,#273812,#273813,#273814,#273815,#273816,#273817,#273818,
#273819,#273820,#273821,#273822,#273823,#273824,#273825,#273826,#273827,
#273828,#273829,#273830,#273831,#273832,#273833,#273834,#273835,#273836,
#273837,#273838,#273839,#273840,#273841,#273842,#273843,#273844,#273845,
#273846,#273847,#273848,#273849,#273850,#273851,#273852,#273853,#273854,
#273855,#273856,#273857,#273858,#273859,#273860,#273861,#273862,#273863,
#273864,#273865,#273866,#273867,#273868,#273869,#273870,#273871,#273872,
#273873,#273874,#273875,#273876,#273877,#273878,#273879,#273880,#273881,
#273882,#273883,#273884,#273885,#273886,#273887,#273888,#273889,#273890,
#273891,#273892,#273893,#273894,#273895,#273896,#273897,#273898,#273899,
#273900,#273901,#273902,#273903,#273904,#273905,#273906,#273907,#273908,
#273909,#273910,#273911,#273912,#273913,#273914,#273915,#273916,#273917,
#273918,#273919,#273920,#273921,#273922,#273923,#273924,#273925,#273926,
#273927,#273928,#273929,#273930,#273931,#273932,#273933,#273934,#273935,
#273936,#273937,#273938,#273939,#273940,#273941,#273942,#273943,#273944,
#273945,#273946,#273947,#273948,#273949,#273950,#273951,#273952,#273953,
#273954,#273955,#273956,#273957,#273958,#273959,#273960,#273961,#273962,
#273963,#273964,#273965,#273966,#273967,#273968,#273969,#273970,#273971,
#273972,#273973,#273974,#273975,#273976,#273977,#273978,#273979,#273980,
#273981,#273982,#273983,#273984,#273985,#273986,#273987,#273988,#273989,
#273990,#273991,#273992,#273993,#273994,#273995,#273996,#273997,#273998,
#273999,#274000,#274001,#274002,#274003,#274004,#274005,#274006,#274007,
#274008,#274009,#274010,#274011,#274012,#274013,#274014,#274015,#274016,
#274017,#274018,#274019,#274020,#274021,#274022,#274023,#274024,#274025,
#274026,#274027,#274028,#274029,#274030,#274031,#274032,#274033,#274034,
#274035,#274036,#274037,#274038,#274039,#274040,#274041,#274042,#274043,
#274044,#274045,#274046,#274047,#274048,#274049,#274050,#274051,#274052,
#274053,#274054,#274055,#274056,#274057,#274058,#274059,#274060,#274061,
#274062,#274063,#274064,#274065,#274066,#274067,#274068,#274069,#274070,
#274071,#274072,#274073,#274074,#274075,#274076,#274077,#274078,#274079,
#274080,#274081,#274082,#274083,#274084,#274085,#274086,#274087,#274088,
#274089,#274090,#274091,#274092,#274093,#274094,#274095,#274096,#274097,
#274098,#274099,#274100,#274101,#274102,#274103,#274104,#274105,#274106,
#274107,#274108,#274109,#274110,#274111,#274112),.UNSPECIFIED.,.F.,.F.,
(4,3,3,3,3,3,3,3,3,3,3,3,3,3,3,3,3,3,3,3,3,3,3,3,3,3,3,3,3,3,3,3,3,3,3,
3,3,3,3,3,3,3,3,3,3,3,3,3,3,3,3,3,3,3,3,3,3,3,3,3,3,3,3,3,3,3,3,3,3,3,3,
3,3,3,3,3,3,3,3,3,3,3,3,3,3,3,3,3,3,3,3,3,3,3,3,3,3,3,3,3,3,3,3,3,3,3,3,
3,4),(0.143172102,0.15412844,0.165137615,0.176146789,0.187155963,0.198165138,
0.209174312,0.220183486,0.231192661,0.242201835,0.253211009,0.264220183,
0.275229358,0.286238532,0.297247706,0.308256881,0.319266055,0.330275229,
0.341284404,0.352293578,0.363302752,0.374311927,0.385321101,0.396330275,
0.405504587,0.414678899,0.423853211,0.433027523,0.442201835,0.451376147,
0.460550459,0.469724771,0.478899083,0.488073394,0.497247706,0.506422018,
0.517431193,0.526605505,0.533944954,0.541284404,0.548623853,0.555963303,
0.563302752,0.570642202,0.577981651,0.585321101,0.59266055,0.6,0.60733945,
0.614678899,0.622018349,0.629357798,0.636697248,0.64587156,0.655045872,
0.662385321,0.669724771,0.67706422,0.68440367,0.691743119,0.699082569,0.706422018,
0.713761468,0.721100917,0.728440367,0.735779817,0.743119266,0.750458716,
0.757798165,0.765137615,0.774311927,0.781651376,0.788990826,0.796330275,
0.803669725,0.811009174,0.816513761,0.822018349,0.827522936,0.833027523,
0.83853211,0.844036697,0.849541284,0.855045872,0.860550459,0.869724771,
0.875229358,0.880733945,0.886238532,0.891743119,0.897247706,0.902752294,
0.908256881,0.913761468,0.919266055,0.926605505,0.932110092,0.937614679,
0.943119266,0.948623853,0.95412844,0.959633028,0.966972477,0.972477064,
0.977981651,0.983486239,0.988990826,0.994495413,1.),.UNSPECIFIED.);
#24464=B_SPLINE_CURVE_WITH_KNOTS('',3,(#274113,#274114,#274115,#274116,
#274117,#274118,#274119,#274120,#274121,#274122,#274123,#274124,#274125,
#274126,#274127,#274128,#274129,#274130,#274131,#274132,#274133,#274134,
#274135,#274136,#274137,#274138,#274139,#274140,#274141,#274142,#274143,
#274144,#274145,#274146,#274147,#274148,#274149,#274150,#274151,#274152,
#274153,#274154,#274155,#274156,#274157,#274158,#274159,#274160,#274161,
#274162,#274163,#274164,#274165,#274166,#274167,#274168,#274169,#274170,
#274171,#274172,#274173,#274174,#274175,#274176,#274177,#274178,#274179,
#274180,#274181,#274182,#274183,#274184,#274185,#274186,#274187,#274188,
#274189,#274190,#274191,#274192,#274193,#274194,#274195,#274196,#274197,
#274198,#274199,#274200,#274201,#274202,#274203,#274204,#274205,#274206,
#274207,#274208,#274209,#274210,#274211,#274212,#274213,#274214,#274215,
#274216,#274217,#274218,#274219,#274220,#274221,#274222,#274223,#274224,
#274225,#274226,#274227,#274228,#274229,#274230,#274231,#274232,#274233,
#274234,#274235,#274236,#274237,#274238,#274239,#274240,#274241,#274242,
#274243,#274244,#274245,#274246,#274247,#274248,#274249,#274250,#274251,
#274252,#274253,#274254,#274255,#274256,#274257,#274258,#274259,#274260,
#274261,#274262,#274263,#274264,#274265,#274266,#274267,#274268,#274269,
#274270,#274271,#274272,#274273,#274274,#274275,#274276,#274277,#274278,
#274279,#274280,#274281,#274282,#274283,#274284,#274285,#274286,#274287,
#274288,#274289,#274290,#274291,#274292,#274293,#274294,#274295,#274296,
#274297,#274298,#274299,#274300,#274301,#274302,#274303,#274304,#274305,
#274306,#274307,#274308,#274309,#274310,#274311,#274312,#274313,#274314,
#274315,#274316,#274317,#274318,#274319,#274320,#274321,#274322,#274323,
#274324,#274325,#274326,#274327,#274328,#274329,#274330,#274331,#274332,
#274333,#274334,#274335,#274336,#274337,#274338,#274339,#274340,#274341,
#274342,#274343,#274344,#274345,#274346,#274347,#274348,#274349,#274350,
#274351,#274352,#274353,#274354,#274355,#274356,#274357,#274358,#274359,
#274360,#274361,#274362,#274363,#274364,#274365,#274366,#274367,#274368,
#274369,#274370,#274371,#274372,#274373,#274374,#274375,#274376,#274377,
#274378,#274379,#274380,#274381,#274382,#274383,#274384,#274385,#274386,
#274387,#274388,#274389,#274390,#274391,#274392,#274393,#274394,#274395,
#274396,#274397,#274398,#274399,#274400,#274401,#274402,#274403,#274404,
#274405,#274406,#274407,#274408,#274409,#274410,#274411,#274412,#274413,
#274414,#274415,#274416,#274417,#274418,#274419,#274420,#274421,#274422,
#274423,#274424,#274425,#274426,#274427,#274428,#274429,#274430,#274431,
#274432,#274433,#274434,#274435,#274436,#274437),.UNSPECIFIED.,.F.,.F.,
(4,3,3,3,3,3,3,3,3,3,3,3,3,3,3,3,3,3,3,3,3,3,3,3,3,3,3,3,3,3,3,3,3,3,3,
3,3,3,3,3,3,3,3,3,3,3,3,3,3,3,3,3,3,3,3,3,3,3,3,3,3,3,3,3,3,3,3,3,3,3,3,
3,3,3,3,3,3,3,3,3,3,3,3,3,3,3,3,3,3,3,3,3,3,3,3,3,3,3,3,3,3,3,3,3,3,3,3,
3,4),(0.143172102,0.15412844,0.165137615,0.176146789,0.187155963,0.198165138,
0.209174312,0.220183486,0.231192661,0.242201835,0.253211009,0.264220183,
0.275229358,0.286238532,0.297247706,0.308256881,0.319266055,0.330275229,
0.341284404,0.352293578,0.363302752,0.374311927,0.385321101,0.396330275,
0.405504587,0.414678899,0.423853211,0.433027523,0.442201835,0.451376147,
0.460550459,0.469724771,0.478899083,0.488073394,0.497247706,0.506422018,
0.51559633,0.524770642,0.533944954,0.541284404,0.548623853,0.555963303,
0.563302752,0.570642202,0.577981651,0.585321101,0.59266055,0.6,0.60733945,
0.614678899,0.622018349,0.629357798,0.636697248,0.644036697,0.651376147,
0.658715596,0.666055046,0.673394495,0.680733945,0.688073394,0.695412844,
0.706422018,0.713761468,0.721100917,0.728440367,0.735779817,0.743119266,
0.750458716,0.757798165,0.766972477,0.774311927,0.781651376,0.788990826,
0.796330275,0.803669725,0.811009174,0.816513761,0.822018349,0.827522936,
0.833027523,0.83853211,0.844036697,0.849541284,0.855045872,0.860550459,
0.869724771,0.875229358,0.880733945,0.886238532,0.891743119,0.897247706,
0.902752294,0.908256881,0.913761468,0.921100917,0.926605505,0.932110092,
0.937614679,0.943119266,0.948623853,0.95412844,0.959633028,0.966972477,
0.972477064,0.977981651,0.983486239,0.988990826,0.994495413,1.),
 .UNSPECIFIED.);
#24465=B_SPLINE_CURVE_WITH_KNOTS('',3,(#275385,#275386,#275387,#275388,
#275389,#275390,#275391,#275392,#275393,#275394,#275395,#275396,#275397,
#275398,#275399,#275400,#275401,#275402,#275403,#275404,#275405,#275406,
#275407,#275408,#275409,#275410,#275411,#275412,#275413,#275414,#275415,
#275416,#275417,#275418,#275419,#275420,#275421,#275422,#275423,#275424,
#275425,#275426,#275427,#275428,#275429,#275430,#275431,#275432,#275433,
#275434,#275435,#275436,#275437,#275438,#275439,#275440,#275441,#275442,
#275443,#275444,#275445,#275446,#275447,#275448,#275449,#275450,#275451,
#275452,#275453,#275454,#275455,#275456,#275457,#275458,#275459,#275460,
#275461,#275462,#275463,#275464,#275465,#275466,#275467,#275468,#275469,
#275470,#275471,#275472,#275473,#275474,#275475,#275476,#275477,#275478,
#275479,#275480,#275481,#275482,#275483,#275484,#275485,#275486,#275487,
#275488,#275489,#275490,#275491,#275492,#275493,#275494,#275495,#275496,
#275497,#275498,#275499,#275500,#275501,#275502,#275503,#275504,#275505,
#275506,#275507,#275508,#275509,#275510,#275511,#275512,#275513,#275514,
#275515,#275516,#275517,#275518,#275519,#275520,#275521,#275522,#275523,
#275524,#275525,#275526,#275527,#275528,#275529,#275530,#275531,#275532,
#275533,#275534,#275535,#275536,#275537,#275538,#275539,#275540,#275541,
#275542,#275543,#275544,#275545,#275546,#275547,#275548,#275549,#275550,
#275551,#275552,#275553,#275554,#275555,#275556,#275557,#275558,#275559,
#275560,#275561,#275562,#275563,#275564,#275565,#275566,#275567,#275568,
#275569,#275570,#275571,#275572,#275573,#275574,#275575,#275576,#275577,
#275578,#275579,#275580,#275581,#275582,#275583,#275584,#275585,#275586,
#275587,#275588,#275589,#275590,#275591,#275592,#275593,#275594,#275595,
#275596,#275597,#275598,#275599,#275600,#275601,#275602,#275603,#275604,
#275605,#275606,#275607,#275608,#275609,#275610,#275611,#275612,#275613,
#275614,#275615,#275616,#275617,#275618,#275619,#275620,#275621,#275622,
#275623,#275624,#275625,#275626,#275627,#275628,#275629,#275630,#275631,
#275632,#275633,#275634,#275635,#275636,#275637,#275638,#275639,#275640,
#275641,#275642,#275643,#275644,#275645,#275646,#275647,#275648,#275649,
#275650,#275651,#275652,#275653,#275654,#275655,#275656,#275657,#275658,
#275659,#275660,#275661,#275662,#275663,#275664,#275665,#275666,#275667,
#275668,#275669,#275670,#275671,#275672,#275673,#275674,#275675,#275676,
#275677,#275678,#275679,#275680,#275681,#275682,#275683,#275684,#275685,
#275686,#275687,#275688,#275689,#275690,#275691,#275692,#275693,#275694,
#275695,#275696,#275697,#275698,#275699,#275700,#275701,#275702,#275703,
#275704,#275705,#275706,#275707,#275708,#275709),.UNSPECIFIED.,.F.,.F.,
(4,3,3,3,3,3,3,3,3,3,3,3,3,3,3,3,3,3,3,3,3,3,3,3,3,3,3,3,3,3,3,3,3,3,3,
3,3,3,3,3,3,3,3,3,3,3,3,3,3,3,3,3,3,3,3,3,3,3,3,3,3,3,3,3,3,3,3,3,3,3,3,
3,3,3,3,3,3,3,3,3,3,3,3,3,3,3,3,3,3,3,3,3,3,3,3,3,3,3,3,3,3,3,3,3,3,3,3,
3,4),(-1.,-0.99266055,-0.987155963,-0.981651376,-0.976146789,-0.970642202,
-0.965137615,-0.959633028,-0.95412844,-0.948623853,-0.943119266,-0.935779817,
-0.930275229,-0.924770642,-0.919266055,-0.913761468,-0.908256881,-0.900917431,
-0.895412844,-0.889908257,-0.88440367,-0.878899083,-0.873394495,-0.867889908,
-0.862385321,-0.856880734,-0.851376147,-0.84587156,-0.840366972,-0.834862385,
-0.829357798,-0.823853211,-0.818348624,-0.812844037,-0.80733945,-0.8,-0.79266055,
-0.781651376,-0.774311927,-0.766972477,-0.759633028,-0.752293578,-0.744954128,
-0.737614679,-0.730275229,-0.72293578,-0.711926606,-0.704587156,-0.697247706,
-0.689908257,-0.682568807,-0.673394495,-0.666055046,-0.658715596,-0.651376147,
-0.644036697,-0.636697248,-0.629357798,-0.622018349,-0.614678899,-0.60733945,
-0.6,-0.59266055,-0.585321101,-0.577981651,-0.570642202,-0.563302752,-0.555963303,
-0.548623853,-0.541284404,-0.533944954,-0.526605505,-0.517431193,-0.508256881,
-0.499082569,-0.489908257,-0.480733945,-0.471559633,-0.462385321,-0.453211009,
-0.444036697,-0.434862385,-0.425688073,-0.416513761,-0.40733945,-0.398165138,
-0.388990826,-0.377981651,-0.366972477,-0.355963303,-0.344954128,-0.333944954,
-0.32293578,-0.311926606,-0.300917431,-0.289908257,-0.278899083,-0.267889908,
-0.256880734,-0.24587156,-0.234862385,-0.223853211,-0.212844037,-0.201834862,
-0.190825688,-0.179816514,-0.168807339,-0.157798165,-0.143172102),
 .UNSPECIFIED.);
#24466=B_SPLINE_CURVE_WITH_KNOTS('',3,(#275710,#275711,#275712,#275713,
#275714,#275715,#275716,#275717,#275718,#275719,#275720,#275721,#275722,
#275723,#275724,#275725,#275726,#275727,#275728,#275729,#275730,#275731,
#275732,#275733,#275734,#275735,#275736,#275737,#275738,#275739,#275740,
#275741,#275742,#275743,#275744,#275745,#275746,#275747,#275748,#275749,
#275750,#275751,#275752,#275753,#275754,#275755,#275756,#275757,#275758,
#275759,#275760,#275761,#275762,#275763,#275764,#275765,#275766,#275767,
#275768,#275769,#275770,#275771,#275772,#275773,#275774,#275775,#275776,
#275777,#275778,#275779,#275780,#275781,#275782,#275783,#275784,#275785,
#275786,#275787,#275788,#275789,#275790,#275791,#275792,#275793,#275794,
#275795,#275796,#275797,#275798,#275799,#275800,#275801,#275802,#275803,
#275804,#275805,#275806,#275807,#275808,#275809,#275810,#275811,#275812,
#275813,#275814,#275815,#275816,#275817,#275818,#275819,#275820,#275821,
#275822,#275823,#275824,#275825,#275826,#275827,#275828,#275829,#275830,
#275831,#275832,#275833,#275834,#275835,#275836,#275837,#275838,#275839,
#275840,#275841,#275842,#275843,#275844,#275845,#275846,#275847,#275848,
#275849,#275850,#275851,#275852,#275853,#275854,#275855,#275856,#275857,
#275858,#275859,#275860,#275861,#275862,#275863,#275864,#275865,#275866,
#275867,#275868,#275869,#275870,#275871,#275872,#275873,#275874,#275875,
#275876,#275877,#275878,#275879,#275880,#275881,#275882,#275883,#275884,
#275885,#275886,#275887,#275888,#275889,#275890,#275891,#275892,#275893,
#275894,#275895,#275896,#275897,#275898,#275899,#275900,#275901,#275902,
#275903,#275904,#275905,#275906,#275907,#275908,#275909,#275910,#275911,
#275912,#275913,#275914,#275915,#275916,#275917,#275918,#275919,#275920,
#275921,#275922,#275923,#275924,#275925,#275926,#275927,#275928,#275929,
#275930,#275931,#275932,#275933,#275934,#275935,#275936,#275937,#275938,
#275939,#275940,#275941,#275942,#275943,#275944,#275945,#275946,#275947,
#275948,#275949,#275950,#275951,#275952,#275953,#275954,#275955,#275956,
#275957,#275958,#275959,#275960,#275961,#275962,#275963,#275964,#275965,
#275966,#275967,#275968,#275969,#275970,#275971,#275972,#275973,#275974,
#275975,#275976,#275977,#275978,#275979,#275980,#275981,#275982,#275983,
#275984,#275985,#275986,#275987,#275988,#275989,#275990,#275991,#275992,
#275993,#275994,#275995,#275996,#275997,#275998,#275999,#276000,#276001,
#276002,#276003,#276004,#276005,#276006,#276007,#276008,#276009,#276010,
#276011,#276012,#276013,#276014,#276015,#276016,#276017,#276018,#276019,
#276020,#276021,#276022,#276023,#276024,#276025,#276026,#276027,#276028,
#276029,#276030,#276031),.UNSPECIFIED.,.F.,.F.,(4,3,3,3,3,3,3,3,3,3,3,3,
3,3,3,3,3,3,3,3,3,3,3,3,3,3,3,3,3,3,3,3,3,3,3,3,3,3,3,3,3,3,3,3,3,3,3,3,
3,3,3,3,3,3,3,3,3,3,3,3,3,3,3,3,3,3,3,3,3,3,3,3,3,3,3,3,3,3,3,3,3,3,3,3,
3,3,3,3,3,3,3,3,3,3,3,3,3,3,3,3,3,3,3,3,3,3,3,4),(0.143172102,0.15412844,
0.165137615,0.176146789,0.187155963,0.198165138,0.209174312,0.220183486,
0.231192661,0.242201835,0.253211009,0.264220183,0.275229358,0.286238532,
0.297247706,0.308256881,0.319266055,0.330275229,0.341284404,0.352293578,
0.363302752,0.374311927,0.385321101,0.396330275,0.405504587,0.414678899,
0.423853211,0.433027523,0.442201835,0.451376147,0.460550459,0.469724771,
0.478899083,0.488073394,0.497247706,0.506422018,0.51559633,0.524770642,
0.533944954,0.543119266,0.552293578,0.559633028,0.566972477,0.574311927,
0.581651376,0.588990826,0.596330275,0.603669725,0.611009174,0.618348624,
0.625688073,0.633027523,0.640366972,0.647706422,0.655045872,0.662385321,
0.669724771,0.67706422,0.68440367,0.691743119,0.699082569,0.706422018,0.713761468,
0.721100917,0.728440367,0.737614679,0.744954128,0.752293578,0.759633028,
0.766972477,0.774311927,0.781651376,0.788990826,0.796330275,0.805504587,
0.812844037,0.818348624,0.823853211,0.829357798,0.834862385,0.840366972,
0.84587156,0.851376147,0.856880734,0.862385321,0.867889908,0.873394495,
0.878899083,0.886238532,0.891743119,0.897247706,0.902752294,0.910091743,
0.91559633,0.921100917,0.928440367,0.933944954,0.939449541,0.944954128,
0.950458716,0.957798165,0.963302752,0.968807339,0.974311927,0.979816514,
0.985321101,0.990825688,1.),.UNSPECIFIED.);
#24467=B_SPLINE_CURVE_WITH_KNOTS('',5,(#276994,#276995,#276996,#276997,
#276998,#276999,#277000,#277001,#277002,#277003,#277004,#277005,#277006,
#277007,#277008,#277009,#277010,#277011,#277012,#277013,#277014,#277015,
#277016,#277017,#277018,#277019,#277020,#277021,#277022,#277023,#277024,
#277025,#277026,#277027,#277028,#277029,#277030,#277031,#277032,#277033,
#277034,#277035,#277036,#277037,#277038,#277039,#277040,#277041,#277042,
#277043,#277044,#277045,#277046,#277047,#277048,#277049,#277050,#277051,
#277052,#277053,#277054,#277055,#277056,#277057,#277058,#277059,#277060,
#277061,#277062,#277063,#277064,#277065,#277066,#277067,#277068,#277069,
#277070,#277071,#277072,#277073,#277074,#277075,#277076,#277077,#277078,
#277079,#277080,#277081,#277082,#277083,#277084,#277085,#277086,#277087,
#277088,#277089,#277090,#277091,#277092,#277093,#277094,#277095,#277096,
#277097,#277098,#277099,#277100,#277101,#277102,#277103,#277104,#277105,
#277106,#277107,#277108,#277109,#277110,#277111,#277112,#277113,#277114,
#277115,#277116,#277117,#277118,#277119,#277120,#277121,#277122,#277123,
#277124,#277125,#277126,#277127,#277128,#277129,#277130,#277131,#277132,
#277133,#277134,#277135,#277136,#277137,#277138,#277139,#277140,#277141,
#277142,#277143,#277144,#277145,#277146,#277147,#277148,#277149,#277150,
#277151,#277152,#277153,#277154,#277155,#277156,#277157,#277158,#277159,
#277160,#277161,#277162,#277163,#277164,#277165,#277166,#277167,#277168,
#277169,#277170,#277171,#277172,#277173,#277174,#277175,#277176,#277177,
#277178,#277179,#277180,#277181,#277182,#277183,#277184,#277185,#277186,
#277187,#277188,#277189,#277190,#277191,#277192,#277193,#277194,#277195,
#277196,#277197,#277198,#277199,#277200,#277201,#277202,#277203,#277204,
#277205,#277206,#277207,#277208,#277209,#277210,#277211,#277212,#277213,
#277214,#277215,#277216,#277217,#277218,#277219,#277220,#277221,#277222,
#277223,#277224,#277225,#277226,#277227,#277228,#277229,#277230,#277231,
#277232,#277233,#277234,#277235,#277236,#277237,#277238,#277239,#277240,
#277241,#277242,#277243,#277244,#277245,#277246,#277247,#277248,#277249,
#277250,#277251,#277252,#277253,#277254,#277255,#277256,#277257,#277258,
#277259,#277260,#277261,#277262,#277263,#277264,#277265,#277266,#277267,
#277268,#277269,#277270,#277271,#277272,#277273,#277274,#277275,#277276,
#277277,#277278,#277279,#277280,#277281,#277282,#277283,#277284,#277285,
#277286,#277287,#277288,#277289,#277290,#277291,#277292,#277293,#277294,
#277295,#277296,#277297,#277298,#277299,#277300,#277301,#277302,#277303,
#277304,#277305,#277306,#277307,#277308,#277309,#277310,#277311,#277312,
#277313,#277314,#277315,#277316,#277317,#277318,#277319,#277320,#277321,
#277322,#277323,#277324,#277325,#277326,#277327,#277328,#277329,#277330,
#277331,#277332,#277333,#277334,#277335,#277336,#277337,#277338,#277339,
#277340,#277341,#277342,#277343,#277344,#277345,#277346,#277347,#277348,
#277349,#277350,#277351,#277352,#277353,#277354,#277355,#277356,#277357,
#277358,#277359,#277360,#277361,#277362,#277363,#277364,#277365,#277366,
#277367,#277368,#277369,#277370,#277371,#277372,#277373,#277374,#277375,
#277376,#277377,#277378,#277379,#277380,#277381,#277382,#277383,#277384,
#277385,#277386,#277387,#277388,#277389,#277390,#277391,#277392,#277393,
#277394,#277395,#277396,#277397,#277398,#277399,#277400,#277401,#277402,
#277403,#277404,#277405,#277406,#277407,#277408,#277409,#277410,#277411,
#277412,#277413,#277414,#277415,#277416,#277417,#277418,#277419,#277420,
#277421,#277422,#277423,#277424,#277425,#277426,#277427,#277428,#277429,
#277430,#277431,#277432,#277433,#277434,#277435,#277436,#277437,#277438,
#277439,#277440,#277441,#277442,#277443,#277444,#277445,#277446,#277447,
#277448,#277449,#277450,#277451,#277452,#277453,#277454,#277455,#277456,
#277457,#277458,#277459,#277460,#277461,#277462,#277463,#277464),
 .UNSPECIFIED.,.F.,.F.,(6,1,1,1,1,1,1,1,1,1,1,1,1,1,1,1,1,1,1,1,1,1,1,1,
1,1,1,1,1,1,1,1,1,1,1,1,1,1,1,1,1,1,1,1,1,1,1,1,1,1,1,1,1,1,1,1,1,1,1,1,
1,1,1,1,1,1,1,1,1,1,1,1,1,1,1,1,1,1,1,1,1,1,1,1,1,1,1,1,1,1,1,1,1,1,1,1,
1,1,1,1,1,1,1,1,1,1,1,1,1,1,1,1,1,1,1,1,1,1,1,1,1,1,1,1,1,1,1,1,1,1,1,1,
1,1,1,1,1,1,1,1,1,1,1,1,1,1,1,1,1,1,1,1,1,1,1,1,1,1,1,1,1,1,1,1,1,1,1,1,
1,1,1,1,1,1,1,1,1,1,1,1,1,1,1,1,1,1,1,1,1,1,1,1,1,1,1,1,1,1,1,1,1,1,1,1,
1,1,1,1,1,1,1,1,1,1,1,1,1,1,1,1,1,1,1,1,1,1,1,1,1,1,1,1,1,1,1,1,1,1,1,1,
1,1,1,1,1,1,1,1,1,1,1,1,1,1,1,1,1,1,1,1,1,1,1,1,1,1,1,1,1,1,1,1,1,1,1,1,
1,1,1,1,1,1,1,1,1,1,1,1,1,1,1,1,1,1,1,1,1,1,1,1,1,1,1,1,1,1,1,1,1,1,1,1,
1,1,1,1,1,1,1,1,1,1,1,1,1,1,1,1,1,1,1,1,1,1,1,1,1,1,1,1,1,1,1,1,1,1,1,1,
1,1,1,1,1,1,1,1,1,1,1,1,1,1,1,1,1,1,1,1,1,1,1,1,1,1,1,1,1,1,1,1,1,1,1,1,
1,1,1,1,1,1,1,1,1,1,1,1,1,1,1,1,1,1,1,1,1,1,1,1,1,1,1,1,1,1,1,1,1,1,1,1,
1,1,1,1,1,1,1,1,1,1,1,1,1,1,1,1,1,1,1,1,1,1,1,1,1,1,1,1,1,1,1,1,1,1,1,1,
1,1,1,1,1,1,1,1,1,1,6),(-1.,-0.998165138,-0.996330275,-0.994495413,-0.99266055,
-0.990825688,-0.988990826,-0.987155963,-0.985321101,-0.983486239,-0.981651376,
-0.979816514,-0.977981651,-0.976146789,-0.974311927,-0.972477064,-0.970642202,
-0.968807339,-0.966972477,-0.965137615,-0.963302752,-0.96146789,-0.959633028,
-0.957798165,-0.955963303,-0.95412844,-0.952293578,-0.950458716,-0.948623853,
-0.946788991,-0.944954128,-0.943119266,-0.941284404,-0.939449541,-0.937614679,
-0.935779817,-0.933944954,-0.932110092,-0.930275229,-0.928440367,-0.926605505,
-0.924770642,-0.92293578,-0.921100917,-0.919266055,-0.917431193,-0.91559633,
-0.913761468,-0.911926606,-0.910091743,-0.908256881,-0.906422018,-0.904587156,
-0.902752294,-0.900917431,-0.899082569,-0.897247706,-0.895412844,-0.893577982,
-0.889908257,-0.888073394,-0.886238532,-0.88440367,-0.882568807,-0.880733945,
-0.878899083,-0.87706422,-0.875229358,-0.873394495,-0.871559633,-0.869724771,
-0.867889908,-0.866055046,-0.864220183,-0.862385321,-0.860550459,-0.858715596,
-0.856880734,-0.855045872,-0.853211009,-0.851376147,-0.849541284,-0.847706422,
-0.84587156,-0.844036697,-0.842201835,-0.840366972,-0.83853211,-0.836697248,
-0.834862385,-0.833027523,-0.831192661,-0.829357798,-0.827522936,-0.825688073,
-0.823853211,-0.822018349,-0.820183486,-0.818348624,-0.816513761,-0.814678899,
-0.812844037,-0.811009174,-0.809174312,-0.80733945,-0.805504587,-0.803669725,
-0.801834862,-0.8,-0.798165138,-0.796330275,-0.794495413,-0.79266055,-0.790825688,
-0.788990826,-0.787155963,-0.785321101,-0.783486239,-0.781651376,-0.779816514,
-0.777981651,-0.776146789,-0.774311927,-0.772477064,-0.770642202,-0.768807339,
-0.766972477,-0.765137615,-0.763302752,-0.76146789,-0.759633028,-0.757798165,
-0.755963303,-0.75412844,-0.752293578,-0.750458716,-0.748623853,-0.746788991,
-0.744954128,-0.743119266,-0.741284404,-0.739449541,-0.737614679,-0.735779817,
-0.733944954,-0.732110092,-0.730275229,-0.728440367,-0.726605505,-0.724770642,
-0.72293578,-0.721100917,-0.719266055,-0.717431193,-0.71559633,-0.713761468,
-0.711926606,-0.710091743,-0.708256881,-0.706422018,-0.704587156,-0.702752294,
-0.700917431,-0.699082569,-0.697247706,-0.695412844,-0.693577982,-0.691743119,
-0.689908257,-0.688073394,-0.686238532,-0.68440367,-0.682568807,-0.680733945,
-0.678899083,-0.67706422,-0.675229358,-0.673394495,-0.671559633,-0.669724771,
-0.667889908,-0.666055046,-0.664220183,-0.662385321,-0.660550459,-0.658715596,
-0.656880734,-0.655045872,-0.653211009,-0.651376147,-0.649541284,-0.647706422,
-0.64587156,-0.644036697,-0.642201835,-0.640366972,-0.63853211,-0.636697248,
-0.634862385,-0.633027523,-0.631192661,-0.629357798,-0.627522936,-0.625688073,
-0.623853211,-0.622018349,-0.620183486,-0.618348624,-0.616513761,-0.614678899,
-0.612844037,-0.611009174,-0.609174312,-0.60733945,-0.605504587,-0.603669725,
-0.601834862,-0.6,-0.598165138,-0.596330275,-0.594495413,-0.59266055,-0.590825688,
-0.588990826,-0.587155963,-0.585321101,-0.583486239,-0.581651376,-0.579816514,
-0.577981651,-0.576146789,-0.574311927,-0.572477064,-0.570642202,-0.568807339,
-0.566972477,-0.565137615,-0.563302752,-0.56146789,-0.559633028,-0.557798165,
-0.555963303,-0.55412844,-0.552293578,-0.550458716,-0.548623853,-0.546788991,
-0.544954128,-0.543119266,-0.541284404,-0.539449541,-0.537614679,-0.535779817,
-0.533944954,-0.532110092,-0.530275229,-0.528440367,-0.526605505,-0.524770642,
-0.52293578,-0.521100917,-0.519266055,-0.517431193,-0.51559633,-0.513761468,
-0.511926606,-0.510091743,-0.508256881,-0.506422018,-0.504587156,-0.502752294,
-0.500917431,-0.499082569,-0.497247706,-0.495412844,-0.493577982,-0.491743119,
-0.489908257,-0.488073394,-0.486238532,-0.48440367,-0.482568807,-0.480733945,
-0.478899083,-0.47706422,-0.475229358,-0.473394495,-0.471559633,-0.469724771,
-0.467889908,-0.466055046,-0.464220183,-0.462385321,-0.460550459,-0.458715596,
-0.456880734,-0.455045872,-0.453211009,-0.451376147,-0.449541284,-0.447706422,
-0.44587156,-0.444036697,-0.442201835,-0.440366972,-0.43853211,-0.436697248,
-0.434862385,-0.433027523,-0.431192661,-0.429357798,-0.427522936,-0.425688073,
-0.423853211,-0.422018349,-0.420183486,-0.418348624,-0.416513761,-0.414678899,
-0.412844037,-0.411009174,-0.409174312,-0.40733945,-0.405504587,-0.403669725,
-0.401834862,-0.4,-0.398165138,-0.396330275,-0.394495413,-0.39266055,-0.390825688,
-0.388990826,-0.387155963,-0.385321101,-0.383486239,-0.381651376,-0.379816514,
-0.377981651,-0.376146789,-0.374311927,-0.372477064,-0.370642202,-0.368807339,
-0.366972477,-0.365137615,-0.363302752,-0.36146789,-0.359633028,-0.357798165,
-0.355963303,-0.35412844,-0.352293578,-0.350458716,-0.348623853,-0.346788991,
-0.344954128,-0.343119266,-0.341284404,-0.339449541,-0.337614679,-0.335779817,
-0.333944954,-0.332110092,-0.330275229,-0.328440367,-0.326605505,-0.324770642,
-0.32293578,-0.321100917,-0.319266055,-0.317431193,-0.31559633,-0.313761468,
-0.311926606,-0.310091743,-0.308256881,-0.306422018,-0.304587156,-0.302752294,
-0.300917431,-0.299082569,-0.297247706,-0.295412844,-0.293577982,-0.291743119,
-0.289908257,-0.288073394,-0.286238532,-0.28440367,-0.282568807,-0.280733945,
-0.278899083,-0.27706422,-0.275229358,-0.273394495,-0.271559633,-0.269724771,
-0.267889908,-0.266055046,-0.264220183,-0.262385321,-0.260550459,-0.258715596,
-0.256880734,-0.255045872,-0.253211009,-0.251376147,-0.249541284,-0.247706422,
-0.24587156,-0.244036697,-0.242201835,-0.240366972,-0.23853211,-0.236697248,
-0.234862385,-0.233027523,-0.231192661,-0.229357798,-0.227522936,-0.225688073,
-0.223853211,-0.222018349,-0.220183486,-0.218348624,-0.216513761,-0.214678899,
-0.212844037,-0.211009174,-0.209174312,-0.20733945,-0.205504587,-0.203669725,
-0.201834862,-0.2,-0.198165138,-0.196330275,-0.194495413,-0.19266055,-0.190825688,
-0.188990826,-0.187155963,-0.185321101,-0.183486239,-0.181651376,-0.179816514,
-0.177981651,-0.176146789,-0.174311927,-0.172477064,-0.170642202,-0.168807339,
-0.166972477,-0.165137615,-0.163302752,-0.16146789,-0.159633028,-0.157798165,
-0.155963303,-0.15412844,-0.152293578,-0.150458716,-0.148623853,-0.146788991,
-0.144954128,-0.143172102),.UNSPECIFIED.);
#24468=B_SPLINE_CURVE_WITH_KNOTS('',5,(#277465,#277466,#277467,#277468,
#277469,#277470,#277471,#277472,#277473,#277474,#277475,#277476,#277477,
#277478,#277479,#277480,#277481,#277482,#277483,#277484,#277485,#277486,
#277487,#277488,#277489,#277490,#277491,#277492,#277493,#277494,#277495,
#277496,#277497,#277498,#277499,#277500,#277501,#277502,#277503,#277504,
#277505,#277506,#277507,#277508,#277509,#277510,#277511,#277512,#277513,
#277514,#277515,#277516,#277517,#277518,#277519,#277520,#277521,#277522,
#277523,#277524,#277525,#277526,#277527,#277528,#277529,#277530,#277531,
#277532,#277533,#277534,#277535,#277536,#277537,#277538,#277539,#277540,
#277541,#277542,#277543,#277544,#277545,#277546,#277547,#277548,#277549,
#277550,#277551,#277552,#277553,#277554,#277555,#277556,#277557,#277558,
#277559,#277560,#277561,#277562,#277563,#277564,#277565,#277566,#277567,
#277568,#277569,#277570,#277571,#277572,#277573,#277574,#277575,#277576,
#277577,#277578,#277579,#277580,#277581,#277582,#277583,#277584,#277585,
#277586,#277587,#277588,#277589,#277590,#277591,#277592,#277593,#277594,
#277595,#277596,#277597,#277598,#277599,#277600,#277601,#277602,#277603,
#277604,#277605,#277606,#277607,#277608,#277609,#277610,#277611,#277612,
#277613,#277614,#277615,#277616,#277617,#277618,#277619,#277620,#277621,
#277622,#277623,#277624,#277625,#277626,#277627,#277628,#277629,#277630,
#277631,#277632,#277633,#277634,#277635,#277636,#277637,#277638,#277639,
#277640,#277641,#277642,#277643,#277644,#277645,#277646,#277647,#277648,
#277649,#277650,#277651,#277652,#277653,#277654,#277655,#277656,#277657,
#277658,#277659,#277660,#277661,#277662,#277663,#277664,#277665,#277666,
#277667,#277668,#277669,#277670,#277671,#277672,#277673,#277674,#277675,
#277676,#277677,#277678,#277679,#277680,#277681,#277682,#277683,#277684,
#277685,#277686,#277687,#277688,#277689,#277690,#277691,#277692,#277693,
#277694,#277695,#277696,#277697,#277698,#277699,#277700,#277701,#277702,
#277703,#277704,#277705,#277706,#277707,#277708,#277709,#277710,#277711,
#277712,#277713,#277714,#277715,#277716,#277717,#277718,#277719,#277720,
#277721,#277722,#277723,#277724,#277725,#277726,#277727,#277728,#277729,
#277730,#277731,#277732,#277733,#277734,#277735,#277736,#277737,#277738,
#277739,#277740,#277741,#277742,#277743,#277744,#277745,#277746,#277747,
#277748,#277749,#277750,#277751,#277752,#277753,#277754,#277755,#277756,
#277757,#277758,#277759,#277760,#277761,#277762,#277763,#277764,#277765,
#277766,#277767,#277768,#277769,#277770,#277771,#277772,#277773,#277774,
#277775,#277776,#277777,#277778,#277779,#277780,#277781,#277782,#277783,
#277784,#277785,#277786,#277787,#277788,#277789,#277790,#277791,#277792,
#277793,#277794,#277795,#277796,#277797,#277798,#277799,#277800,#277801,
#277802,#277803,#277804,#277805,#277806,#277807,#277808,#277809,#277810,
#277811,#277812,#277813,#277814,#277815,#277816,#277817,#277818,#277819,
#277820,#277821,#277822,#277823,#277824,#277825,#277826,#277827,#277828,
#277829,#277830,#277831,#277832,#277833,#277834,#277835,#277836,#277837,
#277838,#277839,#277840,#277841,#277842,#277843,#277844,#277845,#277846,
#277847,#277848,#277849,#277850,#277851,#277852,#277853,#277854,#277855,
#277856,#277857,#277858,#277859,#277860,#277861,#277862,#277863,#277864,
#277865,#277866,#277867,#277868,#277869,#277870,#277871,#277872,#277873,
#277874,#277875,#277876,#277877,#277878,#277879,#277880,#277881,#277882,
#277883,#277884,#277885,#277886,#277887,#277888,#277889,#277890,#277891,
#277892,#277893,#277894,#277895,#277896,#277897,#277898,#277899,#277900,
#277901,#277902,#277903,#277904,#277905,#277906,#277907,#277908,#277909,
#277910,#277911,#277912,#277913,#277914,#277915,#277916,#277917,#277918,
#277919,#277920,#277921,#277922,#277923,#277924,#277925,#277926,#277927,
#277928,#277929,#277930,#277931,#277932,#277933,#277934,#277935),
 .UNSPECIFIED.,.F.,.F.,(6,1,1,1,1,1,1,1,1,1,1,1,1,1,1,1,1,1,1,1,1,1,1,1,
1,1,1,1,1,1,1,1,1,1,1,1,1,1,1,1,1,1,1,1,1,1,1,1,1,1,1,1,1,1,1,1,1,1,1,1,
1,1,1,1,1,1,1,1,1,1,1,1,1,1,1,1,1,1,1,1,1,1,1,1,1,1,1,1,1,1,1,1,1,1,1,1,
1,1,1,1,1,1,1,1,1,1,1,1,1,1,1,1,1,1,1,1,1,1,1,1,1,1,1,1,1,1,1,1,1,1,1,1,
1,1,1,1,1,1,1,1,1,1,1,1,1,1,1,1,1,1,1,1,1,1,1,1,1,1,1,1,1,1,1,1,1,1,1,1,
1,1,1,1,1,1,1,1,1,1,1,1,1,1,1,1,1,1,1,1,1,1,1,1,1,1,1,1,1,1,1,1,1,1,1,1,
1,1,1,1,1,1,1,1,1,1,1,1,1,1,1,1,1,1,1,1,1,1,1,1,1,1,1,1,1,1,1,1,1,1,1,1,
1,1,1,1,1,1,1,1,1,1,1,1,1,1,1,1,1,1,1,1,1,1,1,1,1,1,1,1,1,1,1,1,1,1,1,1,
1,1,1,1,1,1,1,1,1,1,1,1,1,1,1,1,1,1,1,1,1,1,1,1,1,1,1,1,1,1,1,1,1,1,1,1,
1,1,1,1,1,1,1,1,1,1,1,1,1,1,1,1,1,1,1,1,1,1,1,1,1,1,1,1,1,1,1,1,1,1,1,1,
1,1,1,1,1,1,1,1,1,1,1,1,1,1,1,1,1,1,1,1,1,1,1,1,1,1,1,1,1,1,1,1,1,1,1,1,
1,1,1,1,1,1,1,1,1,1,1,1,1,1,1,1,1,1,1,1,1,1,1,1,1,1,1,1,1,1,1,1,1,1,1,1,
1,1,1,1,1,1,1,1,1,1,1,1,1,1,1,1,1,1,1,1,1,1,1,1,1,1,1,1,1,1,1,1,1,1,1,1,
1,1,1,1,1,1,1,1,1,1,6),(0.143172102,0.144954128,0.146788991,0.148623853,
0.150458716,0.152293578,0.15412844,0.155963303,0.157798165,0.159633028,
0.16146789,0.163302752,0.165137615,0.166972477,0.168807339,0.170642202,
0.172477064,0.174311927,0.176146789,0.177981651,0.179816514,0.181651376,
0.183486239,0.185321101,0.187155963,0.188990826,0.190825688,0.19266055,
0.194495413,0.196330275,0.198165138,0.2,0.201834862,0.203669725,0.205504587,
0.20733945,0.209174312,0.211009174,0.212844037,0.214678899,0.216513761,
0.218348624,0.220183486,0.222018349,0.223853211,0.225688073,0.227522936,
0.229357798,0.231192661,0.233027523,0.234862385,0.236697248,0.23853211,
0.240366972,0.242201835,0.244036697,0.24587156,0.247706422,0.249541284,
0.251376147,0.253211009,0.255045872,0.256880734,0.258715596,0.260550459,
0.262385321,0.264220183,0.266055046,0.267889908,0.269724771,0.271559633,
0.273394495,0.275229358,0.27706422,0.278899083,0.280733945,0.282568807,
0.28440367,0.286238532,0.288073394,0.289908257,0.291743119,0.293577982,
0.295412844,0.297247706,0.299082569,0.300917431,0.302752294,0.304587156,
0.306422018,0.308256881,0.310091743,0.311926606,0.313761468,0.31559633,
0.317431193,0.319266055,0.321100917,0.32293578,0.324770642,0.326605505,
0.328440367,0.330275229,0.332110092,0.333944954,0.335779817,0.337614679,
0.339449541,0.341284404,0.343119266,0.344954128,0.346788991,0.348623853,
0.350458716,0.352293578,0.35412844,0.355963303,0.357798165,0.359633028,
0.36146789,0.363302752,0.365137615,0.366972477,0.368807339,0.370642202,
0.372477064,0.374311927,0.376146789,0.377981651,0.379816514,0.381651376,
0.383486239,0.385321101,0.387155963,0.388990826,0.390825688,0.39266055,
0.394495413,0.396330275,0.398165138,0.4,0.401834862,0.403669725,0.405504587,
0.40733945,0.409174312,0.411009174,0.412844037,0.414678899,0.416513761,
0.418348624,0.420183486,0.422018349,0.423853211,0.425688073,0.427522936,
0.429357798,0.431192661,0.433027523,0.434862385,0.436697248,0.43853211,
0.440366972,0.442201835,0.444036697,0.44587156,0.447706422,0.449541284,
0.451376147,0.453211009,0.455045872,0.456880734,0.458715596,0.460550459,
0.462385321,0.464220183,0.466055046,0.467889908,0.469724771,0.471559633,
0.473394495,0.475229358,0.47706422,0.478899083,0.480733945,0.482568807,
0.48440367,0.486238532,0.488073394,0.489908257,0.491743119,0.493577982,
0.495412844,0.497247706,0.499082569,0.500917431,0.502752294,0.504587156,
0.506422018,0.508256881,0.510091743,0.511926606,0.513761468,0.51559633,
0.517431193,0.519266055,0.521100917,0.52293578,0.524770642,0.526605505,
0.528440367,0.530275229,0.532110092,0.533944954,0.535779817,0.537614679,
0.539449541,0.541284404,0.543119266,0.544954128,0.546788991,0.548623853,
0.550458716,0.552293578,0.55412844,0.555963303,0.557798165,0.559633028,
0.56146789,0.563302752,0.565137615,0.566972477,0.568807339,0.570642202,
0.572477064,0.574311927,0.576146789,0.577981651,0.579816514,0.581651376,
0.583486239,0.585321101,0.587155963,0.588990826,0.590825688,0.59266055,
0.594495413,0.596330275,0.598165138,0.6,0.601834862,0.603669725,0.605504587,
0.60733945,0.609174312,0.611009174,0.612844037,0.614678899,0.616513761,
0.618348624,0.620183486,0.622018349,0.623853211,0.625688073,0.627522936,
0.629357798,0.631192661,0.633027523,0.634862385,0.636697248,0.63853211,
0.640366972,0.642201835,0.644036697,0.64587156,0.647706422,0.649541284,
0.651376147,0.653211009,0.655045872,0.656880734,0.658715596,0.660550459,
0.662385321,0.664220183,0.666055046,0.667889908,0.669724771,0.671559633,
0.673394495,0.675229358,0.67706422,0.678899083,0.680733945,0.682568807,
0.68440367,0.686238532,0.688073394,0.689908257,0.691743119,0.693577982,
0.695412844,0.697247706,0.699082569,0.700917431,0.702752294,0.704587156,
0.706422018,0.708256881,0.710091743,0.711926606,0.713761468,0.71559633,
0.717431193,0.719266055,0.721100917,0.72293578,0.724770642,0.726605505,
0.728440367,0.730275229,0.732110092,0.733944954,0.735779817,0.737614679,
0.739449541,0.741284404,0.743119266,0.744954128,0.746788991,0.748623853,
0.750458716,0.752293578,0.75412844,0.755963303,0.757798165,0.759633028,
0.76146789,0.763302752,0.765137615,0.766972477,0.768807339,0.770642202,
0.772477064,0.774311927,0.776146789,0.777981651,0.779816514,0.781651376,
0.783486239,0.785321101,0.787155963,0.788990826,0.790825688,0.79266055,
0.794495413,0.796330275,0.798165138,0.8,0.801834862,0.803669725,0.805504587,
0.80733945,0.809174312,0.811009174,0.812844037,0.814678899,0.816513761,
0.818348624,0.820183486,0.822018349,0.823853211,0.825688073,0.827522936,
0.829357798,0.831192661,0.833027523,0.834862385,0.836697248,0.83853211,
0.840366972,0.842201835,0.844036697,0.84587156,0.847706422,0.849541284,
0.851376147,0.853211009,0.855045872,0.856880734,0.858715596,0.860550459,
0.862385321,0.864220183,0.866055046,0.867889908,0.869724771,0.871559633,
0.873394495,0.875229358,0.87706422,0.878899083,0.880733945,0.882568807,
0.88440367,0.886238532,0.888073394,0.889908257,0.893577982,0.895412844,
0.897247706,0.899082569,0.900917431,0.902752294,0.904587156,0.906422018,
0.908256881,0.910091743,0.911926606,0.913761468,0.91559633,0.917431193,
0.919266055,0.921100917,0.92293578,0.924770642,0.926605505,0.928440367,
0.930275229,0.932110092,0.933944954,0.935779817,0.937614679,0.939449541,
0.941284404,0.943119266,0.944954128,0.946788991,0.948623853,0.950458716,
0.952293578,0.95412844,0.955963303,0.957798165,0.959633028,0.96146789,0.963302752,
0.965137615,0.966972477,0.968807339,0.970642202,0.972477064,0.974311927,
0.976146789,0.977981651,0.979816514,0.981651376,0.983486239,0.985321101,
0.987155963,0.988990826,0.990825688,0.99266055,0.994495413,0.996330275,
0.998165138,1.),.UNSPECIFIED.);
#24469=B_SPLINE_CURVE_WITH_KNOTS('',3,(#278880,#278881,#278882,#278883,
#278884,#278885,#278886,#278887,#278888,#278889,#278890,#278891,#278892,
#278893,#278894,#278895,#278896,#278897,#278898,#278899,#278900,#278901,
#278902,#278903,#278904,#278905,#278906,#278907,#278908,#278909,#278910,
#278911,#278912,#278913,#278914,#278915,#278916,#278917,#278918,#278919,
#278920,#278921,#278922,#278923,#278924,#278925,#278926,#278927,#278928,
#278929,#278930,#278931,#278932,#278933,#278934,#278935,#278936,#278937,
#278938,#278939,#278940,#278941,#278942,#278943,#278944,#278945,#278946,
#278947,#278948,#278949,#278950,#278951,#278952,#278953,#278954,#278955,
#278956,#278957,#278958,#278959,#278960,#278961,#278962,#278963,#278964,
#278965,#278966,#278967,#278968,#278969,#278970,#278971,#278972,#278973,
#278974,#278975,#278976,#278977,#278978,#278979,#278980,#278981,#278982,
#278983,#278984,#278985,#278986,#278987,#278988,#278989,#278990,#278991,
#278992,#278993,#278994,#278995,#278996,#278997,#278998,#278999,#279000,
#279001,#279002,#279003,#279004,#279005,#279006,#279007,#279008,#279009,
#279010,#279011,#279012,#279013,#279014,#279015,#279016,#279017,#279018,
#279019,#279020,#279021,#279022,#279023,#279024,#279025,#279026,#279027,
#279028,#279029,#279030,#279031,#279032,#279033,#279034,#279035,#279036,
#279037,#279038,#279039,#279040,#279041,#279042,#279043,#279044,#279045,
#279046,#279047,#279048,#279049,#279050,#279051,#279052,#279053,#279054,
#279055,#279056,#279057,#279058,#279059,#279060,#279061,#279062,#279063,
#279064,#279065,#279066,#279067,#279068,#279069,#279070,#279071,#279072,
#279073,#279074,#279075,#279076,#279077,#279078,#279079,#279080,#279081,
#279082,#279083,#279084,#279085,#279086,#279087,#279088,#279089,#279090,
#279091,#279092,#279093,#279094,#279095,#279096,#279097,#279098,#279099,
#279100,#279101,#279102,#279103,#279104,#279105,#279106,#279107,#279108,
#279109,#279110,#279111,#279112,#279113,#279114,#279115,#279116,#279117,
#279118,#279119,#279120,#279121,#279122,#279123,#279124,#279125,#279126,
#279127,#279128,#279129,#279130,#279131,#279132,#279133,#279134,#279135,
#279136,#279137,#279138,#279139,#279140,#279141,#279142,#279143,#279144,
#279145,#279146,#279147,#279148,#279149,#279150,#279151,#279152,#279153,
#279154,#279155,#279156,#279157,#279158,#279159,#279160,#279161,#279162,
#279163,#279164,#279165,#279166,#279167,#279168,#279169,#279170,#279171,
#279172,#279173,#279174,#279175,#279176,#279177,#279178,#279179,#279180,
#279181,#279182,#279183,#279184,#279185,#279186,#279187,#279188,#279189,
#279190,#279191,#279192,#279193,#279194,#279195,#279196,#279197,#279198,
#279199,#279200,#279201),.UNSPECIFIED.,.F.,.F.,(4,3,3,3,3,3,3,3,3,3,3,3,
3,3,3,3,3,3,3,3,3,3,3,3,3,3,3,3,3,3,3,3,3,3,3,3,3,3,3,3,3,3,3,3,3,3,3,3,
3,3,3,3,3,3,3,3,3,3,3,3,3,3,3,3,3,3,3,3,3,3,3,3,3,3,3,3,3,3,3,3,3,3,3,3,
3,3,3,3,3,3,3,3,3,3,3,3,3,3,3,3,3,3,3,3,3,3,3,4),(0.143172102,0.15412844,
0.165137615,0.176146789,0.187155963,0.198165138,0.209174312,0.220183486,
0.231192661,0.242201835,0.253211009,0.264220183,0.275229358,0.286238532,
0.297247706,0.308256881,0.319266055,0.330275229,0.341284404,0.352293578,
0.363302752,0.374311927,0.385321101,0.396330275,0.405504587,0.414678899,
0.423853211,0.433027523,0.442201835,0.451376147,0.460550459,0.469724771,
0.478899083,0.488073394,0.497247706,0.506422018,0.51559633,0.524770642,
0.533944954,0.541284404,0.548623853,0.555963303,0.563302752,0.570642202,
0.577981651,0.585321101,0.59266055,0.6,0.60733945,0.614678899,0.622018349,
0.631192661,0.63853211,0.64587156,0.655045872,0.662385321,0.669724771,0.67706422,
0.68440367,0.691743119,0.699082569,0.708256881,0.71559633,0.72293578,0.730275229,
0.737614679,0.746788991,0.75412844,0.76146789,0.768807339,0.776146789,0.783486239,
0.790825688,0.798165138,0.805504587,0.811009174,0.816513761,0.822018349,
0.827522936,0.833027523,0.840366972,0.84587156,0.851376147,0.856880734,
0.862385321,0.867889908,0.873394495,0.878899083,0.88440367,0.889908257,
0.895412844,0.902752294,0.908256881,0.913761468,0.919266055,0.928440367,
0.935779817,0.941284404,0.946788991,0.952293578,0.959633028,0.966972477,
0.972477064,0.977981651,0.983486239,0.988990826,0.994495413,1.),
 .UNSPECIFIED.);
#24470=B_SPLINE_CURVE_WITH_KNOTS('',3,(#279202,#279203,#279204,#279205,
#279206,#279207,#279208,#279209,#279210,#279211,#279212,#279213,#279214,
#279215,#279216,#279217,#279218,#279219,#279220,#279221,#279222,#279223,
#279224,#279225,#279226,#279227,#279228,#279229,#279230,#279231,#279232,
#279233,#279234,#279235,#279236,#279237,#279238,#279239,#279240,#279241,
#279242,#279243,#279244,#279245,#279246,#279247,#279248,#279249,#279250,
#279251,#279252,#279253,#279254,#279255,#279256,#279257,#279258,#279259,
#279260,#279261,#279262,#279263,#279264,#279265,#279266,#279267,#279268,
#279269,#279270,#279271,#279272,#279273,#279274,#279275,#279276,#279277,
#279278,#279279,#279280,#279281,#279282,#279283,#279284,#279285,#279286,
#279287,#279288,#279289,#279290,#279291,#279292,#279293,#279294,#279295,
#279296,#279297,#279298,#279299,#279300,#279301,#279302,#279303,#279304,
#279305,#279306,#279307,#279308,#279309,#279310,#279311,#279312,#279313,
#279314,#279315,#279316,#279317,#279318,#279319,#279320,#279321,#279322,
#279323,#279324,#279325,#279326,#279327,#279328,#279329,#279330,#279331,
#279332,#279333,#279334,#279335,#279336,#279337,#279338,#279339,#279340,
#279341,#279342,#279343,#279344,#279345,#279346,#279347,#279348,#279349,
#279350,#279351,#279352,#279353,#279354,#279355,#279356,#279357,#279358,
#279359,#279360,#279361,#279362,#279363,#279364,#279365,#279366,#279367,
#279368,#279369,#279370,#279371,#279372,#279373,#279374,#279375,#279376,
#279377,#279378,#279379,#279380,#279381,#279382,#279383,#279384,#279385,
#279386,#279387,#279388,#279389,#279390,#279391,#279392,#279393,#279394,
#279395,#279396,#279397,#279398,#279399,#279400,#279401,#279402,#279403,
#279404,#279405,#279406,#279407,#279408,#279409,#279410,#279411,#279412,
#279413,#279414,#279415,#279416,#279417,#279418,#279419,#279420,#279421,
#279422,#279423,#279424,#279425,#279426,#279427,#279428,#279429,#279430,
#279431,#279432,#279433,#279434,#279435,#279436,#279437,#279438,#279439,
#279440,#279441,#279442,#279443,#279444,#279445,#279446,#279447,#279448,
#279449,#279450,#279451,#279452,#279453,#279454,#279455,#279456,#279457,
#279458,#279459,#279460,#279461,#279462,#279463,#279464,#279465,#279466,
#279467,#279468,#279469,#279470,#279471,#279472,#279473,#279474,#279475,
#279476,#279477,#279478,#279479,#279480,#279481,#279482,#279483,#279484,
#279485,#279486,#279487,#279488,#279489,#279490,#279491,#279492,#279493,
#279494,#279495,#279496,#279497,#279498,#279499,#279500,#279501,#279502,
#279503,#279504,#279505,#279506,#279507,#279508,#279509,#279510,#279511,
#279512,#279513,#279514,#279515,#279516,#279517,#279518,#279519,#279520,
#279521,#279522,#279523,#279524,#279525,#279526),.UNSPECIFIED.,.F.,.F.,
(4,3,3,3,3,3,3,3,3,3,3,3,3,3,3,3,3,3,3,3,3,3,3,3,3,3,3,3,3,3,3,3,3,3,3,
3,3,3,3,3,3,3,3,3,3,3,3,3,3,3,3,3,3,3,3,3,3,3,3,3,3,3,3,3,3,3,3,3,3,3,3,
3,3,3,3,3,3,3,3,3,3,3,3,3,3,3,3,3,3,3,3,3,3,3,3,3,3,3,3,3,3,3,3,3,3,3,3,
3,4),(0.143172102,0.15412844,0.165137615,0.176146789,0.187155963,0.198165138,
0.209174312,0.220183486,0.231192661,0.242201835,0.253211009,0.264220183,
0.275229358,0.286238532,0.297247706,0.308256881,0.319266055,0.330275229,
0.341284404,0.352293578,0.363302752,0.374311927,0.385321101,0.396330275,
0.405504587,0.414678899,0.423853211,0.433027523,0.442201835,0.451376147,
0.460550459,0.469724771,0.478899083,0.488073394,0.497247706,0.506422018,
0.51559633,0.524770642,0.533944954,0.541284404,0.548623853,0.555963303,
0.563302752,0.570642202,0.579816514,0.587155963,0.594495413,0.601834862,
0.609174312,0.616513761,0.623853211,0.631192661,0.63853211,0.64587156,0.653211009,
0.664220183,0.671559633,0.678899083,0.686238532,0.693577982,0.700917431,
0.708256881,0.71559633,0.72293578,0.730275229,0.737614679,0.744954128,0.752293578,
0.759633028,0.766972477,0.774311927,0.781651376,0.788990826,0.796330275,
0.803669725,0.811009174,0.816513761,0.822018349,0.827522936,0.833027523,
0.83853211,0.844036697,0.849541284,0.855045872,0.860550459,0.866055046,
0.871559633,0.87706422,0.882568807,0.889908257,0.895412844,0.902752294,
0.908256881,0.913761468,0.919266055,0.924770642,0.930275229,0.935779817,
0.941284404,0.946788991,0.952293578,0.957798165,0.966972477,0.972477064,
0.977981651,0.983486239,0.988990826,0.994495413,1.),.UNSPECIFIED.);
#24471=B_SPLINE_CURVE_WITH_KNOTS('',3,(#280486,#280487,#280488,#280489,
#280490,#280491,#280492,#280493,#280494,#280495,#280496,#280497,#280498,
#280499,#280500,#280501,#280502,#280503,#280504,#280505,#280506,#280507,
#280508,#280509,#280510,#280511,#280512,#280513,#280514,#280515,#280516,
#280517,#280518,#280519,#280520,#280521,#280522,#280523,#280524,#280525,
#280526,#280527,#280528,#280529,#280530,#280531,#280532,#280533,#280534,
#280535,#280536,#280537,#280538,#280539,#280540,#280541,#280542,#280543,
#280544,#280545,#280546,#280547,#280548,#280549,#280550,#280551,#280552,
#280553,#280554,#280555,#280556,#280557,#280558,#280559,#280560,#280561,
#280562,#280563,#280564,#280565,#280566,#280567,#280568,#280569,#280570,
#280571,#280572,#280573,#280574,#280575,#280576,#280577,#280578,#280579,
#280580,#280581,#280582,#280583,#280584,#280585,#280586,#280587,#280588,
#280589,#280590,#280591,#280592,#280593,#280594,#280595,#280596,#280597,
#280598,#280599,#280600,#280601,#280602,#280603,#280604,#280605,#280606,
#280607,#280608,#280609,#280610,#280611,#280612,#280613,#280614,#280615,
#280616,#280617,#280618,#280619,#280620,#280621,#280622,#280623,#280624,
#280625,#280626,#280627,#280628,#280629,#280630,#280631,#280632,#280633,
#280634,#280635,#280636,#280637,#280638,#280639,#280640,#280641,#280642,
#280643,#280644,#280645,#280646,#280647,#280648,#280649,#280650,#280651,
#280652,#280653,#280654,#280655,#280656,#280657,#280658,#280659,#280660,
#280661,#280662,#280663,#280664,#280665,#280666,#280667,#280668,#280669,
#280670,#280671,#280672,#280673,#280674,#280675,#280676,#280677,#280678,
#280679,#280680,#280681,#280682,#280683,#280684,#280685,#280686,#280687,
#280688,#280689,#280690,#280691,#280692,#280693,#280694,#280695,#280696,
#280697,#280698,#280699,#280700,#280701,#280702,#280703,#280704,#280705,
#280706,#280707,#280708,#280709,#280710,#280711,#280712,#280713,#280714,
#280715,#280716,#280717,#280718,#280719,#280720,#280721,#280722,#280723,
#280724,#280725,#280726,#280727,#280728,#280729,#280730,#280731,#280732,
#280733,#280734,#280735,#280736,#280737,#280738,#280739,#280740,#280741,
#280742,#280743,#280744,#280745,#280746,#280747,#280748,#280749,#280750,
#280751,#280752,#280753,#280754,#280755,#280756,#280757,#280758,#280759,
#280760,#280761,#280762,#280763,#280764,#280765,#280766,#280767,#280768,
#280769,#280770,#280771,#280772,#280773,#280774,#280775,#280776,#280777,
#280778,#280779,#280780,#280781,#280782,#280783,#280784,#280785,#280786,
#280787,#280788,#280789,#280790,#280791,#280792,#280793,#280794,#280795,
#280796,#280797,#280798,#280799,#280800,#280801,#280802,#280803,#280804,
#280805,#280806,#280807,#280808,#280809,#280810),.UNSPECIFIED.,.F.,.F.,
(4,3,3,3,3,3,3,3,3,3,3,3,3,3,3,3,3,3,3,3,3,3,3,3,3,3,3,3,3,3,3,3,3,3,3,
3,3,3,3,3,3,3,3,3,3,3,3,3,3,3,3,3,3,3,3,3,3,3,3,3,3,3,3,3,3,3,3,3,3,3,3,
3,3,3,3,3,3,3,3,3,3,3,3,3,3,3,3,3,3,3,3,3,3,3,3,3,3,3,3,3,3,3,3,3,3,3,3,
3,4),(0.143172102,0.15412844,0.165137615,0.176146789,0.187155963,0.198165138,
0.209174312,0.220183486,0.231192661,0.242201835,0.253211009,0.264220183,
0.275229358,0.286238532,0.297247706,0.308256881,0.319266055,0.330275229,
0.341284404,0.352293578,0.363302752,0.374311927,0.385321101,0.396330275,
0.405504587,0.414678899,0.423853211,0.433027523,0.442201835,0.451376147,
0.460550459,0.469724771,0.478899083,0.488073394,0.497247706,0.506422018,
0.51559633,0.526605505,0.533944954,0.541284404,0.550458716,0.557798165,
0.565137615,0.572477064,0.579816514,0.587155963,0.594495413,0.601834862,
0.611009174,0.618348624,0.625688073,0.633027523,0.640366972,0.647706422,
0.655045872,0.662385321,0.671559633,0.678899083,0.686238532,0.693577982,
0.700917431,0.708256881,0.71559633,0.72293578,0.730275229,0.737614679,0.744954128,
0.752293578,0.759633028,0.766972477,0.774311927,0.781651376,0.788990826,
0.798165138,0.80733945,0.812844037,0.818348624,0.823853211,0.829357798,
0.834862385,0.840366972,0.84587156,0.851376147,0.856880734,0.862385321,
0.867889908,0.873394495,0.878899083,0.88440367,0.889908257,0.895412844,
0.902752294,0.908256881,0.913761468,0.919266055,0.924770642,0.930275229,
0.935779817,0.941284404,0.946788991,0.952293578,0.959633028,0.965137615,
0.970642202,0.976146789,0.981651376,0.987155963,0.99266055,1.),
 .UNSPECIFIED.);
#24472=B_SPLINE_CURVE_WITH_KNOTS('',3,(#280811,#280812,#280813,#280814,
#280815,#280816,#280817,#280818,#280819,#280820,#280821,#280822,#280823,
#280824,#280825,#280826,#280827,#280828,#280829,#280830,#280831,#280832,
#280833,#280834,#280835,#280836,#280837,#280838,#280839,#280840,#280841,
#280842,#280843,#280844,#280845,#280846,#280847,#280848,#280849,#280850,
#280851,#280852,#280853,#280854,#280855,#280856,#280857,#280858,#280859,
#280860,#280861,#280862,#280863,#280864,#280865,#280866,#280867,#280868,
#280869,#280870,#280871,#280872,#280873,#280874,#280875,#280876,#280877,
#280878,#280879,#280880,#280881,#280882,#280883,#280884,#280885,#280886,
#280887,#280888,#280889,#280890,#280891,#280892,#280893,#280894,#280895,
#280896,#280897,#280898,#280899,#280900,#280901,#280902,#280903,#280904,
#280905,#280906,#280907,#280908,#280909,#280910,#280911,#280912,#280913,
#280914,#280915,#280916,#280917,#280918,#280919,#280920,#280921,#280922,
#280923,#280924,#280925,#280926,#280927,#280928,#280929,#280930,#280931,
#280932,#280933,#280934,#280935,#280936,#280937,#280938,#280939,#280940,
#280941,#280942,#280943,#280944,#280945,#280946,#280947,#280948,#280949,
#280950,#280951,#280952,#280953,#280954,#280955,#280956,#280957,#280958,
#280959,#280960,#280961,#280962,#280963,#280964,#280965,#280966,#280967,
#280968,#280969,#280970,#280971,#280972,#280973,#280974,#280975,#280976,
#280977,#280978,#280979,#280980,#280981,#280982,#280983,#280984,#280985,
#280986,#280987,#280988,#280989,#280990,#280991,#280992,#280993,#280994,
#280995,#280996,#280997,#280998,#280999,#281000,#281001,#281002,#281003,
#281004,#281005,#281006,#281007,#281008,#281009,#281010,#281011,#281012,
#281013,#281014,#281015,#281016,#281017,#281018,#281019,#281020,#281021,
#281022,#281023,#281024,#281025,#281026,#281027,#281028,#281029,#281030,
#281031,#281032,#281033,#281034,#281035,#281036,#281037,#281038,#281039,
#281040,#281041,#281042,#281043,#281044,#281045,#281046,#281047,#281048,
#281049,#281050,#281051,#281052,#281053,#281054,#281055,#281056,#281057,
#281058,#281059,#281060,#281061,#281062,#281063,#281064,#281065,#281066,
#281067,#281068,#281069,#281070,#281071,#281072,#281073,#281074,#281075,
#281076,#281077,#281078,#281079,#281080,#281081,#281082,#281083,#281084,
#281085,#281086,#281087,#281088,#281089,#281090,#281091,#281092,#281093,
#281094,#281095,#281096,#281097,#281098,#281099,#281100,#281101,#281102,
#281103,#281104,#281105,#281106,#281107,#281108,#281109,#281110,#281111,
#281112,#281113,#281114,#281115,#281116,#281117,#281118,#281119,#281120,
#281121,#281122,#281123,#281124,#281125,#281126,#281127,#281128,#281129,
#281130,#281131,#281132),.UNSPECIFIED.,.F.,.F.,(4,3,3,3,3,3,3,3,3,3,3,3,
3,3,3,3,3,3,3,3,3,3,3,3,3,3,3,3,3,3,3,3,3,3,3,3,3,3,3,3,3,3,3,3,3,3,3,3,
3,3,3,3,3,3,3,3,3,3,3,3,3,3,3,3,3,3,3,3,3,3,3,3,3,3,3,3,3,3,3,3,3,3,3,3,
3,3,3,3,3,3,3,3,3,3,3,3,3,3,3,3,3,3,3,3,3,3,3,4),(0.143172102,0.15412844,
0.165137615,0.176146789,0.187155963,0.198165138,0.209174312,0.220183486,
0.231192661,0.242201835,0.253211009,0.264220183,0.275229358,0.286238532,
0.297247706,0.308256881,0.319266055,0.330275229,0.341284404,0.352293578,
0.363302752,0.374311927,0.385321101,0.396330275,0.405504587,0.414678899,
0.423853211,0.433027523,0.442201835,0.451376147,0.460550459,0.469724771,
0.478899083,0.488073394,0.497247706,0.506422018,0.51559633,0.524770642,
0.533944954,0.543119266,0.550458716,0.557798165,0.565137615,0.572477064,
0.579816514,0.587155963,0.594495413,0.601834862,0.609174312,0.616513761,
0.623853211,0.631192661,0.63853211,0.64587156,0.653211009,0.660550459,0.667889908,
0.67706422,0.68440367,0.691743119,0.699082569,0.706422018,0.713761468,0.721100917,
0.728440367,0.735779817,0.743119266,0.750458716,0.757798165,0.765137615,
0.772477064,0.779816514,0.787155963,0.794495413,0.803669725,0.811009174,
0.818348624,0.823853211,0.829357798,0.834862385,0.840366972,0.84587156,
0.851376147,0.856880734,0.862385321,0.867889908,0.873394495,0.878899083,
0.886238532,0.891743119,0.899082569,0.904587156,0.910091743,0.91559633,
0.921100917,0.926605505,0.932110092,0.937614679,0.943119266,0.948623853,
0.95412844,0.959633028,0.965137615,0.972477064,0.979816514,0.985321101,
0.990825688,1.),.UNSPECIFIED.);
#24473=B_SPLINE_CURVE_WITH_KNOTS('',3,(#282080,#282081,#282082,#282083,
#282084,#282085,#282086,#282087,#282088,#282089,#282090,#282091,#282092,
#282093,#282094,#282095,#282096,#282097,#282098,#282099,#282100,#282101,
#282102,#282103,#282104,#282105,#282106,#282107,#282108,#282109,#282110,
#282111,#282112,#282113,#282114,#282115,#282116,#282117,#282118,#282119,
#282120,#282121,#282122,#282123,#282124,#282125,#282126,#282127,#282128,
#282129,#282130,#282131,#282132,#282133,#282134,#282135,#282136,#282137,
#282138,#282139,#282140,#282141,#282142,#282143,#282144,#282145,#282146,
#282147,#282148,#282149,#282150,#282151,#282152,#282153,#282154,#282155,
#282156,#282157,#282158,#282159,#282160,#282161,#282162,#282163,#282164,
#282165,#282166,#282167,#282168,#282169,#282170,#282171,#282172,#282173,
#282174,#282175,#282176,#282177,#282178,#282179,#282180,#282181,#282182,
#282183,#282184,#282185,#282186,#282187,#282188,#282189,#282190,#282191,
#282192,#282193,#282194,#282195,#282196,#282197,#282198,#282199,#282200,
#282201,#282202,#282203,#282204,#282205,#282206,#282207,#282208,#282209,
#282210,#282211,#282212,#282213,#282214,#282215,#282216,#282217,#282218,
#282219,#282220,#282221,#282222,#282223,#282224,#282225,#282226,#282227,
#282228,#282229,#282230,#282231,#282232,#282233,#282234,#282235,#282236,
#282237,#282238,#282239,#282240,#282241,#282242,#282243,#282244,#282245,
#282246,#282247,#282248,#282249,#282250,#282251,#282252,#282253,#282254,
#282255,#282256,#282257,#282258,#282259,#282260,#282261,#282262,#282263,
#282264,#282265,#282266,#282267,#282268,#282269,#282270,#282271,#282272,
#282273,#282274,#282275,#282276,#282277,#282278,#282279,#282280,#282281,
#282282,#282283,#282284,#282285,#282286,#282287,#282288,#282289,#282290,
#282291,#282292,#282293,#282294,#282295,#282296,#282297,#282298,#282299,
#282300,#282301,#282302,#282303,#282304,#282305,#282306,#282307,#282308,
#282309,#282310,#282311,#282312,#282313,#282314,#282315,#282316,#282317,
#282318,#282319,#282320,#282321,#282322,#282323,#282324,#282325,#282326,
#282327,#282328,#282329,#282330,#282331,#282332,#282333,#282334,#282335,
#282336,#282337,#282338,#282339,#282340,#282341,#282342,#282343,#282344,
#282345,#282346,#282347,#282348,#282349,#282350,#282351,#282352,#282353,
#282354,#282355,#282356,#282357,#282358,#282359,#282360,#282361,#282362,
#282363,#282364,#282365,#282366,#282367,#282368,#282369,#282370,#282371,
#282372,#282373,#282374,#282375,#282376,#282377,#282378,#282379,#282380,
#282381,#282382,#282383,#282384,#282385,#282386,#282387,#282388,#282389,
#282390,#282391,#282392,#282393,#282394,#282395,#282396,#282397,#282398,
#282399,#282400,#282401,#282402,#282403,#282404,#282405,#282406,#282407),
 .UNSPECIFIED.,.F.,.F.,(4,3,3,3,3,3,3,3,3,3,3,3,3,3,3,3,3,3,3,3,3,3,3,3,
3,3,3,3,3,3,3,3,3,3,3,3,3,3,3,3,3,3,3,3,3,3,3,3,3,3,3,3,3,3,3,3,3,3,3,3,
3,3,3,3,3,3,3,3,3,3,3,3,3,3,3,3,3,3,3,3,3,3,3,3,3,3,3,3,3,3,3,3,3,3,3,3,
3,3,3,3,3,3,3,3,3,3,3,3,3,4),(-1.,-0.994495413,-0.988990826,-0.983486239,
-0.977981651,-0.972477064,-0.966972477,-0.959633028,-0.95412844,-0.948623853,
-0.943119266,-0.937614679,-0.932110092,-0.926605505,-0.921100917,-0.91559633,
-0.910091743,-0.904587156,-0.899082569,-0.893577982,-0.888073394,-0.882568807,
-0.87706422,-0.871559633,-0.866055046,-0.860550459,-0.855045872,-0.849541284,
-0.844036697,-0.83853211,-0.833027523,-0.827522936,-0.822018349,-0.816513761,
-0.811009174,-0.805504587,-0.798165138,-0.790825688,-0.783486239,-0.776146789,
-0.768807339,-0.76146789,-0.75412844,-0.746788991,-0.739449541,-0.732110092,
-0.724770642,-0.717431193,-0.710091743,-0.702752294,-0.695412844,-0.688073394,
-0.680733945,-0.673394495,-0.666055046,-0.658715596,-0.651376147,-0.644036697,
-0.636697248,-0.629357798,-0.622018349,-0.614678899,-0.60733945,-0.6,-0.59266055,
-0.585321101,-0.577981651,-0.570642202,-0.559633028,-0.552293578,-0.544954128,
-0.537614679,-0.530275229,-0.521100917,-0.511926606,-0.502752294,-0.493577982,
-0.48440367,-0.475229358,-0.466055046,-0.456880734,-0.447706422,-0.43853211,
-0.429357798,-0.420183486,-0.411009174,-0.401834862,-0.39266055,-0.381651376,
-0.370642202,-0.359633028,-0.348623853,-0.337614679,-0.326605505,-0.31559633,
-0.304587156,-0.293577982,-0.282568807,-0.271559633,-0.260550459,-0.249541284,
-0.23853211,-0.227522936,-0.216513761,-0.205504587,-0.194495413,-0.183486239,
-0.172477064,-0.16146789,-0.143172102),.UNSPECIFIED.);
#24474=B_SPLINE_CURVE_WITH_KNOTS('',3,(#282408,#282409,#282410,#282411,
#282412,#282413,#282414,#282415,#282416,#282417,#282418,#282419,#282420,
#282421,#282422,#282423,#282424,#282425,#282426,#282427,#282428,#282429,
#282430,#282431,#282432,#282433,#282434,#282435,#282436,#282437,#282438,
#282439,#282440,#282441,#282442,#282443,#282444,#282445,#282446,#282447,
#282448,#282449,#282450,#282451,#282452,#282453,#282454,#282455,#282456,
#282457,#282458,#282459,#282460,#282461,#282462,#282463,#282464,#282465,
#282466,#282467,#282468,#282469,#282470,#282471,#282472,#282473,#282474,
#282475,#282476,#282477,#282478,#282479,#282480,#282481,#282482,#282483,
#282484,#282485,#282486,#282487,#282488,#282489,#282490,#282491,#282492,
#282493,#282494,#282495,#282496,#282497,#282498,#282499,#282500,#282501,
#282502,#282503,#282504,#282505,#282506,#282507,#282508,#282509,#282510,
#282511,#282512,#282513,#282514,#282515,#282516,#282517,#282518,#282519,
#282520,#282521,#282522,#282523,#282524,#282525,#282526,#282527,#282528,
#282529,#282530,#282531,#282532,#282533,#282534,#282535,#282536,#282537,
#282538,#282539,#282540,#282541,#282542,#282543,#282544,#282545,#282546,
#282547,#282548,#282549,#282550,#282551,#282552,#282553,#282554,#282555,
#282556,#282557,#282558,#282559,#282560,#282561,#282562,#282563,#282564,
#282565,#282566,#282567,#282568,#282569,#282570,#282571,#282572,#282573,
#282574,#282575,#282576,#282577,#282578,#282579,#282580,#282581,#282582,
#282583,#282584,#282585,#282586,#282587,#282588,#282589,#282590,#282591,
#282592,#282593,#282594,#282595,#282596,#282597,#282598,#282599,#282600,
#282601,#282602,#282603,#282604,#282605,#282606,#282607,#282608,#282609,
#282610,#282611,#282612,#282613,#282614,#282615,#282616,#282617,#282618,
#282619,#282620,#282621,#282622,#282623,#282624,#282625,#282626,#282627,
#282628,#282629,#282630,#282631,#282632,#282633,#282634,#282635,#282636,
#282637,#282638,#282639,#282640,#282641,#282642,#282643,#282644,#282645,
#282646,#282647,#282648,#282649,#282650,#282651,#282652,#282653,#282654,
#282655,#282656,#282657,#282658,#282659,#282660,#282661,#282662,#282663,
#282664,#282665,#282666,#282667,#282668,#282669,#282670,#282671,#282672,
#282673,#282674,#282675,#282676,#282677,#282678,#282679,#282680,#282681,
#282682,#282683,#282684,#282685,#282686,#282687,#282688,#282689,#282690,
#282691,#282692,#282693,#282694,#282695,#282696,#282697,#282698,#282699,
#282700,#282701,#282702,#282703,#282704,#282705,#282706,#282707,#282708,
#282709,#282710,#282711,#282712,#282713,#282714,#282715,#282716,#282717,
#282718,#282719,#282720,#282721,#282722,#282723,#282724,#282725,#282726,
#282727,#282728,#282729,#282730,#282731,#282732,#282733,#282734,#282735),
 .UNSPECIFIED.,.F.,.F.,(4,3,3,3,3,3,3,3,3,3,3,3,3,3,3,3,3,3,3,3,3,3,3,3,
3,3,3,3,3,3,3,3,3,3,3,3,3,3,3,3,3,3,3,3,3,3,3,3,3,3,3,3,3,3,3,3,3,3,3,3,
3,3,3,3,3,3,3,3,3,3,3,3,3,3,3,3,3,3,3,3,3,3,3,3,3,3,3,3,3,3,3,3,3,3,3,3,
3,3,3,3,3,3,3,3,3,3,3,3,3,4),(0.143172102,0.15412844,0.165137615,0.176146789,
0.187155963,0.198165138,0.209174312,0.220183486,0.231192661,0.242201835,
0.253211009,0.264220183,0.275229358,0.286238532,0.297247706,0.308256881,
0.319266055,0.330275229,0.341284404,0.352293578,0.363302752,0.374311927,
0.385321101,0.396330275,0.405504587,0.414678899,0.423853211,0.433027523,
0.442201835,0.451376147,0.460550459,0.469724771,0.478899083,0.488073394,
0.497247706,0.506422018,0.51559633,0.524770642,0.533944954,0.541284404,
0.548623853,0.555963303,0.563302752,0.572477064,0.579816514,0.587155963,
0.594495413,0.601834862,0.609174312,0.616513761,0.623853211,0.631192661,
0.63853211,0.64587156,0.653211009,0.660550459,0.667889908,0.675229358,0.682568807,
0.689908257,0.697247706,0.704587156,0.711926606,0.719266055,0.726605505,
0.733944954,0.741284404,0.748623853,0.755963303,0.763302752,0.770642202,
0.777981651,0.785321101,0.79266055,0.8,0.809174312,0.814678899,0.820183486,
0.825688073,0.831192661,0.836697248,0.842201835,0.847706422,0.853211009,
0.858715596,0.864220183,0.869724771,0.875229358,0.880733945,0.886238532,
0.891743119,0.897247706,0.902752294,0.908256881,0.913761468,0.919266055,
0.924770642,0.930275229,0.935779817,0.941284404,0.946788991,0.952293578,
0.957798165,0.963302752,0.968807339,0.974311927,0.979816514,0.985321101,
0.990825688,1.),.UNSPECIFIED.);
#24475=B_SPLINE_CURVE_WITH_KNOTS('',5,(#283698,#283699,#283700,#283701,
#283702,#283703,#283704,#283705,#283706,#283707,#283708,#283709,#283710,
#283711,#283712,#283713,#283714,#283715,#283716,#283717,#283718,#283719,
#283720,#283721,#283722,#283723,#283724,#283725,#283726,#283727,#283728,
#283729,#283730,#283731,#283732,#283733,#283734,#283735,#283736,#283737,
#283738,#283739,#283740,#283741,#283742,#283743,#283744,#283745,#283746,
#283747,#283748,#283749,#283750,#283751,#283752,#283753,#283754,#283755,
#283756,#283757,#283758,#283759,#283760,#283761,#283762,#283763,#283764,
#283765,#283766,#283767,#283768,#283769,#283770,#283771,#283772,#283773,
#283774,#283775,#283776,#283777,#283778,#283779,#283780,#283781,#283782,
#283783,#283784,#283785,#283786,#283787,#283788,#283789,#283790,#283791,
#283792,#283793,#283794,#283795,#283796,#283797,#283798,#283799,#283800,
#283801,#283802,#283803,#283804,#283805,#283806,#283807,#283808,#283809,
#283810,#283811,#283812,#283813,#283814,#283815,#283816,#283817,#283818,
#283819,#283820,#283821,#283822,#283823,#283824,#283825,#283826,#283827,
#283828,#283829,#283830,#283831,#283832,#283833,#283834,#283835,#283836,
#283837,#283838,#283839,#283840,#283841,#283842,#283843,#283844,#283845,
#283846,#283847,#283848,#283849,#283850,#283851,#283852,#283853,#283854,
#283855,#283856,#283857,#283858,#283859,#283860,#283861,#283862,#283863,
#283864,#283865,#283866,#283867,#283868,#283869,#283870,#283871,#283872,
#283873,#283874,#283875,#283876,#283877,#283878,#283879,#283880,#283881,
#283882,#283883,#283884,#283885,#283886,#283887,#283888,#283889,#283890,
#283891,#283892,#283893,#283894,#283895,#283896,#283897,#283898,#283899,
#283900,#283901,#283902,#283903,#283904,#283905,#283906,#283907,#283908,
#283909,#283910,#283911,#283912,#283913,#283914,#283915,#283916,#283917,
#283918,#283919,#283920,#283921,#283922,#283923,#283924,#283925,#283926,
#283927,#283928,#283929,#283930,#283931,#283932,#283933,#283934,#283935,
#283936,#283937,#283938,#283939,#283940,#283941,#283942,#283943,#283944,
#283945,#283946,#283947,#283948,#283949,#283950,#283951,#283952,#283953,
#283954,#283955,#283956,#283957,#283958,#283959,#283960,#283961,#283962,
#283963,#283964,#283965,#283966,#283967,#283968,#283969,#283970,#283971,
#283972,#283973,#283974,#283975,#283976,#283977,#283978,#283979,#283980,
#283981,#283982,#283983,#283984,#283985,#283986,#283987,#283988,#283989,
#283990,#283991,#283992,#283993,#283994,#283995,#283996,#283997,#283998,
#283999,#284000,#284001,#284002,#284003,#284004,#284005,#284006,#284007,
#284008,#284009,#284010,#284011,#284012,#284013,#284014,#284015,#284016,
#284017,#284018,#284019,#284020,#284021,#284022,#284023,#284024,#284025,
#284026,#284027,#284028,#284029,#284030,#284031,#284032,#284033,#284034,
#284035,#284036,#284037,#284038,#284039,#284040,#284041,#284042,#284043,
#284044,#284045,#284046,#284047,#284048,#284049,#284050,#284051,#284052,
#284053,#284054,#284055,#284056,#284057,#284058,#284059,#284060,#284061,
#284062,#284063,#284064,#284065,#284066,#284067,#284068,#284069,#284070,
#284071,#284072,#284073,#284074,#284075,#284076,#284077,#284078,#284079,
#284080,#284081,#284082,#284083,#284084,#284085,#284086,#284087,#284088,
#284089,#284090,#284091,#284092,#284093,#284094,#284095,#284096,#284097,
#284098,#284099,#284100,#284101,#284102,#284103,#284104,#284105,#284106,
#284107,#284108,#284109,#284110,#284111,#284112,#284113,#284114,#284115,
#284116,#284117,#284118,#284119,#284120,#284121,#284122,#284123,#284124,
#284125,#284126,#284127,#284128,#284129,#284130,#284131,#284132,#284133,
#284134,#284135,#284136,#284137,#284138,#284139,#284140,#284141,#284142,
#284143,#284144,#284145,#284146,#284147,#284148,#284149,#284150,#284151,
#284152,#284153,#284154,#284155,#284156,#284157,#284158,#284159,#284160,
#284161,#284162,#284163,#284164,#284165,#284166,#284167,#284168,#284169),
 .UNSPECIFIED.,.F.,.F.,(6,1,1,1,1,1,1,1,1,1,1,1,1,1,1,1,1,1,1,1,1,1,1,1,
1,1,1,1,1,1,1,1,1,1,1,1,1,1,1,1,1,1,1,1,1,1,1,1,1,1,1,1,1,1,1,1,1,1,1,1,
1,1,1,1,1,1,1,1,1,1,1,1,1,1,1,1,1,1,1,1,1,1,1,1,1,1,1,1,1,1,1,1,1,1,1,1,
1,1,1,1,1,1,1,1,1,1,1,1,1,1,1,1,1,1,1,1,1,1,1,1,1,1,1,1,1,1,1,1,1,1,1,1,
1,1,1,1,1,1,1,1,1,1,1,1,1,1,1,1,1,1,1,1,1,1,1,1,1,1,1,1,1,1,1,1,1,1,1,1,
1,1,1,1,1,1,1,1,1,1,1,1,1,1,1,1,1,1,1,1,1,1,1,1,1,1,1,1,1,1,1,1,1,1,1,1,
1,1,1,1,1,1,1,1,1,1,1,1,1,1,1,1,1,1,1,1,1,1,1,1,1,1,1,1,1,1,1,1,1,1,1,1,
1,1,1,1,1,1,1,1,1,1,1,1,1,1,1,1,1,1,1,1,1,1,1,1,1,1,1,1,1,1,1,1,1,1,1,1,
1,1,1,1,1,1,1,1,1,1,1,1,1,1,1,1,1,1,1,1,1,1,1,1,1,1,1,1,1,1,1,1,1,1,1,1,
1,1,1,1,1,1,1,1,1,1,1,1,1,1,1,1,1,1,1,1,1,1,1,1,1,1,1,1,1,1,1,1,1,1,1,1,
1,1,1,1,1,1,1,1,1,1,1,1,1,1,1,1,1,1,1,1,1,1,1,1,1,1,1,1,1,1,1,1,1,1,1,1,
1,1,1,1,1,1,1,1,1,1,1,1,1,1,1,1,1,1,1,1,1,1,1,1,1,1,1,1,1,1,1,1,1,1,1,1,
1,1,1,1,1,1,1,1,1,1,1,1,1,1,1,1,1,1,1,1,1,1,1,1,1,1,1,1,1,1,1,1,1,1,1,1,
1,1,1,1,1,1,1,1,1,1,1,6),(-1.,-0.998165138,-0.996330275,-0.994495413,-0.99266055,
-0.990825688,-0.988990826,-0.987155963,-0.985321101,-0.983486239,-0.981651376,
-0.979816514,-0.977981651,-0.976146789,-0.974311927,-0.972477064,-0.970642202,
-0.968807339,-0.966972477,-0.965137615,-0.963302752,-0.96146789,-0.959633028,
-0.957798165,-0.955963303,-0.95412844,-0.952293578,-0.950458716,-0.948623853,
-0.946788991,-0.944954128,-0.943119266,-0.941284404,-0.939449541,-0.937614679,
-0.935779817,-0.933944954,-0.932110092,-0.930275229,-0.928440367,-0.926605505,
-0.924770642,-0.92293578,-0.921100917,-0.919266055,-0.917431193,-0.91559633,
-0.913761468,-0.911926606,-0.910091743,-0.908256881,-0.906422018,-0.904587156,
-0.902752294,-0.900917431,-0.899082569,-0.897247706,-0.895412844,-0.893577982,
-0.891743119,-0.889908257,-0.888073394,-0.886238532,-0.88440367,-0.882568807,
-0.880733945,-0.878899083,-0.87706422,-0.875229358,-0.873394495,-0.871559633,
-0.869724771,-0.867889908,-0.866055046,-0.864220183,-0.862385321,-0.860550459,
-0.858715596,-0.856880734,-0.855045872,-0.853211009,-0.851376147,-0.849541284,
-0.847706422,-0.84587156,-0.844036697,-0.842201835,-0.840366972,-0.83853211,
-0.836697248,-0.834862385,-0.833027523,-0.831192661,-0.829357798,-0.827522936,
-0.825688073,-0.823853211,-0.822018349,-0.820183486,-0.818348624,-0.816513761,
-0.814678899,-0.812844037,-0.811009174,-0.809174312,-0.80733945,-0.805504587,
-0.803669725,-0.801834862,-0.8,-0.798165138,-0.796330275,-0.794495413,-0.79266055,
-0.790825688,-0.788990826,-0.787155963,-0.785321101,-0.783486239,-0.781651376,
-0.779816514,-0.777981651,-0.776146789,-0.774311927,-0.772477064,-0.770642202,
-0.768807339,-0.766972477,-0.765137615,-0.763302752,-0.76146789,-0.759633028,
-0.757798165,-0.755963303,-0.75412844,-0.752293578,-0.750458716,-0.748623853,
-0.746788991,-0.744954128,-0.743119266,-0.741284404,-0.739449541,-0.737614679,
-0.735779817,-0.733944954,-0.732110092,-0.730275229,-0.728440367,-0.726605505,
-0.724770642,-0.72293578,-0.721100917,-0.719266055,-0.717431193,-0.71559633,
-0.713761468,-0.711926606,-0.710091743,-0.708256881,-0.706422018,-0.704587156,
-0.702752294,-0.700917431,-0.699082569,-0.697247706,-0.695412844,-0.693577982,
-0.691743119,-0.689908257,-0.688073394,-0.686238532,-0.68440367,-0.682568807,
-0.680733945,-0.678899083,-0.67706422,-0.675229358,-0.673394495,-0.671559633,
-0.669724771,-0.667889908,-0.666055046,-0.664220183,-0.662385321,-0.660550459,
-0.658715596,-0.656880734,-0.655045872,-0.653211009,-0.651376147,-0.649541284,
-0.647706422,-0.64587156,-0.644036697,-0.642201835,-0.640366972,-0.63853211,
-0.636697248,-0.634862385,-0.633027523,-0.631192661,-0.629357798,-0.627522936,
-0.625688073,-0.623853211,-0.622018349,-0.620183486,-0.618348624,-0.616513761,
-0.614678899,-0.612844037,-0.611009174,-0.609174312,-0.60733945,-0.605504587,
-0.603669725,-0.601834862,-0.6,-0.598165138,-0.596330275,-0.594495413,-0.59266055,
-0.590825688,-0.588990826,-0.587155963,-0.585321101,-0.583486239,-0.581651376,
-0.579816514,-0.577981651,-0.576146789,-0.574311927,-0.572477064,-0.570642202,
-0.568807339,-0.566972477,-0.565137615,-0.563302752,-0.56146789,-0.559633028,
-0.557798165,-0.555963303,-0.55412844,-0.552293578,-0.550458716,-0.548623853,
-0.546788991,-0.544954128,-0.543119266,-0.541284404,-0.539449541,-0.537614679,
-0.535779817,-0.533944954,-0.532110092,-0.530275229,-0.528440367,-0.526605505,
-0.524770642,-0.52293578,-0.521100917,-0.519266055,-0.517431193,-0.51559633,
-0.513761468,-0.511926606,-0.510091743,-0.508256881,-0.506422018,-0.504587156,
-0.502752294,-0.500917431,-0.499082569,-0.497247706,-0.495412844,-0.493577982,
-0.491743119,-0.489908257,-0.488073394,-0.486238532,-0.48440367,-0.482568807,
-0.480733945,-0.478899083,-0.47706422,-0.475229358,-0.473394495,-0.471559633,
-0.469724771,-0.467889908,-0.466055046,-0.464220183,-0.462385321,-0.460550459,
-0.458715596,-0.456880734,-0.455045872,-0.453211009,-0.451376147,-0.449541284,
-0.447706422,-0.44587156,-0.444036697,-0.442201835,-0.440366972,-0.43853211,
-0.436697248,-0.434862385,-0.433027523,-0.431192661,-0.429357798,-0.427522936,
-0.425688073,-0.423853211,-0.422018349,-0.420183486,-0.418348624,-0.416513761,
-0.414678899,-0.412844037,-0.411009174,-0.409174312,-0.40733945,-0.405504587,
-0.403669725,-0.401834862,-0.4,-0.398165138,-0.396330275,-0.394495413,-0.39266055,
-0.390825688,-0.388990826,-0.387155963,-0.385321101,-0.383486239,-0.381651376,
-0.379816514,-0.377981651,-0.376146789,-0.374311927,-0.372477064,-0.370642202,
-0.368807339,-0.366972477,-0.365137615,-0.363302752,-0.36146789,-0.359633028,
-0.357798165,-0.355963303,-0.35412844,-0.352293578,-0.350458716,-0.348623853,
-0.346788991,-0.344954128,-0.343119266,-0.341284404,-0.339449541,-0.337614679,
-0.335779817,-0.333944954,-0.332110092,-0.330275229,-0.328440367,-0.326605505,
-0.324770642,-0.32293578,-0.321100917,-0.319266055,-0.317431193,-0.31559633,
-0.313761468,-0.311926606,-0.310091743,-0.308256881,-0.306422018,-0.304587156,
-0.302752294,-0.300917431,-0.299082569,-0.297247706,-0.295412844,-0.293577982,
-0.291743119,-0.289908257,-0.288073394,-0.286238532,-0.28440367,-0.282568807,
-0.280733945,-0.278899083,-0.27706422,-0.275229358,-0.273394495,-0.271559633,
-0.269724771,-0.267889908,-0.266055046,-0.264220183,-0.262385321,-0.260550459,
-0.258715596,-0.256880734,-0.255045872,-0.253211009,-0.251376147,-0.249541284,
-0.247706422,-0.24587156,-0.244036697,-0.242201835,-0.240366972,-0.23853211,
-0.236697248,-0.234862385,-0.233027523,-0.231192661,-0.229357798,-0.227522936,
-0.225688073,-0.223853211,-0.222018349,-0.220183486,-0.218348624,-0.216513761,
-0.214678899,-0.212844037,-0.211009174,-0.209174312,-0.20733945,-0.205504587,
-0.203669725,-0.201834862,-0.2,-0.198165138,-0.196330275,-0.194495413,-0.19266055,
-0.190825688,-0.188990826,-0.187155963,-0.185321101,-0.183486239,-0.181651376,
-0.179816514,-0.177981651,-0.176146789,-0.174311927,-0.172477064,-0.170642202,
-0.168807339,-0.166972477,-0.165137615,-0.163302752,-0.16146789,-0.159633028,
-0.157798165,-0.155963303,-0.15412844,-0.152293578,-0.150458716,-0.148623853,
-0.146788991,-0.144954128,-0.143172102),.UNSPECIFIED.);
#24476=B_SPLINE_CURVE_WITH_KNOTS('',5,(#284170,#284171,#284172,#284173,
#284174,#284175,#284176,#284177,#284178,#284179,#284180,#284181,#284182,
#284183,#284184,#284185,#284186,#284187,#284188,#284189,#284190,#284191,
#284192,#284193,#284194,#284195,#284196,#284197,#284198,#284199,#284200,
#284201,#284202,#284203,#284204,#284205,#284206,#284207,#284208,#284209,
#284210,#284211,#284212,#284213,#284214,#284215,#284216,#284217,#284218,
#284219,#284220,#284221,#284222,#284223,#284224,#284225,#284226,#284227,
#284228,#284229,#284230,#284231,#284232,#284233,#284234,#284235,#284236,
#284237,#284238,#284239,#284240,#284241,#284242,#284243,#284244,#284245,
#284246,#284247,#284248,#284249,#284250,#284251,#284252,#284253,#284254,
#284255,#284256,#284257,#284258,#284259,#284260,#284261,#284262,#284263,
#284264,#284265,#284266,#284267,#284268,#284269,#284270,#284271,#284272,
#284273,#284274,#284275,#284276,#284277,#284278,#284279,#284280,#284281,
#284282,#284283,#284284,#284285,#284286,#284287,#284288,#284289,#284290,
#284291,#284292,#284293,#284294,#284295,#284296,#284297,#284298,#284299,
#284300,#284301,#284302,#284303,#284304,#284305,#284306,#284307,#284308,
#284309,#284310,#284311,#284312,#284313,#284314,#284315,#284316,#284317,
#284318,#284319,#284320,#284321,#284322,#284323,#284324,#284325,#284326,
#284327,#284328,#284329,#284330,#284331,#284332,#284333,#284334,#284335,
#284336,#284337,#284338,#284339,#284340,#284341,#284342,#284343,#284344,
#284345,#284346,#284347,#284348,#284349,#284350,#284351,#284352,#284353,
#284354,#284355,#284356,#284357,#284358,#284359,#284360,#284361,#284362,
#284363,#284364,#284365,#284366,#284367,#284368,#284369,#284370,#284371,
#284372,#284373,#284374,#284375,#284376,#284377,#284378,#284379,#284380,
#284381,#284382,#284383,#284384,#284385,#284386,#284387,#284388,#284389,
#284390,#284391,#284392,#284393,#284394,#284395,#284396,#284397,#284398,
#284399,#284400,#284401,#284402,#284403,#284404,#284405,#284406,#284407,
#284408,#284409,#284410,#284411,#284412,#284413,#284414,#284415,#284416,
#284417,#284418,#284419,#284420,#284421,#284422,#284423,#284424,#284425,
#284426,#284427,#284428,#284429,#284430,#284431,#284432,#284433,#284434,
#284435,#284436,#284437,#284438,#284439,#284440,#284441,#284442,#284443,
#284444,#284445,#284446,#284447,#284448,#284449,#284450,#284451,#284452,
#284453,#284454,#284455,#284456,#284457,#284458,#284459,#284460,#284461,
#284462,#284463,#284464,#284465,#284466,#284467,#284468,#284469,#284470,
#284471,#284472,#284473,#284474,#284475,#284476,#284477,#284478,#284479,
#284480,#284481,#284482,#284483,#284484,#284485,#284486,#284487,#284488,
#284489,#284490,#284491,#284492,#284493,#284494,#284495,#284496,#284497,
#284498,#284499,#284500,#284501,#284502,#284503,#284504,#284505,#284506,
#284507,#284508,#284509,#284510,#284511,#284512,#284513,#284514,#284515,
#284516,#284517,#284518,#284519,#284520,#284521,#284522,#284523,#284524,
#284525,#284526,#284527,#284528,#284529,#284530,#284531,#284532,#284533,
#284534,#284535,#284536,#284537,#284538,#284539,#284540,#284541,#284542,
#284543,#284544,#284545,#284546,#284547,#284548,#284549,#284550,#284551,
#284552,#284553,#284554,#284555,#284556,#284557,#284558,#284559,#284560,
#284561,#284562,#284563,#284564,#284565,#284566,#284567,#284568,#284569,
#284570,#284571,#284572,#284573,#284574,#284575,#284576,#284577,#284578,
#284579,#284580,#284581,#284582,#284583,#284584,#284585,#284586,#284587,
#284588,#284589,#284590,#284591,#284592,#284593,#284594,#284595,#284596,
#284597,#284598,#284599,#284600,#284601,#284602,#284603,#284604,#284605,
#284606,#284607,#284608,#284609,#284610,#284611,#284612,#284613,#284614,
#284615,#284616,#284617,#284618,#284619,#284620,#284621,#284622,#284623,
#284624,#284625,#284626,#284627,#284628,#284629,#284630,#284631,#284632,
#284633,#284634,#284635,#284636,#284637,#284638,#284639,#284640,#284641),
 .UNSPECIFIED.,.F.,.F.,(6,1,1,1,1,1,1,1,1,1,1,1,1,1,1,1,1,1,1,1,1,1,1,1,
1,1,1,1,1,1,1,1,1,1,1,1,1,1,1,1,1,1,1,1,1,1,1,1,1,1,1,1,1,1,1,1,1,1,1,1,
1,1,1,1,1,1,1,1,1,1,1,1,1,1,1,1,1,1,1,1,1,1,1,1,1,1,1,1,1,1,1,1,1,1,1,1,
1,1,1,1,1,1,1,1,1,1,1,1,1,1,1,1,1,1,1,1,1,1,1,1,1,1,1,1,1,1,1,1,1,1,1,1,
1,1,1,1,1,1,1,1,1,1,1,1,1,1,1,1,1,1,1,1,1,1,1,1,1,1,1,1,1,1,1,1,1,1,1,1,
1,1,1,1,1,1,1,1,1,1,1,1,1,1,1,1,1,1,1,1,1,1,1,1,1,1,1,1,1,1,1,1,1,1,1,1,
1,1,1,1,1,1,1,1,1,1,1,1,1,1,1,1,1,1,1,1,1,1,1,1,1,1,1,1,1,1,1,1,1,1,1,1,
1,1,1,1,1,1,1,1,1,1,1,1,1,1,1,1,1,1,1,1,1,1,1,1,1,1,1,1,1,1,1,1,1,1,1,1,
1,1,1,1,1,1,1,1,1,1,1,1,1,1,1,1,1,1,1,1,1,1,1,1,1,1,1,1,1,1,1,1,1,1,1,1,
1,1,1,1,1,1,1,1,1,1,1,1,1,1,1,1,1,1,1,1,1,1,1,1,1,1,1,1,1,1,1,1,1,1,1,1,
1,1,1,1,1,1,1,1,1,1,1,1,1,1,1,1,1,1,1,1,1,1,1,1,1,1,1,1,1,1,1,1,1,1,1,1,
1,1,1,1,1,1,1,1,1,1,1,1,1,1,1,1,1,1,1,1,1,1,1,1,1,1,1,1,1,1,1,1,1,1,1,1,
1,1,1,1,1,1,1,1,1,1,1,1,1,1,1,1,1,1,1,1,1,1,1,1,1,1,1,1,1,1,1,1,1,1,1,1,
1,1,1,1,1,1,1,1,1,1,1,6),(0.143172102,0.144954128,0.146788991,0.148623853,
0.150458716,0.152293578,0.15412844,0.155963303,0.157798165,0.159633028,
0.16146789,0.163302752,0.165137615,0.166972477,0.168807339,0.170642202,
0.172477064,0.174311927,0.176146789,0.177981651,0.179816514,0.181651376,
0.183486239,0.185321101,0.187155963,0.188990826,0.190825688,0.19266055,
0.194495413,0.196330275,0.198165138,0.2,0.201834862,0.203669725,0.205504587,
0.20733945,0.209174312,0.211009174,0.212844037,0.214678899,0.216513761,
0.218348624,0.220183486,0.222018349,0.223853211,0.225688073,0.227522936,
0.229357798,0.231192661,0.233027523,0.234862385,0.236697248,0.23853211,
0.240366972,0.242201835,0.244036697,0.24587156,0.247706422,0.249541284,
0.251376147,0.253211009,0.255045872,0.256880734,0.258715596,0.260550459,
0.262385321,0.264220183,0.266055046,0.267889908,0.269724771,0.271559633,
0.273394495,0.275229358,0.27706422,0.278899083,0.280733945,0.282568807,
0.28440367,0.286238532,0.288073394,0.289908257,0.291743119,0.293577982,
0.295412844,0.297247706,0.299082569,0.300917431,0.302752294,0.304587156,
0.306422018,0.308256881,0.310091743,0.311926606,0.313761468,0.31559633,
0.317431193,0.319266055,0.321100917,0.32293578,0.324770642,0.326605505,
0.328440367,0.330275229,0.332110092,0.333944954,0.335779817,0.337614679,
0.339449541,0.341284404,0.343119266,0.344954128,0.346788991,0.348623853,
0.350458716,0.352293578,0.35412844,0.355963303,0.357798165,0.359633028,
0.36146789,0.363302752,0.365137615,0.366972477,0.368807339,0.370642202,
0.372477064,0.374311927,0.376146789,0.377981651,0.379816514,0.381651376,
0.383486239,0.385321101,0.387155963,0.388990826,0.390825688,0.39266055,
0.394495413,0.396330275,0.398165138,0.4,0.401834862,0.403669725,0.405504587,
0.40733945,0.409174312,0.411009174,0.412844037,0.414678899,0.416513761,
0.418348624,0.420183486,0.422018349,0.423853211,0.425688073,0.427522936,
0.429357798,0.431192661,0.433027523,0.434862385,0.436697248,0.43853211,
0.440366972,0.442201835,0.444036697,0.44587156,0.447706422,0.449541284,
0.451376147,0.453211009,0.455045872,0.456880734,0.458715596,0.460550459,
0.462385321,0.464220183,0.466055046,0.467889908,0.469724771,0.471559633,
0.473394495,0.475229358,0.47706422,0.478899083,0.480733945,0.482568807,
0.48440367,0.486238532,0.488073394,0.489908257,0.491743119,0.493577982,
0.495412844,0.497247706,0.499082569,0.500917431,0.502752294,0.504587156,
0.506422018,0.508256881,0.510091743,0.511926606,0.513761468,0.51559633,
0.517431193,0.519266055,0.521100917,0.52293578,0.524770642,0.526605505,
0.528440367,0.530275229,0.532110092,0.533944954,0.535779817,0.537614679,
0.539449541,0.541284404,0.543119266,0.544954128,0.546788991,0.548623853,
0.550458716,0.552293578,0.55412844,0.555963303,0.557798165,0.559633028,
0.56146789,0.563302752,0.565137615,0.566972477,0.568807339,0.570642202,
0.572477064,0.574311927,0.576146789,0.577981651,0.579816514,0.581651376,
0.583486239,0.585321101,0.587155963,0.588990826,0.590825688,0.59266055,
0.594495413,0.596330275,0.598165138,0.6,0.601834862,0.603669725,0.605504587,
0.60733945,0.609174312,0.611009174,0.612844037,0.614678899,0.616513761,
0.618348624,0.620183486,0.622018349,0.623853211,0.625688073,0.627522936,
0.629357798,0.631192661,0.633027523,0.634862385,0.636697248,0.63853211,
0.640366972,0.642201835,0.644036697,0.64587156,0.647706422,0.649541284,
0.651376147,0.653211009,0.655045872,0.656880734,0.658715596,0.660550459,
0.662385321,0.664220183,0.666055046,0.667889908,0.669724771,0.671559633,
0.673394495,0.675229358,0.67706422,0.678899083,0.680733945,0.682568807,
0.68440367,0.686238532,0.688073394,0.689908257,0.691743119,0.693577982,
0.695412844,0.697247706,0.699082569,0.700917431,0.702752294,0.704587156,
0.706422018,0.708256881,0.710091743,0.711926606,0.713761468,0.71559633,
0.717431193,0.719266055,0.721100917,0.72293578,0.724770642,0.726605505,
0.728440367,0.730275229,0.732110092,0.733944954,0.735779817,0.737614679,
0.739449541,0.741284404,0.743119266,0.744954128,0.746788991,0.748623853,
0.750458716,0.752293578,0.75412844,0.755963303,0.757798165,0.759633028,
0.76146789,0.763302752,0.765137615,0.766972477,0.768807339,0.770642202,
0.772477064,0.774311927,0.776146789,0.777981651,0.779816514,0.781651376,
0.783486239,0.785321101,0.787155963,0.788990826,0.790825688,0.79266055,
0.794495413,0.796330275,0.798165138,0.8,0.801834862,0.803669725,0.805504587,
0.80733945,0.809174312,0.811009174,0.812844037,0.814678899,0.816513761,
0.818348624,0.820183486,0.822018349,0.823853211,0.825688073,0.827522936,
0.829357798,0.831192661,0.833027523,0.834862385,0.836697248,0.83853211,
0.840366972,0.842201835,0.844036697,0.84587156,0.847706422,0.849541284,
0.851376147,0.853211009,0.855045872,0.856880734,0.858715596,0.860550459,
0.862385321,0.864220183,0.866055046,0.867889908,0.869724771,0.871559633,
0.873394495,0.875229358,0.87706422,0.878899083,0.880733945,0.882568807,
0.88440367,0.886238532,0.888073394,0.889908257,0.891743119,0.893577982,
0.895412844,0.897247706,0.899082569,0.900917431,0.902752294,0.904587156,
0.906422018,0.908256881,0.910091743,0.911926606,0.913761468,0.91559633,
0.917431193,0.919266055,0.921100917,0.92293578,0.924770642,0.926605505,
0.928440367,0.930275229,0.932110092,0.933944954,0.935779817,0.937614679,
0.939449541,0.941284404,0.943119266,0.944954128,0.946788991,0.948623853,
0.950458716,0.952293578,0.95412844,0.955963303,0.957798165,0.959633028,
0.96146789,0.963302752,0.965137615,0.966972477,0.968807339,0.970642202,
0.972477064,0.974311927,0.976146789,0.977981651,0.979816514,0.981651376,
0.983486239,0.985321101,0.987155963,0.988990826,0.990825688,0.99266055,
0.994495413,0.996330275,0.998165138,1.),.UNSPECIFIED.);
#24477=B_SPLINE_CURVE_WITH_KNOTS('',5,(#285586,#285587,#285588,#285589,
#285590,#285591,#285592,#285593,#285594,#285595,#285596,#285597,#285598,
#285599,#285600,#285601,#285602,#285603,#285604,#285605,#285606,#285607,
#285608,#285609,#285610,#285611,#285612,#285613,#285614,#285615,#285616,
#285617,#285618,#285619,#285620,#285621,#285622,#285623,#285624,#285625,
#285626,#285627,#285628,#285629,#285630,#285631,#285632,#285633,#285634,
#285635,#285636,#285637,#285638,#285639,#285640,#285641,#285642,#285643,
#285644,#285645,#285646,#285647,#285648,#285649,#285650,#285651,#285652,
#285653,#285654,#285655,#285656,#285657,#285658,#285659,#285660,#285661,
#285662,#285663,#285664,#285665,#285666,#285667,#285668,#285669,#285670,
#285671,#285672,#285673,#285674,#285675,#285676,#285677,#285678,#285679,
#285680,#285681,#285682,#285683,#285684,#285685,#285686,#285687,#285688,
#285689,#285690,#285691,#285692,#285693,#285694,#285695,#285696,#285697,
#285698,#285699,#285700,#285701,#285702,#285703,#285704,#285705,#285706,
#285707,#285708,#285709,#285710,#285711,#285712,#285713,#285714,#285715,
#285716,#285717,#285718,#285719,#285720,#285721,#285722,#285723,#285724,
#285725,#285726,#285727,#285728,#285729,#285730,#285731,#285732,#285733,
#285734,#285735,#285736,#285737,#285738,#285739,#285740,#285741,#285742,
#285743,#285744,#285745,#285746,#285747,#285748,#285749,#285750,#285751,
#285752,#285753,#285754,#285755,#285756,#285757,#285758,#285759,#285760,
#285761,#285762,#285763,#285764,#285765,#285766,#285767,#285768,#285769,
#285770,#285771,#285772,#285773,#285774,#285775,#285776,#285777,#285778,
#285779,#285780,#285781,#285782,#285783,#285784,#285785,#285786,#285787,
#285788,#285789,#285790,#285791,#285792,#285793,#285794,#285795,#285796,
#285797,#285798,#285799,#285800,#285801,#285802,#285803,#285804,#285805,
#285806,#285807,#285808,#285809,#285810,#285811,#285812,#285813,#285814,
#285815,#285816,#285817,#285818,#285819,#285820,#285821,#285822,#285823,
#285824,#285825,#285826,#285827,#285828,#285829,#285830,#285831,#285832,
#285833,#285834,#285835,#285836,#285837,#285838,#285839,#285840,#285841,
#285842,#285843,#285844,#285845,#285846,#285847,#285848,#285849,#285850,
#285851,#285852,#285853,#285854,#285855,#285856,#285857,#285858,#285859,
#285860,#285861,#285862,#285863,#285864,#285865,#285866,#285867,#285868,
#285869,#285870,#285871,#285872,#285873,#285874,#285875,#285876,#285877,
#285878,#285879,#285880,#285881,#285882,#285883,#285884,#285885,#285886,
#285887,#285888,#285889,#285890,#285891,#285892,#285893,#285894,#285895,
#285896,#285897,#285898,#285899,#285900,#285901,#285902,#285903,#285904,
#285905,#285906,#285907,#285908,#285909,#285910,#285911,#285912,#285913,
#285914,#285915,#285916,#285917,#285918,#285919,#285920,#285921,#285922,
#285923,#285924,#285925,#285926,#285927,#285928,#285929,#285930,#285931,
#285932,#285933,#285934,#285935,#285936,#285937,#285938,#285939,#285940,
#285941,#285942,#285943,#285944,#285945,#285946,#285947,#285948,#285949,
#285950,#285951,#285952,#285953,#285954,#285955,#285956,#285957,#285958,
#285959,#285960,#285961,#285962,#285963,#285964,#285965,#285966,#285967,
#285968,#285969,#285970,#285971,#285972,#285973,#285974,#285975,#285976,
#285977,#285978,#285979,#285980,#285981,#285982,#285983,#285984,#285985,
#285986,#285987,#285988,#285989,#285990,#285991,#285992,#285993,#285994,
#285995,#285996,#285997,#285998,#285999,#286000,#286001,#286002,#286003,
#286004,#286005,#286006,#286007,#286008,#286009,#286010,#286011,#286012,
#286013,#286014,#286015,#286016,#286017,#286018,#286019,#286020,#286021,
#286022,#286023,#286024,#286025,#286026,#286027,#286028,#286029,#286030,
#286031,#286032,#286033,#286034,#286035,#286036,#286037,#286038,#286039,
#286040,#286041,#286042,#286043,#286044,#286045,#286046,#286047,#286048,
#286049,#286050,#286051,#286052,#286053,#286054,#286055,#286056,#286057),
 .UNSPECIFIED.,.F.,.F.,(6,1,1,1,1,1,1,1,1,1,1,1,1,1,1,1,1,1,1,1,1,1,1,1,
1,1,1,1,1,1,1,1,1,1,1,1,1,1,1,1,1,1,1,1,1,1,1,1,1,1,1,1,1,1,1,1,1,1,1,1,
1,1,1,1,1,1,1,1,1,1,1,1,1,1,1,1,1,1,1,1,1,1,1,1,1,1,1,1,1,1,1,1,1,1,1,1,
1,1,1,1,1,1,1,1,1,1,1,1,1,1,1,1,1,1,1,1,1,1,1,1,1,1,1,1,1,1,1,1,1,1,1,1,
1,1,1,1,1,1,1,1,1,1,1,1,1,1,1,1,1,1,1,1,1,1,1,1,1,1,1,1,1,1,1,1,1,1,1,1,
1,1,1,1,1,1,1,1,1,1,1,1,1,1,1,1,1,1,1,1,1,1,1,1,1,1,1,1,1,1,1,1,1,1,1,1,
1,1,1,1,1,1,1,1,1,1,1,1,1,1,1,1,1,1,1,1,1,1,1,1,1,1,1,1,1,1,1,1,1,1,1,1,
1,1,1,1,1,1,1,1,1,1,1,1,1,1,1,1,1,1,1,1,1,1,1,1,1,1,1,1,1,1,1,1,1,1,1,1,
1,1,1,1,1,1,1,1,1,1,1,1,1,1,1,1,1,1,1,1,1,1,1,1,1,1,1,1,1,1,1,1,1,1,1,1,
1,1,1,1,1,1,1,1,1,1,1,1,1,1,1,1,1,1,1,1,1,1,1,1,1,1,1,1,1,1,1,1,1,1,1,1,
1,1,1,1,1,1,1,1,1,1,1,1,1,1,1,1,1,1,1,1,1,1,1,1,1,1,1,1,1,1,1,1,1,1,1,1,
1,1,1,1,1,1,1,1,1,1,1,1,1,1,1,1,1,1,1,1,1,1,1,1,1,1,1,1,1,1,1,1,1,1,1,1,
1,1,1,1,1,1,1,1,1,1,1,1,1,1,1,1,1,1,1,1,1,1,1,1,1,1,1,1,1,1,1,1,1,1,1,1,
1,1,1,1,1,1,1,1,1,1,1,6),(0.143172102,0.144954128,0.146788991,0.148623853,
0.150458716,0.152293578,0.15412844,0.155963303,0.157798165,0.159633028,
0.16146789,0.163302752,0.165137615,0.166972477,0.168807339,0.170642202,
0.172477064,0.174311927,0.176146789,0.177981651,0.179816514,0.181651376,
0.183486239,0.185321101,0.187155963,0.188990826,0.190825688,0.19266055,
0.194495413,0.196330275,0.198165138,0.2,0.201834862,0.203669725,0.205504587,
0.20733945,0.209174312,0.211009174,0.212844037,0.214678899,0.216513761,
0.218348624,0.220183486,0.222018349,0.223853211,0.225688073,0.227522936,
0.229357798,0.231192661,0.233027523,0.234862385,0.236697248,0.23853211,
0.240366972,0.242201835,0.244036697,0.24587156,0.247706422,0.249541284,
0.251376147,0.253211009,0.255045872,0.256880734,0.258715596,0.260550459,
0.262385321,0.264220183,0.266055046,0.267889908,0.269724771,0.271559633,
0.273394495,0.275229358,0.27706422,0.278899083,0.280733945,0.282568807,
0.28440367,0.286238532,0.288073394,0.289908257,0.291743119,0.293577982,
0.295412844,0.297247706,0.299082569,0.300917431,0.302752294,0.304587156,
0.306422018,0.308256881,0.310091743,0.311926606,0.313761468,0.31559633,
0.317431193,0.319266055,0.321100917,0.32293578,0.324770642,0.326605505,
0.328440367,0.330275229,0.332110092,0.333944954,0.335779817,0.337614679,
0.339449541,0.341284404,0.343119266,0.344954128,0.346788991,0.348623853,
0.350458716,0.352293578,0.35412844,0.355963303,0.357798165,0.359633028,
0.36146789,0.363302752,0.365137615,0.366972477,0.368807339,0.370642202,
0.372477064,0.374311927,0.376146789,0.377981651,0.379816514,0.381651376,
0.383486239,0.385321101,0.387155963,0.388990826,0.390825688,0.39266055,
0.394495413,0.396330275,0.398165138,0.4,0.401834862,0.403669725,0.405504587,
0.40733945,0.409174312,0.411009174,0.412844037,0.414678899,0.416513761,
0.418348624,0.420183486,0.422018349,0.423853211,0.425688073,0.427522936,
0.429357798,0.431192661,0.433027523,0.434862385,0.436697248,0.43853211,
0.440366972,0.442201835,0.444036697,0.44587156,0.447706422,0.449541284,
0.451376147,0.453211009,0.455045872,0.456880734,0.458715596,0.460550459,
0.462385321,0.464220183,0.466055046,0.467889908,0.469724771,0.471559633,
0.473394495,0.475229358,0.47706422,0.478899083,0.480733945,0.482568807,
0.48440367,0.486238532,0.488073394,0.489908257,0.491743119,0.493577982,
0.495412844,0.497247706,0.499082569,0.500917431,0.502752294,0.504587156,
0.506422018,0.508256881,0.510091743,0.511926606,0.513761468,0.51559633,
0.517431193,0.519266055,0.521100917,0.52293578,0.524770642,0.526605505,
0.528440367,0.530275229,0.532110092,0.533944954,0.535779817,0.537614679,
0.539449541,0.541284404,0.543119266,0.544954128,0.546788991,0.548623853,
0.550458716,0.552293578,0.55412844,0.555963303,0.557798165,0.559633028,
0.56146789,0.563302752,0.565137615,0.566972477,0.568807339,0.570642202,
0.572477064,0.574311927,0.576146789,0.577981651,0.579816514,0.581651376,
0.583486239,0.585321101,0.587155963,0.588990826,0.590825688,0.59266055,
0.594495413,0.596330275,0.598165138,0.6,0.601834862,0.603669725,0.605504587,
0.60733945,0.609174312,0.611009174,0.612844037,0.614678899,0.616513761,
0.618348624,0.620183486,0.622018349,0.623853211,0.625688073,0.627522936,
0.629357798,0.631192661,0.633027523,0.634862385,0.636697248,0.63853211,
0.640366972,0.642201835,0.644036697,0.64587156,0.647706422,0.649541284,
0.651376147,0.653211009,0.655045872,0.656880734,0.658715596,0.660550459,
0.662385321,0.664220183,0.666055046,0.667889908,0.669724771,0.671559633,
0.673394495,0.675229358,0.67706422,0.678899083,0.680733945,0.682568807,
0.68440367,0.686238532,0.688073394,0.689908257,0.691743119,0.693577982,
0.695412844,0.697247706,0.699082569,0.700917431,0.702752294,0.704587156,
0.706422018,0.708256881,0.710091743,0.711926606,0.713761468,0.71559633,
0.717431193,0.719266055,0.721100917,0.72293578,0.724770642,0.726605505,
0.728440367,0.730275229,0.732110092,0.733944954,0.735779817,0.737614679,
0.739449541,0.741284404,0.743119266,0.744954128,0.746788991,0.748623853,
0.750458716,0.752293578,0.75412844,0.755963303,0.757798165,0.759633028,
0.76146789,0.763302752,0.765137615,0.766972477,0.768807339,0.770642202,
0.772477064,0.774311927,0.776146789,0.777981651,0.779816514,0.781651376,
0.783486239,0.785321101,0.787155963,0.788990826,0.790825688,0.79266055,
0.794495413,0.796330275,0.798165138,0.8,0.801834862,0.803669725,0.805504587,
0.80733945,0.809174312,0.811009174,0.812844037,0.814678899,0.816513761,
0.818348624,0.820183486,0.822018349,0.823853211,0.825688073,0.827522936,
0.829357798,0.831192661,0.833027523,0.834862385,0.836697248,0.83853211,
0.840366972,0.842201835,0.844036697,0.84587156,0.847706422,0.849541284,
0.851376147,0.853211009,0.855045872,0.856880734,0.858715596,0.860550459,
0.862385321,0.864220183,0.866055046,0.867889908,0.869724771,0.871559633,
0.873394495,0.875229358,0.87706422,0.878899083,0.880733945,0.882568807,
0.88440367,0.886238532,0.888073394,0.889908257,0.891743119,0.893577982,
0.895412844,0.897247706,0.899082569,0.900917431,0.902752294,0.904587156,
0.906422018,0.908256881,0.910091743,0.911926606,0.913761468,0.91559633,
0.917431193,0.919266055,0.921100917,0.92293578,0.924770642,0.926605505,
0.928440367,0.930275229,0.932110092,0.933944954,0.935779817,0.937614679,
0.939449541,0.941284404,0.943119266,0.944954128,0.946788991,0.948623853,
0.950458716,0.952293578,0.95412844,0.955963303,0.957798165,0.959633028,
0.96146789,0.963302752,0.965137615,0.966972477,0.968807339,0.970642202,
0.972477064,0.974311927,0.976146789,0.977981651,0.979816514,0.981651376,
0.983486239,0.985321101,0.987155963,0.988990826,0.990825688,0.99266055,
0.994495413,0.996330275,0.998165138,1.),.UNSPECIFIED.);
#24478=B_SPLINE_CURVE_WITH_KNOTS('',5,(#286058,#286059,#286060,#286061,
#286062,#286063,#286064,#286065,#286066,#286067,#286068,#286069,#286070,
#286071,#286072,#286073,#286074,#286075,#286076,#286077,#286078,#286079,
#286080,#286081,#286082,#286083,#286084,#286085,#286086,#286087,#286088,
#286089,#286090,#286091,#286092,#286093,#286094,#286095,#286096,#286097,
#286098,#286099,#286100,#286101,#286102,#286103,#286104,#286105,#286106,
#286107,#286108,#286109,#286110,#286111,#286112,#286113,#286114,#286115,
#286116,#286117,#286118,#286119,#286120,#286121,#286122,#286123,#286124,
#286125,#286126,#286127,#286128,#286129,#286130,#286131,#286132,#286133,
#286134,#286135,#286136,#286137,#286138,#286139,#286140,#286141,#286142,
#286143,#286144,#286145,#286146,#286147,#286148,#286149,#286150,#286151,
#286152,#286153,#286154,#286155,#286156,#286157,#286158,#286159,#286160,
#286161,#286162,#286163,#286164,#286165,#286166,#286167,#286168,#286169,
#286170,#286171,#286172,#286173,#286174,#286175,#286176,#286177,#286178,
#286179,#286180,#286181,#286182,#286183,#286184,#286185,#286186,#286187,
#286188,#286189,#286190,#286191,#286192,#286193,#286194,#286195,#286196,
#286197,#286198,#286199,#286200,#286201,#286202,#286203,#286204,#286205,
#286206,#286207,#286208,#286209,#286210,#286211,#286212,#286213,#286214,
#286215,#286216,#286217,#286218,#286219,#286220,#286221,#286222,#286223,
#286224,#286225,#286226,#286227,#286228,#286229,#286230,#286231,#286232,
#286233,#286234,#286235,#286236,#286237,#286238,#286239,#286240,#286241,
#286242,#286243,#286244,#286245,#286246,#286247,#286248,#286249,#286250,
#286251,#286252,#286253,#286254,#286255,#286256,#286257,#286258,#286259,
#286260,#286261,#286262,#286263,#286264,#286265,#286266,#286267,#286268,
#286269,#286270,#286271,#286272,#286273,#286274,#286275,#286276,#286277,
#286278,#286279,#286280,#286281,#286282,#286283,#286284,#286285,#286286,
#286287,#286288,#286289,#286290,#286291,#286292,#286293,#286294,#286295,
#286296,#286297,#286298,#286299,#286300,#286301,#286302,#286303,#286304,
#286305,#286306,#286307,#286308,#286309,#286310,#286311,#286312,#286313,
#286314,#286315,#286316,#286317,#286318,#286319,#286320,#286321,#286322,
#286323,#286324,#286325,#286326,#286327,#286328,#286329,#286330,#286331,
#286332,#286333,#286334,#286335,#286336,#286337,#286338,#286339,#286340,
#286341,#286342,#286343,#286344,#286345,#286346,#286347,#286348,#286349,
#286350,#286351,#286352,#286353,#286354,#286355,#286356,#286357,#286358,
#286359,#286360,#286361,#286362,#286363,#286364,#286365,#286366,#286367,
#286368,#286369,#286370,#286371,#286372,#286373,#286374,#286375,#286376,
#286377,#286378,#286379,#286380,#286381,#286382,#286383,#286384,#286385,
#286386,#286387,#286388,#286389,#286390,#286391,#286392,#286393,#286394,
#286395,#286396,#286397,#286398,#286399,#286400,#286401,#286402,#286403,
#286404,#286405,#286406,#286407,#286408,#286409,#286410,#286411,#286412,
#286413,#286414,#286415,#286416,#286417,#286418,#286419,#286420,#286421,
#286422,#286423,#286424,#286425,#286426,#286427,#286428,#286429,#286430,
#286431,#286432,#286433,#286434,#286435,#286436,#286437,#286438,#286439,
#286440,#286441,#286442,#286443,#286444,#286445,#286446,#286447,#286448,
#286449,#286450,#286451,#286452,#286453,#286454,#286455,#286456,#286457,
#286458,#286459,#286460,#286461,#286462,#286463,#286464,#286465,#286466,
#286467,#286468,#286469,#286470,#286471,#286472,#286473,#286474,#286475,
#286476,#286477,#286478,#286479,#286480,#286481,#286482,#286483,#286484,
#286485,#286486,#286487,#286488,#286489,#286490,#286491,#286492,#286493,
#286494,#286495,#286496,#286497,#286498,#286499,#286500,#286501,#286502,
#286503,#286504,#286505,#286506,#286507,#286508,#286509,#286510,#286511,
#286512,#286513,#286514,#286515,#286516,#286517,#286518,#286519,#286520,
#286521,#286522,#286523,#286524,#286525,#286526,#286527,#286528,#286529),
 .UNSPECIFIED.,.F.,.F.,(6,1,1,1,1,1,1,1,1,1,1,1,1,1,1,1,1,1,1,1,1,1,1,1,
1,1,1,1,1,1,1,1,1,1,1,1,1,1,1,1,1,1,1,1,1,1,1,1,1,1,1,1,1,1,1,1,1,1,1,1,
1,1,1,1,1,1,1,1,1,1,1,1,1,1,1,1,1,1,1,1,1,1,1,1,1,1,1,1,1,1,1,1,1,1,1,1,
1,1,1,1,1,1,1,1,1,1,1,1,1,1,1,1,1,1,1,1,1,1,1,1,1,1,1,1,1,1,1,1,1,1,1,1,
1,1,1,1,1,1,1,1,1,1,1,1,1,1,1,1,1,1,1,1,1,1,1,1,1,1,1,1,1,1,1,1,1,1,1,1,
1,1,1,1,1,1,1,1,1,1,1,1,1,1,1,1,1,1,1,1,1,1,1,1,1,1,1,1,1,1,1,1,1,1,1,1,
1,1,1,1,1,1,1,1,1,1,1,1,1,1,1,1,1,1,1,1,1,1,1,1,1,1,1,1,1,1,1,1,1,1,1,1,
1,1,1,1,1,1,1,1,1,1,1,1,1,1,1,1,1,1,1,1,1,1,1,1,1,1,1,1,1,1,1,1,1,1,1,1,
1,1,1,1,1,1,1,1,1,1,1,1,1,1,1,1,1,1,1,1,1,1,1,1,1,1,1,1,1,1,1,1,1,1,1,1,
1,1,1,1,1,1,1,1,1,1,1,1,1,1,1,1,1,1,1,1,1,1,1,1,1,1,1,1,1,1,1,1,1,1,1,1,
1,1,1,1,1,1,1,1,1,1,1,1,1,1,1,1,1,1,1,1,1,1,1,1,1,1,1,1,1,1,1,1,1,1,1,1,
1,1,1,1,1,1,1,1,1,1,1,1,1,1,1,1,1,1,1,1,1,1,1,1,1,1,1,1,1,1,1,1,1,1,1,1,
1,1,1,1,1,1,1,1,1,1,1,1,1,1,1,1,1,1,1,1,1,1,1,1,1,1,1,1,1,1,1,1,1,1,1,1,
1,1,1,1,1,1,1,1,1,1,1,6),(0.143172102,0.144954128,0.146788991,0.148623853,
0.150458716,0.152293578,0.15412844,0.155963303,0.157798165,0.159633028,
0.16146789,0.163302752,0.165137615,0.166972477,0.168807339,0.170642202,
0.172477064,0.174311927,0.176146789,0.177981651,0.179816514,0.181651376,
0.183486239,0.185321101,0.187155963,0.188990826,0.190825688,0.19266055,
0.194495413,0.196330275,0.198165138,0.2,0.201834862,0.203669725,0.205504587,
0.20733945,0.209174312,0.211009174,0.212844037,0.214678899,0.216513761,
0.218348624,0.220183486,0.222018349,0.223853211,0.225688073,0.227522936,
0.229357798,0.231192661,0.233027523,0.234862385,0.236697248,0.23853211,
0.240366972,0.242201835,0.244036697,0.24587156,0.247706422,0.249541284,
0.251376147,0.253211009,0.255045872,0.256880734,0.258715596,0.260550459,
0.262385321,0.264220183,0.266055046,0.267889908,0.269724771,0.271559633,
0.273394495,0.275229358,0.27706422,0.278899083,0.280733945,0.282568807,
0.28440367,0.286238532,0.288073394,0.289908257,0.291743119,0.293577982,
0.295412844,0.297247706,0.299082569,0.300917431,0.302752294,0.304587156,
0.306422018,0.308256881,0.310091743,0.311926606,0.313761468,0.31559633,
0.317431193,0.319266055,0.321100917,0.32293578,0.324770642,0.326605505,
0.328440367,0.330275229,0.332110092,0.333944954,0.335779817,0.337614679,
0.339449541,0.341284404,0.343119266,0.344954128,0.346788991,0.348623853,
0.350458716,0.352293578,0.35412844,0.355963303,0.357798165,0.359633028,
0.36146789,0.363302752,0.365137615,0.366972477,0.368807339,0.370642202,
0.372477064,0.374311927,0.376146789,0.377981651,0.379816514,0.381651376,
0.383486239,0.385321101,0.387155963,0.388990826,0.390825688,0.39266055,
0.394495413,0.396330275,0.398165138,0.4,0.401834862,0.403669725,0.405504587,
0.40733945,0.409174312,0.411009174,0.412844037,0.414678899,0.416513761,
0.418348624,0.420183486,0.422018349,0.423853211,0.425688073,0.427522936,
0.429357798,0.431192661,0.433027523,0.434862385,0.436697248,0.43853211,
0.440366972,0.442201835,0.444036697,0.44587156,0.447706422,0.449541284,
0.451376147,0.453211009,0.455045872,0.456880734,0.458715596,0.460550459,
0.462385321,0.464220183,0.466055046,0.467889908,0.469724771,0.471559633,
0.473394495,0.475229358,0.47706422,0.478899083,0.480733945,0.482568807,
0.48440367,0.486238532,0.488073394,0.489908257,0.491743119,0.493577982,
0.495412844,0.497247706,0.499082569,0.500917431,0.502752294,0.504587156,
0.506422018,0.508256881,0.510091743,0.511926606,0.513761468,0.51559633,
0.517431193,0.519266055,0.521100917,0.52293578,0.524770642,0.526605505,
0.528440367,0.530275229,0.532110092,0.533944954,0.535779817,0.537614679,
0.539449541,0.541284404,0.543119266,0.544954128,0.546788991,0.548623853,
0.550458716,0.552293578,0.55412844,0.555963303,0.557798165,0.559633028,
0.56146789,0.563302752,0.565137615,0.566972477,0.568807339,0.570642202,
0.572477064,0.574311927,0.576146789,0.577981651,0.579816514,0.581651376,
0.583486239,0.585321101,0.587155963,0.588990826,0.590825688,0.59266055,
0.594495413,0.596330275,0.598165138,0.6,0.601834862,0.603669725,0.605504587,
0.60733945,0.609174312,0.611009174,0.612844037,0.614678899,0.616513761,
0.618348624,0.620183486,0.622018349,0.623853211,0.625688073,0.627522936,
0.629357798,0.631192661,0.633027523,0.634862385,0.636697248,0.63853211,
0.640366972,0.642201835,0.644036697,0.64587156,0.647706422,0.649541284,
0.651376147,0.653211009,0.655045872,0.656880734,0.658715596,0.660550459,
0.662385321,0.664220183,0.666055046,0.667889908,0.669724771,0.671559633,
0.673394495,0.675229358,0.67706422,0.678899083,0.680733945,0.682568807,
0.68440367,0.686238532,0.688073394,0.689908257,0.691743119,0.693577982,
0.695412844,0.697247706,0.699082569,0.700917431,0.702752294,0.704587156,
0.706422018,0.708256881,0.710091743,0.711926606,0.713761468,0.71559633,
0.717431193,0.719266055,0.721100917,0.72293578,0.724770642,0.726605505,
0.728440367,0.730275229,0.732110092,0.733944954,0.735779817,0.737614679,
0.739449541,0.741284404,0.743119266,0.744954128,0.746788991,0.748623853,
0.750458716,0.752293578,0.75412844,0.755963303,0.757798165,0.759633028,
0.76146789,0.763302752,0.765137615,0.766972477,0.768807339,0.770642202,
0.772477064,0.774311927,0.776146789,0.777981651,0.779816514,0.781651376,
0.783486239,0.785321101,0.787155963,0.788990826,0.790825688,0.79266055,
0.794495413,0.796330275,0.798165138,0.8,0.801834862,0.803669725,0.805504587,
0.80733945,0.809174312,0.811009174,0.812844037,0.814678899,0.816513761,
0.818348624,0.820183486,0.822018349,0.823853211,0.825688073,0.827522936,
0.829357798,0.831192661,0.833027523,0.834862385,0.836697248,0.83853211,
0.840366972,0.842201835,0.844036697,0.84587156,0.847706422,0.849541284,
0.851376147,0.853211009,0.855045872,0.856880734,0.858715596,0.860550459,
0.862385321,0.864220183,0.866055046,0.867889908,0.869724771,0.871559633,
0.873394495,0.875229358,0.87706422,0.878899083,0.880733945,0.882568807,
0.88440367,0.886238532,0.888073394,0.889908257,0.891743119,0.893577982,
0.895412844,0.897247706,0.899082569,0.900917431,0.902752294,0.904587156,
0.906422018,0.908256881,0.910091743,0.911926606,0.913761468,0.91559633,
0.917431193,0.919266055,0.921100917,0.92293578,0.924770642,0.926605505,
0.928440367,0.930275229,0.932110092,0.933944954,0.935779817,0.937614679,
0.939449541,0.941284404,0.943119266,0.944954128,0.946788991,0.948623853,
0.950458716,0.952293578,0.95412844,0.955963303,0.957798165,0.959633028,
0.96146789,0.963302752,0.965137615,0.966972477,0.968807339,0.970642202,
0.972477064,0.974311927,0.976146789,0.977981651,0.979816514,0.981651376,
0.983486239,0.985321101,0.987155963,0.988990826,0.990825688,0.99266055,
0.994495413,0.996330275,0.998165138,1.),.UNSPECIFIED.);
#24479=B_SPLINE_CURVE_WITH_KNOTS('',5,(#287489,#287490,#287491,#287492,
#287493,#287494,#287495,#287496,#287497,#287498,#287499,#287500,#287501,
#287502,#287503,#287504,#287505,#287506,#287507,#287508,#287509,#287510,
#287511,#287512,#287513,#287514,#287515,#287516,#287517,#287518,#287519,
#287520,#287521,#287522,#287523,#287524,#287525,#287526,#287527,#287528,
#287529,#287530,#287531,#287532,#287533,#287534,#287535,#287536,#287537,
#287538,#287539,#287540,#287541,#287542,#287543,#287544,#287545,#287546,
#287547,#287548,#287549,#287550,#287551,#287552,#287553,#287554,#287555,
#287556,#287557,#287558,#287559,#287560,#287561,#287562,#287563,#287564,
#287565,#287566,#287567,#287568,#287569,#287570,#287571,#287572,#287573,
#287574,#287575,#287576,#287577,#287578,#287579,#287580,#287581,#287582,
#287583,#287584,#287585,#287586,#287587,#287588,#287589,#287590,#287591,
#287592,#287593,#287594,#287595,#287596,#287597,#287598,#287599,#287600,
#287601,#287602,#287603,#287604,#287605,#287606,#287607,#287608,#287609,
#287610,#287611,#287612,#287613,#287614,#287615,#287616,#287617,#287618,
#287619,#287620,#287621,#287622,#287623,#287624,#287625,#287626,#287627,
#287628,#287629,#287630,#287631,#287632,#287633,#287634,#287635,#287636,
#287637,#287638,#287639,#287640,#287641,#287642,#287643,#287644,#287645,
#287646,#287647,#287648,#287649,#287650,#287651,#287652,#287653,#287654,
#287655,#287656,#287657,#287658,#287659,#287660,#287661,#287662,#287663,
#287664,#287665,#287666,#287667,#287668,#287669,#287670,#287671,#287672,
#287673,#287674,#287675,#287676,#287677,#287678,#287679,#287680,#287681,
#287682,#287683,#287684,#287685,#287686,#287687,#287688,#287689,#287690,
#287691,#287692,#287693,#287694,#287695,#287696,#287697,#287698,#287699,
#287700,#287701,#287702,#287703,#287704,#287705,#287706,#287707,#287708,
#287709,#287710,#287711,#287712,#287713,#287714,#287715,#287716,#287717,
#287718,#287719,#287720,#287721,#287722,#287723,#287724,#287725,#287726,
#287727,#287728,#287729,#287730,#287731,#287732,#287733,#287734,#287735,
#287736,#287737,#287738,#287739,#287740,#287741,#287742,#287743,#287744,
#287745,#287746,#287747,#287748,#287749,#287750,#287751,#287752,#287753,
#287754,#287755,#287756,#287757,#287758,#287759,#287760,#287761,#287762,
#287763,#287764,#287765,#287766,#287767,#287768,#287769,#287770,#287771,
#287772,#287773,#287774,#287775,#287776,#287777,#287778,#287779,#287780,
#287781,#287782,#287783,#287784,#287785,#287786,#287787,#287788,#287789,
#287790,#287791,#287792,#287793,#287794,#287795,#287796,#287797,#287798,
#287799,#287800,#287801,#287802,#287803,#287804,#287805,#287806,#287807,
#287808,#287809,#287810,#287811,#287812,#287813,#287814,#287815,#287816,
#287817,#287818,#287819,#287820,#287821,#287822,#287823,#287824,#287825,
#287826,#287827,#287828,#287829,#287830,#287831,#287832,#287833,#287834,
#287835,#287836,#287837,#287838,#287839,#287840,#287841,#287842,#287843,
#287844,#287845,#287846,#287847,#287848,#287849,#287850,#287851,#287852,
#287853,#287854,#287855,#287856,#287857,#287858,#287859,#287860,#287861,
#287862,#287863,#287864,#287865,#287866,#287867,#287868,#287869,#287870,
#287871,#287872,#287873,#287874,#287875,#287876,#287877,#287878,#287879,
#287880,#287881,#287882,#287883,#287884,#287885,#287886,#287887,#287888,
#287889,#287890,#287891,#287892,#287893,#287894,#287895,#287896,#287897,
#287898,#287899,#287900,#287901,#287902,#287903,#287904,#287905,#287906,
#287907,#287908,#287909,#287910,#287911,#287912,#287913,#287914,#287915,
#287916,#287917,#287918,#287919,#287920,#287921,#287922,#287923,#287924,
#287925,#287926,#287927,#287928,#287929,#287930,#287931,#287932,#287933,
#287934,#287935,#287936,#287937,#287938,#287939,#287940,#287941,#287942,
#287943,#287944,#287945,#287946,#287947,#287948,#287949,#287950,#287951,
#287952,#287953,#287954,#287955,#287956,#287957,#287958,#287959),
 .UNSPECIFIED.,.F.,.F.,(6,1,1,1,1,1,1,1,1,1,1,1,1,1,1,1,1,1,1,1,1,1,1,1,
1,1,1,1,1,1,1,1,1,1,1,1,1,1,1,1,1,1,1,1,1,1,1,1,1,1,1,1,1,1,1,1,1,1,1,1,
1,1,1,1,1,1,1,1,1,1,1,1,1,1,1,1,1,1,1,1,1,1,1,1,1,1,1,1,1,1,1,1,1,1,1,1,
1,1,1,1,1,1,1,1,1,1,1,1,1,1,1,1,1,1,1,1,1,1,1,1,1,1,1,1,1,1,1,1,1,1,1,1,
1,1,1,1,1,1,1,1,1,1,1,1,1,1,1,1,1,1,1,1,1,1,1,1,1,1,1,1,1,1,1,1,1,1,1,1,
1,1,1,1,1,1,1,1,1,1,1,1,1,1,1,1,1,1,1,1,1,1,1,1,1,1,1,1,1,1,1,1,1,1,1,1,
1,1,1,1,1,1,1,1,1,1,1,1,1,1,1,1,1,1,1,1,1,1,1,1,1,1,1,1,1,1,1,1,1,1,1,1,
1,1,1,1,1,1,1,1,1,1,1,1,1,1,1,1,1,1,1,1,1,1,1,1,1,1,1,1,1,1,1,1,1,1,1,1,
1,1,1,1,1,1,1,1,1,1,1,1,1,1,1,1,1,1,1,1,1,1,1,1,1,1,1,1,1,1,1,1,1,1,1,1,
1,1,1,1,1,1,1,1,1,1,1,1,1,1,1,1,1,1,1,1,1,1,1,1,1,1,1,1,1,1,1,1,1,1,1,1,
1,1,1,1,1,1,1,1,1,1,1,1,1,1,1,1,1,1,1,1,1,1,1,1,1,1,1,1,1,1,1,1,1,1,1,1,
1,1,1,1,1,1,1,1,1,1,1,1,1,1,1,1,1,1,1,1,1,1,1,1,1,1,1,1,1,1,1,1,1,1,1,1,
1,1,1,1,1,1,1,1,1,1,1,1,1,1,1,1,1,1,1,1,1,1,1,1,1,1,1,1,1,1,1,1,1,1,1,1,
1,1,1,1,1,1,1,1,1,1,6),(0.143172102,0.144954128,0.146788991,0.148623853,
0.150458716,0.152293578,0.15412844,0.155963303,0.157798165,0.159633028,
0.16146789,0.163302752,0.165137615,0.166972477,0.168807339,0.170642202,
0.172477064,0.174311927,0.176146789,0.177981651,0.179816514,0.181651376,
0.183486239,0.185321101,0.187155963,0.188990826,0.190825688,0.19266055,
0.194495413,0.196330275,0.198165138,0.2,0.201834862,0.203669725,0.205504587,
0.20733945,0.209174312,0.211009174,0.212844037,0.214678899,0.216513761,
0.218348624,0.220183486,0.222018349,0.223853211,0.225688073,0.227522936,
0.229357798,0.231192661,0.233027523,0.234862385,0.236697248,0.23853211,
0.240366972,0.242201835,0.244036697,0.24587156,0.247706422,0.249541284,
0.251376147,0.253211009,0.255045872,0.256880734,0.258715596,0.260550459,
0.262385321,0.264220183,0.266055046,0.267889908,0.269724771,0.271559633,
0.273394495,0.275229358,0.27706422,0.278899083,0.280733945,0.282568807,
0.28440367,0.286238532,0.288073394,0.289908257,0.291743119,0.293577982,
0.295412844,0.297247706,0.299082569,0.300917431,0.302752294,0.304587156,
0.306422018,0.308256881,0.310091743,0.311926606,0.313761468,0.31559633,
0.317431193,0.319266055,0.321100917,0.32293578,0.324770642,0.326605505,
0.328440367,0.330275229,0.332110092,0.333944954,0.335779817,0.337614679,
0.339449541,0.341284404,0.343119266,0.344954128,0.346788991,0.348623853,
0.350458716,0.352293578,0.35412844,0.355963303,0.357798165,0.359633028,
0.36146789,0.363302752,0.365137615,0.366972477,0.368807339,0.370642202,
0.372477064,0.374311927,0.376146789,0.377981651,0.379816514,0.381651376,
0.383486239,0.385321101,0.387155963,0.388990826,0.390825688,0.39266055,
0.394495413,0.396330275,0.398165138,0.4,0.401834862,0.403669725,0.405504587,
0.40733945,0.409174312,0.411009174,0.412844037,0.414678899,0.416513761,
0.418348624,0.420183486,0.422018349,0.423853211,0.425688073,0.427522936,
0.429357798,0.431192661,0.433027523,0.434862385,0.436697248,0.43853211,
0.440366972,0.442201835,0.444036697,0.44587156,0.447706422,0.449541284,
0.451376147,0.453211009,0.455045872,0.456880734,0.458715596,0.460550459,
0.462385321,0.464220183,0.466055046,0.467889908,0.469724771,0.471559633,
0.473394495,0.475229358,0.47706422,0.478899083,0.480733945,0.482568807,
0.48440367,0.486238532,0.488073394,0.489908257,0.491743119,0.493577982,
0.495412844,0.497247706,0.499082569,0.500917431,0.502752294,0.504587156,
0.506422018,0.508256881,0.510091743,0.511926606,0.513761468,0.51559633,
0.517431193,0.519266055,0.521100917,0.52293578,0.524770642,0.526605505,
0.528440367,0.530275229,0.532110092,0.533944954,0.535779817,0.537614679,
0.539449541,0.541284404,0.543119266,0.544954128,0.546788991,0.548623853,
0.550458716,0.552293578,0.55412844,0.555963303,0.557798165,0.559633028,
0.56146789,0.563302752,0.565137615,0.566972477,0.568807339,0.570642202,
0.572477064,0.574311927,0.576146789,0.577981651,0.579816514,0.581651376,
0.583486239,0.585321101,0.587155963,0.588990826,0.590825688,0.59266055,
0.594495413,0.596330275,0.598165138,0.6,0.601834862,0.603669725,0.605504587,
0.60733945,0.609174312,0.611009174,0.612844037,0.614678899,0.616513761,
0.618348624,0.620183486,0.622018349,0.623853211,0.625688073,0.627522936,
0.629357798,0.631192661,0.633027523,0.634862385,0.636697248,0.63853211,
0.640366972,0.642201835,0.644036697,0.64587156,0.647706422,0.649541284,
0.651376147,0.653211009,0.655045872,0.656880734,0.658715596,0.660550459,
0.662385321,0.664220183,0.666055046,0.667889908,0.669724771,0.673394495,
0.675229358,0.67706422,0.678899083,0.680733945,0.682568807,0.68440367,0.686238532,
0.688073394,0.689908257,0.691743119,0.693577982,0.695412844,0.697247706,
0.699082569,0.700917431,0.702752294,0.704587156,0.706422018,0.708256881,
0.710091743,0.711926606,0.713761468,0.71559633,0.717431193,0.719266055,
0.721100917,0.72293578,0.724770642,0.726605505,0.728440367,0.730275229,
0.732110092,0.733944954,0.735779817,0.737614679,0.739449541,0.741284404,
0.743119266,0.744954128,0.746788991,0.748623853,0.750458716,0.752293578,
0.75412844,0.755963303,0.757798165,0.759633028,0.76146789,0.763302752,0.765137615,
0.766972477,0.768807339,0.770642202,0.772477064,0.774311927,0.776146789,
0.777981651,0.779816514,0.781651376,0.783486239,0.785321101,0.787155963,
0.788990826,0.790825688,0.79266055,0.794495413,0.796330275,0.798165138,
0.8,0.801834862,0.803669725,0.805504587,0.80733945,0.809174312,0.811009174,
0.812844037,0.814678899,0.816513761,0.818348624,0.820183486,0.822018349,
0.823853211,0.825688073,0.827522936,0.829357798,0.831192661,0.833027523,
0.834862385,0.836697248,0.83853211,0.840366972,0.842201835,0.844036697,
0.84587156,0.847706422,0.849541284,0.851376147,0.853211009,0.855045872,
0.856880734,0.858715596,0.860550459,0.862385321,0.864220183,0.866055046,
0.867889908,0.869724771,0.871559633,0.873394495,0.875229358,0.87706422,
0.878899083,0.880733945,0.882568807,0.88440367,0.886238532,0.888073394,
0.889908257,0.891743119,0.893577982,0.895412844,0.897247706,0.899082569,
0.900917431,0.902752294,0.904587156,0.906422018,0.908256881,0.910091743,
0.911926606,0.913761468,0.91559633,0.917431193,0.919266055,0.921100917,
0.92293578,0.924770642,0.926605505,0.928440367,0.930275229,0.932110092,
0.933944954,0.935779817,0.937614679,0.939449541,0.941284404,0.943119266,
0.944954128,0.946788991,0.948623853,0.950458716,0.952293578,0.95412844,
0.955963303,0.957798165,0.959633028,0.96146789,0.963302752,0.965137615,
0.966972477,0.968807339,0.970642202,0.972477064,0.974311927,0.976146789,
0.977981651,0.979816514,0.981651376,0.983486239,0.985321101,0.987155963,
0.988990826,0.990825688,0.99266055,0.994495413,0.996330275,0.998165138,
1.),.UNSPECIFIED.);
#24480=B_SPLINE_CURVE_WITH_KNOTS('',5,(#287960,#287961,#287962,#287963,
#287964,#287965,#287966,#287967,#287968,#287969,#287970,#287971,#287972,
#287973,#287974,#287975,#287976,#287977,#287978,#287979,#287980,#287981,
#287982,#287983,#287984,#287985,#287986,#287987,#287988,#287989,#287990,
#287991,#287992,#287993,#287994,#287995,#287996,#287997,#287998,#287999,
#288000,#288001,#288002,#288003,#288004,#288005,#288006,#288007,#288008,
#288009,#288010,#288011,#288012,#288013,#288014,#288015,#288016,#288017,
#288018,#288019,#288020,#288021,#288022,#288023,#288024,#288025,#288026,
#288027,#288028,#288029,#288030,#288031,#288032,#288033,#288034,#288035,
#288036,#288037,#288038,#288039,#288040,#288041,#288042,#288043,#288044,
#288045,#288046,#288047,#288048,#288049,#288050,#288051,#288052,#288053,
#288054,#288055,#288056,#288057,#288058,#288059,#288060,#288061,#288062,
#288063,#288064,#288065,#288066,#288067,#288068,#288069,#288070,#288071,
#288072,#288073,#288074,#288075,#288076,#288077,#288078,#288079,#288080,
#288081,#288082,#288083,#288084,#288085,#288086,#288087,#288088,#288089,
#288090,#288091,#288092,#288093,#288094,#288095,#288096,#288097,#288098,
#288099,#288100,#288101,#288102,#288103,#288104,#288105,#288106,#288107,
#288108,#288109,#288110,#288111,#288112,#288113,#288114,#288115,#288116,
#288117,#288118,#288119,#288120,#288121,#288122,#288123,#288124,#288125,
#288126,#288127,#288128,#288129,#288130,#288131,#288132,#288133,#288134,
#288135,#288136,#288137,#288138,#288139,#288140,#288141,#288142,#288143,
#288144,#288145,#288146,#288147,#288148,#288149,#288150,#288151,#288152,
#288153,#288154,#288155,#288156,#288157,#288158,#288159,#288160,#288161,
#288162,#288163,#288164,#288165,#288166,#288167,#288168,#288169,#288170,
#288171,#288172,#288173,#288174,#288175,#288176,#288177,#288178,#288179,
#288180,#288181,#288182,#288183,#288184,#288185,#288186,#288187,#288188,
#288189,#288190,#288191,#288192,#288193,#288194,#288195,#288196,#288197,
#288198,#288199,#288200,#288201,#288202,#288203,#288204,#288205,#288206,
#288207,#288208,#288209,#288210,#288211,#288212,#288213,#288214,#288215,
#288216,#288217,#288218,#288219,#288220,#288221,#288222,#288223,#288224,
#288225,#288226,#288227,#288228,#288229,#288230,#288231,#288232,#288233,
#288234,#288235,#288236,#288237,#288238,#288239,#288240,#288241,#288242,
#288243,#288244,#288245,#288246,#288247,#288248,#288249,#288250,#288251,
#288252,#288253,#288254,#288255,#288256,#288257,#288258,#288259,#288260,
#288261,#288262,#288263,#288264,#288265,#288266,#288267,#288268,#288269,
#288270,#288271,#288272,#288273,#288274,#288275,#288276,#288277,#288278,
#288279,#288280,#288281,#288282,#288283,#288284,#288285,#288286,#288287,
#288288,#288289,#288290,#288291,#288292,#288293,#288294,#288295,#288296,
#288297,#288298,#288299,#288300,#288301,#288302,#288303,#288304,#288305,
#288306,#288307,#288308,#288309,#288310,#288311,#288312,#288313,#288314,
#288315,#288316,#288317,#288318,#288319,#288320,#288321,#288322,#288323,
#288324,#288325,#288326,#288327,#288328,#288329,#288330,#288331,#288332,
#288333,#288334,#288335,#288336,#288337,#288338,#288339,#288340,#288341,
#288342,#288343,#288344,#288345,#288346,#288347,#288348,#288349,#288350,
#288351,#288352,#288353,#288354,#288355,#288356,#288357,#288358,#288359,
#288360,#288361,#288362,#288363,#288364,#288365,#288366,#288367,#288368,
#288369,#288370,#288371,#288372,#288373,#288374,#288375,#288376,#288377,
#288378,#288379,#288380,#288381,#288382,#288383,#288384,#288385,#288386,
#288387,#288388,#288389,#288390,#288391,#288392,#288393,#288394,#288395,
#288396,#288397,#288398,#288399,#288400,#288401,#288402,#288403,#288404,
#288405,#288406,#288407,#288408,#288409,#288410,#288411,#288412,#288413,
#288414,#288415,#288416,#288417,#288418,#288419,#288420,#288421,#288422,
#288423,#288424,#288425,#288426,#288427,#288428,#288429,#288430),
 .UNSPECIFIED.,.F.,.F.,(6,1,1,1,1,1,1,1,1,1,1,1,1,1,1,1,1,1,1,1,1,1,1,1,
1,1,1,1,1,1,1,1,1,1,1,1,1,1,1,1,1,1,1,1,1,1,1,1,1,1,1,1,1,1,1,1,1,1,1,1,
1,1,1,1,1,1,1,1,1,1,1,1,1,1,1,1,1,1,1,1,1,1,1,1,1,1,1,1,1,1,1,1,1,1,1,1,
1,1,1,1,1,1,1,1,1,1,1,1,1,1,1,1,1,1,1,1,1,1,1,1,1,1,1,1,1,1,1,1,1,1,1,1,
1,1,1,1,1,1,1,1,1,1,1,1,1,1,1,1,1,1,1,1,1,1,1,1,1,1,1,1,1,1,1,1,1,1,1,1,
1,1,1,1,1,1,1,1,1,1,1,1,1,1,1,1,1,1,1,1,1,1,1,1,1,1,1,1,1,1,1,1,1,1,1,1,
1,1,1,1,1,1,1,1,1,1,1,1,1,1,1,1,1,1,1,1,1,1,1,1,1,1,1,1,1,1,1,1,1,1,1,1,
1,1,1,1,1,1,1,1,1,1,1,1,1,1,1,1,1,1,1,1,1,1,1,1,1,1,1,1,1,1,1,1,1,1,1,1,
1,1,1,1,1,1,1,1,1,1,1,1,1,1,1,1,1,1,1,1,1,1,1,1,1,1,1,1,1,1,1,1,1,1,1,1,
1,1,1,1,1,1,1,1,1,1,1,1,1,1,1,1,1,1,1,1,1,1,1,1,1,1,1,1,1,1,1,1,1,1,1,1,
1,1,1,1,1,1,1,1,1,1,1,1,1,1,1,1,1,1,1,1,1,1,1,1,1,1,1,1,1,1,1,1,1,1,1,1,
1,1,1,1,1,1,1,1,1,1,1,1,1,1,1,1,1,1,1,1,1,1,1,1,1,1,1,1,1,1,1,1,1,1,1,1,
1,1,1,1,1,1,1,1,1,1,1,1,1,1,1,1,1,1,1,1,1,1,1,1,1,1,1,1,1,1,1,1,1,1,1,1,
1,1,1,1,1,1,1,1,1,1,6),(0.143172102,0.144954128,0.146788991,0.148623853,
0.150458716,0.152293578,0.15412844,0.155963303,0.157798165,0.159633028,
0.16146789,0.163302752,0.165137615,0.166972477,0.168807339,0.170642202,
0.172477064,0.174311927,0.176146789,0.177981651,0.179816514,0.181651376,
0.183486239,0.185321101,0.187155963,0.188990826,0.190825688,0.19266055,
0.194495413,0.196330275,0.198165138,0.2,0.201834862,0.203669725,0.205504587,
0.20733945,0.209174312,0.211009174,0.212844037,0.214678899,0.216513761,
0.218348624,0.220183486,0.222018349,0.223853211,0.225688073,0.227522936,
0.229357798,0.231192661,0.233027523,0.234862385,0.236697248,0.23853211,
0.240366972,0.242201835,0.244036697,0.24587156,0.247706422,0.249541284,
0.251376147,0.253211009,0.255045872,0.256880734,0.258715596,0.260550459,
0.262385321,0.264220183,0.266055046,0.267889908,0.269724771,0.271559633,
0.273394495,0.275229358,0.27706422,0.278899083,0.280733945,0.282568807,
0.28440367,0.286238532,0.288073394,0.289908257,0.291743119,0.293577982,
0.295412844,0.297247706,0.299082569,0.300917431,0.302752294,0.304587156,
0.306422018,0.308256881,0.310091743,0.311926606,0.313761468,0.31559633,
0.317431193,0.319266055,0.321100917,0.32293578,0.324770642,0.326605505,
0.328440367,0.330275229,0.332110092,0.333944954,0.335779817,0.337614679,
0.339449541,0.341284404,0.343119266,0.344954128,0.346788991,0.348623853,
0.350458716,0.352293578,0.35412844,0.355963303,0.357798165,0.359633028,
0.36146789,0.363302752,0.365137615,0.366972477,0.368807339,0.370642202,
0.372477064,0.374311927,0.376146789,0.377981651,0.379816514,0.381651376,
0.383486239,0.385321101,0.387155963,0.388990826,0.390825688,0.39266055,
0.394495413,0.396330275,0.398165138,0.4,0.401834862,0.403669725,0.405504587,
0.40733945,0.409174312,0.411009174,0.412844037,0.414678899,0.416513761,
0.418348624,0.420183486,0.422018349,0.423853211,0.425688073,0.427522936,
0.429357798,0.431192661,0.433027523,0.434862385,0.436697248,0.43853211,
0.440366972,0.442201835,0.444036697,0.44587156,0.447706422,0.449541284,
0.451376147,0.453211009,0.455045872,0.456880734,0.458715596,0.460550459,
0.462385321,0.464220183,0.466055046,0.467889908,0.469724771,0.471559633,
0.473394495,0.475229358,0.47706422,0.478899083,0.480733945,0.482568807,
0.48440367,0.486238532,0.488073394,0.489908257,0.491743119,0.493577982,
0.495412844,0.497247706,0.499082569,0.500917431,0.502752294,0.504587156,
0.506422018,0.508256881,0.510091743,0.511926606,0.513761468,0.51559633,
0.517431193,0.519266055,0.521100917,0.52293578,0.524770642,0.526605505,
0.528440367,0.530275229,0.532110092,0.533944954,0.535779817,0.537614679,
0.539449541,0.541284404,0.543119266,0.544954128,0.546788991,0.548623853,
0.550458716,0.552293578,0.55412844,0.555963303,0.557798165,0.559633028,
0.56146789,0.563302752,0.565137615,0.566972477,0.568807339,0.570642202,
0.572477064,0.574311927,0.576146789,0.577981651,0.579816514,0.581651376,
0.583486239,0.585321101,0.587155963,0.588990826,0.590825688,0.59266055,
0.594495413,0.596330275,0.598165138,0.6,0.601834862,0.603669725,0.605504587,
0.60733945,0.609174312,0.611009174,0.612844037,0.614678899,0.616513761,
0.618348624,0.620183486,0.622018349,0.623853211,0.625688073,0.627522936,
0.629357798,0.631192661,0.633027523,0.634862385,0.636697248,0.63853211,
0.640366972,0.642201835,0.644036697,0.64587156,0.647706422,0.649541284,
0.651376147,0.653211009,0.655045872,0.656880734,0.658715596,0.660550459,
0.662385321,0.664220183,0.666055046,0.667889908,0.669724771,0.673394495,
0.675229358,0.67706422,0.678899083,0.680733945,0.682568807,0.68440367,0.686238532,
0.688073394,0.689908257,0.691743119,0.693577982,0.695412844,0.697247706,
0.699082569,0.700917431,0.702752294,0.704587156,0.706422018,0.708256881,
0.710091743,0.711926606,0.713761468,0.71559633,0.717431193,0.719266055,
0.721100917,0.72293578,0.724770642,0.726605505,0.728440367,0.730275229,
0.732110092,0.733944954,0.735779817,0.737614679,0.739449541,0.741284404,
0.743119266,0.744954128,0.746788991,0.748623853,0.750458716,0.752293578,
0.75412844,0.755963303,0.757798165,0.759633028,0.76146789,0.763302752,0.765137615,
0.766972477,0.768807339,0.770642202,0.772477064,0.774311927,0.776146789,
0.777981651,0.779816514,0.781651376,0.783486239,0.785321101,0.787155963,
0.788990826,0.790825688,0.79266055,0.794495413,0.796330275,0.798165138,
0.8,0.801834862,0.803669725,0.805504587,0.80733945,0.809174312,0.811009174,
0.812844037,0.814678899,0.816513761,0.818348624,0.820183486,0.822018349,
0.823853211,0.825688073,0.827522936,0.829357798,0.831192661,0.833027523,
0.834862385,0.836697248,0.83853211,0.840366972,0.842201835,0.844036697,
0.84587156,0.847706422,0.849541284,0.851376147,0.853211009,0.855045872,
0.856880734,0.858715596,0.860550459,0.862385321,0.864220183,0.866055046,
0.867889908,0.869724771,0.871559633,0.873394495,0.875229358,0.87706422,
0.878899083,0.880733945,0.882568807,0.88440367,0.886238532,0.888073394,
0.889908257,0.891743119,0.893577982,0.895412844,0.897247706,0.899082569,
0.900917431,0.902752294,0.904587156,0.906422018,0.908256881,0.910091743,
0.911926606,0.913761468,0.91559633,0.917431193,0.919266055,0.921100917,
0.92293578,0.924770642,0.926605505,0.928440367,0.930275229,0.932110092,
0.933944954,0.935779817,0.937614679,0.939449541,0.941284404,0.943119266,
0.944954128,0.946788991,0.948623853,0.950458716,0.952293578,0.95412844,
0.955963303,0.957798165,0.959633028,0.96146789,0.963302752,0.965137615,
0.966972477,0.968807339,0.970642202,0.972477064,0.974311927,0.976146789,
0.977981651,0.979816514,0.981651376,0.983486239,0.985321101,0.987155963,
0.988990826,0.990825688,0.99266055,0.994495413,0.996330275,0.998165138,
1.),.UNSPECIFIED.);
#24481=B_SPLINE_CURVE_WITH_KNOTS('',3,(#289378,#289379,#289380,#289381,
#289382,#289383,#289384,#289385,#289386,#289387,#289388,#289389,#289390,
#289391,#289392,#289393,#289394,#289395,#289396,#289397,#289398,#289399,
#289400,#289401,#289402,#289403,#289404,#289405,#289406,#289407,#289408,
#289409,#289410,#289411,#289412,#289413,#289414,#289415,#289416,#289417,
#289418,#289419,#289420,#289421,#289422,#289423,#289424,#289425,#289426,
#289427,#289428,#289429,#289430,#289431,#289432,#289433,#289434,#289435,
#289436,#289437,#289438,#289439,#289440,#289441,#289442,#289443,#289444,
#289445,#289446,#289447,#289448,#289449,#289450,#289451,#289452,#289453,
#289454,#289455,#289456,#289457,#289458,#289459,#289460,#289461,#289462,
#289463,#289464,#289465,#289466,#289467,#289468,#289469,#289470,#289471,
#289472,#289473,#289474,#289475,#289476,#289477,#289478,#289479,#289480,
#289481,#289482,#289483,#289484,#289485,#289486,#289487,#289488,#289489,
#289490,#289491,#289492,#289493,#289494,#289495,#289496,#289497,#289498,
#289499,#289500,#289501,#289502,#289503,#289504,#289505,#289506,#289507,
#289508,#289509,#289510,#289511,#289512,#289513,#289514,#289515,#289516,
#289517,#289518,#289519,#289520,#289521,#289522,#289523,#289524,#289525,
#289526,#289527,#289528,#289529,#289530,#289531,#289532,#289533,#289534,
#289535,#289536,#289537,#289538,#289539,#289540,#289541,#289542,#289543,
#289544,#289545,#289546,#289547,#289548,#289549,#289550,#289551,#289552,
#289553,#289554,#289555,#289556,#289557,#289558,#289559,#289560,#289561,
#289562,#289563,#289564,#289565,#289566,#289567,#289568,#289569,#289570,
#289571,#289572,#289573,#289574,#289575,#289576,#289577,#289578,#289579,
#289580,#289581,#289582,#289583,#289584,#289585,#289586,#289587,#289588,
#289589,#289590,#289591,#289592,#289593,#289594,#289595,#289596,#289597,
#289598,#289599,#289600,#289601,#289602,#289603,#289604,#289605,#289606,
#289607,#289608,#289609,#289610,#289611,#289612,#289613,#289614,#289615,
#289616,#289617,#289618,#289619,#289620,#289621,#289622,#289623,#289624,
#289625,#289626,#289627,#289628,#289629,#289630,#289631,#289632,#289633,
#289634,#289635,#289636,#289637,#289638,#289639,#289640,#289641,#289642,
#289643,#289644,#289645,#289646,#289647,#289648,#289649,#289650,#289651,
#289652,#289653,#289654,#289655,#289656,#289657,#289658,#289659,#289660,
#289661,#289662,#289663,#289664,#289665,#289666,#289667,#289668,#289669,
#289670,#289671,#289672,#289673,#289674,#289675,#289676,#289677,#289678,
#289679,#289680,#289681,#289682,#289683,#289684,#289685,#289686,#289687,
#289688,#289689,#289690,#289691,#289692,#289693,#289694,#289695,#289696,
#289697,#289698,#289699,#289700,#289701,#289702),.UNSPECIFIED.,.F.,.F.,
(4,3,3,3,3,3,3,3,3,3,3,3,3,3,3,3,3,3,3,3,3,3,3,3,3,3,3,3,3,3,3,3,3,3,3,
3,3,3,3,3,3,3,3,3,3,3,3,3,3,3,3,3,3,3,3,3,3,3,3,3,3,3,3,3,3,3,3,3,3,3,3,
3,3,3,3,3,3,3,3,3,3,3,3,3,3,3,3,3,3,3,3,3,3,3,3,3,3,3,3,3,3,3,3,3,3,3,3,
3,4),(-1.,-0.994495413,-0.988990826,-0.983486239,-0.977981651,-0.972477064,
-0.966972477,-0.959633028,-0.95412844,-0.948623853,-0.943119266,-0.937614679,
-0.932110092,-0.926605505,-0.921100917,-0.913761468,-0.908256881,-0.902752294,
-0.897247706,-0.891743119,-0.886238532,-0.880733945,-0.875229358,-0.867889908,
-0.862385321,-0.856880734,-0.851376147,-0.84587156,-0.840366972,-0.834862385,
-0.829357798,-0.823853211,-0.818348624,-0.812844037,-0.80733945,-0.798165138,
-0.790825688,-0.783486239,-0.776146789,-0.768807339,-0.76146789,-0.75412844,
-0.746788991,-0.737614679,-0.730275229,-0.72293578,-0.71559633,-0.708256881,
-0.700917431,-0.693577982,-0.686238532,-0.678899083,-0.671559633,-0.664220183,
-0.656880734,-0.649541284,-0.642201835,-0.634862385,-0.627522936,-0.620183486,
-0.611009174,-0.603669725,-0.596330275,-0.588990826,-0.581651376,-0.574311927,
-0.566972477,-0.559633028,-0.552293578,-0.544954128,-0.537614679,-0.530275229,
-0.521100917,-0.511926606,-0.502752294,-0.493577982,-0.482568807,-0.473394495,
-0.464220183,-0.455045872,-0.44587156,-0.436697248,-0.427522936,-0.418348624,
-0.409174312,-0.4,-0.390825688,-0.379816514,-0.368807339,-0.357798165,-0.346788991,
-0.335779817,-0.324770642,-0.313761468,-0.302752294,-0.291743119,-0.280733945,
-0.269724771,-0.258715596,-0.247706422,-0.234862385,-0.223853211,-0.212844037,
-0.201834862,-0.190825688,-0.179816514,-0.168807339,-0.157798165,-0.143172102),
 .UNSPECIFIED.);
#24482=B_SPLINE_CURVE_WITH_KNOTS('',3,(#289703,#289704,#289705,#289706,
#289707,#289708,#289709,#289710,#289711,#289712,#289713,#289714,#289715,
#289716,#289717,#289718,#289719,#289720,#289721,#289722,#289723,#289724,
#289725,#289726,#289727,#289728,#289729,#289730,#289731,#289732,#289733,
#289734,#289735,#289736,#289737,#289738,#289739,#289740,#289741,#289742,
#289743,#289744,#289745,#289746,#289747,#289748,#289749,#289750,#289751,
#289752,#289753,#289754,#289755,#289756,#289757,#289758,#289759,#289760,
#289761,#289762,#289763,#289764,#289765,#289766,#289767,#289768,#289769,
#289770,#289771,#289772,#289773,#289774,#289775,#289776,#289777,#289778,
#289779,#289780,#289781,#289782,#289783,#289784,#289785,#289786,#289787,
#289788,#289789,#289790,#289791,#289792,#289793,#289794,#289795,#289796,
#289797,#289798,#289799,#289800,#289801,#289802,#289803,#289804,#289805,
#289806,#289807,#289808,#289809,#289810,#289811,#289812,#289813,#289814,
#289815,#289816,#289817,#289818,#289819,#289820,#289821,#289822,#289823,
#289824,#289825,#289826,#289827,#289828,#289829,#289830,#289831,#289832,
#289833,#289834,#289835,#289836,#289837,#289838,#289839,#289840,#289841,
#289842,#289843,#289844,#289845,#289846,#289847,#289848,#289849,#289850,
#289851,#289852,#289853,#289854,#289855,#289856,#289857,#289858,#289859,
#289860,#289861,#289862,#289863,#289864,#289865,#289866,#289867,#289868,
#289869,#289870,#289871,#289872,#289873,#289874,#289875,#289876,#289877,
#289878,#289879,#289880,#289881,#289882,#289883,#289884,#289885,#289886,
#289887,#289888,#289889,#289890,#289891,#289892,#289893,#289894,#289895,
#289896,#289897,#289898,#289899,#289900,#289901,#289902,#289903,#289904,
#289905,#289906,#289907,#289908,#289909,#289910,#289911,#289912,#289913,
#289914,#289915,#289916,#289917,#289918,#289919,#289920,#289921,#289922,
#289923,#289924,#289925,#289926,#289927,#289928,#289929,#289930,#289931,
#289932,#289933,#289934,#289935,#289936,#289937,#289938,#289939,#289940,
#289941,#289942,#289943,#289944,#289945,#289946,#289947,#289948,#289949,
#289950,#289951,#289952,#289953,#289954,#289955,#289956,#289957,#289958,
#289959,#289960,#289961,#289962,#289963,#289964,#289965,#289966,#289967,
#289968,#289969,#289970,#289971,#289972,#289973,#289974,#289975,#289976,
#289977,#289978,#289979,#289980,#289981,#289982,#289983,#289984,#289985,
#289986,#289987,#289988,#289989,#289990,#289991,#289992,#289993,#289994,
#289995,#289996,#289997,#289998,#289999,#290000,#290001,#290002,#290003,
#290004,#290005,#290006,#290007,#290008,#290009,#290010,#290011,#290012,
#290013,#290014,#290015,#290016,#290017,#290018,#290019,#290020,#290021,
#290022,#290023,#290024),.UNSPECIFIED.,.F.,.F.,(4,3,3,3,3,3,3,3,3,3,3,3,
3,3,3,3,3,3,3,3,3,3,3,3,3,3,3,3,3,3,3,3,3,3,3,3,3,3,3,3,3,3,3,3,3,3,3,3,
3,3,3,3,3,3,3,3,3,3,3,3,3,3,3,3,3,3,3,3,3,3,3,3,3,3,3,3,3,3,3,3,3,3,3,3,
3,3,3,3,3,3,3,3,3,3,3,3,3,3,3,3,3,3,3,3,3,3,3,4),(0.143172102,0.15412844,
0.165137615,0.176146789,0.187155963,0.198165138,0.209174312,0.220183486,
0.231192661,0.242201835,0.253211009,0.264220183,0.275229358,0.286238532,
0.297247706,0.308256881,0.319266055,0.330275229,0.341284404,0.352293578,
0.363302752,0.374311927,0.385321101,0.396330275,0.405504587,0.414678899,
0.423853211,0.433027523,0.442201835,0.451376147,0.460550459,0.471559633,
0.480733945,0.491743119,0.500917431,0.510091743,0.519266055,0.528440367,
0.535779817,0.543119266,0.550458716,0.557798165,0.565137615,0.572477064,
0.579816514,0.587155963,0.594495413,0.601834862,0.609174312,0.616513761,
0.623853211,0.631192661,0.63853211,0.64587156,0.653211009,0.662385321,0.669724771,
0.67706422,0.68440367,0.691743119,0.699082569,0.706422018,0.713761468,0.721100917,
0.728440367,0.737614679,0.744954128,0.752293578,0.759633028,0.766972477,
0.776146789,0.783486239,0.790825688,0.798165138,0.805504587,0.811009174,
0.820183486,0.825688073,0.831192661,0.840366972,0.84587156,0.851376147,
0.856880734,0.862385321,0.867889908,0.873394495,0.878899083,0.88440367,
0.889908257,0.895412844,0.900917431,0.906422018,0.911926606,0.917431193,
0.92293578,0.928440367,0.933944954,0.939449541,0.944954128,0.950458716,
0.955963303,0.963302752,0.968807339,0.974311927,0.981651376,0.987155963,
0.99266055,1.),.UNSPECIFIED.);
#24483=B_SPLINE_CURVE_WITH_KNOTS('',3,(#290987,#290988,#290989,#290990,
#290991,#290992,#290993,#290994,#290995,#290996,#290997,#290998,#290999,
#291000,#291001,#291002,#291003,#291004,#291005,#291006,#291007,#291008,
#291009,#291010,#291011,#291012,#291013,#291014,#291015,#291016,#291017,
#291018,#291019,#291020,#291021,#291022,#291023,#291024,#291025,#291026,
#291027,#291028,#291029,#291030,#291031,#291032,#291033,#291034,#291035,
#291036,#291037,#291038,#291039,#291040,#291041,#291042,#291043,#291044,
#291045,#291046,#291047,#291048,#291049,#291050,#291051,#291052,#291053,
#291054,#291055,#291056,#291057,#291058,#291059,#291060,#291061,#291062,
#291063,#291064,#291065,#291066,#291067,#291068,#291069,#291070,#291071,
#291072,#291073,#291074,#291075,#291076,#291077,#291078,#291079,#291080,
#291081,#291082,#291083,#291084,#291085,#291086,#291087,#291088,#291089,
#291090,#291091,#291092,#291093,#291094,#291095,#291096,#291097,#291098,
#291099,#291100,#291101,#291102,#291103,#291104,#291105,#291106,#291107,
#291108,#291109,#291110,#291111,#291112,#291113,#291114,#291115,#291116,
#291117,#291118,#291119,#291120,#291121,#291122,#291123,#291124,#291125,
#291126,#291127,#291128,#291129,#291130,#291131,#291132,#291133,#291134,
#291135,#291136,#291137,#291138,#291139,#291140,#291141,#291142,#291143,
#291144,#291145,#291146,#291147,#291148,#291149,#291150,#291151,#291152,
#291153,#291154,#291155,#291156,#291157,#291158,#291159,#291160,#291161,
#291162,#291163,#291164,#291165,#291166,#291167,#291168,#291169,#291170,
#291171,#291172,#291173,#291174,#291175,#291176,#291177,#291178,#291179,
#291180,#291181,#291182,#291183,#291184,#291185,#291186,#291187,#291188,
#291189,#291190,#291191,#291192,#291193,#291194,#291195,#291196,#291197,
#291198,#291199,#291200,#291201,#291202,#291203,#291204,#291205,#291206,
#291207,#291208,#291209,#291210,#291211,#291212,#291213,#291214,#291215,
#291216,#291217,#291218,#291219,#291220,#291221,#291222,#291223,#291224,
#291225,#291226,#291227,#291228,#291229,#291230,#291231,#291232,#291233,
#291234,#291235,#291236,#291237,#291238,#291239,#291240,#291241,#291242,
#291243,#291244,#291245,#291246,#291247,#291248,#291249,#291250,#291251,
#291252,#291253,#291254,#291255,#291256,#291257,#291258,#291259,#291260,
#291261,#291262,#291263,#291264,#291265,#291266,#291267,#291268,#291269,
#291270,#291271,#291272,#291273,#291274,#291275,#291276,#291277,#291278,
#291279,#291280,#291281,#291282,#291283,#291284,#291285,#291286,#291287,
#291288,#291289,#291290,#291291,#291292,#291293,#291294,#291295,#291296,
#291297,#291298,#291299,#291300,#291301,#291302,#291303,#291304,#291305,
#291306,#291307,#291308,#291309,#291310,#291311),.UNSPECIFIED.,.F.,.F.,
(4,3,3,3,3,3,3,3,3,3,3,3,3,3,3,3,3,3,3,3,3,3,3,3,3,3,3,3,3,3,3,3,3,3,3,
3,3,3,3,3,3,3,3,3,3,3,3,3,3,3,3,3,3,3,3,3,3,3,3,3,3,3,3,3,3,3,3,3,3,3,3,
3,3,3,3,3,3,3,3,3,3,3,3,3,3,3,3,3,3,3,3,3,3,3,3,3,3,3,3,3,3,3,3,3,3,3,3,
3,4),(-1.,-0.994495413,-0.988990826,-0.983486239,-0.977981651,-0.972477064,
-0.965137615,-0.957798165,-0.952293578,-0.946788991,-0.941284404,-0.935779817,
-0.930275229,-0.924770642,-0.919266055,-0.913761468,-0.908256881,-0.900917431,
-0.895412844,-0.889908257,-0.88440367,-0.878899083,-0.873394495,-0.867889908,
-0.862385321,-0.856880734,-0.851376147,-0.84587156,-0.840366972,-0.834862385,
-0.829357798,-0.823853211,-0.814678899,-0.809174312,-0.801834862,-0.794495413,
-0.787155963,-0.779816514,-0.772477064,-0.765137615,-0.757798165,-0.750458716,
-0.743119266,-0.735779817,-0.728440367,-0.721100917,-0.713761468,-0.706422018,
-0.699082569,-0.691743119,-0.68440367,-0.67706422,-0.669724771,-0.662385321,
-0.655045872,-0.647706422,-0.640366972,-0.633027523,-0.625688073,-0.618348624,
-0.611009174,-0.603669725,-0.596330275,-0.588990826,-0.581651376,-0.574311927,
-0.566972477,-0.557798165,-0.550458716,-0.543119266,-0.535779817,-0.528440367,
-0.519266055,-0.510091743,-0.500917431,-0.491743119,-0.482568807,-0.473394495,
-0.464220183,-0.455045872,-0.44587156,-0.436697248,-0.427522936,-0.418348624,
-0.409174312,-0.4,-0.390825688,-0.379816514,-0.368807339,-0.357798165,-0.346788991,
-0.335779817,-0.324770642,-0.313761468,-0.302752294,-0.291743119,-0.280733945,
-0.269724771,-0.258715596,-0.247706422,-0.236697248,-0.225688073,-0.214678899,
-0.203669725,-0.19266055,-0.181651376,-0.170642202,-0.159633028,-0.143172102),
 .UNSPECIFIED.);
#24484=B_SPLINE_CURVE_WITH_KNOTS('',3,(#291312,#291313,#291314,#291315,
#291316,#291317,#291318,#291319,#291320,#291321,#291322,#291323,#291324,
#291325,#291326,#291327,#291328,#291329,#291330,#291331,#291332,#291333,
#291334,#291335,#291336,#291337,#291338,#291339,#291340,#291341,#291342,
#291343,#291344,#291345,#291346,#291347,#291348,#291349,#291350,#291351,
#291352,#291353,#291354,#291355,#291356,#291357,#291358,#291359,#291360,
#291361,#291362,#291363,#291364,#291365,#291366,#291367,#291368,#291369,
#291370,#291371,#291372,#291373,#291374,#291375,#291376,#291377,#291378,
#291379,#291380,#291381,#291382,#291383,#291384,#291385,#291386,#291387,
#291388,#291389,#291390,#291391,#291392,#291393,#291394,#291395,#291396,
#291397,#291398,#291399,#291400,#291401,#291402,#291403,#291404,#291405,
#291406,#291407,#291408,#291409,#291410,#291411,#291412,#291413,#291414,
#291415,#291416,#291417,#291418,#291419,#291420,#291421,#291422,#291423,
#291424,#291425,#291426,#291427,#291428,#291429,#291430,#291431,#291432,
#291433,#291434,#291435,#291436,#291437,#291438,#291439,#291440,#291441,
#291442,#291443,#291444,#291445,#291446,#291447,#291448,#291449,#291450,
#291451,#291452,#291453,#291454,#291455,#291456,#291457,#291458,#291459,
#291460,#291461,#291462,#291463,#291464,#291465,#291466,#291467,#291468,
#291469,#291470,#291471,#291472,#291473,#291474,#291475,#291476,#291477,
#291478,#291479,#291480,#291481,#291482,#291483,#291484,#291485,#291486,
#291487,#291488,#291489,#291490,#291491,#291492,#291493,#291494,#291495,
#291496,#291497,#291498,#291499,#291500,#291501,#291502,#291503,#291504,
#291505,#291506,#291507,#291508,#291509,#291510,#291511,#291512,#291513,
#291514,#291515,#291516,#291517,#291518,#291519,#291520,#291521,#291522,
#291523,#291524,#291525,#291526,#291527,#291528,#291529,#291530,#291531,
#291532,#291533,#291534,#291535,#291536,#291537,#291538,#291539,#291540,
#291541,#291542,#291543,#291544,#291545,#291546,#291547,#291548,#291549,
#291550,#291551,#291552,#291553,#291554,#291555,#291556,#291557,#291558,
#291559,#291560,#291561,#291562,#291563,#291564,#291565,#291566,#291567,
#291568,#291569,#291570,#291571,#291572,#291573,#291574,#291575,#291576,
#291577,#291578,#291579,#291580,#291581,#291582,#291583,#291584,#291585,
#291586,#291587,#291588,#291589,#291590,#291591,#291592,#291593,#291594,
#291595,#291596,#291597,#291598,#291599,#291600,#291601,#291602,#291603,
#291604,#291605,#291606,#291607,#291608,#291609,#291610,#291611,#291612,
#291613,#291614,#291615,#291616,#291617,#291618,#291619,#291620,#291621,
#291622,#291623,#291624,#291625,#291626,#291627,#291628,#291629,#291630,
#291631,#291632,#291633),.UNSPECIFIED.,.F.,.F.,(4,3,3,3,3,3,3,3,3,3,3,3,
3,3,3,3,3,3,3,3,3,3,3,3,3,3,3,3,3,3,3,3,3,3,3,3,3,3,3,3,3,3,3,3,3,3,3,3,
3,3,3,3,3,3,3,3,3,3,3,3,3,3,3,3,3,3,3,3,3,3,3,3,3,3,3,3,3,3,3,3,3,3,3,3,
3,3,3,3,3,3,3,3,3,3,3,3,3,3,3,3,3,3,3,3,3,3,3,4),(0.143172102,0.15412844,
0.165137615,0.176146789,0.187155963,0.198165138,0.209174312,0.220183486,
0.231192661,0.242201835,0.253211009,0.264220183,0.275229358,0.286238532,
0.297247706,0.308256881,0.319266055,0.330275229,0.341284404,0.352293578,
0.363302752,0.374311927,0.385321101,0.396330275,0.405504587,0.414678899,
0.423853211,0.433027523,0.442201835,0.451376147,0.460550459,0.469724771,
0.478899083,0.488073394,0.497247706,0.506422018,0.51559633,0.524770642,
0.533944954,0.541284404,0.548623853,0.555963303,0.563302752,0.572477064,
0.579816514,0.587155963,0.594495413,0.601834862,0.609174312,0.616513761,
0.623853211,0.631192661,0.63853211,0.64587156,0.653211009,0.662385321,0.669724771,
0.67706422,0.68440367,0.691743119,0.699082569,0.706422018,0.713761468,0.721100917,
0.728440367,0.737614679,0.744954128,0.752293578,0.759633028,0.766972477,
0.776146789,0.783486239,0.790825688,0.798165138,0.805504587,0.811009174,
0.820183486,0.825688073,0.831192661,0.840366972,0.84587156,0.853211009,
0.858715596,0.864220183,0.869724771,0.875229358,0.880733945,0.886238532,
0.891743119,0.897247706,0.902752294,0.910091743,0.91559633,0.921100917,
0.926605505,0.932110092,0.937614679,0.943119266,0.948623853,0.95412844,
0.96146789,0.966972477,0.972477064,0.977981651,0.983486239,0.988990826,
0.994495413,1.),.UNSPECIFIED.);
#24485=B_SPLINE_CURVE_WITH_KNOTS('',3,(#292578,#292579,#292580,#292581,
#292582,#292583,#292584,#292585,#292586,#292587,#292588,#292589,#292590,
#292591,#292592,#292593,#292594,#292595,#292596,#292597,#292598,#292599,
#292600,#292601,#292602,#292603,#292604,#292605,#292606,#292607,#292608,
#292609,#292610,#292611,#292612,#292613,#292614,#292615,#292616,#292617,
#292618,#292619,#292620,#292621,#292622,#292623,#292624,#292625,#292626,
#292627,#292628,#292629,#292630,#292631,#292632,#292633,#292634,#292635,
#292636,#292637,#292638,#292639,#292640,#292641,#292642,#292643,#292644,
#292645,#292646,#292647,#292648,#292649,#292650,#292651,#292652,#292653,
#292654,#292655,#292656,#292657,#292658,#292659,#292660,#292661,#292662,
#292663,#292664,#292665,#292666,#292667,#292668,#292669,#292670,#292671,
#292672,#292673,#292674,#292675,#292676,#292677,#292678,#292679,#292680,
#292681,#292682,#292683,#292684,#292685,#292686,#292687,#292688,#292689,
#292690,#292691,#292692,#292693,#292694,#292695,#292696,#292697,#292698,
#292699,#292700,#292701,#292702,#292703,#292704,#292705,#292706,#292707,
#292708,#292709,#292710,#292711,#292712,#292713,#292714,#292715,#292716,
#292717,#292718,#292719,#292720,#292721,#292722,#292723,#292724,#292725,
#292726,#292727,#292728,#292729,#292730,#292731,#292732,#292733,#292734,
#292735,#292736,#292737,#292738,#292739,#292740,#292741,#292742,#292743,
#292744,#292745,#292746,#292747,#292748,#292749,#292750,#292751,#292752,
#292753,#292754,#292755,#292756,#292757,#292758,#292759,#292760,#292761,
#292762,#292763,#292764,#292765,#292766,#292767,#292768,#292769,#292770,
#292771,#292772,#292773,#292774,#292775,#292776,#292777,#292778,#292779,
#292780,#292781,#292782,#292783,#292784,#292785,#292786,#292787,#292788,
#292789,#292790,#292791,#292792,#292793,#292794,#292795,#292796,#292797,
#292798,#292799,#292800,#292801,#292802,#292803,#292804,#292805,#292806,
#292807,#292808,#292809,#292810,#292811,#292812,#292813,#292814,#292815,
#292816,#292817,#292818,#292819,#292820,#292821,#292822,#292823,#292824,
#292825,#292826,#292827,#292828,#292829,#292830,#292831,#292832,#292833,
#292834,#292835,#292836,#292837,#292838,#292839,#292840,#292841,#292842,
#292843,#292844,#292845,#292846,#292847,#292848,#292849,#292850,#292851,
#292852,#292853,#292854,#292855,#292856,#292857,#292858,#292859,#292860,
#292861,#292862,#292863,#292864,#292865,#292866,#292867,#292868,#292869,
#292870,#292871,#292872,#292873,#292874,#292875,#292876,#292877,#292878,
#292879,#292880,#292881,#292882,#292883,#292884,#292885,#292886,#292887,
#292888,#292889,#292890),.UNSPECIFIED.,.F.,.F.,(4,3,3,3,3,3,3,3,3,3,3,3,
3,3,3,3,3,3,3,3,3,3,3,3,3,3,3,3,3,3,3,3,3,3,3,3,3,3,3,3,3,3,3,3,3,3,3,3,
3,3,3,3,3,3,3,3,3,3,3,3,3,3,3,3,3,3,3,3,3,3,3,3,3,3,3,3,3,3,3,3,3,3,3,3,
3,3,3,3,3,3,3,3,3,3,3,3,3,3,3,3,3,3,3,3,4),(0.143172102,0.15412844,0.165137615,
0.176146789,0.187155963,0.198165138,0.209174312,0.220183486,0.231192661,
0.242201835,0.253211009,0.264220183,0.275229358,0.286238532,0.297247706,
0.308256881,0.319266055,0.330275229,0.341284404,0.352293578,0.365137615,
0.376146789,0.388990826,0.398165138,0.40733945,0.416513761,0.425688073,
0.436697248,0.44587156,0.455045872,0.464220183,0.473394495,0.482568807,
0.495412844,0.504587156,0.513761468,0.52293578,0.532110092,0.539449541,
0.546788991,0.55412844,0.56146789,0.568807339,0.576146789,0.583486239,0.590825688,
0.598165138,0.60733945,0.614678899,0.622018349,0.631192661,0.63853211,0.64587156,
0.653211009,0.660550459,0.667889908,0.678899083,0.686238532,0.693577982,
0.702752294,0.711926606,0.719266055,0.726605505,0.735779817,0.743119266,
0.750458716,0.759633028,0.766972477,0.774311927,0.781651376,0.788990826,
0.796330275,0.803669725,0.812844037,0.818348624,0.823853211,0.831192661,
0.836697248,0.842201835,0.847706422,0.853211009,0.860550459,0.866055046,
0.871559633,0.878899083,0.88440367,0.889908257,0.895412844,0.902752294,
0.908256881,0.913761468,0.919266055,0.928440367,0.935779817,0.941284404,
0.946788991,0.952293578,0.96146789,0.966972477,0.972477064,0.977981651,
0.983486239,0.988990826,0.994495413,1.),.UNSPECIFIED.);
#24486=B_SPLINE_CURVE_WITH_KNOTS('',3,(#292891,#292892,#292893,#292894,
#292895,#292896,#292897,#292898,#292899,#292900,#292901,#292902,#292903,
#292904,#292905,#292906,#292907,#292908,#292909,#292910,#292911,#292912,
#292913,#292914,#292915,#292916,#292917,#292918,#292919,#292920,#292921,
#292922,#292923,#292924,#292925,#292926,#292927,#292928,#292929,#292930,
#292931,#292932,#292933,#292934,#292935,#292936,#292937,#292938,#292939,
#292940,#292941,#292942,#292943,#292944,#292945,#292946,#292947,#292948,
#292949,#292950,#292951,#292952,#292953,#292954,#292955,#292956,#292957,
#292958,#292959,#292960,#292961,#292962,#292963,#292964,#292965,#292966,
#292967,#292968,#292969,#292970,#292971,#292972,#292973,#292974,#292975,
#292976,#292977,#292978,#292979,#292980,#292981,#292982,#292983,#292984,
#292985,#292986,#292987,#292988,#292989,#292990,#292991,#292992,#292993,
#292994,#292995,#292996,#292997,#292998,#292999,#293000,#293001,#293002,
#293003,#293004,#293005,#293006,#293007,#293008,#293009,#293010,#293011,
#293012,#293013,#293014,#293015,#293016,#293017,#293018,#293019,#293020,
#293021,#293022,#293023,#293024,#293025,#293026,#293027,#293028,#293029,
#293030,#293031,#293032,#293033,#293034,#293035,#293036,#293037,#293038,
#293039,#293040,#293041,#293042,#293043,#293044,#293045,#293046,#293047,
#293048,#293049,#293050,#293051,#293052,#293053,#293054,#293055,#293056,
#293057,#293058,#293059,#293060,#293061,#293062,#293063,#293064,#293065,
#293066,#293067,#293068,#293069,#293070,#293071,#293072,#293073,#293074,
#293075,#293076,#293077,#293078,#293079,#293080,#293081,#293082,#293083,
#293084,#293085,#293086,#293087,#293088,#293089,#293090,#293091,#293092,
#293093,#293094,#293095,#293096,#293097,#293098,#293099,#293100,#293101,
#293102,#293103,#293104,#293105,#293106,#293107,#293108,#293109,#293110,
#293111,#293112,#293113,#293114,#293115,#293116,#293117,#293118,#293119,
#293120,#293121,#293122,#293123,#293124,#293125,#293126,#293127,#293128,
#293129,#293130,#293131,#293132,#293133,#293134,#293135,#293136,#293137,
#293138,#293139,#293140,#293141,#293142,#293143,#293144,#293145,#293146,
#293147,#293148,#293149,#293150,#293151,#293152,#293153,#293154,#293155,
#293156,#293157,#293158,#293159,#293160,#293161,#293162,#293163,#293164,
#293165,#293166,#293167,#293168,#293169,#293170,#293171,#293172,#293173,
#293174,#293175,#293176,#293177,#293178,#293179,#293180,#293181,#293182,
#293183,#293184,#293185,#293186,#293187,#293188,#293189,#293190,#293191,
#293192,#293193,#293194,#293195,#293196,#293197,#293198,#293199,#293200,
#293201,#293202,#293203,#293204,#293205,#293206,#293207,#293208,#293209,
#293210,#293211,#293212),.UNSPECIFIED.,.F.,.F.,(4,3,3,3,3,3,3,3,3,3,3,3,
3,3,3,3,3,3,3,3,3,3,3,3,3,3,3,3,3,3,3,3,3,3,3,3,3,3,3,3,3,3,3,3,3,3,3,3,
3,3,3,3,3,3,3,3,3,3,3,3,3,3,3,3,3,3,3,3,3,3,3,3,3,3,3,3,3,3,3,3,3,3,3,3,
3,3,3,3,3,3,3,3,3,3,3,3,3,3,3,3,3,3,3,3,3,3,3,4),(0.143172102,0.15412844,
0.165137615,0.176146789,0.187155963,0.198165138,0.209174312,0.220183486,
0.231192661,0.242201835,0.253211009,0.264220183,0.275229358,0.286238532,
0.297247706,0.308256881,0.319266055,0.330275229,0.341284404,0.352293578,
0.363302752,0.374311927,0.385321101,0.396330275,0.405504587,0.414678899,
0.423853211,0.433027523,0.442201835,0.451376147,0.460550459,0.469724771,
0.478899083,0.488073394,0.499082569,0.508256881,0.517431193,0.526605505,
0.533944954,0.541284404,0.548623853,0.555963303,0.563302752,0.570642202,
0.577981651,0.585321101,0.59266055,0.6,0.60733945,0.614678899,0.622018349,
0.629357798,0.636697248,0.644036697,0.651376147,0.658715596,0.666055046,
0.673394495,0.680733945,0.688073394,0.695412844,0.702752294,0.710091743,
0.717431193,0.724770642,0.732110092,0.739449541,0.748623853,0.755963303,
0.763302752,0.770642202,0.777981651,0.785321101,0.79266055,0.8,0.80733945,
0.812844037,0.820183486,0.827522936,0.833027523,0.842201835,0.847706422,
0.853211009,0.858715596,0.864220183,0.869724771,0.875229358,0.880733945,
0.886238532,0.891743119,0.897247706,0.902752294,0.908256881,0.913761468,
0.919266055,0.924770642,0.930275229,0.935779817,0.941284404,0.946788991,
0.952293578,0.957798165,0.966972477,0.972477064,0.979816514,0.985321101,
0.990825688,1.),.UNSPECIFIED.);
#24487=B_SPLINE_CURVE_WITH_KNOTS('',3,(#294172,#294173,#294174,#294175,
#294176,#294177,#294178,#294179,#294180,#294181,#294182,#294183,#294184,
#294185,#294186,#294187,#294188,#294189,#294190,#294191,#294192,#294193,
#294194,#294195,#294196,#294197,#294198,#294199,#294200,#294201,#294202,
#294203,#294204,#294205,#294206,#294207,#294208,#294209,#294210,#294211,
#294212,#294213,#294214,#294215,#294216,#294217,#294218,#294219,#294220,
#294221,#294222,#294223,#294224,#294225,#294226,#294227,#294228,#294229,
#294230,#294231,#294232,#294233,#294234,#294235,#294236,#294237,#294238,
#294239,#294240,#294241,#294242,#294243,#294244,#294245,#294246,#294247,
#294248,#294249,#294250,#294251,#294252,#294253,#294254,#294255,#294256,
#294257,#294258,#294259,#294260,#294261,#294262,#294263,#294264,#294265,
#294266,#294267,#294268,#294269,#294270,#294271,#294272,#294273,#294274,
#294275,#294276,#294277,#294278,#294279,#294280,#294281,#294282,#294283,
#294284,#294285,#294286,#294287,#294288,#294289,#294290,#294291,#294292,
#294293,#294294,#294295,#294296,#294297,#294298,#294299,#294300,#294301,
#294302,#294303,#294304,#294305,#294306,#294307,#294308,#294309,#294310,
#294311,#294312,#294313,#294314,#294315,#294316,#294317,#294318,#294319,
#294320,#294321,#294322,#294323,#294324,#294325,#294326,#294327,#294328,
#294329,#294330,#294331,#294332,#294333,#294334,#294335,#294336,#294337,
#294338,#294339,#294340,#294341,#294342,#294343,#294344,#294345,#294346,
#294347,#294348,#294349,#294350,#294351,#294352,#294353,#294354,#294355,
#294356,#294357,#294358,#294359,#294360,#294361,#294362,#294363,#294364,
#294365,#294366,#294367,#294368,#294369,#294370,#294371,#294372,#294373,
#294374,#294375,#294376,#294377,#294378,#294379,#294380,#294381,#294382,
#294383,#294384,#294385,#294386,#294387,#294388,#294389,#294390,#294391,
#294392,#294393,#294394,#294395,#294396,#294397,#294398,#294399,#294400,
#294401,#294402,#294403,#294404,#294405,#294406,#294407,#294408,#294409,
#294410,#294411,#294412,#294413,#294414,#294415,#294416,#294417,#294418,
#294419,#294420,#294421,#294422,#294423,#294424,#294425,#294426,#294427,
#294428,#294429,#294430,#294431,#294432,#294433,#294434,#294435,#294436,
#294437,#294438,#294439,#294440,#294441,#294442,#294443,#294444,#294445,
#294446,#294447,#294448,#294449,#294450,#294451,#294452,#294453,#294454,
#294455,#294456,#294457,#294458,#294459,#294460,#294461,#294462,#294463,
#294464,#294465,#294466,#294467,#294468,#294469,#294470,#294471,#294472,
#294473,#294474,#294475,#294476,#294477,#294478,#294479,#294480,#294481,
#294482,#294483,#294484,#294485,#294486,#294487),.UNSPECIFIED.,.F.,.F.,
(4,3,3,3,3,3,3,3,3,3,3,3,3,3,3,3,3,3,3,3,3,3,3,3,3,3,3,3,3,3,3,3,3,3,3,
3,3,3,3,3,3,3,3,3,3,3,3,3,3,3,3,3,3,3,3,3,3,3,3,3,3,3,3,3,3,3,3,3,3,3,3,
3,3,3,3,3,3,3,3,3,3,3,3,3,3,3,3,3,3,3,3,3,3,3,3,3,3,3,3,3,3,3,3,3,3,4),
(0.143172102,0.15412844,0.165137615,0.176146789,0.187155963,0.198165138,
0.209174312,0.220183486,0.231192661,0.242201835,0.253211009,0.264220183,
0.275229358,0.286238532,0.297247706,0.308256881,0.319266055,0.330275229,
0.341284404,0.352293578,0.363302752,0.374311927,0.385321101,0.396330275,
0.405504587,0.414678899,0.423853211,0.433027523,0.442201835,0.451376147,
0.460550459,0.469724771,0.478899083,0.488073394,0.499082569,0.508256881,
0.517431193,0.526605505,0.533944954,0.541284404,0.548623853,0.555963303,
0.565137615,0.572477064,0.579816514,0.587155963,0.594495413,0.601834862,
0.609174312,0.616513761,0.623853211,0.631192661,0.63853211,0.64587156,0.653211009,
0.660550459,0.667889908,0.678899083,0.686238532,0.693577982,0.700917431,
0.711926606,0.719266055,0.726605505,0.733944954,0.741284404,0.750458716,
0.757798165,0.765137615,0.772477064,0.779816514,0.788990826,0.796330275,
0.803669725,0.812844037,0.818348624,0.823853211,0.831192661,0.836697248,
0.842201835,0.847706422,0.855045872,0.860550459,0.866055046,0.871559633,
0.87706422,0.882568807,0.888073394,0.893577982,0.902752294,0.908256881,
0.913761468,0.919266055,0.928440367,0.935779817,0.941284404,0.946788991,
0.952293578,0.957798165,0.963302752,0.970642202,0.976146789,0.981651376,
0.987155963,0.99266055,1.),.UNSPECIFIED.);
#24488=B_SPLINE_CURVE_WITH_KNOTS('',3,(#294488,#294489,#294490,#294491,
#294492,#294493,#294494,#294495,#294496,#294497,#294498,#294499,#294500,
#294501,#294502,#294503,#294504,#294505,#294506,#294507,#294508,#294509,
#294510,#294511,#294512,#294513,#294514,#294515,#294516,#294517,#294518,
#294519,#294520,#294521,#294522,#294523,#294524,#294525,#294526,#294527,
#294528,#294529,#294530,#294531,#294532,#294533,#294534,#294535,#294536,
#294537,#294538,#294539,#294540,#294541,#294542,#294543,#294544,#294545,
#294546,#294547,#294548,#294549,#294550,#294551,#294552,#294553,#294554,
#294555,#294556,#294557,#294558,#294559,#294560,#294561,#294562,#294563,
#294564,#294565,#294566,#294567,#294568,#294569,#294570,#294571,#294572,
#294573,#294574,#294575,#294576,#294577,#294578,#294579,#294580,#294581,
#294582,#294583,#294584,#294585,#294586,#294587,#294588,#294589,#294590,
#294591,#294592,#294593,#294594,#294595,#294596,#294597,#294598,#294599,
#294600,#294601,#294602,#294603,#294604,#294605,#294606,#294607,#294608,
#294609,#294610,#294611,#294612,#294613,#294614,#294615,#294616,#294617,
#294618,#294619,#294620,#294621,#294622,#294623,#294624,#294625,#294626,
#294627,#294628,#294629,#294630,#294631,#294632,#294633,#294634,#294635,
#294636,#294637,#294638,#294639,#294640,#294641,#294642,#294643,#294644,
#294645,#294646,#294647,#294648,#294649,#294650,#294651,#294652,#294653,
#294654,#294655,#294656,#294657,#294658,#294659,#294660,#294661,#294662,
#294663,#294664,#294665,#294666,#294667,#294668,#294669,#294670,#294671,
#294672,#294673,#294674,#294675,#294676,#294677,#294678,#294679,#294680,
#294681,#294682,#294683,#294684,#294685,#294686,#294687,#294688,#294689,
#294690,#294691,#294692,#294693,#294694,#294695,#294696,#294697,#294698,
#294699,#294700,#294701,#294702,#294703,#294704,#294705,#294706,#294707,
#294708,#294709,#294710,#294711,#294712,#294713,#294714,#294715,#294716,
#294717,#294718,#294719,#294720,#294721,#294722,#294723,#294724,#294725,
#294726,#294727,#294728,#294729,#294730,#294731,#294732,#294733,#294734,
#294735,#294736,#294737,#294738,#294739,#294740,#294741,#294742,#294743,
#294744,#294745,#294746,#294747,#294748,#294749,#294750,#294751,#294752,
#294753,#294754,#294755,#294756,#294757,#294758,#294759,#294760,#294761,
#294762,#294763,#294764,#294765,#294766,#294767,#294768,#294769,#294770,
#294771,#294772,#294773,#294774,#294775,#294776,#294777,#294778,#294779,
#294780,#294781,#294782,#294783,#294784,#294785,#294786,#294787,#294788,
#294789,#294790,#294791,#294792,#294793,#294794,#294795,#294796,#294797,
#294798,#294799,#294800,#294801,#294802,#294803,#294804,#294805,#294806),
 .UNSPECIFIED.,.F.,.F.,(4,3,3,3,3,3,3,3,3,3,3,3,3,3,3,3,3,3,3,3,3,3,3,3,
3,3,3,3,3,3,3,3,3,3,3,3,3,3,3,3,3,3,3,3,3,3,3,3,3,3,3,3,3,3,3,3,3,3,3,3,
3,3,3,3,3,3,3,3,3,3,3,3,3,3,3,3,3,3,3,3,3,3,3,3,3,3,3,3,3,3,3,3,3,3,3,3,
3,3,3,3,3,3,3,3,3,3,4),(0.143172102,0.15412844,0.165137615,0.176146789,
0.187155963,0.198165138,0.209174312,0.220183486,0.231192661,0.242201835,
0.253211009,0.264220183,0.275229358,0.286238532,0.297247706,0.308256881,
0.319266055,0.330275229,0.341284404,0.352293578,0.363302752,0.374311927,
0.385321101,0.396330275,0.405504587,0.414678899,0.423853211,0.433027523,
0.442201835,0.451376147,0.460550459,0.469724771,0.478899083,0.488073394,
0.499082569,0.508256881,0.517431193,0.526605505,0.533944954,0.543119266,
0.550458716,0.559633028,0.566972477,0.574311927,0.581651376,0.588990826,
0.596330275,0.603669725,0.612844037,0.620183486,0.627522936,0.634862385,
0.642201835,0.649541284,0.656880734,0.664220183,0.673394495,0.680733945,
0.688073394,0.695412844,0.702752294,0.710091743,0.717431193,0.724770642,
0.733944954,0.741284404,0.748623853,0.755963303,0.763302752,0.772477064,
0.781651376,0.788990826,0.796330275,0.805504587,0.811009174,0.816513761,
0.822018349,0.827522936,0.833027523,0.83853211,0.844036697,0.849541284,
0.855045872,0.860550459,0.866055046,0.871559633,0.87706422,0.882568807,
0.888073394,0.893577982,0.900917431,0.906422018,0.911926606,0.921100917,
0.930275229,0.935779817,0.941284404,0.946788991,0.952293578,0.957798165,
0.963302752,0.968807339,0.976146789,0.981651376,0.987155963,0.994495413,
1.),.UNSPECIFIED.);
#24489=B_SPLINE_CURVE_WITH_KNOTS('',5,(#295754,#295755,#295756,#295757,
#295758,#295759,#295760,#295761,#295762,#295763,#295764,#295765,#295766,
#295767,#295768,#295769,#295770,#295771,#295772,#295773,#295774,#295775,
#295776,#295777,#295778,#295779,#295780,#295781,#295782,#295783,#295784,
#295785,#295786,#295787,#295788,#295789,#295790,#295791,#295792,#295793,
#295794,#295795,#295796,#295797,#295798,#295799,#295800,#295801,#295802,
#295803,#295804,#295805,#295806,#295807,#295808,#295809,#295810,#295811,
#295812,#295813,#295814,#295815,#295816,#295817,#295818,#295819,#295820,
#295821,#295822,#295823,#295824,#295825,#295826,#295827,#295828,#295829,
#295830,#295831,#295832,#295833,#295834,#295835,#295836,#295837,#295838,
#295839,#295840,#295841,#295842,#295843,#295844,#295845,#295846,#295847,
#295848,#295849,#295850,#295851,#295852,#295853,#295854,#295855,#295856,
#295857,#295858,#295859,#295860,#295861,#295862,#295863,#295864,#295865,
#295866,#295867,#295868,#295869,#295870,#295871,#295872,#295873,#295874,
#295875,#295876,#295877,#295878,#295879,#295880,#295881,#295882,#295883,
#295884,#295885,#295886,#295887,#295888,#295889,#295890,#295891,#295892,
#295893,#295894,#295895,#295896,#295897,#295898,#295899,#295900,#295901,
#295902,#295903,#295904,#295905,#295906,#295907,#295908,#295909,#295910,
#295911,#295912,#295913,#295914,#295915,#295916,#295917,#295918,#295919,
#295920,#295921,#295922,#295923,#295924,#295925,#295926,#295927,#295928,
#295929,#295930,#295931,#295932,#295933,#295934,#295935,#295936,#295937,
#295938,#295939,#295940,#295941,#295942,#295943,#295944,#295945,#295946,
#295947,#295948,#295949,#295950,#295951,#295952,#295953,#295954,#295955,
#295956,#295957,#295958,#295959,#295960,#295961,#295962,#295963,#295964,
#295965,#295966,#295967,#295968,#295969,#295970,#295971,#295972,#295973,
#295974,#295975,#295976,#295977,#295978,#295979,#295980,#295981,#295982,
#295983,#295984,#295985,#295986,#295987,#295988,#295989,#295990,#295991,
#295992,#295993,#295994,#295995,#295996,#295997,#295998,#295999,#296000,
#296001,#296002,#296003,#296004,#296005,#296006,#296007,#296008,#296009,
#296010,#296011,#296012,#296013,#296014,#296015,#296016,#296017,#296018,
#296019,#296020,#296021,#296022,#296023,#296024,#296025,#296026,#296027,
#296028,#296029,#296030,#296031,#296032,#296033,#296034,#296035,#296036,
#296037,#296038,#296039,#296040,#296041,#296042,#296043,#296044,#296045,
#296046,#296047,#296048,#296049,#296050,#296051,#296052,#296053,#296054,
#296055,#296056,#296057,#296058,#296059,#296060,#296061,#296062,#296063,
#296064,#296065,#296066,#296067,#296068,#296069,#296070,#296071,#296072,
#296073,#296074,#296075,#296076,#296077,#296078,#296079,#296080,#296081,
#296082,#296083,#296084,#296085,#296086,#296087,#296088,#296089,#296090,
#296091,#296092,#296093,#296094,#296095,#296096,#296097,#296098,#296099,
#296100,#296101,#296102,#296103,#296104,#296105,#296106,#296107,#296108,
#296109,#296110,#296111,#296112,#296113,#296114,#296115,#296116,#296117,
#296118,#296119,#296120,#296121,#296122,#296123,#296124,#296125,#296126,
#296127,#296128,#296129,#296130,#296131,#296132,#296133,#296134,#296135,
#296136,#296137,#296138,#296139,#296140,#296141,#296142,#296143,#296144,
#296145,#296146,#296147,#296148,#296149,#296150,#296151,#296152,#296153,
#296154,#296155,#296156,#296157,#296158,#296159,#296160,#296161,#296162,
#296163,#296164,#296165,#296166,#296167,#296168,#296169,#296170,#296171,
#296172,#296173,#296174,#296175,#296176,#296177,#296178,#296179,#296180,
#296181,#296182,#296183,#296184,#296185,#296186,#296187,#296188,#296189,
#296190,#296191,#296192,#296193,#296194,#296195,#296196,#296197,#296198,
#296199,#296200,#296201,#296202,#296203,#296204,#296205,#296206,#296207,
#296208,#296209,#296210,#296211,#296212,#296213,#296214,#296215,#296216,
#296217,#296218,#296219,#296220,#296221,#296222,#296223,#296224,#296225),
 .UNSPECIFIED.,.F.,.F.,(6,1,1,1,1,1,1,1,1,1,1,1,1,1,1,1,1,1,1,1,1,1,1,1,
1,1,1,1,1,1,1,1,1,1,1,1,1,1,1,1,1,1,1,1,1,1,1,1,1,1,1,1,1,1,1,1,1,1,1,1,
1,1,1,1,1,1,1,1,1,1,1,1,1,1,1,1,1,1,1,1,1,1,1,1,1,1,1,1,1,1,1,1,1,1,1,1,
1,1,1,1,1,1,1,1,1,1,1,1,1,1,1,1,1,1,1,1,1,1,1,1,1,1,1,1,1,1,1,1,1,1,1,1,
1,1,1,1,1,1,1,1,1,1,1,1,1,1,1,1,1,1,1,1,1,1,1,1,1,1,1,1,1,1,1,1,1,1,1,1,
1,1,1,1,1,1,1,1,1,1,1,1,1,1,1,1,1,1,1,1,1,1,1,1,1,1,1,1,1,1,1,1,1,1,1,1,
1,1,1,1,1,1,1,1,1,1,1,1,1,1,1,1,1,1,1,1,1,1,1,1,1,1,1,1,1,1,1,1,1,1,1,1,
1,1,1,1,1,1,1,1,1,1,1,1,1,1,1,1,1,1,1,1,1,1,1,1,1,1,1,1,1,1,1,1,1,1,1,1,
1,1,1,1,1,1,1,1,1,1,1,1,1,1,1,1,1,1,1,1,1,1,1,1,1,1,1,1,1,1,1,1,1,1,1,1,
1,1,1,1,1,1,1,1,1,1,1,1,1,1,1,1,1,1,1,1,1,1,1,1,1,1,1,1,1,1,1,1,1,1,1,1,
1,1,1,1,1,1,1,1,1,1,1,1,1,1,1,1,1,1,1,1,1,1,1,1,1,1,1,1,1,1,1,1,1,1,1,1,
1,1,1,1,1,1,1,1,1,1,1,1,1,1,1,1,1,1,1,1,1,1,1,1,1,1,1,1,1,1,1,1,1,1,1,1,
1,1,1,1,1,1,1,1,1,1,1,1,1,1,1,1,1,1,1,1,1,1,1,1,1,1,1,1,1,1,1,1,1,1,1,1,
1,1,1,1,1,1,1,1,1,1,1,6),(-1.,-0.998165138,-0.996330275,-0.994495413,-0.99266055,
-0.990825688,-0.988990826,-0.987155963,-0.985321101,-0.983486239,-0.981651376,
-0.979816514,-0.977981651,-0.976146789,-0.974311927,-0.972477064,-0.970642202,
-0.968807339,-0.966972477,-0.965137615,-0.963302752,-0.96146789,-0.959633028,
-0.957798165,-0.955963303,-0.95412844,-0.952293578,-0.950458716,-0.948623853,
-0.946788991,-0.944954128,-0.943119266,-0.941284404,-0.939449541,-0.937614679,
-0.935779817,-0.933944954,-0.932110092,-0.930275229,-0.928440367,-0.926605505,
-0.924770642,-0.92293578,-0.921100917,-0.919266055,-0.917431193,-0.91559633,
-0.913761468,-0.911926606,-0.910091743,-0.908256881,-0.906422018,-0.904587156,
-0.902752294,-0.900917431,-0.899082569,-0.897247706,-0.895412844,-0.893577982,
-0.891743119,-0.889908257,-0.888073394,-0.886238532,-0.88440367,-0.882568807,
-0.880733945,-0.878899083,-0.87706422,-0.875229358,-0.873394495,-0.871559633,
-0.869724771,-0.867889908,-0.866055046,-0.864220183,-0.862385321,-0.860550459,
-0.858715596,-0.856880734,-0.855045872,-0.853211009,-0.851376147,-0.849541284,
-0.847706422,-0.84587156,-0.844036697,-0.842201835,-0.840366972,-0.83853211,
-0.836697248,-0.834862385,-0.833027523,-0.831192661,-0.829357798,-0.827522936,
-0.825688073,-0.823853211,-0.822018349,-0.820183486,-0.818348624,-0.816513761,
-0.814678899,-0.812844037,-0.811009174,-0.809174312,-0.80733945,-0.805504587,
-0.803669725,-0.801834862,-0.8,-0.798165138,-0.796330275,-0.794495413,-0.79266055,
-0.790825688,-0.788990826,-0.787155963,-0.785321101,-0.783486239,-0.781651376,
-0.779816514,-0.777981651,-0.776146789,-0.774311927,-0.772477064,-0.770642202,
-0.768807339,-0.766972477,-0.765137615,-0.763302752,-0.76146789,-0.759633028,
-0.757798165,-0.755963303,-0.75412844,-0.752293578,-0.750458716,-0.748623853,
-0.746788991,-0.744954128,-0.743119266,-0.741284404,-0.739449541,-0.737614679,
-0.735779817,-0.733944954,-0.732110092,-0.730275229,-0.728440367,-0.726605505,
-0.724770642,-0.72293578,-0.721100917,-0.719266055,-0.717431193,-0.71559633,
-0.713761468,-0.711926606,-0.710091743,-0.708256881,-0.706422018,-0.704587156,
-0.702752294,-0.700917431,-0.699082569,-0.697247706,-0.695412844,-0.693577982,
-0.691743119,-0.689908257,-0.688073394,-0.686238532,-0.68440367,-0.682568807,
-0.680733945,-0.678899083,-0.67706422,-0.675229358,-0.673394495,-0.671559633,
-0.669724771,-0.667889908,-0.666055046,-0.664220183,-0.662385321,-0.660550459,
-0.658715596,-0.656880734,-0.655045872,-0.653211009,-0.651376147,-0.649541284,
-0.647706422,-0.64587156,-0.644036697,-0.642201835,-0.640366972,-0.63853211,
-0.636697248,-0.634862385,-0.633027523,-0.631192661,-0.629357798,-0.627522936,
-0.625688073,-0.623853211,-0.622018349,-0.620183486,-0.618348624,-0.616513761,
-0.614678899,-0.612844037,-0.611009174,-0.609174312,-0.60733945,-0.605504587,
-0.603669725,-0.601834862,-0.6,-0.598165138,-0.596330275,-0.594495413,-0.59266055,
-0.590825688,-0.588990826,-0.587155963,-0.585321101,-0.583486239,-0.581651376,
-0.579816514,-0.577981651,-0.576146789,-0.574311927,-0.572477064,-0.570642202,
-0.568807339,-0.566972477,-0.565137615,-0.563302752,-0.56146789,-0.559633028,
-0.557798165,-0.555963303,-0.55412844,-0.552293578,-0.550458716,-0.548623853,
-0.546788991,-0.544954128,-0.543119266,-0.541284404,-0.539449541,-0.537614679,
-0.535779817,-0.533944954,-0.532110092,-0.530275229,-0.528440367,-0.526605505,
-0.524770642,-0.52293578,-0.521100917,-0.519266055,-0.517431193,-0.51559633,
-0.513761468,-0.511926606,-0.510091743,-0.508256881,-0.506422018,-0.504587156,
-0.502752294,-0.500917431,-0.499082569,-0.497247706,-0.495412844,-0.493577982,
-0.491743119,-0.489908257,-0.488073394,-0.486238532,-0.48440367,-0.482568807,
-0.480733945,-0.478899083,-0.47706422,-0.475229358,-0.473394495,-0.471559633,
-0.469724771,-0.467889908,-0.466055046,-0.464220183,-0.462385321,-0.460550459,
-0.458715596,-0.456880734,-0.455045872,-0.453211009,-0.451376147,-0.449541284,
-0.447706422,-0.44587156,-0.444036697,-0.442201835,-0.440366972,-0.43853211,
-0.436697248,-0.434862385,-0.433027523,-0.431192661,-0.429357798,-0.427522936,
-0.425688073,-0.423853211,-0.422018349,-0.420183486,-0.418348624,-0.416513761,
-0.414678899,-0.412844037,-0.411009174,-0.409174312,-0.40733945,-0.405504587,
-0.403669725,-0.401834862,-0.4,-0.398165138,-0.396330275,-0.394495413,-0.39266055,
-0.390825688,-0.388990826,-0.387155963,-0.385321101,-0.383486239,-0.381651376,
-0.379816514,-0.377981651,-0.376146789,-0.374311927,-0.372477064,-0.370642202,
-0.368807339,-0.366972477,-0.365137615,-0.363302752,-0.36146789,-0.359633028,
-0.357798165,-0.355963303,-0.35412844,-0.352293578,-0.350458716,-0.348623853,
-0.346788991,-0.344954128,-0.343119266,-0.341284404,-0.339449541,-0.337614679,
-0.335779817,-0.333944954,-0.332110092,-0.330275229,-0.328440367,-0.326605505,
-0.324770642,-0.32293578,-0.321100917,-0.319266055,-0.317431193,-0.31559633,
-0.313761468,-0.311926606,-0.310091743,-0.308256881,-0.306422018,-0.304587156,
-0.302752294,-0.300917431,-0.299082569,-0.297247706,-0.295412844,-0.293577982,
-0.291743119,-0.289908257,-0.288073394,-0.286238532,-0.28440367,-0.282568807,
-0.280733945,-0.278899083,-0.27706422,-0.275229358,-0.273394495,-0.271559633,
-0.269724771,-0.267889908,-0.266055046,-0.264220183,-0.262385321,-0.260550459,
-0.258715596,-0.256880734,-0.255045872,-0.253211009,-0.251376147,-0.249541284,
-0.247706422,-0.24587156,-0.244036697,-0.242201835,-0.240366972,-0.23853211,
-0.236697248,-0.234862385,-0.233027523,-0.231192661,-0.229357798,-0.227522936,
-0.225688073,-0.223853211,-0.222018349,-0.220183486,-0.218348624,-0.216513761,
-0.214678899,-0.212844037,-0.211009174,-0.209174312,-0.20733945,-0.205504587,
-0.203669725,-0.201834862,-0.2,-0.198165138,-0.196330275,-0.194495413,-0.19266055,
-0.190825688,-0.188990826,-0.187155963,-0.185321101,-0.183486239,-0.181651376,
-0.179816514,-0.177981651,-0.176146789,-0.174311927,-0.172477064,-0.170642202,
-0.168807339,-0.166972477,-0.165137615,-0.163302752,-0.16146789,-0.159633028,
-0.157798165,-0.155963303,-0.15412844,-0.152293578,-0.150458716,-0.148623853,
-0.146788991,-0.144954128,-0.143172102),.UNSPECIFIED.);
#24490=B_SPLINE_CURVE_WITH_KNOTS('',5,(#296226,#296227,#296228,#296229,
#296230,#296231,#296232,#296233,#296234,#296235,#296236,#296237,#296238,
#296239,#296240,#296241,#296242,#296243,#296244,#296245,#296246,#296247,
#296248,#296249,#296250,#296251,#296252,#296253,#296254,#296255,#296256,
#296257,#296258,#296259,#296260,#296261,#296262,#296263,#296264,#296265,
#296266,#296267,#296268,#296269,#296270,#296271,#296272,#296273,#296274,
#296275,#296276,#296277,#296278,#296279,#296280,#296281,#296282,#296283,
#296284,#296285,#296286,#296287,#296288,#296289,#296290,#296291,#296292,
#296293,#296294,#296295,#296296,#296297,#296298,#296299,#296300,#296301,
#296302,#296303,#296304,#296305,#296306,#296307,#296308,#296309,#296310,
#296311,#296312,#296313,#296314,#296315,#296316,#296317,#296318,#296319,
#296320,#296321,#296322,#296323,#296324,#296325,#296326,#296327,#296328,
#296329,#296330,#296331,#296332,#296333,#296334,#296335,#296336,#296337,
#296338,#296339,#296340,#296341,#296342,#296343,#296344,#296345,#296346,
#296347,#296348,#296349,#296350,#296351,#296352,#296353,#296354,#296355,
#296356,#296357,#296358,#296359,#296360,#296361,#296362,#296363,#296364,
#296365,#296366,#296367,#296368,#296369,#296370,#296371,#296372,#296373,
#296374,#296375,#296376,#296377,#296378,#296379,#296380,#296381,#296382,
#296383,#296384,#296385,#296386,#296387,#296388,#296389,#296390,#296391,
#296392,#296393,#296394,#296395,#296396,#296397,#296398,#296399,#296400,
#296401,#296402,#296403,#296404,#296405,#296406,#296407,#296408,#296409,
#296410,#296411,#296412,#296413,#296414,#296415,#296416,#296417,#296418,
#296419,#296420,#296421,#296422,#296423,#296424,#296425,#296426,#296427,
#296428,#296429,#296430,#296431,#296432,#296433,#296434,#296435,#296436,
#296437,#296438,#296439,#296440,#296441,#296442,#296443,#296444,#296445,
#296446,#296447,#296448,#296449,#296450,#296451,#296452,#296453,#296454,
#296455,#296456,#296457,#296458,#296459,#296460,#296461,#296462,#296463,
#296464,#296465,#296466,#296467,#296468,#296469,#296470,#296471,#296472,
#296473,#296474,#296475,#296476,#296477,#296478,#296479,#296480,#296481,
#296482,#296483,#296484,#296485,#296486,#296487,#296488,#296489,#296490,
#296491,#296492,#296493,#296494,#296495,#296496,#296497,#296498,#296499,
#296500,#296501,#296502,#296503,#296504,#296505,#296506,#296507,#296508,
#296509,#296510,#296511,#296512,#296513,#296514,#296515,#296516,#296517,
#296518,#296519,#296520,#296521,#296522,#296523,#296524,#296525,#296526,
#296527,#296528,#296529,#296530,#296531,#296532,#296533,#296534,#296535,
#296536,#296537,#296538,#296539,#296540,#296541,#296542,#296543,#296544,
#296545,#296546,#296547,#296548,#296549,#296550,#296551,#296552,#296553,
#296554,#296555,#296556,#296557,#296558,#296559,#296560,#296561,#296562,
#296563,#296564,#296565,#296566,#296567,#296568,#296569,#296570,#296571,
#296572,#296573,#296574,#296575,#296576,#296577,#296578,#296579,#296580,
#296581,#296582,#296583,#296584,#296585,#296586,#296587,#296588,#296589,
#296590,#296591,#296592,#296593,#296594,#296595,#296596,#296597,#296598,
#296599,#296600,#296601,#296602,#296603,#296604,#296605,#296606,#296607,
#296608,#296609,#296610,#296611,#296612,#296613,#296614,#296615,#296616,
#296617,#296618,#296619,#296620,#296621,#296622,#296623,#296624,#296625,
#296626,#296627,#296628,#296629,#296630,#296631,#296632,#296633,#296634,
#296635,#296636,#296637,#296638,#296639,#296640,#296641,#296642,#296643,
#296644,#296645,#296646,#296647,#296648,#296649,#296650,#296651,#296652,
#296653,#296654,#296655,#296656,#296657,#296658,#296659,#296660,#296661,
#296662,#296663,#296664,#296665,#296666,#296667,#296668,#296669,#296670,
#296671,#296672,#296673,#296674,#296675,#296676,#296677,#296678,#296679,
#296680,#296681,#296682,#296683,#296684,#296685,#296686,#296687,#296688,
#296689,#296690,#296691,#296692,#296693,#296694,#296695,#296696,#296697),
 .UNSPECIFIED.,.F.,.F.,(6,1,1,1,1,1,1,1,1,1,1,1,1,1,1,1,1,1,1,1,1,1,1,1,
1,1,1,1,1,1,1,1,1,1,1,1,1,1,1,1,1,1,1,1,1,1,1,1,1,1,1,1,1,1,1,1,1,1,1,1,
1,1,1,1,1,1,1,1,1,1,1,1,1,1,1,1,1,1,1,1,1,1,1,1,1,1,1,1,1,1,1,1,1,1,1,1,
1,1,1,1,1,1,1,1,1,1,1,1,1,1,1,1,1,1,1,1,1,1,1,1,1,1,1,1,1,1,1,1,1,1,1,1,
1,1,1,1,1,1,1,1,1,1,1,1,1,1,1,1,1,1,1,1,1,1,1,1,1,1,1,1,1,1,1,1,1,1,1,1,
1,1,1,1,1,1,1,1,1,1,1,1,1,1,1,1,1,1,1,1,1,1,1,1,1,1,1,1,1,1,1,1,1,1,1,1,
1,1,1,1,1,1,1,1,1,1,1,1,1,1,1,1,1,1,1,1,1,1,1,1,1,1,1,1,1,1,1,1,1,1,1,1,
1,1,1,1,1,1,1,1,1,1,1,1,1,1,1,1,1,1,1,1,1,1,1,1,1,1,1,1,1,1,1,1,1,1,1,1,
1,1,1,1,1,1,1,1,1,1,1,1,1,1,1,1,1,1,1,1,1,1,1,1,1,1,1,1,1,1,1,1,1,1,1,1,
1,1,1,1,1,1,1,1,1,1,1,1,1,1,1,1,1,1,1,1,1,1,1,1,1,1,1,1,1,1,1,1,1,1,1,1,
1,1,1,1,1,1,1,1,1,1,1,1,1,1,1,1,1,1,1,1,1,1,1,1,1,1,1,1,1,1,1,1,1,1,1,1,
1,1,1,1,1,1,1,1,1,1,1,1,1,1,1,1,1,1,1,1,1,1,1,1,1,1,1,1,1,1,1,1,1,1,1,1,
1,1,1,1,1,1,1,1,1,1,1,1,1,1,1,1,1,1,1,1,1,1,1,1,1,1,1,1,1,1,1,1,1,1,1,1,
1,1,1,1,1,1,1,1,1,1,1,6),(0.143172102,0.144954128,0.146788991,0.148623853,
0.150458716,0.152293578,0.15412844,0.155963303,0.157798165,0.159633028,
0.16146789,0.163302752,0.165137615,0.166972477,0.168807339,0.170642202,
0.172477064,0.174311927,0.176146789,0.177981651,0.179816514,0.181651376,
0.183486239,0.185321101,0.187155963,0.188990826,0.190825688,0.19266055,
0.194495413,0.196330275,0.198165138,0.2,0.201834862,0.203669725,0.205504587,
0.20733945,0.209174312,0.211009174,0.212844037,0.214678899,0.216513761,
0.218348624,0.220183486,0.222018349,0.223853211,0.225688073,0.227522936,
0.229357798,0.231192661,0.233027523,0.234862385,0.236697248,0.23853211,
0.240366972,0.242201835,0.244036697,0.24587156,0.247706422,0.249541284,
0.251376147,0.253211009,0.255045872,0.256880734,0.258715596,0.260550459,
0.262385321,0.264220183,0.266055046,0.267889908,0.269724771,0.271559633,
0.273394495,0.275229358,0.27706422,0.278899083,0.280733945,0.282568807,
0.28440367,0.286238532,0.288073394,0.289908257,0.291743119,0.293577982,
0.295412844,0.297247706,0.299082569,0.300917431,0.302752294,0.304587156,
0.306422018,0.308256881,0.310091743,0.311926606,0.313761468,0.31559633,
0.317431193,0.319266055,0.321100917,0.32293578,0.324770642,0.326605505,
0.328440367,0.330275229,0.332110092,0.333944954,0.335779817,0.337614679,
0.339449541,0.341284404,0.343119266,0.344954128,0.346788991,0.348623853,
0.350458716,0.352293578,0.35412844,0.355963303,0.357798165,0.359633028,
0.36146789,0.363302752,0.365137615,0.366972477,0.368807339,0.370642202,
0.372477064,0.374311927,0.376146789,0.377981651,0.379816514,0.381651376,
0.383486239,0.385321101,0.387155963,0.388990826,0.390825688,0.39266055,
0.394495413,0.396330275,0.398165138,0.4,0.401834862,0.403669725,0.405504587,
0.40733945,0.409174312,0.411009174,0.412844037,0.414678899,0.416513761,
0.418348624,0.420183486,0.422018349,0.423853211,0.425688073,0.427522936,
0.429357798,0.431192661,0.433027523,0.434862385,0.436697248,0.43853211,
0.440366972,0.442201835,0.444036697,0.44587156,0.447706422,0.449541284,
0.451376147,0.453211009,0.455045872,0.456880734,0.458715596,0.460550459,
0.462385321,0.464220183,0.466055046,0.467889908,0.469724771,0.471559633,
0.473394495,0.475229358,0.47706422,0.478899083,0.480733945,0.482568807,
0.48440367,0.486238532,0.488073394,0.489908257,0.491743119,0.493577982,
0.495412844,0.497247706,0.499082569,0.500917431,0.502752294,0.504587156,
0.506422018,0.508256881,0.510091743,0.511926606,0.513761468,0.51559633,
0.517431193,0.519266055,0.521100917,0.52293578,0.524770642,0.526605505,
0.528440367,0.530275229,0.532110092,0.533944954,0.535779817,0.537614679,
0.539449541,0.541284404,0.543119266,0.544954128,0.546788991,0.548623853,
0.550458716,0.552293578,0.55412844,0.555963303,0.557798165,0.559633028,
0.56146789,0.563302752,0.565137615,0.566972477,0.568807339,0.570642202,
0.572477064,0.574311927,0.576146789,0.577981651,0.579816514,0.581651376,
0.583486239,0.585321101,0.587155963,0.588990826,0.590825688,0.59266055,
0.594495413,0.596330275,0.598165138,0.6,0.601834862,0.603669725,0.605504587,
0.60733945,0.609174312,0.611009174,0.612844037,0.614678899,0.616513761,
0.618348624,0.620183486,0.622018349,0.623853211,0.625688073,0.627522936,
0.629357798,0.631192661,0.633027523,0.634862385,0.636697248,0.63853211,
0.640366972,0.642201835,0.644036697,0.64587156,0.647706422,0.649541284,
0.651376147,0.653211009,0.655045872,0.656880734,0.658715596,0.660550459,
0.662385321,0.664220183,0.666055046,0.667889908,0.669724771,0.671559633,
0.673394495,0.675229358,0.67706422,0.678899083,0.680733945,0.682568807,
0.68440367,0.686238532,0.688073394,0.689908257,0.691743119,0.693577982,
0.695412844,0.697247706,0.699082569,0.700917431,0.702752294,0.704587156,
0.706422018,0.708256881,0.710091743,0.711926606,0.713761468,0.71559633,
0.717431193,0.719266055,0.721100917,0.72293578,0.724770642,0.726605505,
0.728440367,0.730275229,0.732110092,0.733944954,0.735779817,0.737614679,
0.739449541,0.741284404,0.743119266,0.744954128,0.746788991,0.748623853,
0.750458716,0.752293578,0.75412844,0.755963303,0.757798165,0.759633028,
0.76146789,0.763302752,0.765137615,0.766972477,0.768807339,0.770642202,
0.772477064,0.774311927,0.776146789,0.777981651,0.779816514,0.781651376,
0.783486239,0.785321101,0.787155963,0.788990826,0.790825688,0.79266055,
0.794495413,0.796330275,0.798165138,0.8,0.801834862,0.803669725,0.805504587,
0.80733945,0.809174312,0.811009174,0.812844037,0.814678899,0.816513761,
0.818348624,0.820183486,0.822018349,0.823853211,0.825688073,0.827522936,
0.829357798,0.831192661,0.833027523,0.834862385,0.836697248,0.83853211,
0.840366972,0.842201835,0.844036697,0.84587156,0.847706422,0.849541284,
0.851376147,0.853211009,0.855045872,0.856880734,0.858715596,0.860550459,
0.862385321,0.864220183,0.866055046,0.867889908,0.869724771,0.871559633,
0.873394495,0.875229358,0.87706422,0.878899083,0.880733945,0.882568807,
0.88440367,0.886238532,0.888073394,0.889908257,0.891743119,0.893577982,
0.895412844,0.897247706,0.899082569,0.900917431,0.902752294,0.904587156,
0.906422018,0.908256881,0.910091743,0.911926606,0.913761468,0.91559633,
0.917431193,0.919266055,0.921100917,0.92293578,0.924770642,0.926605505,
0.928440367,0.930275229,0.932110092,0.933944954,0.935779817,0.937614679,
0.939449541,0.941284404,0.943119266,0.944954128,0.946788991,0.948623853,
0.950458716,0.952293578,0.95412844,0.955963303,0.957798165,0.959633028,
0.96146789,0.963302752,0.965137615,0.966972477,0.968807339,0.970642202,
0.972477064,0.974311927,0.976146789,0.977981651,0.979816514,0.981651376,
0.983486239,0.985321101,0.987155963,0.988990826,0.990825688,0.99266055,
0.994495413,0.996330275,0.998165138,1.),.UNSPECIFIED.);
#24491=B_SPLINE_CURVE_WITH_KNOTS('',5,(#296704,#296705,#296706,#296707,
#296708,#296709,#296710,#296711,#296712,#296713,#296714,#296715,#296716,
#296717,#296718,#296719,#296720,#296721,#296722,#296723,#296724,#296725,
#296726,#296727,#296728,#296729,#296730,#296731,#296732,#296733,#296734,
#296735,#296736,#296737,#296738,#296739,#296740,#296741,#296742,#296743,
#296744,#296745,#296746,#296747,#296748,#296749,#296750,#296751,#296752,
#296753,#296754,#296755,#296756,#296757,#296758,#296759,#296760,#296761,
#296762,#296763,#296764,#296765,#296766,#296767,#296768,#296769,#296770,
#296771,#296772,#296773,#296774,#296775,#296776,#296777,#296778,#296779,
#296780,#296781,#296782,#296783,#296784,#296785,#296786,#296787,#296788,
#296789,#296790,#296791,#296792,#296793,#296794,#296795,#296796,#296797,
#296798,#296799,#296800,#296801,#296802,#296803,#296804,#296805,#296806,
#296807,#296808,#296809,#296810,#296811,#296812,#296813,#296814,#296815,
#296816,#296817,#296818,#296819,#296820,#296821,#296822,#296823,#296824,
#296825,#296826,#296827,#296828,#296829,#296830,#296831,#296832,#296833,
#296834,#296835,#296836,#296837,#296838,#296839,#296840,#296841,#296842,
#296843,#296844,#296845,#296846,#296847,#296848,#296849,#296850,#296851,
#296852,#296853,#296854,#296855,#296856,#296857,#296858,#296859,#296860,
#296861,#296862,#296863,#296864,#296865,#296866,#296867,#296868,#296869,
#296870,#296871,#296872,#296873,#296874,#296875,#296876,#296877,#296878,
#296879,#296880,#296881,#296882,#296883,#296884,#296885,#296886,#296887,
#296888,#296889,#296890,#296891,#296892,#296893,#296894,#296895,#296896,
#296897,#296898,#296899,#296900,#296901,#296902,#296903,#296904,#296905,
#296906,#296907,#296908,#296909,#296910,#296911,#296912,#296913,#296914,
#296915,#296916,#296917,#296918,#296919,#296920,#296921,#296922,#296923,
#296924,#296925,#296926,#296927,#296928,#296929,#296930,#296931,#296932,
#296933,#296934,#296935,#296936,#296937,#296938,#296939,#296940,#296941,
#296942,#296943,#296944,#296945,#296946,#296947,#296948,#296949,#296950,
#296951,#296952,#296953,#296954,#296955,#296956,#296957,#296958,#296959,
#296960,#296961,#296962,#296963,#296964,#296965,#296966,#296967,#296968,
#296969,#296970,#296971,#296972,#296973,#296974,#296975,#296976,#296977,
#296978,#296979,#296980,#296981,#296982,#296983,#296984,#296985,#296986,
#296987,#296988,#296989,#296990,#296991,#296992,#296993,#296994,#296995,
#296996,#296997,#296998,#296999,#297000,#297001,#297002,#297003,#297004,
#297005,#297006,#297007,#297008,#297009,#297010,#297011,#297012,#297013,
#297014,#297015,#297016,#297017,#297018,#297019,#297020,#297021,#297022,
#297023,#297024,#297025,#297026,#297027,#297028,#297029,#297030,#297031,
#297032,#297033,#297034,#297035,#297036,#297037,#297038,#297039,#297040,
#297041,#297042,#297043,#297044,#297045,#297046,#297047,#297048,#297049,
#297050,#297051,#297052,#297053,#297054,#297055,#297056,#297057,#297058,
#297059,#297060,#297061,#297062,#297063,#297064,#297065,#297066,#297067,
#297068,#297069,#297070,#297071,#297072,#297073,#297074,#297075,#297076,
#297077,#297078,#297079,#297080,#297081,#297082,#297083,#297084,#297085,
#297086,#297087,#297088,#297089,#297090,#297091,#297092,#297093,#297094,
#297095,#297096,#297097,#297098,#297099,#297100,#297101,#297102,#297103,
#297104,#297105,#297106,#297107,#297108,#297109,#297110,#297111,#297112,
#297113,#297114,#297115,#297116,#297117,#297118,#297119,#297120,#297121,
#297122,#297123,#297124,#297125,#297126,#297127,#297128,#297129,#297130,
#297131,#297132,#297133,#297134,#297135,#297136,#297137,#297138,#297139,
#297140,#297141,#297142,#297143,#297144,#297145,#297146,#297147,#297148,
#297149,#297150,#297151,#297152,#297153,#297154,#297155,#297156,#297157,
#297158,#297159,#297160,#297161,#297162,#297163,#297164,#297165,#297166,
#297167,#297168,#297169,#297170,#297171,#297172,#297173,#297174),
 .UNSPECIFIED.,.F.,.F.,(6,1,1,1,1,1,1,1,1,1,1,1,1,1,1,1,1,1,1,1,1,1,1,1,
1,1,1,1,1,1,1,1,1,1,1,1,1,1,1,1,1,1,1,1,1,1,1,1,1,1,1,1,1,1,1,1,1,1,1,1,
1,1,1,1,1,1,1,1,1,1,1,1,1,1,1,1,1,1,1,1,1,1,1,1,1,1,1,1,1,1,1,1,1,1,1,1,
1,1,1,1,1,1,1,1,1,1,1,1,1,1,1,1,1,1,1,1,1,1,1,1,1,1,1,1,1,1,1,1,1,1,1,1,
1,1,1,1,1,1,1,1,1,1,1,1,1,1,1,1,1,1,1,1,1,1,1,1,1,1,1,1,1,1,1,1,1,1,1,1,
1,1,1,1,1,1,1,1,1,1,1,1,1,1,1,1,1,1,1,1,1,1,1,1,1,1,1,1,1,1,1,1,1,1,1,1,
1,1,1,1,1,1,1,1,1,1,1,1,1,1,1,1,1,1,1,1,1,1,1,1,1,1,1,1,1,1,1,1,1,1,1,1,
1,1,1,1,1,1,1,1,1,1,1,1,1,1,1,1,1,1,1,1,1,1,1,1,1,1,1,1,1,1,1,1,1,1,1,1,
1,1,1,1,1,1,1,1,1,1,1,1,1,1,1,1,1,1,1,1,1,1,1,1,1,1,1,1,1,1,1,1,1,1,1,1,
1,1,1,1,1,1,1,1,1,1,1,1,1,1,1,1,1,1,1,1,1,1,1,1,1,1,1,1,1,1,1,1,1,1,1,1,
1,1,1,1,1,1,1,1,1,1,1,1,1,1,1,1,1,1,1,1,1,1,1,1,1,1,1,1,1,1,1,1,1,1,1,1,
1,1,1,1,1,1,1,1,1,1,1,1,1,1,1,1,1,1,1,1,1,1,1,1,1,1,1,1,1,1,1,1,1,1,1,1,
1,1,1,1,1,1,1,1,1,1,1,1,1,1,1,1,1,1,1,1,1,1,1,1,1,1,1,1,1,1,1,1,1,1,1,1,
1,1,1,1,1,1,1,1,1,1,6),(0.143172102,0.144954128,0.146788991,0.148623853,
0.150458716,0.152293578,0.15412844,0.155963303,0.157798165,0.159633028,
0.16146789,0.163302752,0.165137615,0.166972477,0.168807339,0.170642202,
0.172477064,0.174311927,0.176146789,0.177981651,0.179816514,0.181651376,
0.183486239,0.185321101,0.187155963,0.188990826,0.190825688,0.19266055,
0.194495413,0.196330275,0.198165138,0.2,0.201834862,0.203669725,0.205504587,
0.20733945,0.209174312,0.211009174,0.212844037,0.214678899,0.216513761,
0.218348624,0.220183486,0.222018349,0.223853211,0.225688073,0.227522936,
0.229357798,0.231192661,0.233027523,0.234862385,0.236697248,0.23853211,
0.240366972,0.242201835,0.244036697,0.24587156,0.247706422,0.249541284,
0.251376147,0.253211009,0.255045872,0.256880734,0.258715596,0.260550459,
0.262385321,0.264220183,0.266055046,0.267889908,0.269724771,0.271559633,
0.273394495,0.275229358,0.27706422,0.278899083,0.280733945,0.282568807,
0.28440367,0.286238532,0.288073394,0.289908257,0.291743119,0.293577982,
0.295412844,0.297247706,0.299082569,0.300917431,0.302752294,0.304587156,
0.306422018,0.308256881,0.310091743,0.311926606,0.313761468,0.31559633,
0.317431193,0.319266055,0.321100917,0.32293578,0.324770642,0.326605505,
0.328440367,0.330275229,0.332110092,0.333944954,0.335779817,0.337614679,
0.339449541,0.341284404,0.343119266,0.344954128,0.346788991,0.348623853,
0.350458716,0.352293578,0.35412844,0.355963303,0.357798165,0.359633028,
0.36146789,0.363302752,0.365137615,0.366972477,0.368807339,0.370642202,
0.372477064,0.374311927,0.376146789,0.377981651,0.379816514,0.381651376,
0.383486239,0.385321101,0.387155963,0.388990826,0.390825688,0.39266055,
0.394495413,0.396330275,0.398165138,0.4,0.401834862,0.403669725,0.405504587,
0.40733945,0.409174312,0.411009174,0.412844037,0.414678899,0.416513761,
0.418348624,0.420183486,0.422018349,0.423853211,0.425688073,0.427522936,
0.429357798,0.431192661,0.433027523,0.434862385,0.436697248,0.43853211,
0.440366972,0.442201835,0.444036697,0.44587156,0.447706422,0.449541284,
0.451376147,0.453211009,0.455045872,0.456880734,0.458715596,0.460550459,
0.462385321,0.464220183,0.466055046,0.467889908,0.469724771,0.471559633,
0.473394495,0.475229358,0.47706422,0.478899083,0.480733945,0.482568807,
0.48440367,0.486238532,0.488073394,0.489908257,0.491743119,0.493577982,
0.495412844,0.497247706,0.499082569,0.500917431,0.502752294,0.504587156,
0.506422018,0.508256881,0.511926606,0.513761468,0.51559633,0.517431193,
0.519266055,0.521100917,0.52293578,0.524770642,0.526605505,0.528440367,
0.530275229,0.532110092,0.533944954,0.535779817,0.537614679,0.539449541,
0.541284404,0.543119266,0.544954128,0.546788991,0.548623853,0.550458716,
0.552293578,0.55412844,0.555963303,0.557798165,0.559633028,0.56146789,0.563302752,
0.565137615,0.566972477,0.568807339,0.570642202,0.572477064,0.574311927,
0.576146789,0.577981651,0.579816514,0.581651376,0.583486239,0.585321101,
0.587155963,0.588990826,0.590825688,0.59266055,0.594495413,0.596330275,
0.598165138,0.6,0.601834862,0.603669725,0.605504587,0.60733945,0.609174312,
0.611009174,0.612844037,0.614678899,0.616513761,0.618348624,0.620183486,
0.622018349,0.623853211,0.625688073,0.627522936,0.629357798,0.631192661,
0.633027523,0.634862385,0.636697248,0.63853211,0.640366972,0.642201835,
0.644036697,0.64587156,0.647706422,0.649541284,0.651376147,0.653211009,
0.655045872,0.656880734,0.658715596,0.660550459,0.662385321,0.664220183,
0.666055046,0.667889908,0.669724771,0.671559633,0.673394495,0.675229358,
0.67706422,0.678899083,0.680733945,0.682568807,0.68440367,0.686238532,0.688073394,
0.689908257,0.691743119,0.693577982,0.695412844,0.697247706,0.699082569,
0.700917431,0.702752294,0.704587156,0.706422018,0.708256881,0.710091743,
0.711926606,0.713761468,0.71559633,0.717431193,0.719266055,0.721100917,
0.72293578,0.724770642,0.726605505,0.728440367,0.730275229,0.732110092,
0.733944954,0.735779817,0.737614679,0.739449541,0.741284404,0.743119266,
0.744954128,0.746788991,0.748623853,0.750458716,0.752293578,0.75412844,
0.755963303,0.757798165,0.759633028,0.76146789,0.763302752,0.765137615,
0.766972477,0.768807339,0.770642202,0.772477064,0.774311927,0.776146789,
0.777981651,0.779816514,0.781651376,0.783486239,0.785321101,0.787155963,
0.788990826,0.790825688,0.79266055,0.794495413,0.796330275,0.798165138,
0.8,0.801834862,0.803669725,0.805504587,0.80733945,0.809174312,0.811009174,
0.812844037,0.814678899,0.816513761,0.818348624,0.820183486,0.822018349,
0.823853211,0.825688073,0.827522936,0.829357798,0.831192661,0.833027523,
0.834862385,0.836697248,0.83853211,0.840366972,0.842201835,0.844036697,
0.84587156,0.847706422,0.849541284,0.851376147,0.853211009,0.855045872,
0.856880734,0.858715596,0.860550459,0.862385321,0.864220183,0.866055046,
0.867889908,0.869724771,0.871559633,0.873394495,0.875229358,0.87706422,
0.878899083,0.880733945,0.882568807,0.88440367,0.886238532,0.888073394,
0.889908257,0.891743119,0.893577982,0.895412844,0.897247706,0.899082569,
0.900917431,0.902752294,0.904587156,0.906422018,0.908256881,0.910091743,
0.911926606,0.913761468,0.91559633,0.917431193,0.919266055,0.921100917,
0.92293578,0.924770642,0.926605505,0.928440367,0.930275229,0.932110092,
0.933944954,0.935779817,0.937614679,0.939449541,0.941284404,0.943119266,
0.944954128,0.946788991,0.948623853,0.950458716,0.952293578,0.95412844,
0.955963303,0.957798165,0.959633028,0.96146789,0.963302752,0.965137615,
0.966972477,0.968807339,0.970642202,0.972477064,0.974311927,0.976146789,
0.977981651,0.979816514,0.981651376,0.983486239,0.985321101,0.987155963,
0.988990826,0.990825688,0.99266055,0.994495413,0.996330275,0.998165138,
1.),.UNSPECIFIED.);
#24492=B_SPLINE_CURVE_WITH_KNOTS('',3,(#297177,#297178,#297179,#297180,
#297181,#297182,#297183,#297184,#297185,#297186,#297187,#297188,#297189,
#297190,#297191,#297192,#297193,#297194,#297195,#297196,#297197,#297198,
#297199,#297200,#297201,#297202,#297203,#297204,#297205,#297206,#297207,
#297208,#297209,#297210,#297211,#297212,#297213,#297214,#297215,#297216,
#297217,#297218,#297219,#297220,#297221,#297222,#297223,#297224,#297225,
#297226,#297227,#297228,#297229,#297230,#297231,#297232,#297233,#297234,
#297235,#297236,#297237,#297238,#297239,#297240,#297241,#297242,#297243,
#297244,#297245,#297246,#297247,#297248,#297249,#297250,#297251,#297252,
#297253,#297254,#297255,#297256,#297257,#297258,#297259,#297260,#297261,
#297262,#297263,#297264,#297265,#297266,#297267,#297268,#297269,#297270,
#297271,#297272,#297273,#297274,#297275,#297276,#297277,#297278,#297279,
#297280,#297281,#297282,#297283,#297284,#297285,#297286,#297287,#297288,
#297289,#297290,#297291,#297292,#297293,#297294,#297295,#297296,#297297,
#297298,#297299,#297300,#297301,#297302,#297303,#297304,#297305,#297306,
#297307,#297308,#297309,#297310,#297311,#297312,#297313,#297314,#297315,
#297316,#297317,#297318,#297319,#297320,#297321,#297322,#297323,#297324,
#297325,#297326,#297327,#297328,#297329,#297330,#297331,#297332,#297333,
#297334,#297335,#297336,#297337,#297338,#297339,#297340,#297341,#297342,
#297343,#297344,#297345,#297346,#297347,#297348,#297349,#297350,#297351,
#297352,#297353,#297354,#297355,#297356,#297357,#297358,#297359,#297360,
#297361,#297362,#297363,#297364,#297365,#297366,#297367,#297368,#297369,
#297370,#297371,#297372,#297373,#297374,#297375,#297376,#297377,#297378,
#297379,#297380,#297381,#297382,#297383,#297384,#297385,#297386,#297387,
#297388,#297389,#297390,#297391,#297392,#297393,#297394,#297395,#297396,
#297397,#297398,#297399,#297400,#297401,#297402,#297403,#297404,#297405,
#297406,#297407,#297408,#297409,#297410,#297411,#297412,#297413,#297414,
#297415,#297416,#297417,#297418,#297419,#297420,#297421,#297422,#297423,
#297424,#297425,#297426,#297427,#297428,#297429,#297430,#297431,#297432,
#297433,#297434,#297435,#297436,#297437,#297438,#297439,#297440,#297441,
#297442,#297443,#297444,#297445,#297446,#297447,#297448,#297449,#297450,
#297451,#297452,#297453,#297454,#297455,#297456,#297457,#297458,#297459,
#297460,#297461,#297462,#297463,#297464,#297465,#297466,#297467,#297468,
#297469,#297470,#297471,#297472,#297473,#297474,#297475,#297476,#297477,
#297478,#297479,#297480,#297481,#297482,#297483,#297484,#297485,#297486,
#297487,#297488,#297489,#297490,#297491,#297492,#297493,#297494,#297495,
#297496,#297497,#297498),.UNSPECIFIED.,.F.,.F.,(4,3,3,3,3,3,3,3,3,3,3,3,
3,3,3,3,3,3,3,3,3,3,3,3,3,3,3,3,3,3,3,3,3,3,3,3,3,3,3,3,3,3,3,3,3,3,3,3,
3,3,3,3,3,3,3,3,3,3,3,3,3,3,3,3,3,3,3,3,3,3,3,3,3,3,3,3,3,3,3,3,3,3,3,3,
3,3,3,3,3,3,3,3,3,3,3,3,3,3,3,3,3,3,3,3,3,3,3,4),(0.143172102,0.15412844,
0.165137615,0.176146789,0.187155963,0.198165138,0.209174312,0.220183486,
0.231192661,0.242201835,0.253211009,0.264220183,0.275229358,0.286238532,
0.297247706,0.308256881,0.319266055,0.330275229,0.341284404,0.352293578,
0.366972477,0.377981651,0.388990826,0.398165138,0.40733945,0.416513761,
0.425688073,0.434862385,0.444036697,0.455045872,0.464220183,0.473394495,
0.48440367,0.493577982,0.502752294,0.511926606,0.52293578,0.532110092,0.539449541,
0.546788991,0.555963303,0.565137615,0.572477064,0.579816514,0.587155963,
0.594495413,0.601834862,0.611009174,0.618348624,0.625688073,0.633027523,
0.640366972,0.647706422,0.655045872,0.662385321,0.669724771,0.67706422,
0.68440367,0.691743119,0.699082569,0.706422018,0.713761468,0.721100917,
0.728440367,0.735779817,0.743119266,0.750458716,0.757798165,0.765137615,
0.774311927,0.783486239,0.790825688,0.798165138,0.805504587,0.812844037,
0.818348624,0.823853211,0.829357798,0.834862385,0.840366972,0.84587156,
0.851376147,0.856880734,0.862385321,0.867889908,0.873394495,0.878899083,
0.88440367,0.889908257,0.895412844,0.902752294,0.908256881,0.913761468,
0.919266055,0.928440367,0.933944954,0.939449541,0.944954128,0.950458716,
0.955963303,0.96146789,0.966972477,0.972477064,0.977981651,0.983486239,
0.988990826,0.994495413,1.),.UNSPECIFIED.);
#24493=B_SPLINE_CURVE_WITH_KNOTS('',5,(#298459,#298460,#298461,#298462,
#298463,#298464,#298465,#298466,#298467,#298468,#298469,#298470,#298471,
#298472,#298473,#298474,#298475,#298476,#298477,#298478,#298479,#298480,
#298481,#298482,#298483,#298484,#298485,#298486,#298487,#298488,#298489,
#298490,#298491,#298492,#298493,#298494,#298495,#298496,#298497,#298498,
#298499,#298500,#298501,#298502,#298503,#298504,#298505,#298506,#298507,
#298508,#298509,#298510,#298511,#298512,#298513,#298514,#298515,#298516,
#298517,#298518,#298519,#298520,#298521,#298522,#298523,#298524,#298525,
#298526,#298527,#298528,#298529,#298530,#298531,#298532,#298533,#298534,
#298535,#298536,#298537,#298538,#298539,#298540,#298541,#298542,#298543,
#298544,#298545,#298546,#298547,#298548,#298549,#298550,#298551,#298552,
#298553,#298554,#298555,#298556,#298557,#298558,#298559,#298560,#298561,
#298562,#298563,#298564,#298565,#298566,#298567,#298568,#298569,#298570,
#298571,#298572,#298573,#298574,#298575,#298576,#298577,#298578,#298579,
#298580,#298581,#298582,#298583,#298584,#298585,#298586,#298587,#298588,
#298589,#298590,#298591,#298592,#298593,#298594,#298595,#298596,#298597,
#298598,#298599,#298600,#298601,#298602,#298603,#298604,#298605,#298606,
#298607,#298608,#298609,#298610,#298611,#298612,#298613,#298614,#298615,
#298616,#298617,#298618,#298619,#298620,#298621,#298622,#298623,#298624,
#298625,#298626,#298627,#298628,#298629,#298630,#298631,#298632,#298633,
#298634,#298635,#298636,#298637,#298638,#298639,#298640,#298641,#298642,
#298643,#298644,#298645,#298646,#298647,#298648,#298649,#298650,#298651,
#298652,#298653,#298654,#298655,#298656,#298657,#298658,#298659,#298660,
#298661,#298662,#298663,#298664,#298665,#298666,#298667,#298668,#298669,
#298670,#298671,#298672,#298673,#298674,#298675,#298676,#298677,#298678,
#298679,#298680,#298681,#298682,#298683,#298684,#298685,#298686,#298687,
#298688,#298689,#298690,#298691,#298692,#298693,#298694,#298695,#298696,
#298697,#298698,#298699,#298700,#298701,#298702,#298703,#298704,#298705,
#298706,#298707,#298708,#298709,#298710,#298711,#298712,#298713,#298714,
#298715,#298716,#298717,#298718,#298719,#298720,#298721,#298722,#298723,
#298724,#298725,#298726,#298727,#298728,#298729,#298730,#298731,#298732,
#298733,#298734,#298735,#298736,#298737,#298738,#298739,#298740,#298741,
#298742,#298743,#298744,#298745,#298746,#298747,#298748,#298749,#298750,
#298751,#298752,#298753,#298754,#298755,#298756,#298757,#298758,#298759,
#298760,#298761,#298762,#298763,#298764,#298765,#298766,#298767,#298768,
#298769,#298770,#298771,#298772,#298773,#298774,#298775,#298776,#298777,
#298778,#298779,#298780,#298781,#298782,#298783,#298784,#298785,#298786,
#298787,#298788,#298789,#298790,#298791,#298792,#298793,#298794,#298795,
#298796,#298797,#298798,#298799,#298800,#298801,#298802,#298803,#298804,
#298805,#298806,#298807,#298808,#298809,#298810,#298811,#298812,#298813,
#298814,#298815,#298816,#298817,#298818,#298819,#298820,#298821,#298822,
#298823,#298824,#298825,#298826,#298827,#298828,#298829,#298830,#298831,
#298832,#298833,#298834,#298835,#298836,#298837,#298838,#298839,#298840,
#298841,#298842,#298843,#298844,#298845,#298846,#298847,#298848,#298849,
#298850,#298851,#298852,#298853,#298854,#298855,#298856,#298857,#298858,
#298859,#298860,#298861,#298862,#298863,#298864,#298865,#298866,#298867,
#298868,#298869,#298870,#298871,#298872,#298873,#298874,#298875,#298876,
#298877,#298878,#298879,#298880,#298881,#298882,#298883,#298884,#298885,
#298886,#298887,#298888,#298889,#298890,#298891,#298892,#298893,#298894,
#298895,#298896,#298897,#298898,#298899,#298900,#298901,#298902,#298903,
#298904,#298905,#298906,#298907,#298908,#298909,#298910,#298911,#298912,
#298913,#298914,#298915,#298916,#298917,#298918,#298919,#298920,#298921,
#298922,#298923,#298924,#298925,#298926,#298927,#298928,#298929),
 .UNSPECIFIED.,.F.,.F.,(6,1,1,1,1,1,1,1,1,1,1,1,1,1,1,1,1,1,1,1,1,1,1,1,
1,1,1,1,1,1,1,1,1,1,1,1,1,1,1,1,1,1,1,1,1,1,1,1,1,1,1,1,1,1,1,1,1,1,1,1,
1,1,1,1,1,1,1,1,1,1,1,1,1,1,1,1,1,1,1,1,1,1,1,1,1,1,1,1,1,1,1,1,1,1,1,1,
1,1,1,1,1,1,1,1,1,1,1,1,1,1,1,1,1,1,1,1,1,1,1,1,1,1,1,1,1,1,1,1,1,1,1,1,
1,1,1,1,1,1,1,1,1,1,1,1,1,1,1,1,1,1,1,1,1,1,1,1,1,1,1,1,1,1,1,1,1,1,1,1,
1,1,1,1,1,1,1,1,1,1,1,1,1,1,1,1,1,1,1,1,1,1,1,1,1,1,1,1,1,1,1,1,1,1,1,1,
1,1,1,1,1,1,1,1,1,1,1,1,1,1,1,1,1,1,1,1,1,1,1,1,1,1,1,1,1,1,1,1,1,1,1,1,
1,1,1,1,1,1,1,1,1,1,1,1,1,1,1,1,1,1,1,1,1,1,1,1,1,1,1,1,1,1,1,1,1,1,1,1,
1,1,1,1,1,1,1,1,1,1,1,1,1,1,1,1,1,1,1,1,1,1,1,1,1,1,1,1,1,1,1,1,1,1,1,1,
1,1,1,1,1,1,1,1,1,1,1,1,1,1,1,1,1,1,1,1,1,1,1,1,1,1,1,1,1,1,1,1,1,1,1,1,
1,1,1,1,1,1,1,1,1,1,1,1,1,1,1,1,1,1,1,1,1,1,1,1,1,1,1,1,1,1,1,1,1,1,1,1,
1,1,1,1,1,1,1,1,1,1,1,1,1,1,1,1,1,1,1,1,1,1,1,1,1,1,1,1,1,1,1,1,1,1,1,1,
1,1,1,1,1,1,1,1,1,1,1,1,1,1,1,1,1,1,1,1,1,1,1,1,1,1,1,1,1,1,1,1,1,1,1,1,
1,1,1,1,1,1,1,1,1,1,6),(-1.,-0.998165138,-0.996330275,-0.994495413,-0.99266055,
-0.990825688,-0.988990826,-0.987155963,-0.985321101,-0.983486239,-0.981651376,
-0.979816514,-0.977981651,-0.976146789,-0.974311927,-0.972477064,-0.970642202,
-0.968807339,-0.966972477,-0.965137615,-0.963302752,-0.96146789,-0.959633028,
-0.957798165,-0.955963303,-0.95412844,-0.952293578,-0.950458716,-0.948623853,
-0.946788991,-0.944954128,-0.943119266,-0.941284404,-0.939449541,-0.937614679,
-0.935779817,-0.933944954,-0.932110092,-0.930275229,-0.928440367,-0.926605505,
-0.924770642,-0.92293578,-0.921100917,-0.919266055,-0.917431193,-0.91559633,
-0.913761468,-0.911926606,-0.910091743,-0.908256881,-0.906422018,-0.904587156,
-0.902752294,-0.900917431,-0.899082569,-0.897247706,-0.895412844,-0.893577982,
-0.891743119,-0.889908257,-0.888073394,-0.886238532,-0.88440367,-0.882568807,
-0.880733945,-0.878899083,-0.87706422,-0.875229358,-0.873394495,-0.871559633,
-0.869724771,-0.867889908,-0.866055046,-0.864220183,-0.862385321,-0.860550459,
-0.858715596,-0.856880734,-0.855045872,-0.853211009,-0.851376147,-0.849541284,
-0.847706422,-0.84587156,-0.844036697,-0.842201835,-0.840366972,-0.83853211,
-0.836697248,-0.834862385,-0.833027523,-0.831192661,-0.829357798,-0.827522936,
-0.825688073,-0.823853211,-0.822018349,-0.820183486,-0.818348624,-0.816513761,
-0.814678899,-0.812844037,-0.811009174,-0.809174312,-0.80733945,-0.805504587,
-0.803669725,-0.801834862,-0.8,-0.798165138,-0.796330275,-0.794495413,-0.79266055,
-0.790825688,-0.788990826,-0.787155963,-0.785321101,-0.783486239,-0.781651376,
-0.779816514,-0.777981651,-0.776146789,-0.774311927,-0.772477064,-0.770642202,
-0.768807339,-0.766972477,-0.765137615,-0.763302752,-0.76146789,-0.759633028,
-0.757798165,-0.755963303,-0.75412844,-0.752293578,-0.750458716,-0.748623853,
-0.746788991,-0.744954128,-0.743119266,-0.741284404,-0.739449541,-0.737614679,
-0.735779817,-0.733944954,-0.732110092,-0.730275229,-0.728440367,-0.726605505,
-0.724770642,-0.72293578,-0.721100917,-0.719266055,-0.717431193,-0.71559633,
-0.713761468,-0.711926606,-0.710091743,-0.708256881,-0.706422018,-0.704587156,
-0.702752294,-0.700917431,-0.699082569,-0.697247706,-0.695412844,-0.693577982,
-0.691743119,-0.689908257,-0.688073394,-0.686238532,-0.68440367,-0.682568807,
-0.680733945,-0.678899083,-0.67706422,-0.675229358,-0.673394495,-0.671559633,
-0.669724771,-0.667889908,-0.666055046,-0.664220183,-0.662385321,-0.660550459,
-0.658715596,-0.656880734,-0.655045872,-0.653211009,-0.651376147,-0.649541284,
-0.647706422,-0.64587156,-0.644036697,-0.642201835,-0.640366972,-0.63853211,
-0.636697248,-0.634862385,-0.633027523,-0.631192661,-0.629357798,-0.627522936,
-0.625688073,-0.623853211,-0.622018349,-0.620183486,-0.618348624,-0.616513761,
-0.614678899,-0.612844037,-0.611009174,-0.609174312,-0.60733945,-0.605504587,
-0.603669725,-0.601834862,-0.6,-0.598165138,-0.596330275,-0.594495413,-0.59266055,
-0.590825688,-0.588990826,-0.587155963,-0.585321101,-0.583486239,-0.581651376,
-0.579816514,-0.577981651,-0.576146789,-0.574311927,-0.572477064,-0.570642202,
-0.568807339,-0.566972477,-0.565137615,-0.563302752,-0.56146789,-0.559633028,
-0.557798165,-0.555963303,-0.55412844,-0.552293578,-0.550458716,-0.548623853,
-0.546788991,-0.544954128,-0.543119266,-0.541284404,-0.539449541,-0.537614679,
-0.535779817,-0.533944954,-0.532110092,-0.530275229,-0.528440367,-0.526605505,
-0.524770642,-0.52293578,-0.521100917,-0.519266055,-0.517431193,-0.51559633,
-0.513761468,-0.511926606,-0.508256881,-0.506422018,-0.504587156,-0.502752294,
-0.500917431,-0.499082569,-0.497247706,-0.495412844,-0.493577982,-0.491743119,
-0.489908257,-0.488073394,-0.486238532,-0.48440367,-0.482568807,-0.480733945,
-0.478899083,-0.47706422,-0.475229358,-0.473394495,-0.471559633,-0.469724771,
-0.467889908,-0.466055046,-0.464220183,-0.462385321,-0.460550459,-0.458715596,
-0.456880734,-0.455045872,-0.453211009,-0.451376147,-0.449541284,-0.447706422,
-0.44587156,-0.444036697,-0.442201835,-0.440366972,-0.43853211,-0.436697248,
-0.434862385,-0.433027523,-0.431192661,-0.429357798,-0.427522936,-0.425688073,
-0.423853211,-0.422018349,-0.420183486,-0.418348624,-0.416513761,-0.414678899,
-0.412844037,-0.411009174,-0.409174312,-0.40733945,-0.405504587,-0.403669725,
-0.401834862,-0.4,-0.398165138,-0.396330275,-0.394495413,-0.39266055,-0.390825688,
-0.388990826,-0.387155963,-0.385321101,-0.383486239,-0.381651376,-0.379816514,
-0.377981651,-0.376146789,-0.374311927,-0.372477064,-0.370642202,-0.368807339,
-0.366972477,-0.365137615,-0.363302752,-0.36146789,-0.359633028,-0.357798165,
-0.355963303,-0.35412844,-0.352293578,-0.350458716,-0.348623853,-0.346788991,
-0.344954128,-0.343119266,-0.341284404,-0.339449541,-0.337614679,-0.335779817,
-0.333944954,-0.332110092,-0.330275229,-0.328440367,-0.326605505,-0.324770642,
-0.32293578,-0.321100917,-0.319266055,-0.317431193,-0.31559633,-0.313761468,
-0.311926606,-0.310091743,-0.308256881,-0.306422018,-0.304587156,-0.302752294,
-0.300917431,-0.299082569,-0.297247706,-0.295412844,-0.293577982,-0.291743119,
-0.289908257,-0.288073394,-0.286238532,-0.28440367,-0.282568807,-0.280733945,
-0.278899083,-0.27706422,-0.275229358,-0.273394495,-0.271559633,-0.269724771,
-0.267889908,-0.266055046,-0.264220183,-0.262385321,-0.260550459,-0.258715596,
-0.256880734,-0.255045872,-0.253211009,-0.251376147,-0.249541284,-0.247706422,
-0.24587156,-0.244036697,-0.242201835,-0.240366972,-0.23853211,-0.236697248,
-0.234862385,-0.233027523,-0.231192661,-0.229357798,-0.227522936,-0.225688073,
-0.223853211,-0.222018349,-0.220183486,-0.218348624,-0.216513761,-0.214678899,
-0.212844037,-0.211009174,-0.209174312,-0.20733945,-0.205504587,-0.203669725,
-0.201834862,-0.2,-0.198165138,-0.196330275,-0.194495413,-0.19266055,-0.190825688,
-0.188990826,-0.187155963,-0.185321101,-0.183486239,-0.181651376,-0.179816514,
-0.177981651,-0.176146789,-0.174311927,-0.172477064,-0.170642202,-0.168807339,
-0.166972477,-0.165137615,-0.163302752,-0.16146789,-0.159633028,-0.157798165,
-0.155963303,-0.15412844,-0.152293578,-0.150458716,-0.148623853,-0.146788991,
-0.144954128,-0.143172102),.UNSPECIFIED.);
#24494=B_SPLINE_CURVE_WITH_KNOTS('',3,(#299874,#299875,#299876,#299877,
#299878,#299879,#299880,#299881,#299882,#299883,#299884,#299885,#299886,
#299887,#299888,#299889,#299890,#299891,#299892,#299893,#299894,#299895,
#299896,#299897,#299898,#299899,#299900,#299901,#299902,#299903,#299904,
#299905,#299906,#299907,#299908,#299909,#299910,#299911,#299912,#299913,
#299914,#299915,#299916,#299917,#299918,#299919,#299920,#299921,#299922,
#299923,#299924,#299925,#299926,#299927,#299928,#299929,#299930,#299931,
#299932,#299933,#299934,#299935,#299936,#299937,#299938,#299939,#299940,
#299941,#299942,#299943,#299944,#299945,#299946,#299947,#299948,#299949,
#299950,#299951,#299952,#299953,#299954,#299955,#299956,#299957,#299958,
#299959,#299960,#299961,#299962,#299963,#299964,#299965,#299966,#299967,
#299968,#299969,#299970,#299971,#299972,#299973,#299974,#299975,#299976,
#299977,#299978,#299979,#299980,#299981,#299982,#299983,#299984,#299985,
#299986,#299987,#299988,#299989,#299990,#299991,#299992,#299993,#299994,
#299995,#299996,#299997,#299998,#299999,#300000,#300001,#300002,#300003,
#300004,#300005,#300006,#300007,#300008,#300009,#300010,#300011,#300012,
#300013,#300014,#300015,#300016,#300017,#300018,#300019,#300020,#300021,
#300022,#300023,#300024,#300025,#300026,#300027,#300028,#300029,#300030,
#300031,#300032,#300033,#300034,#300035,#300036,#300037,#300038,#300039,
#300040,#300041,#300042,#300043,#300044,#300045,#300046,#300047,#300048,
#300049,#300050,#300051,#300052,#300053,#300054,#300055,#300056,#300057,
#300058,#300059,#300060,#300061,#300062,#300063,#300064,#300065,#300066,
#300067,#300068,#300069,#300070,#300071,#300072,#300073,#300074,#300075,
#300076,#300077,#300078,#300079,#300080,#300081,#300082,#300083,#300084,
#300085,#300086,#300087,#300088,#300089,#300090,#300091,#300092,#300093,
#300094,#300095,#300096,#300097,#300098,#300099,#300100,#300101,#300102,
#300103,#300104,#300105,#300106,#300107,#300108,#300109,#300110,#300111,
#300112,#300113,#300114,#300115,#300116,#300117,#300118,#300119,#300120,
#300121,#300122,#300123,#300124,#300125,#300126,#300127,#300128,#300129,
#300130,#300131,#300132,#300133,#300134,#300135,#300136,#300137,#300138,
#300139,#300140,#300141,#300142,#300143,#300144,#300145,#300146,#300147,
#300148,#300149,#300150,#300151,#300152,#300153,#300154,#300155,#300156,
#300157,#300158,#300159,#300160,#300161,#300162,#300163,#300164,#300165,
#300166,#300167,#300168,#300169,#300170,#300171,#300172,#300173,#300174,
#300175,#300176,#300177,#300178,#300179,#300180,#300181,#300182,#300183,
#300184,#300185,#300186,#300187,#300188,#300189,#300190,#300191,#300192,
#300193,#300194,#300195),.UNSPECIFIED.,.F.,.F.,(4,3,3,3,3,3,3,3,3,3,3,3,
3,3,3,3,3,3,3,3,3,3,3,3,3,3,3,3,3,3,3,3,3,3,3,3,3,3,3,3,3,3,3,3,3,3,3,3,
3,3,3,3,3,3,3,3,3,3,3,3,3,3,3,3,3,3,3,3,3,3,3,3,3,3,3,3,3,3,3,3,3,3,3,3,
3,3,3,3,3,3,3,3,3,3,3,3,3,3,3,3,3,3,3,3,3,3,3,4),(0.143172102,0.15412844,
0.165137615,0.176146789,0.187155963,0.198165138,0.209174312,0.220183486,
0.231192661,0.242201835,0.253211009,0.264220183,0.275229358,0.286238532,
0.297247706,0.308256881,0.319266055,0.330275229,0.341284404,0.352293578,
0.363302752,0.374311927,0.385321101,0.396330275,0.405504587,0.414678899,
0.423853211,0.433027523,0.442201835,0.451376147,0.460550459,0.471559633,
0.480733945,0.489908257,0.499082569,0.508256881,0.517431193,0.526605505,
0.533944954,0.541284404,0.550458716,0.557798165,0.565137615,0.572477064,
0.579816514,0.587155963,0.594495413,0.601834862,0.609174312,0.616513761,
0.623853211,0.631192661,0.63853211,0.64587156,0.653211009,0.660550459,0.667889908,
0.675229358,0.682568807,0.689908257,0.697247706,0.706422018,0.713761468,
0.72293578,0.733944954,0.741284404,0.748623853,0.755963303,0.763302752,
0.770642202,0.777981651,0.785321101,0.79266055,0.8,0.80733945,0.812844037,
0.818348624,0.823853211,0.829357798,0.834862385,0.842201835,0.847706422,
0.853211009,0.858715596,0.864220183,0.869724771,0.875229358,0.880733945,
0.886238532,0.891743119,0.897247706,0.902752294,0.908256881,0.913761468,
0.921100917,0.928440367,0.933944954,0.939449541,0.944954128,0.950458716,
0.955963303,0.96146789,0.966972477,0.972477064,0.979816514,0.985321101,
0.990825688,1.),.UNSPECIFIED.);
#24495=B_SPLINE_CURVE_WITH_KNOTS('',3,(#300224,#300225,#300226,#300227,
#300228,#300229,#300230,#300231,#300232,#300233,#300234,#300235,#300236,
#300237),.UNSPECIFIED.,.F.,.F.,(4,2,2,2,2,2,4),(2.25701232429112E-11,0.00014460912609736,
0.000387015548692996,0.00125700195661841,0.00435168228607041,0.0129718164294565,
0.0227694264116158),.UNSPECIFIED.);
#24496=B_SPLINE_CURVE_WITH_KNOTS('',3,(#300241,#300242,#300243,#300244,
#300245,#300246,#300247,#300248,#300249,#300250,#300251,#300252,#300253,
#300254,#300255,#300256,#300257,#300258,#300259,#300260,#300261,#300262,
#300263,#300264,#300265,#300266,#300267,#300268,#300269,#300270,#300271,
#300272,#300273,#300274,#300275,#300276,#300277,#300278,#300279,#300280,
#300281,#300282,#300283),.UNSPECIFIED.,.F.,.F.,(4,3,3,3,3,3,3,3,3,3,3,3,
3,3,4),(0.,9.41174796889181E-5,0.000189798325007615,0.000281495822455474,
0.000370505462955499,0.000455579152157681,0.000536999972207846,0.000612533789895692,
0.000685472418224339,0.000755118709112169,0.000789941854556085,0.000807353427278042,
0.000816059213639021,0.000822483140370077,0.000824765),.UNSPECIFIED.);
#24497=B_SPLINE_CURVE_WITH_KNOTS('',3,(#300291,#300292,#300293,#300294,
#300295,#300296,#300297,#300298,#300299,#300300,#300301,#300302,#300303,
#300304,#300305,#300306),.UNSPECIFIED.,.F.,.F.,(4,2,2,2,2,2,2,4),(7.39439642544424E-11,
8.13967315243824E-5,0.000253968783894778,0.000853738707014911,0.00300176120327824,
0.0106434682371973,0.0317998204262259,0.0557341748263668),.UNSPECIFIED.);
#24498=B_SPLINE_CURVE_WITH_KNOTS('',3,(#300310,#300311,#300312,#300313,
#300314,#300315,#300316,#300317,#300318,#300319,#300320,#300321,#300322,
#300323,#300324,#300325,#300326,#300327,#300328,#300329,#300330,#300331,
#300332,#300333,#300334,#300335,#300336,#300337,#300338,#300339,#300340,
#300341,#300342,#300343,#300344,#300345,#300346,#300347,#300348,#300349,
#300350,#300351,#300352,#300353,#300354,#300355),.UNSPECIFIED.,.F.,.F.,
(4,3,3,3,3,3,3,3,3,3,3,3,3,3,3,4),(0.,4.941415498036E-5,0.000146434010607815,
0.000239410220049695,0.000329337302265598,0.000416482292794944,0.00049829791801492,
0.00058011668851119,0.000653699456822933,0.000724251506183855,0.000774912253091927,
0.000800242626545964,0.000812907813272982,0.000820432326079254,0.000824400885159964,
0.000825573),.UNSPECIFIED.);
#24499=B_SPLINE_CURVE_WITH_KNOTS('',3,(#300363,#300364,#300365,#300366,
#300367,#300368,#300369,#300370,#300371,#300372,#300373,#300374,#300375,
#300376,#300377,#300378),.UNSPECIFIED.,.F.,.F.,(4,2,2,2,2,2,2,4),(2.13294581190719E-11,
8.13972158757993E-5,0.000254130774603711,0.00085480314270949,0.00300872290067678,
0.0106706763397779,0.0320130172357565,0.0562945640523578),.UNSPECIFIED.);
#24500=B_SPLINE_CURVE_WITH_KNOTS('',3,(#300382,#300383,#300384,#300385,
#300386,#300387,#300388,#300389,#300390,#300391,#300392,#300393,#300394,
#300395,#300396,#300397,#300398,#300399,#300400,#300401,#300402,#300403,
#300404,#300405,#300406,#300407,#300408,#300409,#300410,#300411,#300412,
#300413,#300414,#300415,#300416,#300417,#300418,#300419,#300420,#300421,
#300422,#300423,#300424,#300425,#300426,#300427),.UNSPECIFIED.,.F.,.F.,
(4,3,3,3,3,3,3,3,3,3,3,3,3,3,3,4),(0.,5.42807591518338E-5,0.000150811400407988,
0.000244155385409474,0.000333984770718417,0.000420334676603205,0.000503129576977275,
0.000583740432732957,0.000657800501529321,0.000728470586106261,0.000777021793053131,
0.000801297396526565,0.000813435198263283,0.000820820805650379,0.000824774446497117,
0.000825573),.UNSPECIFIED.);
#24501=B_SPLINE_CURVE_WITH_KNOTS('',3,(#300435,#300436,#300437,#300438,
#300439,#300440,#300441,#300442,#300443,#300444,#300445,#300446,#300447,
#300448,#300449,#300450),.UNSPECIFIED.,.F.,.F.,(4,2,2,2,2,2,2,4),(6.59801867899649E-11,
8.13970156620257E-5,0.000253894448343603,0.000852930654053306,0.00300001860986496,
0.0106403949523925,0.0318561104701801,0.055916116834572),.UNSPECIFIED.);
#24502=B_SPLINE_CURVE_WITH_KNOTS('',3,(#300454,#300455,#300456,#300457,
#300458,#300459,#300460,#300461,#300462,#300463,#300464,#300465,#300466,
#300467,#300468,#300469,#300470,#300471,#300472,#300473,#300474,#300475,
#300476,#300477,#300478,#300479,#300480,#300481,#300482,#300483,#300484,
#300485,#300486,#300487,#300488,#300489,#300490,#300491,#300492,#300493,
#300494,#300495,#300496,#300497,#300498,#300499),.UNSPECIFIED.,.F.,.F.,
(4,3,3,3,3,3,3,3,3,3,3,3,3,3,3,4),(0.,5.29278932285465E-5,0.000149986829614398,
0.000243421723444812,0.000333607658851719,0.000420839426742773,0.000504993867908082,
0.000585138650931061,0.000659165774865394,0.000730100379889144,0.000777836689944572,
0.000801704844972286,0.000813638922486143,0.000820965828956536,0.000825017897538137,
0.000825573),.UNSPECIFIED.);
#24503=B_SPLINE_CURVE_WITH_KNOTS('',3,(#300507,#300508,#300509,#300510,
#300511,#300512,#300513,#300514,#300515,#300516,#300517,#300518,#300519,
#300520),.UNSPECIFIED.,.F.,.F.,(4,2,2,2,2,2,4),(0.,5.18053291669203E-5,
0.000134730876905741,0.000431948787567479,0.0014896022211569,0.00442861890037952,
0.00776247261062754),.UNSPECIFIED.);
#24504=B_SPLINE_CURVE_WITH_KNOTS('',3,(#300524,#300525,#300526,#300527,
#300528,#300529,#300530,#300531,#300532,#300533,#300534,#300535,#300536,
#300537,#300538,#300539,#300540,#300541,#300542,#300543,#300544,#300545,
#300546,#300547,#300548,#300549,#300550,#300551,#300552,#300553,#300554,
#300555,#300556,#300557,#300558,#300559,#300560,#300561,#300562,#300563,
#300564,#300565,#300566),.UNSPECIFIED.,.F.,.F.,(4,3,3,3,3,3,3,3,3,3,3,3,
3,3,4),(0.,6.51902922437498E-5,0.000162212835330501,0.000255542669811936,
0.00034594997855667,0.000431821393210348,0.000515057799381166,0.000592686599535874,
0.000666391521959597,0.000737527223809127,0.000781550111904564,0.000803561555952282,
0.000814567277976141,0.000821645382533787,0.000825573),.UNSPECIFIED.);
#24505=B_SPLINE_CURVE_WITH_KNOTS('',3,(#300574,#300575,#300576,#300577,
#300578,#300579,#300580,#300581,#300582,#300583,#300584,#300585,#300586,
#300587,#300588,#300589),.UNSPECIFIED.,.F.,.F.,(4,2,2,2,2,2,2,4),(3.51269554446888E-11,
8.1397365043496E-5,0.000254102099395071,0.000854503471652061,0.00300783666884981,
0.0106666072947153,0.03195064404952,0.0561014629629725),.UNSPECIFIED.);
#24506=B_SPLINE_CURVE_WITH_KNOTS('',3,(#300593,#300594,#300595,#300596,
#300597,#300598,#300599,#300600,#300601,#300602,#300603,#300604,#300605,
#300606,#300607,#300608),.UNSPECIFIED.,.F.,.F.,(4,2,2,2,2,2,2,4),(0.,0.0414356907890881,
0.078170361387943,0.0913935848277746,0.0950979482415805,0.0961248369214223,
0.0964175430082423,0.0964926788806888),.UNSPECIFIED.);
#24507=B_SPLINE_CURVE_WITH_KNOTS('',3,(#300616,#300617,#300618,#300619,
#300620,#300621,#300622,#300623,#300624,#300625,#300626,#300627,#300628,
#300629,#300630,#300631),.UNSPECIFIED.,.F.,.F.,(4,2,2,2,2,2,2,4),(0.,8.13972245530873E-5,
0.00025378453400524,0.000851890925250522,0.00299507223923743,0.0106160714793745,
0.0318434026249517,0.0559770818334918),.UNSPECIFIED.);
#24508=B_SPLINE_CURVE_WITH_KNOTS('',3,(#300635,#300636,#300637,#300638,
#300639,#300640,#300641,#300642,#300643,#300644,#300645,#300646,#300647,
#300648,#300649,#300650,#300651,#300652,#300653,#300654,#300655,#300656,
#300657,#300658,#300659,#300660,#300661,#300662,#300663,#300664,#300665,
#300666,#300667,#300668,#300669,#300670,#300671,#300672,#300673,#300674,
#300675,#300676,#300677,#300678,#300679,#300680),.UNSPECIFIED.,.F.,.F.,
(4,3,3,3,3,3,3,3,3,3,3,3,3,3,3,4),(0.,5.66433572362371E-5,0.000153093585172818,
0.000245871068686411,0.000336099718589312,0.000423313353825591,0.000506253798565061,
0.000586083598923796,0.000659559573703011,0.000729754691205078,0.000777663845602539,
0.00080161842280127,0.000813595711400635,0.000820938523245592,0.000824948241415582,
0.000825573),.UNSPECIFIED.);
#24509=B_SPLINE_CURVE_WITH_KNOTS('',3,(#300688,#300689,#300690,#300691,
#300692,#300693,#300694,#300695,#300696,#300697,#300698,#300699,#300700,
#300701,#300702,#300703),.UNSPECIFIED.,.F.,.F.,(4,2,2,2,2,2,2,4),(2.38027376745489E-11,
8.13970695358414E-5,0.000253842437580032,0.00085198275120837,0.00299535207411838,
0.0106223872937026,0.0317449404823533,0.0556503449296871),.UNSPECIFIED.);
#24510=B_SPLINE_CURVE_WITH_KNOTS('',3,(#300707,#300708,#300709,#300710,
#300711,#300712,#300713,#300714,#300715,#300716),.UNSPECIFIED.,.F.,.F.,
(4,2,2,2,4),(0.,0.0415132221635862,0.0782472088689811,0.0914322683673314,
0.100763837421976),.UNSPECIFIED.);
#24511=B_SPLINE_CURVE_WITH_KNOTS('',3,(#300724,#300725,#300726,#300727,
#300728,#300729,#300730,#300731,#300732,#300733,#300734,#300735,#300736,
#300737,#300738,#300739),.UNSPECIFIED.,.F.,.F.,(4,2,2,2,2,2,2,4),(2.53031513835136E-11,
8.13974294458811E-5,0.000254077418613046,0.000853925999930095,0.00300624123794232,
0.0106626452969989,0.0319062118029417,0.0559886272275276),.UNSPECIFIED.);
#24512=B_SPLINE_CURVE_WITH_KNOTS('',3,(#300743,#300744,#300745,#300746,
#300747,#300748,#300749,#300750,#300751,#300752,#300753,#300754,#300755,
#300756,#300757,#300758,#300759,#300760,#300761,#300762,#300763,#300764,
#300765,#300766,#300767,#300768,#300769,#300770,#300771,#300772,#300773,
#300774,#300775,#300776,#300777,#300778,#300779,#300780,#300781,#300782,
#300783,#300784,#300785),.UNSPECIFIED.,.F.,.F.,(4,3,3,3,3,3,3,3,3,3,3,3,
3,3,4),(0.,5.2655145774557E-5,0.000149453317664655,0.00024236950728625,
0.00033244565288107,0.000419142399915971,0.000502353712462079,0.00058294328434656,
0.000656613938861597,0.000727097094331266,0.000775904547165633,0.000800308273582816,
0.000812510136791408,0.000820061384306642,0.000824712),.UNSPECIFIED.);
#24513=B_SPLINE_CURVE_WITH_KNOTS('',3,(#300793,#300794,#300795,#300796,
#300797,#300798,#300799,#300800,#300801,#300802,#300803,#300804,#300805,
#300806,#300807,#300808),.UNSPECIFIED.,.F.,.F.,(4,2,2,2,2,2,2,4),(0.,8.13968219775296E-5,
0.000253912214223537,0.000852767064929133,0.00299685323830034,0.0106260266679204,
0.0318487307217364,0.0559555570626083),.UNSPECIFIED.);
#24514=B_SPLINE_CURVE_WITH_KNOTS('',3,(#300812,#300813,#300814,#300815,
#300816,#300817,#300818,#300819,#300820,#300821,#300822,#300823,#300824,
#300825,#300826,#300827,#300828,#300829,#300830,#300831,#300832,#300833,
#300834,#300835,#300836,#300837,#300838,#300839,#300840,#300841,#300842,
#300843,#300844,#300845,#300846,#300847,#300848,#300849,#300850,#300851,
#300852,#300853,#300854),.UNSPECIFIED.,.F.,.F.,(4,3,3,3,3,3,3,3,3,3,3,3,
3,3,4),(0.,7.64101055378754E-5,0.000172695683197778,0.000265061951152557,
0.000354046629123992,0.000439529472553468,0.000521166539457513,0.000597300157860763,
0.000670487364037656,0.000740507990601729,0.000782608495300864,0.000803658747650432,
0.000814183873825216,0.000821298407202764,0.000824709),.UNSPECIFIED.);
#24515=B_SPLINE_CURVE_WITH_KNOTS('',3,(#300862,#300863,#300864,#300865,
#300866,#300867,#300868,#300869,#300870,#300871,#300872,#300873,#300874,
#300875,#300876,#300877),.UNSPECIFIED.,.F.,.F.,(4,2,2,2,2,2,2,4),(1.23364205350419E-12,
8.13969099647976E-5,0.000253632227414641,0.00085030471521368,0.00299164645435722,
0.0106059199915171,0.0317135536556019,0.0556224300991424),.UNSPECIFIED.);
#24516=B_SPLINE_CURVE_WITH_KNOTS('',3,(#300881,#300882,#300883,#300884,
#300885,#300886,#300887,#300888,#300889,#300890,#300891,#300892,#300893,
#300894,#300895,#300896),.UNSPECIFIED.,.F.,.F.,(4,2,2,2,2,2,2,4),(0.,0.0414635861754931,
0.0780958470122907,0.0912237647252485,0.0949045241674999,0.0959245951421665,
0.0962158581650039,0.0962727721750899),.UNSPECIFIED.);
#24517=B_SPLINE_CURVE_WITH_KNOTS('',3,(#300904,#300905,#300906,#300907,
#300908,#300909,#300910,#300911,#300912,#300913,#300914,#300915,#300916,
#300917,#300918,#300919),.UNSPECIFIED.,.F.,.F.,(4,2,2,2,2,2,2,4),(0.,8.13968331260338E-5,
0.000253734977402965,0.000851565104860571,0.00299597558175975,0.0106208094079658,
0.0318922880572177,0.0561185877997889),.UNSPECIFIED.);
#24518=B_SPLINE_CURVE_WITH_KNOTS('',3,(#300923,#300924,#300925,#300926,
#300927,#300928,#300929,#300930,#300931,#300932,#300933,#300934,#300935,
#300936,#300937,#300938,#300939,#300940,#300941,#300942,#300943,#300944,
#300945,#300946,#300947,#300948,#300949,#300950,#300951,#300952,#300953,
#300954,#300955,#300956,#300957,#300958,#300959,#300960,#300961,#300962,
#300963,#300964,#300965),.UNSPECIFIED.,.F.,.F.,(4,3,3,3,3,3,3,3,3,3,3,3,
3,3,4),(0.,7.71827982783351E-5,0.000173267568397164,0.000265457127481624,
0.0003540795695718,0.000439673818397658,0.000522355464935158,0.000598683552368119,
0.0006716060037561,0.000741338134319915,0.000783024567159957,0.000803867783579979,
0.000814289391789989,0.000821380251972883,0.000824711),.UNSPECIFIED.);
#24519=B_SPLINE_CURVE_WITH_KNOTS('',3,(#300973,#300974,#300975,#300976,
#300977,#300978,#300979,#300980,#300981,#300982,#300983,#300984,#300985,
#300986,#300987,#300988),.UNSPECIFIED.,.F.,.F.,(4,2,2,2,2,2,2,4),(1.6950339357606E-6,
8.82509104672641E-5,0.000704155174850886,0.00283747057980027,0.0104852329216673,
0.0376789761788421,0.11313592873392,0.19853018900161),.UNSPECIFIED.);
#24520=B_SPLINE_CURVE_WITH_KNOTS('',3,(#300992,#300993,#300994,#300995,
#300996,#300997,#300998,#300999,#301000,#301001,#301002,#301003,#301004,
#301005,#301006,#301007),.UNSPECIFIED.,.F.,.F.,(4,2,2,2,2,2,2,4),(0.,0.0413890254871353,
0.0780848812299061,0.0912986210594108,0.0950019425466635,0.0960280210265948,
0.0963205431802688,0.0964550788246295),.UNSPECIFIED.);
#24521=B_SPLINE_CURVE_WITH_KNOTS('',3,(#301015,#301016,#301017,#301018,
#301019,#301020,#301021,#301022,#301023,#301024,#301025,#301026,#301027,
#301028,#301029,#301030),.UNSPECIFIED.,.F.,.F.,(4,2,2,2,2,2,2,4),(7.86880354660446E-11,
8.13969307468172E-5,0.000254285399398094,0.000856228019329295,0.00301522849587095,
0.0106963537451455,0.0320464903672051,0.0562777029252997),.UNSPECIFIED.);
#24522=B_SPLINE_CURVE_WITH_KNOTS('',3,(#301034,#301035,#301036,#301037,
#301038,#301039,#301040,#301041,#301042,#301043,#301044,#301045,#301046,
#301047,#301048,#301049,#301050,#301051,#301052,#301053,#301054,#301055,
#301056,#301057,#301058,#301059,#301060,#301061,#301062,#301063,#301064,
#301065,#301066,#301067,#301068,#301069,#301070,#301071,#301072,#301073,
#301074,#301075,#301076),.UNSPECIFIED.,.F.,.F.,(4,3,3,3,3,3,3,3,3,3,3,3,
3,3,4),(0.,6.16345978401115E-5,0.000157957361618997,0.000250880688269924,
0.000340624421210286,0.000427077761505101,0.000509302370494405,0.000588154777870804,
0.000661875915878424,0.000732225403571121,0.00077846870178556,0.00080159035089278,
0.00081315117544639,0.000820521674856106,0.000824712),.UNSPECIFIED.);
#24523=B_SPLINE_CURVE_WITH_KNOTS('',3,(#301084,#301085,#301086,#301087,
#301088,#301089,#301090,#301091,#301092,#301093,#301094,#301095,#301096,
#301097,#301098,#301099),.UNSPECIFIED.,.F.,.F.,(4,2,2,2,2,2,2,4),(1.62974308173078E-11,
8.13975100572819E-5,0.000253856508698745,0.000852553741698134,0.0030001595828361,
0.0106431662956009,0.0318223136662569,0.0558016233755454),.UNSPECIFIED.);
#24524=B_SPLINE_CURVE_WITH_KNOTS('',3,(#301103,#301104,#301105,#301106,
#301107,#301108,#301109,#301110,#301111,#301112,#301113,#301114,#301115,
#301116,#301117,#301118,#301119,#301120,#301121,#301122,#301123,#301124,
#301125,#301126,#301127,#301128,#301129,#301130,#301131,#301132,#301133,
#301134,#301135,#301136,#301137,#301138,#301139,#301140,#301141,#301142,
#301143,#301144,#301145),.UNSPECIFIED.,.F.,.F.,(4,3,3,3,3,3,3,3,3,3,3,3,
3,3,4),(0.,6.92664471239441E-5,0.000165721395816546,0.000258076923380911,
0.000348102201228441,0.000435018589131858,0.000517171174703187,0.000594273881027391,
0.000667353678705221,0.000738000738388034,0.000781791369194017,0.000803686684597008,
0.000814634342298504,0.000821856532347001,0.000825582),.UNSPECIFIED.);
#24525=B_SPLINE_CURVE_WITH_KNOTS('',3,(#301153,#301154,#301155,#301156,
#301157,#301158,#301159,#301160,#301161,#301162,#301163,#301164,#301165,
#301166),.UNSPECIFIED.,.F.,.F.,(4,2,2,2,2,2,4),(0.,5.18051394548469E-5,
0.000128367922845272,0.000402522208456775,0.00137771990788599,0.00408898979740982,
0.00716687083262862),.UNSPECIFIED.);
#24526=B_SPLINE_CURVE_WITH_KNOTS('',3,(#301170,#301171,#301172,#301173,
#301174,#301175,#301176,#301177,#301178,#301179,#301180,#301181,#301182,
#301183,#301184,#301185,#301186,#301187,#301188,#301189,#301190,#301191,
#301192,#301193,#301194,#301195,#301196,#301197,#301198,#301199,#301200,
#301201,#301202,#301203,#301204,#301205,#301206,#301207,#301208,#301209,
#301210,#301211,#301212),.UNSPECIFIED.,.F.,.F.,(4,3,3,3,3,3,3,3,3,3,3,3,
3,3,4),(0.,5.58746352433121E-5,0.000152354364357929,0.000245709469640099,
0.000335378676716353,0.000422057938872853,0.000505266205972759,0.00058512740447957,
0.000658497474695901,0.000728864330876048,0.000776787665438024,0.000800749332719012,
0.000812730166359506,0.000820221726102288,0.000824711),.UNSPECIFIED.);
#24527=B_SPLINE_CURVE_WITH_KNOTS('',3,(#301220,#301221,#301222,#301223,
#301224,#301225,#301226,#301227,#301228,#301229,#301230,#301231,#301232,
#301233,#301234,#301235),.UNSPECIFIED.,.F.,.F.,(4,2,2,2,2,2,2,4),(0.,8.14316271732823E-5,
0.000254019368615236,0.000852992249264539,0.00300118055688404,0.0106403867837904,
0.0318742301277796,0.055957326667169),.UNSPECIFIED.);
#24528=B_SPLINE_CURVE_WITH_KNOTS('',3,(#301238,#301239,#301240,#301241,
#301242,#301243,#301244,#301245,#301246,#301247,#301248,#301249,#301250,
#301251,#301252,#301253,#301254,#301255,#301256,#301257,#301258,#301259,
#301260,#301261,#301262,#301263,#301264,#301265,#301266,#301267,#301268,
#301269,#301270,#301271,#301272,#301273,#301274,#301275,#301276,#301277,
#301278,#301279,#301280),.UNSPECIFIED.,.F.,.F.,(4,3,3,3,3,3,3,3,3,3,3,3,
3,3,4),(0.,5.65234098039017E-5,0.000152655733578414,0.000245589277354889,
0.000335372303709341,0.000421703798891314,0.000505835941831361,0.000585772456373521,
0.000659530275651245,0.000729462549350524,0.000777522274675262,0.000801552137337631,
0.000813567068668815,0.000821068664650334,0.000825582),.UNSPECIFIED.);
#24529=B_SPLINE_CURVE_WITH_KNOTS('',3,(#302948,#302949,#302950,#302951,
#302952,#302953,#302954,#302955),.UNSPECIFIED.,.F.,.F.,(4,2,2,4),(-0.0072109809393628,
-0.00368662560464412,-5.07022257993201E-5,0.),.UNSPECIFIED.);
#24530=B_SPLINE_CURVE_WITH_KNOTS('',3,(#304623,#304624,#304625,#304626,
#304627,#304628,#304629,#304630),.UNSPECIFIED.,.F.,.F.,(4,2,2,4),(-0.132132384477265,
-0.103054333069165,-0.0714351436644779,0.),.UNSPECIFIED.);
#24531=B_SPLINE_CURVE_WITH_KNOTS('',3,(#306287,#306288,#306289,#306290,
#306291,#306292,#306293,#306294),.UNSPECIFIED.,.F.,.F.,(4,2,2,4),(-0.00667991057808912,
-0.00369121128660005,-5.07020425170668E-5,0.),.UNSPECIFIED.);
#24532=B_SPLINE_CURVE_WITH_KNOTS('',3,(#307962,#307963,#307964,#307965,
#307966,#307967,#307968,#307969,#307970,#307971,#307972,#307973),
 .UNSPECIFIED.,.F.,.F.,(4,2,2,2,2,4),(-0.14481831420152,-0.141838119346234,
-0.137576959447593,-0.122254984206309,-0.0793476321617013,0.),
 .UNSPECIFIED.);
#24533=B_SPLINE_CURVE_WITH_KNOTS('',3,(#309630,#309631,#309632,#309633,
#309634,#309635,#309636,#309637),.UNSPECIFIED.,.F.,.F.,(4,2,2,4),(-0.00705981267369703,
-0.00371696437757226,-5.07022406769822E-5,0.),.UNSPECIFIED.);
#24534=B_SPLINE_CURVE_WITH_KNOTS('',3,(#311302,#311303,#311304,#311305,
#311306,#311307,#311308,#311309,#311310,#311311,#311312,#311313),
 .UNSPECIFIED.,.F.,.F.,(4,2,2,2,2,4),(-0.141987502057799,-0.138780518129329,
-0.134636509194115,-0.119855977748107,-0.0784036114991811,0.),
 .UNSPECIFIED.);
#24535=B_SPLINE_CURVE_WITH_KNOTS('',3,(#312970,#312971,#312972,#312973,
#312974,#312975,#312976,#312977),.UNSPECIFIED.,.F.,.F.,(4,2,2,4),(-0.00741228757948683,
-0.0037123551597383,-5.07021491017289E-5,0.),.UNSPECIFIED.);
#24536=B_SPLINE_CURVE_WITH_KNOTS('',3,(#314645,#314646,#314647,#314648,
#314649,#314650,#314651,#314652,#314653,#314654,#314655,#314656,#314657,
#314658,#314659,#314660),.UNSPECIFIED.,.F.,.F.,(4,2,2,2,2,2,2,4),(-0.132441264289709,
-0.132301752201889,-0.132011244623169,-0.130974107930178,-0.127242136360118,
-0.113828931045309,-0.0760058952801183,0.),.UNSPECIFIED.);
#24537=B_SPLINE_CURVE_WITH_KNOTS('',3,(#316317,#316318,#316319,#316320,
#316321,#316322,#316323,#316324),.UNSPECIFIED.,.F.,.F.,(4,2,2,4),(-0.00163871356828074,
-0.00100690578806506,-0.00010312555215194,0.),.UNSPECIFIED.);
#24538=B_SPLINE_CURVE_WITH_KNOTS('',3,(#317992,#317993,#317994,#317995,
#317996,#317997,#317998,#317999,#318000,#318001,#318002,#318003,#318004,
#318005,#318006,#318007),.UNSPECIFIED.,.F.,.F.,(4,2,2,2,2,2,2,4),(-0.138323148368157,
-0.138172915844685,-0.137860160282058,-0.13674324792726,-0.132729597365935,
-0.11829388670653,-0.0778047121160501,0.),.UNSPECIFIED.);
#24539=B_SPLINE_CURVE_WITH_KNOTS('',3,(#319664,#319665,#319666,#319667,
#319668,#319669,#319670,#319671),.UNSPECIFIED.,.F.,.F.,(4,2,2,4),(-0.00683207530728584,
-0.00374062884194389,-5.07020744551543E-5,0.),.UNSPECIFIED.);
#24540=B_SPLINE_CURVE_WITH_KNOTS('',3,(#321339,#321340,#321341,#321342,
#321343,#321344,#321345,#321346,#321347,#321348,#321349,#321350,#321351,
#321352,#321353,#321354),.UNSPECIFIED.,.F.,.F.,(4,2,2,2,2,2,2,4),(-0.143767075145791,
-0.143608474326114,-0.143277668302111,-0.142095827417839,-0.137843826166185,
-0.122558719084724,-0.0796101518115738,0.),.UNSPECIFIED.);
#24541=B_SPLINE_CURVE_WITH_KNOTS('',3,(#323011,#323012,#323013,#323014,
#323015,#323016,#323017,#323018),.UNSPECIFIED.,.F.,.F.,(4,2,2,4),(-0.00719768080497297,
-0.00370110887005153,-5.07021894051734E-5,0.),.UNSPECIFIED.);
#24542=B_SPLINE_CURVE_WITH_KNOTS('',3,(#324686,#324687,#324688,#324689,
#324690,#324691,#324692,#324693,#324694,#324695,#324696,#324697,#324698,
#324699,#324700,#324701),.UNSPECIFIED.,.F.,.F.,(4,2,2,2,2,2,2,4),(-0.14363224299588,
-0.143472580603887,-0.143140928986925,-0.141961284557612,-0.137718803195773,
-0.122454797987602,-0.0795494190128052,0.),.UNSPECIFIED.);
#24543=B_SPLINE_CURVE_WITH_KNOTS('',3,(#326358,#326359,#326360,#326361,
#326362,#326363,#326364,#326365),.UNSPECIFIED.,.F.,.F.,(4,2,2,4),(-0.00605122429428347,
-0.00366238405600456,-4.18241591403333E-5,0.),.UNSPECIFIED.);
#24544=B_SPLINE_CURVE_WITH_KNOTS('',3,(#328033,#328034,#328035,#328036,
#328037,#328038,#328039,#328040,#328041,#328042,#328043,#328044),
 .UNSPECIFIED.,.F.,.F.,(4,2,2,2,2,4),(-0.119546192578266,-0.117359437610194,
-0.114219520548498,-0.102929956115504,-0.0710513220875969,0.),
 .UNSPECIFIED.);
#24545=B_SPLINE_CURVE_WITH_KNOTS('',3,(#329701,#329702,#329703,#329704,
#329705,#329706,#329707,#329708),.UNSPECIFIED.,.F.,.F.,(4,2,2,4),(-0.0418544645696711,
-0.0252942680361084,-6.99729050106145E-5,0.),.UNSPECIFIED.);
#24546=B_SPLINE_CURVE_WITH_KNOTS('',3,(#329719,#329720,#329721,#329722,
#329723,#329724,#329725,#329726,#329727,#329728,#329729,#329730,#329731,
#329732,#329733,#329734),.UNSPECIFIED.,.F.,.F.,(4,2,2,2,2,2,2,4),(-0.129150425464729,
-0.129016270743863,-0.128736621265872,-0.127737293228282,-0.124145204909972,
-0.111227880552902,-0.0748499805365921,0.),.UNSPECIFIED.);
#24547=B_SPLINE_CURVE_WITH_KNOTS('',3,(#329738,#329739,#329740,#329741,
#329742,#329743,#329744,#329745),.UNSPECIFIED.,.F.,.F.,(4,2,2,4),(-0.00689158150654533,
-0.00365899181017955,-4.19445996243972E-5,0.),.UNSPECIFIED.);
#24548=B_SPLINE_CURVE_WITH_KNOTS('',3,(#329753,#329754,#329755,#329756,
#329757,#329758,#329759,#329760,#329761,#329762,#329763,#329764,#329765,
#329766,#329767,#329768),.UNSPECIFIED.,.F.,.F.,(4,2,2,2,2,2,2,4),(-0.119393705608938,
-0.119274862081618,-0.119027348912843,-0.118143922497865,-0.114963738502735,
-0.103517110080035,-0.0713053200773227,0.),.UNSPECIFIED.);
#24549=B_SPLINE_CURVE_WITH_KNOTS('',3,(#329772,#329773,#329774,#329775,
#329776,#329777,#329778,#329779),.UNSPECIFIED.,.F.,.F.,(4,2,2,4),(-0.00148881294802438,
-0.000834884330736283,-3.083227021591E-5,0.),.UNSPECIFIED.);
#24550=B_SPLINE_CURVE_WITH_KNOTS('',3,(#329787,#329788,#329789,#329790,
#329791,#329792,#329793,#329794,#329795,#329796,#329797,#329798,#329799,
#329800,#329801,#329802),.UNSPECIFIED.,.F.,.F.,(4,2,2,2,2,2,2,4),(-0.135670819220167,
-0.135524749497021,-0.13522124870382,-0.134142504666,-0.130258362648282,
-0.116280070506163,-0.0769984882364565,0.),.UNSPECIFIED.);
#24551=B_SPLINE_CURVE_WITH_KNOTS('',3,(#329806,#329807,#329808,#329809,
#329810,#329811,#329812,#329813),.UNSPECIFIED.,.F.,.F.,(4,2,2,4),(-0.00613306070600771,
-0.00372520969540507,-5.07021786216344E-5,0.),.UNSPECIFIED.);
#24552=B_SPLINE_CURVE_WITH_KNOTS('',3,(#329821,#329822,#329823,#329824,
#329825,#329826,#329827,#329828,#329829,#329830,#329831,#329832),
 .UNSPECIFIED.,.F.,.F.,(4,2,2,2,2,4),(-0.143766791143142,-0.140872566153918,
-0.136680946811064,-0.121606689071448,-0.079163682256657,0.),
 .UNSPECIFIED.);
#24553=B_SPLINE_CURVE_WITH_KNOTS('',3,(#329836,#329837,#329838,#329839,
#329840,#329841,#329842,#329843),.UNSPECIFIED.,.F.,.F.,(4,2,2,4),(-0.00698848173989863,
-0.00380836019302225,-5.82110553478941E-5,0.),.UNSPECIFIED.);
#24554=B_SPLINE_CURVE_WITH_KNOTS('',3,(#329851,#329852,#329853,#329854,
#329855,#329856,#329857,#329858,#329859,#329860,#329861,#329862,#329863,
#329864,#329865,#329866),.UNSPECIFIED.,.F.,.F.,(4,2,2,2,2,2,2,4),(-0.135883900824496,
-0.13573820087219,-0.135435129549483,-0.134354905429447,-0.130469586234427,
-0.116508674488936,-0.077137265891236,0.),.UNSPECIFIED.);
#24555=B_SPLINE_CURVE_WITH_KNOTS('',3,(#329870,#329871,#329872,#329873,
#329874,#329875,#329876,#329877),.UNSPECIFIED.,.F.,.F.,(4,2,2,4),(-0.00128524516781947,
-0.000715215174727928,-4.8121161636398E-5,0.),.UNSPECIFIED.);
#24556=B_SPLINE_CURVE_WITH_KNOTS('',3,(#329885,#329886,#329887,#329888,
#329889,#329890,#329891,#329892,#329893,#329894,#329895,#329896,#329897,
#329898,#329899,#329900),.UNSPECIFIED.,.F.,.F.,(4,2,2,2,2,2,2,4),(-0.120303146869983,
-0.120182939666542,-0.119932412090095,-0.119036963258739,-0.115814297142423,
-0.104228098096731,-0.0716487624400435,0.),.UNSPECIFIED.);
#24557=B_SPLINE_CURVE_WITH_KNOTS('',3,(#329904,#329905,#329906,#329907,
#329908,#329909,#329910,#329911),.UNSPECIFIED.,.F.,.F.,(4,2,2,4),(-0.009308619177808,
-0.00476368906676523,-9.53428458459868E-5,0.),.UNSPECIFIED.);
#24558=B_SPLINE_CURVE_WITH_KNOTS('',3,(#329919,#329920,#329921,#329922,
#329923,#329924,#329925,#329926,#329927,#329928,#329929,#329930,#329931,
#329932,#329933,#329934),.UNSPECIFIED.,.F.,.F.,(4,2,2,2,2,2,2,4),(-0.143067411193629,
-0.143035855582011,-0.142707176832962,-0.141532914776148,-0.13731284965564,
-0.122133314646075,-0.0793821783049702,0.),.UNSPECIFIED.);
#24559=B_SPLINE_CURVE_WITH_KNOTS('',3,(#329938,#329939,#329940,#329941,
#329942,#329943,#329944,#329945),.UNSPECIFIED.,.F.,.F.,(4,2,2,4),(-0.00671278728818733,
-0.00366284788260162,-4.11768380858013E-5,0.),.UNSPECIFIED.);
#24560=B_SPLINE_CURVE_WITH_KNOTS('',3,(#329953,#329954,#329955,#329956,
#329957,#329958,#329959,#329960,#329961,#329962,#329963,#329964,#329965,
#329966),.UNSPECIFIED.,.F.,.F.,(4,2,2,2,2,2,4),(-0.127252636197906,-0.126633344669922,
-0.125660614619547,-0.122153555706485,-0.109544864528012,-0.0740863921140504,
0.),.UNSPECIFIED.);
#24561=B_SPLINE_CURVE_WITH_KNOTS('',3,(#329970,#329971,#329972,#329973,
#329974,#329975,#329976,#329977),.UNSPECIFIED.,.F.,.F.,(4,2,2,4),(-0.00702763263084672,
-0.00369143312405739,-5.07019646426106E-5,0.),.UNSPECIFIED.);
#24562=B_SPLINE_CURVE_WITH_KNOTS('',3,(#329984,#329985,#329986,#329987,
#329988,#329989,#329990,#329991,#329992,#329993),.UNSPECIFIED.,.F.,.F.,
(4,2,2,2,4),(-0.183717286685379,-0.168622483379294,-0.147423609245421,-0.0876957493345989,
0.),.UNSPECIFIED.);
#24563=B_SPLINE_CURVE_WITH_KNOTS('',3,(#359506,#359507,#359508,#359509,
#359510,#359511,#359512,#359513,#359514,#359515,#359516,#359517,#359518,
#359519,#359520,#359521),.UNSPECIFIED.,.F.,.F.,(4,2,2,2,2,2,2,4),(-29.2770358934888,
-29.2362857521938,-29.1955119506722,-29.1366692553965,-29.0768920699773,
-29.0195042768758,-28.9598835040274,-28.9203929548343),.UNSPECIFIED.);
#24564=B_SPLINE_CURVE_WITH_KNOTS('',3,(#359526,#359527,#359528,#359529,
#359530,#359531,#359532,#359533,#359534,#359535,#359536,#359537,#359538,
#359539,#359540,#359541,#359542,#359543,#359544,#359545,#359546,#359547,
#359548,#359549,#359550,#359551,#359552,#359553,#359554,#359555,#359556,
#359557,#359558,#359559,#359560,#359561),.UNSPECIFIED.,.F.,.F.,(4,2,2,2,
2,2,2,2,2,2,2,2,2,2,2,2,2,4),(-0.94601066902327,-0.905572650935517,-0.846069453129944,
-0.78879284938284,-0.729101573772443,-0.670375555962728,-0.613287938392507,
-0.553575227518369,-0.495501327642977,-0.437451545284286,-0.377809327518591,
-0.320409512233013,-0.260253652075058,-0.201407883721806,-0.144421016431325,
-0.0847464676700296,-0.0416443989073922,-1.00000010494483E-6),
 .UNSPECIFIED.);
#24565=B_SPLINE_CURVE_WITH_KNOTS('',3,(#359562,#359563,#359564,#359565,
#359566,#359567,#359568,#359569,#359570,#359571,#359572,#359573,#359574,
#359575,#359576,#359577,#359578,#359579,#359580,#359581,#359582,#359583,
#359584,#359585,#359586,#359587,#359588,#359589,#359590,#359591,#359592,
#359593,#359594,#359595,#359596,#359597),.UNSPECIFIED.,.F.,.F.,(4,2,2,2,
2,2,2,2,2,2,2,2,2,2,2,2,2,4),(-28.9203929548343,-28.9013438219494,-28.8432744956346,
-28.7828952739219,-28.7255724465968,-28.6668280638283,-28.6070165834198,
-28.5498007229944,-28.4904108948662,-28.4314603756214,-28.3735947373694,
-28.3134411876362,-28.2559721336729,-28.1974344995555,-28.137651101191,
-28.080550994228,-28.0213654657236,-27.9725898263478),.UNSPECIFIED.);
#24566=B_SPLINE_CURVE_WITH_KNOTS('',3,(#359602,#359603,#359604,#359605,
#359606,#359607,#359608,#359609,#359610,#359611,#359612,#359613,#359614,
#359615,#359616,#359617,#359618,#359619,#359620,#359621,#359622,#359623,
#359624,#359625,#359626,#359627,#359628,#359629,#359630,#359631,#359632,
#359633,#359634,#359635,#359636,#359637),.UNSPECIFIED.,.F.,.F.,(4,2,2,2,
2,2,2,2,2,2,2,2,2,2,2,2,2,4),(-1.8926695413163,-1.84291005897148,-1.78382950075986,
-1.72680324523774,-1.66708657324484,-1.60865369543663,-1.55120091496044,
-1.49115806194456,-1.43339609076476,-1.37440371886069,-1.31512569084528,
-1.25800575207285,-1.19826779235354,-1.13963510223288,-1.08235073620415,
-1.02208914923483,-0.964129934552806,-0.94601066902327),.UNSPECIFIED.);
#24567=B_SPLINE_CURVE_WITH_KNOTS('',3,(#359638,#359639,#359640,#359641,
#359642,#359643,#359644,#359645,#359646,#359647,#359648,#359649,#359650,
#359651,#359652,#359653,#359654,#359655,#359656,#359657,#359658,#359659,
#359660,#359661,#359662,#359663,#359664,#359665,#359666,#359667,#359668,
#359669,#359670,#359671,#359672,#359673),.UNSPECIFIED.,.F.,.F.,(4,2,2,2,
2,2,2,2,2,2,2,2,2,2,2,2,2,4),(-27.9725898263478,-27.9619006210563,-27.9042087329266,
-27.8442484956794,-27.7865362065019,-27.7281728793652,-27.6683879590505,
-27.6113049906475,-27.552291595915,-27.4922363274911,-27.4346836129977,
-27.3748790713291,-27.3168429779888,-27.2586164050606,-27.1988025070983,
-27.1416465003213,-27.0827674848282,-27.0250189260883),.UNSPECIFIED.);
#24568=B_SPLINE_CURVE_WITH_KNOTS('',3,(#359678,#359679,#359680,#359681,
#359682,#359683,#359684,#359685,#359686,#359687,#359688,#359689,#359690,
#359691,#359692,#359693,#359694,#359695,#359696,#359697,#359698,#359699,
#359700,#359701,#359702,#359703,#359704,#359705,#359706,#359707,#359708,
#359709,#359710,#359711,#359712,#359713),.UNSPECIFIED.,.F.,.F.,(4,2,2,2,
2,2,2,2,2,2,2,2,2,2,2,2,2,4),(-2.83930461628737,-2.78070942430762,-2.72191816145488,
-2.6647972069617,-2.60503799392433,-2.54689906316616,-2.48884583546765,
-2.42913478010044,-2.37166991679545,-2.3115421817861,-2.25262568519442,
-2.19559552368152,-2.13587110462393,-2.07760446420945,-2.0198890025174,
-1.96003137986963,-1.9024357257172,-1.8926695413163),.UNSPECIFIED.);
#24569=B_SPLINE_CURVE_WITH_KNOTS('',3,(#359714,#359715,#359716,#359717,
#359718,#359719,#359720,#359721,#359722,#359723,#359724,#359725,#359726,
#359727,#359728,#359729,#359730,#359731,#359732,#359733,#359734,#359735,
#359736,#359737,#359738,#359739,#359740,#359741,#359742,#359743,#359744,
#359745,#359746,#359747,#359748,#359749,#359750,#359751),.UNSPECIFIED.,
 .F.,.F.,(4,2,2,2,2,2,2,2,2,2,2,2,2,2,2,2,2,2,4),(-27.0250189260883,-27.0229709630833,
-26.9655490869138,-26.9058917673861,-26.8473869725484,-26.789284343176,
-26.7288687611185,-26.6715498658954,-26.6127715994654,-26.5529475275648,
-26.495704256368,-26.4362808054032,-26.3773789390475,-26.3194833378924,
-26.2592970104669,-26.2018442363091,-26.1432763083209,-26.0834840806869,
-26.0768560357195),.UNSPECIFIED.);
#24570=B_SPLINE_CURVE_WITH_KNOTS('',3,(#359756,#359757,#359758,#359759,
#359760,#359761,#359762,#359763,#359764,#359765,#359766,#359767,#359768,
#359769,#359770,#359771,#359772,#359773,#359774,#359775,#359776,#359777,
#359778,#359779,#359780,#359781,#359782,#359783,#359784,#359785,#359786,
#359787,#359788,#359789,#359790,#359791,#359792,#359793),.UNSPECIFIED.,
 .F.,.F.,(4,2,2,2,2,2,2,2,2,2,2,2,2,2,2,2,2,2,4),(-3.78674073016776,-3.77914273671298,
-3.71938890886991,-3.66089758697167,-3.6034363230487,-3.54333169828402,
-3.48551187697086,-3.42654362802735,-3.36720317419242,-3.31003012797249,
-3.25025122193717,-3.19155616962155,-3.13425093289176,-3.07392365536491,
-3.01590295314771,-2.95735628517826,-2.89778737068896,-2.84044861901574,
-2.83930461628737),.UNSPECIFIED.);
#24571=B_SPLINE_CURVE_WITH_KNOTS('',3,(#359794,#359795,#359796,#359797,
#359798,#359799,#359800,#359801,#359802,#359803,#359804,#359805,#359806,
#359807,#359808,#359809,#359810,#359811,#359812,#359813,#359814,#359815,
#359816,#359817,#359818,#359819,#359820,#359821,#359822,#359823,#359824,
#359825,#359826,#359827,#359828,#359829),.UNSPECIFIED.,.F.,.F.,(4,2,2,2,
2,2,2,2,2,2,2,2,2,2,2,2,2,4),(-26.0768560357195,-26.0263685270805,-25.9671528988416,
-25.9077479135651,-25.8500299500852,-25.7900411558174,-25.7323562797147,
-25.6739668845061,-25.6141765859204,-25.5570898656,-25.4980505900865,-25.4380625593129,
-25.3804882052171,-25.320659935685,-25.2626595733453,-25.2044117340995,
-25.1445956843974,-25.1292817558394),.UNSPECIFIED.);
#24572=B_SPLINE_CURVE_WITH_KNOTS('',3,(#359834,#359835,#359836,#359837,
#359838,#359839,#359840,#359841,#359842,#359843,#359844,#359845,#359846,
#359847,#359848,#359849,#359850,#359851,#359852,#359853,#359854,#359855,
#359856,#359857,#359858,#359859,#359860,#359861,#359862,#359863,#359864,
#359865,#359866,#359867,#359868,#359869),.UNSPECIFIED.,.F.,.F.,(4,2,2,2,
2,2,2,2,2,2,2,2,2,2,2,2,2,4),(-4.73379937711506,-4.71760993607862,-4.65782029343659,
-4.59963256224015,-4.54158930230178,-4.48182617663283,-4.42431237784908,
-4.36422553346581,-4.30525502901722,-4.24819587084784,-4.18843777163506,
-4.13011723963591,-4.07240407682471,-4.01248924293099,-3.95483993189503,
-3.89534884352174,-3.8362097215891,-3.78674073016776),.UNSPECIFIED.);
#24573=B_SPLINE_CURVE_WITH_KNOTS('',3,(#359870,#359871,#359872,#359873,
#359874,#359875,#359876,#359877,#359878,#359879,#359880,#359881,#359882,
#359883,#359884,#359885,#359886,#359887,#359888,#359889,#359890,#359891,
#359892,#359893,#359894,#359895,#359896,#359897,#359898,#359899,#359900,
#359901,#359902,#359903,#359904,#359905),.UNSPECIFIED.,.F.,.F.,(4,2,2,2,
2,2,2,2,2,2,2,2,2,2,2,2,2,4),(-25.1292817558394,-25.0874460424636,-25.0285459963092,
-24.9687457625083,-24.9113046781623,-24.851626239461,-24.7931712161292,
-24.7350502895988,-24.6746139124586,-24.6173132140707,-24.5585162222061,
-24.4986952887874,-24.4414384282637,-24.3819967053851,-24.3231589306908,
-24.2652483109868,-24.205044695016,-24.181124288547),.UNSPECIFIED.);
#24574=B_SPLINE_CURVE_WITH_KNOTS('',3,(#359910,#359911,#359912,#359913,
#359914,#359915,#359916,#359917,#359918,#359919,#359920,#359921,#359922,
#359923,#359924,#359925,#359926,#359927,#359928,#359929,#359930,#359931,
#359932,#359933,#359934,#359935,#359936,#359937,#359938,#359939,#359940,
#359941,#359942,#359943,#359944,#359945),.UNSPECIFIED.,.F.,.F.,(4,2,2,2,
2,2,2,2,2,2,2,2,2,2,2,2,2,4),(-5.68164266866445,-5.65672900808728,-5.59657896987309,
-5.53871701905266,-5.47978603931155,-5.42039942184852,-5.36318772406343,
-5.30338370045807,-5.24464237047255,-5.18732994589727,-5.1269535569688,
-5.06888728475205,-5.01036436220717,-4.95074625365402,-4.89336124156495,
-4.83359016895416,-4.77475004818097,-4.73379937711506),.UNSPECIFIED.);
#24575=B_SPLINE_CURVE_WITH_KNOTS('',3,(#359946,#359947,#359948,#359949,
#359950,#359951,#359952,#359953,#359954,#359955,#359956,#359957,#359958,
#359959,#359960,#359961,#359962,#359963,#359964,#359965,#359966,#359967,
#359968,#359969,#359970,#359971,#359972,#359973,#359974,#359975,#359976,
#359977,#359978,#359979,#359980,#359981),.UNSPECIFIED.,.F.,.F.,(4,2,2,2,
2,2,2,2,2,2,2,2,2,2,2,2,2,4),(-24.181124288547,-24.1476227904716,-24.089039655252,
-24.0292544286749,-23.9721373554774,-23.9129069011809,-23.8535779480638,
-23.7958488025427,-23.7358468798957,-23.6782043827208,-23.6198039524279,
-23.5600241998517,-23.5029479631018,-23.4438980195044,-23.3839942080211,
-23.3264130818869,-23.2665764840907,-23.2336871318211),.UNSPECIFIED.);
#24576=B_SPLINE_CURVE_WITH_KNOTS('',3,(#359986,#359987,#359988,#359989,
#359990,#359991,#359992,#359993,#359994,#359995,#359996,#359997,#359998,
#359999,#360000,#360001,#360002,#360003,#360004,#360005,#360006,#360007,
#360008,#360009,#360010,#360011,#360012,#360013,#360014,#360015,#360016,
#360017,#360018,#360019,#360020,#360021),.UNSPECIFIED.,.F.,.F.,(4,2,2,2,
2,2,2,2,2,2,2,2,2,2,2,2,2,4),(-6.6289785836689,-6.59514941924382,-6.53535013671941,
-6.47780271809717,-6.4177707840938,-6.35876208546021,-6.30168794247145,
-6.24191189860981,-6.18355312246758,-6.12585592843799,-6.06590001355162,
-6.00821256016226,-5.94876952995814,-5.88958788307532,-5.83249429561485,
-5.7727190919009,-5.71418519391065,-5.68164266866445),.UNSPECIFIED.);
#24577=B_SPLINE_CURVE_WITH_KNOTS('',3,(#360022,#360023,#360024,#360025,
#360026,#360027,#360028,#360029,#360030,#360031,#360032,#360033,#360034,
#360035,#360036,#360037,#360038,#360039,#360040,#360041,#360042,#360043,
#360044,#360045,#360046,#360047,#360048,#360049,#360050,#360051,#360052,
#360053,#360054,#360055,#360056,#360057),.UNSPECIFIED.,.F.,.F.,(4,2,2,2,
2,2,2,2,2,2,2,2,2,2,2,2,2,4),(-23.2336871318211,-23.2086275557579,-23.1503734650017,
-23.0905712748626,-23.033442679821,-22.9745367926783,-22.9147487560726,
-22.8573032676543,-22.797619037379,-22.7392300501316,-22.6811057829897,
-22.6206640846457,-22.5633965282484,-22.5045959144076,-22.4447942837391,
-22.3875376301589,-22.3280929476983,-22.2857741951284),.UNSPECIFIED.);
#24578=B_SPLINE_CURVE_WITH_KNOTS('',3,(#360062,#360063,#360064,#360065,
#360066,#360067,#360068,#360069,#360070,#360071,#360072,#360073,#360074,
#360075,#360076,#360077,#360078,#360079,#360080,#360081,#360082,#360083,
#360084,#360085,#360086,#360087,#360088,#360089,#360090,#360091,#360092,
#360093,#360094,#360095,#360096,#360097),.UNSPECIFIED.,.F.,.F.,(4,2,2,2,
2,2,2,2,2,2,2,2,2,2,2,2,2,4),(-7.57699195719593,-7.5336040360614,-7.47418686850509,
-7.41695052210019,-7.35713701526706,-7.29836483713746,-7.24105913548731,
-7.18064950623535,-7.1225529356128,-7.06406775513403,-7.00441619331711,
-6.94700007863283,-6.88721276951991,-6.8283393945683,-6.77119421074264,
-6.71138983189206,-6.65316874394789,-6.6289785836689),.UNSPECIFIED.);
#24579=B_SPLINE_CURVE_WITH_KNOTS('',3,(#360098,#360099,#360100,#360101,
#360102,#360103,#360104,#360105,#360106,#360107,#360108,#360109,#360110,
#360111,#360112,#360113,#360114,#360115,#360116,#360117,#360118,#360119,
#360120,#360121,#360122,#360123,#360124,#360125,#360126,#360127,#360128,
#360129,#360130,#360131,#360132,#360133),.UNSPECIFIED.,.F.,.F.,(4,2,2,2,
2,2,2,2,2,2,2,2,2,2,2,2,2,4),(-22.2857741951284,-22.2693364072178,-22.2114257342202,
-22.1512203014804,-22.0938448119875,-22.0352615756877,-21.9754997082272,
-21.9183952653275,-21.859165292854,-21.7999305404075,-21.7422052085182,
-21.6822056562023,-21.6246217930565,-21.5662254676702,-21.5064727995311,
-21.449421768801,-21.3903764906121,-21.3386984476615),.UNSPECIFIED.);
#24580=B_SPLINE_CURVE_WITH_KNOTS('',3,(#360138,#360139,#360140,#360141,
#360142,#360143,#360144,#360145,#360146,#360147,#360148,#360149,#360150,
#360151,#360152,#360153,#360154,#360155,#360156,#360157,#360158,#360159,
#360160,#360161,#360162,#360163,#360164,#360165,#360166,#360167,#360168,
#360169,#360170,#360171,#360172,#360173),.UNSPECIFIED.,.F.,.F.,(4,2,2,2,
2,2,2,2,2,2,2,2,2,2,2,2,2,4),(-8.52439085180131,-8.47165190932738,-8.41262036103156,
-8.3555452676041,-8.29576697778077,-8.23738512988965,-8.17971826146527,
-8.11973686813537,-8.06202630831729,-8.00264619984432,-7.94343750413151,
-7.88633123192098,-7.82655031957626,-7.76798914240985,-7.71055206906101,
-7.65037235147109,-7.59248342397278,-7.57699195719593),.UNSPECIFIED.);
#24581=B_SPLINE_CURVE_WITH_KNOTS('',3,(#360174,#360175,#360176,#360177,
#360178,#360179,#360180,#360181,#360182,#360183,#360184,#360185,#360186,
#360187,#360188,#360189,#360190,#360191,#360192,#360193,#360194,#360195,
#360196,#360197,#360198,#360199,#360200,#360201,#360202,#360203,#360204,
#360205,#360206,#360207,#360208,#360209,#360210,#360211),.UNSPECIFIED.,
 .F.,.F.,(4,2,2,2,2,2,2,2,2,2,2,2,2,2,2,2,2,2,4),(-21.3386984476615,-21.3305761052758,
-21.273003270418,-21.213173915207,-21.1552935809097,-21.0970484612882,-21.0372768361306,
-20.9801847091942,-20.9212883924184,-20.8615291182862,-20.8040942717974,
-20.7444197976042,-20.6861149111606,-20.6280025247625,-20.5675712071319,
-20.5103527388457,-20.4515638671961,-20.3917985314428,-20.3912808464162),
 .UNSPECIFIED.);
#24582=B_SPLINE_CURVE_WITH_KNOTS('',3,(#360216,#360217,#360218,#360219,
#360220,#360221,#360222,#360223,#360224,#360225,#360226,#360227,#360228,
#360229,#360230,#360231,#360232,#360233,#360234,#360235,#360236,#360237,
#360238,#360239,#360240,#360241,#360242,#360243,#360244,#360245,#360246,
#360247,#360248,#360249,#360250,#360251,#360252,#360253),.UNSPECIFIED.,
 .F.,.F.,(4,2,2,2,2,2,2,2,2,2,2,2,2,2,2,2,2,2,4),(-9.47234169396005,-9.47079131440874,
-9.41098410876783,-9.35219620204647,-9.2949115979019,-9.23448424708455,
-9.1763723465148,-9.11794003645549,-9.0582704006571,-9.00083801663931,-8.94105012120809,
-8.88215873334131,-8.82502278464254,-8.76521939714966,-8.70698002683787,
-8.64899944808623,-8.58917950168627,-8.53161339913665,-8.52439085180131),
 .UNSPECIFIED.);
#24583=B_SPLINE_CURVE_WITH_KNOTS('',3,(#360254,#360255,#360256,#360257,
#360258,#360259,#360260,#360261,#360262,#360263,#360264,#360265,#360266,
#360267,#360268,#360269,#360270,#360271,#360272,#360273,#360274,#360275,
#360276,#360277,#360278,#360279,#360280,#360281,#360282,#360283,#360284,
#360285,#360286,#360287,#360288,#360289),.UNSPECIFIED.,.F.,.F.,(4,2,2,2,
2,2,2,2,2,2,2,2,2,2,2,2,2,4),(-20.3912808464162,-20.334556071801,-20.2751240267045,
-20.2164680585815,-20.1585726374241,-20.0983811658138,-20.041068963067,
-19.9825010710361,-19.9227798618537,-19.8657026684406,-19.8064888467141,
-19.7473690371157,-19.6896629420058,-19.6296816582903,-19.5721744062189,
-19.5137977586576,-19.4540897591255,-19.4447457737501),.UNSPECIFIED.);
#24584=B_SPLINE_CURVE_WITH_KNOTS('',3,(#360294,#360295,#360296,#360297,
#360298,#360299,#360300,#360301,#360302,#360303,#360304,#360305,#360306,
#360307,#360308,#360309,#360310,#360311,#360312,#360313,#360314,#360315,
#360316,#360317,#360318,#360319,#360320,#360321,#360322,#360323,#360324,
#360325,#360326,#360327,#360328,#360329),.UNSPECIFIED.,.F.,.F.,(4,2,2,2,
2,2,2,2,2,2,2,2,2,2,2,2,2,4),(-10.4196492469242,-10.4092374309108,-10.3494729075107,
-10.2910830142037,-10.233461608822,-10.1734701511741,-10.1157513707506,
-10.0564507135166,-9.99723022113808,-9.9401252138231,-9.88035449510157,
-9.82178110147787,-9.76437789214267,-9.70418395253122,-9.64628296916424,
-9.58747091595993,-9.52803851322082,-9.47234169396005),.UNSPECIFIED.);
#24585=B_SPLINE_CURVE_WITH_KNOTS('',3,(#360330,#360331,#360332,#360333,
#360334,#360335,#360336,#360337,#360338,#360339,#360340,#360341,#360342,
#360343,#360344,#360345,#360346,#360347,#360348,#360349,#360350,#360351,
#360352,#360353,#360354,#360355,#360356,#360357,#360358,#360359,#360360,
#360361,#360362,#360363,#360364,#360365),.UNSPECIFIED.,.F.,.F.,(4,2,2,2,
2,2,2,2,2,2,2,2,2,2,2,2,2,4),(-19.4447457737501,-19.3970794408228,-19.3380546146096,
-19.2783797548411,-19.2208308040997,-19.161024772293,-19.1032321601674,
-19.0450117778471,-18.9852885651626,-18.9282494273001,-18.869378655352,
-18.8090891815156,-18.7516607032691,-18.6919900130941,-18.6338439477108,
-18.5757401634432,-18.5159751173138,-18.4982475217245),.UNSPECIFIED.);
#24586=B_SPLINE_CURVE_WITH_KNOTS('',3,(#360370,#360371,#360372,#360373,
#360374,#360375,#360376,#360377,#360378,#360379,#360380,#360381,#360382,
#360383,#360384,#360385,#360386,#360387,#360388,#360389,#360390,#360391,
#360392,#360393,#360394,#360395,#360396,#360397,#360398,#360399,#360400,
#360401,#360402,#360403,#360404,#360405),.UNSPECIFIED.,.F.,.F.,(4,2,2,2,
2,2,2,2,2,2,2,2,2,2,2,2,2,4),(-11.3671613030629,-11.3483513921095,-11.2879218103826,
-11.2298095608741,-11.171446702329,-11.1117743353272,-11.0543405061875,
-10.9945680299796,-10.9356738342456,-10.8785619212499,-10.8187756395274,
-10.7605330146923,-10.7026071376232,-10.6427819322376,-10.5852120241117,
-10.5253383567006,-10.4662991670699,-10.4196492469242),.UNSPECIFIED.);
#24587=B_SPLINE_CURVE_WITH_KNOTS('',3,(#360406,#360407,#360408,#360409,
#360410,#360411,#360412,#360413,#360414,#360415,#360416,#360417,#360418,
#360419,#360420,#360421,#360422,#360423,#360424,#360425,#360426,#360427,
#360428,#360429,#360430,#360431,#360432,#360433,#360434,#360435,#360436,
#360437,#360438,#360439,#360440,#360441),.UNSPECIFIED.,.F.,.F.,(4,2,2,2,
2,2,2,2,2,2,2,2,2,2,2,2,2,4),(-18.4982475217245,-18.4588246892297,-18.4000678912934,
-18.3403257329831,-18.2830174724236,-18.223482590589,-18.1648133289671,
-18.1068206532574,-18.0465261169426,-17.9891653866314,-17.9304989893709,
-17.8707028571648,-17.8135408598337,-17.7542281137836,-17.6951092021336,
-17.6373101990686,-17.5772305525968,-17.5506080199207),.UNSPECIFIED.);
#24588=B_SPLINE_CURVE_WITH_KNOTS('',3,(#360446,#360447,#360448,#360449,
#360450,#360451,#360452,#360453,#360454,#360455,#360456,#360457,#360458,
#360459,#360460,#360461,#360462,#360463,#360464,#360465,#360466,#360467,
#360468,#360469,#360470,#360471,#360472,#360473,#360474,#360475,#360476,
#360477,#360478,#360479,#360480,#360481),.UNSPECIFIED.,.F.,.F.,(4,2,2,2,
2,2,2,2,2,2,2,2,2,2,2,2,2,4),(-12.314277429601,-12.2865423449001,-12.2265563711873,
-12.1688444212435,-12.1096418385269,-12.0504248995809,-11.9933353775088,
-11.9335913590392,-11.8750208936681,-11.817667321657,-11.7574746635353,
-11.6995766283184,-11.6408494403391,-11.5814171422987,-11.5241729057154,
-11.4643882936125,-11.4055997852911,-11.3671613030629),.UNSPECIFIED.);
#24589=B_SPLINE_CURVE_WITH_KNOTS('',3,(#360482,#360483,#360484,#360485,
#360486,#360487,#360488,#360489,#360490,#360491,#360492,#360493,#360494,
#360495,#360496,#360497,#360498,#360499,#360500,#360501,#360502,#360503,
#360504,#360505,#360506,#360507,#360508,#360509,#360510,#360511,#360512,
#360513,#360514,#360515,#360516,#360517),.UNSPECIFIED.,.F.,.F.,(4,2,2,2,
2,2,2,2,2,2,2,2,2,2,2,2,2,4),(-17.5506080199207,-17.5196882325723,-17.4612177719407,
-17.401439017662,-17.3443578226861,-17.285238717623,-17.2255751036821,-17.1679382057827,
-17.1080392136975,-17.0502227508961,-16.99191393138,-16.9321237907676,-16.8750265151245,
-16.8160668605451,-16.7557941095397,-16.698283187946,-16.638525529114,-16.6031179891744),
 .UNSPECIFIED.);
#24590=B_SPLINE_CURVE_WITH_KNOTS('',3,(#360522,#360523,#360524,#360525,
#360526,#360527,#360528,#360529,#360530,#360531,#360532,#360533,#360534,
#360535,#360536,#360537,#360538,#360539,#360540,#360541,#360542,#360543,
#360544,#360545,#360546,#360547,#360548,#360549,#360550,#360551,#360552,
#360553,#360554,#360555,#360556,#360557),.UNSPECIFIED.,.F.,.F.,(4,2,2,2,
2,2,2,2,2,2,2,2,2,2,2,2,2,4),(-13.2611275241497,-13.2240332453506,-13.1643737747774,
-13.1069536302929,-13.0472133148037,-12.9883318031598,-12.9312595314886,
-12.8715072459355,-12.8132766664862,-12.7554229928843,-12.6956081697718,
-12.6380495940693,-12.5782834655373,-12.519252027863,-12.4622184993239,
-12.4024844482838,-12.3441017059567,-12.314277429601),.UNSPECIFIED.);
#24591=B_SPLINE_CURVE_WITH_KNOTS('',3,(#360558,#360559,#360560,#360561,
#360562,#360563,#360564,#360565,#360566,#360567,#360568,#360569,#360570,
#360571,#360572,#360573,#360574,#360575,#360576,#360577,#360578,#360579,
#360580,#360581,#360582,#360583,#360584,#360585,#360586,#360587,#360588,
#360589,#360590,#360591,#360592,#360593),.UNSPECIFIED.,.F.,.F.,(4,2,2,2,
2,2,2,2,2,2,2,2,2,2,2,2,2,4),(-16.6031179891744,-16.5803630906363,-16.5221767759143,
-16.462348383425,-16.4051501161605,-16.3463104187655,-16.2865035095385,
-16.2291160249035,-16.1694976410878,-16.1108266704695,-16.0527553084712,
-15.9923771273555,-15.9349817326151,-15.876235592733,-15.8163819401178,
-15.7591514407899,-15.6997587114897,-15.654611343672),.UNSPECIFIED.);
#24592=B_SPLINE_CURVE_WITH_KNOTS('',3,(#360598,#360599,#360600,#360601,
#360602,#360603,#360604,#360605,#360606,#360607,#360608,#360609,#360610,
#360611,#360612,#360613,#360614,#360615,#360616,#360617,#360618,#360619,
#360620,#360621,#360622,#360623,#360624,#360625,#360626,#360627,#360628,
#360629,#360630,#360631,#360632,#360633),.UNSPECIFIED.,.F.,.F.,(4,2,2,2,
2,2,2,2,2,2,2,2,2,2,2,2,2,4),(-14.2078226042407,-14.1616527561318,-14.102455149493,
-14.0453958531341,-13.9856960744249,-13.9271440872338,-13.8698573378326,
-13.8096818371734,-13.7518021599383,-13.6931796831918,-13.6337631805218,
-13.5765359534962,-13.5167911415227,-13.4580174836316,-13.4008214879835,
-13.340405458723,-13.2823081702298,-13.2611275241497),.UNSPECIFIED.);
#24593=B_SPLINE_CURVE_WITH_KNOTS('',3,(#360634,#360635,#360636,#360637,
#360638,#360639,#360640,#360641,#360642,#360643,#360644,#360645,#360646,
#360647,#360648,#360649,#360650,#360651,#360652,#360653,#360654,#360655,
#360656,#360657,#360658,#360659,#360660,#360661,#360662,#360663,#360664,
#360665,#360666,#360667,#360668,#360669),.UNSPECIFIED.,.F.,.F.,(4,2,2,2,
2,2,2,2,2,2,2,2,2,2,2,2,2,4),(-15.654611343672,-15.6406517898237,-15.5827780369757,
-15.5226189958196,-15.4650548029905,-15.4065088447247,-15.3466765037092,
-15.2895398121176,-15.2303449176205,-15.170703619353,-15.1129964866102,
-15.0530230138708,-14.99519558114,-14.9368161615171,-14.8769760423813,-14.8177008154817,
-14.7583766231312,-14.7063679063436),.UNSPECIFIED.);
#24594=B_SPLINE_CURVE_WITH_KNOTS('',3,(#360674,#360675,#360676,#360677,
#360678,#360679,#360680,#360681,#360682,#360683,#360684,#360685,#360686,
#360687,#360688,#360689,#360690,#360691,#360692,#360693,#360694,#360695,
#360696,#360697,#360698,#360699,#360700,#360701,#360702,#360703,#360704,
#360705,#360706,#360707,#360708,#360709),.UNSPECIFIED.,.F.,.F.,(4,2,2,2,
2,2,2,2,2,2,2,2,2,2,2,2,2,4),(-15.1537653436456,-15.1002345835303,-15.0409821852976,
-14.9820358340952,-14.9242995477987,-14.8642830082815,-14.8068674757668,
-14.7470792575717,-14.6895477527618,-14.6299119365804,-14.5709041670138,
-14.5139145448345,-14.4542288146403,-14.3958689208766,-14.3383899716655,
-14.278425498234,-14.2207359254435,-14.2078226042407),.UNSPECIFIED.);
#24595=B_SPLINE_CURVE_WITH_KNOTS('',3,(#360710,#360711,#360712,#360713,
#360714,#360715,#360716,#360717,#360718,#360719,#360720,#360721,#360722,
#360723,#360724,#360725,#360726,#360727,#360728,#360729,#360730,#360731,
#360732,#360733,#360734,#360735,#360736,#360737,#360738,#360739,#360740,
#360741,#360742,#360743,#360744,#360745,#360746,#360747),.UNSPECIFIED.,
 .F.,.F.,(4,2,2,2,2,2,2,2,2,2,2,2,2,2,2,2,2,2,4),(-14.7063679063436,-14.7011878444491,
-14.6413441342094,-14.5826673668123,-14.5252266321471,-14.4649240950712,
-14.4069210059505,-14.3481170771853,-14.2885758826815,-14.2312275238881,
-14.1713416201138,-14.1124451307885,-14.0551048133669,-13.9945636453226,
-13.9363447517743,-13.8779000977309,-13.8181173661783,-13.76057775001,-13.7572072092418),
 .UNSPECIFIED.);
#24596=B_SPLINE_CURVE_WITH_KNOTS('',3,(#360752,#360753,#360754,#360755,
#360756,#360757,#360758,#360759,#360760,#360761,#360762,#360763,#360764,
#360765,#360766,#360767,#360768,#360769,#360770,#360771,#360772,#360773,
#360774,#360775,#360776,#360777,#360778,#360779,#360780,#360781,#360782,
#360783,#360784,#360785,#360786,#360787,#360788,#360789),.UNSPECIFIED.,
 .F.,.F.,(4,2,2,2,2,2,2,2,2,2,2,2,2,2,2,2,2,2,4),(-16.0998751798599,-16.0944661699573,
-16.0370900178806,-15.9774720925845,-15.9194611350742,-15.8614113663036,
-15.8017283017216,-15.7446717478584,-15.6859702556362,-15.6263082822782,
-15.5690559565789,-15.5095777085928,-15.4510629443817,-15.3931286818612,
-15.3328926225813,-15.2756424697563,-15.2170349859268,-15.1573280589623,
-15.1537653436456),.UNSPECIFIED.);
#24597=B_SPLINE_CURVE_WITH_KNOTS('',3,(#360790,#360791,#360792,#360793,
#360794,#360795,#360796,#360797,#360798,#360799,#360800,#360801,#360802,
#360803,#360804,#360805,#360806,#360807,#360808,#360809,#360810,#360811,
#360812,#360813,#360814,#360815,#360816,#360817,#360818,#360819,#360820,
#360821,#360822,#360823,#360824,#360825),.UNSPECIFIED.,.F.,.F.,(4,2,2,2,
2,2,2,2,2,2,2,2,2,2,2,2,2,4),(-13.7572072092418,-13.7007013703789,-13.6416982254372,
-13.5844902227664,-13.524600640322,-13.4662500986182,-13.4082378308948,
-13.348301084172,-13.2906243016887,-13.2306727337995,-13.1715225948561,
-13.1143609273779,-13.0544919256689,-12.995992124977,-12.93828143513,-12.8781764070513,
-12.8203488950124,-12.8083351637663),.UNSPECIFIED.);
#24598=B_SPLINE_CURVE_WITH_KNOTS('',3,(#360830,#360831,#360832,#360833,
#360834,#360835,#360836,#360837,#360838,#360839,#360840,#360841,#360842,
#360843,#360844,#360845,#360846,#360847,#360848,#360849,#360850,#360851,
#360852,#360853,#360854,#360855,#360856,#360857,#360858,#360859,#360860,
#360861,#360862,#360863,#360864,#360865),.UNSPECIFIED.,.F.,.F.,(4,2,2,2,
2,2,2,2,2,2,2,2,2,2,2,2,2,4),(-17.0450106813388,-17.0315098527715,-16.9738440378701,
-16.9139024253291,-16.8565055613141,-16.7981698690676,-16.7385346215828,
-16.6815895160318,-16.6226068061299,-16.5631048921601,-16.5056018619694,
-16.4458416325847,-16.3881739594714,-16.3300006825261,-16.2703549519301,
-16.2133967316551,-16.1545742555269,-16.0998751798599),.UNSPECIFIED.);
#24599=B_SPLINE_CURVE_WITH_KNOTS('',3,(#360866,#360867,#360868,#360869,
#360870,#360871,#360872,#360873,#360874,#360875,#360876,#360877,#360878,
#360879,#360880,#360881,#360882,#360883,#360884,#360885,#360886,#360887,
#360888,#360889,#360890,#360891,#360892,#360893,#360894,#360895,#360896,
#360897,#360898,#360899,#360900,#360901),.UNSPECIFIED.,.F.,.F.,(4,2,2,2,
2,2,2,2,2,2,2,2,2,2,2,2,2,4),(-12.8083351637663,-12.7609682207284,-12.7016349620055,
-12.6444255352263,-12.5845490220204,-12.5258638923139,-12.4683675412153,
-12.4080581728529,-12.3500467510207,-12.2911510845023,-12.2316043006535,
-12.1742480499109,-12.1143335601395,-12.0554322699415,-11.9980500980351,
-11.9375056408414,-11.8792817438646,-11.8589296630317),.UNSPECIFIED.);
#24600=B_SPLINE_CURVE_WITH_KNOTS('',3,(#360906,#360907,#360908,#360909,
#360910,#360911,#360912,#360913,#360914,#360915,#360916,#360917,#360918,
#360919,#360920,#360921,#360922,#360923,#360924,#360925,#360926,#360927,
#360928,#360929,#360930,#360931,#360932,#360933,#360934,#360935,#360936,
#360937,#360938,#360939,#360940,#360941),.UNSPECIFIED.,.F.,.F.,(4,2,2,2,
2,2,2,2,2,2,2,2,2,2,2,2,2,4),(-17.9903076061228,-17.9680233235286,-17.9100516126546,
-17.8504276638631,-17.7934153544959,-17.7347922515903,-17.6751907972335,
-17.6180133387519,-17.5586140507017,-17.5000981285757,-17.4422381848549,
-17.3820812044448,-17.3248623632732,-17.2663302079828,-17.2066766767308,
-17.1496478221714,-17.0904709505879,-17.0450106813388),.UNSPECIFIED.);
#24601=B_SPLINE_CURVE_WITH_KNOTS('',3,(#360942,#360943,#360944,#360945,
#360946,#360947,#360948,#360949,#360950,#360951,#360952,#360953,#360954,
#360955,#360956,#360957,#360958,#360959,#360960,#360961,#360962,#360963,
#360964,#360965,#360966,#360967,#360968,#360969,#360970,#360971,#360972,
#360973,#360974,#360975,#360976,#360977),.UNSPECIFIED.,.F.,.F.,(4,2,2,2,
2,2,2,2,2,2,2,2,2,2,2,2,2,4),(-11.8589296630317,-11.8207612239523,-11.7609757586343,
-11.7034322981271,-11.6435346624504,-11.584528908831,-11.5272914226937,
-11.4673788469843,-11.4090262099659,-11.3509531564106,-11.2910161981842,
-11.2333379281589,-11.1732917062938,-11.1141438241308,-11.0569636057153,
-10.9970750114197,-10.938577939892,-10.909574098799),.UNSPECIFIED.);
#24602=B_SPLINE_CURVE_WITH_KNOTS('',3,(#360982,#360983,#360984,#360985,
#360986,#360987,#360988,#360989,#360990,#360991,#360992,#360993,#360994,
#360995,#360996,#360997,#360998,#360999,#361000,#361001,#361002,#361003,
#361004,#361005,#361006,#361007,#361008,#361009,#361010,#361011,#361012,
#361013,#361014,#361015,#361016,#361017),.UNSPECIFIED.,.F.,.F.,(4,2,2,2,
2,2,2,2,2,2,2,2,2,2,2,2,2,4),(-18.9344980393133,-18.9041379145137,-18.8458912748405,
-18.7863224126782,-18.7294442575711,-18.670551023092,-18.6110353760674,
-18.553615705937,-18.4939436450504,-18.4362967240132,-18.3782072667762,
-18.3186241661682,-18.2617203663546,-18.2029821150101,-18.1428547423791,
-18.0855565847922,-18.0260209865782,-17.9903076061228),.UNSPECIFIED.);
#24603=B_SPLINE_CURVE_WITH_KNOTS('',3,(#361018,#361019,#361020,#361021,
#361022,#361023,#361024,#361025,#361026,#361027,#361028,#361029,#361030,
#361031,#361032,#361033,#361034,#361035,#361036,#361037,#361038,#361039,
#361040,#361041,#361042,#361043,#361044,#361045,#361046,#361047,#361048,
#361049,#361050,#361051,#361052,#361053),.UNSPECIFIED.,.F.,.F.,(4,2,2,2,
2,2,2,2,2,2,2,2,2,2,2,2,2,4),(-10.909574098799,-10.8808160295316,-10.8207156251837,
-10.7628910685625,-10.7034244813183,-10.6440976476971,-10.5868819744247,
-10.5269895075939,-10.4683112939554,-10.4107755782778,-10.3504750047583,
-10.2924703878915,-10.2335012948907,-10.173964376334,-10.1166141325046,
-10.0566876526939,-9.99779679495118,-9.9601521371041),.UNSPECIFIED.);
#24604=B_SPLINE_CURVE_WITH_KNOTS('',3,(#361058,#361059,#361060,#361061,
#361062,#361063,#361064,#361065,#361066,#361067,#361068,#361069,#361070,
#361071,#361072,#361073,#361074,#361075,#361076,#361077,#361078,#361079,
#361080,#361081,#361082,#361083,#361084,#361085,#361086,#361087,#361088,
#361089,#361090,#361091,#361092,#361093),.UNSPECIFIED.,.F.,.F.,(4,2,2,2,
2,2,2,2,2,2,2,2,2,2,2,2,2,4),(-19.8790955780054,-19.8401576940368,-19.7814977581655,
-19.7218695712742,-19.6647531524489,-19.6054516486236,-19.5469463032725,
-19.4891787722589,-19.4291197855388,-19.3719460257536,-19.3135074828106,
-19.2539244283835,-19.1969761629465,-19.1378932788518,-19.0789287482696,
-19.0213511210655,-18.9615029338211,-18.9344980393133),.UNSPECIFIED.);
#24605=B_SPLINE_CURVE_WITH_KNOTS('',3,(#361094,#361095,#361096,#361097,
#361098,#361099,#361100,#361101,#361102,#361103,#361104,#361105,#361106,
#361107,#361108,#361109,#361110,#361111,#361112,#361113,#361114,#361115,
#361116,#361117,#361118,#361119,#361120,#361121,#361122,#361123,#361124,
#361125,#361126,#361127,#361128,#361129),.UNSPECIFIED.,.F.,.F.,(4,2,2,2,
2,2,2,2,2,2,2,2,2,2,2,2,2,4),(-9.9601521371041,-9.94038824764174,-9.87985608738636,
-9.82164227553691,-9.76306311461492,-9.70329035061682,-9.64575796925551,
-9.58585532697708,-9.52686226224796,-9.46961036732748,-9.40969116987352,
-9.3513515529105,-9.29323419349764,-9.2333125037998,-9.17564770763484,-9.11552500244563,
-9.05639464257743,-9.01053220002199),.UNSPECIFIED.);
#24606=B_SPLINE_CURVE_WITH_KNOTS('',3,(#361134,#361135,#361136,#361137,
#361138,#361139,#361140,#361141,#361142,#361143,#361144,#361145,#361146,
#361147,#361148,#361149,#361150,#361151,#361152,#361153,#361154,#361155,
#361156,#361157,#361158,#361159,#361160,#361161,#361162,#361163,#361164,
#361165,#361166,#361167,#361168,#361169),.UNSPECIFIED.,.F.,.F.,(4,2,2,2,
2,2,2,2,2,2,2,2,2,2,2,2,2,4),(-20.8242710457994,-20.7765261092298,-20.7175778727164,
-20.6580053703026,-20.6005320267931,-20.540804205626,-20.4831026281961,
-20.4249588649431,-20.3653197791477,-20.3083624391667,-20.2495692688034,
-20.1899400450114,-20.1326074527045,-20.0730374502272,-20.0149326855893,
-19.9569251490987,-19.8972414747414,-19.8790955780054),.UNSPECIFIED.);
#24607=B_SPLINE_CURVE_WITH_KNOTS('',3,(#361170,#361171,#361172,#361173,
#361174,#361175,#361176,#361177,#361178,#361179,#361180,#361181,#361182,
#361183,#361184,#361185,#361186,#361187,#361188,#361189,#361190,#361191,
#361192,#361193,#361194,#361195,#361196,#361197,#361198,#361199,#361200,
#361201,#361202,#361203,#361204,#361205),.UNSPECIFIED.,.F.,.F.,(4,2,2,2,
2,2,2,2,2,2,2,2,2,2,2,2,2,4),(-9.01053220002199,-8.99921036745133,-8.9393184222242,
-8.88083915842011,-8.82304162701373,-8.76296130024007,-8.70515463521909,
-8.64561937780934,-8.58631424828878,-8.52910637261322,-8.46921405362235,
-8.41055784034516,-8.35299786190215,-8.29272154966623,-8.2347386804068,
-8.17571251580717,-8.11620077877754,-8.06130686846712),.UNSPECIFIED.);
#24608=B_SPLINE_CURVE_WITH_KNOTS('',3,(#361210,#361211,#361212,#361213,
#361214,#361215,#361216,#361217,#361218,#361219,#361220,#361221,#361222,
#361223,#361224,#361225,#361226,#361227,#361228,#361229,#361230,#361231,
#361232,#361233,#361234,#361235,#361236,#361237,#361238,#361239,#361240,
#361241,#361242,#361243,#361244,#361245),.UNSPECIFIED.,.F.,.F.,(4,2,2,2,
2,2,2,2,2,2,2,2,2,2,2,2,2,4),(-21.7695040114687,-21.712712284324,-21.6533554921043,
-21.5947945436566,-21.5369731193153,-21.4768581247202,-21.4196304517696,
-21.3611373908272,-21.3014984463427,-21.244496915496,-21.1853589043874,
-21.1263381651216,-21.0687067734505,-21.008802722821,-20.951383448243,-20.8930824171696,
-20.8334576289181,-20.8242710457994),.UNSPECIFIED.);
#24609=B_SPLINE_CURVE_WITH_KNOTS('',3,(#361246,#361247,#361248,#361249,
#361250,#361251,#361252,#361253,#361254,#361255,#361256,#361257,#361258,
#361259,#361260,#361261,#361262,#361263,#361264,#361265,#361266,#361267,
#361268,#361269,#361270,#361271,#361272,#361273,#361274,#361275,#361276,
#361277,#361278,#361279,#361280,#361281,#361282,#361283),.UNSPECIFIED.,
 .F.,.F.,(4,2,2,2,2,2,2,2,2,2,2,2,2,2,2,2,2,2,4),(-8.06130686846712,-8.05887034571654,
-7.99894782700157,-7.94008251681837,-7.88266222291039,-7.82215786151287,
-7.76396910049182,-7.70534692624004,-7.64560222270824,-7.58809574321899,
-7.52820385905816,-7.469238704033,-7.41198687597557,-7.35207690934848,-7.29376536285336,
-7.23561890186185,-7.17572793492865,-7.11809152052509,-7.11163898392485),
 .UNSPECIFIED.);
#24610=B_SPLINE_CURVE_WITH_KNOTS('',3,(#361288,#361289,#361290,#361291,
#361292,#361293,#361294,#361295,#361296,#361297,#361298,#361299,#361300,
#361301,#361302,#361303,#361304,#361305,#361306,#361307,#361308,#361309,
#361310,#361311,#361312,#361313,#361314,#361315,#361316,#361317,#361318,
#361319,#361320,#361321,#361322,#361323,#361324,#361325),.UNSPECIFIED.,
 .F.,.F.,(4,2,2,2,2,2,2,2,2,2,2,2,2,2,2,2,2,2,4),(-22.7156509715054,-22.7074186159329,
-22.6499177691702,-22.5901628966359,-22.5323690215547,-22.4741968613821,
-22.4145051589581,-22.3574909491047,-22.2986685245253,-22.238988725518,
-22.1816262395564,-22.1220266368737,-22.0638123939024,-22.0057734757511,
-21.9454180869479,-21.888280649569,-21.8295660328567,-21.7698819675377,
-21.7695040114687),.UNSPECIFIED.);
#24611=B_SPLINE_CURVE_WITH_KNOTS('',3,(#361326,#361327,#361328,#361329,
#361330,#361331,#361332,#361333,#361334,#361335,#361336,#361337,#361338,
#361339,#361340,#361341,#361342,#361343,#361344,#361345,#361346,#361347,
#361348,#361349,#361350,#361351,#361352,#361353,#361354,#361355,#361356,
#361357,#361358,#361359,#361360,#361361),.UNSPECIFIED.,.F.,.F.,(4,2,2,2,
2,2,2,2,2,2,2,2,2,2,2,2,2,4),(-7.11163898392485,-7.05790850141027,-6.99881095248213,
-6.94163674888716,-6.88175725112074,-6.82331090824414,-6.76549239782104,
-6.70544767686958,-6.64767387857181,-6.58808539206054,-6.52881735557916,
-6.47163120579824,-6.41175477442895,-6.353135767859,-6.29556581029132,-6.23532938765596,
-6.17738332888142,-6.16270708252577),.UNSPECIFIED.);
#24612=B_SPLINE_CURVE_WITH_KNOTS('',3,(#361366,#361367,#361368,#361369,
#361370,#361371,#361372,#361373,#361374,#361375,#361376,#361377,#361378,
#361379,#361380,#361381,#361382,#361383,#361384,#361385,#361386,#361387,
#361388,#361389,#361390,#361391,#361392,#361393,#361394,#361395,#361396,
#361397,#361398,#361399,#361400,#361401),.UNSPECIFIED.,.F.,.F.,(4,2,2,2,
2,2,2,2,2,2,2,2,2,2,2,2,2,4),(-23.6614844833627,-23.6449424473843,-23.5871022365362,
-23.5269696420123,-23.4696746996857,-23.4111627281875,-23.3514790699787,
-23.2944469148207,-23.2352891329381,-23.1761484454631,-23.1184942467699,
-23.0585682521832,-23.0010680928138,-22.9427437794047,-22.8830701897237,
-22.8260943458677,-22.7671220016819,-22.7156509715054),.UNSPECIFIED.);
#24613=B_SPLINE_CURVE_WITH_KNOTS('',3,(#361402,#361403,#361404,#361405,
#361406,#361407,#361408,#361409,#361410,#361411,#361412,#361413,#361414,
#361415,#361416,#361417,#361418,#361419,#361420,#361421,#361422,#361423,
#361424,#361425,#361426,#361427,#361428,#361429,#361430,#361431,#361432,
#361433,#361434,#361435,#361436,#361437),.UNSPECIFIED.,.F.,.F.,(4,2,2,2,
2,2,2,2,2,2,2,2,2,2,2,2,2,4),(-6.16270708252577,-6.11831491034659,-6.05884385447613,
-6.0015471618534,-5.94164428182563,-5.88281983108641,-5.82540186288241,
-5.76494103865069,-5.70679248475467,-5.64814168995376,-5.58844065129154,
-5.53097510832359,-5.47110961753744,-5.41218783882286,-5.35495023861937,
-5.29506519854675,-5.23679702670757,-5.21335483239024),.UNSPECIFIED.);
#24614=B_SPLINE_CURVE_WITH_KNOTS('',3,(#361442,#361443,#361444,#361445,
#361446,#361447,#361448,#361449,#361450,#361451,#361452,#361453,#361454,
#361455,#361456,#361457,#361458,#361459,#361460,#361461,#361462,#361463,
#361464,#361465,#361466,#361467,#361468,#361469,#361470,#361471,#361472,
#361473,#361474,#361475,#361476,#361477),.UNSPECIFIED.,.F.,.F.,(4,2,2,2,
2,2,2,2,2,2,2,2,2,2,2,2,2,4),(-24.6081837710824,-24.5830421019898,-24.5248574668377,
-24.4651313068841,-24.4080770368428,-24.3492414934905,-24.2895290755028,
-24.2321524812782,-24.1725395439001,-24.11423689657,-24.0561825895792,-23.9958132061658,
-23.9386229442598,-23.8798930451998,-23.8201687128849,-23.7629816327952,
-23.7036086069725,-23.6614844833627),.UNSPECIFIED.);
#24615=B_SPLINE_CURVE_WITH_KNOTS('',3,(#361478,#361479,#361480,#361481,
#361482,#361483,#361484,#361485,#361486,#361487,#361488,#361489,#361490,
#361491,#361492,#361493,#361494,#361495,#361496,#361497,#361498,#361499,
#361500,#361501,#361502,#361503,#361504,#361505,#361506,#361507,#361508,
#361509,#361510,#361511,#361512,#361513),.UNSPECIFIED.,.F.,.F.,(4,2,2,2,
2,2,2,2,2,2,2,2,2,2,2,2,2,4),(-5.21335483239024,-5.17863572644285,-5.11879123767709,
-5.06119837726108,-5.00096959629774,-4.94192049622973,-4.88477038234289,
-4.82491904471437,-4.7665210924622,-4.70869551497814,-4.64870233321989,
-4.59097673694955,-4.53134899118521,-4.47213387698101,-4.41498350464237,
-4.35513869118441,-4.29657254663883,-4.26486323252877),.UNSPECIFIED.);
#24616=B_SPLINE_CURVE_WITH_KNOTS('',3,(#361518,#361519,#361520,#361521,
#361522,#361523,#361524,#361525,#361526,#361527,#361528,#361529,#361530,
#361531,#361532,#361533,#361534,#361535,#361536,#361537,#361538,#361539,
#361540,#361541,#361542,#361543,#361544,#361545,#361546,#361547,#361548,
#361549,#361550,#361551,#361552,#361553),.UNSPECIFIED.,.F.,.F.,(4,2,2,2,
2,2,2,2,2,2,2,2,2,2,2,2,2,4),(-25.5544342108731,-25.5208509453158,-25.4623356142421,
-25.4026248008999,-25.3455767658485,-25.2864149936997,-25.2271757643632,
-25.1695143091372,-25.1095823895211,-25.0520197529052,-24.9936878585783,
-24.933983338271,-24.8769788824494,-24.8179983510985,-24.7581869330707,
-24.7006743283785,-24.6409086331248,-24.6081837710824),.UNSPECIFIED.);
#24617=B_SPLINE_CURVE_WITH_KNOTS('',3,(#361554,#361555,#361556,#361557,
#361558,#361559,#361560,#361561,#361562,#361563,#361564,#361565,#361566,
#361567,#361568,#361569,#361570,#361571,#361572,#361573,#361574,#361575,
#361576,#361577,#361578,#361579,#361580,#361581,#361582,#361583,#361584,
#361585,#361586,#361587,#361588,#361589),.UNSPECIFIED.,.F.,.F.,(4,2,2,2,
2,2,2,2,2,2,2,2,2,2,2,2,2,4),(-4.26486323252877,-4.23900633934104,-4.17882593258559,
-4.12093219325187,-4.06183508651317,-4.00242073272712,-3.94517207381186,
-3.88530458267638,-3.82653683258786,-3.76913495426055,-3.70873398371094,
-3.65064131432519,-3.59197531230959,-3.53233413127258,-3.47492510292252,
-3.4151018542262,-3.35623950860372,-3.31605621561602),.UNSPECIFIED.);
#24618=B_SPLINE_CURVE_WITH_KNOTS('',3,(#361594,#361595,#361596,#361597,
#361598,#361599,#361600,#361601,#361602,#361603,#361604,#361605,#361606,
#361607,#361608,#361609,#361610,#361611,#361612,#361613,#361614,#361615,
#361616,#361617,#361618,#361619,#361620,#361621,#361622,#361623,#361624,
#361625,#361626,#361627,#361628,#361629),.UNSPECIFIED.,.F.,.F.,(4,2,2,2,
2,2,2,2,2,2,2,2,2,2,2,2,2,4),(-26.5014317973833,-26.4595354955269,-26.4007023230101,
-26.3409740379703,-26.2835984636918,-26.2239878166713,-26.1656152908853,
-26.1075609039662,-26.0471933067983,-25.9899664269833,-25.9312366963228,
-25.8714893191867,-25.8142988852649,-25.754925315871,-25.6961738469028,
-25.6383302605847,-25.5781959419109,-25.5544342108731),.UNSPECIFIED.);
#24619=B_SPLINE_CURVE_WITH_KNOTS('',3,(#361630,#361631,#361632,#361633,
#361634,#361635,#361636,#361637,#361638,#361639,#361640,#361641,#361642,
#361643,#361644,#361645,#361646,#361647,#361648,#361649,#361650,#361651,
#361652,#361653,#361654,#361655,#361656,#361657,#361658,#361659,#361660,
#361661,#361662,#361663,#361664,#361665),.UNSPECIFIED.,.F.,.F.,(4,2,2,2,
2,2,2,2,2,2,2,2,2,2,2,2,2,4),(-3.31605621561602,-3.29903024172096,-3.23918601511716,
-3.18097711727524,-3.12281455031644,-3.0630329501645,-3.00549942169575,
-2.94523805588053,-2.88625374908926,-2.82914188076935,-2.76933468040783,
-2.71100129868167,-2.65318201778556,-2.5932570807603,-2.53559573555263,
-2.47594142993198,-2.41679587971833,-2.36822369355669),.UNSPECIFIED.);
#24620=B_SPLINE_CURVE_WITH_KNOTS('',3,(#361670,#361671,#361672,#361673,
#361674,#361675,#361676,#361677,#361678,#361679,#361680,#361681,#361682,
#361683,#361684,#361685,#361686,#361687,#361688,#361689,#361690,#361691,
#361692,#361693,#361694,#361695,#361696,#361697,#361698,#361699,#361700,
#361701,#361702,#361703,#361704,#361705),.UNSPECIFIED.,.F.,.F.,(4,2,2,2,
2,2,2,2,2,2,2,2,2,2,2,2,2,4),(-27.4478726632988,-27.3973197261978,-27.3381693061291,
-27.2788502071366,-27.2211965408828,-27.1612742376035,-27.1036657370775,
-27.0453414526527,-26.985622716861,-26.9286045043193,-26.8696311738349,
-26.8097314960196,-26.7522222685197,-26.6924613878446,-26.6345397360654,
-26.5763579231836,-26.5166142076797,-26.5014317973833),.UNSPECIFIED.);
#24621=B_SPLINE_CURVE_WITH_KNOTS('',3,(#361706,#361707,#361708,#361709,
#361710,#361711,#361712,#361713,#361714,#361715,#361716,#361717,#361718,
#361719,#361720,#361721,#361722,#361723,#361724,#361725,#361726,#361727,
#361728,#361729,#361730,#361731,#361732,#361733,#361734,#361735,#361736,
#361737,#361738,#361739,#361740,#361741,#361742,#361743),.UNSPECIFIED.,
 .F.,.F.,(4,2,2,2,2,2,2,2,2,2,2,2,2,2,2,2,2,2,4),(-2.36822369355669,-2.35969570935163,
-2.29989858662437,-2.24140177574115,-2.18385270788337,-2.12374532233508,
-2.06592022370505,-2.00680691534119,-1.94746619110531,-1.89028049072034,
-1.8304645649493,-1.77177026671126,-1.71439815249335,-1.65407432487789,
-1.59605411659167,-1.53738550579103,-1.47782136059953,-1.42048534994002,
-1.42021042679425),.UNSPECIFIED.);
#24622=B_SPLINE_CURVE_WITH_KNOTS('',3,(#361748,#361749,#361750,#361751,
#361752,#361753,#361754,#361755,#361756,#361757,#361758,#361759,#361760,
#361761,#361762,#361763,#361764,#361765,#361766,#361767,#361768,#361769,
#361770,#361771,#361772,#361773,#361774,#361775,#361776,#361777,#361778,
#361779,#361780,#361781,#361782,#361783,#361784,#361785),.UNSPECIFIED.,
 .F.,.F.,(4,2,2,2,2,2,2,2,2,2,2,2,2,2,2,2,2,2,4),(-28.394928409372,-28.3927695114757,
-28.335409770902,-28.2758167453806,-28.2173909528416,-28.1593514570261,
-28.0990011252068,-28.0417527514382,-27.9830383059222,-27.9232841801495,
-27.8661041969916,-27.8067454140552,-27.7479262063714,-27.6900942406652,
-27.6299736919414,-27.5725944329335,-27.5140908788942,-27.4543694236753,
-27.4478726632988),.UNSPECIFIED.);
#24623=B_SPLINE_CURVE_WITH_KNOTS('',3,(#361786,#361787,#361788,#361789,
#361790,#361791,#361792,#361793,#361794,#361795,#361796,#361797,#361798,
#361799,#361800,#361801,#361802,#361803,#361804,#361805,#361806,#361807,
#361808,#361809,#361810,#361811,#361812,#361813,#361814,#361815,#361816,
#361817,#361818,#361819,#361820,#361821),.UNSPECIFIED.,.F.,.F.,(4,2,2,2,
2,2,2,2,2,2,2,2,2,2,2,2,2,4),(-1.42021042679425,-1.36072076805539,-1.30193490150738,
-1.24476826914458,-1.18498130105108,-1.12684856833088,-1.06869780383765,
-1.00899657270127,-0.951539157864885,-0.891257122095936,-0.832355083013897,
-0.77529600850504,-0.715549563214565,-0.657298062625355,-0.599498063457814,
-0.539659288862095,-0.482079378649015,-0.473202703359355),.UNSPECIFIED.);
#24624=B_SPLINE_CURVE_WITH_KNOTS('',3,(#361844,#361845,#361846,#361847,
#361848,#361849,#361850,#361851,#361852,#361853,#361854,#361855),
 .UNSPECIFIED.,.F.,.F.,(4,2,2,2,2,4),(-0.173463023786657,-0.144399277485174,
-0.113776308502816,-0.0827143528997853,-0.0458804636919242,-1.0000001323951E-6),
 .UNSPECIFIED.);
#24625=B_SPLINE_CURVE_WITH_KNOTS('',3,(#361859,#361860,#361861,#361862,
#361863,#361864,#361865,#361866,#361867,#361868,#361869,#361870,#361871,
#361872,#361873,#361874,#361875,#361876,#361877,#361878,#361879,#361880,
#361881,#361882),.UNSPECIFIED.,.F.,.F.,(4,2,2,2,2,2,2,2,2,2,2,4),(-0.791270207765327,
-0.749036169028397,-0.706407085981735,-0.662154327887133,-0.624122080956691,
-0.588829396109561,-0.540761862599491,-0.472209855066893,-0.406689863879307,
-0.338868299808933,-0.273977253007298,-0.246317319594991),.UNSPECIFIED.);
#24626=B_SPLINE_CURVE_WITH_KNOTS('',3,(#361886,#361887,#361888,#361889,
#361890,#361891,#361892,#361893,#361894,#361895,#361896,#361897,#361898,
#361899,#361900,#361901),.UNSPECIFIED.,.F.,.F.,(4,2,2,2,2,2,2,4),(-0.246317319594991,
-0.226472527001757,-0.19198199334467,-0.155250487805907,-0.119808408672289,
-0.0860490564446136,-0.045855268046708,0.),.UNSPECIFIED.);
#24627=B_SPLINE_CURVE_WITH_KNOTS('',3,(#361904,#361905,#361906,#361907,
#361908,#361909,#361910,#361911,#361912,#361913,#361914,#361915,#361916,
#361917,#361918,#361919,#361920,#361921,#361922,#361923),.UNSPECIFIED.,
 .F.,.F.,(4,2,2,2,2,2,2,2,2,4),(-0.473202703359355,-0.422410017693474,-0.363351937608626,
-0.306317042413269,-0.246584411472418,-0.188174667531023,-0.130655960205244,
-0.0706399456385561,-0.0347067012271464,0.),.UNSPECIFIED.);
#24628=B_SPLINE_CURVE_WITH_KNOTS('',3,(#361931,#361932,#361933,#361934,
#361935,#361936,#361937,#361938,#361939,#361940,#361941,#361942,#361943,
#361944,#361945,#361946,#361947,#361948,#361949,#361950,#361951,#361952,
#361953,#361954,#361955,#361956,#361957,#361958),.UNSPECIFIED.,.F.,.F.,
(4,2,2,2,2,2,2,2,2,2,2,2,2,4),(-29.1046910466764,-29.0706370137762,-29.0374414130779,
-28.9804238291734,-28.9214729766087,-28.8615025430861,-28.8040116402705,
-28.7442710501027,-28.6863103369922,-28.628146444495,-28.568401372388,-28.5113131027202,
-28.4524975774518,-28.394928409372),.UNSPECIFIED.);
#24629=B_SPLINE_CURVE_WITH_KNOTS('',3,(#361961,#361962,#361963,#361964,
#361965,#361966,#361967,#361968,#361969,#361970,#361971,#361972,#361973,
#361974,#361975,#361976,#361977,#361978),.UNSPECIFIED.,.F.,.F.,(4,2,2,2,
2,2,2,2,4),(0.,0.0314998749400598,0.0537169728612125,0.079677450094962,
0.104184647840863,0.128403600561281,0.152338152262454,0.16487497823377,
0.178500527166238),.UNSPECIFIED.);
#24630=B_SPLINE_CURVE_WITH_KNOTS('',3,(#361979,#361980,#361981,#361982,
#361983,#361984,#361985,#361986,#361987,#361988,#361989,#361990,#361991,
#361992,#361993,#361994),.UNSPECIFIED.,.F.,.F.,(4,2,2,2,2,2,2,4),(0.,0.0490384475420047,
0.0900695236875757,0.13296300706505,0.166655888849848,0.19179904034312,
0.208292684427657,0.22546835719786),.UNSPECIFIED.);
#24631=B_SPLINE_CURVE_WITH_KNOTS('',3,(#363851,#363852,#363853,#363854,
#363855,#363856,#363857,#363858,#363859,#363860,#363861,#363862,#363863,
#363864,#363865,#363866,#363867,#363868,#363869,#363870,#363871,#363872,
#363873,#363874,#363875,#363876,#363877,#363878,#363879),.UNSPECIFIED.,
 .F.,.F.,(4,1,1,1,1,1,1,1,1,1,1,1,1,1,1,1,1,1,1,1,1,1,1,1,1,1,4),(0.,0.0310703336761616,
0.0624385278003938,0.0937144048499659,0.124978469089869,0.166663774179581,
0.208294236860357,0.249966520356582,0.291641529650434,0.3332733240007,0.374947073344913,
0.416620808022619,0.458253030541402,0.499926784452264,0.54160045129851,
0.583232674441905,0.624906496125386,0.666580158626562,0.708211959489969,
0.749887054558503,0.791559255246094,0.833189756589646,0.87487513422873,
0.906139159779086,0.937415106668169,0.968783217665703,1.),.UNSPECIFIED.);
#24632=B_SPLINE_CURVE_WITH_KNOTS('',3,(#363883,#363884,#363885,#363886,
#363887,#363888,#363889,#363890,#363891,#363892,#363893,#363894,#363895,
#363896,#363897,#363898,#363899,#363900,#363901,#363902,#363903,#363904,
#363905,#363906,#363907,#363908,#363909,#363910,#363911),.UNSPECIFIED.,
 .F.,.F.,(4,1,1,1,1,1,1,1,1,1,1,1,1,1,1,1,1,1,1,1,1,1,1,1,1,1,4),(0.,0.0310703336761616,
0.0624385278003938,0.0937144048499659,0.124978469089869,0.166663774179581,
0.208294236860357,0.249966520356582,0.291641529650434,0.3332733240007,0.374947073344913,
0.416620808022619,0.458253030541402,0.499926784452264,0.54160045129851,
0.583232674441905,0.624906496125386,0.666580158626562,0.708211959489969,
0.749887054558503,0.791559255246094,0.833189756589646,0.87487513422873,
0.906139159779086,0.937415106668169,0.968783217665703,1.),.UNSPECIFIED.);
#24633=B_SPLINE_CURVE_WITH_KNOTS('',3,(#364611,#364612,#364613,#364614,
#364615,#364616,#364617,#364618,#364619,#364620,#364621,#364622,#364623,
#364624,#364625,#364626,#364627,#364628,#364629,#364630,#364631,#364632,
#364633,#364634,#364635,#364636,#364637,#364638,#364639,#364640,#364641,
#364642,#364643,#364644,#364645,#364646,#364647,#364648,#364649,#364650,
#364651,#364652,#364653,#364654,#364655,#364656,#364657,#364658,#364659,
#364660,#364661,#364662,#364663,#364664,#364665,#364666,#364667,#364668,
#364669,#364670,#364671,#364672,#364673,#364674,#364675,#364676,#364677,
#364678,#364679,#364680,#364681,#364682,#364683,#364684,#364685,#364686,
#364687,#364688,#364689,#364690,#364691,#364692,#364693,#364694,#364695,
#364696,#364697,#364698,#364699,#364700,#364701,#364702,#364703,#364704,
#364705,#364706,#364707,#364708,#364709),.UNSPECIFIED.,.F.,.F.,(4,1,1,1,
1,1,1,1,1,1,1,1,1,1,1,1,1,1,1,1,1,1,1,1,1,1,1,1,1,1,1,1,1,1,1,1,1,1,1,1,
1,1,1,1,1,1,1,1,1,1,1,1,1,1,1,1,1,1,1,1,1,1,1,1,1,1,1,1,1,1,1,1,1,1,1,1,
1,1,1,1,1,1,1,1,1,1,1,1,1,1,1,1,1,1,1,1,4),(0.,0.0104467457848562,0.0208697051534179,
0.0312830741812588,0.0417059245369557,0.0521151844214314,0.0625350854994869,
0.072955523619078,0.0833651614361216,0.093785355257659,0.104205506224069,
0.114615259182489,0.125035444608255,0.135455580151817,0.145865343296126,
0.156285526040368,0.166705661591602,0.177115425208493,0.187535607700786,
0.197955743339009,0.208365506953668,0.218785689432554,0.229205825080053,
0.239615588692213,0.250035771170918,0.260455906818944,0.270865670430874,
0.281285852909622,0.291705988557657,0.302115752169577,0.312535934648329,
0.322956070296362,0.333365833908282,0.343786016387035,0.354206152035067,
0.364615915646988,0.375036098125741,0.385456233773773,0.395865997385694,
0.406286179864446,0.416706315512479,0.427116079124399,0.437536261603152,
0.447956397251184,0.458366160863105,0.468786343341857,0.47920647898989,
0.48961624260181,0.500036425080563,0.510456560728595,0.520866324340516,
0.531286506819269,0.541706642467301,0.552116406079222,0.562536588557974,
0.572956724206007,0.583366487817927,0.59378667029668,0.604206805944712,
0.614616569556633,0.625036752035385,0.635456887683418,0.645866651295338,
0.656286833774091,0.666706969422123,0.677116733034044,0.687536915512797,
0.697957051160829,0.708366814772749,0.718786997251504,0.729207132899531,
0.739616896511461,0.750037078990207,0.760457214638192,0.770866978250353,
0.781287160728572,0.791707296376735,0.802117059991444,0.812537242460403,
0.822957378121908,0.833367141740239,0.843787324122365,0.85420746003523,
0.864617223206175,0.875037405580635,0.885457544175532,0.895867297492078,
0.906287495257385,0.916707642366043,0.927117283641006,0.937537767903979,
0.947957624414904,0.958366904818021,0.968789794286159,0.979203137018726,
0.989626134310512,1.),.UNSPECIFIED.);
#24634=B_SPLINE_CURVE_WITH_KNOTS('',3,(#364710,#364711,#364712,#364713,
#364714,#364715,#364716,#364717,#364718,#364719,#364720,#364721,#364722,
#364723,#364724,#364725,#364726,#364727,#364728,#364729,#364730,#364731,
#364732,#364733,#364734,#364735,#364736,#364737,#364738,#364739,#364740,
#364741,#364742,#364743,#364744,#364745,#364746,#364747,#364748,#364749,
#364750,#364751,#364752,#364753,#364754,#364755,#364756,#364757,#364758,
#364759,#364760,#364761,#364762,#364763,#364764,#364765,#364766,#364767,
#364768,#364769,#364770,#364771,#364772,#364773,#364774,#364775,#364776,
#364777,#364778,#364779,#364780,#364781,#364782,#364783,#364784,#364785,
#364786,#364787,#364788,#364789,#364790,#364791,#364792,#364793,#364794,
#364795,#364796,#364797,#364798,#364799,#364800,#364801,#364802,#364803,
#364804,#364805,#364806,#364807,#364808),.UNSPECIFIED.,.F.,.F.,(4,1,1,1,
1,1,1,1,1,1,1,1,1,1,1,1,1,1,1,1,1,1,1,1,1,1,1,1,1,1,1,1,1,1,1,1,1,1,1,1,
1,1,1,1,1,1,1,1,1,1,1,1,1,1,1,1,1,1,1,1,1,1,1,1,1,1,1,1,1,1,1,1,1,1,1,1,
1,1,1,1,1,1,1,1,1,1,1,1,1,1,1,1,1,1,1,1,4),(0.,0.0104467457848562,0.0208697051534179,
0.0312830741812588,0.0417059245369557,0.0521151844214314,0.0625350854994869,
0.072955523619078,0.0833651614361216,0.093785355257659,0.104205506224069,
0.114615259182489,0.125035444608255,0.135455580151817,0.145865343296126,
0.156285526040368,0.166705661591602,0.177115425208493,0.187535607700786,
0.197955743339009,0.208365506953668,0.218785689432554,0.229205825080053,
0.239615588692213,0.250035771170918,0.260455906818944,0.270865670430874,
0.281285852909622,0.291705988557657,0.302115752169577,0.312535934648329,
0.322956070296362,0.333365833908282,0.343786016387035,0.354206152035067,
0.364615915646988,0.375036098125741,0.385456233773773,0.395865997385694,
0.406286179864446,0.416706315512479,0.427116079124399,0.437536261603152,
0.447956397251184,0.458366160863105,0.468786343341857,0.47920647898989,
0.48961624260181,0.500036425080563,0.510456560728595,0.520866324340516,
0.531286506819269,0.541706642467301,0.552116406079222,0.562536588557974,
0.572956724206007,0.583366487817927,0.59378667029668,0.604206805944712,
0.614616569556633,0.625036752035385,0.635456887683418,0.645866651295338,
0.656286833774091,0.666706969422123,0.677116733034044,0.687536915512797,
0.697957051160829,0.708366814772749,0.718786997251504,0.729207132899531,
0.739616896511461,0.750037078990207,0.760457214638192,0.770866978250353,
0.781287160728572,0.791707296376735,0.802117059991444,0.812537242460403,
0.822957378121908,0.833367141740239,0.843787324122365,0.85420746003523,
0.864617223206175,0.875037405580635,0.885457544175532,0.895867297492078,
0.906287495257385,0.916707642366043,0.927117283641006,0.937537767903979,
0.947957624414904,0.958366904818021,0.968789794286159,0.979203137018726,
0.989626134310512,1.),.UNSPECIFIED.);
#24635=B_SPLINE_CURVE_WITH_KNOTS('',3,(#365015,#365016,#365017,#365018,
#365019,#365020,#365021,#365022,#365023,#365024,#365025,#365026,#365027,
#365028,#365029,#365030,#365031,#365032,#365033,#365034,#365035,#365036,
#365037,#365038,#365039,#365040,#365041,#365042,#365043),.UNSPECIFIED.,
 .F.,.F.,(4,1,1,1,1,1,1,1,1,1,1,1,1,1,1,1,1,1,1,1,1,1,1,1,1,1,4),(0.,0.0311997468912562,
0.0625509890871527,0.0938098447846757,0.1250568872711,0.166719530856106,
0.208327420639085,0.249977065870109,0.291629399375196,0.333238604634684,
0.374889730322128,0.41654078485731,0.458150415717,0.499801548056339,0.541452534012182,
0.583062165488229,0.624713366295055,0.666364346005318,0.707973557473876,
0.749626035232519,0.791275541260273,0.832883464833855,0.874546235186119,
0.905793212129613,0.937052173453026,0.968403278656631,1.),.UNSPECIFIED.);
#24636=B_SPLINE_CURVE_WITH_KNOTS('',3,(#365044,#365045,#365046,#365047,
#365048,#365049,#365050,#365051,#365052,#365053,#365054,#365055,#365056,
#365057,#365058,#365059,#365060,#365061,#365062,#365063,#365064,#365065,
#365066,#365067,#365068,#365069,#365070,#365071,#365072),.UNSPECIFIED.,
 .F.,.F.,(4,1,1,1,1,1,1,1,1,1,1,1,1,1,1,1,1,1,1,1,1,1,1,1,1,1,4),(0.,0.0311997468912562,
0.0625509890871527,0.0938098447846757,0.1250568872711,0.166719530856106,
0.208327420639085,0.249977065870109,0.291629399375196,0.333238604634684,
0.374889730322128,0.41654078485731,0.458150415717,0.499801548056339,0.541452534012182,
0.583062165488229,0.624713366295055,0.666364346005318,0.707973557473876,
0.749626035232519,0.791275541260273,0.832883464833855,0.874546235186119,
0.905793212129613,0.937052173453026,0.968403278656631,1.),.UNSPECIFIED.);
#24637=B_SPLINE_CURVE_WITH_KNOTS('',3,(#366792,#366793,#366794,#366795,
#366796,#366797,#366798,#366799,#366800,#366801,#366802,#366803,#366804,
#366805,#366806,#366807,#366808,#366809,#366810,#366811),.UNSPECIFIED.,
 .F.,.F.,(4,2,2,2,2,2,2,2,2,4),(-0.472935221504104,-0.468281727374519,-0.40861909809339,
-0.350099286965046,-0.292852212802115,-0.232709468647884,-0.174861617189299,
-0.116285936215957,-0.057358849632408,-1.00000015934576E-6),
 .UNSPECIFIED.);
#24638=B_SPLINE_CURVE_WITH_KNOTS('',3,(#366814,#366815,#366816,#366817,
#366818,#366819,#366820,#366821,#366822,#366823,#366824,#366825,#366826,
#366827,#366828,#366829),.UNSPECIFIED.,.F.,.F.,(4,2,2,2,2,2,2,4),(-14.4244566354324,
-14.3874883625153,-14.3508960651526,-14.2924027349825,-14.2326831946865,
-14.1756382437387,-14.1164979545906,-14.0682546416151),.UNSPECIFIED.);
#24639=B_SPLINE_CURVE_WITH_KNOTS('',3,(#366834,#366835,#366836,#366837,
#366838,#366839,#366840,#366841,#366842,#366843,#366844,#366845,#366846,
#366847,#366848,#366849,#366850,#366851,#366852,#366853,#366854,#366855,
#366856,#366857,#366858,#366859,#366860,#366861,#366862,#366863,#366864,
#366865,#366866,#366867,#366868,#366869),.UNSPECIFIED.,.F.,.F.,(4,2,2,2,
2,2,2,2,2,2,2,2,2,2,2,2,2,4),(-1.4182683932457,-1.40482153675579,-1.34515976227263,
-1.28699062464975,-1.22927287309242,-1.16951868844722,-1.1120201872427,
-1.05243602696549,-0.993461412427311,-0.93650728968302,-0.876859278600447,
-0.818532079283255,-0.761095127096905,-0.701163911011217,-0.643506626123397,
-0.584472913219241,-0.525307825223644,-0.472935221504104),.UNSPECIFIED.);
#24640=B_SPLINE_CURVE_WITH_KNOTS('',3,(#366870,#366871,#366872,#366873,
#366874,#366875,#366876,#366877,#366878,#366879,#366880,#366881,#366882,
#366883,#366884,#366885,#366886,#366887,#366888,#366889,#366890,#366891,
#366892,#366893,#366894,#366895,#366896,#366897,#366898,#366899,#366900,
#366901,#366902,#366903,#366904,#366905),.UNSPECIFIED.,.F.,.F.,(4,2,2,2,
2,2,2,2,2,2,2,2,2,2,2,2,2,4),(-14.0682546416151,-14.0571544660327,-13.9995094275063,
-13.9395966573438,-13.8819763204238,-13.8236606522955,-13.7639424951785,
-13.7069245007115,-13.6479596977281,-13.5880326674721,-13.5305303753149,
-13.4707771853322,-13.4128404091712,-13.3546653789508,-13.2949209937328,
-13.2378385489244,-13.1790120528285,-13.1217523389391),.UNSPECIFIED.);
#24641=B_SPLINE_CURVE_WITH_KNOTS('',3,(#366910,#366911,#366912,#366913,
#366914,#366915,#366916,#366917,#366918,#366919,#366920,#366921,#366922,
#366923,#366924,#366925,#366926,#366927,#366928,#366929,#366930,#366931,
#366932,#366933,#366934,#366935,#366936,#366937,#366938,#366939,#366940,
#366941,#366942,#366943,#366944,#366945),.UNSPECIFIED.,.F.,.F.,(4,2,2,2,
2,2,2,2,2,2,2,2,2,2,2,2,2,4),(-2.36378944550582,-2.34137896891538,-2.2812945893873,
-2.22350291328147,-2.16498583386054,-2.10565909540148,-2.04851852095586,
-1.98886851842519,-1.9301835034246,-1.87308085031929,-1.81337506824985,
-1.75534263888906,-1.69722393727412,-1.63762800227697,-1.58027065314222,
-1.52061845232211,-1.46179970044729,-1.4182683932457),.UNSPECIFIED.);
#24642=B_SPLINE_CURVE_WITH_KNOTS('',3,(#366946,#366947,#366948,#366949,
#366950,#366951,#366952,#366953,#366954,#366955,#366956,#366957,#366958,
#366959,#366960,#366961,#366962,#366963,#366964,#366965,#366966,#366967,
#366968,#366969,#366970,#366971,#366972,#366973,#366974,#366975,#366976,
#366977,#366978,#366979,#366980,#366981,#366982,#366983),.UNSPECIFIED.,
 .F.,.F.,(4,2,2,2,2,2,2,2,2,2,2,2,2,2,2,2,2,2,4),(-13.1217523389391,-13.119283714129,
-13.0619141558394,-13.0023102136998,-12.943917103158,-12.8858683733419,
-12.8255073497059,-12.7682721708645,-12.7095482508193,-12.6497981540076,
-12.5926117849825,-12.5332438298209,-12.4744661438345,-12.4166269551953,
-12.3564978650863,-12.2991396139021,-12.240628743601,-12.1809136964986,
-12.1747564163304),.UNSPECIFIED.);
#24643=B_SPLINE_CURVE_WITH_KNOTS('',3,(#366988,#366989,#366990,#366991,
#366992,#366993,#366994,#366995,#366996,#366997,#366998,#366999,#367000,
#367001,#367002,#367003,#367004,#367005,#367006,#367007,#367008,#367009,
#367010,#367011,#367012,#367013,#367014,#367015,#367016,#367017,#367018,
#367019,#367020,#367021,#367022,#367023),.UNSPECIFIED.,.F.,.F.,(4,2,2,2,
2,2,2,2,2,2,2,2,2,2,2,2,2,4),(-3.30827342425045,-3.27687972744449,-3.21718384712782,
-3.15974147950733,-3.10021755192438,-3.04130042987265,-2.98440223902953,
-2.92481287203565,-2.86654252262006,-2.8091627094274,-2.74928986692013,
-2.69168877540808,-2.63271453390828,-2.57360703640158,-2.51663665270488,
-2.45703247238319,-2.39856948678001,-2.36378944550582),.UNSPECIFIED.);
#24644=B_SPLINE_CURVE_WITH_KNOTS('',3,(#367024,#367025,#367026,#367027,
#367028,#367029,#367030,#367031,#367032,#367033,#367034,#367035,#367036,
#367037,#367038,#367039,#367040,#367041,#367042,#367043,#367044,#367045,
#367046,#367047,#367048,#367049,#367050,#367051,#367052,#367053,#367054,
#367055,#367056,#367057,#367058,#367059),.UNSPECIFIED.,.F.,.F.,(4,2,2,2,
2,2,2,2,2,2,2,2,2,2,2,2,2,4),(-12.1747564163304,-12.1238650424603,-12.064707563846,
-12.0054373680747,-11.9477788345207,-11.8878505439664,-11.8302701344871,
-11.771941095994,-11.7122309526739,-11.6552211790534,-11.5962433434009,
-11.536397643427,-11.4788862588776,-11.4191223407857,-11.361234396967,-11.3030507704824,
-11.2433176900185,-11.2284495394774),.UNSPECIFIED.);
#24645=B_SPLINE_CURVE_WITH_KNOTS('',3,(#367064,#367065,#367066,#367067,
#367068,#367069,#367070,#367071,#367072,#367073,#367074,#367075,#367076,
#367077,#367078,#367079,#367080,#367081,#367082,#367083,#367084,#367085,
#367086,#367087,#367088,#367089,#367090,#367091,#367092,#367093,#367094,
#367095,#367096,#367097,#367098,#367099),.UNSPECIFIED.,.F.,.F.,(4,2,2,2,
2,2,2,2,2,2,2,2,2,2,2,2,2,4),(-4.25326910634686,-4.21251454639597,-4.15309289586531,
-4.09589408206557,-4.03627301194829,-3.97762776411373,-3.92059880643218,
-3.86095544391126,-3.80296175193752,-3.74495194469459,-3.68539344318783,
-3.62807342906873,-3.56793846932016,-3.50917716188511,-3.45225521027217,
-3.3926521707181,-3.33453983230326,-3.30827342425045),.UNSPECIFIED.);
#24646=B_SPLINE_CURVE_WITH_KNOTS('',3,(#367100,#367101,#367102,#367103,
#367104,#367105,#367106,#367107,#367108,#367109,#367110,#367111,#367112,
#367113,#367114,#367115,#367116,#367117,#367118,#367119,#367120,#367121,
#367122,#367123,#367124,#367125,#367126,#367127,#367128,#367129,#367130,
#367131,#367132,#367133,#367134,#367135),.UNSPECIFIED.,.F.,.F.,(4,2,2,2,
2,2,2,2,2,2,2,2,2,2,2,2,2,4),(-11.2284495394774,-11.1862539313897,-11.1274192209345,
-11.0677005448575,-11.0103242661127,-10.9507121374681,-10.8923823346891,
-10.8343279213107,-10.7739591575687,-10.7167546877142,-10.6580247804181,
-10.5982913927564,-10.5411030669475,-10.4817297521307,-10.4230303926228,
-10.3651887976557,-10.3050554630025,-10.2816571097042),.UNSPECIFIED.);
#24647=B_SPLINE_CURVE_WITH_KNOTS('',3,(#367140,#367141,#367142,#367143,
#367144,#367145,#367146,#367147,#367148,#367149,#367150,#367151,#367152,
#367153,#367154,#367155,#367156,#367157,#367158,#367159,#367160,#367161,
#367162,#367163,#367164,#367165,#367166,#367167,#367168,#367169,#367170,
#367171,#367172,#367173,#367174,#367175),.UNSPECIFIED.,.F.,.F.,(4,2,2,2,
2,2,2,2,2,2,2,2,2,2,2,2,2,4),(-5.19889150766547,-5.14881365823251,-5.08980980299638,
-5.03284693005632,-4.97319371313394,-4.91483702785059,-4.85742729771692,
-4.7974638444269,-4.73977725885472,-4.68080804808204,-4.62160937476519,
-4.56456081276647,-4.50488872766924,-4.44633491517977,-4.38910134791393,
-4.32892185865653,-4.2710405265478,-4.25326910634686),.UNSPECIFIED.);
#24648=B_SPLINE_CURVE_WITH_KNOTS('',3,(#367176,#367177,#367178,#367179,
#367180,#367181,#367182,#367183,#367184,#367185,#367186,#367187,#367188,
#367189,#367190,#367191,#367192,#367193,#367194,#367195,#367196,#367197,
#367198,#367199,#367200,#367201,#367202,#367203,#367204,#367205,#367206,
#367207,#367208,#367209,#367210,#367211),.UNSPECIFIED.,.F.,.F.,(4,2,2,2,
2,2,2,2,2,2,2,2,2,2,2,2,2,4),(-10.2816571097042,-10.2477410641564,-10.1892277178352,
-10.1295333942322,-10.0724951191448,-10.0133357139472,-9.95415661279037,
-9.8964995248753,-9.83657116169116,-9.77904666811989,-9.72071934329227,
-9.66103360979029,-9.60404666701626,-9.54507107346665,-9.48532550181212,
-9.42782001815589,-9.36806087538511,-9.33568992122532),.UNSPECIFIED.);
#24649=B_SPLINE_CURVE_WITH_KNOTS('',3,(#367216,#367217,#367218,#367219,
#367220,#367221,#367222,#367223,#367224,#367225,#367226,#367227,#367228,
#367229,#367230,#367231,#367232,#367233,#367234,#367235,#367236,#367237,
#367238,#367239,#367240,#367241,#367242,#367243,#367244,#367245,#367246,
#367247,#367248,#367249,#367250,#367251),.UNSPECIFIED.,.F.,.F.,(4,2,2,2,
2,2,2,2,2,2,2,2,2,2,2,2,2,4),(-6.14456421576452,-6.08570958308235,-6.02698853788712,
-5.9699174554043,-5.91021744604823,-5.85214826557745,-5.79412704547714,
-5.73448887961226,-5.67709342547849,-5.61697940243931,-5.55813653734526,
-5.50116233608994,-5.44149916775544,-5.3833056527042,-5.32562667315605,
-5.26584536369006,-5.20832226100928,-5.19889150766547),.UNSPECIFIED.);
#24650=B_SPLINE_CURVE_WITH_KNOTS('',3,(#367252,#367253,#367254,#367255,
#367256,#367257,#367258,#367259,#367260,#367261,#367262,#367263,#367264,
#367265,#367266,#367267,#367268,#367269,#367270,#367271,#367272,#367273,
#367274,#367275,#367276,#367277,#367278,#367279,#367280,#367281,#367282,
#367283,#367284,#367285,#367286,#367287),.UNSPECIFIED.,.F.,.F.,(4,2,2,2,
2,2,2,2,2,2,2,2,2,2,2,2,2,4),(-9.33568992122532,-9.31068519693683,-9.25063120253579,
-9.19286127678687,-9.1340053853449,-9.07471389558202,-9.01759257466977,
-8.95787936125444,-8.89923227045455,-8.84200302383332,-8.78172385728799,
-8.72375069837283,-8.66530546515211,-8.60578351513382,-8.54849080424378,
-8.48881207353315,-8.43006692171669,-8.3892918312322),.UNSPECIFIED.);
#24651=B_SPLINE_CURVE_WITH_KNOTS('',3,(#367292,#367293,#367294,#367295,
#367296,#367297,#367298,#367299,#367300,#367301,#367302,#367303,#367304,
#367305,#367306,#367307,#367308,#367309,#367310,#367311,#367312,#367313,
#367314,#367315,#367316,#367317,#367318,#367319,#367320,#367321,#367322,
#367323,#367324,#367325,#367326,#367327,#367328,#367329),.UNSPECIFIED.,
 .F.,.F.,(4,2,2,2,2,2,2,2,2,2,2,2,2,2,2,2,2,2,4),(-7.09111164764165,-7.08318036416534,
-7.02348003126206,-6.96505465777705,-6.90762820237831,-6.84759239829551,
-6.7898378115135,-6.73088509922959,-6.67161346650712,-6.6145025289804,-6.55477946680844,
-6.49615286724619,-6.43888999233079,-6.37863405000312,-6.32068091409213,
-6.26215787945088,-6.20265987977463,-6.14538870527694,-6.14456421576452),
 .UNSPECIFIED.);
#24652=B_SPLINE_CURVE_WITH_KNOTS('',3,(#367330,#367331,#367332,#367333,
#367334,#367335,#367336,#367337,#367338,#367339,#367340,#367341,#367342,
#367343,#367344,#367345,#367346,#367347,#367348,#367349,#367350,#367351,
#367352,#367353,#367354,#367355,#367356,#367357,#367358,#367359,#367360,
#367361,#367362,#367363,#367364,#367365),.UNSPECIFIED.,.F.,.F.,(4,2,2,2,
2,2,2,2,2,2,2,2,2,2,2,2,2,4),(-8.3892918312322,-8.37301252043267,-8.31331490309094,
-8.2552211998388,-8.19725815925277,-8.13759205793883,-8.08017135706559,
-8.02016045184272,-7.96128628900145,-7.90431503125115,-7.84464966750369,
-7.78642452640327,-7.72879292598016,-7.66897651712038,-7.6114215848653,
-7.55200710016729,-7.49296560778789,-7.44370351434638),.UNSPECIFIED.);
#24653=B_SPLINE_CURVE_WITH_KNOTS('',3,(#367370,#367371,#367372,#367373,
#367374,#367375,#367376,#367377,#367378,#367379,#367380,#367381,#367382,
#367383,#367384,#367385,#367386,#367387,#367388,#367389,#367390,#367391,
#367392,#367393,#367394,#367395,#367396,#367397,#367398,#367399,#367400,
#367401,#367402,#367403,#367404,#367405),.UNSPECIFIED.,.F.,.F.,(4,2,2,2,
2,2,2,2,2,2,2,2,2,2,2,2,2,4),(-8.03735473147222,-8.02087464960411,-7.9611343773927,
-7.9030065244771,-7.84498694102494,-7.78528651218867,-7.72783232454958,
-7.66775115919979,-7.60884413001691,-7.55183217733595,-7.49212543402685,
-7.43386797250469,-7.37618308062694,-7.31633417516343,-7.25874744107932,
-7.19926567335177,-7.14019290496742,-7.09111164764165),.UNSPECIFIED.);
#24654=B_SPLINE_CURVE_WITH_KNOTS('',3,(#367406,#367407,#367408,#367409,
#367410,#367411,#367412,#367413,#367414,#367415,#367416,#367417,#367418,
#367419,#367420,#367421,#367422,#367423,#367424,#367425,#367426,#367427,
#367428,#367429,#367430,#367431,#367432,#367433,#367434,#367435,#367436,
#367437,#367438,#367439,#367440,#367441,#367442,#367443),.UNSPECIFIED.,
 .F.,.F.,(4,2,2,2,2,2,2,2,2,2,2,2,2,2,2,2,2,2,4),(-7.44370351434638,-7.43598926663215,
-7.37632897618584,-7.31793433550879,-7.26055680051354,-7.20055191970967,
-7.14282768443292,-7.0839377587198,-7.02469610678344,-6.96761672070063,
-6.9079322695684,-6.84933508841591,-6.79211623975549,-6.73188992322172,
-6.67396592905681,-6.61550012837161,-6.55603108184469,-6.49878820169375,
-6.49776578706861),.UNSPECIFIED.);
#24655=B_SPLINE_CURVE_WITH_KNOTS('',3,(#367448,#367449,#367450,#367451,
#367452,#367453,#367454,#367455,#367456,#367457,#367458,#367459,#367460,
#367461,#367462,#367463,#367464,#367465,#367466,#367467,#367468,#367469,
#367470,#367471,#367472,#367473,#367474,#367475,#367476,#367477,#367478,
#367479,#367480,#367481,#367482,#367483),.UNSPECIFIED.,.F.,.F.,(4,2,2,2,
2,2,2,2,2,2,2,2,2,2,2,2,2,4),(-8.98445161616762,-8.95921638570029,-8.89912516429285,
-8.8413188294932,-8.7823951007912,-8.72306736360276,-8.6659089173167,-8.60615099812978,
-8.54746829055918,-8.49018974871482,-8.42987456712495,-8.37186613263263,
-8.31335863269924,-8.2538013865138,-8.19647428240418,-8.13675347140136,
-8.07797359942355,-8.03735473147222),.UNSPECIFIED.);
#24656=B_SPLINE_CURVE_WITH_KNOTS('',3,(#367484,#367485,#367486,#367487,
#367488,#367489,#367490,#367491,#367492,#367493,#367494,#367495,#367496,
#367497,#367498,#367499,#367500,#367501,#367502,#367503,#367504,#367505,
#367506,#367507,#367508,#367509,#367510,#367511,#367512,#367513,#367514,
#367515,#367516,#367517,#367518,#367519),.UNSPECIFIED.,.F.,.F.,(4,2,2,2,
2,2,2,2,2,2,2,2,2,2,2,2,2,4),(-6.49776578706861,-6.43914500581034,-6.38045238997202,
-6.3234204168521,-6.26375689717225,-6.20571563565091,-6.14774582037313,
-6.08813554490324,-6.03076739211196,-5.97071874702609,-5.91190232887527,
-5.85496333454488,-5.79533533481046,-5.73716778380854,-5.67953701682865,
-5.61978163527879,-5.56228402810339,-5.55265580416904),.UNSPECIFIED.);
#24657=B_SPLINE_CURVE_WITH_KNOTS('',3,(#367524,#367525,#367526,#367527,
#367528,#367529,#367530,#367531,#367532,#367533,#367534,#367535,#367536,
#367537,#367538,#367539,#367540,#367541,#367542,#367543,#367544,#367545,
#367546,#367547,#367548,#367549,#367550,#367551,#367552,#367553,#367554,
#367555,#367556,#367557,#367558,#367559),.UNSPECIFIED.,.F.,.F.,(4,2,2,2,
2,2,2,2,2,2,2,2,2,2,2,2,2,4),(-9.93112270433081,-9.89704456919083,-9.83848209313174,
-9.77874344022364,-9.72166028386723,-9.66245135212457,-9.60324573067881,
-9.54554119238533,-9.48556311336624,-9.42800470870366,-9.36810484432635,
-9.31047046348868,-9.25102823330278,-9.19190312444107,-9.13485529115929,
-9.07512386137383,-9.01664620276166,-8.98445161616762),.UNSPECIFIED.);
#24658=B_SPLINE_CURVE_WITH_KNOTS('',3,(#367560,#367561,#367562,#367563,
#367564,#367565,#367566,#367567,#367568,#367569,#367570,#367571,#367572,
#367573,#367574,#367575,#367576,#367577,#367578,#367579,#367580,#367581,
#367582,#367583,#367584,#367585,#367586,#367587,#367588,#367589,#367590,
#367591,#367592,#367593,#367594,#367595),.UNSPECIFIED.,.F.,.F.,(4,2,2,2,
2,2,2,2,2,2,2,2,2,2,2,2,2,4),(-5.55265580416904,-5.50283799464443,-5.44385886442445,
-5.38692656343666,-5.3273071294198,-5.26897469201179,-5.21160876172262,
-5.15166953125696,-5.09400687100007,-5.0350957859107,-4.97592041893457,
-4.91889754803401,-4.85925776188592,-4.80072676094053,-4.74353195103695,
-4.68337526350125,-4.62551653539798,-4.60754988443217),.UNSPECIFIED.);
#24659=B_SPLINE_CURVE_WITH_KNOTS('',3,(#367600,#367601,#367602,#367603,
#367604,#367605,#367606,#367607,#367608,#367609,#367610,#367611,#367612,
#367613,#367614,#367615,#367616,#367617,#367618,#367619,#367620,#367621,
#367622,#367623,#367624,#367625,#367626,#367627,#367628,#367629,#367630,
#367631,#367632,#367633,#367634,#367635),.UNSPECIFIED.,.F.,.F.,(4,2,2,2,
2,2,2,2,2,2,2,2,2,2,2,2,2,4),(-10.8786408780219,-10.8362900188463,-10.7774045193324,
-10.7176387373802,-10.6602132403304,-10.6005496747681,-10.5421870475221,
-10.4840831015066,-10.4236623739244,-10.3664179393046,-10.3076378611891,
-10.2478591049355,-10.1906227194181,-10.1311988593382,-10.072470136304,
-10.0145799907407,-9.95439574519051,-9.93112270433081),.UNSPECIFIED.);
#24660=B_SPLINE_CURVE_WITH_KNOTS('',3,(#367636,#367637,#367638,#367639,
#367640,#367641,#367642,#367643,#367644,#367645,#367646,#367647,#367648,
#367649,#367650,#367651,#367652,#367653,#367654,#367655,#367656,#367657,
#367658,#367659,#367660,#367661,#367662,#367663,#367664,#367665,#367666,
#367667,#367668,#367669,#367670,#367671),.UNSPECIFIED.,.F.,.F.,(4,2,2,2,
2,2,2,2,2,2,2,2,2,2,2,2,2,4),(-4.60754988443217,-4.56704304466917,-4.507643564291,
-4.45046653171621,-4.39087495730951,-4.33225140646798,-4.275256004067,-4.2156426957743,
-4.15767024985269,-4.0997068740148,-4.04016935074741,-3.98287000564575,
-3.9227960098371,-3.86405423063106,-3.80716180627627,-3.74758742087661,
-3.68949419100672,-3.66302281083744),.UNSPECIFIED.);
#24661=B_SPLINE_CURVE_WITH_KNOTS('',3,(#367676,#367677,#367678,#367679,
#367680,#367681,#367682,#367683,#367684,#367685,#367686,#367687,#367688,
#367689,#367690,#367691,#367692,#367693,#367694,#367695,#367696,#367697,
#367698,#367699,#367700,#367701,#367702,#367703,#367704,#367705,#367706,
#367707,#367708,#367709,#367710,#367711),.UNSPECIFIED.,.F.,.F.,(4,2,2,2,
2,2,2,2,2,2,2,2,2,2,2,2,2,4),(-11.8257014074602,-11.7746324045687,-11.7154216905502,
-11.6561202632027,-11.5984106352401,-11.5384288683135,-11.4808104074964,
-11.4224297436371,-11.3626721032327,-11.3056169669095,-11.246587051771,
-11.1867116959658,-11.1291504097255,-11.0693343169958,-11.011410332405,
-10.9531763630212,-10.8933965781418,-10.8786408780219),.UNSPECIFIED.);
#24662=B_SPLINE_CURVE_WITH_KNOTS('',3,(#367712,#367713,#367714,#367715,
#367716,#367717,#367718,#367719,#367720,#367721,#367722,#367723,#367724,
#367725,#367726,#367727,#367728,#367729,#367730,#367731,#367732,#367733,
#367734,#367735,#367736,#367737,#367738,#367739,#367740,#367741,#367742,
#367743,#367744,#367745,#367746,#367747),.UNSPECIFIED.,.F.,.F.,(4,2,2,2,
2,2,2,2,2,2,2,2,2,2,2,2,2,4),(-3.66302281083744,-3.63187733807794,-3.57220028358447,
-3.51477660438808,-3.45531097923445,-3.39641147727633,-3.33953793696864,
-3.27997575463458,-3.22172261505027,-3.1643815174916,-3.10452560936109,
-3.04694146598837,-2.9880210703399,-2.9289296021329,-2.87197863419305,-2.81240006452607,
-2.75395268194537,-2.7189587610551),.UNSPECIFIED.);
#24663=B_SPLINE_CURVE_WITH_KNOTS('',3,(#367752,#367753,#367754,#367755,
#367756,#367757,#367758,#367759,#367760,#367761,#367762,#367763,#367764,
#367765,#367766,#367767,#367768,#367769,#367770,#367771,#367772,#367773,
#367774,#367775,#367776,#367777,#367778,#367779,#367780,#367781,#367782,
#367783,#367784,#367785,#367786,#367787,#367788,#367789),.UNSPECIFIED.,
 .F.,.F.,(4,2,2,2,2,2,2,2,2,2,2,2,2,2,2,2,2,2,4),(-12.7734810909064,-12.7708880798203,
-12.7134657322968,-12.6538066602905,-12.5953765749201,-12.5372747014855,
-12.4768579845627,-12.4195791202852,-12.360801383851,-12.3010019386788,
-12.2437641789621,-12.1843419798448,-12.1255305150722,-12.0676391518563,
-12.0074554104525,-11.9500564718063,-11.89149281404,-11.831729396117,-11.8257014074602),
 .UNSPECIFIED.);
#24664=B_SPLINE_CURVE_WITH_KNOTS('',3,(#367790,#367791,#367792,#367793,
#367794,#367795,#367796,#367797,#367798,#367799,#367800,#367801,#367802,
#367803,#367804,#367805,#367806,#367807,#367808,#367809,#367810,#367811,
#367812,#367813,#367814,#367815,#367816,#367817,#367818,#367819,#367820,
#367821,#367822,#367823,#367824,#367825),.UNSPECIFIED.,.F.,.F.,(4,2,2,2,
2,2,2,2,2,2,2,2,2,2,2,2,2,4),(-2.7189587610551,-2.69679557934989,-2.63672654084043,
-2.57895033520473,-2.52048127345029,-2.46116927811905,-2.40404315464007,
-2.34441705383858,-2.28574632003949,-2.22867155763538,-2.16898900265649,
-2.11097046107922,-2.05289358459059,-1.99331097554254,-1.93596696793388,
-1.87574108507994,-1.81695797180762,-1.77380203185272),.UNSPECIFIED.);
#24665=B_SPLINE_CURVE_WITH_KNOTS('',3,(#367830,#367831,#367832,#367833,
#367834,#367835,#367836,#367837,#367838,#367839,#367840,#367841,#367842,
#367843,#367844,#367845,#367846,#367847,#367848,#367849,#367850,#367851,
#367852,#367853,#367854,#367855,#367856,#367857,#367858,#367859,#367860,
#367861,#367862,#367863,#367864,#367865),.UNSPECIFIED.,.F.,.F.,(4,2,2,2,
2,2,2,2,2,2,2,2,2,2,2,2,2,4),(-13.7207949142504,-13.7095635100018,-13.6518638060279,
-13.5918938652479,-13.5342317348891,-13.4758608361514,-13.4160912900698,
-13.3590244568557,-13.3000039242801,-13.2400428544059,-13.1824870816294,
-13.1226780144681,-13.0647012309748,-13.0064722417789,-12.9466772279908,
-12.8895483636782,-12.8306674186845,-12.7734810909064),.UNSPECIFIED.);
#24666=B_SPLINE_CURVE_WITH_KNOTS('',3,(#367866,#367867,#367868,#367869,
#367870,#367871,#367872,#367873,#367874,#367875,#367876,#367877,#367878,
#367879,#367880,#367881,#367882,#367883,#367884,#367885,#367886,#367887,
#367888,#367889,#367890,#367891,#367892,#367893,#367894,#367895,#367896,
#367897,#367898,#367899,#367900,#367901),.UNSPECIFIED.,.F.,.F.,(4,2,2,2,
2,2,2,2,2,2,2,2,2,2,2,2,2,4),(-1.77380203185272,-1.75999682284082,-1.70035692226662,
-1.64222336071123,-1.58450128192949,-1.52478495274704,-1.46732195812214,
-1.4077112263667,-1.34877556108029,-1.29184626088159,-1.23222248252541,
-1.17393415405485,-1.11649978042292,-1.05660972626645,-0.998990984886199,
-0.939937104231028,-0.880813803640254,-0.828855918263461),.UNSPECIFIED.);
#24667=B_SPLINE_CURVE_WITH_KNOTS('',3,(#367922,#367923,#367924,#367925,
#367926,#367927,#367928,#367929,#367930,#367931,#367932,#367933),
 .UNSPECIFIED.,.F.,.F.,(4,2,2,2,2,4),(-0.17346262697256,-0.144399563151948,
-0.113776683209733,-0.0827144356874581,-0.0458811973302938,-9.99999999945489E-7),
 .UNSPECIFIED.);
#24668=B_SPLINE_CURVE_WITH_KNOTS('',3,(#367937,#367938,#367939,#367940,
#367941,#367942,#367943,#367944,#367945,#367946,#367947,#367948,#367949,
#367950,#367951,#367952,#367953,#367954,#367955,#367956,#367957,#367958,
#367959,#367960,#367961,#367962),.UNSPECIFIED.,.F.,.F.,(4,2,2,2,2,2,2,2,
2,2,2,2,4),(-1.02018564821439,-0.975662064295862,-0.931763813839812,-0.852134429154344,
-0.755247005225842,-0.6619508555074,-0.580085930087374,-0.508496324409023,
-0.441275520650989,-0.407325938090968,-0.339348399346137,-0.274302988628325,
-0.24661014220574),.UNSPECIFIED.);
#24669=B_SPLINE_CURVE_WITH_KNOTS('',3,(#367966,#367967,#367968,#367969,
#367970,#367971,#367972,#367973,#367974,#367975,#367976,#367977,#367978,
#367979,#367980,#367981),.UNSPECIFIED.,.F.,.F.,(4,2,2,2,2,2,2,4),(-0.24661014220574,
-0.2267185418882,-0.192167788882823,-0.155378136435479,-0.119884038074694,
-0.0860669040899276,-0.0458325307501637,0.),.UNSPECIFIED.);
#24670=B_SPLINE_CURVE_WITH_KNOTS('',3,(#367983,#367984,#367985,#367986,
#367987,#367988,#367989,#367990,#367991,#367992,#367993,#367994,#367995,
#367996,#367997,#367998,#367999,#368000,#368001,#368002,#368003,#368004,
#368005,#368006,#368007,#368008,#368009,#368010,#368011,#368012,#368013,
#368014,#368015,#368016),.UNSPECIFIED.,.F.,.F.,(4,2,2,2,2,2,2,2,2,2,2,2,
2,2,2,2,4),(-0.828855918263461,-0.823821086481886,-0.76418512040139,-0.705706920149708,
-0.648470618047626,-0.588371772381769,-0.530564989186055,-0.471977820133801,
-0.412637508461358,-0.355483018030889,-0.295804085119263,-0.237106144384037,
-0.179966956442961,-0.119629528710579,-0.0616069572388075,-0.031150014909439,
0.),.UNSPECIFIED.);
#24671=B_SPLINE_CURVE_WITH_KNOTS('',3,(#368017,#368018,#368019,#368020,
#368021,#368022,#368023,#368024,#368025,#368026,#368027,#368028,#368029,
#368030,#368031,#368032,#368033,#368034,#368035,#368036,#368037,#368038,
#368039,#368040,#368041,#368042,#368043,#368044),.UNSPECIFIED.,.F.,.F.,
(4,2,2,2,2,2,2,2,2,2,2,2,2,4),(-14.4312618797178,-14.3922640324926,-14.3545407029447,
-14.2973154490866,-14.2379103131024,-14.1790334897097,-14.1211559666463,
-14.0609882938093,-14.0035573096291,-13.9450076696767,-13.8852359857398,
-13.8281394143352,-13.7689423216674,-13.7207949142504),.UNSPECIFIED.);
#24672=B_SPLINE_CURVE_WITH_KNOTS('',3,(#368048,#368049,#368050,#368051,
#368052,#368053,#368054,#368055,#368056,#368057,#368058,#368059,#368060,
#368061,#368062,#368063,#368064,#368065),.UNSPECIFIED.,.F.,.F.,(4,2,2,2,
2,2,2,2,4),(0.,0.0314990983415605,0.0537157834318906,0.0796765738993867,
0.104184920565216,0.128404183892005,0.152339319821176,0.164876349211554,
0.178501629664245),.UNSPECIFIED.);
#24673=B_SPLINE_CURVE_WITH_KNOTS('',3,(#368068,#368069,#368070,#368071,
#368072,#368073,#368074,#368075,#368076,#368077,#368078,#368079,#368080,
#368081,#368082,#368083),.UNSPECIFIED.,.F.,.F.,(4,2,2,2,2,2,2,4),(0.,0.049039335524975,
0.0900736384682671,0.132971048637076,0.166666317630351,0.191811791938321,
0.208306699924898,0.225483082815066),.UNSPECIFIED.);
#24674=B_SPLINE_CURVE_WITH_KNOTS('',3,(#369434,#369435,#369436,#369437,
#369438,#369439,#369440,#369441,#369442,#369443,#369444,#369445,#369446,
#369447,#369448,#369449),.UNSPECIFIED.,.F.,.F.,(4,2,2,2,2,2,2,4),(-0.297225196933553,
-0.280367832092781,-0.230062986451411,-0.181680660100882,-0.132941021745363,
-0.0832685681768193,-0.0412377906385104,-1.00000019265245E-6),
 .UNSPECIFIED.);
#24675=B_SPLINE_CURVE_WITH_KNOTS('',3,(#369452,#369453,#369454,#369455,
#369456,#369457,#369458,#369459,#369460,#369461,#369462,#369463),
 .UNSPECIFIED.,.F.,.F.,(4,2,2,2,2,4),(-11.0969330641696,-11.0506498768724,
-11.0060400646789,-10.9574795152701,-10.9078210422652,-10.9002432379435),
 .UNSPECIFIED.);
#24676=B_SPLINE_CURVE_WITH_KNOTS('',3,(#369468,#369469,#369470,#369471,
#369472,#369473,#369474,#369475,#369476,#369477,#369478,#369479,#369480,
#369481,#369482,#369483,#369484,#369485,#369486,#369487,#369488,#369489,
#369490,#369491,#369492,#369493,#369494,#369495,#369496,#369497,#369498,
#369499,#369500,#369501,#369502,#369503),.UNSPECIFIED.,.F.,.F.,(4,2,2,2,
2,2,2,2,2,2,2,2,2,2,2,2,2,4),(-1.08629683604889,-1.06212709216772,-1.01217701512861,
-0.964116528793942,-0.914651515668606,-0.865348804113709,-0.817791776405739,
-0.768003359154763,-0.719235136420373,-0.671389710240228,-0.621277273749783,
-0.573069866056996,-0.524011681351026,-0.474536688662335,-0.426872955991605,
-0.377053394668109,-0.328108386382734,-0.297225196933553),.UNSPECIFIED.);
#24677=B_SPLINE_CURVE_WITH_KNOTS('',3,(#369504,#369505,#369506,#369507,
#369508,#369509,#369510,#369511,#369512,#369513,#369514,#369515,#369516,
#369517,#369518,#369519,#369520,#369521,#369522,#369523,#369524,#369525,
#369526,#369527,#369528,#369529,#369530,#369531,#369532,#369533,#369534,
#369535,#369536,#369537,#369538,#369539),.UNSPECIFIED.,.F.,.F.,(4,2,2,2,
2,2,2,2,2,2,2,2,2,2,2,2,2,4),(-10.9002432379435,-10.8604065333801,-10.8113104443889,
-10.761713814826,-10.7138417906742,-10.6640923927412,-10.616045003083,-10.5676123012695,
-10.5179413964518,-10.470506852643,-10.4215353486384,-10.371439901378,-10.3236642057133,
-10.2740225073813,-10.2256879132737,-10.1773476975794,-10.1276391307857,
-10.1132239534235),.UNSPECIFIED.);
#24678=B_SPLINE_CURVE_WITH_KNOTS('',3,(#369544,#369545,#369546,#369547,
#369548,#369549,#369550,#369551,#369552,#369553,#369554,#369555,#369556,
#369557,#369558,#369559,#369560,#369561,#369562,#369563,#369564,#369565,
#369566,#369567,#369568,#369569,#369570,#369571,#369572,#369573,#369574,
#369575,#369576,#369577,#369578,#369579),.UNSPECIFIED.,.F.,.F.,(4,2,2,2,
2,2,2,2,2,2,2,2,2,2,2,2,2,4),(-1.87536861874309,-1.84355584199448,-1.79384949462906,
-1.74600741502996,-1.69621082068226,-1.64716056762169,-1.59957435410145,
-1.5497648282856,-1.5012562446633,-1.45296588180679,-1.40314413691098,-1.35519906350488,
-1.305259866274,-1.25610014245001,-1.20856696990882,-1.15878121320228,-1.11015973495678,
-1.08629683604889),.UNSPECIFIED.);
#24679=B_SPLINE_CURVE_WITH_KNOTS('',3,(#369580,#369581,#369582,#369583,
#369584,#369585,#369586,#369587,#369588,#369589,#369590,#369591,#369592,
#369593,#369594,#369595,#369596,#369597,#369598,#369599,#369600,#369601,
#369602,#369603,#369604,#369605,#369606,#369607,#369608,#369609,#369610,
#369611,#369612,#369613,#369614,#369615),.UNSPECIFIED.,.F.,.F.,(4,2,2,2,
2,2,2,2,2,2,2,2,2,2,2,2,2,4),(-10.1132239534235,-10.0801144057446,-10.0312319726685,
-9.98154103730301,-9.93385667477381,-9.88431791432676,-9.83555841579789,
-9.78730128208498,-9.73712994715777,-9.68943338837994,-9.64061521762979,
-9.59087875638848,-9.54332419146615,-9.49397528474752,-9.44486869631985,
-9.3967780067164,-9.34679000923077,-9.3251899560265),.UNSPECIFIED.);
#24680=B_SPLINE_CURVE_WITH_KNOTS('',3,(#369620,#369621,#369622,#369623,
#369624,#369625,#369626,#369627,#369628,#369629,#369630,#369631,#369632,
#369633,#369634,#369635,#369636,#369637,#369638,#369639,#369640,#369641,
#369642,#369643,#369644,#369645,#369646,#369647,#369648,#369649,#369650,
#369651,#369652,#369653,#369654,#369655),.UNSPECIFIED.,.F.,.F.,(4,2,2,2,
2,2,2,2,2,2,2,2,2,2,2,2,2,4),(-2.66450830210884,-2.62523893706397,-2.57591415214878,
-2.52835492082748,-2.47857795237277,-2.42978650601587,-2.38198894395603,
-2.33185002481024,-2.28361946775828,-2.23466059104454,-2.18515729676512,
-2.1374720120089,-2.08765685324303,-2.03868217100641,-1.99096903863913,
-1.94063103897361,-1.89221929222858,-1.87536861874309),.UNSPECIFIED.);
#24681=B_SPLINE_CURVE_WITH_KNOTS('',3,(#369656,#369657,#369658,#369659,
#369660,#369661,#369662,#369663,#369664,#369665,#369666,#369667,#369668,
#369669,#369670,#369671,#369672,#369673,#369674,#369675,#369676,#369677,
#369678,#369679,#369680,#369681,#369682,#369683,#369684,#369685,#369686,
#369687,#369688,#369689,#369690,#369691),.UNSPECIFIED.,.F.,.F.,(4,2,2,2,
2,2,2,2,2,2,2,2,2,2,2,2,2,4),(-9.3251899560265,-9.29896232620477,-9.25031178750326,
-9.20059733433329,-9.15312351256986,-9.10393801333592,-9.05440164539032,
-9.00644825470644,-8.95661223118013,-8.90857392265958,-8.86005981037984,
-8.81033962393501,-8.76286474277573,-8.71381206706934,-8.66378663798527,
-8.61593806564963,-8.56621891848283,-8.53743262087695),.UNSPECIFIED.);
#24682=B_SPLINE_CURVE_WITH_KNOTS('',3,(#369696,#369697,#369698,#369699,
#369700,#369701,#369702,#369703,#369704,#369705,#369706,#369707,#369708,
#369709,#369710,#369711,#369712,#369713,#369714,#369715,#369716,#369717,
#369718,#369719,#369720,#369721,#369722,#369723,#369724,#369725,#369726,
#369727,#369728,#369729,#369730,#369731),.UNSPECIFIED.,.F.,.F.,(4,2,2,2,
2,2,2,2,2,2,2,2,2,2,2,2,2,4),(-3.45311041785451,-3.40640578800035,-3.35734889527748,
-3.30979687791647,-3.26001136181265,-3.21149516431656,-3.16328629585956,
-3.11345375633878,-3.06550007523919,-3.01569323829511,-2.96651867048036,
-2.91900255270055,-2.86923473474433,-2.8205974011257,-2.77263121805615,
-2.72266205646393,-2.6745852915141,-2.66450830210884),.UNSPECIFIED.);
#24683=B_SPLINE_CURVE_WITH_KNOTS('',3,(#369732,#369733,#369734,#369735,
#369736,#369737,#369738,#369739,#369740,#369741,#369742,#369743,#369744,
#369745,#369746,#369747,#369748,#369749,#369750,#369751,#369752,#369753,
#369754,#369755,#369756,#369757,#369758,#369759,#369760,#369761,#369762,
#369763,#369764,#369765,#369766,#369767),.UNSPECIFIED.,.F.,.F.,(4,2,2,2,
2,2,2,2,2,2,2,2,2,2,2,2,2,4),(-8.53743262087695,-8.51790557886756,-8.4694930188994,
-8.41974122096977,-8.37219191612705,-8.32323738821537,-8.27350131454077,
-8.22574932274126,-8.17613872282825,-8.12742281473662,-8.07909951276689,
-8.0288568753523,-7.98115537034797,-7.9322702522769,-7.8825002114564,-7.83489172319436,
-7.7854767277125,-7.74885616038243),.UNSPECIFIED.);
#24684=B_SPLINE_CURVE_WITH_KNOTS('',3,(#369772,#369773,#369774,#369775,
#369776,#369777,#369778,#369779,#369780,#369781,#369782,#369783,#369784,
#369785,#369786,#369787,#369788,#369789,#369790,#369791,#369792,#369793,
#369794,#369795,#369796,#369797,#369798,#369799,#369800,#369801,#369802,
#369803,#369804,#369805,#369806,#369807,#369808,#369809),.UNSPECIFIED.,
 .F.,.F.,(4,2,2,2,2,2,2,2,2,2,2,2,2,2,2,2,2,2,4),(-4.24192213155039,-4.23809792147632,
-4.18836234856388,-4.13957498951885,-4.09185274799052,-4.04171529566761,
-3.9934886596208,-3.94465978359765,-3.89515592670361,-3.84747283207717,
-3.79769147839944,-3.74871439112587,-3.7010548294868,-3.65071175267311,
-3.60229775019791,-3.55373929331727,-3.50402693278433,-3.45618073503253,
-3.45311041785451),.UNSPECIFIED.);
#24685=B_SPLINE_CURVE_WITH_KNOTS('',3,(#369810,#369811,#369812,#369813,
#369814,#369815,#369816,#369817,#369818,#369819,#369820,#369821,#369822,
#369823,#369824,#369825,#369826,#369827,#369828,#369829,#369830,#369831,
#369832,#369833,#369834,#369835,#369836,#369837,#369838,#369839,#369840,
#369841,#369842,#369843,#369844,#369845),.UNSPECIFIED.,.F.,.F.,(4,2,2,2,
2,2,2,2,2,2,2,2,2,2,2,2,2,4),(-7.74885616038243,-7.73643534531436,-7.68828489874703,
-7.63823245858939,-7.59041958736585,-7.54170890559822,-7.49196769011302,
-7.44445938896145,-7.39521440060387,-7.34576049706096,-7.2977545191574,
-7.24786179061972,-7.19985584140599,-7.15128928192139,-7.10154861462626,
-7.05405787738374,-7.00495329873603,-6.96074678199533),.UNSPECIFIED.);
#24686=B_SPLINE_CURVE_WITH_KNOTS('',3,(#369850,#369851,#369852,#369853,
#369854,#369855,#369856,#369857,#369858,#369859,#369860,#369861,#369862,
#369863,#369864,#369865,#369866,#369867,#369868,#369869,#369870,#369871,
#369872,#369873,#369874,#369875,#369876,#369877,#369878,#369879,#369880,
#369881,#369882,#369883,#369884,#369885),.UNSPECIFIED.,.F.,.F.,(4,2,2,2,
2,2,2,2,2,2,2,2,2,2,2,2,2,4),(-5.02972443161939,-5.0187363541838,-4.96900575987408,
-4.92050955509127,-4.87241366245925,-4.82259855136958,-4.77466360731621,
-4.72502503301001,-4.67586344949185,-4.62839019418675,-4.57867076701161,
-4.53004498522224,-4.48217452916704,-4.43221432415173,-4.38414845254951,
-4.33495397914721,-4.28563488367131,-4.24192213155039),.UNSPECIFIED.);
#24687=B_SPLINE_CURVE_WITH_KNOTS('',3,(#369886,#369887,#369888,#369889,
#369890,#369891,#369892,#369893,#369894,#369895,#369896,#369897,#369898,
#369899,#369900,#369901,#369902,#369903,#369904,#369905,#369906,#369907,
#369908,#369909,#369910,#369911,#369912,#369913,#369914,#369915,#369916,
#369917,#369918,#369919,#369920,#369921,#369922,#369923),.UNSPECIFIED.,
 .F.,.F.,(4,2,2,2,2,2,2,2,2,2,2,2,2,2,2,2,2,2,4),(-6.96074678199533,-6.95502152207767,
-6.90527708144643,-6.85655770199055,-6.80874804770292,-6.75868624361776,
-6.71052715808686,-6.66149720058363,-6.61207258246791,-6.56445611871926,
-6.51468173086547,-6.46578683168715,-6.41808529513843,-6.36783220114316,
-6.31949923703344,-6.27079116033409,-6.2211700228527,-6.17340813772743,
-6.17206263548208),.UNSPECIFIED.);
#24688=B_SPLINE_CURVE_WITH_KNOTS('',3,(#369928,#369929,#369930,#369931,
#369932,#369933,#369934,#369935,#369936,#369937,#369938,#369939,#369940,
#369941,#369942,#369943,#369944,#369945,#369946,#369947,#369948,#369949,
#369950,#369951,#369952,#369953,#369954,#369955,#369956,#369957,#369958,
#369959,#369960,#369961,#369962,#369963),.UNSPECIFIED.,.F.,.F.,(4,2,2,2,
2,2,2,2,2,2,2,2,2,2,2,2,2,4),(-5.81829984350504,-5.80046863144242,-5.75023363519347,
-5.70191564674989,-5.65311229785516,-5.60351043799573,-5.55576557565544,
-5.50601560630357,-5.45707070341708,-5.40949261239909,-5.35972528079792,
-5.31132312095601,-5.26294159013347,-5.21323577254684,-5.16539862838024,
-5.11526216484913,-5.06622663267278,-5.02972443161939),.UNSPECIFIED.);
#24689=B_SPLINE_CURVE_WITH_KNOTS('',3,(#369964,#369965,#369966,#369967,
#369968,#369969,#369970,#369971,#369972,#369973,#369974,#369975,#369976,
#369977,#369978,#369979,#369980,#369981,#369982,#369983,#369984,#369985,
#369986,#369987,#369988,#369989,#369990,#369991,#369992,#369993,#369994,
#369995,#369996,#369997,#369998,#369999),.UNSPECIFIED.,.F.,.F.,(4,2,2,2,
2,2,2,2,2,2,2,2,2,2,2,2,2,4),(-6.17206263548208,-6.12366583999162,-6.07470074073969,
-6.02714826734756,-5.97739057213024,-5.92896739037585,-5.88065826419392,
-5.83092771067481,-5.78306843191849,-5.73305506215986,-5.68399039252467,
-5.63650975764823,-5.58678270549522,-5.53825654861325,-5.49022040156367,
-5.44037153355227,-5.39240610619022,-5.38405069970025),.UNSPECIFIED.);
#24690=B_SPLINE_CURVE_WITH_KNOTS('',3,(#370004,#370005,#370006,#370007,
#370008,#370009,#370010,#370011,#370012,#370013,#370014,#370015,#370016,
#370017,#370018,#370019,#370020,#370021,#370022,#370023,#370024,#370025,
#370026,#370027,#370028,#370029,#370030,#370031,#370032,#370033,#370034,
#370035,#370036,#370037,#370038,#370039),.UNSPECIFIED.,.F.,.F.,(4,2,2,2,
2,2,2,2,2,2,2,2,2,2,2,2,2,4),(-6.60703756023774,-6.58187604768098,-6.53197903755641,
-6.48396727026408,-6.43439222014541,-6.38514596147057,-6.3376172967117,
-6.28784666941341,-6.23913583046104,-6.19126067984556,-6.14121030559726,
-6.09305995544669,-6.04391250359479,-5.99450161250507,-5.94688905770524,
-5.89709533587369,-5.84821560509502,-5.81829984350504),.UNSPECIFIED.);
#24691=B_SPLINE_CURVE_WITH_KNOTS('',3,(#370040,#370041,#370042,#370043,
#370044,#370045,#370046,#370047,#370048,#370049,#370050,#370051,#370052,
#370053,#370054,#370055,#370056,#370057,#370058,#370059,#370060,#370061,
#370062,#370063,#370064,#370065,#370066,#370067,#370068,#370069,#370070,
#370071,#370072,#370073,#370074,#370075),.UNSPECIFIED.,.F.,.F.,(4,2,2,2,
2,2,2,2,2,2,2,2,2,2,2,2,2,4),(-5.38405069970025,-5.34288008366044,-5.29368130835127,
-5.24619867625064,-5.19647632389707,-5.14781244101478,-5.09998408356202,
-5.04998193383878,-5.00187799656936,-4.95277901109365,-4.90341570644776,
-4.85584909893607,-4.80610361642015,-4.75727094726801,-4.70957047324575,
-4.65938382194792,-4.61111235420568,-4.59595956437439),.UNSPECIFIED.);
#24692=B_SPLINE_CURVE_WITH_KNOTS('',3,(#370080,#370081,#370082,#370083,
#370084,#370085,#370086,#370087,#370088,#370089,#370090,#370091,#370092,
#370093,#370094,#370095,#370096,#370097,#370098,#370099,#370100,#370101,
#370102,#370103,#370104,#370105,#370106,#370107,#370108,#370109,#370110,
#370111,#370112,#370113,#370114,#370115),.UNSPECIFIED.,.F.,.F.,(4,2,2,2,
2,2,2,2,2,2,2,2,2,2,2,2,2,4),(-7.39570158201985,-7.36254636003036,-7.31362768878039,
-7.26390072255125,-7.21618108953506,-7.16660564252708,-7.11781333282715,
-7.06952057237752,-7.02105052930277,-6.97269388442146,-6.92291523017473,
-6.87500964654849,-6.82494668210698,-6.77583459408507,-6.72830776969244,
-6.67853238433299,-6.62995933898348,-6.60703756023774),.UNSPECIFIED.);
#24693=B_SPLINE_CURVE_WITH_KNOTS('',3,(#370116,#370117,#370118,#370119,
#370120,#370121,#370122,#370123,#370124,#370125,#370126,#370127,#370128,
#370129,#370130,#370131,#370132,#370133,#370134,#370135,#370136,#370137,
#370138,#370139,#370140,#370141,#370142,#370143,#370144,#370145,#370146,
#370147,#370148,#370149,#370150,#370151),.UNSPECIFIED.,.F.,.F.,(4,2,2,2,
2,2,2,2,2,2,2,2,2,2,2,2,2,4),(-4.59595956437439,-4.56235695294563,-4.51280281574693,
-4.46510390240623,-4.41540203036628,-4.36650420699104,-4.31897228058962,
-4.269253079062,-4.22089746757123,-4.17256328077253,-4.12290523769736,-4.07511408620101,
-4.0250270996101,-3.97603865570477,-3.92859432163572,-3.87891176911502,
-3.83046212492628,-3.80838734160697),.UNSPECIFIED.);
#24694=B_SPLINE_CURVE_WITH_KNOTS('',3,(#370156,#370157,#370158,#370159,
#370160,#370161,#370162,#370163,#370164,#370165,#370166,#370167,#370168,
#370169,#370170,#370171,#370172,#370173,#370174,#370175,#370176,#370177,
#370178,#370179,#370180,#370181,#370182,#370183,#370184,#370185,#370186,
#370187,#370188,#370189,#370190,#370191),.UNSPECIFIED.,.F.,.F.,(4,2,2,2,
2,2,2,2,2,2,2,2,2,2,2,2,2,4),(-8.18329352926,-8.14340210893405,-8.09426912520822,
-8.04463960472576,-7.99673177620422,-7.94694511105315,-7.89886443645484,
-7.85039553897279,-7.80068849465037,-7.75321967281652,-7.70421160318344,
-7.654083175026,-7.60627199042295,-7.55659336826637,-7.50822562336118,-7.45984954124163,
-7.41010498272117,-7.39570158201985),.UNSPECIFIED.);
#24695=B_SPLINE_CURVE_WITH_KNOTS('',3,(#370192,#370193,#370194,#370195,
#370196,#370197,#370198,#370199,#370200,#370201,#370202,#370203,#370204,
#370205,#370206,#370207,#370208,#370209,#370210,#370211,#370212,#370213,
#370214,#370215,#370216,#370217,#370218,#370219,#370220,#370221,#370222,
#370223,#370224,#370225,#370226,#370227),.UNSPECIFIED.,.F.,.F.,(4,2,2,2,
2,2,2,2,2,2,2,2,2,2,2,2,2,4),(-3.80838734160697,-3.78241319552622,-3.73264588502551,
-3.68475695452833,-3.63516729185455,-3.58605284696992,-3.53862535621508,
-3.48895390409539,-3.44037473596106,-3.39255087588116,-3.34263853913331,
-3.2946187404684,-3.24547260749217,-3.19620074039827,-3.14870942771508,
-3.09902178513712,-3.05028113183768,-3.02126527915157),.UNSPECIFIED.);
#24696=B_SPLINE_CURVE_WITH_KNOTS('',3,(#370232,#370233,#370234,#370235,
#370236,#370237,#370238,#370239,#370240,#370241,#370242,#370243,#370244,
#370245,#370246,#370247,#370248,#370249,#370250,#370251,#370252,#370253,
#370254,#370255,#370256,#370257,#370258,#370259,#370260,#370261,#370262,
#370263,#370264,#370265,#370266,#370267),.UNSPECIFIED.,.F.,.F.,(4,2,2,2,
2,2,2,2,2,2,2,2,2,2,2,2,2,4),(-8.97097791248705,-8.92371187470672,-8.8742385366992,
-8.82542327411857,-8.77722580886648,-8.72711902037387,-8.67941669194377,
-8.63065883194959,-8.58094855992311,-8.5334381898614,-8.48414871101692,
-8.43496520836685,-8.38692752659352,-8.33699692985527,-8.28914382647278,
-8.24054650130081,-8.19085146033859,-8.18329352926),.UNSPECIFIED.);
#24697=B_SPLINE_CURVE_WITH_KNOTS('',3,(#370268,#370269,#370270,#370271,
#370272,#370273,#370274,#370275,#370276,#370277,#370278,#370279,#370280,
#370281,#370282,#370283,#370284,#370285,#370286,#370287,#370288,#370289,
#370290,#370291,#370292,#370293,#370294,#370295,#370296,#370297,#370298,
#370299,#370300,#370301,#370302,#370303),.UNSPECIFIED.,.F.,.F.,(4,2,2,2,
2,2,2,2,2,2,2,2,2,2,2,2,2,4),(-3.02126527915157,-3.00260516806742,-2.95251569085902,
-2.90433522308815,-2.85555414669426,-2.80609764269441,-2.75846016823742,
-2.70872672337365,-2.6597964690442,-2.61218293988413,-2.56188798012619,
-2.51352027335298,-2.46500914259868,-2.41534428872647,-2.36754382854494,
-2.31781668136951,-2.26880666392932,-2.23313514244992),.UNSPECIFIED.);
#24698=B_SPLINE_CURVE_WITH_KNOTS('',3,(#370308,#370309,#370310,#370311,
#370312,#370313,#370314,#370315,#370316,#370317,#370318,#370319,#370320,
#370321,#370322,#370323,#370324,#370325,#370326,#370327,#370328,#370329,
#370330,#370331,#370332,#370333,#370334,#370335,#370336,#370337,#370338,
#370339,#370340,#370341,#370342,#370343,#370344,#370345),.UNSPECIFIED.,
 .F.,.F.,(4,2,2,2,2,2,2,2,2,2,2,2,2,2,2,2,2,2,4),(-9.75953055606769,-9.75289518479629,
-9.70497206855282,-9.65517152839672,-9.60698210655507,-9.55849670090529,
-9.508738741953,-9.46121175815317,-9.4121858661215,-9.36243877625384,-9.31462252400408,
-9.26494150013379,-9.21639972157875,-9.16801578697161,-9.11770432709358,
-9.07006743064845,-9.02112077880878,-8.97136573631902,-8.97097791248705),
 .UNSPECIFIED.);
#24699=B_SPLINE_CURVE_WITH_KNOTS('',3,(#370346,#370347,#370348,#370349,
#370350,#370351,#370352,#370353,#370354,#370355,#370356,#370357,#370358,
#370359,#370360,#370361,#370362,#370363,#370364,#370365,#370366,#370367,
#370368,#370369,#370370,#370371,#370372,#370373,#370374,#370375,#370376,
#370377,#370378,#370379,#370380,#370381),.UNSPECIFIED.,.F.,.F.,(4,2,2,2,
2,2,2,2,2,2,2,2,2,2,2,2,2,4),(-2.23313514244992,-2.22130041501826,-2.17156272926473,
-2.12309288159397,-2.0749308070373,-2.02514585029162,-1.97723797307212,
-1.92747988450581,-1.87835223712549,-1.83088170783493,-1.78116165238413,
-1.73257071664056,-1.68465096511949,-1.63472944881252,-1.58669854238685,
-1.53740037538244,-1.48812259544505,-1.44532777081289),.UNSPECIFIED.);
#24700=B_SPLINE_CURVE_WITH_KNOTS('',3,(#370386,#370387,#370388,#370389,
#370390,#370391,#370392,#370393,#370394,#370395,#370396,#370397,#370398,
#370399,#370400,#370401,#370402,#370403,#370404,#370405,#370406,#370407,
#370408,#370409,#370410,#370411,#370412,#370413,#370414,#370415,#370416,
#370417,#370418,#370419,#370420,#370421),.UNSPECIFIED.,.F.,.F.,(4,2,2,2,
2,2,2,2,2,2,2,2,2,2,2,2,2,4),(-10.5477144568492,-10.5343257988314,-10.4861277850314,
-10.4360230035294,-10.3882489608822,-10.3394904162225,-10.2897425906394,
-10.2422130277014,-10.1929213240059,-10.143590495231,-10.0955453254922,
-10.0456092788967,-9.99766435067504,-9.94905890957184,-9.89931940611708,
-9.85183049354891,-9.80268801893929,-9.75953055606769),.UNSPECIFIED.);
#24701=B_SPLINE_CURVE_WITH_KNOTS('',3,(#370422,#370423,#370424,#370425,
#370426,#370427,#370428,#370429,#370430,#370431,#370432,#370433,#370434,
#370435,#370436,#370437,#370438,#370439,#370440,#370441,#370442,#370443,
#370444,#370445,#370446,#370447,#370448,#370449,#370450,#370451,#370452,
#370453,#370454,#370455,#370456,#370457,#370458,#370459),.UNSPECIFIED.,
 .F.,.F.,(4,2,2,2,2,2,2,2,2,2,2,2,2,2,2,2,2,2,4),(-1.44532777081289,-1.44060883240002,
-1.39087958066294,-1.34213461919547,-1.2943831702068,-1.24429199807141,
-1.19610739026894,-1.14719616446327,-1.09773999499641,-1.05010013906413,
-1.00033267427764,-0.951404599399516,-0.903737328903778,-0.853447213420372,
-0.805081539111285,-0.756465263702377,-0.706806190913238,-0.659009625901751,
-0.656744776062406),.UNSPECIFIED.);
#24702=B_SPLINE_CURVE_WITH_KNOTS('',3,(#370463,#370464,#370465,#370466,
#370467,#370468,#370469,#370470,#370471,#370472,#370473,#370474),
 .UNSPECIFIED.,.F.,.F.,(4,2,2,2,2,4),(-0.147125121134148,-0.128349501591643,
-0.105314013958521,-0.0783046855556977,-0.042089246328591,-1.00000017627666E-6),
 .UNSPECIFIED.);
#24703=B_SPLINE_CURVE_WITH_KNOTS('',3,(#370476,#370477,#370478,#370479,
#370480,#370481,#370482,#370483,#370484,#370485,#370486,#370487,#370488,
#370489,#370490,#370491,#370492,#370493,#370494,#370495,#370496,#370497,
#370498,#370499),.UNSPECIFIED.,.F.,.F.,(4,2,2,2,2,2,2,2,2,2,2,4),(-1.13468288871823,
-1.0706043934222,-1.00734719961197,-0.908024292964587,-0.805111116080014,
-0.706602531207623,-0.634633508201914,-0.578664318892748,-0.526740212001412,
-0.472667922135714,-0.421519787488127,-0.367202841889784),.UNSPECIFIED.);
#24704=B_SPLINE_CURVE_WITH_KNOTS('',3,(#370503,#370504,#370505,#370506,
#370507,#370508,#370509,#370510,#370511,#370512,#370513,#370514,#370515,
#370516,#370517,#370518,#370519,#370520),.UNSPECIFIED.,.F.,.F.,(4,2,2,2,
2,2,2,2,4),(-0.367202841889784,-0.360788898680035,-0.297043709635829,-0.22884142572636,
-0.166869586833399,-0.11581538945378,-0.0610544135172069,-0.0270530161618892,
-1.00000019448432E-6),.UNSPECIFIED.);
#24705=B_SPLINE_CURVE_WITH_KNOTS('',3,(#370523,#370524,#370525,#370526,
#370527,#370528,#370529,#370530,#370531,#370532,#370533,#370534,#370535,
#370536,#370537,#370538,#370539,#370540,#370541,#370542,#370543,#370544,
#370545,#370546,#370547,#370548,#370549,#370550,#370551,#370552),
 .UNSPECIFIED.,.F.,.F.,(4,2,2,2,2,2,2,2,2,2,2,2,2,2,4),(-0.656744776062406,
-0.609260683930364,-0.560257149562067,-0.51271659362795,-0.462954754241167,
-0.414492365041179,-0.366248708414827,-0.31647438439645,-0.26857495964527,
-0.218684447711158,-0.1695714801609,-0.122083779620549,-0.0723456381913861,
-0.035554498052184,-1.00000012637214E-6),.UNSPECIFIED.);
#24706=B_SPLINE_CURVE_WITH_KNOTS('',3,(#370555,#370556,#370557,#370558,
#370559,#370560,#370561,#370562,#370563,#370564,#370565,#370566,#370567,
#370568,#370569,#370570,#370571,#370572,#370573,#370574,#370575,#370576,
#370577,#370578,#370579,#370580),.UNSPECIFIED.,.F.,.F.,(4,2,2,2,2,2,2,2,
2,2,2,2,4),(-11.1077295770696,-11.0661775997393,-11.0237973371211,-10.9741258386803,
-10.9254829944382,-10.8771047475493,-10.8268019041466,-10.7791148973966,
-10.7301741164739,-10.6803891069329,-10.6327360727518,-10.5832668289047,
-10.5477144568492),.UNSPECIFIED.);
#24707=B_SPLINE_CURVE_WITH_KNOTS('',3,(#370599,#370600,#370601,#370602,
#370603,#370604,#370605,#370606,#370607,#370608,#370609,#370610,#370611,
#370612,#370613,#370614,#370615,#370616,#370617,#370618,#370619,#370620,
#370621,#370622),.UNSPECIFIED.,.F.,.F.,(4,2,2,2,2,2,2,2,2,2,2,4),(-0.370205279453778,
-0.350219365145943,-0.329577799848427,-0.293539528040863,-0.259747571198344,
-0.227982662210344,-0.199662873529425,-0.16494855267263,-0.124437197575316,
-0.0810928930749654,-0.0392683201053638,-9.99999999307111E-7),
 .UNSPECIFIED.);
#24708=B_SPLINE_CURVE_WITH_KNOTS('',3,(#370624,#370625,#370626,#370627,
#370628,#370629,#370630,#370631,#370632,#370633,#370634,#370635,#370636,
#370637,#370638,#370639,#370640,#370641,#370642,#370643,#370644,#370645,
#370646,#370647,#370648,#370649,#370650,#370651,#370652,#370653,#370654,
#370655,#370656,#370657,#370658,#370659,#370660),.UNSPECIFIED.,.F.,.F.,
(4,3,3,3,3,3,3,3,3,3,3,3,4),(2.99491710979115E-14,0.000108371923709533,
0.00021803673379923,0.000304842679092563,0.000415181043997034,0.000525308370927796,
0.000609685358155176,0.000711172109786132,0.000812850073501961,0.000914528037217789,
0.00102917412252272,0.00114325983251636,0.0012193707162804),
 .UNSPECIFIED.);
#24709=B_SPLINE_CURVE_WITH_KNOTS('',3,(#370673,#370674,#370675,#370676,
#370677,#370678,#370679,#370680,#370681,#370682),.UNSPECIFIED.,.F.,.F.,
(4,2,2,2,4),(-0.115181813240965,-0.083642902448367,-0.0518196847902682,
-0.0231633114822182,0.),.UNSPECIFIED.);
#24710=B_SPLINE_CURVE_WITH_KNOTS('',3,(#370683,#370684,#370685,#370686,
#370687,#370688,#370689,#370690,#370691,#370692),.UNSPECIFIED.,.F.,.F.,
(4,2,2,2,4),(-0.0961593141722214,-0.0719589549439694,-0.0481092230513157,
-0.0251497984388369,-1.00000015684776E-6),.UNSPECIFIED.);
#24711=B_SPLINE_CURVE_WITH_KNOTS('',3,(#372462,#372463,#372464,#372465,
#372466,#372467,#372468,#372469,#372470,#372471,#372472,#372473,#372474,
#372475,#372476,#372477,#372478,#372479,#372480,#372481),.UNSPECIFIED.,
 .F.,.F.,(4,2,2,2,2,2,2,2,2,4),(-0.472681567119335,-0.442142555193499,-0.38234022419326,
-0.324797632394375,-0.265317638921683,-0.206291871345753,-0.149316840539157,
-0.0896533162312005,-0.0440651229089899,-9.99999998696488E-7),
 .UNSPECIFIED.);
#24712=B_SPLINE_CURVE_WITH_KNOTS('',3,(#372489,#372490,#372491,#372492,
#372493,#372494,#372495,#372496,#372497,#372498,#372499,#372500,#372501,
#372502,#372503,#372504),.UNSPECIFIED.,.F.,.F.,(4,2,2,2,2,2,2,4),(-26.8667509318511,
-26.824104786793,-26.7812253116685,-26.722294429582,-26.6622259040102,-26.6047498917014,
-26.5450263135477,-26.510596166175),.UNSPECIFIED.);
#24713=B_SPLINE_CURVE_WITH_KNOTS('',3,(#372509,#372510,#372511,#372512,
#372513,#372514,#372515,#372516,#372517,#372518,#372519,#372520,#372521,
#372522,#372523,#372524,#372525,#372526,#372527,#372528,#372529,#372530,
#372531,#372532,#372533,#372534,#372535,#372536,#372537,#372538,#372539,
#372540,#372541,#372542,#372543,#372544),.UNSPECIFIED.,.F.,.F.,(4,2,2,2,
2,2,2,2,2,2,2,2,2,2,2,2,2,4),(-1.41871218540484,-1.37878681735941,-1.31927200836046,
-1.26198522748958,-1.20229853529282,-1.14356070615823,-1.08648876969871,
-1.02678193345692,-0.968695892866923,-0.91068951354503,-0.851032976951095,
-0.793620463744822,-0.733538162871584,-0.674675729532023,-0.617695493756087,
-0.558023751508197,-0.499810626571642,-0.472681567119335),.UNSPECIFIED.);
#24714=B_SPLINE_CURVE_WITH_KNOTS('',3,(#372545,#372546,#372547,#372548,
#372549,#372550,#372551,#372552,#372553,#372554,#372555,#372556,#372557,
#372558,#372559,#372560,#372561,#372562,#372563,#372564,#372565,#372566,
#372567,#372568,#372569,#372570,#372571,#372572,#372573,#372574,#372575,
#372576,#372577,#372578,#372579,#372580),.UNSPECIFIED.,.F.,.F.,(4,2,2,2,
2,2,2,2,2,2,2,2,2,2,2,2,2,4),(-26.510596166175,-26.4870074929446,-26.4288576683979,
-26.3691024203233,-26.3119929596958,-26.2531910582434,-26.1934547120385,
-26.1361066574089,-26.0765272079356,-26.0180256611724,-25.9599965037028,
-25.899659107618,-25.8423746572756,-25.7836709165709,-25.7239000681539,
-25.6667235836525,-25.6073748228045,-25.5633168472621),.UNSPECIFIED.);
#24715=B_SPLINE_CURVE_WITH_KNOTS('',3,(#372585,#372586,#372587,#372588,
#372589,#372590,#372591,#372592,#372593,#372594,#372595,#372596,#372597,
#372598,#372599,#372600,#372601,#372602,#372603,#372604,#372605,#372606,
#372607,#372608,#372609,#372610,#372611,#372612,#372613,#372614,#372615,
#372616,#372617,#372618,#372619,#372620),.UNSPECIFIED.,.F.,.F.,(4,2,2,2,
2,2,2,2,2,2,2,2,2,2,2,2,2,4),(-2.36518766847454,-2.31596416709828,-2.25687811886001,
-2.1998608458798,-2.14015848136392,-2.08171970311433,-2.02430530224587,
-1.96425483793624,-1.90648696306987,-1.84756358898257,-1.78827674448427,
-1.73115470781314,-1.671427658721,-1.6127856936622,-1.55552841531158,-1.49525585707669,
-1.43728761568309,-1.41871218540484),.UNSPECIFIED.);
#24716=B_SPLINE_CURVE_WITH_KNOTS('',3,(#372621,#372622,#372623,#372624,
#372625,#372626,#372627,#372628,#372629,#372630,#372631,#372632,#372633,
#372634,#372635,#372636,#372637,#372638,#372639,#372640,#372641,#372642,
#372643,#372644,#372645,#372646,#372647,#372648,#372649,#372650,#372651,
#372652,#372653,#372654,#372655,#372656),.UNSPECIFIED.,.F.,.F.,(4,2,2,2,
2,2,2,2,2,2,2,2,2,2,2,2,2,4),(-25.5633168472621,-25.5484622494425,-25.4906365280881,
-25.4305245287703,-25.3730935305106,-25.3145962757104,-25.2548533628906,
-25.1977921450971,-25.1386474249518,-25.079220496869,-25.0215682750396,
-24.9616493129352,-24.9039748678532,-24.8456516573957,-24.7859071065283,
-24.7288626191054,-24.6698897716537,-24.6165058202546),.UNSPECIFIED.);
#24717=B_SPLINE_CURVE_WITH_KNOTS('',3,(#372661,#372662,#372663,#372664,
#372665,#372666,#372667,#372668,#372669,#372670,#372671,#372672,#372673,
#372674,#372675,#372676,#372677,#372678,#372679,#372680,#372681,#372682,
#372683,#372684,#372685,#372686,#372687,#372688,#372689,#372690,#372691,
#372692,#372693,#372694,#372695,#372696),.UNSPECIFIED.,.F.,.F.,(4,2,2,2,
2,2,2,2,2,2,2,2,2,2,2,2,2,4),(-3.31153449026076,-3.25341108907696,-3.19462285744369,
-3.13753038095501,-3.07779156837013,-3.01965519836493,-2.96165742705592,
-2.90194724384513,-2.84448427844684,-2.78444151548969,-2.72552350666032,
-2.66851289666458,-2.60880592198192,-2.55053735406635,-2.49287018538501,
-2.43300891651653,-2.37541100753461,-2.36518766847454),.UNSPECIFIED.);
#24718=B_SPLINE_CURVE_WITH_KNOTS('',3,(#372697,#372698,#372699,#372700,
#372701,#372702,#372703,#372704,#372705,#372706,#372707,#372708,#372709,
#372710,#372711,#372712,#372713,#372714,#372715,#372716,#372717,#372718,
#372719,#372720,#372721,#372722,#372723,#372724,#372725,#372726,#372727,
#372728,#372729,#372730,#372731,#372732,#372733,#372734),.UNSPECIFIED.,
 .F.,.F.,(4,2,2,2,2,2,2,2,2,2,2,2,2,2,2,2,2,2,4),(-24.6165058202546,-24.6098725741468,
-24.5523592800399,-24.4925957429875,-24.4345974342447,-24.3764107212499,
-24.316637102574,-24.2595192853478,-24.2006805602332,-24.1409243580283,
-24.0835417301909,-24.0239252260488,-23.9654580555157,-23.9073951002302,
-23.8470208311425,-23.789739831929,-23.7310017078749,-23.6712177426758,
-23.6690063317509),.UNSPECIFIED.);
#24719=B_SPLINE_CURVE_WITH_KNOTS('',3,(#372739,#372740,#372741,#372742,
#372743,#372744,#372745,#372746,#372747,#372748,#372749,#372750,#372751,
#372752,#372753,#372754,#372755,#372756,#372757,#372758,#372759,#372760,
#372761,#372762,#372763,#372764,#372765,#372766,#372767,#372768,#372769,
#372770,#372771,#372772,#372773,#372774,#372775,#372776),.UNSPECIFIED.,
 .F.,.F.,(4,2,2,2,2,2,2,2,2,2,2,2,2,2,2,2,2,2,4),(-4.25857656298863,-4.2514694638124,
-4.19174418285107,-4.13326131706642,-4.0758506244679,-4.01575319141907,
-3.95794168972433,-3.89905419814863,-3.83971964604971,-3.78255757670404,
-3.72280387132181,-3.66411410258304,-3.60684827544134,-3.54652503551378,
-3.48850971369039,-3.43003130272675,-3.37046574183593,-3.31313120077023,
-3.31153449026076),.UNSPECIFIED.);
#24720=B_SPLINE_CURVE_WITH_KNOTS('',3,(#372777,#372778,#372779,#372780,
#372781,#372782,#372783,#372784,#372785,#372786,#372787,#372788,#372789,
#372790,#372791,#372792,#372793,#372794,#372795,#372796,#372797,#372798,
#372799,#372800,#372801,#372802,#372803,#372804,#372805,#372806,#372807,
#372808,#372809,#372810,#372811,#372812),.UNSPECIFIED.,.F.,.F.,(4,2,2,2,
2,2,2,2,2,2,2,2,2,2,2,2,2,4),(-23.6690063317509,-23.6140133906547,-23.5546305007402,
-23.4957660462814,-23.4379098683801,-23.3777645802384,-23.320349365966,
-23.2618213189778,-23.2020690471691,-23.144991918597,-23.085816594075,-23.0264489632798,
-22.9687701730377,-22.9088221435739,-22.8511745951465,-22.792824818853,
-22.7330743558813,-22.7219983497172),.UNSPECIFIED.);
#24721=B_SPLINE_CURVE_WITH_KNOTS('',3,(#372817,#372818,#372819,#372820,
#372821,#372822,#372823,#372824,#372825,#372826,#372827,#372828,#372829,
#372830,#372831,#372832,#372833,#372834,#372835,#372836,#372837,#372838,
#372839,#372840,#372841,#372842,#372843,#372844,#372845,#372846,#372847,
#372848,#372849,#372850,#372851,#372852),.UNSPECIFIED.,.F.,.F.,(4,2,2,2,
2,2,2,2,2,2,2,2,2,2,2,2,2,4),(-5.2051363729884,-5.189395380046,-5.12964028728551,
-5.07146907437671,-5.01349379691273,-4.95374592874799,-4.89624787076232,
-4.83625851640013,-4.77730079908221,-4.72027382656529,-4.66054736488245,
-4.60223905529108,-4.54458645660951,-4.48468256608512,-4.427045030502,-4.36764481083087,
-4.30851470872145,-4.25857656298863),.UNSPECIFIED.);
#24722=B_SPLINE_CURVE_WITH_KNOTS('',3,(#372853,#372854,#372855,#372856,
#372857,#372858,#372859,#372860,#372861,#372862,#372863,#372864,#372865,
#372866,#372867,#372868,#372869,#372870,#372871,#372872,#372873,#372874,
#372875,#372876,#372877,#372878,#372879,#372880,#372881,#372882,#372883,
#372884,#372885,#372886,#372887,#372888),.UNSPECIFIED.,.F.,.F.,(4,2,2,2,
2,2,2,2,2,2,2,2,2,2,2,2,2,4),(-22.7219983497172,-22.676025638359,-22.6170264062843,
-22.5570758550377,-22.4995404278066,-22.4397526520792,-22.3817895352109,
-22.3235810572964,-22.2638047492202,-22.2066928005975,-22.1478325402814,
-22.0880720923164,-22.0306697641681,-21.9710316316543,-21.9126136704354,
-21.8545319204267,-21.7941363419943,-21.774643414205),.UNSPECIFIED.);
#24723=B_SPLINE_CURVE_WITH_KNOTS('',3,(#372893,#372894,#372895,#372896,
#372897,#372898,#372899,#372900,#372901,#372902,#372903,#372904,#372905,
#372906,#372907,#372908,#372909,#372910,#372911,#372912,#372913,#372914,
#372915,#372916,#372917,#372918,#372919,#372920,#372921,#372922,#372923,
#372924,#372925,#372926,#372927,#372928),.UNSPECIFIED.,.F.,.F.,(4,2,2,2,
2,2,2,2,2,2,2,2,2,2,2,2,2,4),(-6.1523798421435,-6.12797812550971,-6.0678494908681,
-6.01000954370658,-5.95117211963111,-5.89180550891634,-5.83461743202877,
-5.77485269586351,-5.71613058941083,-5.65887008025812,-5.59851207052264,
-5.54046497563872,-5.48202283843936,-5.4224223083538,-5.36505520297181,
-5.30531731824665,-5.24649433002998,-5.2051363729884),.UNSPECIFIED.);
#24724=B_SPLINE_CURVE_WITH_KNOTS('',3,(#372929,#372930,#372931,#372932,
#372933,#372934,#372935,#372936,#372937,#372938,#372939,#372940,#372941,
#372942,#372943,#372944,#372945,#372946,#372947,#372948,#372949,#372950,
#372951,#372952,#372953,#372954,#372955,#372956,#372957,#372958,#372959,
#372960,#372961,#372962,#372963,#372964),.UNSPECIFIED.,.F.,.F.,(4,2,2,2,
2,2,2,2,2,2,2,2,2,2,2,2,2,4),(-21.774643414205,-21.7368730308334,-21.6781156789626,
-21.6183343079821,-21.5611159054543,-21.5017142341325,-21.4429132756257,
-21.3850415803725,-21.3248784884646,-21.2674936111313,-21.2089498534046,
-21.149204030924,-21.092124905939,-21.0329342450041,-20.9736420131981,-20.9159515399632,
-20.8559898647572,-20.8275345885065),.UNSPECIFIED.);
#24725=B_SPLINE_CURVE_WITH_KNOTS('',3,(#372969,#372970,#372971,#372972,
#372973,#372974,#372975,#372976,#372977,#372978,#372979,#372980,#372981,
#372982,#372983,#372984,#372985,#372986,#372987,#372988,#372989,#372990,
#372991,#372992,#372993,#372994,#372995,#372996,#372997,#372998,#372999,
#373000,#373001,#373002,#373003,#373004),.UNSPECIFIED.,.F.,.F.,(4,2,2,2,
2,2,2,2,2,2,2,2,2,2,2,2,2,4),(-7.09901119411086,-7.06567228001258,-7.00590223384986,
-6.94838403007552,-6.88846344256541,-6.82948138012582,-6.77245205477943,
-6.71272178020251,-6.65438892106381,-6.59676515840048,-6.53683427285854,
-6.47917216681261,-6.41983327135308,-6.36067461928401,-6.30361531883792,
-6.24388277166941,-6.18537114395674,-6.1523798421435),.UNSPECIFIED.);
#24726=B_SPLINE_CURVE_WITH_KNOTS('',3,(#373005,#373006,#373007,#373008,
#373009,#373010,#373011,#373012,#373013,#373014,#373015,#373016,#373017,
#373018,#373019,#373020,#373021,#373022,#373023,#373024,#373025,#373026,
#373027,#373028,#373029,#373030,#373031,#373032,#373033,#373034,#373035,
#373036,#373037,#373038,#373039,#373040),.UNSPECIFIED.,.F.,.F.,(4,2,2,2,
2,2,2,2,2,2,2,2,2,2,2,2,2,4),(-20.8275345885065,-20.7983841401464,-20.7400228228779,
-20.680282347261,-20.6232436137976,-20.5642332011706,-20.5043661995887,
-20.4468234957869,-20.3870268705767,-20.3291145956587,-20.2708993561363,
-20.2111363425319,-20.154044915108,-20.0951782972609,-20.0354294865687,
-19.9780222496325,-19.9183778042751,-19.8805406314171),.UNSPECIFIED.);
#24727=B_SPLINE_CURVE_WITH_KNOTS('',3,(#373045,#373046,#373047,#373048,
#373049,#373050,#373051,#373052,#373053,#373054,#373055,#373056,#373057,
#373058,#373059,#373060,#373061,#373062,#373063,#373064,#373065,#373066,
#373067,#373068,#373069,#373070,#373071,#373072,#373073,#373074,#373075,
#373076,#373077,#373078,#373079,#373080),.UNSPECIFIED.,.F.,.F.,(4,2,2,2,
2,2,2,2,2,2,2,2,2,2,2,2,2,4),(-8.04621999375094,-8.00339153938214,-7.94400818753495,
-7.88680789834694,-7.82704787254924,-7.76830855204655,-7.71106766615472,
-7.65069041300283,-7.59262651715672,-7.53423564470816,-7.47461553332632,
-7.41723070274837,-7.35749066635497,-7.29864817158818,-7.24155700962402,
-7.18180133260471,-7.12361036089949,-7.09901119411086),.UNSPECIFIED.);
#24728=B_SPLINE_CURVE_WITH_KNOTS('',3,(#373081,#373082,#373083,#373084,
#373085,#373086,#373087,#373088,#373089,#373090,#373091,#373092,#373093,
#373094,#373095,#373096,#373097,#373098,#373099,#373100,#373101,#373102,
#373103,#373104,#373105,#373106,#373107,#373108,#373109,#373110,#373111,
#373112,#373113,#373114,#373115,#373116),.UNSPECIFIED.,.F.,.F.,(4,2,2,2,
2,2,2,2,2,2,2,2,2,2,2,2,2,4),(-19.8805406314171,-19.8600252528234,-19.8019396512075,
-19.7415382248585,-19.6843075087862,-19.6255460191888,-19.5657833749241,
-19.5085647062022,-19.4491595516306,-19.3904391548914,-19.3325668916662,
-19.2724014527642,-19.2150624092272,-19.156518030977,-19.0967949805335,
-19.0397279879862,-18.9805372818409,-18.9335464702939),.UNSPECIFIED.);
#24729=B_SPLINE_CURVE_WITH_KNOTS('',3,(#373121,#373122,#373123,#373124,
#373125,#373126,#373127,#373128,#373129,#373130,#373131,#373132,#373133,
#373134,#373135,#373136,#373137,#373138,#373139,#373140,#373141,#373142,
#373143,#373144,#373145,#373146,#373147,#373148,#373149,#373150,#373151,
#373152,#373153,#373154,#373155,#373156),.UNSPECIFIED.,.F.,.F.,(4,2,2,2,
2,2,2,2,2,2,2,2,2,2,2,2,2,4),(-8.99270588822923,-8.94052710995247,-8.88153589757056,
-8.82451847670245,-8.76480034119745,-8.70645794702851,-8.64887805663563,
-8.58893558193575,-8.53126377998128,-8.47200254273577,-8.41283058825612,
-8.35577115681652,-8.29604719351854,-8.23752186338507,-8.18016117488032,
-8.12001679633652,-8.06216332125115,-8.04621999375094),.UNSPECIFIED.);
#24730=B_SPLINE_CURVE_WITH_KNOTS('',3,(#373157,#373158,#373159,#373160,
#373161,#373162,#373163,#373164,#373165,#373166,#373167,#373168,#373169,
#373170,#373171,#373172,#373173,#373174,#373175,#373176,#373177,#373178,
#373179,#373180,#373181,#373182,#373183,#373184,#373185,#373186,#373187,
#373188,#373189,#373190,#373191,#373192),.UNSPECIFIED.,.F.,.F.,(4,2,2,2,
2,2,2,2,2,2,2,2,2,2,2,2,2,4),(-18.9335464702939,-18.9213385289384,-18.8636513496498,
-18.8036915093517,-18.7461437979602,-18.6877860607051,-18.6280720722102,
-18.571058014142,-18.5120517347588,-18.4522873912988,-18.3947524521812,
-18.3349625266769,-18.2771181850067,-18.2189113839145,-18.1591783284847,
-18.1021228024093,-18.0432652150961,-17.9871364878283),.UNSPECIFIED.);
#24731=B_SPLINE_CURVE_WITH_KNOTS('',3,(#373197,#373198,#373199,#373200,
#373201,#373202,#373203,#373204,#373205,#373206,#373207,#373208,#373209,
#373210,#373211,#373212,#373213,#373214,#373215,#373216,#373217,#373218,
#373219,#373220,#373221,#373222,#373223,#373224,#373225,#373226,#373227,
#373228,#373229,#373230,#373231,#373232,#373233,#373234),.UNSPECIFIED.,
 .F.,.F.,(4,2,2,2,2,2,2,2,2,2,2,2,2,2,2,2,2,2,4),(-9.93964057167184,-9.93859371440356,
-9.87885461052393,-9.82011317594689,-9.76290692726508,-9.70252589737089,
-9.64446015422855,-9.58613695209657,-9.52651257914626,-9.46912482257077,
-9.40939857554009,-9.35055175623928,-9.29348310865754,-9.23374289372987,
-9.17554716939251,-9.11766209798999,-9.05788526054439,-9.0003617689204,
-8.99270588822923),.UNSPECIFIED.);
#24732=B_SPLINE_CURVE_WITH_KNOTS('',3,(#373235,#373236,#373237,#373238,
#373239,#373240,#373241,#373242,#373243,#373244,#373245,#373246,#373247,
#373248,#373249,#373250,#373251,#373252,#373253,#373254,#373255,#373256,
#373257,#373258,#373259,#373260,#373261,#373262,#373263,#373264,#373265,
#373266,#373267,#373268,#373269,#373270,#373271,#373272),.UNSPECIFIED.,
 .F.,.F.,(4,2,2,2,2,2,2,2,2,2,2,2,2,2,2,2,2,2,4),(-17.9871364878283,-17.9835445667985,
-17.9261474434672,-17.8665122096331,-17.8082430505961,-17.7501687941794,
-17.6897771981761,-17.6325949724155,-17.573844684739,-17.5141177124938,
-17.4569127452413,-17.3975196787185,-17.3388990838463,-17.2810415304577,
-17.220889495943,-17.1636130941139,-17.1050835132873,-17.0454004826462,
-17.0404914447298),.UNSPECIFIED.);
#24733=B_SPLINE_CURVE_WITH_KNOTS('',3,(#373277,#373278,#373279,#373280,
#373281,#373282,#373283,#373284,#373285,#373286,#373287,#373288,#373289,
#373290,#373291,#373292,#373293,#373294,#373295,#373296,#373297,#373298,
#373299,#373300,#373301,#373302,#373303,#373304,#373305,#373306,#373307,
#373308,#373309,#373310,#373311,#373312),.UNSPECIFIED.,.F.,.F.,(4,2,2,2,
2,2,2,2,2,2,2,2,2,2,2,2,2,4),(-10.8858166820195,-10.8759296830837,-10.8162402914887,
-10.7579035150976,-10.700383897791,-10.6404453416983,-10.5827788519651,
-10.5236136488423,-10.4644437054219,-10.4073983139873,-10.3476993498427,
-10.2891754274228,-10.2318627119956,-10.1717180615585,-10.1138660280208,
-10.0551772063632,-9.99579242400764,-9.93964057167184),.UNSPECIFIED.);
#24734=B_SPLINE_CURVE_WITH_KNOTS('',3,(#373313,#373314,#373315,#373316,
#373317,#373318,#373319,#373320,#373321,#373322,#373323,#373324,#373325,
#373326,#373327,#373328,#373329,#373330,#373331,#373332,#373333,#373334,
#373335,#373336,#373337,#373338,#373339,#373340,#373341,#373342,#373343,
#373344,#373345,#373346,#373347,#373348),.UNSPECIFIED.,.F.,.F.,(4,2,2,2,
2,2,2,2,2,2,2,2,2,2,2,2,2,4),(-17.0404914447298,-16.9883602116983,-16.9291851008246,
-16.8701004552366,-16.812431962457,-16.7524898253569,-16.6950180268766,
-16.6366794116705,-16.5770094388777,-16.5200355200857,-16.4610491286714,
-16.4014094152831,-16.343897799262,-16.2841306201495,-16.2263732495688,
-16.1681906180146,-16.108505308808,-16.0948122175984),.UNSPECIFIED.);
#24735=B_SPLINE_CURVE_WITH_KNOTS('',3,(#373353,#373354,#373355,#373356,
#373357,#373358,#373359,#373360,#373361,#373362,#373363,#373364,#373365,
#373366,#373367,#373368,#373369,#373370,#373371,#373372,#373373,#373374,
#373375,#373376,#373377,#373378,#373379,#373380,#373381,#373382,#373383,
#373384,#373385,#373386,#373387,#373388),.UNSPECIFIED.,.F.,.F.,(4,2,2,2,
2,2,2,2,2,2,2,2,2,2,2,2,2,4),(-11.832087351168,-11.8138339556462,-11.7534648756654,
-11.6954125353176,-11.6371752570596,-11.5775621943317,-11.5201865842648,
-11.4604907625775,-11.4016550546539,-11.3446244188633,-11.284916446333,
-11.2267312150998,-11.16891646552,-11.1091484269857,-11.051634732786,-10.9919054425779,
-10.9329204280484,-10.8858166820195),.UNSPECIFIED.);
#24736=B_SPLINE_CURVE_WITH_KNOTS('',3,(#373389,#373390,#373391,#373392,
#373393,#373394,#373395,#373396,#373397,#373398,#373399,#373400,#373401,
#373402,#373403,#373404,#373405,#373406,#373407,#373408,#373409,#373410,
#373411,#373412,#373413,#373414,#373415,#373416,#373417,#373418,#373419,
#373420,#373421,#373422,#373423,#373424),.UNSPECIFIED.,.F.,.F.,(4,2,2,2,
2,2,2,2,2,2,2,2,2,2,2,2,2,4),(-16.0948122175984,-16.0515021496427,-15.9926695313415,
-15.9324153923589,-15.8750239845731,-15.8153918569545,-15.7572809932452,
-15.6992146839251,-15.6394874422163,-15.5823727082596,-15.5236537869628,
-15.463949466107,-15.4066780911298,-15.3471815689713,-15.2885473168338,
-15.2305919148884,-15.1703361945366,-15.1482252818032),.UNSPECIFIED.);
#24737=B_SPLINE_CURVE_WITH_KNOTS('',3,(#373429,#373430,#373431,#373432,
#373433,#373434,#373435,#373436,#373437,#373438,#373439,#373440,#373441,
#373442,#373443,#373444,#373445,#373446,#373447,#373448,#373449,#373450,
#373451,#373452,#373453,#373454,#373455,#373456,#373457,#373458,#373459,
#373460,#373461,#373462,#373463,#373464),.UNSPECIFIED.,.F.,.F.,(4,2,2,2,
2,2,2,2,2,2,2,2,2,2,2,2,2,4),(-12.7778456201867,-12.7507159363548,-12.6907972398182,
-12.63315153128,-12.5741033789915,-12.5149511544153,-12.457934468101,-12.3982779039036,
-12.3397708709816,-12.2825231389776,-12.2223940274391,-12.164558777205,
-12.1059724860861,-12.0466019010626,-11.9894187744342,-11.9297176737972,
-11.8709895175493,-11.832087351168),.UNSPECIFIED.);
#24738=B_SPLINE_CURVE_WITH_KNOTS('',3,(#373465,#373466,#373467,#373468,
#373469,#373470,#373471,#373472,#373473,#373474,#373475,#373476,#373477,
#373478,#373479,#373480,#373481,#373482,#373483,#373484,#373485,#373486,
#373487,#373488,#373489,#373490,#373491,#373492,#373493,#373494,#373495,
#373496,#373497,#373498,#373499,#373500),.UNSPECIFIED.,.F.,.F.,(4,2,2,2,
2,2,2,2,2,2,2,2,2,2,2,2,2,4),(-15.1482252818032,-15.113010827952,-15.0543821418657,
-14.9946236313547,-14.9374980414962,-14.87822340049,-14.8191393023084,-14.7593854651451,
-14.7011228135253,-14.6433226319139,-14.583472042581,-14.5258810193432,
-14.4662175738346,-14.4071474015193,-14.3501042723806,-14.2903635975994,
-14.2319417973738,-14.2013196209283),.UNSPECIFIED.);
#24739=B_SPLINE_CURVE_WITH_KNOTS('',3,(#373505,#373506,#373507,#373508,
#373509,#373510,#373511,#373512,#373513,#373514,#373515,#373516,#373517,
#373518,#373519,#373520,#373521,#373522,#373523,#373524,#373525,#373526,
#373527,#373528,#373529,#373530,#373531,#373532,#373533,#373534,#373535,
#373536,#373537,#373538,#373539,#373540),.UNSPECIFIED.,.F.,.F.,(4,2,2,2,
2,2,2,2,2,2,2,2,2,2,2,2,2,4),(-13.7232155909417,-13.6873757907163,-13.6277684747862,
-13.5704011152273,-13.5101862567796,-13.4513776947496,-13.3944017068863,
-13.3347439479979,-13.2765850339693,-13.2188599447086,-13.1591168402254,
-13.1016285928867,-13.0420270820403,-12.9830641004007,-12.926115617869,
-12.8664726675182,-12.8081571280792,-12.7778456201867),.UNSPECIFIED.);
#24740=B_SPLINE_CURVE_WITH_KNOTS('',3,(#373541,#373542,#373543,#373544,
#373545,#373546,#373547,#373548,#373549,#373550,#373551,#373552,#373553,
#373554,#373555,#373556,#373557,#373558,#373559,#373560,#373561,#373562,
#373563,#373564,#373565,#373566,#373567,#373568,#373569,#373570,#373571,
#373572,#373573,#373574,#373575,#373576),.UNSPECIFIED.,.F.,.F.,(4,2,2,2,
2,2,2,2,2,2,2,2,2,2,2,2,2,4),(-14.2013196209283,-14.1744209827898,-14.1143922449389,
-14.056641417422,-13.9975274962971,-13.9382658377259,-13.881148369121,-13.8213922549119,
-13.7627766957579,-13.7054437170459,-13.6452022732368,-13.5872597923407,
-13.5286021059723,-13.4691201312833,-13.4118301565226,-13.3520274598016,
-13.2931887753002,-13.2539690630572),.UNSPECIFIED.);
#24741=B_SPLINE_CURVE_WITH_KNOTS('',3,(#373581,#373582,#373583,#373584,
#373585,#373586,#373587,#373588,#373589,#373590,#373591,#373592,#373593,
#373594,#373595,#373596,#373597,#373598,#373599,#373600,#373601,#373602,
#373603,#373604,#373605,#373606,#373607,#373608,#373609,#373610,#373611,
#373612,#373613,#373614,#373615,#373616),.UNSPECIFIED.,.F.,.F.,(4,2,2,2,
2,2,2,2,2,2,2,2,2,2,2,2,2,4),(-14.6697112969214,-14.6241050026354,-14.5648559098276,
-14.5077561722265,-14.4480265312735,-14.3894230310587,-14.332128195858,
-14.2718981321671,-14.2139676440574,-14.1553691716209,-14.095897854982,
-14.038650897544,-13.9789744407945,-13.9202803244159,-13.8631942070711,
-13.8034950271421,-13.7454531716399,-13.7232155909417),.UNSPECIFIED.);
#24742=B_SPLINE_CURVE_WITH_KNOTS('',3,(#373617,#373618,#373619,#373620,
#373621,#373622,#373623,#373624,#373625,#373626,#373627,#373628,#373629,
#373630,#373631,#373632,#373633,#373634,#373635,#373636,#373637,#373638,
#373639,#373640,#373641,#373642,#373643,#373644,#373645,#373646,#373647,
#373648,#373649,#373650,#373651,#373652),.UNSPECIFIED.,.F.,.F.,(4,2,2,2,
2,2,2,2,2,2,2,2,2,2,2,2,2,4),(-13.2539690630572,-13.2359418394137,-13.176082960855,
-13.1178984829625,-13.0596379491205,-12.9998855188218,-12.9423777451317,
-12.8819525589879,-12.8230027330433,-12.765872417961,-12.7060572753572,
-12.6477589855018,-12.5898562582822,-12.5299712805315,-12.4723456099784,
-12.4125388540839,-12.3534374372755,-12.3060149682094),.UNSPECIFIED.);
#24743=B_SPLINE_CURVE_WITH_KNOTS('',3,(#373657,#373658,#373659,#373660,
#373661,#373662,#373663,#373664,#373665,#373666,#373667,#373668,#373669,
#373670,#373671,#373672,#373673,#373674,#373675,#373676,#373677,#373678,
#373679,#373680,#373681,#373682,#373683,#373684,#373685,#373686,#373687,
#373688,#373689,#373690,#373691,#373692),.UNSPECIFIED.,.F.,.F.,(4,2,2,2,
2,2,2,2,2,2,2,2,2,2,2,2,2,4),(-15.6160643869164,-15.5633841295623,-15.50414397945,
-15.4450746347767,-15.3873455777041,-15.3273390514912,-15.2698532500883,
-15.2114535121035,-15.1517412598184,-15.0947244496642,-15.0356767186234,
-14.9760606921884,-14.9184924702182,-14.8586652119684,-14.8009028783926,
-14.7408878749948,-14.6831512235933,-14.6697112969214),.UNSPECIFIED.);
#24744=B_SPLINE_CURVE_WITH_KNOTS('',3,(#373693,#373694,#373695,#373696,
#373697,#373698,#373699,#373700,#373701,#373702,#373703,#373704,#373705,
#373706,#373707,#373708,#373709,#373710,#373711,#373712,#373713,#373714,
#373715,#373716,#373717,#373718,#373719,#373720,#373721,#373722,#373723,
#373724,#373725,#373726,#373727,#373728),.UNSPECIFIED.,.F.,.F.,(4,2,2,2,
2,2,2,2,2,2,2,2,2,2,2,2,2,4),(-12.3060149682094,-12.2963423900386,-12.2365444281595,
-12.1780923177588,-12.1204810997582,-12.060423290409,-12.002642705299,-11.9433971991263,
-11.8841087980352,-11.8269538089724,-11.7671447134874,-11.7085033852916,
-11.6510943928729,-11.5908283874767,-11.5328603255245,-11.4740867043324,
-11.4145816503773,-11.3580906752407),.UNSPECIFIED.);
#24745=B_SPLINE_CURVE_WITH_KNOTS('',3,(#373733,#373734,#373735,#373736,
#373737,#373738,#373739,#373740,#373741,#373742,#373743,#373744,#373745,
#373746,#373747,#373748,#373749,#373750,#373751,#373752,#373753,#373754,
#373755,#373756,#373757,#373758,#373759,#373760,#373761,#373762,#373763,
#373764,#373765,#373766,#373767,#373768,#373769,#373770),.UNSPECIFIED.,
 .F.,.F.,(4,2,2,2,2,2,2,2,2,2,2,2,2,2,2,2,2,2,4),(-16.5634944095663,-16.558847104806,
-16.5013588527821,-16.4416263782018,-16.3834028937152,-16.3252384039002,
-16.2654055499546,-16.2081869526806,-16.1493686256731,-16.0895923551828,
-16.0323225157354,-15.9728613083516,-15.9142445390969,-15.8563229646398,
-15.7961028021386,-15.7388015559079,-15.6802071166945,-15.6204784650606,
-15.6160643869164),.UNSPECIFIED.);
#24746=B_SPLINE_CURVE_WITH_KNOTS('',3,(#373771,#373772,#373773,#373774,
#373775,#373776,#373777,#373778,#373779,#373780,#373781,#373782,#373783,
#373784,#373785,#373786,#373787,#373788,#373789,#373790,#373791,#373792,
#373793,#373794,#373795,#373796,#373797,#373798,#373799,#373800,#373801,
#373802,#373803,#373804,#373805,#373806,#373807,#373808),.UNSPECIFIED.,
 .F.,.F.,(4,2,2,2,2,2,2,2,2,2,2,2,2,2,2,2,2,2,4),(-11.3580906752407,-11.3572679784,
-11.2974169823782,-11.2385562886582,-11.1812485195102,-11.1207442499487,
-11.0625607234322,-11.0041471616058,-10.9444008964664,-10.8868963018946,
-10.8270552846813,-10.7680881341343,-10.7109133691843,-10.6510590470825,
-10.5927441318147,-10.5347636363483,-10.4748636050938,-10.4172220728686,
-10.4093537637416),.UNSPECIFIED.);
#24747=B_SPLINE_CURVE_WITH_KNOTS('',3,(#373813,#373814,#373815,#373816,
#373817,#373818,#373819,#373820,#373821,#373822,#373823,#373824,#373825,
#373826,#373827,#373828,#373829,#373830,#373831,#373832,#373833,#373834,
#373835,#373836,#373837,#373838,#373839,#373840,#373841,#373842,#373843,
#373844,#373845,#373846,#373847,#373848),.UNSPECIFIED.,.F.,.F.,(4,2,2,2,
2,2,2,2,2,2,2,2,2,2,2,2,2,4),(-17.5108474815656,-17.4981824073433,-17.4404188094185,
-17.3803782022338,-17.3227989832027,-17.264364113181,-17.2045902413959,
-17.1475176485416,-17.0884338098363,-17.0286723787512,-16.971064882126,
-16.9111983964038,-16.8533306609307,-16.7950509066526,-16.7352608424757,
-16.6781562232155,-16.6192252795436,-16.5634944095663),.UNSPECIFIED.);
#24748=B_SPLINE_CURVE_WITH_KNOTS('',3,(#373849,#373850,#373851,#373852,
#373853,#373854,#373855,#373856,#373857,#373858,#373859,#373860,#373861,
#373862,#373863,#373864,#373865,#373866,#373867,#373868,#373869,#373870,
#373871,#373872,#373873,#373874,#373875,#373876,#373877,#373878,#373879,
#373880,#373881,#373882,#373883,#373884),.UNSPECIFIED.,.F.,.F.,(4,2,2,2,
2,2,2,2,2,2,2,2,2,2,2,2,2,4),(-10.4093537637416,-10.357301350092,-10.2981875964388,
-10.2410598266438,-10.1812262852967,-10.1227625009788,-10.0650840056295,
-10.0050160951117,-9.94722420042477,-9.88787458177181,-9.8285780775151,
-9.77140334689103,-9.71156252645465,-9.65291378504466,-9.59545024275255,
-9.53517837450292,-9.47720292034625,-9.46102060630963),.UNSPECIFIED.);
#24749=B_SPLINE_CURVE_WITH_KNOTS('',3,(#373889,#373890,#373891,#373892,
#373893,#373894,#373895,#373896,#373897,#373898,#373899,#373900,#373901,
#373902,#373903,#373904,#373905,#373906,#373907,#373908,#373909,#373910,
#373911,#373912,#373913,#373914,#373915,#373916,#373917,#373918,#373919,
#373920,#373921,#373922,#373923,#373924),.UNSPECIFIED.,.F.,.F.,(4,2,2,2,
2,2,2,2,2,2,2,2,2,2,2,2,2,4),(-18.4588843632361,-18.4379249591453,-18.3797565748226,
-18.3192675325481,-18.2619844588132,-18.2031390102249,-18.1433099118157,
-18.08601177282,-18.0265223329137,-17.9677872345947,-17.9098351539592,-17.8495852647835,
-17.7922047206241,-17.7335795360629,-17.6737934777643,-17.6166574153344,
-17.5573855039092,-17.5108474815656),.UNSPECIFIED.);
#24750=B_SPLINE_CURVE_WITH_KNOTS('',3,(#373925,#373926,#373927,#373928,
#373929,#373930,#373931,#373932,#373933,#373934,#373935,#373936,#373937,
#373938,#373939,#373940,#373941,#373942,#373943,#373944,#373945,#373946,
#373947,#373948,#373949,#373950,#373951,#373952,#373953,#373954,#373955,
#373956,#373957,#373958,#373959,#373960),.UNSPECIFIED.,.F.,.F.,(4,2,2,2,
2,2,2,2,2,2,2,2,2,2,2,2,2,4),(-9.46102060630963,-9.41833880180209,-9.3588291150787,
-9.30150841089207,-9.24162988543094,-9.1827653326874,-9.12541671025634,
-9.06491011306255,-9.00672251636901,-8.94823424111932,-8.88848619394602,
-8.83097867682595,-8.77111742934779,-8.71214861344168,-8.65494532622163,
-8.59506904630521,-8.53675296718138,-8.51191438852878),.UNSPECIFIED.);
#24751=B_SPLINE_CURVE_WITH_KNOTS('',3,(#373965,#373966,#373967,#373968,
#373969,#373970,#373971,#373972,#373973,#373974,#373975,#373976,#373977,
#373978,#373979,#373980,#373981,#373982,#373983,#373984,#373985,#373986,
#373987,#373988,#373989,#373990,#373991,#373992,#373993,#373994,#373995,
#373996,#373997,#373998,#373999,#374000),.UNSPECIFIED.,.F.,.F.,(4,2,2,2,
2,2,2,2,2,2,2,2,2,2,2,2,2,4),(-19.4070183691008,-19.3774063864679,-19.3189557693523,
-19.2591417053657,-19.2020323274699,-19.1429320225021,-19.0830507906155,
-19.0254233516887,-18.965537605045,-18.9075870649366,-18.8492865591321,
-18.7894526316521,-18.7322992275162,-18.6733467783119,-18.6135256785197,
-18.5560357625839,-18.4963044063323,-18.4588843632361),.UNSPECIFIED.);
#24752=B_SPLINE_CURVE_WITH_KNOTS('',3,(#374001,#374002,#374003,#374004,
#374005,#374006,#374007,#374008,#374009,#374010,#374011,#374012,#374013,
#374014,#374015,#374016,#374017,#374018,#374019,#374020,#374021,#374022,
#374023,#374024,#374025,#374026,#374027,#374028,#374029,#374030,#374031,
#374032,#374033,#374034,#374035,#374036),.UNSPECIFIED.,.F.,.F.,(4,2,2,2,
2,2,2,2,2,2,2,2,2,2,2,2,2,4),(-8.51191438852878,-8.4787127733909,-8.41881348215695,
-8.36117138372012,-8.30115724125843,-8.24204667981905,-8.18490127059537,
-8.12504915972689,-8.06658902788,-8.00886034197012,-7.94879799919023,-7.89100997426156,
-7.83157560792974,-7.77228645996014,-7.71510635148775,-7.65525058713637,
-7.59660968033924,-7.56334284916346),.UNSPECIFIED.);
#24753=B_SPLINE_CURVE_WITH_KNOTS('',3,(#374041,#374042,#374043,#374044,
#374045,#374046,#374047,#374048,#374049,#374050,#374051,#374052,#374053,
#374054,#374055,#374056,#374057,#374058,#374059,#374060,#374061,#374062,
#374063,#374064,#374065,#374066,#374067,#374068,#374069,#374070,#374071,
#374072,#374073,#374074,#374075,#374076),.UNSPECIFIED.,.F.,.F.,(4,2,2,2,
2,2,2,2,2,2,2,2,2,2,2,2,2,4),(-20.3553623627869,-20.3171217343121,-20.2582684118752,
-20.1984073311347,-20.1410985076455,-20.0816003588123,-20.0227696675249,
-19.9648061934378,-19.9045463176452,-19.8471067919944,-19.7884701564408,
-19.7286478374059,-19.6714882098823,-19.6122040986311,-19.5528914181738,
-19.4951124766427,-19.4350576110104,-19.4070183691008),.UNSPECIFIED.);
#24754=B_SPLINE_CURVE_WITH_KNOTS('',3,(#374077,#374078,#374079,#374080,
#374081,#374082,#374083,#374084,#374085,#374086,#374087,#374088,#374089,
#374090,#374091,#374092,#374093,#374094,#374095,#374096,#374097,#374098,
#374099,#374100,#374101,#374102,#374103,#374104,#374105,#374106,#374107,
#374108,#374109,#374110,#374111,#374112),.UNSPECIFIED.,.F.,.F.,(4,2,2,2,
2,2,2,2,2,2,2,2,2,2,2,2,2,4),(-7.56334284916346,-7.53910774863586,-7.47884561490593,
-7.42087787571869,-7.3619414253141,-7.3024425331232,-7.2451286750284,-7.18523915485486,
-7.12638595068181,-7.06901188301772,-7.00851852031134,-6.95034191610438,
-6.89179603136193,-6.83206161385348,-6.77456607327972,-6.71470079446401,
-6.65574558736659,-6.61411156553163),.UNSPECIFIED.);
#24755=B_SPLINE_CURVE_WITH_KNOTS('',3,(#374117,#374118,#374119,#374120,
#374121,#374122,#374123,#374124,#374125,#374126,#374127,#374128,#374129,
#374130,#374131,#374132,#374133,#374134,#374135,#374136,#374137,#374138,
#374139,#374140,#374141,#374142,#374143,#374144,#374145,#374146,#374147,
#374148,#374149,#374150,#374151,#374152),.UNSPECIFIED.,.F.,.F.,(4,2,2,2,
2,2,2,2,2,2,2,2,2,2,2,2,2,4),(-21.3040471329169,-21.2575869056411,-21.1984857890134,
-21.1385060759405,-21.0808741357872,-21.020985062299,-20.9629703139414,
-20.9046646674613,-20.8448044072256,-20.7876184410835,-20.7286603001414,
-20.6688146325854,-20.6113178626411,-20.5515806625315,-20.4931217480668,
-20.4349453158928,-20.3744498438103,-20.3553623627869),.UNSPECIFIED.);
#24756=B_SPLINE_CURVE_WITH_KNOTS('',3,(#374153,#374154,#374155,#374156,
#374157,#374158,#374159,#374160,#374161,#374162,#374163,#374164,#374165,
#374166,#374167,#374168,#374169,#374170,#374171,#374172,#374173,#374174,
#374175,#374176,#374177,#374178,#374179,#374180,#374181,#374182,#374183,
#374184,#374185,#374186,#374187,#374188),.UNSPECIFIED.,.F.,.F.,(4,2,2,2,
2,2,2,2,2,2,2,2,2,2,2,2,2,4),(-6.61411156553163,-6.59852879776156,-6.53864687862724,
-6.48034472857874,-6.42226121693166,-6.36237812530755,-6.30475040045785,
-6.24466086149623,-6.18556874055552,-6.12842014710544,-6.06856566040906,
-6.0101242433252,-5.95236086994519,-5.89231953448862,-5.83455029960576,
-5.77504829554932,-5.71578177090393,-5.66552160898876),.UNSPECIFIED.);
#24757=B_SPLINE_CURVE_WITH_KNOTS('',3,(#374193,#374194,#374195,#374196,
#374197,#374198,#374199,#374200,#374201,#374202,#374203,#374204,#374205,
#374206,#374207,#374208,#374209,#374210,#374211,#374212,#374213,#374214,
#374215,#374216,#374217,#374218,#374219,#374220,#374221,#374222,#374223,
#374224,#374225,#374226,#374227,#374228),.UNSPECIFIED.,.F.,.F.,(4,2,2,2,
2,2,2,2,2,2,2,2,2,2,2,2,2,4),(-22.2524744631594,-22.1969643549059,-22.1374730057097,
-22.078565472214,-22.0206058074863,-21.9603516293046,-21.902869637356,-21.844236894089,
-21.7843953507018,-21.7272266490843,-21.6679458988016,-21.6085436857681,
-21.5507646986687,-21.4907113549369,-21.4330056552389,-21.3745547375389,
-21.3147177745165,-21.3040471329169),.UNSPECIFIED.);
#24758=B_SPLINE_CURVE_WITH_KNOTS('',3,(#374229,#374230,#374231,#374232,
#374233,#374234,#374235,#374236,#374237,#374238,#374239,#374240,#374241,
#374242,#374243,#374244,#374245,#374246,#374247,#374248,#374249,#374250,
#374251,#374252,#374253,#374254,#374255,#374256,#374257,#374258,#374259,
#374260,#374261,#374262,#374263,#374264,#374265,#374266),.UNSPECIFIED.,
 .F.,.F.,(4,2,2,2,2,2,2,2,2,2,2,2,2,2,2,2,2,2,4),(-5.66552160898876,-5.65861030605964,
-5.59875565665915,-5.54013765782867,-5.48261237053247,-5.42237542882488,
-5.36443033631434,-5.30543779450035,-5.24596500552574,-5.18867179004698,
-5.12878718949535,-5.06996044256316,-5.01257550757565,-4.95211087682467,
-4.89396022413654,-4.83537226336453,-4.77566683082353,-4.71819808424915,
-4.71640257571924),.UNSPECIFIED.);
#24759=B_SPLINE_CURVE_WITH_KNOTS('',3,(#374271,#374272,#374273,#374274,
#374275,#374276,#374277,#374278,#374279,#374280,#374281,#374282,#374283,
#374284,#374285,#374286,#374287,#374288,#374289,#374290,#374291,#374292,
#374293,#374294,#374295,#374296,#374297,#374298,#374299,#374300,#374301,
#374302,#374303,#374304,#374305,#374306,#374307,#374308),.UNSPECIFIED.,
 .F.,.F.,(4,2,2,2,2,2,2,2,2,2,2,2,2,2,2,2,2,2,4),(-23.2014899391179,-23.1944741493812,
-23.1368527057195,-23.0769758166295,-23.018913629611,-22.9606179964716,
-22.9007479118989,-22.8435446030669,-22.784596109354,-22.7247422526117,
-22.667253597635,-22.6075260296607,-22.5490052317576,-22.4908358902754,
-22.4303496168354,-22.3729921479549,-22.3141462340828,-22.2542699309318,
-22.2524744631594),.UNSPECIFIED.);
#24760=B_SPLINE_CURVE_WITH_KNOTS('',3,(#374309,#374310,#374311,#374312,
#374313,#374314,#374315,#374316,#374317,#374318,#374319,#374320,#374321,
#374322,#374323,#374324,#374325,#374326,#374327,#374328,#374329,#374330,
#374331,#374332,#374333,#374334,#374335,#374336,#374337,#374338,#374339,
#374340,#374341,#374342,#374343,#374344),.UNSPECIFIED.,.F.,.F.,(4,2,2,2,
2,2,2,2,2,2,2,2,2,2,2,2,2,4),(-4.71640257571924,-4.65834451124209,-4.59941813000702,
-4.54220227768689,-4.48233054243417,-4.42405736880598,-4.36594566804926,
-4.30609422957073,-4.24849578389153,-4.18834689967496,-4.1292885102004,
-4.07215083811356,-4.01230974894481,-3.95390216281254,-3.89611869200024,
-3.83611389751589,-3.77837843111154,-3.76793502765558),.UNSPECIFIED.);
#24761=B_SPLINE_CURVE_WITH_KNOTS('',3,(#374349,#374350,#374351,#374352,
#374353,#374354,#374355,#374356,#374357,#374358,#374359,#374360,#374361,
#374362,#374363,#374364,#374365,#374366,#374367,#374368,#374369,#374370,
#374371,#374372,#374373,#374374,#374375,#374376,#374377,#374378,#374379,
#374380,#374381,#374382,#374383,#374384),.UNSPECIFIED.,.F.,.F.,(4,2,2,2,
2,2,2,2,2,2,2,2,2,2,2,2,2,4),(-24.1499027888804,-24.1346238268317,-24.0766829154348,
-24.0164498947841,-23.9589407260275,-23.9003269603049,-23.8404823973082,
-23.7833187058296,-23.7240565994254,-23.6645824940566,-23.6068184151902,
-23.5467820581576,-23.4890377631433,-23.4306016418707,-23.3707581422136,
-23.3136203700441,-23.2545337284766,-23.2014899391179),.UNSPECIFIED.);
#24762=B_SPLINE_CURVE_WITH_KNOTS('',3,(#374385,#374386,#374387,#374388,
#374389,#374390,#374391,#374392,#374393,#374394,#374395,#374396,#374397,
#374398,#374399,#374400,#374401,#374402,#374403,#374404,#374405,#374406,
#374407,#374408,#374409,#374410,#374411,#374412,#374413,#374414,#374415,
#374416,#374417,#374418,#374419,#374420),.UNSPECIFIED.,.F.,.F.,(4,2,2,2,
2,2,2,2,2,2,2,2,2,2,2,2,2,4),(-3.76793502765558,-3.71882412297623,-3.65959561825608,
-3.60244671733181,-3.54260890239311,-3.48402902622074,-3.4264946173028,
-3.36629850670476,-3.30839113203855,-3.24935722391666,-3.18992604999305,
-3.1326674133047,-3.07280339483725,-3.01401842998219,-2.95663666569317,
-2.89621652056965,-2.83810698830649,-2.81929352507592),.UNSPECIFIED.);
#24763=B_SPLINE_CURVE_WITH_KNOTS('',3,(#374425,#374426,#374427,#374428,
#374429,#374430,#374431,#374432,#374433,#374434,#374435,#374436,#374437,
#374438,#374439,#374440,#374441,#374442,#374443,#374444,#374445,#374446,
#374447,#374448,#374449,#374450,#374451,#374452,#374453,#374454,#374455,
#374456,#374457,#374458,#374459,#374460),.UNSPECIFIED.,.F.,.F.,(4,2,2,2,
2,2,2,2,2,2,2,2,2,2,2,2,2,4),(-25.0988774139147,-25.0748748133069,-25.0166042193354,
-24.9567402234876,-24.8995341312701,-24.8406104828899,-24.7807642560441,
-24.723298521872,-24.6635959223151,-24.6050291412632,-24.546881843457,-24.4864202492779,
-24.4290481820111,-24.3702247779384,-24.3103492878962,-24.253060753562,
-24.193591509621,-24.1499027888804),.UNSPECIFIED.);
#24764=B_SPLINE_CURVE_WITH_KNOTS('',3,(#374461,#374462,#374463,#374464,
#374465,#374466,#374467,#374468,#374469,#374470,#374471,#374472,#374473,
#374474,#374475,#374476,#374477,#374478,#374479,#374480,#374481,#374482,
#374483,#374484,#374485,#374486,#374487,#374488,#374489,#374490,#374491,
#374492,#374493,#374494,#374495,#374496),.UNSPECIFIED.,.F.,.F.,(4,2,2,2,
2,2,2,2,2,2,2,2,2,2,2,2,2,4),(-2.81929352507592,-2.77949126923264,-2.71983044208255,
-2.66240353815619,-2.60257729967794,-2.54369522708906,-2.48649445360784,
-2.42664858989673,-2.36841971353789,-2.31029402853068,-2.25049001822912,
-2.19293604132315,-2.13274226536931,-2.07373326798044,-2.0166205280456,
-1.9568085453459,-1.8984502829867,-1.87105276048628),.UNSPECIFIED.);
#24765=B_SPLINE_CURVE_WITH_KNOTS('',3,(#374501,#374502,#374503,#374504,
#374505,#374506,#374507,#374508,#374509,#374510,#374511,#374512,#374513,
#374514,#374515,#374516,#374517,#374518,#374519,#374520,#374521,#374522,
#374523,#374524,#374525,#374526,#374527,#374528,#374529,#374530,#374531,
#374532,#374533,#374534,#374535,#374536),.UNSPECIFIED.,.F.,.F.,(4,2,2,2,
2,2,2,2,2,2,2,2,2,2,2,2,2,4),(-26.0471246382356,-26.014786013898,-25.9562063699669,
-25.8963745576448,-25.8392297972985,-25.780001663451,-25.7204714222612,
-25.6627371816127,-25.6027332862293,-25.5449651735138,-25.4865589174191,
-25.4267247255602,-25.3695942187353,-25.3105372981954,-25.2504143722874,
-25.1928183063652,-25.132969022655,-25.0988774139147),.UNSPECIFIED.);
#24766=B_SPLINE_CURVE_WITH_KNOTS('',3,(#374537,#374538,#374539,#374540,
#374541,#374542,#374543,#374544,#374545,#374546,#374547,#374548,#374549,
#374550,#374551,#374552,#374553,#374554,#374555,#374556,#374557,#374558,
#374559,#374560,#374561,#374562,#374563,#374564,#374565,#374566,#374567,
#374568,#374569,#374570,#374571,#374572),.UNSPECIFIED.,.F.,.F.,(4,2,2,2,
2,2,2,2,2,2,2,2,2,2,2,2,2,4),(-1.87105276048628,-1.84066057871695,-1.78070828476016,
-1.72302194556017,-1.66342921249075,-1.60425458530026,-1.54714230655092,
-1.4873370572563,-1.42881098805722,-1.3712811519465,-1.31114203082431,-1.25328791183393,
-1.19422612501562,-1.13485262074985,-1.07764287772901,-1.01781519741776,
-0.959087889976359,-0.923094486905693),.UNSPECIFIED.);
#24767=B_SPLINE_CURVE_WITH_KNOTS('',3,(#374577,#374578,#374579,#374580,
#374581,#374582,#374583,#374584,#374585,#374586,#374587,#374588,#374589,
#374590),.UNSPECIFIED.,.F.,.F.,(4,2,2,2,2,2,4),(-0.0885266411023889,-0.0801647036685068,
-0.0712344835087916,-0.0543173269975797,-0.031179370811489,-0.0186636990760277,
-9.9995278037468E-7),.UNSPECIFIED.);
#24768=B_SPLINE_CURVE_WITH_KNOTS('',3,(#374593,#374594,#374595,#374596,
#374597,#374598,#374599,#374600,#374601,#374602),.UNSPECIFIED.,.F.,.F.,
(4,2,2,2,4),(0.,0.0261902001057277,0.0515478142334988,0.0956791429839492,
0.112627808033314),.UNSPECIFIED.);
#24769=B_SPLINE_CURVE_WITH_KNOTS('',3,(#374607,#374608,#374609,#374610,
#374611,#374612,#374613,#374614,#374615,#374616,#374617,#374618,#374619,
#374620,#374621,#374622,#374623,#374624,#374625,#374626,#374627,#374628,
#374629,#374630,#374631,#374632,#374633,#374634),.UNSPECIFIED.,.F.,.F.,
(4,2,2,2,2,2,2,2,2,2,2,2,2,4),(-0.8274758898732,-0.742569538402508,-0.675901844511659,
-0.62317760234926,-0.574257833858176,-0.509286803493012,-0.421718441648047,
-0.331990489069755,-0.251855537588908,-0.165988637839021,-0.104830893630237,
-0.0601605470835078,-0.0309643052748887,0.),.UNSPECIFIED.);
#24770=B_SPLINE_CURVE_WITH_KNOTS('',3,(#374639,#374640,#374641,#374642,
#374643,#374644,#374645,#374646,#374647,#374648,#374649,#374650,#374651,
#374652),.UNSPECIFIED.,.F.,.F.,(4,2,2,2,2,2,4),(1.00000009773572E-6,0.0321609114607883,
0.0622225044979538,0.116840717683487,0.162125154778588,0.187837242944783,
0.212522064408195),.UNSPECIFIED.);
#24771=B_SPLINE_CURVE_WITH_KNOTS('',3,(#374655,#374656,#374657,#374658,
#374659,#374660,#374661,#374662,#374663,#374664,#374665,#374666,#374667,
#374668),.UNSPECIFIED.,.F.,.F.,(4,2,2,2,2,2,4),(-1.28815859321983,-1.20510585719494,
-1.12916275151302,-1.02246205795895,-0.923777683161166,-0.830690938202541,
-0.8274758898732),.UNSPECIFIED.);
#24772=B_SPLINE_CURVE_WITH_KNOTS('',3,(#374670,#374671,#374672,#374673,
#374674,#374675,#374676,#374677,#374678,#374679,#374680,#374681,#374682,
#374683,#374684,#374685,#374686,#374687,#374688,#374689,#374690,#374691,
#374692,#374693,#374694,#374695,#374696,#374697,#374698,#374699,#374700,
#374701),.UNSPECIFIED.,.F.,.F.,(4,2,2,2,2,2,2,2,2,2,2,2,2,2,2,4),(0.112627808033314,
0.149387855061838,0.209041889520592,0.264760139455438,0.319335059686991,
0.366312336217241,0.415214237389767,0.462499478525696,0.513472152163099,
0.578307516406786,0.666355563097664,0.758679715521255,0.848684132039911,
0.941858489596729,1.01877466686786,1.0988436208123),.UNSPECIFIED.);
#24773=B_SPLINE_CURVE_WITH_KNOTS('',3,(#374703,#374704,#374705,#374706,
#374707,#374708,#374709,#374710,#374711,#374712,#374713,#374714,#374715,
#374716,#374717,#374718,#374719,#374720,#374721,#374722,#374723,#374724,
#374725,#374726,#374727,#374728,#374729,#374730,#374731,#374732,#374733,
#374734,#374735,#374736,#374737,#374738),.UNSPECIFIED.,.F.,.F.,(4,2,2,2,
2,2,2,2,2,2,2,2,2,2,2,2,2,4),(-0.923094486905693,-0.901723063681326,-0.841363823302868,
-0.783311185390732,-0.724681122997764,-0.665081196534761,-0.607711810661505,
-0.547928834753099,-0.489107229536437,-0.431935698290824,-0.372131671145491,
-0.313963092952632,-0.255837015396937,-0.196096950836227,-0.138603322235919,
-0.078377809682703,-0.0389284678633673,-1.00000011094004E-6),
 .UNSPECIFIED.);
#24774=B_SPLINE_CURVE_WITH_KNOTS('',3,(#374739,#374740,#374741,#374742,
#374743,#374744,#374745,#374746,#374747,#374748,#374749,#374750,#374751,
#374752,#374753,#374754,#374755,#374756,#374757,#374758,#374759,#374760,
#374761,#374762,#374763,#374764,#374765,#374766,#374767,#374768,#374769,
#374770),.UNSPECIFIED.,.F.,.F.,(4,2,2,2,2,2,2,2,2,2,2,2,2,2,2,4),(-26.8550566050564,
-26.8176636569728,-26.7789214528464,-26.7192594122446,-26.6606613243223,
-26.6025512227894,-26.5421300349857,-26.4847575911641,-26.4259720044066,
-26.3661130930589,-26.3088555463882,-26.249423905818,-26.1904112321546,
-26.1325041472705,-26.072307916167,-26.0471246382356),.UNSPECIFIED.);
#24775=B_SPLINE_CURVE_WITH_KNOTS('',3,(#374816,#374817,#374818,#374819,
#374820,#374821,#374822),.UNSPECIFIED.,.F.,.F.,(4,3,4),(9.48676900924816E-20,
2.5000002149412E-5,9.54746331310774E-5),.UNSPECIFIED.);
#24776=B_SPLINE_CURVE_WITH_KNOTS('',3,(#374826,#374827,#374828,#374829,
#374830,#374831,#374832),.UNSPECIFIED.,.F.,.F.,(4,3,4),(0.,2.50000024491141E-5,
9.54746329568079E-5),.UNSPECIFIED.);
#24777=B_SPLINE_CURVE_WITH_KNOTS('',3,(#374836,#374837,#374838,#374839,
#374840,#374841,#374842),.UNSPECIFIED.,.F.,.F.,(4,3,4),(8.13151629364128E-20,
2.50000021494121E-5,9.54746331310775E-5),.UNSPECIFIED.);
#24778=B_SPLINE_CURVE_WITH_KNOTS('',3,(#374846,#374847,#374848,#374849,
#374850,#374851,#374852),.UNSPECIFIED.,.F.,.F.,(4,3,4),(0.,2.50000024491136E-5,
9.54746329568078E-5),.UNSPECIFIED.);
#24779=B_SPLINE_CURVE_WITH_KNOTS('',3,(#374856,#374857,#374858,#374859,
#374860,#374861,#374862),.UNSPECIFIED.,.F.,.F.,(4,3,4),(5.42101086242752E-20,
2.50000021494117E-5,9.5474633131077E-5),.UNSPECIFIED.);
#24780=B_SPLINE_CURVE_WITH_KNOTS('',3,(#374866,#374867,#374868,#374869,
#374870,#374871,#374872),.UNSPECIFIED.,.F.,.F.,(4,3,4),(0.,2.50000024491138E-5,
9.54746329568077E-5),.UNSPECIFIED.);
#24781=B_SPLINE_CURVE_WITH_KNOTS('',3,(#374876,#374877,#374878,#374879,
#374880,#374881,#374882),.UNSPECIFIED.,.F.,.F.,(4,3,4),(1.0842021724855E-19,
2.50000021494118E-5,9.54746331310773E-5),.UNSPECIFIED.);
#24782=B_SPLINE_CURVE_WITH_KNOTS('',3,(#374886,#374887,#374888,#374889,
#374890,#374891,#374892),.UNSPECIFIED.,.F.,.F.,(4,3,4),(0.,2.50000024491138E-5,
9.54746329568075E-5),.UNSPECIFIED.);
#24783=B_SPLINE_CURVE_WITH_KNOTS('',3,(#374896,#374897,#374898,#374899,
#374900,#374901,#374902),.UNSPECIFIED.,.F.,.F.,(4,3,4),(4.33680868994202E-19,
2.50000021494122E-5,9.54746331310774E-5),.UNSPECIFIED.);
#24784=B_SPLINE_CURVE_WITH_KNOTS('',3,(#374906,#374907,#374908,#374909,
#374910,#374911,#374912),.UNSPECIFIED.,.F.,.F.,(4,3,4),(0.,2.5000002449114E-5,
9.54746329568081E-5),.UNSPECIFIED.);
#24785=B_SPLINE_CURVE_WITH_KNOTS('',3,(#374916,#374917,#374918,#374919,
#374920,#374921,#374922),.UNSPECIFIED.,.F.,.F.,(4,3,4),(4.33680868994202E-19,
2.5000002149412E-5,9.54746331310775E-5),.UNSPECIFIED.);
#24786=B_SPLINE_CURVE_WITH_KNOTS('',3,(#374926,#374927,#374928,#374929,
#374930,#374931,#374932),.UNSPECIFIED.,.F.,.F.,(4,3,4),(0.,2.50000024491139E-5,
9.54746329568077E-5),.UNSPECIFIED.);
#24787=B_SPLINE_CURVE_WITH_KNOTS('',3,(#374936,#374937,#374938,#374939,
#374940,#374941,#374942),.UNSPECIFIED.,.F.,.F.,(4,3,4),(4.33680868994202E-19,
2.50000021494119E-5,9.54746331310775E-5),.UNSPECIFIED.);
#24788=B_SPLINE_CURVE_WITH_KNOTS('',3,(#374946,#374947,#374948,#374949,
#374950,#374951,#374952),.UNSPECIFIED.,.F.,.F.,(4,3,4),(0.,2.50000024491138E-5,
9.5474632956808E-5),.UNSPECIFIED.);
#24789=B_SPLINE_CURVE_WITH_KNOTS('',3,(#374956,#374957,#374958,#374959,
#374960,#374961,#374962),.UNSPECIFIED.,.F.,.F.,(4,3,4),(4.33680868994202E-19,
2.5000002149412E-5,9.54746331310776E-5),.UNSPECIFIED.);
#24790=B_SPLINE_CURVE_WITH_KNOTS('',3,(#374966,#374967,#374968,#374969,
#374970,#374971,#374972),.UNSPECIFIED.,.F.,.F.,(4,3,4),(0.,2.5000002449114E-5,
9.54746329568075E-5),.UNSPECIFIED.);
#24791=B_SPLINE_CURVE_WITH_KNOTS('',3,(#374976,#374977,#374978,#374979,
#374980,#374981,#374982),.UNSPECIFIED.,.F.,.F.,(4,3,4),(4.33680868994202E-19,
2.50000021494117E-5,9.54746331310776E-5),.UNSPECIFIED.);
#24792=B_SPLINE_CURVE_WITH_KNOTS('',3,(#374986,#374987,#374988,#374989,
#374990,#374991,#374992),.UNSPECIFIED.,.F.,.F.,(4,3,4),(0.,2.50000024491139E-5,
9.54746329568078E-5),.UNSPECIFIED.);
#24793=B_SPLINE_CURVE_WITH_KNOTS('',3,(#374996,#374997,#374998,#374999,
#375000,#375001,#375002),.UNSPECIFIED.,.F.,.F.,(4,3,4),(4.33680868994202E-19,
2.50000021494117E-5,9.54746331310774E-5),.UNSPECIFIED.);
#24794=B_SPLINE_CURVE_WITH_KNOTS('',3,(#375006,#375007,#375008,#375009,
#375010,#375011,#375012),.UNSPECIFIED.,.F.,.F.,(4,3,4),(0.,2.50000024491137E-5,
9.54746329568078E-5),.UNSPECIFIED.);
#24795=B_SPLINE_CURVE_WITH_KNOTS('',3,(#375016,#375017,#375018,#375019,
#375020,#375021,#375022),.UNSPECIFIED.,.F.,.F.,(4,3,4),(4.33680868994202E-19,
2.50000021494118E-5,9.54746331310774E-5),.UNSPECIFIED.);
#24796=B_SPLINE_CURVE_WITH_KNOTS('',3,(#375026,#375027,#375028,#375029,
#375030,#375031,#375032),.UNSPECIFIED.,.F.,.F.,(4,3,4),(0.,2.50000024491138E-5,
9.54746329568079E-5),.UNSPECIFIED.);
#24797=B_SPLINE_CURVE_WITH_KNOTS('',3,(#375036,#375037,#375038,#375039,
#375040,#375041,#375042),.UNSPECIFIED.,.F.,.F.,(4,3,4),(4.33680868994202E-19,
2.50000021494117E-5,9.54746331310776E-5),.UNSPECIFIED.);
#24798=B_SPLINE_CURVE_WITH_KNOTS('',3,(#375046,#375047,#375048,#375049,
#375050,#375051,#375052),.UNSPECIFIED.,.F.,.F.,(4,3,4),(0.,2.50000024491139E-5,
9.54746329568078E-5),.UNSPECIFIED.);
#24799=B_SPLINE_CURVE_WITH_KNOTS('',3,(#375056,#375057,#375058,#375059,
#375060,#375061,#375062),.UNSPECIFIED.,.F.,.F.,(4,3,4),(2.16840434497101E-19,
2.50000021494119E-5,9.54746331310775E-5),.UNSPECIFIED.);
#24800=B_SPLINE_CURVE_WITH_KNOTS('',3,(#375066,#375067,#375068,#375069,
#375070,#375071,#375072),.UNSPECIFIED.,.F.,.F.,(4,3,4),(0.,2.5000002449114E-5,
9.54746329568076E-5),.UNSPECIFIED.);
#24801=B_SPLINE_CURVE_WITH_KNOTS('',3,(#375076,#375077,#375078,#375079,
#375080,#375081,#375082),.UNSPECIFIED.,.F.,.F.,(4,3,4),(2.16840434497101E-19,
2.50000021494119E-5,9.54746331310775E-5),.UNSPECIFIED.);
#24802=B_SPLINE_CURVE_WITH_KNOTS('',3,(#375086,#375087,#375088,#375089,
#375090,#375091,#375092),.UNSPECIFIED.,.F.,.F.,(4,3,4),(0.,2.50000024491139E-5,
9.54746329568076E-5),.UNSPECIFIED.);
#24803=B_SPLINE_CURVE_WITH_KNOTS('',3,(#375096,#375097,#375098,#375099,
#375100,#375101,#375102),.UNSPECIFIED.,.F.,.F.,(4,3,4),(0.,2.5000002149412E-5,
9.54746331310776E-5),.UNSPECIFIED.);
#24804=B_SPLINE_CURVE_WITH_KNOTS('',3,(#375106,#375107,#375108,#375109,
#375110,#375111,#375112),.UNSPECIFIED.,.F.,.F.,(4,3,4),(0.,2.5000002449114E-5,
9.54746329568076E-5),.UNSPECIFIED.);
#24805=B_SPLINE_CURVE_WITH_KNOTS('',3,(#375116,#375117,#375118,#375119,
#375120,#375121,#375122),.UNSPECIFIED.,.F.,.F.,(4,3,4),(0.,2.50000021494119E-5,
9.54746331310776E-5),.UNSPECIFIED.);
#24806=B_SPLINE_CURVE_WITH_KNOTS('',3,(#375126,#375127,#375128,#375129,
#375130,#375131,#375132),.UNSPECIFIED.,.F.,.F.,(4,3,4),(0.,2.50000024491138E-5,
9.54746329568075E-5),.UNSPECIFIED.);
#24807=B_SPLINE_CURVE_WITH_KNOTS('',3,(#375136,#375137,#375138,#375139,
#375140,#375141,#375142),.UNSPECIFIED.,.F.,.F.,(4,3,4),(2.16840434497101E-19,
2.50000021494118E-5,9.54746331310777E-5),.UNSPECIFIED.);
#24808=B_SPLINE_CURVE_WITH_KNOTS('',3,(#375146,#375147,#375148,#375149,
#375150,#375151,#375152),.UNSPECIFIED.,.F.,.F.,(4,3,4),(0.,2.50000024491137E-5,
9.54746329568079E-5),.UNSPECIFIED.);
#24809=B_SPLINE_CURVE_WITH_KNOTS('',3,(#375156,#375157,#375158,#375159,
#375160,#375161,#375162),.UNSPECIFIED.,.F.,.F.,(4,3,4),(2.16840434497101E-19,
2.5000002149412E-5,9.54746331310779E-5),.UNSPECIFIED.);
#24810=B_SPLINE_CURVE_WITH_KNOTS('',3,(#375166,#375167,#375168,#375169,
#375170,#375171,#375172),.UNSPECIFIED.,.F.,.F.,(4,3,4),(0.,2.50000024491141E-5,
9.5474632956808E-5),.UNSPECIFIED.);
#24811=B_SPLINE_CURVE_WITH_KNOTS('',3,(#375176,#375177,#375178,#375179,
#375180,#375181,#375182),.UNSPECIFIED.,.F.,.F.,(4,3,4),(2.16840434497101E-19,
2.50000021494116E-5,9.54746331310775E-5),.UNSPECIFIED.);
#24812=B_SPLINE_CURVE_WITH_KNOTS('',3,(#375186,#375187,#375188,#375189,
#375190,#375191,#375192),.UNSPECIFIED.,.F.,.F.,(4,3,4),(0.,2.50000024491134E-5,
9.54746329568073E-5),.UNSPECIFIED.);
#24813=B_SPLINE_CURVE_WITH_KNOTS('',3,(#375196,#375197,#375198,#375199,
#375200,#375201,#375202),.UNSPECIFIED.,.F.,.F.,(4,3,4),(2.16840434497101E-19,
2.50000021494119E-5,9.54746331310774E-5),.UNSPECIFIED.);
#24814=B_SPLINE_CURVE_WITH_KNOTS('',3,(#375206,#375207,#375208,#375209,
#375210,#375211,#375212),.UNSPECIFIED.,.F.,.F.,(4,3,4),(0.,2.5000002449114E-5,
9.54746329568077E-5),.UNSPECIFIED.);
#24815=B_SPLINE_CURVE_WITH_KNOTS('',3,(#375216,#375217,#375218,#375219,
#375220,#375221,#375222),.UNSPECIFIED.,.F.,.F.,(4,3,4),(1.0842021724855E-19,
2.5000002149412E-5,9.54746331310776E-5),.UNSPECIFIED.);
#24816=B_SPLINE_CURVE_WITH_KNOTS('',3,(#375226,#375227,#375228,#375229,
#375230,#375231,#375232),.UNSPECIFIED.,.F.,.F.,(4,3,4),(0.,2.50000024491137E-5,
9.54746329568074E-5),.UNSPECIFIED.);
#24817=B_SPLINE_CURVE_WITH_KNOTS('',3,(#375236,#375237,#375238,#375239,
#375240,#375241,#375242),.UNSPECIFIED.,.F.,.F.,(4,3,4),(1.0842021724855E-19,
2.50000021494121E-5,9.54746331310777E-5),.UNSPECIFIED.);
#24818=B_SPLINE_CURVE_WITH_KNOTS('',3,(#375246,#375247,#375248,#375249,
#375250,#375251,#375252),.UNSPECIFIED.,.F.,.F.,(4,3,4),(0.,2.50000024491138E-5,
9.54746329568079E-5),.UNSPECIFIED.);
#24819=B_SPLINE_CURVE_WITH_KNOTS('',3,(#375256,#375257,#375258,#375259,
#375260,#375261,#375262),.UNSPECIFIED.,.F.,.F.,(4,3,4),(1.0842021724855E-19,
2.50000021494117E-5,9.54746331310775E-5),.UNSPECIFIED.);
#24820=B_SPLINE_CURVE_WITH_KNOTS('',3,(#375266,#375267,#375268,#375269,
#375270,#375271,#375272),.UNSPECIFIED.,.F.,.F.,(4,3,4),(0.,2.50000024491141E-5,
9.54746329568077E-5),.UNSPECIFIED.);
#24821=B_SPLINE_CURVE_WITH_KNOTS('',3,(#375276,#375277,#375278,#375279,
#375280,#375281,#375282),.UNSPECIFIED.,.F.,.F.,(4,3,4),(1.0842021724855E-19,
2.5000002149412E-5,9.54746331310775E-5),.UNSPECIFIED.);
#24822=B_SPLINE_CURVE_WITH_KNOTS('',3,(#375286,#375287,#375288,#375289,
#375290,#375291,#375292),.UNSPECIFIED.,.F.,.F.,(4,3,4),(0.,2.50000024491137E-5,
9.54746329568075E-5),.UNSPECIFIED.);
#24823=B_SPLINE_CURVE_WITH_KNOTS('',3,(#375296,#375297,#375298,#375299,
#375300,#375301,#375302),.UNSPECIFIED.,.F.,.F.,(4,3,4),(1.01643953670516E-19,
2.50000021494119E-5,9.54746331310775E-5),.UNSPECIFIED.);
#24824=B_SPLINE_CURVE_WITH_KNOTS('',3,(#375306,#375307,#375308,#375309,
#375310,#375311,#375312),.UNSPECIFIED.,.F.,.F.,(4,3,4),(0.,2.50000024491139E-5,
9.54746329568077E-5),.UNSPECIFIED.);
#24825=B_SPLINE_CURVE_WITH_KNOTS('',3,(#375316,#375317,#375318,#375319,
#375320,#375321,#375322),.UNSPECIFIED.,.F.,.F.,(4,3,4),(8.13151629364128E-20,
2.50000021494123E-5,9.54746331310776E-5),.UNSPECIFIED.);
#24826=B_SPLINE_CURVE_WITH_KNOTS('',3,(#375326,#375327,#375328,#375329,
#375330,#375331,#375332),.UNSPECIFIED.,.F.,.F.,(4,3,4),(0.,2.50000024491137E-5,
9.54746329568075E-5),.UNSPECIFIED.);
#24827=B_SPLINE_CURVE_WITH_KNOTS('',3,(#375336,#375337,#375338,#375339,
#375340,#375341,#375342),.UNSPECIFIED.,.F.,.F.,(4,3,4),(5.42101086242752E-20,
2.50000021494119E-5,9.54746331310775E-5),.UNSPECIFIED.);
#24828=B_SPLINE_CURVE_WITH_KNOTS('',3,(#375346,#375347,#375348,#375349,
#375350,#375351,#375352),.UNSPECIFIED.,.F.,.F.,(4,3,4),(0.,2.50000024491138E-5,
9.54746329568073E-5),.UNSPECIFIED.);
#24829=B_SPLINE_CURVE_WITH_KNOTS('',3,(#375356,#375357,#375358,#375359,
#375360,#375361,#375362),.UNSPECIFIED.,.F.,.F.,(4,3,4),(5.42101086242752E-20,
2.5000002149412E-5,9.54746331310778E-5),.UNSPECIFIED.);
#24830=B_SPLINE_CURVE_WITH_KNOTS('',3,(#375366,#375367,#375368,#375369,
#375370,#375371,#375372),.UNSPECIFIED.,.F.,.F.,(4,3,4),(0.,2.50000024491139E-5,
9.54746329568078E-5),.UNSPECIFIED.);
#24831=B_SPLINE_CURVE_WITH_KNOTS('',3,(#375376,#375377,#375378,#375379,
#375380,#375381,#375382),.UNSPECIFIED.,.F.,.F.,(4,3,4),(0.,2.50000021494121E-5,
9.54746331310777E-5),.UNSPECIFIED.);
#24832=B_SPLINE_CURVE_WITH_KNOTS('',3,(#375386,#375387,#375388,#375389,
#375390,#375391,#375392),.UNSPECIFIED.,.F.,.F.,(4,3,4),(0.,2.50000024491139E-5,
9.54746329568077E-5),.UNSPECIFIED.);
#24833=B_SPLINE_CURVE_WITH_KNOTS('',3,(#375396,#375397,#375398,#375399,
#375400,#375401,#375402),.UNSPECIFIED.,.F.,.F.,(4,3,4),(4.33680868994202E-19,
2.50000021494121E-5,9.54746331310774E-5),.UNSPECIFIED.);
#24834=B_SPLINE_CURVE_WITH_KNOTS('',3,(#375406,#375407,#375408,#375409,
#375410,#375411,#375412),.UNSPECIFIED.,.F.,.F.,(4,3,4),(0.,2.50000024491139E-5,
9.54746329568078E-5),.UNSPECIFIED.);
#24835=B_SPLINE_CURVE_WITH_KNOTS('',3,(#375416,#375417,#375418,#375419,
#375420,#375421,#375422),.UNSPECIFIED.,.F.,.F.,(4,3,4),(4.33680868994202E-19,
2.50000021494119E-5,9.54746331310773E-5),.UNSPECIFIED.);
#24836=B_SPLINE_CURVE_WITH_KNOTS('',3,(#375426,#375427,#375428,#375429,
#375430,#375431,#375432),.UNSPECIFIED.,.F.,.F.,(4,3,4),(0.,2.50000024491138E-5,
9.54746329568077E-5),.UNSPECIFIED.);
#24837=B_SPLINE_CURVE_WITH_KNOTS('',3,(#375436,#375437,#375438,#375439,
#375440,#375441,#375442),.UNSPECIFIED.,.F.,.F.,(4,3,4),(4.33680868994202E-19,
2.5000002149412E-5,9.54746331310777E-5),.UNSPECIFIED.);
#24838=B_SPLINE_CURVE_WITH_KNOTS('',3,(#375446,#375447,#375448,#375449,
#375450,#375451,#375452),.UNSPECIFIED.,.F.,.F.,(4,3,4),(0.,2.5000002449114E-5,
9.54746329568079E-5),.UNSPECIFIED.);
#24839=B_SPLINE_CURVE_WITH_KNOTS('',3,(#375456,#375457,#375458,#375459,
#375460,#375461,#375462),.UNSPECIFIED.,.F.,.F.,(4,3,4),(4.33680868994202E-19,
2.50000021494121E-5,9.54746331310776E-5),.UNSPECIFIED.);
#24840=B_SPLINE_CURVE_WITH_KNOTS('',3,(#375466,#375467,#375468,#375469,
#375470,#375471,#375472),.UNSPECIFIED.,.F.,.F.,(4,3,4),(0.,2.50000024491138E-5,
9.5474632956808E-5),.UNSPECIFIED.);
#24841=B_SPLINE_CURVE_WITH_KNOTS('',3,(#375476,#375477,#375478,#375479,
#375480,#375481,#375482),.UNSPECIFIED.,.F.,.F.,(4,3,4),(4.33680868994202E-19,
2.50000021494121E-5,9.54746331310774E-5),.UNSPECIFIED.);
#24842=B_SPLINE_CURVE_WITH_KNOTS('',3,(#375486,#375487,#375488,#375489,
#375490,#375491,#375492),.UNSPECIFIED.,.F.,.F.,(4,3,4),(0.,2.50000024491138E-5,
9.54746329568077E-5),.UNSPECIFIED.);
#24843=B_SPLINE_CURVE_WITH_KNOTS('',3,(#375496,#375497,#375498,#375499,
#375500,#375501,#375502),.UNSPECIFIED.,.F.,.F.,(4,3,4),(4.33680868994202E-19,
2.50000021494118E-5,9.54746331310775E-5),.UNSPECIFIED.);
#24844=B_SPLINE_CURVE_WITH_KNOTS('',3,(#375506,#375507,#375508,#375509,
#375510,#375511,#375512),.UNSPECIFIED.,.F.,.F.,(4,3,4),(0.,2.50000024491139E-5,
9.54746329568079E-5),.UNSPECIFIED.);
#24845=B_SPLINE_CURVE_WITH_KNOTS('',3,(#375516,#375517,#375518,#375519,
#375520,#375521,#375522),.UNSPECIFIED.,.F.,.F.,(4,3,4),(4.33680868994202E-19,
2.50000021494117E-5,9.54746331310775E-5),.UNSPECIFIED.);
#24846=B_SPLINE_CURVE_WITH_KNOTS('',3,(#375526,#375527,#375528,#375529,
#375530,#375531,#375532),.UNSPECIFIED.,.F.,.F.,(4,3,4),(0.,2.50000024491138E-5,
9.54746329568079E-5),.UNSPECIFIED.);
#24847=B_SPLINE_CURVE_WITH_KNOTS('',3,(#375536,#375537,#375538,#375539,
#375540,#375541,#375542),.UNSPECIFIED.,.F.,.F.,(4,3,4),(4.33680868994202E-19,
2.50000021494119E-5,9.54746331310774E-5),.UNSPECIFIED.);
#24848=B_SPLINE_CURVE_WITH_KNOTS('',3,(#375546,#375547,#375548,#375549,
#375550,#375551,#375552),.UNSPECIFIED.,.F.,.F.,(4,3,4),(0.,2.50000024491139E-5,
9.54746329568077E-5),.UNSPECIFIED.);
#24849=B_SPLINE_CURVE_WITH_KNOTS('',3,(#375556,#375557,#375558,#375559,
#375560,#375561,#375562),.UNSPECIFIED.,.F.,.F.,(4,3,4),(2.16840434497101E-19,
2.50000021494119E-5,9.54746331310775E-5),.UNSPECIFIED.);
#24850=B_SPLINE_CURVE_WITH_KNOTS('',3,(#375566,#375567,#375568,#375569,
#375570,#375571,#375572),.UNSPECIFIED.,.F.,.F.,(4,3,4),(0.,2.50000024491139E-5,
9.5474632956808E-5),.UNSPECIFIED.);
#24851=B_SPLINE_CURVE_WITH_KNOTS('',3,(#375576,#375577,#375578,#375579,
#375580,#375581,#375582),.UNSPECIFIED.,.F.,.F.,(4,3,4),(2.16840434497101E-19,
2.5000002149412E-5,9.54746331310775E-5),.UNSPECIFIED.);
#24852=B_SPLINE_CURVE_WITH_KNOTS('',3,(#375586,#375587,#375588,#375589,
#375590,#375591,#375592),.UNSPECIFIED.,.F.,.F.,(4,3,4),(0.,2.50000024491142E-5,
9.54746329568079E-5),.UNSPECIFIED.);
#24853=B_SPLINE_CURVE_WITH_KNOTS('',3,(#375596,#375597,#375598,#375599,
#375600,#375601,#375602),.UNSPECIFIED.,.F.,.F.,(4,3,4),(2.16840434497101E-19,
2.5000002149412E-5,9.54746331310776E-5),.UNSPECIFIED.);
#24854=B_SPLINE_CURVE_WITH_KNOTS('',3,(#375606,#375607,#375608,#375609,
#375610,#375611,#375612),.UNSPECIFIED.,.F.,.F.,(4,3,4),(0.,2.50000024491136E-5,
9.54746329568075E-5),.UNSPECIFIED.);
#24855=B_SPLINE_CURVE_WITH_KNOTS('',3,(#375616,#375617,#375618,#375619,
#375620,#375621,#375622),.UNSPECIFIED.,.F.,.F.,(4,3,4),(2.16840434497101E-19,
2.50000021494117E-5,9.54746331310776E-5),.UNSPECIFIED.);
#24856=B_SPLINE_CURVE_WITH_KNOTS('',3,(#375626,#375627,#375628,#375629,
#375630,#375631,#375632),.UNSPECIFIED.,.F.,.F.,(4,3,4),(0.,2.50000024491138E-5,
9.54746329568075E-5),.UNSPECIFIED.);
#24857=B_SPLINE_CURVE_WITH_KNOTS('',3,(#375636,#375637,#375638,#375639,
#375640,#375641,#375642),.UNSPECIFIED.,.F.,.F.,(4,3,4),(2.16840434497101E-19,
2.50000021494118E-5,9.54746331310776E-5),.UNSPECIFIED.);
#24858=B_SPLINE_CURVE_WITH_KNOTS('',3,(#375646,#375647,#375648,#375649,
#375650,#375651,#375652),.UNSPECIFIED.,.F.,.F.,(4,3,4),(0.,2.50000024491139E-5,
9.54746329568075E-5),.UNSPECIFIED.);
#24859=B_SPLINE_CURVE_WITH_KNOTS('',3,(#375656,#375657,#375658,#375659,
#375660,#375661,#375662),.UNSPECIFIED.,.F.,.F.,(4,3,4),(2.16840434497101E-19,
2.5000002149412E-5,9.54746331310774E-5),.UNSPECIFIED.);
#24860=B_SPLINE_CURVE_WITH_KNOTS('',3,(#375666,#375667,#375668,#375669,
#375670,#375671,#375672),.UNSPECIFIED.,.F.,.F.,(4,3,4),(0.,2.5000002449114E-5,
9.54746329568077E-5),.UNSPECIFIED.);
#24861=B_SPLINE_CURVE_WITH_KNOTS('',3,(#375676,#375677,#375678,#375679,
#375680,#375681,#375682),.UNSPECIFIED.,.F.,.F.,(4,3,4),(2.16840434497101E-19,
2.50000021494121E-5,9.54746331310778E-5),.UNSPECIFIED.);
#24862=B_SPLINE_CURVE_WITH_KNOTS('',3,(#375686,#375687,#375688,#375689,
#375690,#375691,#375692),.UNSPECIFIED.,.F.,.F.,(4,3,4),(0.,2.50000024491136E-5,
9.54746329568075E-5),.UNSPECIFIED.);
#24863=B_SPLINE_CURVE_WITH_KNOTS('',3,(#375696,#375697,#375698,#375699,
#375700,#375701,#375702),.UNSPECIFIED.,.F.,.F.,(4,3,4),(0.,2.5000002149412E-5,
9.54746331310776E-5),.UNSPECIFIED.);
#24864=B_SPLINE_CURVE_WITH_KNOTS('',3,(#375706,#375707,#375708,#375709,
#375710,#375711,#375712),.UNSPECIFIED.,.F.,.F.,(4,3,4),(0.,2.5000002449114E-5,
9.54746329568075E-5),.UNSPECIFIED.);
#24865=B_SPLINE_CURVE_WITH_KNOTS('',3,(#375716,#375717,#375718,#375719,
#375720,#375721,#375722),.UNSPECIFIED.,.F.,.F.,(4,3,4),(1.0842021724855E-19,
2.50000021494118E-5,9.54746331310777E-5),.UNSPECIFIED.);
#24866=B_SPLINE_CURVE_WITH_KNOTS('',3,(#375726,#375727,#375728,#375729,
#375730,#375731,#375732),.UNSPECIFIED.,.F.,.F.,(4,3,4),(0.,2.50000024491137E-5,
9.5474632956808E-5),.UNSPECIFIED.);
#24867=B_SPLINE_CURVE_WITH_KNOTS('',3,(#375736,#375737,#375738,#375739,
#375740,#375741,#375742),.UNSPECIFIED.,.F.,.F.,(4,3,4),(1.0842021724855E-19,
2.50000021494119E-5,9.54746331310774E-5),.UNSPECIFIED.);
#24868=B_SPLINE_CURVE_WITH_KNOTS('',3,(#375746,#375747,#375748,#375749,
#375750,#375751,#375752),.UNSPECIFIED.,.F.,.F.,(4,3,4),(0.,2.50000024491138E-5,
9.54746329568078E-5),.UNSPECIFIED.);
#24869=B_SPLINE_CURVE_WITH_KNOTS('',3,(#375756,#375757,#375758,#375759,
#375760,#375761,#375762),.UNSPECIFIED.,.F.,.F.,(4,3,4),(1.0842021724855E-19,
2.50000021494117E-5,9.54746331310775E-5),.UNSPECIFIED.);
#24870=B_SPLINE_CURVE_WITH_KNOTS('',3,(#375766,#375767,#375768,#375769,
#375770,#375771,#375772),.UNSPECIFIED.,.F.,.F.,(4,3,4),(0.,2.50000024491139E-5,
9.54746329568076E-5),.UNSPECIFIED.);
#24871=B_SPLINE_CURVE_WITH_KNOTS('',3,(#375776,#375777,#375778,#375779,
#375780,#375781,#375782),.UNSPECIFIED.,.F.,.F.,(4,3,4),(1.0842021724855E-19,
2.5000002149412E-5,9.54746331310773E-5),.UNSPECIFIED.);
#24872=B_SPLINE_CURVE_WITH_KNOTS('',3,(#375786,#375787,#375788,#375789,
#375790,#375791,#375792),.UNSPECIFIED.,.F.,.F.,(4,3,4),(0.,2.50000024491138E-5,
9.54746329568079E-5),.UNSPECIFIED.);
#24873=B_SPLINE_CURVE_WITH_KNOTS('',3,(#375803,#375804,#375805,#375806,
#375807,#375808,#375809),.UNSPECIFIED.,.F.,.F.,(4,3,4),(9.48676900924816E-20,
2.50000021494119E-5,9.54746331310775E-5),.UNSPECIFIED.);
#24874=B_SPLINE_CURVE_WITH_KNOTS('',3,(#375813,#375814,#375815,#375816,
#375817,#375818,#375819),.UNSPECIFIED.,.F.,.F.,(4,3,4),(0.,2.50000024491136E-5,
9.54746329568077E-5),.UNSPECIFIED.);
#24875=B_SPLINE_CURVE_WITH_KNOTS('',3,(#375823,#375824,#375825,#375826,
#375827,#375828,#375829),.UNSPECIFIED.,.F.,.F.,(4,3,4),(8.13151629364128E-20,
2.5000002149412E-5,9.54746331310776E-5),.UNSPECIFIED.);
#24876=B_SPLINE_CURVE_WITH_KNOTS('',3,(#375833,#375834,#375835,#375836,
#375837,#375838,#375839),.UNSPECIFIED.,.F.,.F.,(4,3,4),(0.,2.5000002449114E-5,
9.54746329568077E-5),.UNSPECIFIED.);
#24877=B_SPLINE_CURVE_WITH_KNOTS('',3,(#375843,#375844,#375845,#375846,
#375847,#375848,#375849),.UNSPECIFIED.,.F.,.F.,(4,3,4),(5.42101086242752E-20,
2.5000002149412E-5,9.54746331310776E-5),.UNSPECIFIED.);
#24878=B_SPLINE_CURVE_WITH_KNOTS('',3,(#375853,#375854,#375855,#375856,
#375857,#375858,#375859),.UNSPECIFIED.,.F.,.F.,(4,3,4),(0.,2.50000024491138E-5,
9.54746329568079E-5),.UNSPECIFIED.);
#24879=B_SPLINE_CURVE_WITH_KNOTS('',3,(#375863,#375864,#375865,#375866,
#375867,#375868,#375869),.UNSPECIFIED.,.F.,.F.,(4,3,4),(1.0842021724855E-19,
2.50000021494121E-5,9.54746331310775E-5),.UNSPECIFIED.);
#24880=B_SPLINE_CURVE_WITH_KNOTS('',3,(#375873,#375874,#375875,#375876,
#375877,#375878,#375879),.UNSPECIFIED.,.F.,.F.,(4,3,4),(0.,2.50000024491138E-5,
9.54746329568079E-5),.UNSPECIFIED.);
#24881=B_SPLINE_CURVE_WITH_KNOTS('',3,(#375883,#375884,#375885,#375886,
#375887,#375888,#375889),.UNSPECIFIED.,.F.,.F.,(4,3,4),(4.33680868994202E-19,
2.50000021494119E-5,9.54746331310774E-5),.UNSPECIFIED.);
#24882=B_SPLINE_CURVE_WITH_KNOTS('',3,(#375893,#375894,#375895,#375896,
#375897,#375898,#375899),.UNSPECIFIED.,.F.,.F.,(4,3,4),(0.,2.50000024491138E-5,
9.54746329568078E-5),.UNSPECIFIED.);
#24883=B_SPLINE_CURVE_WITH_KNOTS('',3,(#375903,#375904,#375905,#375906,
#375907,#375908,#375909),.UNSPECIFIED.,.F.,.F.,(4,3,4),(4.33680868994202E-19,
2.5000002149412E-5,9.54746331310775E-5),.UNSPECIFIED.);
#24884=B_SPLINE_CURVE_WITH_KNOTS('',3,(#375913,#375914,#375915,#375916,
#375917,#375918,#375919),.UNSPECIFIED.,.F.,.F.,(4,3,4),(0.,2.50000024491135E-5,
9.54746329568076E-5),.UNSPECIFIED.);
#24885=B_SPLINE_CURVE_WITH_KNOTS('',3,(#375923,#375924,#375925,#375926,
#375927,#375928,#375929),.UNSPECIFIED.,.F.,.F.,(4,3,4),(4.33680868994202E-19,
2.50000021494119E-5,9.54746331310774E-5),.UNSPECIFIED.);
#24886=B_SPLINE_CURVE_WITH_KNOTS('',3,(#375933,#375934,#375935,#375936,
#375937,#375938,#375939),.UNSPECIFIED.,.F.,.F.,(4,3,4),(0.,2.5000002449114E-5,
9.54746329568078E-5),.UNSPECIFIED.);
#24887=B_SPLINE_CURVE_WITH_KNOTS('',3,(#375943,#375944,#375945,#375946,
#375947,#375948,#375949),.UNSPECIFIED.,.F.,.F.,(4,3,4),(0.,2.5000002149412E-5,
9.54746331310773E-5),.UNSPECIFIED.);
#24888=B_SPLINE_CURVE_WITH_KNOTS('',3,(#375953,#375954,#375955,#375956,
#375957,#375958,#375959),.UNSPECIFIED.,.F.,.F.,(4,3,4),(0.,2.50000024491138E-5,
9.54746329568076E-5),.UNSPECIFIED.);
#24889=B_SPLINE_CURVE_WITH_KNOTS('',3,(#375963,#375964,#375965,#375966,
#375967,#375968,#375969),.UNSPECIFIED.,.F.,.F.,(4,3,4),(4.33680868994202E-19,
2.5000002149412E-5,9.54746331310777E-5),.UNSPECIFIED.);
#24890=B_SPLINE_CURVE_WITH_KNOTS('',3,(#375973,#375974,#375975,#375976,
#375977,#375978,#375979),.UNSPECIFIED.,.F.,.F.,(4,3,4),(0.,2.50000024491138E-5,
9.54746329568077E-5),.UNSPECIFIED.);
#24891=B_SPLINE_CURVE_WITH_KNOTS('',3,(#375983,#375984,#375985,#375986,
#375987,#375988,#375989),.UNSPECIFIED.,.F.,.F.,(4,3,4),(4.33680868994202E-19,
2.5000002149412E-5,9.54746331310777E-5),.UNSPECIFIED.);
#24892=B_SPLINE_CURVE_WITH_KNOTS('',3,(#375993,#375994,#375995,#375996,
#375997,#375998,#375999),.UNSPECIFIED.,.F.,.F.,(4,3,4),(0.,2.50000024491139E-5,
9.5474632956808E-5),.UNSPECIFIED.);
#24893=B_SPLINE_CURVE_WITH_KNOTS('',3,(#376003,#376004,#376005,#376006,
#376007,#376008,#376009),.UNSPECIFIED.,.F.,.F.,(4,3,4),(4.33680868994202E-19,
2.50000021494121E-5,9.54746331310776E-5),.UNSPECIFIED.);
#24894=B_SPLINE_CURVE_WITH_KNOTS('',3,(#376013,#376014,#376015,#376016,
#376017,#376018,#376019),.UNSPECIFIED.,.F.,.F.,(4,3,4),(0.,2.50000024491141E-5,
9.5474632956808E-5),.UNSPECIFIED.);
#24895=B_SPLINE_CURVE_WITH_KNOTS('',3,(#376023,#376024,#376025,#376026,
#376027,#376028,#376029),.UNSPECIFIED.,.F.,.F.,(4,3,4),(0.,2.50000021494123E-5,
9.54746331310777E-5),.UNSPECIFIED.);
#24896=B_SPLINE_CURVE_WITH_KNOTS('',3,(#376033,#376034,#376035,#376036,
#376037,#376038,#376039),.UNSPECIFIED.,.F.,.F.,(4,3,4),(0.,2.50000024491141E-5,
9.54746329568078E-5),.UNSPECIFIED.);
#24897=B_SPLINE_CURVE_WITH_KNOTS('',3,(#376043,#376044,#376045,#376046,
#376047,#376048,#376049),.UNSPECIFIED.,.F.,.F.,(4,3,4),(2.16840434497101E-19,
2.50000021494118E-5,9.54746331310777E-5),.UNSPECIFIED.);
#24898=B_SPLINE_CURVE_WITH_KNOTS('',3,(#376053,#376054,#376055,#376056,
#376057,#376058,#376059),.UNSPECIFIED.,.F.,.F.,(4,3,4),(0.,2.50000024491138E-5,
9.54746329568075E-5),.UNSPECIFIED.);
#24899=B_SPLINE_CURVE_WITH_KNOTS('',3,(#376063,#376064,#376065,#376066,
#376067,#376068,#376069),.UNSPECIFIED.,.F.,.F.,(4,3,4),(2.16840434497101E-19,
2.5000002149412E-5,9.54746331310779E-5),.UNSPECIFIED.);
#24900=B_SPLINE_CURVE_WITH_KNOTS('',3,(#376073,#376074,#376075,#376076,
#376077,#376078,#376079),.UNSPECIFIED.,.F.,.F.,(4,3,4),(0.,2.5000002449114E-5,
9.54746329568079E-5),.UNSPECIFIED.);
#24901=B_SPLINE_CURVE_WITH_KNOTS('',3,(#376083,#376084,#376085,#376086,
#376087,#376088,#376089),.UNSPECIFIED.,.F.,.F.,(4,3,4),(2.16840434497101E-19,
2.50000021494118E-5,9.54746331310775E-5),.UNSPECIFIED.);
#24902=B_SPLINE_CURVE_WITH_KNOTS('',3,(#376093,#376094,#376095,#376096,
#376097,#376098,#376099),.UNSPECIFIED.,.F.,.F.,(4,3,4),(0.,2.50000024491142E-5,
9.54746329568079E-5),.UNSPECIFIED.);
#24903=B_SPLINE_CURVE_WITH_KNOTS('',3,(#376103,#376104,#376105,#376106,
#376107,#376108,#376109),.UNSPECIFIED.,.F.,.F.,(4,3,4),(2.16840434497101E-19,
2.50000021494119E-5,9.54746331310776E-5),.UNSPECIFIED.);
#24904=B_SPLINE_CURVE_WITH_KNOTS('',3,(#376113,#376114,#376115,#376116,
#376117,#376118,#376119),.UNSPECIFIED.,.F.,.F.,(4,3,4),(0.,2.50000024491138E-5,
9.54746329568075E-5),.UNSPECIFIED.);
#24905=B_SPLINE_CURVE_WITH_KNOTS('',3,(#376123,#376124,#376125,#376126,
#376127,#376128,#376129),.UNSPECIFIED.,.F.,.F.,(4,3,4),(2.16840434497101E-19,
2.50000021494119E-5,9.54746331310776E-5),.UNSPECIFIED.);
#24906=B_SPLINE_CURVE_WITH_KNOTS('',3,(#376133,#376134,#376135,#376136,
#376137,#376138,#376139),.UNSPECIFIED.,.F.,.F.,(4,3,4),(0.,2.50000024491141E-5,
9.54746329568079E-5),.UNSPECIFIED.);
#24907=B_SPLINE_CURVE_WITH_KNOTS('',3,(#376143,#376144,#376145,#376146,
#376147,#376148,#376149),.UNSPECIFIED.,.F.,.F.,(4,3,4),(2.16840434497101E-19,
2.50000021494117E-5,9.54746331310775E-5),.UNSPECIFIED.);
#24908=B_SPLINE_CURVE_WITH_KNOTS('',3,(#376153,#376154,#376155,#376156,
#376157,#376158,#376159),.UNSPECIFIED.,.F.,.F.,(4,3,4),(0.,2.50000024491134E-5,
9.54746329568077E-5),.UNSPECIFIED.);
#24909=B_SPLINE_CURVE_WITH_KNOTS('',3,(#376163,#376164,#376165,#376166,
#376167,#376168,#376169),.UNSPECIFIED.,.F.,.F.,(4,3,4),(0.,2.5000002149412E-5,
9.54746331310777E-5),.UNSPECIFIED.);
#24910=B_SPLINE_CURVE_WITH_KNOTS('',3,(#376173,#376174,#376175,#376176,
#376177,#376178,#376179),.UNSPECIFIED.,.F.,.F.,(4,3,4),(0.,2.50000024491141E-5,
9.54746329568077E-5),.UNSPECIFIED.);
#24911=B_SPLINE_CURVE_WITH_KNOTS('',3,(#376183,#376184,#376185,#376186,
#376187,#376188,#376189),.UNSPECIFIED.,.F.,.F.,(4,3,4),(1.0842021724855E-19,
2.50000021494119E-5,9.54746331310777E-5),.UNSPECIFIED.);
#24912=B_SPLINE_CURVE_WITH_KNOTS('',3,(#376193,#376194,#376195,#376196,
#376197,#376198,#376199),.UNSPECIFIED.,.F.,.F.,(4,3,4),(0.,2.50000024491137E-5,
9.54746329568078E-5),.UNSPECIFIED.);
#24913=B_SPLINE_CURVE_WITH_KNOTS('',3,(#376203,#376204,#376205,#376206,
#376207,#376208,#376209),.UNSPECIFIED.,.F.,.F.,(4,3,4),(1.0842021724855E-19,
2.50000021494122E-5,9.54746331310776E-5),.UNSPECIFIED.);
#24914=B_SPLINE_CURVE_WITH_KNOTS('',3,(#376213,#376214,#376215,#376216,
#376217,#376218,#376219),.UNSPECIFIED.,.F.,.F.,(4,3,4),(0.,2.5000002449114E-5,
9.54746329568078E-5),.UNSPECIFIED.);
#24915=B_SPLINE_CURVE_WITH_KNOTS('',3,(#376223,#376224,#376225,#376226,
#376227,#376228,#376229),.UNSPECIFIED.,.F.,.F.,(4,3,4),(1.0842021724855E-19,
2.50000021494121E-5,9.54746331310776E-5),.UNSPECIFIED.);
#24916=B_SPLINE_CURVE_WITH_KNOTS('',3,(#376233,#376234,#376235,#376236,
#376237,#376238,#376239),.UNSPECIFIED.,.F.,.F.,(4,3,4),(0.,2.50000024491138E-5,
9.54746329568077E-5),.UNSPECIFIED.);
#24917=B_SPLINE_CURVE_WITH_KNOTS('',3,(#376243,#376244,#376245,#376246,
#376247,#376248,#376249),.UNSPECIFIED.,.F.,.F.,(4,3,4),(1.0842021724855E-19,
2.50000021494122E-5,9.54746331310776E-5),.UNSPECIFIED.);
#24918=B_SPLINE_CURVE_WITH_KNOTS('',3,(#376253,#376254,#376255,#376256,
#376257,#376258,#376259),.UNSPECIFIED.,.F.,.F.,(4,3,4),(0.,2.50000024491135E-5,
9.54746329568075E-5),.UNSPECIFIED.);
#24919=B_SPLINE_CURVE_WITH_KNOTS('',3,(#376263,#376264,#376265,#376266,
#376267,#376268,#376269),.UNSPECIFIED.,.F.,.F.,(4,3,4),(1.0842021724855E-19,
2.5000002149412E-5,9.54746331310773E-5),.UNSPECIFIED.);
#24920=B_SPLINE_CURVE_WITH_KNOTS('',3,(#376273,#376274,#376275,#376276,
#376277,#376278,#376279),.UNSPECIFIED.,.F.,.F.,(4,3,4),(0.,2.5000002449114E-5,
9.54746329568076E-5),.UNSPECIFIED.);
#24921=B_SPLINE_CURVE_WITH_KNOTS('',3,(#376283,#376284,#376285,#376286,
#376287,#376288,#376289),.UNSPECIFIED.,.F.,.F.,(4,3,4),(1.01643953670516E-19,
2.50000021494119E-5,9.54746331310775E-5),.UNSPECIFIED.);
#24922=B_SPLINE_CURVE_WITH_KNOTS('',3,(#376293,#376294,#376295,#376296,
#376297,#376298,#376299),.UNSPECIFIED.,.F.,.F.,(4,3,4),(0.,2.50000024491139E-5,
9.54746329568077E-5),.UNSPECIFIED.);
#24923=B_SPLINE_CURVE_WITH_KNOTS('',3,(#376303,#376304,#376305,#376306,
#376307,#376308,#376309),.UNSPECIFIED.,.F.,.F.,(4,3,4),(8.13151629364128E-20,
2.5000002149412E-5,9.54746331310775E-5),.UNSPECIFIED.);
#24924=B_SPLINE_CURVE_WITH_KNOTS('',3,(#376313,#376314,#376315,#376316,
#376317,#376318,#376319),.UNSPECIFIED.,.F.,.F.,(4,3,4),(0.,2.50000024491139E-5,
9.54746329568076E-5),.UNSPECIFIED.);
#24925=B_SPLINE_CURVE_WITH_KNOTS('',3,(#376323,#376324,#376325,#376326,
#376327,#376328,#376329),.UNSPECIFIED.,.F.,.F.,(4,3,4),(5.42101086242752E-20,
2.50000021494122E-5,9.54746331310777E-5),.UNSPECIFIED.);
#24926=B_SPLINE_CURVE_WITH_KNOTS('',3,(#376333,#376334,#376335,#376336,
#376337,#376338,#376339),.UNSPECIFIED.,.F.,.F.,(4,3,4),(0.,2.5000002449114E-5,
9.54746329568076E-5),.UNSPECIFIED.);
#24927=B_SPLINE_CURVE_WITH_KNOTS('',3,(#376343,#376344,#376345,#376346,
#376347,#376348,#376349),.UNSPECIFIED.,.F.,.F.,(4,3,4),(4.37055868292169E-19,
2.50000021494117E-5,9.54746331310773E-5),.UNSPECIFIED.);
#24928=B_SPLINE_CURVE_WITH_KNOTS('',3,(#376353,#376354,#376355,#376356,
#376357,#376358,#376359),.UNSPECIFIED.,.F.,.F.,(4,3,4),(0.,2.50000024491139E-5,
9.54746329568076E-5),.UNSPECIFIED.);
#24929=B_SPLINE_CURVE_WITH_KNOTS('',3,(#376363,#376364,#376365,#376366,
#376367,#376368,#376369),.UNSPECIFIED.,.F.,.F.,(4,3,4),(4.47028007668187E-19,
2.50000021494118E-5,9.54746331310774E-5),.UNSPECIFIED.);
#24930=B_SPLINE_CURVE_WITH_KNOTS('',3,(#376373,#376374,#376375,#376376,
#376377,#376378,#376379),.UNSPECIFIED.,.F.,.F.,(4,3,4),(0.,2.50000024491138E-5,
9.54746329568077E-5),.UNSPECIFIED.);
#24931=B_SPLINE_CURVE_WITH_KNOTS('',3,(#376383,#376384,#376385,#376386,
#376387,#376388,#376389),.UNSPECIFIED.,.F.,.F.,(4,3,4),(4.33680868994202E-19,
2.50000021494119E-5,9.54746331310775E-5),.UNSPECIFIED.);
#24932=B_SPLINE_CURVE_WITH_KNOTS('',3,(#376393,#376394,#376395,#376396,
#376397,#376398,#376399),.UNSPECIFIED.,.F.,.F.,(4,3,4),(0.,2.50000024491143E-5,
9.54746329568081E-5),.UNSPECIFIED.);
#24933=B_SPLINE_CURVE_WITH_KNOTS('',3,(#376403,#376404,#376405,#376406,
#376407,#376408,#376409),.UNSPECIFIED.,.F.,.F.,(4,3,4),(4.33680868994202E-19,
2.50000021494122E-5,9.54746331310777E-5),.UNSPECIFIED.);
#24934=B_SPLINE_CURVE_WITH_KNOTS('',3,(#376413,#376414,#376415,#376416,
#376417,#376418,#376419),.UNSPECIFIED.,.F.,.F.,(4,3,4),(0.,2.5000002449114E-5,
9.54746329568078E-5),.UNSPECIFIED.);
#24935=B_SPLINE_CURVE_WITH_KNOTS('',3,(#376423,#376424,#376425,#376426,
#376427,#376428,#376429),.UNSPECIFIED.,.F.,.F.,(4,3,4),(4.33680868994202E-19,
2.5000002149412E-5,9.54746331310774E-5),.UNSPECIFIED.);
#24936=B_SPLINE_CURVE_WITH_KNOTS('',3,(#376433,#376434,#376435,#376436,
#376437,#376438,#376439),.UNSPECIFIED.,.F.,.F.,(4,3,4),(0.,2.50000024491139E-5,
9.54746329568078E-5),.UNSPECIFIED.);
#24937=B_SPLINE_CURVE_WITH_KNOTS('',3,(#376443,#376444,#376445,#376446,
#376447,#376448,#376449),.UNSPECIFIED.,.F.,.F.,(4,3,4),(4.33680868994202E-19,
2.50000021494118E-5,9.54746331310773E-5),.UNSPECIFIED.);
#24938=B_SPLINE_CURVE_WITH_KNOTS('',3,(#376453,#376454,#376455,#376456,
#376457,#376458,#376459),.UNSPECIFIED.,.F.,.F.,(4,3,4),(0.,2.50000024491138E-5,
9.54746329568079E-5),.UNSPECIFIED.);
#24939=B_SPLINE_CURVE_WITH_KNOTS('',3,(#376463,#376464,#376465,#376466,
#376467,#376468,#376469),.UNSPECIFIED.,.F.,.F.,(4,3,4),(4.33680868994202E-19,
2.50000021494121E-5,9.54746331310776E-5),.UNSPECIFIED.);
#24940=B_SPLINE_CURVE_WITH_KNOTS('',3,(#376473,#376474,#376475,#376476,
#376477,#376478,#376479),.UNSPECIFIED.,.F.,.F.,(4,3,4),(0.,2.50000024491139E-5,
9.54746329568078E-5),.UNSPECIFIED.);
#24941=B_SPLINE_CURVE_WITH_KNOTS('',3,(#376483,#376484,#376485,#376486,
#376487,#376488,#376489),.UNSPECIFIED.,.F.,.F.,(4,3,4),(0.,2.50000021494121E-5,
9.54746331310774E-5),.UNSPECIFIED.);
#24942=B_SPLINE_CURVE_WITH_KNOTS('',3,(#376493,#376494,#376495,#376496,
#376497,#376498,#376499),.UNSPECIFIED.,.F.,.F.,(4,3,4),(0.,2.50000024491139E-5,
9.54746329568077E-5),.UNSPECIFIED.);
#24943=B_SPLINE_CURVE_WITH_KNOTS('',3,(#376503,#376504,#376505,#376506,
#376507,#376508,#376509),.UNSPECIFIED.,.F.,.F.,(4,3,4),(4.33680868994202E-19,
2.50000021494123E-5,9.54746331310777E-5),.UNSPECIFIED.);
#24944=B_SPLINE_CURVE_WITH_KNOTS('',3,(#376513,#376514,#376515,#376516,
#376517,#376518,#376519),.UNSPECIFIED.,.F.,.F.,(4,3,4),(0.,2.50000024491139E-5,
9.5474632956808E-5),.UNSPECIFIED.);
#24945=B_SPLINE_CURVE_WITH_KNOTS('',3,(#376523,#376524,#376525,#376526,
#376527,#376528,#376529),.UNSPECIFIED.,.F.,.F.,(4,3,4),(4.33680868994202E-19,
2.50000021494122E-5,9.54746331310776E-5),.UNSPECIFIED.);
#24946=B_SPLINE_CURVE_WITH_KNOTS('',3,(#376533,#376534,#376535,#376536,
#376537,#376538,#376539),.UNSPECIFIED.,.F.,.F.,(4,3,4),(0.,2.50000024491141E-5,
9.5474632956808E-5),.UNSPECIFIED.);
#24947=B_SPLINE_CURVE_WITH_KNOTS('',3,(#376543,#376544,#376545,#376546,
#376547,#376548,#376549),.UNSPECIFIED.,.F.,.F.,(4,3,4),(2.16840434497101E-19,
2.50000021494118E-5,9.54746331310776E-5),.UNSPECIFIED.);
#24948=B_SPLINE_CURVE_WITH_KNOTS('',3,(#376553,#376554,#376555,#376556,
#376557,#376558,#376559),.UNSPECIFIED.,.F.,.F.,(4,3,4),(0.,2.50000024491139E-5,
9.54746329568075E-5),.UNSPECIFIED.);
#24949=B_SPLINE_CURVE_WITH_KNOTS('',3,(#376563,#376564,#376565,#376566,
#376567,#376568,#376569),.UNSPECIFIED.,.F.,.F.,(4,3,4),(2.16840434497101E-19,
2.50000021494121E-5,9.54746331310777E-5),.UNSPECIFIED.);
#24950=B_SPLINE_CURVE_WITH_KNOTS('',3,(#376573,#376574,#376575,#376576,
#376577,#376578,#376579),.UNSPECIFIED.,.F.,.F.,(4,3,4),(0.,2.50000024491136E-5,
9.54746329568077E-5),.UNSPECIFIED.);
#24951=B_SPLINE_CURVE_WITH_KNOTS('',3,(#376583,#376584,#376585,#376586,
#376587,#376588,#376589),.UNSPECIFIED.,.F.,.F.,(4,3,4),(2.16840434497101E-19,
2.50000021494119E-5,9.54746331310775E-5),.UNSPECIFIED.);
#24952=B_SPLINE_CURVE_WITH_KNOTS('',3,(#376593,#376594,#376595,#376596,
#376597,#376598,#376599),.UNSPECIFIED.,.F.,.F.,(4,3,4),(0.,2.50000024491136E-5,
9.54746329568076E-5),.UNSPECIFIED.);
#24953=B_SPLINE_CURVE_WITH_KNOTS('',3,(#376603,#376604,#376605,#376606,
#376607,#376608,#376609),.UNSPECIFIED.,.F.,.F.,(4,3,4),(2.16840434497101E-19,
2.50000021494119E-5,9.54746331310777E-5),.UNSPECIFIED.);
#24954=B_SPLINE_CURVE_WITH_KNOTS('',3,(#376613,#376614,#376615,#376616,
#376617,#376618,#376619),.UNSPECIFIED.,.F.,.F.,(4,3,4),(0.,2.50000024491141E-5,
9.54746329568079E-5),.UNSPECIFIED.);
#24955=B_SPLINE_CURVE_WITH_KNOTS('',3,(#376623,#376624,#376625,#376626,
#376627,#376628,#376629),.UNSPECIFIED.,.F.,.F.,(4,3,4),(2.16840434497101E-19,
2.50000021494119E-5,9.54746331310777E-5),.UNSPECIFIED.);
#24956=B_SPLINE_CURVE_WITH_KNOTS('',3,(#376633,#376634,#376635,#376636,
#376637,#376638,#376639),.UNSPECIFIED.,.F.,.F.,(4,3,4),(0.,2.50000024491142E-5,
9.54746329568078E-5),.UNSPECIFIED.);
#24957=B_SPLINE_CURVE_WITH_KNOTS('',3,(#376643,#376644,#376645,#376646,
#376647,#376648,#376649),.UNSPECIFIED.,.F.,.F.,(4,3,4),(0.,2.50000021494122E-5,
9.54746331310779E-5),.UNSPECIFIED.);
#24958=B_SPLINE_CURVE_WITH_KNOTS('',3,(#376653,#376654,#376655,#376656,
#376657,#376658,#376659),.UNSPECIFIED.,.F.,.F.,(4,3,4),(0.,2.5000002449114E-5,
9.54746329568077E-5),.UNSPECIFIED.);
#24959=B_SPLINE_CURVE_WITH_KNOTS('',3,(#376663,#376664,#376665,#376666,
#376667,#376668,#376669),.UNSPECIFIED.,.F.,.F.,(4,3,4),(2.16840434497101E-19,
2.50000021494119E-5,9.54746331310779E-5),.UNSPECIFIED.);
#24960=B_SPLINE_CURVE_WITH_KNOTS('',3,(#376673,#376674,#376675,#376676,
#376677,#376678,#376679),.UNSPECIFIED.,.F.,.F.,(4,3,4),(0.,2.50000024491139E-5,
9.54746329568078E-5),.UNSPECIFIED.);
#24961=B_SPLINE_CURVE_WITH_KNOTS('',3,(#376683,#376684,#376685,#376686,
#376687,#376688,#376689),.UNSPECIFIED.,.F.,.F.,(4,3,4),(2.16840434497101E-19,
2.50000021494118E-5,9.54746331310776E-5),.UNSPECIFIED.);
#24962=B_SPLINE_CURVE_WITH_KNOTS('',3,(#376693,#376694,#376695,#376696,
#376697,#376698,#376699),.UNSPECIFIED.,.F.,.F.,(4,3,4),(0.,2.50000024491143E-5,
9.54746329568081E-5),.UNSPECIFIED.);
#24963=B_SPLINE_CURVE_WITH_KNOTS('',3,(#376703,#376704,#376705,#376706,
#376707,#376708,#376709),.UNSPECIFIED.,.F.,.F.,(4,3,4),(1.0842021724855E-19,
2.50000021494121E-5,9.54746331310775E-5),.UNSPECIFIED.);
#24964=B_SPLINE_CURVE_WITH_KNOTS('',3,(#376713,#376714,#376715,#376716,
#376717,#376718,#376719),.UNSPECIFIED.,.F.,.F.,(4,3,4),(0.,2.50000024491141E-5,
9.54746329568079E-5),.UNSPECIFIED.);
#24965=B_SPLINE_CURVE_WITH_KNOTS('',3,(#376723,#376724,#376725,#376726,
#376727,#376728,#376729),.UNSPECIFIED.,.F.,.F.,(4,3,4),(1.62630325872826E-19,
2.5000002149412E-5,9.54746331310773E-5),.UNSPECIFIED.);
#24966=B_SPLINE_CURVE_WITH_KNOTS('',3,(#376733,#376734,#376735,#376736,
#376737,#376738,#376739),.UNSPECIFIED.,.F.,.F.,(4,3,4),(0.,2.50000024491141E-5,
9.5474632956808E-5),.UNSPECIFIED.);
#24967=B_SPLINE_CURVE_WITH_KNOTS('',3,(#376743,#376744,#376745,#376746,
#376747,#376748,#376749),.UNSPECIFIED.,.F.,.F.,(4,3,4),(1.0842021724855E-19,
2.50000021494122E-5,9.54746331310777E-5),.UNSPECIFIED.);
#24968=B_SPLINE_CURVE_WITH_KNOTS('',3,(#376753,#376754,#376755,#376756,
#376757,#376758,#376759),.UNSPECIFIED.,.F.,.F.,(4,3,4),(0.,2.50000024491138E-5,
9.54746329568075E-5),.UNSPECIFIED.);
#24969=B_SPLINE_CURVE_WITH_KNOTS('',3,(#376763,#376764,#376765,#376766,
#376767,#376768,#376769),.UNSPECIFIED.,.F.,.F.,(4,3,4),(1.0842021724855E-19,
2.50000021494118E-5,9.54746331310775E-5),.UNSPECIFIED.);
#24970=B_SPLINE_CURVE_WITH_KNOTS('',3,(#376772,#376773,#376774,#376775,
#376776,#376777,#376778),.UNSPECIFIED.,.F.,.F.,(4,3,4),(0.,2.50000024491137E-5,
9.54746329568074E-5),.UNSPECIFIED.);
#24971=B_SPLINE_CURVE_WITH_KNOTS('',3,(#378259,#378260,#378261,#378262,
#378263,#378264,#378265,#378266,#378267,#378268,#378269,#378270,#378271,
#378272,#378273,#378274,#378275,#378276,#378277,#378278,#378279,#378280,
#378281,#378282,#378283,#378284,#378285,#378286,#378287,#378288,#378289,
#378290,#378291,#378292,#378293,#378294,#378295,#378296,#378297,#378298,
#378299,#378300,#378301,#378302,#378303,#378304,#378305,#378306,#378307),
 .UNSPECIFIED.,.F.,.F.,(4,3,3,3,3,3,3,3,3,3,3,3,3,3,3,3,4),(0.,1.53100299373414E-6,
4.52554775678511E-6,7.01151246291606E-6,9.267529338009E-6,1.03084066197173E-5,
1.17138990826862E-5,1.22284894984074E-5,1.30315035324817E-5,1.38363728497813E-5,
1.40464197777495E-5,1.5459774956464E-5,1.62073588704069E-5,1.92092968712803E-5,
1.95234416882555E-5,2.37637844577586E-5,2.61487188977262E-5),
 .UNSPECIFIED.);
#24972=B_SPLINE_CURVE_WITH_KNOTS('',3,(#378315,#378316,#378317,#378318),
 .UNSPECIFIED.,.F.,.F.,(4,4),(4.52388553334502E-19,9.54361881492177E-5),
 .UNSPECIFIED.);
#24973=B_SPLINE_CURVE_WITH_KNOTS('',3,(#378320,#378321,#378322,#378323,
#378324,#378325,#378326),.UNSPECIFIED.,.F.,.F.,(4,3,4),(8.470329472543E-22,
6.9863024419149E-5,0.000113969974038089),.UNSPECIFIED.);
#24974=B_SPLINE_CURVE_WITH_KNOTS('',3,(#378330,#378331,#378332,#378333),
 .UNSPECIFIED.,.F.,.F.,(4,4),(0.,9.54361881492174E-5),.UNSPECIFIED.);
#24975=B_SPLINE_CURVE_WITH_KNOTS('',3,(#378338,#378339,#378340,#378341,
#378342,#378343,#378344),.UNSPECIFIED.,.F.,.F.,(4,3,4),(0.,4.41069704323469E-5,
0.000113970027818833),.UNSPECIFIED.);
#24976=B_SPLINE_CURVE_WITH_KNOTS('',3,(#379924,#379925,#379926,#379927),
 .UNSPECIFIED.,.F.,.F.,(4,4),(4.78962492688793E-19,0.00010938435327491),
 .UNSPECIFIED.);
#24977=B_SPLINE_CURVE_WITH_KNOTS('',3,(#379929,#379930,#379931,#379932),
 .UNSPECIFIED.,.F.,.F.,(4,4),(0.,0.000109384345496908),.UNSPECIFIED.);
#24978=B_SPLINE_CURVE_WITH_KNOTS('',3,(#379946,#379947,#379948,#379949,
#379950,#379951,#379952,#379953,#379954,#379955,#379956,#379957,#379958,
#379959,#379960,#379961,#379962,#379963,#379964,#379965,#379966,#379967,
#379968,#379969,#379970,#379971,#379972,#379973,#379974,#379975,#379976),
 .UNSPECIFIED.,.F.,.F.,(4,3,3,3,3,3,3,3,3,3,4),(0.,3.95507910396971E-6,
7.53768426604197E-6,1.19904533335326E-5,1.40475043392548E-5,1.5145210427592E-5,
1.6786627281411E-5,1.69621513005302E-5,1.81338315460649E-5,1.98906334656487E-5,
2.06132424588165E-5),.UNSPECIFIED.);
#24979=B_SPLINE_CURVE_WITH_KNOTS('',3,(#380032,#380033,#380034,#380035,
#380036,#380037,#380038,#380039,#380040,#380041,#380042,#380043,#380044,
#380045,#380046,#380047,#380048,#380049,#380050,#380051,#380052,#380053,
#380054,#380055,#380056,#380057,#380058,#380059,#380060,#380061,#380062,
#380063,#380064,#380065),.UNSPECIFIED.,.F.,.F.,(4,3,3,3,3,3,3,3,3,3,3,4),
(1.35525271560688E-19,2.0962399272944E-6,3.17176647120221E-6,4.82636181944412E-6,
5.01000917339962E-6,6.13126454147496E-6,8.60486650288856E-6,9.21144281170493E-6,
1.24722301136011E-5,1.42666454787857E-5,2.04670653756765E-5,2.08026438176807E-5),
 .UNSPECIFIED.);
#24980=B_SPLINE_CURVE_WITH_KNOTS('',3,(#380139,#380140,#380141,#380142),
 .UNSPECIFIED.,.F.,.F.,(4,4),(0.,9.54361881492174E-5),.UNSPECIFIED.);
#24981=B_SPLINE_CURVE_WITH_KNOTS('',3,(#380147,#380148,#380149,#380150,
#380151,#380152,#380153),.UNSPECIFIED.,.F.,.F.,(4,3,4),(0.,4.41069704323468E-5,
0.000113970027818833),.UNSPECIFIED.);
#24982=B_SPLINE_CURVE_WITH_KNOTS('',3,(#380159,#380160,#380161,#380162),
 .UNSPECIFIED.,.F.,.F.,(4,4),(4.5436350575631E-19,9.54361881492177E-5),
 .UNSPECIFIED.);
#24983=B_SPLINE_CURVE_WITH_KNOTS('',3,(#380166,#380167,#380168,#380169,
#380170,#380171,#380172),.UNSPECIFIED.,.F.,.F.,(4,3,4),(0.,6.98630244191492E-5,
0.000113969974038089),.UNSPECIFIED.);
#24984=B_SPLINE_CURVE_WITH_KNOTS('',3,(#380175,#380176,#380177,#380178,
#380179,#380180,#380181,#380182,#380183,#380184,#380185,#380186,#380187,
#380188,#380189,#380190,#380191,#380192,#380193,#380194,#380195,#380196,
#380197,#380198,#380199,#380200,#380201,#380202,#380203,#380204,#380205,
#380206,#380207,#380208,#380209,#380210,#380211,#380212,#380213,#380214,
#380215,#380216,#380217,#380218,#380219,#380220,#380221,#380222,#380223),
 .UNSPECIFIED.,.F.,.F.,(4,3,3,3,3,3,3,3,3,3,3,3,3,3,3,3,4),(0.,1.53100299373415E-6,
4.52554775679471E-6,7.01151246291607E-6,9.26752933799583E-6,1.03084066197174E-5,
1.17138990826861E-5,1.22284894984074E-5,1.30315035324818E-5,1.38363728497812E-5,
1.40464197777495E-5,1.5459774956464E-5,1.62073588704069E-5,1.92092968712868E-5,
1.95234416882554E-5,2.37637844577581E-5,2.6148718897726E-5),
 .UNSPECIFIED.);
#24985=B_SPLINE_CURVE_WITH_KNOTS('',3,(#380238,#380239,#380240,#380241,
#380242,#380243,#380244,#380245,#380246,#380247,#380248,#380249,#380250,
#380251,#380252,#380253,#380254,#380255,#380256,#380257,#380258,#380259,
#380260,#380261,#380262,#380263,#380264,#380265,#380266,#380267,#380268),
 .UNSPECIFIED.,.F.,.F.,(4,3,3,3,3,3,3,3,3,3,4),(0.,3.955079103984E-6,7.53768426604202E-6,
1.19904533335351E-5,1.40475043392586E-5,1.51452104275965E-5,1.67866272814136E-5,
1.69621513005359E-5,1.81338315460712E-5,1.98906334656503E-5,2.06132424588245E-5),
 .UNSPECIFIED.);
#24986=B_SPLINE_CURVE_WITH_KNOTS('',3,(#380271,#380272,#380273,#380274),
 .UNSPECIFIED.,.F.,.F.,(4,4),(4.97582654080651E-19,0.00010938435327491),
 .UNSPECIFIED.);
#24987=B_SPLINE_CURVE_WITH_KNOTS('',3,(#380301,#380302,#380303,#380304,
#380305,#380306,#380307,#380308,#380309,#380310,#380311,#380312,#380313,
#380314,#380315,#380316,#380317,#380318,#380319,#380320,#380321,#380322,
#380323,#380324,#380325,#380326,#380327,#380328,#380329,#380330,#380331,
#380332,#380333,#380334),.UNSPECIFIED.,.F.,.F.,(4,3,3,3,3,3,3,3,3,3,3,4),
(1.35525271560688E-19,2.09623992729445E-6,3.17176647120226E-6,4.82636181942471E-6,
5.01000917339969E-6,6.13126454147507E-6,8.60486650288873E-6,9.21144281170513E-6,
1.24722301135971E-5,1.4266645478786E-5,2.04670653756875E-5,2.0802643817681E-5),
 .UNSPECIFIED.);
#24988=B_SPLINE_CURVE_WITH_KNOTS('',3,(#380335,#380336,#380337,#380338),
 .UNSPECIFIED.,.F.,.F.,(4,4),(0.,0.000109384345496908),.UNSPECIFIED.);
#24989=B_SPLINE_CURVE_WITH_KNOTS('',3,(#380443,#380444,#380445,#380446),
 .UNSPECIFIED.,.F.,.F.,(4,4),(0.,9.54361881492173E-5),.UNSPECIFIED.);
#24990=B_SPLINE_CURVE_WITH_KNOTS('',3,(#380451,#380452,#380453,#380454,
#380455,#380456,#380457),.UNSPECIFIED.,.F.,.F.,(4,3,4),(0.,4.41069704323468E-5,
0.000113970027818833),.UNSPECIFIED.);
#24991=B_SPLINE_CURVE_WITH_KNOTS('',3,(#380463,#380464,#380465,#380466),
 .UNSPECIFIED.,.F.,.F.,(4,4),(4.47028007668187E-19,9.54361881492177E-5),
 .UNSPECIFIED.);
#24992=B_SPLINE_CURVE_WITH_KNOTS('',3,(#380470,#380471,#380472,#380473,
#380474,#380475,#380476),.UNSPECIFIED.,.F.,.F.,(4,3,4),(0.,6.98630244191489E-5,
0.000113969974038089),.UNSPECIFIED.);
#24993=B_SPLINE_CURVE_WITH_KNOTS('',3,(#380479,#380480,#380481,#380482,
#380483,#380484,#380485,#380486,#380487,#380488,#380489,#380490,#380491,
#380492,#380493,#380494,#380495,#380496,#380497,#380498,#380499,#380500,
#380501,#380502,#380503,#380504,#380505,#380506,#380507,#380508,#380509,
#380510,#380511,#380512,#380513,#380514,#380515,#380516,#380517,#380518,
#380519,#380520,#380521,#380522,#380523,#380524,#380525,#380526,#380527),
 .UNSPECIFIED.,.F.,.F.,(4,3,3,3,3,3,3,3,3,3,3,3,3,3,3,3,4),(0.,1.53100299373405E-6,
4.52554775679585E-6,7.01151246291601E-6,9.26752933800506E-6,1.03084066197174E-5,
1.17138990826862E-5,1.22284894984075E-5,1.30315035324818E-5,1.38363728497813E-5,
1.40464197777496E-5,1.54597749564641E-5,1.62073588704069E-5,1.92092968712673E-5,
1.95234416882556E-5,2.37637844577608E-5,2.61487188977265E-5),
 .UNSPECIFIED.);
#24994=B_SPLINE_CURVE_WITH_KNOTS('',3,(#380542,#380543,#380544,#380545,
#380546,#380547,#380548,#380549,#380550,#380551,#380552,#380553,#380554,
#380555,#380556,#380557,#380558,#380559,#380560,#380561,#380562,#380563,
#380564,#380565,#380566,#380567,#380568,#380569,#380570,#380571,#380572),
 .UNSPECIFIED.,.F.,.F.,(4,3,3,3,3,3,3,3,3,3,4),(0.,3.95507910397942E-6,
7.53768426604206E-6,1.19904533335352E-5,1.40475043392586E-5,1.51452104275965E-5,
1.67866272814147E-5,1.69621513005359E-5,1.81338315460713E-5,1.9890633465653E-5,
2.06132424588247E-5),.UNSPECIFIED.);
#24995=B_SPLINE_CURVE_WITH_KNOTS('',3,(#380575,#380576,#380577,#380578),
 .UNSPECIFIED.,.F.,.F.,(4,4),(4.73369422993816E-19,0.00010938435327491),
 .UNSPECIFIED.);
#24996=B_SPLINE_CURVE_WITH_KNOTS('',3,(#380605,#380606,#380607,#380608,
#380609,#380610,#380611,#380612,#380613,#380614,#380615,#380616,#380617,
#380618,#380619,#380620,#380621,#380622,#380623,#380624,#380625,#380626,
#380627,#380628,#380629,#380630,#380631,#380632,#380633,#380634,#380635,
#380636,#380637,#380638),.UNSPECIFIED.,.F.,.F.,(4,3,3,3,3,3,3,3,3,3,3,4),
(1.35525271560688E-19,2.09623992729439E-6,3.17176647120221E-6,4.82636181945277E-6,
5.01000917339961E-6,6.13126454147493E-6,8.60486650288835E-6,9.21144281170465E-6,
1.24722301135837E-5,1.42666454787848E-5,2.04670653756579E-5,2.08026438176788E-5),
 .UNSPECIFIED.);
#24997=B_SPLINE_CURVE_WITH_KNOTS('',3,(#380639,#380640,#380641,#380642),
 .UNSPECIFIED.,.F.,.F.,(4,4),(0.,0.000109384345496908),.UNSPECIFIED.);
#24998=B_SPLINE_CURVE_WITH_KNOTS('',3,(#380747,#380748,#380749,#380750),
 .UNSPECIFIED.,.F.,.F.,(4,4),(0.,9.54361881492175E-5),.UNSPECIFIED.);
#24999=B_SPLINE_CURVE_WITH_KNOTS('',3,(#380755,#380756,#380757,#380758,
#380759,#380760,#380761),.UNSPECIFIED.,.F.,.F.,(4,3,4),(0.,4.41069704323466E-5,
0.000113970027818833),.UNSPECIFIED.);
#25000=B_SPLINE_CURVE_WITH_KNOTS('',3,(#380767,#380768,#380769,#380770),
 .UNSPECIFIED.,.F.,.F.,(4,4),(4.47028007668187E-19,9.5436188149218E-5),
 .UNSPECIFIED.);
#25001=B_SPLINE_CURVE_WITH_KNOTS('',3,(#380774,#380775,#380776,#380777,
#380778,#380779,#380780),.UNSPECIFIED.,.F.,.F.,(4,3,4),(0.,6.98630244191489E-5,
0.000113969974038089),.UNSPECIFIED.);
#25002=B_SPLINE_CURVE_WITH_KNOTS('',3,(#380783,#380784,#380785,#380786,
#380787,#380788,#380789,#380790,#380791,#380792,#380793,#380794,#380795,
#380796,#380797,#380798,#380799,#380800,#380801,#380802,#380803,#380804,
#380805,#380806,#380807,#380808,#380809,#380810,#380811,#380812,#380813,
#380814,#380815,#380816,#380817,#380818,#380819,#380820,#380821,#380822,
#380823,#380824,#380825,#380826,#380827,#380828,#380829,#380830,#380831),
 .UNSPECIFIED.,.F.,.F.,(4,3,3,3,3,3,3,3,3,3,3,3,3,3,3,3,4),(0.,1.53100299373417E-6,
4.52554775679147E-6,7.01151246291613E-6,9.26752933799189E-6,1.03084066197174E-5,
1.17138990826863E-5,1.22284894984075E-5,1.30315035324818E-5,1.38363728497813E-5,
1.40464197777496E-5,1.54597749564641E-5,1.6207358870407E-5,1.92092968713039E-5,
1.95234416882556E-5,2.37637844577595E-5,2.61487188977263E-5),
 .UNSPECIFIED.);
#25003=B_SPLINE_CURVE_WITH_KNOTS('',3,(#380846,#380847,#380848,#380849,
#380850,#380851,#380852,#380853,#380854,#380855,#380856,#380857,#380858,
#380859,#380860,#380861,#380862,#380863,#380864,#380865,#380866,#380867,
#380868,#380869,#380870,#380871,#380872,#380873,#380874,#380875,#380876),
 .UNSPECIFIED.,.F.,.F.,(4,3,3,3,3,3,3,3,3,3,4),(0.,3.95507910397588E-6,
7.53768426604194E-6,1.1990453333535E-5,1.40475043392586E-5,1.51452104275964E-5,
1.67866272814194E-5,1.69621513005358E-5,1.81338315460711E-5,1.9890633465654E-5,
2.06132424588243E-5),.UNSPECIFIED.);
#25004=B_SPLINE_CURVE_WITH_KNOTS('',3,(#380879,#380880,#380881,#380882),
 .UNSPECIFIED.,.F.,.F.,(4,4),(4.63171371119878E-19,0.00010938435327491),
 .UNSPECIFIED.);
#25005=B_SPLINE_CURVE_WITH_KNOTS('',3,(#380909,#380910,#380911,#380912,
#380913,#380914,#380915,#380916,#380917,#380918,#380919,#380920,#380921,
#380922,#380923,#380924,#380925,#380926,#380927,#380928,#380929,#380930,
#380931,#380932,#380933,#380934,#380935,#380936,#380937,#380938,#380939,
#380940,#380941,#380942),.UNSPECIFIED.,.F.,.F.,(4,3,3,3,3,3,3,3,3,3,3,4),
(1.62630325872826E-19,2.09623992729438E-6,3.17176647120217E-6,4.82636181944348E-6,
5.0100091733996E-6,6.13126454147498E-6,8.60486650288868E-6,9.21144281170502E-6,
1.24722301135972E-5,1.42666454787857E-5,2.04670653756983E-5,2.08026438176807E-5),
 .UNSPECIFIED.);
#25006=B_SPLINE_CURVE_WITH_KNOTS('',3,(#380943,#380944,#380945,#380946),
 .UNSPECIFIED.,.F.,.F.,(4,4),(0.,0.000109384345496908),.UNSPECIFIED.);
#25007=B_SPLINE_CURVE_WITH_KNOTS('',3,(#381051,#381052,#381053,#381054),
 .UNSPECIFIED.,.F.,.F.,(4,4),(0.,9.54361881492172E-5),.UNSPECIFIED.);
#25008=B_SPLINE_CURVE_WITH_KNOTS('',3,(#381059,#381060,#381061,#381062,
#381063,#381064,#381065),.UNSPECIFIED.,.F.,.F.,(4,3,4),(0.,4.41069704323472E-5,
0.000113970027818833),.UNSPECIFIED.);
#25009=B_SPLINE_CURVE_WITH_KNOTS('',3,(#381071,#381072,#381073,#381074),
 .UNSPECIFIED.,.F.,.F.,(4,4),(4.37055868292169E-19,9.54361881492179E-5),
 .UNSPECIFIED.);
#25010=B_SPLINE_CURVE_WITH_KNOTS('',3,(#381078,#381079,#381080,#381081,
#381082,#381083,#381084),.UNSPECIFIED.,.F.,.F.,(4,3,4),(0.,6.98630244191489E-5,
0.000113969974038089),.UNSPECIFIED.);
#25011=B_SPLINE_CURVE_WITH_KNOTS('',3,(#381087,#381088,#381089,#381090,
#381091,#381092,#381093,#381094,#381095,#381096,#381097,#381098,#381099,
#381100,#381101,#381102,#381103,#381104,#381105,#381106,#381107,#381108,
#381109,#381110,#381111,#381112,#381113,#381114,#381115,#381116,#381117,
#381118,#381119,#381120,#381121,#381122,#381123,#381124,#381125,#381126,
#381127,#381128,#381129,#381130,#381131,#381132,#381133,#381134,#381135),
 .UNSPECIFIED.,.F.,.F.,(4,3,3,3,3,3,3,3,3,3,3,3,3,3,3,3,4),(0.,1.53100299373414E-6,
4.52554775679612E-6,7.01151246291615E-6,9.26752933800107E-6,1.03084066197174E-5,
1.17138990826862E-5,1.22284894984074E-5,1.30315035324818E-5,1.38363728497813E-5,
1.40464197777496E-5,1.54597749564641E-5,1.6207358870407E-5,1.9209296871355E-5,
1.95234416882559E-5,2.37637844577606E-5,2.61487188977269E-5),
 .UNSPECIFIED.);
#25012=B_SPLINE_CURVE_WITH_KNOTS('',3,(#381150,#381151,#381152,#381153,
#381154,#381155,#381156,#381157,#381158,#381159,#381160,#381161,#381162,
#381163,#381164,#381165,#381166,#381167,#381168,#381169,#381170,#381171,
#381172,#381173,#381174,#381175,#381176,#381177,#381178,#381179,#381180),
 .UNSPECIFIED.,.F.,.F.,(4,3,3,3,3,3,3,3,3,3,4),(0.,3.9550791039771E-6,7.53768426604201E-6,
1.19904533335351E-5,1.40475043392586E-5,1.51452104275965E-5,1.67866272814208E-5,
1.69621513005358E-5,1.81338315460712E-5,1.9890633465655E-5,2.06132424588245E-5),
 .UNSPECIFIED.);
#25013=B_SPLINE_CURVE_WITH_KNOTS('',3,(#381183,#381184,#381185,#381186),
 .UNSPECIFIED.,.F.,.F.,(4,4),(4.47028007668187E-19,0.00010938435327491),
 .UNSPECIFIED.);
#25014=B_SPLINE_CURVE_WITH_KNOTS('',3,(#381213,#381214,#381215,#381216,
#381217,#381218,#381219,#381220,#381221,#381222,#381223,#381224,#381225,
#381226,#381227,#381228,#381229,#381230,#381231,#381232,#381233,#381234,
#381235,#381236,#381237,#381238,#381239,#381240,#381241,#381242,#381243,
#381244,#381245,#381246),.UNSPECIFIED.,.F.,.F.,(4,3,3,3,3,3,3,3,3,3,3,4),
(1.0842021724855E-19,2.09623992729441E-6,3.17176647120218E-6,4.82636181944089E-6,
5.01000917339966E-6,6.13126454147497E-6,8.60486650288866E-6,9.21144281170497E-6,
1.24722301135846E-5,1.42666454787859E-5,2.04670653756979E-5,2.08026438176808E-5),
 .UNSPECIFIED.);
#25015=B_SPLINE_CURVE_WITH_KNOTS('',3,(#381247,#381248,#381249,#381250),
 .UNSPECIFIED.,.F.,.F.,(4,4),(0.,0.000109384345496908),.UNSPECIFIED.);
#25016=B_SPLINE_CURVE_WITH_KNOTS('',3,(#381355,#381356,#381357,#381358),
 .UNSPECIFIED.,.F.,.F.,(4,4),(0.,9.54361881492173E-5),.UNSPECIFIED.);
#25017=B_SPLINE_CURVE_WITH_KNOTS('',3,(#381363,#381364,#381365,#381366,
#381367,#381368,#381369),.UNSPECIFIED.,.F.,.F.,(4,3,4),(0.,4.41069704323466E-5,
0.000113970027818833),.UNSPECIFIED.);
#25018=B_SPLINE_CURVE_WITH_KNOTS('',3,(#381375,#381376,#381377,#381378),
 .UNSPECIFIED.,.F.,.F.,(4,4),(4.47028007668187E-19,9.54361881492179E-5),
 .UNSPECIFIED.);
#25019=B_SPLINE_CURVE_WITH_KNOTS('',3,(#381382,#381383,#381384,#381385,
#381386,#381387,#381388),.UNSPECIFIED.,.F.,.F.,(4,3,4),(0.,6.98630244191492E-5,
0.000113969974038089),.UNSPECIFIED.);
#25020=B_SPLINE_CURVE_WITH_KNOTS('',3,(#381391,#381392,#381393,#381394,
#381395,#381396,#381397,#381398,#381399,#381400,#381401,#381402,#381403,
#381404,#381405,#381406,#381407,#381408,#381409,#381410,#381411,#381412,
#381413,#381414,#381415,#381416,#381417,#381418,#381419,#381420,#381421,
#381422,#381423,#381424,#381425,#381426,#381427,#381428,#381429,#381430,
#381431,#381432,#381433,#381434,#381435,#381436,#381437,#381438,#381439),
 .UNSPECIFIED.,.F.,.F.,(4,3,3,3,3,3,3,3,3,3,3,3,3,3,3,3,4),(0.,1.53100299373415E-6,
4.52554775679401E-6,7.01151246291589E-6,9.26752933799417E-6,1.03084066197173E-5,
1.1713899082686E-5,1.22284894984072E-5,1.30315035324816E-5,1.38363728497811E-5,
1.40464197777493E-5,1.54597749564639E-5,1.62073588704067E-5,1.92092968713137E-5,
1.95234416882553E-5,2.37637844577647E-5,2.61487188977258E-5),
 .UNSPECIFIED.);
#25021=B_SPLINE_CURVE_WITH_KNOTS('',3,(#381454,#381455,#381456,#381457,
#381458,#381459,#381460,#381461,#381462,#381463,#381464,#381465,#381466,
#381467,#381468,#381469,#381470,#381471,#381472,#381473,#381474,#381475,
#381476,#381477,#381478,#381479,#381480,#381481,#381482,#381483,#381484),
 .UNSPECIFIED.,.F.,.F.,(4,3,3,3,3,3,3,3,3,3,4),(0.,3.95507910398011E-6,
7.53768426604197E-6,1.1990453333535E-5,1.40475043392585E-5,1.51452104275964E-5,
1.67866272814066E-5,1.69621513005359E-5,1.81338315460713E-5,1.98906334656507E-5,
2.06132424588245E-5),.UNSPECIFIED.);
#25022=B_SPLINE_CURVE_WITH_KNOTS('',3,(#381487,#381488,#381489,#381490),
 .UNSPECIFIED.,.F.,.F.,(4,4),(4.47028007668187E-19,0.00010938435327491),
 .UNSPECIFIED.);
#25023=B_SPLINE_CURVE_WITH_KNOTS('',3,(#381517,#381518,#381519,#381520,
#381521,#381522,#381523,#381524,#381525,#381526,#381527,#381528,#381529,
#381530,#381531,#381532,#381533,#381534,#381535,#381536,#381537,#381538,
#381539,#381540,#381541,#381542,#381543,#381544,#381545,#381546,#381547,
#381548,#381549,#381550),.UNSPECIFIED.,.F.,.F.,(4,3,3,3,3,3,3,3,3,3,3,4),
(1.0842021724855E-19,2.09623992729435E-6,3.17176647120225E-6,4.82636181945333E-6,
5.01000917339964E-6,6.13126454147489E-6,8.60486650288845E-6,9.21144281170481E-6,
1.24722301136083E-5,1.42666454787854E-5,2.04670653756731E-5,2.08026438176802E-5),
 .UNSPECIFIED.);
#25024=B_SPLINE_CURVE_WITH_KNOTS('',3,(#381551,#381552,#381553,#381554),
 .UNSPECIFIED.,.F.,.F.,(4,4),(0.,0.000109384345496908),.UNSPECIFIED.);
#25025=B_SPLINE_CURVE_WITH_KNOTS('',3,(#381659,#381660,#381661,#381662),
 .UNSPECIFIED.,.F.,.F.,(4,4),(0.,9.54361881492174E-5),.UNSPECIFIED.);
#25026=B_SPLINE_CURVE_WITH_KNOTS('',3,(#381667,#381668,#381669,#381670,
#381671,#381672,#381673),.UNSPECIFIED.,.F.,.F.,(4,3,4),(0.,4.41069704323472E-5,
0.000113970027818833),.UNSPECIFIED.);
#25027=B_SPLINE_CURVE_WITH_KNOTS('',3,(#381679,#381680,#381681,#381682),
 .UNSPECIFIED.,.F.,.F.,(4,4),(4.47028007668187E-19,9.54361881492179E-5),
 .UNSPECIFIED.);
#25028=B_SPLINE_CURVE_WITH_KNOTS('',3,(#381686,#381687,#381688,#381689,
#381690,#381691,#381692),.UNSPECIFIED.,.F.,.F.,(4,3,4),(0.,6.98630244191489E-5,
0.000113969974038089),.UNSPECIFIED.);
#25029=B_SPLINE_CURVE_WITH_KNOTS('',3,(#381695,#381696,#381697,#381698,
#381699,#381700,#381701,#381702,#381703,#381704,#381705,#381706,#381707,
#381708,#381709,#381710,#381711,#381712,#381713,#381714,#381715,#381716,
#381717,#381718,#381719,#381720,#381721,#381722,#381723,#381724,#381725,
#381726,#381727,#381728,#381729,#381730,#381731,#381732,#381733,#381734,
#381735,#381736,#381737,#381738,#381739,#381740,#381741,#381742,#381743),
 .UNSPECIFIED.,.F.,.F.,(4,3,3,3,3,3,3,3,3,3,3,3,3,3,3,3,4),(0.,1.53100299373425E-6,
4.52554775679595E-6,7.01151246291619E-6,9.26752933800558E-6,1.03084066197173E-5,
1.17138990826862E-5,1.22284894984073E-5,1.30315035324817E-5,1.38363728497812E-5,
1.40464197777493E-5,1.54597749564638E-5,1.62073588704066E-5,1.92092968713467E-5,
1.95234416882551E-5,2.37637844577615E-5,2.61487188977252E-5),
 .UNSPECIFIED.);
#25030=B_SPLINE_CURVE_WITH_KNOTS('',3,(#381758,#381759,#381760,#381761,
#381762,#381763,#381764,#381765,#381766,#381767,#381768,#381769,#381770,
#381771,#381772,#381773,#381774,#381775,#381776,#381777,#381778,#381779,
#381780,#381781,#381782,#381783,#381784,#381785,#381786,#381787,#381788),
 .UNSPECIFIED.,.F.,.F.,(4,3,3,3,3,3,3,3,3,3,4),(0.,3.95507910398648E-6,
7.53768426604196E-6,1.19904533335351E-5,1.40475043392585E-5,1.51452104275965E-5,
1.67866272814172E-5,1.69621513005359E-5,1.81338315460713E-5,1.98906334656488E-5,
2.06132424588247E-5),.UNSPECIFIED.);
#25031=B_SPLINE_CURVE_WITH_KNOTS('',3,(#381791,#381792,#381793,#381794),
 .UNSPECIFIED.,.F.,.F.,(4,4),(4.47028007668187E-19,0.00010938435327491),
 .UNSPECIFIED.);
#25032=B_SPLINE_CURVE_WITH_KNOTS('',3,(#381821,#381822,#381823,#381824,
#381825,#381826,#381827,#381828,#381829,#381830,#381831,#381832,#381833,
#381834,#381835,#381836,#381837,#381838,#381839,#381840,#381841,#381842,
#381843,#381844,#381845,#381846,#381847,#381848,#381849,#381850,#381851,
#381852,#381853,#381854),.UNSPECIFIED.,.F.,.F.,(4,3,3,3,3,3,3,3,3,3,3,4),
(2.16840434497101E-19,2.09623992729427E-6,3.17176647120211E-6,4.82636181942053E-6,
5.01000917339956E-6,6.13126454147484E-6,8.60486650288841E-6,9.21144281170459E-6,
1.24722301135956E-5,1.4266645478785E-5,2.04670653756731E-5,2.08026438176793E-5),
 .UNSPECIFIED.);
#25033=B_SPLINE_CURVE_WITH_KNOTS('',3,(#381855,#381856,#381857,#381858),
 .UNSPECIFIED.,.F.,.F.,(4,4),(0.,0.000109384345496908),.UNSPECIFIED.);
#25034=B_SPLINE_CURVE_WITH_KNOTS('',3,(#381963,#381964,#381965,#381966),
 .UNSPECIFIED.,.F.,.F.,(4,4),(0.,9.54361881492177E-5),.UNSPECIFIED.);
#25035=B_SPLINE_CURVE_WITH_KNOTS('',3,(#381971,#381972,#381973,#381974,
#381975,#381976,#381977),.UNSPECIFIED.,.F.,.F.,(4,3,4),(0.,4.4106970432347E-5,
0.000113970027818833),.UNSPECIFIED.);
#25036=B_SPLINE_CURVE_WITH_KNOTS('',3,(#381983,#381984,#381985,#381986),
 .UNSPECIFIED.,.F.,.F.,(4,4),(0.,9.54361881492179E-5),.UNSPECIFIED.);
#25037=B_SPLINE_CURVE_WITH_KNOTS('',3,(#381990,#381991,#381992,#381993,
#381994,#381995,#381996),.UNSPECIFIED.,.F.,.F.,(4,3,4),(0.,6.98630244191492E-5,
0.000113969974038089),.UNSPECIFIED.);
#25038=B_SPLINE_CURVE_WITH_KNOTS('',3,(#381999,#382000,#382001,#382002,
#382003,#382004,#382005,#382006,#382007,#382008,#382009,#382010,#382011,
#382012,#382013,#382014,#382015,#382016,#382017,#382018,#382019,#382020,
#382021,#382022,#382023,#382024,#382025,#382026,#382027,#382028,#382029,
#382030,#382031,#382032,#382033,#382034,#382035,#382036,#382037,#382038,
#382039,#382040,#382041,#382042,#382043,#382044,#382045,#382046,#382047),
 .UNSPECIFIED.,.F.,.F.,(4,3,3,3,3,3,3,3,3,3,3,3,3,3,3,3,4),(0.,1.53100299373418E-6,
4.52554775680239E-6,7.01151246291602E-6,9.26752933798331E-6,1.03084066197173E-5,
1.17138990826861E-5,1.22284894984073E-5,1.30315035324816E-5,1.38363728497811E-5,
1.40464197777492E-5,1.54597749564639E-5,1.62073588704068E-5,1.92092968713089E-5,
1.95234416882554E-5,2.37637844577582E-5,2.61487188977262E-5),
 .UNSPECIFIED.);
#25039=B_SPLINE_CURVE_WITH_KNOTS('',3,(#382062,#382063,#382064,#382065,
#382066,#382067,#382068,#382069,#382070,#382071,#382072,#382073,#382074,
#382075,#382076,#382077,#382078,#382079,#382080,#382081,#382082,#382083,
#382084,#382085,#382086,#382087,#382088,#382089,#382090,#382091,#382092),
 .UNSPECIFIED.,.F.,.F.,(4,3,3,3,3,3,3,3,3,3,4),(0.,3.95507910398411E-6,
7.53768426604195E-6,1.19904533335351E-5,1.40475043392585E-5,1.51452104275965E-5,
1.6786627281414E-5,1.6962151300536E-5,1.81338315460712E-5,1.98906334656507E-5,
2.06132424588247E-5),.UNSPECIFIED.);
#25040=B_SPLINE_CURVE_WITH_KNOTS('',3,(#382095,#382096,#382097,#382098),
 .UNSPECIFIED.,.F.,.F.,(4,4),(4.33680868994202E-19,0.00010938435327491),
 .UNSPECIFIED.);
#25041=B_SPLINE_CURVE_WITH_KNOTS('',3,(#382125,#382126,#382127,#382128,
#382129,#382130,#382131,#382132,#382133,#382134,#382135,#382136,#382137,
#382138,#382139,#382140,#382141,#382142,#382143,#382144,#382145,#382146,
#382147,#382148,#382149,#382150,#382151,#382152,#382153,#382154,#382155,
#382156,#382157,#382158),.UNSPECIFIED.,.F.,.F.,(4,3,3,3,3,3,3,3,3,3,3,4),
(2.16840434497101E-19,2.09623992729466E-6,3.17176647120241E-6,4.82636181943524E-6,
5.01000917339945E-6,6.13126454147498E-6,8.60486650288857E-6,9.21144281170474E-6,
1.24722301135961E-5,1.42666454787854E-5,2.04670653756923E-5,2.08026438176799E-5),
 .UNSPECIFIED.);
#25042=B_SPLINE_CURVE_WITH_KNOTS('',3,(#382159,#382160,#382161,#382162),
 .UNSPECIFIED.,.F.,.F.,(4,4),(0.,0.000109384345496909),.UNSPECIFIED.);
#25043=B_SPLINE_CURVE_WITH_KNOTS('',3,(#382267,#382268,#382269,#382270),
 .UNSPECIFIED.,.F.,.F.,(4,4),(0.,9.54361881492174E-5),.UNSPECIFIED.);
#25044=B_SPLINE_CURVE_WITH_KNOTS('',3,(#382275,#382276,#382277,#382278,
#382279,#382280,#382281),.UNSPECIFIED.,.F.,.F.,(4,3,4),(0.,4.4106970432347E-5,
0.000113970027818833),.UNSPECIFIED.);
#25045=B_SPLINE_CURVE_WITH_KNOTS('',3,(#382287,#382288,#382289,#382290),
 .UNSPECIFIED.,.F.,.F.,(4,4),(4.33680868994202E-19,9.54361881492179E-5),
 .UNSPECIFIED.);
#25046=B_SPLINE_CURVE_WITH_KNOTS('',3,(#382294,#382295,#382296,#382297,
#382298,#382299,#382300),.UNSPECIFIED.,.F.,.F.,(4,3,4),(0.,6.98630244191489E-5,
0.000113969974038089),.UNSPECIFIED.);
#25047=B_SPLINE_CURVE_WITH_KNOTS('',3,(#382303,#382304,#382305,#382306,
#382307,#382308,#382309,#382310,#382311,#382312,#382313,#382314,#382315,
#382316,#382317,#382318,#382319,#382320,#382321,#382322,#382323,#382324,
#382325,#382326,#382327,#382328,#382329,#382330,#382331,#382332,#382333,
#382334,#382335,#382336,#382337,#382338,#382339,#382340,#382341,#382342,
#382343,#382344,#382345,#382346,#382347,#382348,#382349,#382350,#382351),
 .UNSPECIFIED.,.F.,.F.,(4,3,3,3,3,3,3,3,3,3,3,3,3,3,3,3,4),(0.,1.53100299373401E-6,
4.52554775679861E-6,7.01151246291619E-6,9.26752933802088E-6,1.03084066197173E-5,
1.1713899082686E-5,1.22284894984074E-5,1.30315035324816E-5,1.38363728497811E-5,
1.40464197777492E-5,1.5459774956464E-5,1.62073588704067E-5,1.92092968712723E-5,
1.95234416882556E-5,2.37637844577569E-5,2.61487188977263E-5),
 .UNSPECIFIED.);
#25048=B_SPLINE_CURVE_WITH_KNOTS('',3,(#382366,#382367,#382368,#382369,
#382370,#382371,#382372,#382373,#382374,#382375,#382376,#382377,#382378,
#382379,#382380,#382381,#382382,#382383,#382384,#382385,#382386,#382387,
#382388,#382389,#382390,#382391,#382392,#382393,#382394,#382395,#382396),
 .UNSPECIFIED.,.F.,.F.,(4,3,3,3,3,3,3,3,3,3,4),(0.,3.95507910396927E-6,
7.53768426604198E-6,1.1990453333535E-5,1.40475043392585E-5,1.51452104275963E-5,
1.67866272814057E-5,1.69621513005357E-5,1.8133831546071E-5,1.98906334656562E-5,
2.06132424588242E-5),.UNSPECIFIED.);
#25049=B_SPLINE_CURVE_WITH_KNOTS('',3,(#382399,#382400,#382401,#382402),
 .UNSPECIFIED.,.F.,.F.,(4,4),(4.33680868994202E-19,0.00010938435327491),
 .UNSPECIFIED.);
#25050=B_SPLINE_CURVE_WITH_KNOTS('',3,(#382429,#382430,#382431,#382432,
#382433,#382434,#382435,#382436,#382437,#382438,#382439,#382440,#382441,
#382442,#382443,#382444,#382445,#382446,#382447,#382448,#382449,#382450,
#382451,#382452,#382453,#382454,#382455,#382456,#382457,#382458,#382459,
#382460,#382461,#382462),.UNSPECIFIED.,.F.,.F.,(4,3,3,3,3,3,3,3,3,3,3,4),
(2.16840434497101E-19,2.09623992729424E-6,3.17176647120203E-6,4.82636181944634E-6,
5.01000917339943E-6,6.13126454147496E-6,8.60486650288851E-6,9.21144281170474E-6,
1.24722301136161E-5,1.42666454787853E-5,2.04670653756786E-5,2.08026438176797E-5),
 .UNSPECIFIED.);
#25051=B_SPLINE_CURVE_WITH_KNOTS('',3,(#382463,#382464,#382465,#382466),
 .UNSPECIFIED.,.F.,.F.,(4,4),(0.,0.000109384345496908),.UNSPECIFIED.);
#25052=B_SPLINE_CURVE_WITH_KNOTS('',3,(#382571,#382572,#382573,#382574),
 .UNSPECIFIED.,.F.,.F.,(4,4),(0.,9.54361881492174E-5),.UNSPECIFIED.);
#25053=B_SPLINE_CURVE_WITH_KNOTS('',3,(#382579,#382580,#382581,#382582,
#382583,#382584,#382585),.UNSPECIFIED.,.F.,.F.,(4,3,4),(0.,4.41069704323468E-5,
0.000113970027818833),.UNSPECIFIED.);
#25054=B_SPLINE_CURVE_WITH_KNOTS('',3,(#382591,#382592,#382593,#382594),
 .UNSPECIFIED.,.F.,.F.,(4,4),(4.33680868994202E-19,9.54361881492175E-5),
 .UNSPECIFIED.);
#25055=B_SPLINE_CURVE_WITH_KNOTS('',3,(#382598,#382599,#382600,#382601,
#382602,#382603,#382604),.UNSPECIFIED.,.F.,.F.,(4,3,4),(0.,6.9863024419149E-5,
0.000113969974038089),.UNSPECIFIED.);
#25056=B_SPLINE_CURVE_WITH_KNOTS('',3,(#382607,#382608,#382609,#382610,
#382611,#382612,#382613,#382614,#382615,#382616,#382617,#382618,#382619,
#382620,#382621,#382622,#382623,#382624,#382625,#382626,#382627,#382628,
#382629,#382630,#382631,#382632,#382633,#382634,#382635,#382636,#382637,
#382638,#382639,#382640,#382641,#382642,#382643,#382644,#382645,#382646,
#382647,#382648,#382649,#382650,#382651,#382652,#382653,#382654,#382655),
 .UNSPECIFIED.,.F.,.F.,(4,3,3,3,3,3,3,3,3,3,3,3,3,3,3,3,4),(0.,1.53100299373428E-6,
4.52554775679969E-6,7.01151246291618E-6,9.26752933799351E-6,1.03084066197174E-5,
1.17138990826862E-5,1.22284894984074E-5,1.30315035324818E-5,1.38363728497811E-5,
1.40464197777494E-5,1.54597749564639E-5,1.62073588704067E-5,1.92092968712941E-5,
1.95234416882553E-5,2.37637844577599E-5,2.61487188977258E-5),
 .UNSPECIFIED.);
#25057=B_SPLINE_CURVE_WITH_KNOTS('',3,(#382670,#382671,#382672,#382673,
#382674,#382675,#382676,#382677,#382678,#382679,#382680,#382681,#382682,
#382683,#382684,#382685,#382686,#382687,#382688,#382689,#382690,#382691,
#382692,#382693,#382694,#382695,#382696,#382697,#382698,#382699,#382700),
 .UNSPECIFIED.,.F.,.F.,(4,3,3,3,3,3,3,3,3,3,4),(0.,3.95507910398186E-6,
7.53768426604201E-6,1.19904533335352E-5,1.40475043392585E-5,1.51452104275964E-5,
1.67866272814194E-5,1.69621513005358E-5,1.81338315460712E-5,1.98906334656509E-5,
2.06132424588244E-5),.UNSPECIFIED.);
#25058=B_SPLINE_CURVE_WITH_KNOTS('',3,(#382703,#382704,#382705,#382706),
 .UNSPECIFIED.,.F.,.F.,(4,4),(9.69739903612216E-19,0.00010938435327491),
 .UNSPECIFIED.);
#25059=B_SPLINE_CURVE_WITH_KNOTS('',3,(#382733,#382734,#382735,#382736,
#382737,#382738,#382739,#382740,#382741,#382742,#382743,#382744,#382745,
#382746,#382747,#382748,#382749,#382750,#382751,#382752,#382753,#382754,
#382755,#382756,#382757,#382758,#382759,#382760,#382761,#382762,#382763,
#382764,#382765,#382766),.UNSPECIFIED.,.F.,.F.,(4,3,3,3,3,3,3,3,3,3,3,4),
(0.,2.09623992729434E-6,3.17176647120218E-6,4.82636181943681E-6,5.0100091733997E-6,
6.13126454147484E-6,8.60486650288858E-6,9.21144281170488E-6,1.24722301135974E-5,
1.42666454787854E-5,2.04670653756692E-5,2.08026438176798E-5),
 .UNSPECIFIED.);
#25060=B_SPLINE_CURVE_WITH_KNOTS('',3,(#382767,#382768,#382769,#382770),
 .UNSPECIFIED.,.F.,.F.,(4,4),(0.,0.000109384345496908),.UNSPECIFIED.);
#25061=B_SPLINE_CURVE_WITH_KNOTS('',3,(#382875,#382876,#382877,#382878),
 .UNSPECIFIED.,.F.,.F.,(4,4),(0.,9.54361881492176E-5),.UNSPECIFIED.);
#25062=B_SPLINE_CURVE_WITH_KNOTS('',3,(#382883,#382884,#382885,#382886,
#382887,#382888,#382889),.UNSPECIFIED.,.F.,.F.,(4,3,4),(0.,4.41069704323469E-5,
0.000113970027818833),.UNSPECIFIED.);
#25063=B_SPLINE_CURVE_WITH_KNOTS('',3,(#382895,#382896,#382897,#382898),
 .UNSPECIFIED.,.F.,.F.,(4,4),(4.33680868994202E-19,9.54361881492181E-5),
 .UNSPECIFIED.);
#25064=B_SPLINE_CURVE_WITH_KNOTS('',3,(#382902,#382903,#382904,#382905,
#382906,#382907,#382908),.UNSPECIFIED.,.F.,.F.,(4,3,4),(0.,6.98630244191488E-5,
0.000113969974038089),.UNSPECIFIED.);
#25065=B_SPLINE_CURVE_WITH_KNOTS('',3,(#382911,#382912,#382913,#382914,
#382915,#382916,#382917,#382918,#382919,#382920,#382921,#382922,#382923,
#382924,#382925,#382926,#382927,#382928,#382929,#382930,#382931,#382932,
#382933,#382934,#382935,#382936,#382937,#382938,#382939,#382940,#382941,
#382942,#382943,#382944,#382945,#382946,#382947,#382948,#382949,#382950,
#382951,#382952,#382953,#382954,#382955,#382956,#382957,#382958,#382959),
 .UNSPECIFIED.,.F.,.F.,(4,3,3,3,3,3,3,3,3,3,3,3,3,3,3,3,4),(0.,1.53100299373429E-6,
4.52554775678867E-6,7.01151246291612E-6,9.26752933799565E-6,1.03084066197174E-5,
1.1713899082686E-5,1.22284894984071E-5,1.30315035324816E-5,1.38363728497813E-5,
1.40464197777496E-5,1.5459774956464E-5,1.62073588704069E-5,1.9209296871261E-5,
1.95234416882556E-5,2.37637844577607E-5,2.61487188977264E-5),
 .UNSPECIFIED.);
#25066=B_SPLINE_CURVE_WITH_KNOTS('',3,(#382974,#382975,#382976,#382977,
#382978,#382979,#382980,#382981,#382982,#382983,#382984,#382985,#382986,
#382987,#382988,#382989,#382990,#382991,#382992,#382993,#382994,#382995,
#382996,#382997,#382998,#382999,#383000,#383001,#383002,#383003,#383004),
 .UNSPECIFIED.,.F.,.F.,(4,3,3,3,3,3,3,3,3,3,4),(0.,3.95507910397189E-6,
7.53768426604198E-6,1.19904533335351E-5,1.40475043392586E-5,1.51452104275963E-5,
1.67866272814151E-5,1.69621513005357E-5,1.8133831546071E-5,1.98906334656561E-5,
2.06132424588244E-5),.UNSPECIFIED.);
#25067=B_SPLINE_CURVE_WITH_KNOTS('',3,(#383007,#383008,#383009,#383010),
 .UNSPECIFIED.,.F.,.F.,(4,4),(4.33680868994202E-19,0.00010938435327491),
 .UNSPECIFIED.);
#25068=B_SPLINE_CURVE_WITH_KNOTS('',3,(#383037,#383038,#383039,#383040,
#383041,#383042,#383043,#383044,#383045,#383046,#383047,#383048,#383049,
#383050,#383051,#383052,#383053,#383054,#383055,#383056,#383057,#383058,
#383059,#383060,#383061,#383062,#383063,#383064,#383065,#383066,#383067,
#383068,#383069,#383070),.UNSPECIFIED.,.F.,.F.,(4,3,3,3,3,3,3,3,3,3,3,4),
(2.16840434497101E-19,2.09623992729412E-6,3.17176647120213E-6,4.82636181943927E-6,
5.01000917339946E-6,6.13126454147475E-6,8.60486650288808E-6,9.21144281170435E-6,
1.24722301135917E-5,1.42666454787843E-5,2.04670653757219E-5,2.08026438176781E-5),
 .UNSPECIFIED.);
#25069=B_SPLINE_CURVE_WITH_KNOTS('',3,(#383071,#383072,#383073,#383074),
 .UNSPECIFIED.,.F.,.F.,(4,4),(0.,0.000109384345496908),.UNSPECIFIED.);
#25070=B_SPLINE_CURVE_WITH_KNOTS('',3,(#383179,#383180,#383181,#383182),
 .UNSPECIFIED.,.F.,.F.,(4,4),(0.,9.54361881492176E-5),.UNSPECIFIED.);
#25071=B_SPLINE_CURVE_WITH_KNOTS('',3,(#383187,#383188,#383189,#383190,
#383191,#383192,#383193),.UNSPECIFIED.,.F.,.F.,(4,3,4),(0.,4.4106970432347E-5,
0.000113970027818833),.UNSPECIFIED.);
#25072=B_SPLINE_CURVE_WITH_KNOTS('',3,(#383199,#383200,#383201,#383202),
 .UNSPECIFIED.,.F.,.F.,(4,4),(4.33680868994202E-19,9.5436188149218E-5),
 .UNSPECIFIED.);
#25073=B_SPLINE_CURVE_WITH_KNOTS('',3,(#383206,#383207,#383208,#383209,
#383210,#383211,#383212),.UNSPECIFIED.,.F.,.F.,(4,3,4),(0.,6.98630244191492E-5,
0.000113969974038089),.UNSPECIFIED.);
#25074=B_SPLINE_CURVE_WITH_KNOTS('',3,(#383215,#383216,#383217,#383218,
#383219,#383220,#383221,#383222,#383223,#383224,#383225,#383226,#383227,
#383228,#383229,#383230,#383231,#383232,#383233,#383234,#383235,#383236,
#383237,#383238,#383239,#383240,#383241,#383242,#383243,#383244,#383245,
#383246,#383247,#383248,#383249,#383250,#383251,#383252,#383253,#383254,
#383255,#383256,#383257,#383258,#383259,#383260,#383261,#383262,#383263),
 .UNSPECIFIED.,.F.,.F.,(4,3,3,3,3,3,3,3,3,3,3,3,3,3,3,3,4),(0.,1.53100299373403E-6,
4.5255477567934E-6,7.01151246291602E-6,9.26752933800128E-6,1.03084066197172E-5,
1.17138990826861E-5,1.22284894984074E-5,1.30315035324817E-5,1.3836372849781E-5,
1.40464197777492E-5,1.54597749564639E-5,1.62073588704066E-5,1.92092968712801E-5,
1.95234416882552E-5,2.37637844577568E-5,2.61487188977257E-5),
 .UNSPECIFIED.);
#25075=B_SPLINE_CURVE_WITH_KNOTS('',3,(#383278,#383279,#383280,#383281,
#383282,#383283,#383284,#383285,#383286,#383287,#383288,#383289,#383290,
#383291,#383292,#383293,#383294,#383295,#383296,#383297,#383298,#383299,
#383300,#383301,#383302,#383303,#383304,#383305,#383306,#383307,#383308),
 .UNSPECIFIED.,.F.,.F.,(4,3,3,3,3,3,3,3,3,3,4),(0.,3.95507910397134E-6,
7.53768426604187E-6,1.19904533335349E-5,1.40475043392585E-5,1.51452104275965E-5,
1.67866272814129E-5,1.69621513005357E-5,1.81338315460711E-5,1.98906334656565E-5,
2.06132424588243E-5),.UNSPECIFIED.);
#25076=B_SPLINE_CURVE_WITH_KNOTS('',3,(#383311,#383312,#383313,#383314),
 .UNSPECIFIED.,.F.,.F.,(4,4),(9.69739903612216E-19,0.00010938435327491),
 .UNSPECIFIED.);
#25077=B_SPLINE_CURVE_WITH_KNOTS('',3,(#383341,#383342,#383343,#383344,
#383345,#383346,#383347,#383348,#383349,#383350,#383351,#383352,#383353,
#383354,#383355,#383356,#383357,#383358,#383359,#383360,#383361,#383362,
#383363,#383364,#383365,#383366,#383367,#383368,#383369,#383370,#383371,
#383372,#383373,#383374),.UNSPECIFIED.,.F.,.F.,(4,3,3,3,3,3,3,3,3,3,3,4),
(0.,2.09623992729436E-6,3.17176647120223E-6,4.82636181942795E-6,5.01000917339974E-6,
6.13126454147501E-6,8.60486650288861E-6,9.21144281170489E-6,1.24722301136162E-5,
1.42666454787854E-5,2.04670653756897E-5,2.08026438176798E-5),
 .UNSPECIFIED.);
#25078=B_SPLINE_CURVE_WITH_KNOTS('',3,(#383375,#383376,#383377,#383378),
 .UNSPECIFIED.,.F.,.F.,(4,4),(0.,0.000109384345496908),.UNSPECIFIED.);
#25079=B_SPLINE_CURVE_WITH_KNOTS('',3,(#383483,#383484,#383485,#383486),
 .UNSPECIFIED.,.F.,.F.,(4,4),(0.,9.54361881492176E-5),.UNSPECIFIED.);
#25080=B_SPLINE_CURVE_WITH_KNOTS('',3,(#383491,#383492,#383493,#383494,
#383495,#383496,#383497),.UNSPECIFIED.,.F.,.F.,(4,3,4),(0.,4.41069704323469E-5,
0.000113970027818833),.UNSPECIFIED.);
#25081=B_SPLINE_CURVE_WITH_KNOTS('',3,(#383503,#383504,#383505,#383506),
 .UNSPECIFIED.,.F.,.F.,(4,4),(4.33680868994202E-19,9.54361881492174E-5),
 .UNSPECIFIED.);
#25082=B_SPLINE_CURVE_WITH_KNOTS('',3,(#383510,#383511,#383512,#383513,
#383514,#383515,#383516),.UNSPECIFIED.,.F.,.F.,(4,3,4),(0.,6.98630244191489E-5,
0.000113969974038089),.UNSPECIFIED.);
#25083=B_SPLINE_CURVE_WITH_KNOTS('',3,(#383519,#383520,#383521,#383522,
#383523,#383524,#383525,#383526,#383527,#383528,#383529,#383530,#383531,
#383532,#383533,#383534,#383535,#383536,#383537,#383538,#383539,#383540,
#383541,#383542,#383543,#383544,#383545,#383546,#383547,#383548,#383549,
#383550,#383551,#383552,#383553,#383554,#383555,#383556,#383557,#383558,
#383559,#383560,#383561,#383562,#383563,#383564,#383565,#383566,#383567),
 .UNSPECIFIED.,.F.,.F.,(4,3,3,3,3,3,3,3,3,3,3,3,3,3,3,3,4),(0.,1.5310029937343E-6,
4.52554775679482E-6,7.01151246291627E-6,9.26752933801453E-6,1.03084066197174E-5,
1.17138990826864E-5,1.22284894984078E-5,1.30315035324817E-5,1.38363728497815E-5,
1.40464197777497E-5,1.5459774956464E-5,1.6207358870407E-5,1.92092968713133E-5,
1.95234416882558E-5,2.37637844577604E-5,2.61487188977267E-5),
 .UNSPECIFIED.);
#25084=B_SPLINE_CURVE_WITH_KNOTS('',3,(#383582,#383583,#383584,#383585,
#383586,#383587,#383588,#383589,#383590,#383591,#383592,#383593,#383594,
#383595,#383596,#383597,#383598,#383599,#383600,#383601,#383602,#383603,
#383604,#383605,#383606,#383607,#383608,#383609,#383610,#383611,#383612),
 .UNSPECIFIED.,.F.,.F.,(4,3,3,3,3,3,3,3,3,3,4),(0.,3.95507910397896E-6,
7.53768426604197E-6,1.1990453333535E-5,1.40475043392585E-5,1.51452104275964E-5,
1.67866272814317E-5,1.69621513005359E-5,1.81338315460711E-5,1.9890633465653E-5,
2.06132424588247E-5),.UNSPECIFIED.);
#25085=B_SPLINE_CURVE_WITH_KNOTS('',3,(#383615,#383616,#383617,#383618),
 .UNSPECIFIED.,.F.,.F.,(4,4),(4.33680868994202E-19,0.00010938435327491),
 .UNSPECIFIED.);
#25086=B_SPLINE_CURVE_WITH_KNOTS('',3,(#383645,#383646,#383647,#383648,
#383649,#383650,#383651,#383652,#383653,#383654,#383655,#383656,#383657,
#383658,#383659,#383660,#383661,#383662,#383663,#383664,#383665,#383666,
#383667,#383668,#383669,#383670,#383671,#383672,#383673,#383674,#383675,
#383676,#383677,#383678),.UNSPECIFIED.,.F.,.F.,(4,3,3,3,3,3,3,3,3,3,3,4),
(2.16840434497101E-19,2.09623992729433E-6,3.17176647120203E-6,4.8263618194373E-6,
5.01000917339969E-6,6.13126454147473E-6,8.60486650288812E-6,9.21144281170456E-6,
1.24722301136098E-5,1.42666454787845E-5,2.04670653756581E-5,2.08026438176784E-5),
 .UNSPECIFIED.);
#25087=B_SPLINE_CURVE_WITH_KNOTS('',3,(#383679,#383680,#383681,#383682),
 .UNSPECIFIED.,.F.,.F.,(4,4),(0.,0.000109384345496908),.UNSPECIFIED.);
#25088=B_SPLINE_CURVE_WITH_KNOTS('',3,(#383787,#383788,#383789,#383790),
 .UNSPECIFIED.,.F.,.F.,(4,4),(0.,9.54361881492175E-5),.UNSPECIFIED.);
#25089=B_SPLINE_CURVE_WITH_KNOTS('',3,(#383795,#383796,#383797,#383798,
#383799,#383800,#383801),.UNSPECIFIED.,.F.,.F.,(4,3,4),(0.,4.4106970432347E-5,
0.000113970027818833),.UNSPECIFIED.);
#25090=B_SPLINE_CURVE_WITH_KNOTS('',3,(#383807,#383808,#383809,#383810),
 .UNSPECIFIED.,.F.,.F.,(4,4),(4.33680868994202E-19,9.54361881492178E-5),
 .UNSPECIFIED.);
#25091=B_SPLINE_CURVE_WITH_KNOTS('',3,(#383814,#383815,#383816,#383817,
#383818,#383819,#383820),.UNSPECIFIED.,.F.,.F.,(4,3,4),(0.,6.98630244191491E-5,
0.000113969974038089),.UNSPECIFIED.);
#25092=B_SPLINE_CURVE_WITH_KNOTS('',3,(#383823,#383824,#383825,#383826,
#383827,#383828,#383829,#383830,#383831,#383832,#383833,#383834,#383835,
#383836,#383837,#383838,#383839,#383840,#383841,#383842,#383843,#383844,
#383845,#383846,#383847,#383848,#383849,#383850,#383851,#383852,#383853,
#383854,#383855,#383856,#383857,#383858,#383859,#383860,#383861,#383862,
#383863,#383864,#383865,#383866,#383867,#383868,#383869,#383870,#383871),
 .UNSPECIFIED.,.F.,.F.,(4,3,3,3,3,3,3,3,3,3,3,3,3,3,3,3,4),(0.,1.53100299373408E-6,
4.52554775679743E-6,7.01151246291611E-6,9.2675293380054E-6,1.03084066197173E-5,
1.17138990826862E-5,1.22284894984075E-5,1.30315035324818E-5,1.38363728497812E-5,
1.40464197777494E-5,1.54597749564639E-5,1.6207358870407E-5,1.92092968712166E-5,
1.95234416882556E-5,2.37637844577591E-5,2.61487188977264E-5),
 .UNSPECIFIED.);
#25093=B_SPLINE_CURVE_WITH_KNOTS('',3,(#383886,#383887,#383888,#383889,
#383890,#383891,#383892,#383893,#383894,#383895,#383896,#383897,#383898,
#383899,#383900,#383901,#383902,#383903,#383904,#383905,#383906,#383907,
#383908,#383909,#383910,#383911,#383912,#383913,#383914,#383915,#383916),
 .UNSPECIFIED.,.F.,.F.,(4,3,3,3,3,3,3,3,3,3,4),(0.,3.9550791039714E-6,7.53768426604213E-6,
1.19904533335353E-5,1.40475043392588E-5,1.51452104275968E-5,1.67866272814203E-5,
1.6962151300536E-5,1.81338315460714E-5,1.98906334656568E-5,2.06132424588248E-5),
 .UNSPECIFIED.);
#25094=B_SPLINE_CURVE_WITH_KNOTS('',3,(#383919,#383920,#383921,#383922),
 .UNSPECIFIED.,.F.,.F.,(4,4),(9.93687704810078E-19,0.00010938435327491),
 .UNSPECIFIED.);
#25095=B_SPLINE_CURVE_WITH_KNOTS('',3,(#383949,#383950,#383951,#383952,
#383953,#383954,#383955,#383956,#383957,#383958,#383959,#383960,#383961,
#383962,#383963,#383964,#383965,#383966,#383967,#383968,#383969,#383970,
#383971,#383972,#383973,#383974,#383975,#383976,#383977,#383978,#383979,
#383980,#383981,#383982),.UNSPECIFIED.,.F.,.F.,(4,3,3,3,3,3,3,3,3,3,3,4),
(2.16840434497101E-19,2.09623992729456E-6,3.17176647120225E-6,4.82636181944301E-6,
5.01000917339998E-6,6.13126454147519E-6,8.60486650288873E-6,9.21144281170526E-6,
1.24722301136018E-5,1.42666454787858E-5,2.04670653756884E-5,2.08026438176806E-5),
 .UNSPECIFIED.);
#25096=B_SPLINE_CURVE_WITH_KNOTS('',3,(#383983,#383984,#383985,#383986),
 .UNSPECIFIED.,.F.,.F.,(4,4),(0.,0.000109384345496908),.UNSPECIFIED.);
#25097=B_SPLINE_CURVE_WITH_KNOTS('',3,(#384091,#384092,#384093,#384094),
 .UNSPECIFIED.,.F.,.F.,(4,4),(0.,9.54361881492173E-5),.UNSPECIFIED.);
#25098=B_SPLINE_CURVE_WITH_KNOTS('',3,(#384099,#384100,#384101,#384102,
#384103,#384104,#384105),.UNSPECIFIED.,.F.,.F.,(4,3,4),(0.,4.41069704323469E-5,
0.000113970027818833),.UNSPECIFIED.);
#25099=B_SPLINE_CURVE_WITH_KNOTS('',3,(#384111,#384112,#384113,#384114),
 .UNSPECIFIED.,.F.,.F.,(4,4),(2.16840434497101E-19,9.54361881492178E-5),
 .UNSPECIFIED.);
#25100=B_SPLINE_CURVE_WITH_KNOTS('',3,(#384118,#384119,#384120,#384121,
#384122,#384123,#384124),.UNSPECIFIED.,.F.,.F.,(4,3,4),(0.,6.98630244191491E-5,
0.000113969974038089),.UNSPECIFIED.);
#25101=B_SPLINE_CURVE_WITH_KNOTS('',3,(#384127,#384128,#384129,#384130,
#384131,#384132,#384133,#384134,#384135,#384136,#384137,#384138,#384139,
#384140,#384141,#384142,#384143,#384144,#384145,#384146,#384147,#384148,
#384149,#384150,#384151,#384152,#384153,#384154,#384155,#384156,#384157,
#384158,#384159,#384160,#384161,#384162,#384163,#384164,#384165,#384166,
#384167,#384168,#384169,#384170,#384171,#384172,#384173,#384174,#384175),
 .UNSPECIFIED.,.F.,.F.,(4,3,3,3,3,3,3,3,3,3,3,3,3,3,3,3,4),(0.,1.5310029937342E-6,
4.52554775679593E-6,7.0115124629161E-6,9.26752933800773E-6,1.03084066197173E-5,
1.1713899082686E-5,1.22284894984073E-5,1.30315035324817E-5,1.38363728497814E-5,
1.40464197777494E-5,1.54597749564636E-5,1.62073588704066E-5,1.9209296871252E-5,
1.9523441688255E-5,2.37637844577529E-5,2.61487188977248E-5),
 .UNSPECIFIED.);
#25102=B_SPLINE_CURVE_WITH_KNOTS('',3,(#384190,#384191,#384192,#384193,
#384194,#384195,#384196,#384197,#384198,#384199,#384200,#384201,#384202,
#384203,#384204,#384205,#384206,#384207,#384208,#384209,#384210,#384211,
#384212,#384213,#384214,#384215,#384216,#384217,#384218,#384219,#384220),
 .UNSPECIFIED.,.F.,.F.,(4,3,3,3,3,3,3,3,3,3,4),(0.,3.95507910398813E-6,
7.5376842660421E-6,1.19904533335351E-5,1.40475043392585E-5,1.51452104275963E-5,
1.67866272814151E-5,1.69621513005358E-5,1.81338315460713E-5,1.98906334656507E-5,
2.06132424588243E-5),.UNSPECIFIED.);
#25103=B_SPLINE_CURVE_WITH_KNOTS('',3,(#384223,#384224,#384225,#384226),
 .UNSPECIFIED.,.F.,.F.,(4,4),(9.69739903612216E-19,0.00010938435327491),
 .UNSPECIFIED.);
#25104=B_SPLINE_CURVE_WITH_KNOTS('',3,(#384253,#384254,#384255,#384256,
#384257,#384258,#384259,#384260,#384261,#384262,#384263,#384264,#384265,
#384266,#384267,#384268,#384269,#384270,#384271,#384272,#384273,#384274,
#384275,#384276,#384277,#384278,#384279,#384280,#384281,#384282,#384283,
#384284,#384285,#384286),.UNSPECIFIED.,.F.,.F.,(4,3,3,3,3,3,3,3,3,3,3,4),
(2.16840434497101E-19,2.09623992729424E-6,3.17176647120173E-6,4.82636181943504E-6,
5.01000917339928E-6,6.13126454147462E-6,8.60486650288808E-6,9.2114428117044E-6,
1.24722301136036E-5,1.42666454787847E-5,2.0467065375693E-5,2.08026438176788E-5),
 .UNSPECIFIED.);
#25105=B_SPLINE_CURVE_WITH_KNOTS('',3,(#384287,#384288,#384289,#384290),
 .UNSPECIFIED.,.F.,.F.,(4,4),(0.,0.000109384345496909),.UNSPECIFIED.);
#25106=B_SPLINE_CURVE_WITH_KNOTS('',3,(#384395,#384396,#384397,#384398),
 .UNSPECIFIED.,.F.,.F.,(4,4),(0.,9.54361881492177E-5),.UNSPECIFIED.);
#25107=B_SPLINE_CURVE_WITH_KNOTS('',3,(#384403,#384404,#384405,#384406,
#384407,#384408,#384409),.UNSPECIFIED.,.F.,.F.,(4,3,4),(0.,4.4106970432347E-5,
0.000113970027818833),.UNSPECIFIED.);
#25108=B_SPLINE_CURVE_WITH_KNOTS('',3,(#384415,#384416,#384417,#384418),
 .UNSPECIFIED.,.F.,.F.,(4,4),(2.16840434497101E-19,9.54361881492179E-5),
 .UNSPECIFIED.);
#25109=B_SPLINE_CURVE_WITH_KNOTS('',3,(#384422,#384423,#384424,#384425,
#384426,#384427,#384428),.UNSPECIFIED.,.F.,.F.,(4,3,4),(0.,6.9863024419149E-5,
0.000113969974038089),.UNSPECIFIED.);
#25110=B_SPLINE_CURVE_WITH_KNOTS('',3,(#384431,#384432,#384433,#384434,
#384435,#384436,#384437,#384438,#384439,#384440,#384441,#384442,#384443,
#384444,#384445,#384446,#384447,#384448,#384449,#384450,#384451,#384452,
#384453,#384454,#384455,#384456,#384457,#384458,#384459,#384460,#384461,
#384462,#384463,#384464,#384465,#384466,#384467,#384468,#384469,#384470,
#384471,#384472,#384473,#384474,#384475,#384476,#384477,#384478,#384479),
 .UNSPECIFIED.,.F.,.F.,(4,3,3,3,3,3,3,3,3,3,3,3,3,3,3,3,4),(0.,1.53100299373407E-6,
4.52554775679964E-6,7.01151246291605E-6,9.26752933799828E-6,1.03084066197173E-5,
1.17138990826861E-5,1.22284894984075E-5,1.30315035324815E-5,1.38363728497813E-5,
1.40464197777497E-5,1.54597749564639E-5,1.62073588704066E-5,1.92092968712802E-5,
1.95234416882554E-5,2.37637844577551E-5,2.61487188977257E-5),
 .UNSPECIFIED.);
#25111=B_SPLINE_CURVE_WITH_KNOTS('',3,(#384494,#384495,#384496,#384497,
#384498,#384499,#384500,#384501,#384502,#384503,#384504,#384505,#384506,
#384507,#384508,#384509,#384510,#384511,#384512,#384513,#384514,#384515,
#384516,#384517,#384518,#384519,#384520,#384521,#384522,#384523,#384524),
 .UNSPECIFIED.,.F.,.F.,(4,3,3,3,3,3,3,3,3,3,4),(0.,3.95507910396865E-6,
7.53768426604195E-6,1.19904533335351E-5,1.40475043392586E-5,1.51452104275965E-5,
1.67866272814148E-5,1.6962151300536E-5,1.8133831546071E-5,1.98906334656545E-5,
2.06132424588246E-5),.UNSPECIFIED.);
#25112=B_SPLINE_CURVE_WITH_KNOTS('',3,(#384527,#384528,#384529,#384530),
 .UNSPECIFIED.,.F.,.F.,(4,4),(2.16840434497101E-19,0.00010938435327491),
 .UNSPECIFIED.);
#25113=B_SPLINE_CURVE_WITH_KNOTS('',3,(#384557,#384558,#384559,#384560,
#384561,#384562,#384563,#384564,#384565,#384566,#384567,#384568,#384569,
#384570,#384571,#384572,#384573,#384574,#384575,#384576,#384577,#384578,
#384579,#384580,#384581,#384582,#384583,#384584,#384585,#384586,#384587,
#384588,#384589,#384590),.UNSPECIFIED.,.F.,.F.,(4,3,3,3,3,3,3,3,3,3,3,4),
(0.,2.09623992729435E-6,3.17176647120248E-6,4.82636181943654E-6,5.01000917339974E-6,
6.131264541475E-6,8.60486650288874E-6,9.21144281170515E-6,1.24722301135883E-5,
1.4266645478786E-5,2.04670653756816E-5,2.0802643817681E-5),
 .UNSPECIFIED.);
#25114=B_SPLINE_CURVE_WITH_KNOTS('',3,(#384591,#384592,#384593,#384594),
 .UNSPECIFIED.,.F.,.F.,(4,4),(0.,0.000109384345496908),.UNSPECIFIED.);
#25115=B_SPLINE_CURVE_WITH_KNOTS('',3,(#384699,#384700,#384701,#384702),
 .UNSPECIFIED.,.F.,.F.,(4,4),(0.,9.54361881492176E-5),.UNSPECIFIED.);
#25116=B_SPLINE_CURVE_WITH_KNOTS('',3,(#384707,#384708,#384709,#384710,
#384711,#384712,#384713),.UNSPECIFIED.,.F.,.F.,(4,3,4),(0.,4.41069704323469E-5,
0.000113970027818834),.UNSPECIFIED.);
#25117=B_SPLINE_CURVE_WITH_KNOTS('',3,(#384719,#384720,#384721,#384722),
 .UNSPECIFIED.,.F.,.F.,(4,4),(2.16840434497101E-19,9.54361881492178E-5),
 .UNSPECIFIED.);
#25118=B_SPLINE_CURVE_WITH_KNOTS('',3,(#384726,#384727,#384728,#384729,
#384730,#384731,#384732),.UNSPECIFIED.,.F.,.F.,(4,3,4),(0.,6.9863024419149E-5,
0.000113969974038089),.UNSPECIFIED.);
#25119=B_SPLINE_CURVE_WITH_KNOTS('',3,(#384735,#384736,#384737,#384738,
#384739,#384740,#384741,#384742,#384743,#384744,#384745,#384746,#384747,
#384748,#384749,#384750,#384751,#384752,#384753,#384754,#384755,#384756,
#384757,#384758,#384759,#384760,#384761,#384762,#384763,#384764,#384765,
#384766,#384767,#384768,#384769,#384770,#384771,#384772,#384773,#384774,
#384775,#384776,#384777,#384778,#384779,#384780,#384781,#384782,#384783),
 .UNSPECIFIED.,.F.,.F.,(4,3,3,3,3,3,3,3,3,3,3,3,3,3,3,3,4),(0.,1.53100299373425E-6,
4.52554775679411E-6,7.01151246291613E-6,9.26752933801911E-6,1.03084066197173E-5,
1.17138990826863E-5,1.22284894984073E-5,1.30315035324819E-5,1.38363728497813E-5,
1.40464197777495E-5,1.54597749564641E-5,1.62073588704069E-5,1.920929687123E-5,
1.9523441688256E-5,2.3763784457758E-5,2.61487188977268E-5),
 .UNSPECIFIED.);
#25120=B_SPLINE_CURVE_WITH_KNOTS('',3,(#384798,#384799,#384800,#384801,
#384802,#384803,#384804,#384805,#384806,#384807,#384808,#384809,#384810,
#384811,#384812,#384813,#384814,#384815,#384816,#384817,#384818,#384819,
#384820,#384821,#384822,#384823,#384824,#384825,#384826,#384827,#384828),
 .UNSPECIFIED.,.F.,.F.,(4,3,3,3,3,3,3,3,3,3,4),(0.,3.95507910399092E-6,
7.53768426604211E-6,1.1990453333535E-5,1.40475043392589E-5,1.51452104275967E-5,
1.67866272814072E-5,1.6962151300536E-5,1.81338315460714E-5,1.98906334656527E-5,
2.06132424588247E-5),.UNSPECIFIED.);
#25121=B_SPLINE_CURVE_WITH_KNOTS('',3,(#384831,#384832,#384833,#384834),
 .UNSPECIFIED.,.F.,.F.,(4,4),(2.16840434497101E-19,0.00010938435327491),
 .UNSPECIFIED.);
#25122=B_SPLINE_CURVE_WITH_KNOTS('',3,(#384861,#384862,#384863,#384864,
#384865,#384866,#384867,#384868,#384869,#384870,#384871,#384872,#384873,
#384874,#384875,#384876,#384877,#384878,#384879,#384880,#384881,#384882,
#384883,#384884,#384885,#384886,#384887,#384888,#384889,#384890,#384891,
#384892,#384893,#384894),.UNSPECIFIED.,.F.,.F.,(4,3,3,3,3,3,3,3,3,3,3,4),
(0.,2.09623992729424E-6,3.171766471202E-6,4.82636181944403E-6,5.01000917339938E-6,
6.13126454147494E-6,8.60486650288832E-6,9.21144281170473E-6,1.24722301135726E-5,
1.42666454787854E-5,2.04670653757091E-5,2.08026438176801E-5),
 .UNSPECIFIED.);
#25123=B_SPLINE_CURVE_WITH_KNOTS('',3,(#384895,#384896,#384897,#384898),
 .UNSPECIFIED.,.F.,.F.,(4,4),(0.,0.000109384345496908),.UNSPECIFIED.);
#25124=B_SPLINE_CURVE_WITH_KNOTS('',3,(#385003,#385004,#385005,#385006),
 .UNSPECIFIED.,.F.,.F.,(4,4),(0.,9.54361881492174E-5),.UNSPECIFIED.);
#25125=B_SPLINE_CURVE_WITH_KNOTS('',3,(#385011,#385012,#385013,#385014,
#385015,#385016,#385017),.UNSPECIFIED.,.F.,.F.,(4,3,4),(0.,4.41069704323469E-5,
0.000113970027818833),.UNSPECIFIED.);
#25126=B_SPLINE_CURVE_WITH_KNOTS('',3,(#385023,#385024,#385025,#385026),
 .UNSPECIFIED.,.F.,.F.,(4,4),(2.16840434497101E-19,9.54361881492181E-5),
 .UNSPECIFIED.);
#25127=B_SPLINE_CURVE_WITH_KNOTS('',3,(#385030,#385031,#385032,#385033,
#385034,#385035,#385036),.UNSPECIFIED.,.F.,.F.,(4,3,4),(0.,6.98630244191489E-5,
0.000113969974038089),.UNSPECIFIED.);
#25128=B_SPLINE_CURVE_WITH_KNOTS('',3,(#385039,#385040,#385041,#385042,
#385043,#385044,#385045,#385046,#385047,#385048,#385049,#385050,#385051,
#385052,#385053,#385054,#385055,#385056,#385057,#385058,#385059,#385060,
#385061,#385062,#385063,#385064,#385065,#385066,#385067,#385068,#385069,
#385070,#385071,#385072,#385073,#385074,#385075,#385076,#385077,#385078,
#385079,#385080,#385081,#385082,#385083,#385084,#385085,#385086,#385087),
 .UNSPECIFIED.,.F.,.F.,(4,3,3,3,3,3,3,3,3,3,3,3,3,3,3,3,4),(0.,1.53100299373416E-6,
4.52554775679832E-6,7.01151246291608E-6,9.26752933799768E-6,1.03084066197173E-5,
1.1713899082686E-5,1.22284894984076E-5,1.30315035324819E-5,1.38363728497816E-5,
1.40464197777497E-5,1.54597749564643E-5,1.62073588704072E-5,1.9209296871267E-5,
1.95234416882563E-5,2.37637844577567E-5,2.61487188977274E-5),
 .UNSPECIFIED.);
#25129=B_SPLINE_CURVE_WITH_KNOTS('',3,(#385102,#385103,#385104,#385105,
#385106,#385107,#385108,#385109,#385110,#385111,#385112,#385113,#385114,
#385115,#385116,#385117,#385118,#385119,#385120,#385121,#385122,#385123,
#385124,#385125,#385126,#385127,#385128,#385129,#385130,#385131,#385132),
 .UNSPECIFIED.,.F.,.F.,(4,3,3,3,3,3,3,3,3,3,4),(0.,3.95507910397923E-6,
7.53768426604195E-6,1.19904533335349E-5,1.40475043392586E-5,1.51452104275964E-5,
1.67866272814122E-5,1.69621513005357E-5,1.81338315460711E-5,1.98906334656528E-5,
2.06132424588245E-5),.UNSPECIFIED.);
#25130=B_SPLINE_CURVE_WITH_KNOTS('',3,(#385135,#385136,#385137,#385138),
 .UNSPECIFIED.,.F.,.F.,(4,4),(1.06229684024259E-18,0.00010938435327491),
 .UNSPECIFIED.);
#25131=B_SPLINE_CURVE_WITH_KNOTS('',3,(#385165,#385166,#385167,#385168,
#385169,#385170,#385171,#385172,#385173,#385174,#385175,#385176,#385177,
#385178,#385179,#385180,#385181,#385182,#385183,#385184,#385185,#385186,
#385187,#385188,#385189,#385190,#385191,#385192,#385193,#385194,#385195,
#385196,#385197,#385198),.UNSPECIFIED.,.F.,.F.,(4,3,3,3,3,3,3,3,3,3,3,4),
(0.,2.09623992729422E-6,3.17176647120225E-6,4.82636181943692E-6,5.01000917339947E-6,
6.13126454147503E-6,8.6048665028885E-6,9.2114428117048E-6,1.24722301135852E-5,
1.42666454787854E-5,2.04670653756892E-5,2.080264381768E-5),
 .UNSPECIFIED.);
#25132=B_SPLINE_CURVE_WITH_KNOTS('',3,(#385199,#385200,#385201,#385202),
 .UNSPECIFIED.,.F.,.F.,(4,4),(0.,0.000109384345496908),.UNSPECIFIED.);
#25133=B_SPLINE_CURVE_WITH_KNOTS('',3,(#385307,#385308,#385309,#385310),
 .UNSPECIFIED.,.F.,.F.,(4,4),(0.,9.54361881492175E-5),.UNSPECIFIED.);
#25134=B_SPLINE_CURVE_WITH_KNOTS('',3,(#385315,#385316,#385317,#385318,
#385319,#385320,#385321),.UNSPECIFIED.,.F.,.F.,(4,3,4),(0.,4.41069704323467E-5,
0.000113970027818833),.UNSPECIFIED.);
#25135=B_SPLINE_CURVE_WITH_KNOTS('',3,(#385327,#385328,#385329,#385330),
 .UNSPECIFIED.,.F.,.F.,(4,4),(2.16840434497101E-19,9.54361881492181E-5),
 .UNSPECIFIED.);
#25136=B_SPLINE_CURVE_WITH_KNOTS('',3,(#385334,#385335,#385336,#385337,
#385338,#385339,#385340),.UNSPECIFIED.,.F.,.F.,(4,3,4),(0.,6.9863024419149E-5,
0.000113969974038089),.UNSPECIFIED.);
#25137=B_SPLINE_CURVE_WITH_KNOTS('',3,(#385343,#385344,#385345,#385346,
#385347,#385348,#385349,#385350,#385351,#385352,#385353,#385354,#385355,
#385356,#385357,#385358,#385359,#385360,#385361,#385362,#385363,#385364,
#385365,#385366,#385367,#385368,#385369,#385370,#385371,#385372,#385373,
#385374,#385375,#385376,#385377,#385378,#385379,#385380,#385381,#385382,
#385383,#385384,#385385,#385386,#385387,#385388,#385389,#385390,#385391),
 .UNSPECIFIED.,.F.,.F.,(4,3,3,3,3,3,3,3,3,3,3,3,3,3,3,3,4),(0.,1.53100299373411E-6,
4.52554775679572E-6,7.01151246291604E-6,9.26752933799538E-6,1.03084066197173E-5,
1.1713899082686E-5,1.22284894984074E-5,1.30315035324819E-5,1.3836372849781E-5,
1.40464197777494E-5,1.54597749564636E-5,1.62073588704066E-5,1.9209296871214E-5,
1.95234416882551E-5,2.37637844577601E-5,2.61487188977252E-5),
 .UNSPECIFIED.);
#25138=B_SPLINE_CURVE_WITH_KNOTS('',3,(#385406,#385407,#385408,#385409,
#385410,#385411,#385412,#385413,#385414,#385415,#385416,#385417,#385418,
#385419,#385420,#385421,#385422,#385423,#385424,#385425,#385426,#385427,
#385428,#385429,#385430,#385431,#385432,#385433,#385434,#385435,#385436),
 .UNSPECIFIED.,.F.,.F.,(4,3,3,3,3,3,3,3,3,3,4),(0.,3.95507910398871E-6,
7.53768426604198E-6,1.19904533335351E-5,1.40475043392587E-5,1.51452104275964E-5,
1.67866272814358E-5,1.6962151300536E-5,1.81338315460713E-5,1.98906334656512E-5,
2.06132424588245E-5),.UNSPECIFIED.);
#25139=B_SPLINE_CURVE_WITH_KNOTS('',3,(#385439,#385440,#385441,#385442),
 .UNSPECIFIED.,.F.,.F.,(4,4),(6.1331736667335E-19,0.00010938435327491),
 .UNSPECIFIED.);
#25140=B_SPLINE_CURVE_WITH_KNOTS('',3,(#385469,#385470,#385471,#385472,
#385473,#385474,#385475,#385476,#385477,#385478,#385479,#385480,#385481,
#385482,#385483,#385484,#385485,#385486,#385487,#385488,#385489,#385490,
#385491,#385492,#385493,#385494,#385495,#385496,#385497,#385498,#385499,
#385500,#385501,#385502),.UNSPECIFIED.,.F.,.F.,(4,3,3,3,3,3,3,3,3,3,3,4),
(2.16840434497101E-19,2.09623992729438E-6,3.17176647120237E-6,4.82636181943731E-6,
5.01000917339986E-6,6.13126454147497E-6,8.60486650288864E-6,9.21144281170504E-6,
1.24722301135917E-5,1.42666454787861E-5,2.04670653756963E-5,2.08026438176811E-5),
 .UNSPECIFIED.);
#25141=B_SPLINE_CURVE_WITH_KNOTS('',3,(#385503,#385504,#385505,#385506),
 .UNSPECIFIED.,.F.,.F.,(4,4),(0.,0.000109384345496908),.UNSPECIFIED.);
#25142=B_SPLINE_CURVE_WITH_KNOTS('',3,(#385611,#385612,#385613,#385614),
 .UNSPECIFIED.,.F.,.F.,(4,4),(0.,9.54361881492172E-5),.UNSPECIFIED.);
#25143=B_SPLINE_CURVE_WITH_KNOTS('',3,(#385619,#385620,#385621,#385622,
#385623,#385624,#385625),.UNSPECIFIED.,.F.,.F.,(4,3,4),(0.,4.41069704323469E-5,
0.000113970027818833),.UNSPECIFIED.);
#25144=B_SPLINE_CURVE_WITH_KNOTS('',3,(#385631,#385632,#385633,#385634),
 .UNSPECIFIED.,.F.,.F.,(4,4),(2.16840434497101E-19,9.54361881492179E-5),
 .UNSPECIFIED.);
#25145=B_SPLINE_CURVE_WITH_KNOTS('',3,(#385638,#385639,#385640,#385641,
#385642,#385643,#385644),.UNSPECIFIED.,.F.,.F.,(4,3,4),(0.,6.9863024419149E-5,
0.000113969974038089),.UNSPECIFIED.);
#25146=B_SPLINE_CURVE_WITH_KNOTS('',3,(#385647,#385648,#385649,#385650,
#385651,#385652,#385653,#385654,#385655,#385656,#385657,#385658,#385659,
#385660,#385661,#385662,#385663,#385664,#385665,#385666,#385667,#385668,
#385669,#385670,#385671,#385672,#385673,#385674,#385675,#385676,#385677,
#385678,#385679,#385680,#385681,#385682,#385683,#385684,#385685,#385686,
#385687,#385688,#385689,#385690,#385691,#385692,#385693,#385694,#385695),
 .UNSPECIFIED.,.F.,.F.,(4,3,3,3,3,3,3,3,3,3,3,3,3,3,3,3,4),(0.,1.53100299373413E-6,
4.52554775679023E-6,7.01151246291602E-6,9.26752933801105E-6,1.03084066197174E-5,
1.17138990826861E-5,1.22284894984072E-5,1.30315035324816E-5,1.38363728497811E-5,
1.40464197777495E-5,1.54597749564638E-5,1.62073588704065E-5,1.92092968712831E-5,
1.95234416882549E-5,2.37637844577551E-5,2.61487188977251E-5),
 .UNSPECIFIED.);
#25147=B_SPLINE_CURVE_WITH_KNOTS('',3,(#385710,#385711,#385712,#385713,
#385714,#385715,#385716,#385717,#385718,#385719,#385720,#385721,#385722,
#385723,#385724,#385725,#385726,#385727,#385728,#385729,#385730,#385731,
#385732,#385733,#385734,#385735,#385736,#385737,#385738,#385739,#385740),
 .UNSPECIFIED.,.F.,.F.,(4,3,3,3,3,3,3,3,3,3,4),(0.,3.95507910397591E-6,
7.53768426604203E-6,1.19904533335351E-5,1.40475043392586E-5,1.51452104275964E-5,
1.67866272814308E-5,1.69621513005358E-5,1.81338315460711E-5,1.98906334656559E-5,
2.06132424588246E-5),.UNSPECIFIED.);
#25148=B_SPLINE_CURVE_WITH_KNOTS('',3,(#385743,#385744,#385745,#385746),
 .UNSPECIFIED.,.F.,.F.,(4,4),(6.1331736667335E-19,0.00010938435327491),
 .UNSPECIFIED.);
#25149=B_SPLINE_CURVE_WITH_KNOTS('',3,(#385773,#385774,#385775,#385776,
#385777,#385778,#385779,#385780,#385781,#385782,#385783,#385784,#385785,
#385786,#385787,#385788,#385789,#385790,#385791,#385792,#385793,#385794,
#385795,#385796,#385797,#385798,#385799,#385800,#385801,#385802,#385803,
#385804,#385805,#385806),.UNSPECIFIED.,.F.,.F.,(4,3,3,3,3,3,3,3,3,3,3,4),
(0.,2.09623992729445E-6,3.17176647120217E-6,4.82636181944129E-6,5.01000917339974E-6,
6.13126454147491E-6,8.60486650288863E-6,9.21144281170486E-6,1.24722301136039E-5,
1.42666454787853E-5,2.0467065375687E-5,2.08026438176795E-5),
 .UNSPECIFIED.);
#25150=B_SPLINE_CURVE_WITH_KNOTS('',3,(#385807,#385808,#385809,#385810),
 .UNSPECIFIED.,.F.,.F.,(4,4),(0.,0.000109384345496908),.UNSPECIFIED.);
#25151=B_SPLINE_CURVE_WITH_KNOTS('',3,(#385915,#385916,#385917,#385918),
 .UNSPECIFIED.,.F.,.F.,(4,4),(0.,9.54361881492176E-5),.UNSPECIFIED.);
#25152=B_SPLINE_CURVE_WITH_KNOTS('',3,(#385923,#385924,#385925,#385926,
#385927,#385928,#385929),.UNSPECIFIED.,.F.,.F.,(4,3,4),(0.,4.41069704323467E-5,
0.000113970027818833),.UNSPECIFIED.);
#25153=B_SPLINE_CURVE_WITH_KNOTS('',3,(#385935,#385936,#385937,#385938),
 .UNSPECIFIED.,.F.,.F.,(4,4),(4.84869951806108E-19,9.54361881492178E-5),
 .UNSPECIFIED.);
#25154=B_SPLINE_CURVE_WITH_KNOTS('',3,(#385942,#385943,#385944,#385945,
#385946,#385947,#385948),.UNSPECIFIED.,.F.,.F.,(4,3,4),(0.,6.9863024419149E-5,
0.000113969974038089),.UNSPECIFIED.);
#25155=B_SPLINE_CURVE_WITH_KNOTS('',3,(#385951,#385952,#385953,#385954,
#385955,#385956,#385957,#385958,#385959,#385960,#385961,#385962,#385963,
#385964,#385965,#385966,#385967,#385968,#385969,#385970,#385971,#385972,
#385973,#385974,#385975,#385976,#385977,#385978,#385979,#385980,#385981,
#385982,#385983,#385984,#385985,#385986,#385987,#385988,#385989,#385990,
#385991,#385992,#385993,#385994,#385995,#385996,#385997,#385998,#385999),
 .UNSPECIFIED.,.F.,.F.,(4,3,3,3,3,3,3,3,3,3,3,3,3,3,3,3,4),(0.,1.53100299373415E-6,
4.52554775680005E-6,7.01151246291607E-6,9.26752933800049E-6,1.03084066197174E-5,
1.17138990826862E-5,1.22284894984074E-5,1.30315035324819E-5,1.38363728497813E-5,
1.40464197777493E-5,1.5459774956464E-5,1.6207358870407E-5,1.92092968712743E-5,
1.95234416882557E-5,2.3763784457763E-5,2.61487188977264E-5),
 .UNSPECIFIED.);
#25156=B_SPLINE_CURVE_WITH_KNOTS('',3,(#386014,#386015,#386016,#386017,
#386018,#386019,#386020,#386021,#386022,#386023,#386024,#386025,#386026,
#386027,#386028,#386029,#386030,#386031,#386032,#386033,#386034,#386035,
#386036,#386037,#386038,#386039,#386040,#386041,#386042,#386043,#386044),
 .UNSPECIFIED.,.F.,.F.,(4,3,3,3,3,3,3,3,3,3,4),(0.,3.95507910398088E-6,
7.53768426604196E-6,1.1990453333535E-5,1.40475043392586E-5,1.51452104275965E-5,
1.6786627281432E-5,1.69621513005358E-5,1.81338315460712E-5,1.98906334656528E-5,
2.06132424588243E-5),.UNSPECIFIED.);
#25157=B_SPLINE_CURVE_WITH_KNOTS('',3,(#386047,#386048,#386049,#386050),
 .UNSPECIFIED.,.F.,.F.,(4,4),(4.84869951806108E-19,0.00010938435327491),
 .UNSPECIFIED.);
#25158=B_SPLINE_CURVE_WITH_KNOTS('',3,(#386077,#386078,#386079,#386080,
#386081,#386082,#386083,#386084,#386085,#386086,#386087,#386088,#386089,
#386090,#386091,#386092,#386093,#386094,#386095,#386096,#386097,#386098,
#386099,#386100,#386101,#386102,#386103,#386104,#386105,#386106,#386107,
#386108,#386109,#386110),.UNSPECIFIED.,.F.,.F.,(4,3,3,3,3,3,3,3,3,3,3,4),
(1.0842021724855E-19,2.0962399272944E-6,3.17176647120221E-6,4.82636181943783E-6,
5.01000917339964E-6,6.13126454147497E-6,8.60486650288854E-6,9.2114428117049E-6,
1.24722301135937E-5,1.42666454787856E-5,2.046706537569E-5,2.08026438176804E-5),
 .UNSPECIFIED.);
#25159=B_SPLINE_CURVE_WITH_KNOTS('',3,(#386111,#386112,#386113,#386114),
 .UNSPECIFIED.,.F.,.F.,(4,4),(0.,0.000109384345496908),.UNSPECIFIED.);
#25160=B_SPLINE_CURVE_WITH_KNOTS('',3,(#386219,#386220,#386221,#386222),
 .UNSPECIFIED.,.F.,.F.,(4,4),(0.,9.54361881492172E-5),.UNSPECIFIED.);
#25161=B_SPLINE_CURVE_WITH_KNOTS('',3,(#386227,#386228,#386229,#386230,
#386231,#386232,#386233),.UNSPECIFIED.,.F.,.F.,(4,3,4),(0.,4.4106970432347E-5,
0.000113970027818833),.UNSPECIFIED.);
#25162=B_SPLINE_CURVE_WITH_KNOTS('',3,(#386239,#386240,#386241,#386242),
 .UNSPECIFIED.,.F.,.F.,(4,4),(2.16840434497101E-19,9.54361881492179E-5),
 .UNSPECIFIED.);
#25163=B_SPLINE_CURVE_WITH_KNOTS('',3,(#386246,#386247,#386248,#386249,
#386250,#386251,#386252),.UNSPECIFIED.,.F.,.F.,(4,3,4),(0.,6.98630244191491E-5,
0.000113969974038089),.UNSPECIFIED.);
#25164=B_SPLINE_CURVE_WITH_KNOTS('',3,(#386255,#386256,#386257,#386258,
#386259,#386260,#386261,#386262,#386263,#386264,#386265,#386266,#386267,
#386268,#386269,#386270,#386271,#386272,#386273,#386274,#386275,#386276,
#386277,#386278,#386279,#386280,#386281,#386282,#386283,#386284,#386285,
#386286,#386287,#386288,#386289,#386290,#386291,#386292,#386293,#386294,
#386295,#386296,#386297,#386298,#386299,#386300,#386301,#386302,#386303),
 .UNSPECIFIED.,.F.,.F.,(4,3,3,3,3,3,3,3,3,3,3,3,3,3,3,3,4),(0.,1.53100299373414E-6,
4.52554775678893E-6,7.01151246291594E-6,9.26752933800309E-6,1.03084066197173E-5,
1.17138990826862E-5,1.22284894984075E-5,1.30315035324817E-5,1.38363728497811E-5,
1.40464197777493E-5,1.54597749564637E-5,1.62073588704067E-5,1.92092968712795E-5,
1.95234416882552E-5,2.37637844577611E-5,2.61487188977259E-5),
 .UNSPECIFIED.);
#25165=B_SPLINE_CURVE_WITH_KNOTS('',3,(#386318,#386319,#386320,#386321,
#386322,#386323,#386324,#386325,#386326,#386327,#386328,#386329,#386330,
#386331,#386332,#386333,#386334,#386335,#386336,#386337,#386338,#386339,
#386340,#386341,#386342,#386343,#386344,#386345,#386346,#386347,#386348),
 .UNSPECIFIED.,.F.,.F.,(4,3,3,3,3,3,3,3,3,3,4),(0.,3.95507910398021E-6,
7.53768426604196E-6,1.1990453333535E-5,1.40475043392586E-5,1.51452104275966E-5,
1.67866272814092E-5,1.6962151300536E-5,1.81338315460713E-5,1.98906334656543E-5,
2.06132424588247E-5),.UNSPECIFIED.);
#25166=B_SPLINE_CURVE_WITH_KNOTS('',3,(#386351,#386352,#386353,#386354),
 .UNSPECIFIED.,.F.,.F.,(4,4),(5.42101086242752E-19,0.00010938435327491),
 .UNSPECIFIED.);
#25167=B_SPLINE_CURVE_WITH_KNOTS('',3,(#386381,#386382,#386383,#386384,
#386385,#386386,#386387,#386388,#386389,#386390,#386391,#386392,#386393,
#386394,#386395,#386396,#386397,#386398,#386399,#386400,#386401,#386402,
#386403,#386404,#386405,#386406,#386407,#386408,#386409,#386410,#386411,
#386412,#386413,#386414),.UNSPECIFIED.,.F.,.F.,(4,3,3,3,3,3,3,3,3,3,3,4),
(1.0842021724855E-19,2.09623992729453E-6,3.17176647120237E-6,4.82636181943783E-6,
5.0100091733997E-6,6.13126454147507E-6,8.60486650288873E-6,9.21144281170509E-6,
1.2472230113601E-5,1.42666454787859E-5,2.04670653757014E-5,2.08026438176806E-5),
 .UNSPECIFIED.);
#25168=B_SPLINE_CURVE_WITH_KNOTS('',3,(#386415,#386416,#386417,#386418),
 .UNSPECIFIED.,.F.,.F.,(4,4),(0.,0.000109384345496908),.UNSPECIFIED.);
#25169=B_SPLINE_CURVE_WITH_KNOTS('',3,(#386523,#386524,#386525,#386526),
 .UNSPECIFIED.,.F.,.F.,(4,4),(0.,9.54361881492174E-5),.UNSPECIFIED.);
#25170=B_SPLINE_CURVE_WITH_KNOTS('',3,(#386531,#386532,#386533,#386534,
#386535,#386536,#386537),.UNSPECIFIED.,.F.,.F.,(4,3,4),(0.,4.41069704323469E-5,
0.000113970027818833),.UNSPECIFIED.);
#25171=B_SPLINE_CURVE_WITH_KNOTS('',3,(#386543,#386544,#386545,#386546),
 .UNSPECIFIED.,.F.,.F.,(4,4),(4.84869951806108E-19,9.54361881492178E-5),
 .UNSPECIFIED.);
#25172=B_SPLINE_CURVE_WITH_KNOTS('',3,(#386550,#386551,#386552,#386553,
#386554,#386555,#386556),.UNSPECIFIED.,.F.,.F.,(4,3,4),(0.,6.98630244191491E-5,
0.000113969974038089),.UNSPECIFIED.);
#25173=B_SPLINE_CURVE_WITH_KNOTS('',3,(#386559,#386560,#386561,#386562,
#386563,#386564,#386565,#386566,#386567,#386568,#386569,#386570,#386571,
#386572,#386573,#386574,#386575,#386576,#386577,#386578,#386579,#386580,
#386581,#386582,#386583,#386584,#386585,#386586,#386587,#386588,#386589,
#386590,#386591,#386592,#386593,#386594,#386595,#386596,#386597,#386598,
#386599,#386600,#386601,#386602,#386603,#386604,#386605,#386606,#386607),
 .UNSPECIFIED.,.F.,.F.,(4,3,3,3,3,3,3,3,3,3,3,3,3,3,3,3,4),(0.,1.53100299373411E-6,
4.52554775679701E-6,7.01151246291601E-6,9.26752933800774E-6,1.03084066197173E-5,
1.17138990826861E-5,1.22284894984073E-5,1.30315035324816E-5,1.38363728497812E-5,
1.40464197777494E-5,1.54597749564639E-5,1.62073588704066E-5,1.9209296871257E-5,
1.9523441688255E-5,2.37637844577588E-5,2.61487188977256E-5),
 .UNSPECIFIED.);
#25174=B_SPLINE_CURVE_WITH_KNOTS('',3,(#386622,#386623,#386624,#386625,
#386626,#386627,#386628,#386629,#386630,#386631,#386632,#386633,#386634,
#386635,#386636,#386637,#386638,#386639,#386640,#386641,#386642,#386643,
#386644,#386645,#386646,#386647,#386648,#386649,#386650,#386651,#386652),
 .UNSPECIFIED.,.F.,.F.,(4,3,3,3,3,3,3,3,3,3,4),(0.,3.95507910398915E-6,
7.53768426604197E-6,1.1990453333535E-5,1.40475043392585E-5,1.51452104275964E-5,
1.67866272813909E-5,1.69621513005358E-5,1.81338315460713E-5,1.98906334656509E-5,
2.06132424588247E-5),.UNSPECIFIED.);
#25175=B_SPLINE_CURVE_WITH_KNOTS('',3,(#386655,#386656,#386657,#386658),
 .UNSPECIFIED.,.F.,.F.,(4,4),(5.42101086242752E-19,0.00010938435327491),
 .UNSPECIFIED.);
#25176=B_SPLINE_CURVE_WITH_KNOTS('',3,(#386685,#386686,#386687,#386688,
#386689,#386690,#386691,#386692,#386693,#386694,#386695,#386696,#386697,
#386698,#386699,#386700,#386701,#386702,#386703,#386704,#386705,#386706,
#386707,#386708,#386709,#386710,#386711,#386712,#386713,#386714,#386715,
#386716,#386717,#386718),.UNSPECIFIED.,.F.,.F.,(4,3,3,3,3,3,3,3,3,3,3,4),
(1.0842021724855E-19,2.09623992729424E-6,3.17176647120218E-6,4.82636181943516E-6,
5.01000917339966E-6,6.13126454147493E-6,8.60486650288855E-6,9.21144281170494E-6,
1.24722301135922E-5,1.42666454787859E-5,2.04670653757106E-5,2.08026438176806E-5),
 .UNSPECIFIED.);
#25177=B_SPLINE_CURVE_WITH_KNOTS('',3,(#386719,#386720,#386721,#386722),
 .UNSPECIFIED.,.F.,.F.,(4,4),(0.,0.000109384345496908),.UNSPECIFIED.);
#25178=B_SPLINE_CURVE_WITH_KNOTS('',3,(#386827,#386828,#386829,#386830),
 .UNSPECIFIED.,.F.,.F.,(4,4),(0.,9.54361881492175E-5),.UNSPECIFIED.);
#25179=B_SPLINE_CURVE_WITH_KNOTS('',3,(#386835,#386836,#386837,#386838,
#386839,#386840,#386841),.UNSPECIFIED.,.F.,.F.,(4,3,4),(0.,4.4106970432347E-5,
0.000113970027818833),.UNSPECIFIED.);
#25180=B_SPLINE_CURVE_WITH_KNOTS('',3,(#386847,#386848,#386849,#386850),
 .UNSPECIFIED.,.F.,.F.,(4,4),(5.42101086242752E-20,9.54361881492179E-5),
 .UNSPECIFIED.);
#25181=B_SPLINE_CURVE_WITH_KNOTS('',3,(#386854,#386855,#386856,#386857,
#386858,#386859,#386860),.UNSPECIFIED.,.F.,.F.,(4,3,4),(0.,6.9863024419149E-5,
0.00011396997403809),.UNSPECIFIED.);
#25182=B_SPLINE_CURVE_WITH_KNOTS('',3,(#386863,#386864,#386865,#386866,
#386867,#386868,#386869,#386870,#386871,#386872,#386873,#386874,#386875,
#386876,#386877,#386878,#386879,#386880,#386881,#386882,#386883,#386884,
#386885,#386886,#386887,#386888,#386889,#386890,#386891,#386892,#386893,
#386894,#386895,#386896,#386897,#386898,#386899,#386900,#386901,#386902,
#386903,#386904,#386905,#386906,#386907,#386908,#386909,#386910,#386911),
 .UNSPECIFIED.,.F.,.F.,(4,3,3,3,3,3,3,3,3,3,3,3,3,3,3,3,4),(0.,1.53100299373402E-6,
4.5255477568009E-6,7.01151246291603E-6,9.26752933799214E-6,1.03084066197173E-5,
1.17138990826862E-5,1.22284894984075E-5,1.30315035324817E-5,1.38363728497813E-5,
1.40464197777494E-5,1.5459774956464E-5,1.62073588704069E-5,1.92092968712782E-5,
1.95234416882555E-5,2.37637844577588E-5,2.61487188977261E-5),
 .UNSPECIFIED.);
#25183=B_SPLINE_CURVE_WITH_KNOTS('',3,(#386926,#386927,#386928,#386929,
#386930,#386931,#386932,#386933,#386934,#386935,#386936,#386937,#386938,
#386939,#386940,#386941,#386942,#386943,#386944,#386945,#386946,#386947,
#386948,#386949,#386950,#386951,#386952,#386953,#386954,#386955,#386956),
 .UNSPECIFIED.,.F.,.F.,(4,3,3,3,3,3,3,3,3,3,4),(0.,3.95507910398505E-6,
7.53768426604191E-6,1.19904533335349E-5,1.40475043392584E-5,1.51452104275963E-5,
1.67866272814112E-5,1.69621513005357E-5,1.81338315460712E-5,1.98906334656516E-5,
2.06132424588245E-5),.UNSPECIFIED.);
#25184=B_SPLINE_CURVE_WITH_KNOTS('',3,(#386959,#386960,#386961,#386962),
 .UNSPECIFIED.,.F.,.F.,(4,4),(5.11417141928151E-19,0.00010938435327491),
 .UNSPECIFIED.);
#25185=B_SPLINE_CURVE_WITH_KNOTS('',3,(#386989,#386990,#386991,#386992,
#386993,#386994,#386995,#386996,#386997,#386998,#386999,#387000,#387001,
#387002,#387003,#387004,#387005,#387006,#387007,#387008,#387009,#387010,
#387011,#387012,#387013,#387014,#387015,#387016,#387017,#387018,#387019,
#387020,#387021,#387022),.UNSPECIFIED.,.F.,.F.,(4,3,3,3,3,3,3,3,3,3,3,4),
(1.0842021724855E-19,2.09623992729433E-6,3.17176647120215E-6,4.82636181943702E-6,
5.01000917339958E-6,6.13126454147485E-6,8.60486650288838E-6,9.21144281170471E-6,
1.24722301135986E-5,1.42666454787852E-5,2.0467065375669E-5,2.08026438176793E-5),
 .UNSPECIFIED.);
#25186=B_SPLINE_CURVE_WITH_KNOTS('',3,(#387023,#387024,#387025,#387026),
 .UNSPECIFIED.,.F.,.F.,(4,4),(0.,0.000109384345496908),.UNSPECIFIED.);
#25187=B_SPLINE_CURVE_WITH_KNOTS('',3,(#387131,#387132,#387133,#387134),
 .UNSPECIFIED.,.F.,.F.,(4,4),(0.,9.54361881492177E-5),.UNSPECIFIED.);
#25188=B_SPLINE_CURVE_WITH_KNOTS('',3,(#387139,#387140,#387141,#387142,
#387143,#387144,#387145),.UNSPECIFIED.,.F.,.F.,(4,3,4),(0.,4.41069704323471E-5,
0.000113970027818834),.UNSPECIFIED.);
#25189=B_SPLINE_CURVE_WITH_KNOTS('',3,(#387151,#387152,#387153,#387154),
 .UNSPECIFIED.,.F.,.F.,(4,4),(4.63171371119878E-19,9.5436188149218E-5),
 .UNSPECIFIED.);
#25190=B_SPLINE_CURVE_WITH_KNOTS('',3,(#387158,#387159,#387160,#387161,
#387162,#387163,#387164),.UNSPECIFIED.,.F.,.F.,(4,3,4),(0.,6.98630244191489E-5,
0.000113969974038089),.UNSPECIFIED.);
#25191=B_SPLINE_CURVE_WITH_KNOTS('',3,(#387167,#387168,#387169,#387170,
#387171,#387172,#387173,#387174,#387175,#387176,#387177,#387178,#387179,
#387180,#387181,#387182,#387183,#387184,#387185,#387186,#387187,#387188,
#387189,#387190,#387191,#387192,#387193,#387194,#387195,#387196,#387197,
#387198,#387199,#387200,#387201,#387202,#387203,#387204,#387205,#387206,
#387207,#387208,#387209,#387210,#387211,#387212,#387213,#387214,#387215),
 .UNSPECIFIED.,.F.,.F.,(4,3,3,3,3,3,3,3,3,3,3,3,3,3,3,3,4),(0.,1.53100299373415E-6,
4.52554775679312E-6,7.01151246291606E-6,9.26752933799493E-6,1.03084066197173E-5,
1.17138990826862E-5,1.22284894984075E-5,1.30315035324818E-5,1.38363728497814E-5,
1.40464197777495E-5,1.54597749564641E-5,1.62073588704068E-5,1.9209296871244E-5,
1.95234416882555E-5,2.37637844577537E-5,2.61487188977259E-5),
 .UNSPECIFIED.);
#25192=B_SPLINE_CURVE_WITH_KNOTS('',3,(#387230,#387231,#387232,#387233,
#387234,#387235,#387236,#387237,#387238,#387239,#387240,#387241,#387242,
#387243,#387244,#387245,#387246,#387247,#387248,#387249,#387250,#387251,
#387252,#387253,#387254,#387255,#387256,#387257,#387258,#387259,#387260),
 .UNSPECIFIED.,.F.,.F.,(4,3,3,3,3,3,3,3,3,3,4),(0.,3.95507910398497E-6,
7.53768426604194E-6,1.1990453333535E-5,1.40475043392585E-5,1.51452104275964E-5,
1.67866272814021E-5,1.69621513005358E-5,1.81338315460712E-5,1.98906334656536E-5,
2.06132424588244E-5),.UNSPECIFIED.);
#25193=B_SPLINE_CURVE_WITH_KNOTS('',3,(#387263,#387264,#387265,#387266),
 .UNSPECIFIED.,.F.,.F.,(4,4),(4.84869951806108E-19,0.00010938435327491),
 .UNSPECIFIED.);
#25194=B_SPLINE_CURVE_WITH_KNOTS('',3,(#387293,#387294,#387295,#387296,
#387297,#387298,#387299,#387300,#387301,#387302,#387303,#387304,#387305,
#387306,#387307,#387308,#387309,#387310,#387311,#387312,#387313,#387314,
#387315,#387316,#387317,#387318,#387319,#387320,#387321,#387322,#387323,
#387324,#387325,#387326),.UNSPECIFIED.,.F.,.F.,(4,3,3,3,3,3,3,3,3,3,3,4),
(1.62630325872826E-19,2.09623992729446E-6,3.17176647120217E-6,4.8263618194318E-6,
5.01000917339966E-6,6.13126454147499E-6,8.60486650288858E-6,9.21144281170497E-6,
1.24722301136006E-5,1.42666454787858E-5,2.04670653756983E-5,2.08026438176805E-5),
 .UNSPECIFIED.);
#25195=B_SPLINE_CURVE_WITH_KNOTS('',3,(#387327,#387328,#387329,#387330),
 .UNSPECIFIED.,.F.,.F.,(4,4),(0.,0.000109384345496908),.UNSPECIFIED.);
#25196=B_SPLINE_CURVE_WITH_KNOTS('',3,(#387435,#387436,#387437,#387438),
 .UNSPECIFIED.,.F.,.F.,(4,4),(0.,9.54361881492175E-5),.UNSPECIFIED.);
#25197=B_SPLINE_CURVE_WITH_KNOTS('',3,(#387443,#387444,#387445,#387446,
#387447,#387448,#387449),.UNSPECIFIED.,.F.,.F.,(4,3,4),(0.,4.41069704323468E-5,
0.000113970027818834),.UNSPECIFIED.);
#25198=B_SPLINE_CURVE_WITH_KNOTS('',3,(#387455,#387456,#387457,#387458),
 .UNSPECIFIED.,.F.,.F.,(4,4),(4.5436350575631E-19,9.54361881492175E-5),
 .UNSPECIFIED.);
#25199=B_SPLINE_CURVE_WITH_KNOTS('',3,(#387462,#387463,#387464,#387465,
#387466,#387467,#387468),.UNSPECIFIED.,.F.,.F.,(4,3,4),(0.,6.98630244191489E-5,
0.000113969974038089),.UNSPECIFIED.);
#25200=B_SPLINE_CURVE_WITH_KNOTS('',3,(#387471,#387472,#387473,#387474,
#387475,#387476,#387477,#387478,#387479,#387480,#387481,#387482,#387483,
#387484,#387485,#387486,#387487,#387488,#387489,#387490,#387491,#387492,
#387493,#387494,#387495,#387496,#387497,#387498,#387499,#387500,#387501,
#387502,#387503,#387504,#387505,#387506,#387507,#387508,#387509,#387510,
#387511,#387512,#387513,#387514,#387515,#387516,#387517,#387518,#387519),
 .UNSPECIFIED.,.F.,.F.,(4,3,3,3,3,3,3,3,3,3,3,3,3,3,3,3,4),(0.,1.53100299373424E-6,
4.52554775679508E-6,7.01151246291611E-6,9.26752933800723E-6,1.03084066197174E-5,
1.17138990826861E-5,1.22284894984075E-5,1.30315035324817E-5,1.38363728497813E-5,
1.40464197777495E-5,1.5459774956464E-5,1.62073588704069E-5,1.9209296871253E-5,
1.95234416882555E-5,2.37637844577576E-5,2.61487188977262E-5),
 .UNSPECIFIED.);
#25201=B_SPLINE_CURVE_WITH_KNOTS('',3,(#387534,#387535,#387536,#387537,
#387538,#387539,#387540,#387541,#387542,#387543,#387544,#387545,#387546,
#387547,#387548,#387549,#387550,#387551,#387552,#387553,#387554,#387555,
#387556,#387557,#387558,#387559,#387560,#387561,#387562,#387563,#387564),
 .UNSPECIFIED.,.F.,.F.,(4,3,3,3,3,3,3,3,3,3,4),(0.,3.95507910397967E-6,
7.53768426604193E-6,1.19904533335349E-5,1.40475043392585E-5,1.51452104275964E-5,
1.67866272814196E-5,1.69621513005358E-5,1.81338315460712E-5,1.9890633465654E-5,
2.06132424588246E-5),.UNSPECIFIED.);
#25202=B_SPLINE_CURVE_WITH_KNOTS('',3,(#387567,#387568,#387569,#387570),
 .UNSPECIFIED.,.F.,.F.,(4,4),(4.84869951806108E-19,0.00010938435327491),
 .UNSPECIFIED.);
#25203=B_SPLINE_CURVE_WITH_KNOTS('',3,(#387597,#387598,#387599,#387600,
#387601,#387602,#387603,#387604,#387605,#387606,#387607,#387608,#387609,
#387610,#387611,#387612,#387613,#387614,#387615,#387616,#387617,#387618,
#387619,#387620,#387621,#387622,#387623,#387624,#387625,#387626,#387627,
#387628,#387629,#387630),.UNSPECIFIED.,.F.,.F.,(4,3,3,3,3,3,3,3,3,3,3,4),
(1.35525271560688E-19,2.0962399272944E-6,3.17176647120219E-6,4.82636181944153E-6,
5.01000917339958E-6,6.13126454147489E-6,8.60486650288847E-6,9.21144281170481E-6,
1.24722301136146E-5,1.42666454787853E-5,2.04670653756699E-5,2.08026438176797E-5),
 .UNSPECIFIED.);
#25204=B_SPLINE_CURVE_WITH_KNOTS('',3,(#387631,#387632,#387633,#387634),
 .UNSPECIFIED.,.F.,.F.,(4,4),(0.,0.000109384345496908),.UNSPECIFIED.);
#25205=B_SPLINE_CURVE_WITH_KNOTS('',3,(#387739,#387740,#387741,#387742),
 .UNSPECIFIED.,.F.,.F.,(4,4),(0.,9.54361881492175E-5),.UNSPECIFIED.);
#25206=B_SPLINE_CURVE_WITH_KNOTS('',3,(#387747,#387748,#387749,#387750,
#387751,#387752,#387753),.UNSPECIFIED.,.F.,.F.,(4,3,4),(0.,4.41069704323468E-5,
0.000113970027818833),.UNSPECIFIED.);
#25207=B_SPLINE_CURVE_WITH_KNOTS('',3,(#387759,#387760,#387761,#387762),
 .UNSPECIFIED.,.F.,.F.,(4,4),(4.48719651148014E-19,9.5436188149218E-5),
 .UNSPECIFIED.);
#25208=B_SPLINE_CURVE_WITH_KNOTS('',3,(#387766,#387767,#387768,#387769,
#387770,#387771,#387772),.UNSPECIFIED.,.F.,.F.,(4,3,4),(0.,6.98630244191489E-5,
0.000113969974038089),.UNSPECIFIED.);
#25209=B_SPLINE_CURVE_WITH_KNOTS('',3,(#387775,#387776,#387777,#387778,
#387779,#387780,#387781,#387782,#387783,#387784,#387785,#387786,#387787,
#387788,#387789,#387790,#387791,#387792,#387793,#387794,#387795,#387796,
#387797,#387798,#387799,#387800,#387801,#387802,#387803,#387804,#387805,
#387806,#387807,#387808,#387809,#387810,#387811,#387812,#387813,#387814,
#387815,#387816,#387817,#387818,#387819,#387820,#387821,#387822,#387823),
 .UNSPECIFIED.,.F.,.F.,(4,3,3,3,3,3,3,3,3,3,3,3,3,3,3,3,4),(0.,1.53100299373413E-6,
4.52554775679489E-6,7.01151246291594E-6,9.26752933800405E-6,1.03084066197173E-5,
1.17138990826861E-5,1.22284894984074E-5,1.30315035324817E-5,1.38363728497812E-5,
1.40464197777495E-5,1.54597749564639E-5,1.62073588704068E-5,1.92092968713333E-5,
1.95234416882555E-5,2.37637844577619E-5,2.61487188977262E-5),
 .UNSPECIFIED.);
#25210=B_SPLINE_CURVE_WITH_KNOTS('',3,(#387838,#387839,#387840,#387841,
#387842,#387843,#387844,#387845,#387846,#387847,#387848,#387849,#387850,
#387851,#387852,#387853,#387854,#387855,#387856,#387857,#387858,#387859,
#387860,#387861,#387862,#387863,#387864,#387865,#387866,#387867,#387868),
 .UNSPECIFIED.,.F.,.F.,(4,3,3,3,3,3,3,3,3,3,4),(0.,3.95507910398091E-6,
7.53768426604189E-6,1.1990453333535E-5,1.40475043392585E-5,1.51452104275964E-5,
1.67866272814286E-5,1.69621513005358E-5,1.81338315460712E-5,1.9890633465653E-5,
2.06132424588245E-5),.UNSPECIFIED.);
#25211=B_SPLINE_CURVE_WITH_KNOTS('',3,(#387871,#387872,#387873,#387874),
 .UNSPECIFIED.,.F.,.F.,(4,4),(4.73369422993816E-19,0.00010938435327491),
 .UNSPECIFIED.);
#25212=B_SPLINE_CURVE_WITH_KNOTS('',3,(#387901,#387902,#387903,#387904,
#387905,#387906,#387907,#387908,#387909,#387910,#387911,#387912,#387913,
#387914,#387915,#387916,#387917,#387918,#387919,#387920,#387921,#387922,
#387923,#387924,#387925,#387926,#387927,#387928,#387929,#387930,#387931,
#387932,#387933,#387934),.UNSPECIFIED.,.F.,.F.,(4,3,3,3,3,3,3,3,3,3,3,4),
(1.35525271560688E-19,2.09623992729438E-6,3.1717664712022E-6,4.82636181943525E-6,
5.0100091733996E-6,6.13126454147494E-6,8.6048665028885E-6,9.21144281170483E-6,
1.24722301136046E-5,1.42666454787854E-5,2.0467065375687E-5,2.08026438176799E-5),
 .UNSPECIFIED.);
#25213=B_SPLINE_CURVE_WITH_KNOTS('',3,(#387935,#387936,#387937,#387938),
 .UNSPECIFIED.,.F.,.F.,(4,4),(0.,0.000109384345496908),.UNSPECIFIED.);
#25214=B_SPLINE_CURVE_WITH_KNOTS('',3,(#388043,#388044,#388045,#388046),
 .UNSPECIFIED.,.F.,.F.,(4,4),(0.,9.5436188149217E-5),.UNSPECIFIED.);
#25215=B_SPLINE_CURVE_WITH_KNOTS('',3,(#388051,#388052,#388053,#388054,
#388055,#388056,#388057),.UNSPECIFIED.,.F.,.F.,(4,3,4),(0.,4.41069704323469E-5,
0.000113970027818833),.UNSPECIFIED.);
#25216=B_SPLINE_CURVE_WITH_KNOTS('',3,(#388063,#388064,#388065,#388066),
 .UNSPECIFIED.,.F.,.F.,(4,4),(4.47028007668187E-19,9.54361881492175E-5),
 .UNSPECIFIED.);
#25217=B_SPLINE_CURVE_WITH_KNOTS('',3,(#388070,#388071,#388072,#388073,
#388074,#388075,#388076),.UNSPECIFIED.,.F.,.F.,(4,3,4),(0.,6.9863024419149E-5,
0.000113969974038089),.UNSPECIFIED.);
#25218=B_SPLINE_CURVE_WITH_KNOTS('',3,(#388079,#388080,#388081,#388082,
#388083,#388084,#388085,#388086,#388087,#388088,#388089,#388090,#388091,
#388092,#388093,#388094,#388095,#388096,#388097,#388098,#388099,#388100,
#388101,#388102,#388103,#388104,#388105,#388106,#388107,#388108,#388109,
#388110,#388111,#388112,#388113,#388114,#388115,#388116,#388117,#388118,
#388119,#388120,#388121,#388122,#388123,#388124,#388125,#388126,#388127),
 .UNSPECIFIED.,.F.,.F.,(4,3,3,3,3,3,3,3,3,3,3,3,3,3,3,3,4),(0.,1.5310029937342E-6,
4.52554775679339E-6,7.01151246291608E-6,9.26752933799737E-6,1.03084066197173E-5,
1.17138990826863E-5,1.22284894984074E-5,1.30315035324817E-5,1.38363728497813E-5,
1.40464197777495E-5,1.54597749564639E-5,1.62073588704069E-5,1.92092968712856E-5,
1.95234416882552E-5,2.37637844577629E-5,2.61487188977258E-5),
 .UNSPECIFIED.);
#25219=B_SPLINE_CURVE_WITH_KNOTS('',3,(#388142,#388143,#388144,#388145,
#388146,#388147,#388148,#388149,#388150,#388151,#388152,#388153,#388154,
#388155,#388156,#388157,#388158,#388159,#388160,#388161,#388162,#388163,
#388164,#388165,#388166,#388167,#388168,#388169,#388170,#388171,#388172),
 .UNSPECIFIED.,.F.,.F.,(4,3,3,3,3,3,3,3,3,3,4),(0.,3.95507910398328E-6,
7.53768426604195E-6,1.19904533335349E-5,1.40475043392585E-5,1.51452104275964E-5,
1.67866272814049E-5,1.69621513005358E-5,1.81338315460712E-5,1.98906334656513E-5,
2.06132424588245E-5),.UNSPECIFIED.);
#25220=B_SPLINE_CURVE_WITH_KNOTS('',3,(#388175,#388176,#388177,#388178),
 .UNSPECIFIED.,.F.,.F.,(4,4),(4.63171371119878E-19,0.00010938435327491),
 .UNSPECIFIED.);
#25221=B_SPLINE_CURVE_WITH_KNOTS('',3,(#388205,#388206,#388207,#388208,
#388209,#388210,#388211,#388212,#388213,#388214,#388215,#388216,#388217,
#388218,#388219,#388220,#388221,#388222,#388223,#388224,#388225,#388226,
#388227,#388228,#388229,#388230,#388231,#388232,#388233,#388234,#388235,
#388236,#388237,#388238),.UNSPECIFIED.,.F.,.F.,(4,3,3,3,3,3,3,3,3,3,3,4),
(1.0842021724855E-19,2.09623992729441E-6,3.17176647120221E-6,4.82636181944583E-6,
5.0100091733996E-6,6.13126454147488E-6,8.60486650288823E-6,9.21144281170456E-6,
1.24722301136001E-5,1.42666454787847E-5,2.04670653757054E-5,2.08026438176787E-5),
 .UNSPECIFIED.);
#25222=B_SPLINE_CURVE_WITH_KNOTS('',3,(#388239,#388240,#388241,#388242),
 .UNSPECIFIED.,.F.,.F.,(4,4),(0.,0.000109384345496908),.UNSPECIFIED.);
#25223=B_SPLINE_CURVE_WITH_KNOTS('',3,(#388347,#388348,#388349,#388350),
 .UNSPECIFIED.,.F.,.F.,(4,4),(0.,9.54361881492172E-5),.UNSPECIFIED.);
#25224=B_SPLINE_CURVE_WITH_KNOTS('',3,(#388355,#388356,#388357,#388358,
#388359,#388360,#388361),.UNSPECIFIED.,.F.,.F.,(4,3,4),(0.,4.41069704323469E-5,
0.000113970027818833),.UNSPECIFIED.);
#25225=B_SPLINE_CURVE_WITH_KNOTS('',3,(#388367,#388368,#388369,#388370),
 .UNSPECIFIED.,.F.,.F.,(4,4),(4.47028007668187E-19,9.54361881492179E-5),
 .UNSPECIFIED.);
#25226=B_SPLINE_CURVE_WITH_KNOTS('',3,(#388374,#388375,#388376,#388377,
#388378,#388379,#388380),.UNSPECIFIED.,.F.,.F.,(4,3,4),(0.,6.98630244191492E-5,
0.000113969974038089),.UNSPECIFIED.);
#25227=B_SPLINE_CURVE_WITH_KNOTS('',3,(#388383,#388384,#388385,#388386,
#388387,#388388,#388389,#388390,#388391,#388392,#388393,#388394,#388395,
#388396,#388397,#388398,#388399,#388400,#388401,#388402,#388403,#388404,
#388405,#388406,#388407,#388408,#388409,#388410,#388411,#388412,#388413,
#388414,#388415,#388416,#388417,#388418,#388419,#388420,#388421,#388422,
#388423,#388424,#388425,#388426,#388427,#388428,#388429,#388430,#388431),
 .UNSPECIFIED.,.F.,.F.,(4,3,3,3,3,3,3,3,3,3,3,3,3,3,3,3,4),(0.,1.53100299373398E-6,
4.52554775679955E-6,7.01151246291586E-6,9.2675293380064E-6,1.03084066197173E-5,
1.17138990826862E-5,1.22284894984075E-5,1.30315035324817E-5,1.38363728497813E-5,
1.40464197777495E-5,1.54597749564641E-5,1.6207358870407E-5,1.92092968712452E-5,
1.95234416882558E-5,2.37637844577587E-5,2.61487188977266E-5),
 .UNSPECIFIED.);
#25228=B_SPLINE_CURVE_WITH_KNOTS('',3,(#388446,#388447,#388448,#388449,
#388450,#388451,#388452,#388453,#388454,#388455,#388456,#388457,#388458,
#388459,#388460,#388461,#388462,#388463,#388464,#388465,#388466,#388467,
#388468,#388469,#388470,#388471,#388472,#388473,#388474,#388475,#388476),
 .UNSPECIFIED.,.F.,.F.,(4,3,3,3,3,3,3,3,3,3,4),(0.,3.95507910397912E-6,
7.53768426604201E-6,1.1990453333535E-5,1.40475043392585E-5,1.51452104275963E-5,
1.6786627281435E-5,1.69621513005356E-5,1.81338315460709E-5,1.98906334656537E-5,
2.06132424588241E-5),.UNSPECIFIED.);
#25229=B_SPLINE_CURVE_WITH_KNOTS('',3,(#388479,#388480,#388481,#388482),
 .UNSPECIFIED.,.F.,.F.,(4,4),(4.63171371119878E-19,0.00010938435327491),
 .UNSPECIFIED.);
#25230=B_SPLINE_CURVE_WITH_KNOTS('',3,(#388509,#388510,#388511,#388512,
#388513,#388514,#388515,#388516,#388517,#388518,#388519,#388520,#388521,
#388522,#388523,#388524,#388525,#388526,#388527,#388528,#388529,#388530,
#388531,#388532,#388533,#388534,#388535,#388536,#388537,#388538,#388539,
#388540,#388541,#388542),.UNSPECIFIED.,.F.,.F.,(4,3,3,3,3,3,3,3,3,3,3,4),
(1.62630325872826E-19,2.0962399272944E-6,3.17176647120221E-6,4.82636181943954E-6,
5.01000917339966E-6,6.1312645414749E-6,8.60486650288846E-6,9.21144281170485E-6,
1.24722301136136E-5,1.42666454787854E-5,2.04670653756565E-5,2.080264381768E-5),
 .UNSPECIFIED.);
#25231=B_SPLINE_CURVE_WITH_KNOTS('',3,(#388543,#388544,#388545,#388546),
 .UNSPECIFIED.,.F.,.F.,(4,4),(0.,0.000109384345496908),.UNSPECIFIED.);
#25232=B_SPLINE_CURVE_WITH_KNOTS('',3,(#388651,#388652,#388653,#388654),
 .UNSPECIFIED.,.F.,.F.,(4,4),(0.,9.54361881492171E-5),.UNSPECIFIED.);
#25233=B_SPLINE_CURVE_WITH_KNOTS('',3,(#388659,#388660,#388661,#388662,
#388663,#388664,#388665),.UNSPECIFIED.,.F.,.F.,(4,3,4),(0.,4.41069704323471E-5,
0.000113970027818833),.UNSPECIFIED.);
#25234=B_SPLINE_CURVE_WITH_KNOTS('',3,(#388671,#388672,#388673,#388674),
 .UNSPECIFIED.,.F.,.F.,(4,4),(4.47028007668187E-19,9.54361881492177E-5),
 .UNSPECIFIED.);
#25235=B_SPLINE_CURVE_WITH_KNOTS('',3,(#388678,#388679,#388680,#388681,
#388682,#388683,#388684),.UNSPECIFIED.,.F.,.F.,(4,3,4),(0.,6.98630244191491E-5,
0.000113969974038089),.UNSPECIFIED.);
#25236=B_SPLINE_CURVE_WITH_KNOTS('',3,(#388687,#388688,#388689,#388690,
#388691,#388692,#388693,#388694,#388695,#388696,#388697,#388698,#388699,
#388700,#388701,#388702,#388703,#388704,#388705,#388706,#388707,#388708,
#388709,#388710,#388711,#388712,#388713,#388714,#388715,#388716,#388717,
#388718,#388719,#388720,#388721,#388722,#388723,#388724,#388725,#388726,
#388727,#388728,#388729,#388730,#388731,#388732,#388733,#388734,#388735),
 .UNSPECIFIED.,.F.,.F.,(4,3,3,3,3,3,3,3,3,3,3,3,3,3,3,3,4),(0.,1.53100299373411E-6,
4.52554775679518E-6,7.01151246291603E-6,9.26752933800355E-6,1.03084066197173E-5,
1.17138990826863E-5,1.22284894984076E-5,1.30315035324818E-5,1.38363728497813E-5,
1.40464197777496E-5,1.5459774956464E-5,1.62073588704068E-5,1.92092968713069E-5,
1.95234416882556E-5,2.37637844577537E-5,2.61487188977261E-5),
 .UNSPECIFIED.);
#25237=B_SPLINE_CURVE_WITH_KNOTS('',3,(#388750,#388751,#388752,#388753,
#388754,#388755,#388756,#388757,#388758,#388759,#388760,#388761,#388762,
#388763,#388764,#388765,#388766,#388767,#388768,#388769,#388770,#388771,
#388772,#388773,#388774,#388775,#388776,#388777,#388778,#388779,#388780),
 .UNSPECIFIED.,.F.,.F.,(4,3,3,3,3,3,3,3,3,3,4),(0.,3.95507910397527E-6,
7.53768426604199E-6,1.19904533335351E-5,1.40475043392585E-5,1.51452104275965E-5,
1.67866272814181E-5,1.69621513005357E-5,1.81338315460712E-5,1.98906334656553E-5,
2.06132424588244E-5),.UNSPECIFIED.);
#25238=B_SPLINE_CURVE_WITH_KNOTS('',3,(#388783,#388784,#388785,#388786),
 .UNSPECIFIED.,.F.,.F.,(4,4),(4.47028007668187E-19,0.00010938435327491),
 .UNSPECIFIED.);
#25239=B_SPLINE_CURVE_WITH_KNOTS('',3,(#388813,#388814,#388815,#388816,
#388817,#388818,#388819,#388820,#388821,#388822,#388823,#388824,#388825,
#388826,#388827,#388828,#388829,#388830,#388831,#388832,#388833,#388834,
#388835,#388836,#388837,#388838,#388839,#388840,#388841,#388842,#388843,
#388844,#388845,#388846),.UNSPECIFIED.,.F.,.F.,(4,3,3,3,3,3,3,3,3,3,3,4),
(1.0842021724855E-19,2.09623992729436E-6,3.17176647120224E-6,4.82636181944045E-6,
5.01000917339964E-6,6.13126454147505E-6,8.60486650288846E-6,9.21144281170488E-6,
1.24722301135973E-5,1.42666454787855E-5,2.04670653756798E-5,2.080264381768E-5),
 .UNSPECIFIED.);
#25240=B_SPLINE_CURVE_WITH_KNOTS('',3,(#388847,#388848,#388849,#388850),
 .UNSPECIFIED.,.F.,.F.,(4,4),(0.,0.000109384345496909),.UNSPECIFIED.);
#25241=B_SPLINE_CURVE_WITH_KNOTS('',3,(#388955,#388956,#388957,#388958),
 .UNSPECIFIED.,.F.,.F.,(4,4),(0.,9.54361881492175E-5),.UNSPECIFIED.);
#25242=B_SPLINE_CURVE_WITH_KNOTS('',3,(#388963,#388964,#388965,#388966,
#388967,#388968,#388969),.UNSPECIFIED.,.F.,.F.,(4,3,4),(0.,4.4106970432347E-5,
0.000113970027818833),.UNSPECIFIED.);
#25243=B_SPLINE_CURVE_WITH_KNOTS('',3,(#388975,#388976,#388977,#388978),
 .UNSPECIFIED.,.F.,.F.,(4,4),(4.33680868994202E-19,9.54361881492178E-5),
 .UNSPECIFIED.);
#25244=B_SPLINE_CURVE_WITH_KNOTS('',3,(#388982,#388983,#388984,#388985,
#388986,#388987,#388988),.UNSPECIFIED.,.F.,.F.,(4,3,4),(0.,6.98630244191489E-5,
0.000113969974038089),.UNSPECIFIED.);
#25245=B_SPLINE_CURVE_WITH_KNOTS('',3,(#388991,#388992,#388993,#388994,
#388995,#388996,#388997,#388998,#388999,#389000,#389001,#389002,#389003,
#389004,#389005,#389006,#389007,#389008,#389009,#389010,#389011,#389012,
#389013,#389014,#389015,#389016,#389017,#389018,#389019,#389020,#389021,
#389022,#389023,#389024,#389025,#389026,#389027,#389028,#389029,#389030,
#389031,#389032,#389033,#389034,#389035,#389036,#389037,#389038,#389039),
 .UNSPECIFIED.,.F.,.F.,(4,3,3,3,3,3,3,3,3,3,3,3,3,3,3,3,4),(0.,1.53100299373412E-6,
4.52554775679643E-6,7.01151246291612E-6,9.26752933801457E-6,1.03084066197173E-5,
1.17138990826862E-5,1.22284894984073E-5,1.30315035324817E-5,1.38363728497812E-5,
1.40464197777494E-5,1.54597749564638E-5,1.62073588704067E-5,1.92092968713275E-5,
1.95234416882553E-5,2.3763784457758E-5,2.61487188977258E-5),
 .UNSPECIFIED.);
#25246=B_SPLINE_CURVE_WITH_KNOTS('',3,(#389054,#389055,#389056,#389057,
#389058,#389059,#389060,#389061,#389062,#389063,#389064,#389065,#389066,
#389067,#389068,#389069,#389070,#389071,#389072,#389073,#389074,#389075,
#389076,#389077,#389078,#389079,#389080,#389081,#389082,#389083,#389084),
 .UNSPECIFIED.,.F.,.F.,(4,3,3,3,3,3,3,3,3,3,4),(0.,3.95507910397651E-6,
7.53768426604199E-6,1.1990453333535E-5,1.40475043392585E-5,1.51452104275963E-5,
1.67866272814247E-5,1.69621513005357E-5,1.81338315460712E-5,1.98906334656539E-5,
2.06132424588243E-5),.UNSPECIFIED.);
#25247=B_SPLINE_CURVE_WITH_KNOTS('',3,(#389087,#389088,#389089,#389090),
 .UNSPECIFIED.,.F.,.F.,(4,4),(4.47028007668187E-19,0.00010938435327491),
 .UNSPECIFIED.);
#25248=B_SPLINE_CURVE_WITH_KNOTS('',3,(#389117,#389118,#389119,#389120,
#389121,#389122,#389123,#389124,#389125,#389126,#389127,#389128,#389129,
#389130,#389131,#389132,#389133,#389134,#389135,#389136,#389137,#389138,
#389139,#389140,#389141,#389142,#389143,#389144,#389145,#389146,#389147,
#389148,#389149,#389150),.UNSPECIFIED.,.F.,.F.,(4,3,3,3,3,3,3,3,3,3,3,4),
(2.16840434497101E-19,2.09623992729447E-6,3.17176647120222E-6,4.82636181945244E-6,
5.01000917339954E-6,6.13126454147495E-6,8.60486650288834E-6,9.21144281170472E-6,
1.24722301135988E-5,1.42666454787852E-5,2.0467065375677E-5,2.08026438176796E-5),
 .UNSPECIFIED.);
#25249=B_SPLINE_CURVE_WITH_KNOTS('',3,(#389151,#389152,#389153,#389154),
 .UNSPECIFIED.,.F.,.F.,(4,4),(0.,0.000109384345496908),.UNSPECIFIED.);
#25250=B_SPLINE_CURVE_WITH_KNOTS('',3,(#389259,#389260,#389261,#389262),
 .UNSPECIFIED.,.F.,.F.,(4,4),(0.,9.54361881492176E-5),.UNSPECIFIED.);
#25251=B_SPLINE_CURVE_WITH_KNOTS('',3,(#389267,#389268,#389269,#389270,
#389271,#389272,#389273),.UNSPECIFIED.,.F.,.F.,(4,3,4),(0.,4.41069704323467E-5,
0.000113970027818833),.UNSPECIFIED.);
#25252=B_SPLINE_CURVE_WITH_KNOTS('',3,(#389279,#389280,#389281,#389282),
 .UNSPECIFIED.,.F.,.F.,(4,4),(0.,9.54361881492178E-5),.UNSPECIFIED.);
#25253=B_SPLINE_CURVE_WITH_KNOTS('',3,(#389286,#389287,#389288,#389289,
#389290,#389291,#389292),.UNSPECIFIED.,.F.,.F.,(4,3,4),(0.,6.98630244191494E-5,
0.000113969974038089),.UNSPECIFIED.);
#25254=B_SPLINE_CURVE_WITH_KNOTS('',3,(#389295,#389296,#389297,#389298,
#389299,#389300,#389301,#389302,#389303,#389304,#389305,#389306,#389307,
#389308,#389309,#389310,#389311,#389312,#389313,#389314,#389315,#389316,
#389317,#389318,#389319,#389320,#389321,#389322,#389323,#389324,#389325,
#389326,#389327,#389328,#389329,#389330,#389331,#389332,#389333,#389334,
#389335,#389336,#389337,#389338,#389339,#389340,#389341,#389342,#389343),
 .UNSPECIFIED.,.F.,.F.,(4,3,3,3,3,3,3,3,3,3,3,3,3,3,3,3,4),(0.,1.5310029937341E-6,
4.5255477567998E-6,7.01151246291602E-6,9.26752933800744E-6,1.03084066197172E-5,
1.17138990826861E-5,1.22284894984072E-5,1.30315035324817E-5,1.38363728497813E-5,
1.40464197777494E-5,1.5459774956464E-5,1.6207358870407E-5,1.92092968712811E-5,
1.95234416882557E-5,2.37637844577566E-5,2.61487188977266E-5),
 .UNSPECIFIED.);
#25255=B_SPLINE_CURVE_WITH_KNOTS('',3,(#389358,#389359,#389360,#389361,
#389362,#389363,#389364,#389365,#389366,#389367,#389368,#389369,#389370,
#389371,#389372,#389373,#389374,#389375,#389376,#389377,#389378,#389379,
#389380,#389381,#389382,#389383,#389384,#389385,#389386,#389387,#389388),
 .UNSPECIFIED.,.F.,.F.,(4,3,3,3,3,3,3,3,3,3,4),(0.,3.95507910397734E-6,
7.537684266042E-6,1.1990453333535E-5,1.40475043392585E-5,1.51452104275964E-5,
1.67866272814187E-5,1.69621513005358E-5,1.8133831546071E-5,1.98906334656531E-5,
2.06132424588243E-5),.UNSPECIFIED.);
#25256=B_SPLINE_CURVE_WITH_KNOTS('',3,(#389391,#389392,#389393,#389394),
 .UNSPECIFIED.,.F.,.F.,(4,4),(4.47028007668187E-19,0.00010938435327491),
 .UNSPECIFIED.);
#25257=B_SPLINE_CURVE_WITH_KNOTS('',3,(#389421,#389422,#389423,#389424,
#389425,#389426,#389427,#389428,#389429,#389430,#389431,#389432,#389433,
#389434,#389435,#389436,#389437,#389438,#389439,#389440,#389441,#389442,
#389443,#389444,#389445,#389446,#389447,#389448,#389449,#389450,#389451,
#389452,#389453,#389454),.UNSPECIFIED.,.F.,.F.,(4,3,3,3,3,3,3,3,3,3,3,4),
(2.16840434497101E-19,2.09623992729446E-6,3.17176647120221E-6,4.82636181944466E-6,
5.01000917339944E-6,6.13126454147503E-6,8.60486650288845E-6,9.21144281170482E-6,
1.24722301135897E-5,1.42666454787855E-5,2.04670653756925E-5,2.08026438176801E-5),
 .UNSPECIFIED.);
#25258=B_SPLINE_CURVE_WITH_KNOTS('',3,(#389455,#389456,#389457,#389458),
 .UNSPECIFIED.,.F.,.F.,(4,4),(0.,0.000109384345496908),.UNSPECIFIED.);
#25259=B_SPLINE_CURVE_WITH_KNOTS('',3,(#389563,#389564,#389565,#389566),
 .UNSPECIFIED.,.F.,.F.,(4,4),(0.,9.54361881492174E-5),.UNSPECIFIED.);
#25260=B_SPLINE_CURVE_WITH_KNOTS('',3,(#389571,#389572,#389573,#389574,
#389575,#389576,#389577),.UNSPECIFIED.,.F.,.F.,(4,3,4),(0.,4.41069704323472E-5,
0.000113970027818833),.UNSPECIFIED.);
#25261=B_SPLINE_CURVE_WITH_KNOTS('',3,(#389583,#389584,#389585,#389586),
 .UNSPECIFIED.,.F.,.F.,(4,4),(4.33680868994202E-19,9.54361881492176E-5),
 .UNSPECIFIED.);
#25262=B_SPLINE_CURVE_WITH_KNOTS('',3,(#389590,#389591,#389592,#389593,
#389594,#389595,#389596),.UNSPECIFIED.,.F.,.F.,(4,3,4),(0.,6.9863024419149E-5,
0.000113969974038089),.UNSPECIFIED.);
#25263=B_SPLINE_CURVE_WITH_KNOTS('',3,(#389599,#389600,#389601,#389602,
#389603,#389604,#389605,#389606,#389607,#389608,#389609,#389610,#389611,
#389612,#389613,#389614,#389615,#389616,#389617,#389618,#389619,#389620,
#389621,#389622,#389623,#389624,#389625,#389626,#389627,#389628,#389629,
#389630,#389631,#389632,#389633,#389634,#389635,#389636,#389637,#389638,
#389639,#389640,#389641,#389642,#389643,#389644,#389645,#389646,#389647),
 .UNSPECIFIED.,.F.,.F.,(4,3,3,3,3,3,3,3,3,3,3,3,3,3,3,3,4),(0.,1.53100299373409E-6,
4.52554775678909E-6,7.01151246291593E-6,9.26752933800868E-6,1.03084066197173E-5,
1.17138990826865E-5,1.22284894984075E-5,1.30315035324817E-5,1.38363728497814E-5,
1.40464197777496E-5,1.54597749564642E-5,1.62073588704071E-5,1.92092968712948E-5,
1.95234416882557E-5,2.37637844577641E-5,2.61487188977263E-5),
 .UNSPECIFIED.);
#25264=B_SPLINE_CURVE_WITH_KNOTS('',3,(#389662,#389663,#389664,#389665,
#389666,#389667,#389668,#389669,#389670,#389671,#389672,#389673,#389674,
#389675,#389676,#389677,#389678,#389679,#389680,#389681,#389682,#389683,
#389684,#389685,#389686,#389687,#389688,#389689,#389690,#389691,#389692),
 .UNSPECIFIED.,.F.,.F.,(4,3,3,3,3,3,3,3,3,3,4),(0.,3.95507910398428E-6,
7.53768426604197E-6,1.1990453333535E-5,1.40475043392584E-5,1.51452104275963E-5,
1.67866272814145E-5,1.6962151300536E-5,1.81338315460713E-5,1.9890633465654E-5,
2.06132424588247E-5),.UNSPECIFIED.);
#25265=B_SPLINE_CURVE_WITH_KNOTS('',3,(#389695,#389696,#389697,#389698),
 .UNSPECIFIED.,.F.,.F.,(4,4),(4.33680868994202E-19,0.00010938435327491),
 .UNSPECIFIED.);
#25266=B_SPLINE_CURVE_WITH_KNOTS('',3,(#389725,#389726,#389727,#389728,
#389729,#389730,#389731,#389732,#389733,#389734,#389735,#389736,#389737,
#389738,#389739,#389740,#389741,#389742,#389743,#389744,#389745,#389746,
#389747,#389748,#389749,#389750,#389751,#389752,#389753,#389754,#389755,
#389756,#389757,#389758),.UNSPECIFIED.,.F.,.F.,(4,3,3,3,3,3,3,3,3,3,3,4),
(0.,2.09623992729446E-6,3.1717664712022E-6,4.826361819433E-6,5.01000917339962E-6,
6.13126454147486E-6,8.60486650288814E-6,9.21144281170439E-6,1.24722301135902E-5,
1.42666454787843E-5,2.0467065375698E-5,2.08026438176779E-5),
 .UNSPECIFIED.);
#25267=B_SPLINE_CURVE_WITH_KNOTS('',3,(#389759,#389760,#389761,#389762),
 .UNSPECIFIED.,.F.,.F.,(4,4),(0.,0.000109384345496908),.UNSPECIFIED.);
#25268=B_SPLINE_CURVE_WITH_KNOTS('',3,(#389867,#389868,#389869,#389870),
 .UNSPECIFIED.,.F.,.F.,(4,4),(0.,9.54361881492177E-5),.UNSPECIFIED.);
#25269=B_SPLINE_CURVE_WITH_KNOTS('',3,(#389875,#389876,#389877,#389878,
#389879,#389880,#389881),.UNSPECIFIED.,.F.,.F.,(4,3,4),(0.,4.41069704323467E-5,
0.000113970027818833),.UNSPECIFIED.);
#25270=B_SPLINE_CURVE_WITH_KNOTS('',3,(#389887,#389888,#389889,#389890),
 .UNSPECIFIED.,.F.,.F.,(4,4),(4.33680868994202E-19,9.54361881492182E-5),
 .UNSPECIFIED.);
#25271=B_SPLINE_CURVE_WITH_KNOTS('',3,(#389894,#389895,#389896,#389897,
#389898,#389899,#389900),.UNSPECIFIED.,.F.,.F.,(4,3,4),(0.,6.9863024419149E-5,
0.000113969974038089),.UNSPECIFIED.);
#25272=B_SPLINE_CURVE_WITH_KNOTS('',3,(#389903,#389904,#389905,#389906,
#389907,#389908,#389909,#389910,#389911,#389912,#389913,#389914,#389915,
#389916,#389917,#389918,#389919,#389920,#389921,#389922,#389923,#389924,
#389925,#389926,#389927,#389928,#389929,#389930,#389931,#389932,#389933,
#389934,#389935,#389936,#389937,#389938,#389939,#389940,#389941,#389942,
#389943,#389944,#389945,#389946,#389947,#389948,#389949,#389950,#389951),
 .UNSPECIFIED.,.F.,.F.,(4,3,3,3,3,3,3,3,3,3,3,3,3,3,3,3,4),(0.,1.53100299373416E-6,
4.52554775679403E-6,7.01151246291602E-6,9.26752933799172E-6,1.03084066197174E-5,
1.17138990826862E-5,1.22284894984074E-5,1.30315035324817E-5,1.38363728497811E-5,
1.40464197777497E-5,1.54597749564639E-5,1.62073588704069E-5,1.92092968712594E-5,
1.95234416882556E-5,2.37637844577584E-5,2.61487188977261E-5),
 .UNSPECIFIED.);
#25273=B_SPLINE_CURVE_WITH_KNOTS('',3,(#389966,#389967,#389968,#389969,
#389970,#389971,#389972,#389973,#389974,#389975,#389976,#389977,#389978,
#389979,#389980,#389981,#389982,#389983,#389984,#389985,#389986,#389987,
#389988,#389989,#389990,#389991,#389992,#389993,#389994,#389995,#389996),
 .UNSPECIFIED.,.F.,.F.,(4,3,3,3,3,3,3,3,3,3,4),(0.,3.95507910398383E-6,
7.53768426604193E-6,1.1990453333535E-5,1.40475043392586E-5,1.51452104275962E-5,
1.67866272814302E-5,1.69621513005357E-5,1.81338315460711E-5,1.9890633465653E-5,
2.06132424588243E-5),.UNSPECIFIED.);
#25274=B_SPLINE_CURVE_WITH_KNOTS('',3,(#389999,#390000,#390001,#390002),
 .UNSPECIFIED.,.F.,.F.,(4,4),(4.33680868994202E-19,0.00010938435327491),
 .UNSPECIFIED.);
#25275=B_SPLINE_CURVE_WITH_KNOTS('',3,(#390029,#390030,#390031,#390032,
#390033,#390034,#390035,#390036,#390037,#390038,#390039,#390040,#390041,
#390042,#390043,#390044,#390045,#390046,#390047,#390048,#390049,#390050,
#390051,#390052,#390053,#390054,#390055,#390056,#390057,#390058,#390059,
#390060,#390061,#390062),.UNSPECIFIED.,.F.,.F.,(4,3,3,3,3,3,3,3,3,3,3,4),
(2.16840434497101E-19,2.09623992729435E-6,3.17176647120219E-6,4.82636181943341E-6,
5.01000917339972E-6,6.13126454147492E-6,8.60486650288852E-6,9.21144281170482E-6,
1.24722301135993E-5,1.42666454787856E-5,2.04670653756756E-5,2.08026438176803E-5),
 .UNSPECIFIED.);
#25276=B_SPLINE_CURVE_WITH_KNOTS('',3,(#390063,#390064,#390065,#390066),
 .UNSPECIFIED.,.F.,.F.,(4,4),(0.,0.000109384345496908),.UNSPECIFIED.);
#25277=B_SPLINE_CURVE_WITH_KNOTS('',3,(#390171,#390172,#390173,#390174),
 .UNSPECIFIED.,.F.,.F.,(4,4),(0.,9.54361881492174E-5),.UNSPECIFIED.);
#25278=B_SPLINE_CURVE_WITH_KNOTS('',3,(#390179,#390180,#390181,#390182,
#390183,#390184,#390185),.UNSPECIFIED.,.F.,.F.,(4,3,4),(0.,4.41069704323469E-5,
0.000113970027818833),.UNSPECIFIED.);
#25279=B_SPLINE_CURVE_WITH_KNOTS('',3,(#390191,#390192,#390193,#390194),
 .UNSPECIFIED.,.F.,.F.,(4,4),(4.63171371119878E-19,9.54361881492179E-5),
 .UNSPECIFIED.);
#25280=B_SPLINE_CURVE_WITH_KNOTS('',3,(#390198,#390199,#390200,#390201,
#390202,#390203,#390204),.UNSPECIFIED.,.F.,.F.,(4,3,4),(0.,6.98630244191489E-5,
0.000113969974038089),.UNSPECIFIED.);
#25281=B_SPLINE_CURVE_WITH_KNOTS('',3,(#390207,#390208,#390209,#390210,
#390211,#390212,#390213,#390214,#390215,#390216,#390217,#390218,#390219,
#390220,#390221,#390222,#390223,#390224,#390225,#390226,#390227,#390228,
#390229,#390230,#390231,#390232,#390233,#390234,#390235,#390236,#390237,
#390238,#390239,#390240,#390241,#390242,#390243,#390244,#390245,#390246,
#390247,#390248,#390249,#390250,#390251,#390252,#390253,#390254,#390255),
 .UNSPECIFIED.,.F.,.F.,(4,3,3,3,3,3,3,3,3,3,3,3,3,3,3,3,4),(0.,1.53100299373408E-6,
4.52554775679199E-6,7.01151246291604E-6,9.26752933800014E-6,1.03084066197173E-5,
1.17138990826862E-5,1.22284894984075E-5,1.30315035324817E-5,1.38363728497813E-5,
1.40464197777494E-5,1.5459774956464E-5,1.62073588704068E-5,1.92092968712309E-5,
1.95234416882555E-5,2.37637844577565E-5,2.61487188977261E-5),
 .UNSPECIFIED.);
#25282=B_SPLINE_CURVE_WITH_KNOTS('',3,(#390270,#390271,#390272,#390273,
#390274,#390275,#390276,#390277,#390278,#390279,#390280,#390281,#390282,
#390283,#390284,#390285,#390286,#390287,#390288,#390289,#390290,#390291,
#390292,#390293,#390294,#390295,#390296,#390297,#390298,#390299,#390300),
 .UNSPECIFIED.,.F.,.F.,(4,3,3,3,3,3,3,3,3,3,4),(0.,3.95507910399088E-6,
7.53768426604193E-6,1.19904533335349E-5,1.40475043392585E-5,1.51452104275963E-5,
1.67866272814177E-5,1.69621513005356E-5,1.8133831546071E-5,1.98906334656504E-5,
2.06132424588242E-5),.UNSPECIFIED.);
#25283=B_SPLINE_CURVE_WITH_KNOTS('',3,(#390303,#390304,#390305,#390306),
 .UNSPECIFIED.,.F.,.F.,(4,4),(5.11417141928151E-19,0.00010938435327491),
 .UNSPECIFIED.);
#25284=B_SPLINE_CURVE_WITH_KNOTS('',3,(#390333,#390334,#390335,#390336,
#390337,#390338,#390339,#390340,#390341,#390342,#390343,#390344,#390345,
#390346,#390347,#390348,#390349,#390350,#390351,#390352,#390353,#390354,
#390355,#390356,#390357,#390358,#390359,#390360,#390361,#390362,#390363,
#390364,#390365,#390366),.UNSPECIFIED.,.F.,.F.,(4,3,3,3,3,3,3,3,3,3,3,4),
(1.0842021724855E-19,2.09623992729441E-6,3.17176647120218E-6,4.82636181942557E-6,
5.01000917339962E-6,6.13126454147496E-6,8.60486650288856E-6,9.21144281170495E-6,
1.24722301135921E-5,1.42666454787855E-5,2.04670653756969E-5,2.08026438176802E-5),
 .UNSPECIFIED.);
#25285=B_SPLINE_CURVE_WITH_KNOTS('',3,(#390367,#390368,#390369,#390370),
 .UNSPECIFIED.,.F.,.F.,(4,4),(0.,0.000109384345496908),.UNSPECIFIED.);
#25286=B_SPLINE_CURVE_WITH_KNOTS('',3,(#390475,#390476,#390477,#390478),
 .UNSPECIFIED.,.F.,.F.,(4,4),(0.,9.54361881492174E-5),.UNSPECIFIED.);
#25287=B_SPLINE_CURVE_WITH_KNOTS('',3,(#390483,#390484,#390485,#390486,
#390487,#390488,#390489),.UNSPECIFIED.,.F.,.F.,(4,3,4),(0.,4.41069704323469E-5,
0.000113970027818833),.UNSPECIFIED.);
#25288=B_SPLINE_CURVE_WITH_KNOTS('',3,(#390495,#390496,#390497,#390498),
 .UNSPECIFIED.,.F.,.F.,(4,4),(2.16840434497101E-19,9.5436188149218E-5),
 .UNSPECIFIED.);
#25289=B_SPLINE_CURVE_WITH_KNOTS('',3,(#390502,#390503,#390504,#390505,
#390506,#390507,#390508),.UNSPECIFIED.,.F.,.F.,(4,3,4),(0.,6.98630244191491E-5,
0.000113969974038089),.UNSPECIFIED.);
#25290=B_SPLINE_CURVE_WITH_KNOTS('',3,(#390511,#390512,#390513,#390514,
#390515,#390516,#390517,#390518,#390519,#390520,#390521,#390522,#390523,
#390524,#390525,#390526,#390527,#390528,#390529,#390530,#390531,#390532,
#390533,#390534,#390535,#390536,#390537,#390538,#390539,#390540,#390541,
#390542,#390543,#390544,#390545,#390546,#390547,#390548,#390549,#390550,
#390551,#390552,#390553,#390554,#390555,#390556,#390557,#390558,#390559),
 .UNSPECIFIED.,.F.,.F.,(4,3,3,3,3,3,3,3,3,3,3,3,3,3,3,3,4),(0.,1.53100299373404E-6,
4.52554775679301E-6,7.01151246291608E-6,9.26752933800197E-6,1.03084066197173E-5,
1.17138990826862E-5,1.22284894984074E-5,1.30315035324818E-5,1.38363728497813E-5,
1.40464197777495E-5,1.54597749564641E-5,1.62073588704069E-5,1.92092968712377E-5,
1.95234416882556E-5,2.37637844577636E-5,2.61487188977264E-5),
 .UNSPECIFIED.);
#25291=B_SPLINE_CURVE_WITH_KNOTS('',3,(#390574,#390575,#390576,#390577,
#390578,#390579,#390580,#390581,#390582,#390583,#390584,#390585,#390586,
#390587,#390588,#390589,#390590,#390591,#390592,#390593,#390594,#390595,
#390596,#390597,#390598,#390599,#390600,#390601,#390602,#390603,#390604),
 .UNSPECIFIED.,.F.,.F.,(4,3,3,3,3,3,3,3,3,3,4),(0.,3.95507910397597E-6,
7.53768426604195E-6,1.19904533335351E-5,1.40475043392585E-5,1.51452104275964E-5,
1.67866272814042E-5,1.69621513005359E-5,1.81338315460713E-5,1.98906334656556E-5,
2.06132424588248E-5),.UNSPECIFIED.);
#25292=B_SPLINE_CURVE_WITH_KNOTS('',3,(#390607,#390608,#390609,#390610),
 .UNSPECIFIED.,.F.,.F.,(4,4),(4.84869951806108E-19,0.00010938435327491),
 .UNSPECIFIED.);
#25293=B_SPLINE_CURVE_WITH_KNOTS('',3,(#390637,#390638,#390639,#390640,
#390641,#390642,#390643,#390644,#390645,#390646,#390647,#390648,#390649,
#390650,#390651,#390652,#390653,#390654,#390655,#390656,#390657,#390658,
#390659,#390660,#390661,#390662,#390663,#390664,#390665,#390666,#390667,
#390668,#390669,#390670),.UNSPECIFIED.,.F.,.F.,(4,3,3,3,3,3,3,3,3,3,3,4),
(1.62630325872826E-19,2.09623992729434E-6,3.17176647120212E-6,4.82636181944639E-6,
5.01000917339947E-6,6.13126454147481E-6,8.60486650288819E-6,9.2114428117045E-6,
1.24722301136184E-5,1.42666454787845E-5,2.04670653756707E-5,2.08026438176783E-5),
 .UNSPECIFIED.);
#25294=B_SPLINE_CURVE_WITH_KNOTS('',3,(#390671,#390672,#390673,#390674),
 .UNSPECIFIED.,.F.,.F.,(4,4),(0.,0.000109384345496908),.UNSPECIFIED.);
#25295=B_SPLINE_CURVE_WITH_KNOTS('',3,(#390779,#390780,#390781,#390782),
 .UNSPECIFIED.,.F.,.F.,(4,4),(0.,9.54361881492171E-5),.UNSPECIFIED.);
#25296=B_SPLINE_CURVE_WITH_KNOTS('',3,(#390787,#390788,#390789,#390790,
#390791,#390792,#390793),.UNSPECIFIED.,.F.,.F.,(4,3,4),(0.,4.41069704323471E-5,
0.000113970027818833),.UNSPECIFIED.);
#25297=B_SPLINE_CURVE_WITH_KNOTS('',3,(#390799,#390800,#390801,#390802),
 .UNSPECIFIED.,.F.,.F.,(4,4),(4.84869951806108E-19,9.54361881492178E-5),
 .UNSPECIFIED.);
#25298=B_SPLINE_CURVE_WITH_KNOTS('',3,(#390806,#390807,#390808,#390809,
#390810,#390811,#390812),.UNSPECIFIED.,.F.,.F.,(4,3,4),(0.,6.98630244191492E-5,
0.000113969974038089),.UNSPECIFIED.);
#25299=B_SPLINE_CURVE_WITH_KNOTS('',3,(#390815,#390816,#390817,#390818,
#390819,#390820,#390821,#390822,#390823,#390824,#390825,#390826,#390827,
#390828,#390829,#390830,#390831,#390832,#390833,#390834,#390835,#390836,
#390837,#390838,#390839,#390840,#390841,#390842,#390843,#390844,#390845,
#390846,#390847,#390848,#390849,#390850,#390851,#390852,#390853,#390854,
#390855,#390856,#390857,#390858,#390859,#390860,#390861,#390862,#390863),
 .UNSPECIFIED.,.F.,.F.,(4,3,3,3,3,3,3,3,3,3,3,3,3,3,3,3,4),(0.,1.53100299373407E-6,
4.52554775679799E-6,7.01151246291605E-6,9.2675293380014E-6,1.03084066197173E-5,
1.17138990826862E-5,1.22284894984074E-5,1.30315035324817E-5,1.38363728497813E-5,
1.40464197777495E-5,1.54597749564641E-5,1.62073588704071E-5,1.92092968712794E-5,
1.95234416882559E-5,2.37637844577629E-5,2.61487188977271E-5),
 .UNSPECIFIED.);
#25300=B_SPLINE_CURVE_WITH_KNOTS('',3,(#390878,#390879,#390880,#390881,
#390882,#390883,#390884,#390885,#390886,#390887,#390888,#390889,#390890,
#390891,#390892,#390893,#390894,#390895,#390896,#390897,#390898,#390899,
#390900,#390901,#390902,#390903,#390904,#390905,#390906,#390907,#390908),
 .UNSPECIFIED.,.F.,.F.,(4,3,3,3,3,3,3,3,3,3,4),(0.,3.95507910396868E-6,
7.53768426604184E-6,1.19904533335349E-5,1.40475043392585E-5,1.51452104275964E-5,
1.67866272814194E-5,1.69621513005358E-5,1.8133831546071E-5,1.98906334656556E-5,
2.06132424588244E-5),.UNSPECIFIED.);
#25301=B_SPLINE_CURVE_WITH_KNOTS('',3,(#390911,#390912,#390913,#390914),
 .UNSPECIFIED.,.F.,.F.,(4,4),(5.42101086242752E-19,0.00010938435327491),
 .UNSPECIFIED.);
#25302=B_SPLINE_CURVE_WITH_KNOTS('',3,(#390941,#390942,#390943,#390944,
#390945,#390946,#390947,#390948,#390949,#390950,#390951,#390952,#390953,
#390954,#390955,#390956,#390957,#390958,#390959,#390960,#390961,#390962,
#390963,#390964,#390965,#390966,#390967,#390968,#390969,#390970,#390971,
#390972,#390973,#390974),.UNSPECIFIED.,.F.,.F.,(4,3,3,3,3,3,3,3,3,3,3,4),
(1.0842021724855E-19,2.09623992729447E-6,3.17176647120237E-6,4.82636181943974E-6,
5.01000917339962E-6,6.13126454147495E-6,8.60486650288846E-6,9.2114428117048E-6,
1.24722301136019E-5,1.4266645478785E-5,2.04670653756862E-5,2.08026438176791E-5),
 .UNSPECIFIED.);
#25303=B_SPLINE_CURVE_WITH_KNOTS('',3,(#390975,#390976,#390977,#390978),
 .UNSPECIFIED.,.F.,.F.,(4,4),(0.,0.000109384345496908),.UNSPECIFIED.);
#25304=B_SPLINE_CURVE_WITH_KNOTS('',3,(#391083,#391084,#391085,#391086),
 .UNSPECIFIED.,.F.,.F.,(4,4),(0.,9.54361881492177E-5),.UNSPECIFIED.);
#25305=B_SPLINE_CURVE_WITH_KNOTS('',3,(#391091,#391092,#391093,#391094,
#391095,#391096,#391097),.UNSPECIFIED.,.F.,.F.,(4,3,4),(0.,4.41069704323471E-5,
0.000113970027818833),.UNSPECIFIED.);
#25306=B_SPLINE_CURVE_WITH_KNOTS('',3,(#391103,#391104,#391105,#391106),
 .UNSPECIFIED.,.F.,.F.,(4,4),(1.0842021724855E-19,9.54361881492175E-5),
 .UNSPECIFIED.);
#25307=B_SPLINE_CURVE_WITH_KNOTS('',3,(#391110,#391111,#391112,#391113,
#391114,#391115,#391116),.UNSPECIFIED.,.F.,.F.,(4,3,4),(0.,6.98630244191488E-5,
0.000113969974038089),.UNSPECIFIED.);
#25308=B_SPLINE_CURVE_WITH_KNOTS('',3,(#391119,#391120,#391121,#391122,
#391123,#391124,#391125,#391126,#391127,#391128,#391129,#391130,#391131,
#391132,#391133,#391134,#391135,#391136,#391137,#391138,#391139,#391140,
#391141,#391142,#391143,#391144,#391145,#391146,#391147,#391148,#391149,
#391150,#391151,#391152,#391153,#391154,#391155,#391156,#391157,#391158,
#391159,#391160,#391161,#391162,#391163,#391164,#391165,#391166,#391167),
 .UNSPECIFIED.,.F.,.F.,(4,3,3,3,3,3,3,3,3,3,3,3,3,3,3,3,4),(0.,1.53100299373429E-6,
4.52554775679722E-6,7.01151246291618E-6,9.26752933798786E-6,1.03084066197175E-5,
1.17138990826863E-5,1.22284894984076E-5,1.3031503532482E-5,1.38363728497814E-5,
1.40464197777495E-5,1.54597749564641E-5,1.62073588704071E-5,1.92092968713176E-5,
1.95234416882558E-5,2.37637844577596E-5,2.61487188977265E-5),
 .UNSPECIFIED.);
#25309=B_SPLINE_CURVE_WITH_KNOTS('',3,(#391182,#391183,#391184,#391185,
#391186,#391187,#391188,#391189,#391190,#391191,#391192,#391193,#391194,
#391195,#391196,#391197,#391198,#391199,#391200,#391201,#391202,#391203,
#391204,#391205,#391206,#391207,#391208,#391209,#391210,#391211,#391212),
 .UNSPECIFIED.,.F.,.F.,(4,3,3,3,3,3,3,3,3,3,4),(0.,3.95507910397509E-6,
7.53768426604205E-6,1.19904533335352E-5,1.40475043392586E-5,1.51452104275965E-5,
1.67866272814222E-5,1.69621513005358E-5,1.81338315460713E-5,1.98906334656548E-5,
2.06132424588244E-5),.UNSPECIFIED.);
#25310=B_SPLINE_CURVE_WITH_KNOTS('',3,(#391215,#391216,#391217,#391218),
 .UNSPECIFIED.,.F.,.F.,(4,4),(2.16840434497101E-19,0.00010938435327491),
 .UNSPECIFIED.);
#25311=B_SPLINE_CURVE_WITH_KNOTS('',3,(#391245,#391246,#391247,#391248,
#391249,#391250,#391251,#391252,#391253,#391254,#391255,#391256,#391257,
#391258,#391259,#391260,#391261,#391262,#391263,#391264,#391265,#391266,
#391267,#391268,#391269,#391270,#391271,#391272,#391273,#391274,#391275,
#391276,#391277,#391278),.UNSPECIFIED.,.F.,.F.,(4,3,3,3,3,3,3,3,3,3,3,4),
(1.0842021724855E-19,2.0962399272944E-6,3.17176647120216E-6,4.8263618194377E-6,
5.01000917339973E-6,6.13126454147497E-6,8.60486650288862E-6,9.21144281170494E-6,
1.24722301135921E-5,1.42666454787858E-5,2.04670653756916E-5,2.08026438176805E-5),
 .UNSPECIFIED.);
#25312=B_SPLINE_CURVE_WITH_KNOTS('',3,(#391279,#391280,#391281,#391282),
 .UNSPECIFIED.,.F.,.F.,(4,4),(0.,0.000109384345496909),.UNSPECIFIED.);
#25313=B_SPLINE_CURVE_WITH_KNOTS('',3,(#391387,#391388,#391389,#391390),
 .UNSPECIFIED.,.F.,.F.,(4,4),(0.,9.54361881492175E-5),.UNSPECIFIED.);
#25314=B_SPLINE_CURVE_WITH_KNOTS('',3,(#391395,#391396,#391397,#391398,
#391399,#391400,#391401),.UNSPECIFIED.,.F.,.F.,(4,3,4),(0.,4.4106970432347E-5,
0.000113970027818833),.UNSPECIFIED.);
#25315=B_SPLINE_CURVE_WITH_KNOTS('',3,(#391407,#391408,#391409,#391410),
 .UNSPECIFIED.,.F.,.F.,(4,4),(2.16840434497101E-19,9.54361881492182E-5),
 .UNSPECIFIED.);
#25316=B_SPLINE_CURVE_WITH_KNOTS('',3,(#391414,#391415,#391416,#391417,
#391418,#391419,#391420),.UNSPECIFIED.,.F.,.F.,(4,3,4),(0.,6.98630244191491E-5,
0.000113969974038089),.UNSPECIFIED.);
#25317=B_SPLINE_CURVE_WITH_KNOTS('',3,(#391423,#391424,#391425,#391426,
#391427,#391428,#391429,#391430,#391431,#391432,#391433,#391434,#391435,
#391436,#391437,#391438,#391439,#391440,#391441,#391442,#391443,#391444,
#391445,#391446,#391447,#391448,#391449,#391450,#391451,#391452,#391453,
#391454,#391455,#391456,#391457,#391458,#391459,#391460,#391461,#391462,
#391463,#391464,#391465,#391466,#391467,#391468,#391469,#391470,#391471),
 .UNSPECIFIED.,.F.,.F.,(4,3,3,3,3,3,3,3,3,3,3,3,3,3,3,3,4),(0.,1.53100299373416E-6,
4.52554775679338E-6,7.01151246291604E-6,9.26752933799479E-6,1.03084066197174E-5,
1.1713899082686E-5,1.22284894984072E-5,1.30315035324815E-5,1.3836372849781E-5,
1.40464197777492E-5,1.54597749564636E-5,1.62073588704064E-5,1.92092968712892E-5,
1.95234416882548E-5,2.37637844577542E-5,2.61487188977248E-5),
 .UNSPECIFIED.);
#25318=B_SPLINE_CURVE_WITH_KNOTS('',3,(#391486,#391487,#391488,#391489,
#391490,#391491,#391492,#391493,#391494,#391495,#391496,#391497,#391498,
#391499,#391500,#391501,#391502,#391503,#391504,#391505,#391506,#391507,
#391508,#391509,#391510,#391511,#391512,#391513,#391514,#391515,#391516),
 .UNSPECIFIED.,.F.,.F.,(4,3,3,3,3,3,3,3,3,3,4),(0.,3.95507910398083E-6,
7.53768426604198E-6,1.19904533335351E-5,1.40475043392585E-5,1.51452104275965E-5,
1.67866272814139E-5,1.69621513005358E-5,1.81338315460711E-5,1.98906334656541E-5,
2.06132424588244E-5),.UNSPECIFIED.);
#25319=B_SPLINE_CURVE_WITH_KNOTS('',3,(#391519,#391520,#391521,#391522),
 .UNSPECIFIED.,.F.,.F.,(4,4),(4.84869951806108E-19,0.00010938435327491),
 .UNSPECIFIED.);
#25320=B_SPLINE_CURVE_WITH_KNOTS('',3,(#391549,#391550,#391551,#391552,
#391553,#391554,#391555,#391556,#391557,#391558,#391559,#391560,#391561,
#391562,#391563,#391564,#391565,#391566,#391567,#391568,#391569,#391570,
#391571,#391572,#391573,#391574,#391575,#391576,#391577,#391578,#391579,
#391580,#391581,#391582),.UNSPECIFIED.,.F.,.F.,(4,3,3,3,3,3,3,3,3,3,3,4),
(2.16840434497101E-19,2.0962399272943E-6,3.17176647120214E-6,4.82636181942743E-6,
5.01000917339943E-6,6.13126454147466E-6,8.60486650288832E-6,9.21144281170473E-6,
1.24722301136018E-5,1.42666454787853E-5,2.04670653757024E-5,2.08026438176798E-5),
 .UNSPECIFIED.);
#25321=B_SPLINE_CURVE_WITH_KNOTS('',3,(#391583,#391584,#391585,#391586),
 .UNSPECIFIED.,.F.,.F.,(4,4),(0.,0.000109384345496908),.UNSPECIFIED.);
#25322=B_SPLINE_CURVE_WITH_KNOTS('',3,(#391691,#391692,#391693,#391694),
 .UNSPECIFIED.,.F.,.F.,(4,4),(0.,9.54361881492178E-5),.UNSPECIFIED.);
#25323=B_SPLINE_CURVE_WITH_KNOTS('',3,(#391699,#391700,#391701,#391702,
#391703,#391704,#391705),.UNSPECIFIED.,.F.,.F.,(4,3,4),(0.,4.4106970432347E-5,
0.000113970027818834),.UNSPECIFIED.);
#25324=B_SPLINE_CURVE_WITH_KNOTS('',3,(#391711,#391712,#391713,#391714),
 .UNSPECIFIED.,.F.,.F.,(4,4),(2.16840434497101E-19,9.54361881492179E-5),
 .UNSPECIFIED.);
#25325=B_SPLINE_CURVE_WITH_KNOTS('',3,(#391718,#391719,#391720,#391721,
#391722,#391723,#391724),.UNSPECIFIED.,.F.,.F.,(4,3,4),(0.,6.98630244191491E-5,
0.000113969974038089),.UNSPECIFIED.);
#25326=B_SPLINE_CURVE_WITH_KNOTS('',3,(#391727,#391728,#391729,#391730,
#391731,#391732,#391733,#391734,#391735,#391736,#391737,#391738,#391739,
#391740,#391741,#391742,#391743,#391744,#391745,#391746,#391747,#391748,
#391749,#391750,#391751,#391752,#391753,#391754,#391755,#391756,#391757,
#391758,#391759,#391760,#391761,#391762,#391763,#391764,#391765,#391766,
#391767,#391768,#391769,#391770,#391771,#391772,#391773,#391774,#391775),
 .UNSPECIFIED.,.F.,.F.,(4,3,3,3,3,3,3,3,3,3,3,3,3,3,3,3,4),(0.,1.53100299373418E-6,
4.52554775679414E-6,7.01151246291608E-6,9.26752933800765E-6,1.03084066197173E-5,
1.1713899082686E-5,1.22284894984074E-5,1.30315035324818E-5,1.38363728497812E-5,
1.40464197777496E-5,1.54597749564643E-5,1.62073588704071E-5,1.92092968712819E-5,
1.95234416882561E-5,2.37637844577578E-5,2.61487188977273E-5),
 .UNSPECIFIED.);
#25327=B_SPLINE_CURVE_WITH_KNOTS('',3,(#391790,#391791,#391792,#391793,
#391794,#391795,#391796,#391797,#391798,#391799,#391800,#391801,#391802,
#391803,#391804,#391805,#391806,#391807,#391808,#391809,#391810,#391811,
#391812,#391813,#391814,#391815,#391816,#391817,#391818,#391819,#391820),
 .UNSPECIFIED.,.F.,.F.,(4,3,3,3,3,3,3,3,3,3,4),(0.,3.95507910397348E-6,
7.53768426604206E-6,1.19904533335352E-5,1.40475043392587E-5,1.51452104275967E-5,
1.67866272814203E-5,1.6962151300536E-5,1.81338315460713E-5,1.98906334656551E-5,
2.0613242458825E-5),.UNSPECIFIED.);
#25328=B_SPLINE_CURVE_WITH_KNOTS('',3,(#391823,#391824,#391825,#391826),
 .UNSPECIFIED.,.F.,.F.,(4,4),(4.84869951806108E-19,0.00010938435327491),
 .UNSPECIFIED.);
#25329=B_SPLINE_CURVE_WITH_KNOTS('',3,(#391853,#391854,#391855,#391856,
#391857,#391858,#391859,#391860,#391861,#391862,#391863,#391864,#391865,
#391866,#391867,#391868,#391869,#391870,#391871,#391872,#391873,#391874,
#391875,#391876,#391877,#391878,#391879,#391880,#391881,#391882,#391883,
#391884,#391885,#391886),.UNSPECIFIED.,.F.,.F.,(4,3,3,3,3,3,3,3,3,3,3,4),
(2.16840434497101E-19,2.0962399272944E-6,3.17176647120218E-6,4.82636181944615E-6,
5.01000917339954E-6,6.13126454147516E-6,8.6048665028885E-6,9.21144281170492E-6,
1.24722301135926E-5,1.42666454787855E-5,2.04670653756851E-5,2.08026438176801E-5),
 .UNSPECIFIED.);
#25330=B_SPLINE_CURVE_WITH_KNOTS('',3,(#391887,#391888,#391889,#391890),
 .UNSPECIFIED.,.F.,.F.,(4,4),(0.,0.000109384345496908),.UNSPECIFIED.);
#25331=B_SPLINE_CURVE_WITH_KNOTS('',3,(#391995,#391996,#391997,#391998),
 .UNSPECIFIED.,.F.,.F.,(4,4),(0.,9.54361881492175E-5),.UNSPECIFIED.);
#25332=B_SPLINE_CURVE_WITH_KNOTS('',3,(#392003,#392004,#392005,#392006,
#392007,#392008,#392009),.UNSPECIFIED.,.F.,.F.,(4,3,4),(0.,4.41069704323471E-5,
0.000113970027818833),.UNSPECIFIED.);
#25333=B_SPLINE_CURVE_WITH_KNOTS('',3,(#392015,#392016,#392017,#392018),
 .UNSPECIFIED.,.F.,.F.,(4,4),(2.16840434497101E-19,9.54361881492179E-5),
 .UNSPECIFIED.);
#25334=B_SPLINE_CURVE_WITH_KNOTS('',3,(#392022,#392023,#392024,#392025,
#392026,#392027,#392028),.UNSPECIFIED.,.F.,.F.,(4,3,4),(0.,6.98630244191488E-5,
0.000113969974038089),.UNSPECIFIED.);
#25335=B_SPLINE_CURVE_WITH_KNOTS('',3,(#392031,#392032,#392033,#392034,
#392035,#392036,#392037,#392038,#392039,#392040,#392041,#392042,#392043,
#392044,#392045,#392046,#392047,#392048,#392049,#392050,#392051,#392052,
#392053,#392054,#392055,#392056,#392057,#392058,#392059,#392060,#392061,
#392062,#392063,#392064,#392065,#392066,#392067,#392068,#392069,#392070,
#392071,#392072,#392073,#392074,#392075,#392076,#392077,#392078,#392079),
 .UNSPECIFIED.,.F.,.F.,(4,3,3,3,3,3,3,3,3,3,3,3,3,3,3,3,4),(0.,1.53100299373417E-6,
4.52554775678998E-6,7.01151246291595E-6,9.26752933800364E-6,1.03084066197173E-5,
1.1713899082686E-5,1.22284894984073E-5,1.30315035324817E-5,1.38363728497812E-5,
1.40464197777493E-5,1.54597749564639E-5,1.62073588704067E-5,1.92092968713107E-5,
1.95234416882552E-5,2.37637844577573E-5,2.61487188977257E-5),
 .UNSPECIFIED.);
#25336=B_SPLINE_CURVE_WITH_KNOTS('',3,(#392094,#392095,#392096,#392097,
#392098,#392099,#392100,#392101,#392102,#392103,#392104,#392105,#392106,
#392107,#392108,#392109,#392110,#392111,#392112,#392113,#392114,#392115,
#392116,#392117,#392118,#392119,#392120,#392121,#392122,#392123,#392124),
 .UNSPECIFIED.,.F.,.F.,(4,3,3,3,3,3,3,3,3,3,4),(0.,3.95507910397914E-6,
7.53768426604207E-6,1.19904533335351E-5,1.40475043392588E-5,1.51452104275968E-5,
1.67866272814232E-5,1.69621513005362E-5,1.81338315460716E-5,1.98906334656541E-5,
2.0613242458825E-5),.UNSPECIFIED.);
#25337=B_SPLINE_CURVE_WITH_KNOTS('',3,(#392127,#392128,#392129,#392130),
 .UNSPECIFIED.,.F.,.F.,(4,4),(2.16840434497101E-19,0.00010938435327491),
 .UNSPECIFIED.);
#25338=B_SPLINE_CURVE_WITH_KNOTS('',3,(#392157,#392158,#392159,#392160,
#392161,#392162,#392163,#392164,#392165,#392166,#392167,#392168,#392169,
#392170,#392171,#392172,#392173,#392174,#392175,#392176,#392177,#392178,
#392179,#392180,#392181,#392182,#392183,#392184,#392185,#392186,#392187,
#392188,#392189,#392190),.UNSPECIFIED.,.F.,.F.,(4,3,3,3,3,3,3,3,3,3,3,4),
(4.84869951806108E-19,2.0962399272945E-6,3.17176647120198E-6,4.82636181944282E-6,
5.01000917339938E-6,6.1312645414749E-6,8.60486650288829E-6,9.21144281170457E-6,
1.24722301135921E-5,1.42666454787849E-5,2.04670653756833E-5,2.08026438176789E-5),
 .UNSPECIFIED.);
#25339=B_SPLINE_CURVE_WITH_KNOTS('',3,(#392191,#392192,#392193,#392194),
 .UNSPECIFIED.,.F.,.F.,(4,4),(0.,0.000109384345496908),.UNSPECIFIED.);
#25340=B_SPLINE_CURVE_WITH_KNOTS('',3,(#392299,#392300,#392301,#392302),
 .UNSPECIFIED.,.F.,.F.,(4,4),(0.,9.54361881492172E-5),.UNSPECIFIED.);
#25341=B_SPLINE_CURVE_WITH_KNOTS('',3,(#392307,#392308,#392309,#392310,
#392311,#392312,#392313),.UNSPECIFIED.,.F.,.F.,(4,3,4),(0.,4.41069704323467E-5,
0.000113970027818833),.UNSPECIFIED.);
#25342=B_SPLINE_CURVE_WITH_KNOTS('',3,(#392319,#392320,#392321,#392322),
 .UNSPECIFIED.,.F.,.F.,(4,4),(2.16840434497101E-19,9.54361881492177E-5),
 .UNSPECIFIED.);
#25343=B_SPLINE_CURVE_WITH_KNOTS('',3,(#392326,#392327,#392328,#392329,
#392330,#392331,#392332),.UNSPECIFIED.,.F.,.F.,(4,3,4),(0.,6.9863024419149E-5,
0.000113969974038089),.UNSPECIFIED.);
#25344=B_SPLINE_CURVE_WITH_KNOTS('',3,(#392335,#392336,#392337,#392338,
#392339,#392340,#392341,#392342,#392343,#392344,#392345,#392346,#392347,
#392348,#392349,#392350,#392351,#392352,#392353,#392354,#392355,#392356,
#392357,#392358,#392359,#392360,#392361,#392362,#392363,#392364,#392365,
#392366,#392367,#392368,#392369,#392370,#392371,#392372,#392373,#392374,
#392375,#392376,#392377,#392378,#392379,#392380,#392381,#392382,#392383),
 .UNSPECIFIED.,.F.,.F.,(4,3,3,3,3,3,3,3,3,3,3,3,3,3,3,3,4),(0.,1.53100299373411E-6,
4.52554775678843E-6,7.01151246291605E-6,9.2675293380181E-6,1.03084066197174E-5,
1.17138990826862E-5,1.22284894984073E-5,1.30315035324817E-5,1.38363728497813E-5,
1.40464197777498E-5,1.5459774956464E-5,1.62073588704072E-5,1.92092968712942E-5,
1.9523441688256E-5,2.37637844577598E-5,2.61487188977274E-5),
 .UNSPECIFIED.);
#25345=B_SPLINE_CURVE_WITH_KNOTS('',3,(#392398,#392399,#392400,#392401,
#392402,#392403,#392404,#392405,#392406,#392407,#392408,#392409,#392410,
#392411,#392412,#392413,#392414,#392415,#392416,#392417,#392418,#392419,
#392420,#392421,#392422,#392423,#392424,#392425,#392426,#392427,#392428),
 .UNSPECIFIED.,.F.,.F.,(4,3,3,3,3,3,3,3,3,3,4),(0.,3.95507910397759E-6,
7.53768426604205E-6,1.19904533335349E-5,1.40475043392584E-5,1.51452104275962E-5,
1.67866272813981E-5,1.69621513005359E-5,1.81338315460713E-5,1.98906334656512E-5,
2.06132424588244E-5),.UNSPECIFIED.);
#25346=B_SPLINE_CURVE_WITH_KNOTS('',3,(#392431,#392432,#392433,#392434),
 .UNSPECIFIED.,.F.,.F.,(4,4),(4.33680868994202E-19,0.00010938435327491),
 .UNSPECIFIED.);
#25347=B_SPLINE_CURVE_WITH_KNOTS('',3,(#392461,#392462,#392463,#392464,
#392465,#392466,#392467,#392468,#392469,#392470,#392471,#392472,#392473,
#392474,#392475,#392476,#392477,#392478,#392479,#392480,#392481,#392482,
#392483,#392484,#392485,#392486,#392487,#392488,#392489,#392490,#392491,
#392492,#392493,#392494),.UNSPECIFIED.,.F.,.F.,(4,3,3,3,3,3,3,3,3,3,3,4),
(2.16840434497101E-19,2.09623992729441E-6,3.17176647120199E-6,4.82636181942181E-6,
5.01000917339924E-6,6.13126454147485E-6,8.60486650288836E-6,9.21144281170481E-6,
1.24722301135933E-5,1.42666454787854E-5,2.04670653757255E-5,2.08026438176801E-5),
 .UNSPECIFIED.);
#25348=B_SPLINE_CURVE_WITH_KNOTS('',3,(#392495,#392496,#392497,#392498),
 .UNSPECIFIED.,.F.,.F.,(4,4),(0.,0.000109384345496909),.UNSPECIFIED.);
#25349=B_SPLINE_CURVE_WITH_KNOTS('',3,(#392603,#392604,#392605,#392606),
 .UNSPECIFIED.,.F.,.F.,(4,4),(0.,9.54361881492178E-5),.UNSPECIFIED.);
#25350=B_SPLINE_CURVE_WITH_KNOTS('',3,(#392611,#392612,#392613,#392614,
#392615,#392616,#392617),.UNSPECIFIED.,.F.,.F.,(4,3,4),(0.,4.41069704323472E-5,
0.000113970027818834),.UNSPECIFIED.);
#25351=B_SPLINE_CURVE_WITH_KNOTS('',3,(#392623,#392624,#392625,#392626),
 .UNSPECIFIED.,.F.,.F.,(4,4),(2.16840434497101E-19,9.54361881492178E-5),
 .UNSPECIFIED.);
#25352=B_SPLINE_CURVE_WITH_KNOTS('',3,(#392630,#392631,#392632,#392633,
#392634,#392635,#392636),.UNSPECIFIED.,.F.,.F.,(4,3,4),(0.,6.98630244191492E-5,
0.000113969974038089),.UNSPECIFIED.);
#25353=B_SPLINE_CURVE_WITH_KNOTS('',3,(#392639,#392640,#392641,#392642,
#392643,#392644,#392645,#392646,#392647,#392648,#392649,#392650,#392651,
#392652,#392653,#392654,#392655,#392656,#392657,#392658,#392659,#392660,
#392661,#392662,#392663,#392664,#392665,#392666,#392667,#392668,#392669,
#392670,#392671,#392672,#392673,#392674,#392675,#392676,#392677,#392678,
#392679,#392680,#392681,#392682,#392683,#392684,#392685,#392686,#392687),
 .UNSPECIFIED.,.F.,.F.,(4,3,3,3,3,3,3,3,3,3,3,3,3,3,3,3,4),(0.,1.53100299373412E-6,
4.52554775679078E-6,7.011512462916E-6,9.26752933800588E-6,1.03084066197174E-5,
1.17138990826862E-5,1.22284894984074E-5,1.30315035324818E-5,1.38363728497811E-5,
1.40464197777491E-5,1.54597749564639E-5,1.62073588704066E-5,1.92092968713222E-5,
1.95234416882547E-5,2.37637844577591E-5,2.61487188977244E-5),
 .UNSPECIFIED.);
#25354=B_SPLINE_CURVE_WITH_KNOTS('',3,(#392702,#392703,#392704,#392705,
#392706,#392707,#392708,#392709,#392710,#392711,#392712,#392713,#392714,
#392715,#392716,#392717,#392718,#392719,#392720,#392721,#392722,#392723,
#392724,#392725,#392726,#392727,#392728,#392729,#392730,#392731,#392732),
 .UNSPECIFIED.,.F.,.F.,(4,3,3,3,3,3,3,3,3,3,4),(0.,3.95507910396997E-6,
7.53768426604195E-6,1.19904533335349E-5,1.40475043392585E-5,1.51452104275965E-5,
1.67866272814111E-5,1.69621513005356E-5,1.81338315460712E-5,1.98906334656546E-5,
2.06132424588245E-5),.UNSPECIFIED.);
#25355=B_SPLINE_CURVE_WITH_KNOTS('',3,(#392735,#392736,#392737,#392738),
 .UNSPECIFIED.,.F.,.F.,(4,4),(2.16840434497101E-19,0.00010938435327491),
 .UNSPECIFIED.);
#25356=B_SPLINE_CURVE_WITH_KNOTS('',3,(#392765,#392766,#392767,#392768,
#392769,#392770,#392771,#392772,#392773,#392774,#392775,#392776,#392777,
#392778,#392779,#392780,#392781,#392782,#392783,#392784,#392785,#392786,
#392787,#392788,#392789,#392790,#392791,#392792,#392793,#392794,#392795,
#392796,#392797,#392798),.UNSPECIFIED.,.F.,.F.,(4,3,3,3,3,3,3,3,3,3,3,4),
(0.,2.09623992729438E-6,3.17176647120216E-6,4.82636181943502E-6,5.01000917339982E-6,
6.13126454147495E-6,8.60486650288879E-6,9.21144281170511E-6,1.2472230113587E-5,
1.42666454787859E-5,2.04670653756995E-5,2.08026438176806E-5),
 .UNSPECIFIED.);
#25357=B_SPLINE_CURVE_WITH_KNOTS('',3,(#392799,#392800,#392801,#392802),
 .UNSPECIFIED.,.F.,.F.,(4,4),(0.,0.000109384345496908),.UNSPECIFIED.);
#25358=B_SPLINE_CURVE_WITH_KNOTS('',3,(#392907,#392908,#392909,#392910),
 .UNSPECIFIED.,.F.,.F.,(4,4),(0.,9.54361881492172E-5),.UNSPECIFIED.);
#25359=B_SPLINE_CURVE_WITH_KNOTS('',3,(#392915,#392916,#392917,#392918,
#392919,#392920,#392921),.UNSPECIFIED.,.F.,.F.,(4,3,4),(0.,4.41069704323469E-5,
0.000113970027818833),.UNSPECIFIED.);
#25360=B_SPLINE_CURVE_WITH_KNOTS('',3,(#392927,#392928,#392929,#392930),
 .UNSPECIFIED.,.F.,.F.,(4,4),(2.16840434497101E-19,9.5436188149218E-5),
 .UNSPECIFIED.);
#25361=B_SPLINE_CURVE_WITH_KNOTS('',3,(#392934,#392935,#392936,#392937,
#392938,#392939,#392940),.UNSPECIFIED.,.F.,.F.,(4,3,4),(0.,6.98630244191489E-5,
0.000113969974038089),.UNSPECIFIED.);
#25362=B_SPLINE_CURVE_WITH_KNOTS('',3,(#392943,#392944,#392945,#392946,
#392947,#392948,#392949,#392950,#392951,#392952,#392953,#392954,#392955,
#392956,#392957,#392958,#392959,#392960,#392961,#392962,#392963,#392964,
#392965,#392966,#392967,#392968,#392969,#392970,#392971,#392972,#392973,
#392974,#392975,#392976,#392977,#392978,#392979,#392980,#392981,#392982,
#392983,#392984,#392985,#392986,#392987,#392988,#392989,#392990,#392991),
 .UNSPECIFIED.,.F.,.F.,(4,3,3,3,3,3,3,3,3,3,3,3,3,3,3,3,4),(0.,1.53100299373414E-6,
4.52554775679806E-6,7.0115124629161E-6,9.26752933798902E-6,1.03084066197172E-5,
1.17138990826862E-5,1.22284894984076E-5,1.30315035324815E-5,1.38363728497814E-5,
1.40464197777496E-5,1.54597749564639E-5,1.62073588704069E-5,1.9209296871272E-5,
1.95234416882556E-5,2.37637844577596E-5,2.61487188977267E-5),
 .UNSPECIFIED.);
#25363=B_SPLINE_CURVE_WITH_KNOTS('',3,(#393006,#393007,#393008,#393009,
#393010,#393011,#393012,#393013,#393014,#393015,#393016,#393017,#393018,
#393019,#393020,#393021,#393022,#393023,#393024,#393025,#393026,#393027,
#393028,#393029,#393030,#393031,#393032,#393033,#393034,#393035,#393036),
 .UNSPECIFIED.,.F.,.F.,(4,3,3,3,3,3,3,3,3,3,4),(0.,3.95507910398563E-6,
7.53768426604196E-6,1.1990453333535E-5,1.40475043392585E-5,1.51452104275965E-5,
1.67866272814175E-5,1.69621513005359E-5,1.81338315460713E-5,1.98906334656545E-5,
2.06132424588247E-5),.UNSPECIFIED.);
#25364=B_SPLINE_CURVE_WITH_KNOTS('',3,(#393039,#393040,#393041,#393042),
 .UNSPECIFIED.,.F.,.F.,(4,4),(4.33680868994202E-19,0.00010938435327491),
 .UNSPECIFIED.);
#25365=B_SPLINE_CURVE_WITH_KNOTS('',3,(#393069,#393070,#393071,#393072,
#393073,#393074,#393075,#393076,#393077,#393078,#393079,#393080,#393081,
#393082,#393083,#393084,#393085,#393086,#393087,#393088,#393089,#393090,
#393091,#393092,#393093,#393094,#393095,#393096,#393097,#393098,#393099,
#393100,#393101,#393102),.UNSPECIFIED.,.F.,.F.,(4,3,3,3,3,3,3,3,3,3,3,4),
(0.,2.09623992729478E-6,3.17176647120224E-6,4.82636181942829E-6,5.01000917339992E-6,
6.13126454147526E-6,8.60486650288872E-6,9.21144281170506E-6,1.24722301135961E-5,
1.42666454787857E-5,2.0467065375705E-5,2.08026438176803E-5),
 .UNSPECIFIED.);
#25366=B_SPLINE_CURVE_WITH_KNOTS('',3,(#393103,#393104,#393105,#393106),
 .UNSPECIFIED.,.F.,.F.,(4,4),(0.,0.000109384345496908),.UNSPECIFIED.);
#25367=B_SPLINE_CURVE_WITH_KNOTS('',3,(#393211,#393212,#393213,#393214),
 .UNSPECIFIED.,.F.,.F.,(4,4),(0.,9.54361881492174E-5),.UNSPECIFIED.);
#25368=B_SPLINE_CURVE_WITH_KNOTS('',3,(#393219,#393220,#393221,#393222,
#393223,#393224,#393225),.UNSPECIFIED.,.F.,.F.,(4,3,4),(0.,4.41069704323471E-5,
0.000113970027818833),.UNSPECIFIED.);
#25369=B_SPLINE_CURVE_WITH_KNOTS('',3,(#393231,#393232,#393233,#393234),
 .UNSPECIFIED.,.F.,.F.,(4,4),(2.16840434497101E-19,9.54361881492179E-5),
 .UNSPECIFIED.);
#25370=B_SPLINE_CURVE_WITH_KNOTS('',3,(#393238,#393239,#393240,#393241,
#393242,#393243,#393244),.UNSPECIFIED.,.F.,.F.,(4,3,4),(0.,6.9863024419149E-5,
0.000113969974038089),.UNSPECIFIED.);
#25371=B_SPLINE_CURVE_WITH_KNOTS('',3,(#393247,#393248,#393249,#393250,
#393251,#393252,#393253,#393254,#393255,#393256,#393257,#393258,#393259,
#393260,#393261,#393262,#393263,#393264,#393265,#393266,#393267,#393268,
#393269,#393270,#393271,#393272,#393273,#393274,#393275,#393276,#393277,
#393278,#393279,#393280,#393281,#393282,#393283,#393284,#393285,#393286,
#393287,#393288,#393289,#393290,#393291,#393292,#393293,#393294,#393295),
 .UNSPECIFIED.,.F.,.F.,(4,3,3,3,3,3,3,3,3,3,3,3,3,3,3,3,4),(0.,1.53100299373417E-6,
4.525547756795E-6,7.011512462916E-6,9.26752933799827E-6,1.03084066197174E-5,
1.17138990826862E-5,1.22284894984076E-5,1.30315035324817E-5,1.38363728497811E-5,
1.40464197777495E-5,1.5459774956464E-5,1.62073588704069E-5,1.920929687129E-5,
1.95234416882555E-5,2.37637844577568E-5,2.61487188977261E-5),
 .UNSPECIFIED.);
#25372=B_SPLINE_CURVE_WITH_KNOTS('',3,(#393310,#393311,#393312,#393313,
#393314,#393315,#393316,#393317,#393318,#393319,#393320,#393321,#393322,
#393323,#393324,#393325,#393326,#393327,#393328,#393329,#393330,#393331,
#393332,#393333,#393334,#393335,#393336,#393337,#393338,#393339,#393340),
 .UNSPECIFIED.,.F.,.F.,(4,3,3,3,3,3,3,3,3,3,4),(0.,3.9550791039817E-6,7.537684266042E-6,
1.1990453333535E-5,1.40475043392584E-5,1.51452104275964E-5,1.67866272814146E-5,
1.69621513005355E-5,1.81338315460708E-5,1.98906334656541E-5,2.06132424588239E-5),
 .UNSPECIFIED.);
#25373=B_SPLINE_CURVE_WITH_KNOTS('',3,(#393343,#393344,#393345,#393346),
 .UNSPECIFIED.,.F.,.F.,(4,4),(9.93687704810078E-19,0.00010938435327491),
 .UNSPECIFIED.);
#25374=B_SPLINE_CURVE_WITH_KNOTS('',3,(#393373,#393374,#393375,#393376,
#393377,#393378,#393379,#393380,#393381,#393382,#393383,#393384,#393385,
#393386,#393387,#393388,#393389,#393390,#393391,#393392,#393393,#393394,
#393395,#393396,#393397,#393398,#393399,#393400,#393401,#393402,#393403,
#393404,#393405,#393406),.UNSPECIFIED.,.F.,.F.,(4,3,3,3,3,3,3,3,3,3,3,4),
(4.84869951806108E-19,2.09623992729445E-6,3.17176647120213E-6,4.82636181942555E-6,
5.01000917339949E-6,6.13126454147482E-6,8.6048665028884E-6,9.21144281170475E-6,
1.24722301135981E-5,1.42666454787855E-5,2.04670653756909E-5,2.08026438176802E-5),
 .UNSPECIFIED.);
#25375=B_SPLINE_CURVE_WITH_KNOTS('',3,(#393407,#393408,#393409,#393410),
 .UNSPECIFIED.,.F.,.F.,(4,4),(0.,0.000109384345496908),.UNSPECIFIED.);
#25376=B_SPLINE_CURVE_WITH_KNOTS('',3,(#393515,#393516,#393517,#393518),
 .UNSPECIFIED.,.F.,.F.,(4,4),(0.,9.54361881492174E-5),.UNSPECIFIED.);
#25377=B_SPLINE_CURVE_WITH_KNOTS('',3,(#393523,#393524,#393525,#393526,
#393527,#393528,#393529),.UNSPECIFIED.,.F.,.F.,(4,3,4),(0.,4.41069704323467E-5,
0.000113970027818833),.UNSPECIFIED.);
#25378=B_SPLINE_CURVE_WITH_KNOTS('',3,(#393535,#393536,#393537,#393538),
 .UNSPECIFIED.,.F.,.F.,(4,4),(4.84869951806108E-19,9.54361881492179E-5),
 .UNSPECIFIED.);
#25379=B_SPLINE_CURVE_WITH_KNOTS('',3,(#393542,#393543,#393544,#393545,
#393546,#393547,#393548),.UNSPECIFIED.,.F.,.F.,(4,3,4),(0.,6.98630244191489E-5,
0.000113969974038089),.UNSPECIFIED.);
#25380=B_SPLINE_CURVE_WITH_KNOTS('',3,(#393551,#393552,#393553,#393554,
#393555,#393556,#393557,#393558,#393559,#393560,#393561,#393562,#393563,
#393564,#393565,#393566,#393567,#393568,#393569,#393570,#393571,#393572,
#393573,#393574,#393575,#393576,#393577,#393578,#393579,#393580,#393581,
#393582,#393583,#393584,#393585,#393586,#393587,#393588,#393589,#393590,
#393591,#393592,#393593,#393594,#393595,#393596,#393597,#393598,#393599),
 .UNSPECIFIED.,.F.,.F.,(4,3,3,3,3,3,3,3,3,3,3,3,3,3,3,3,4),(0.,1.53100299373405E-6,
4.52554775679208E-6,7.01151246291602E-6,9.26752933800532E-6,1.03084066197175E-5,
1.17138990826864E-5,1.22284894984073E-5,1.30315035324821E-5,1.38363728497815E-5,
1.40464197777496E-5,1.54597749564641E-5,1.6207358870407E-5,1.9209296871288E-5,
1.95234416882559E-5,2.37637844577587E-5,2.61487188977268E-5),
 .UNSPECIFIED.);
#25381=B_SPLINE_CURVE_WITH_KNOTS('',3,(#393614,#393615,#393616,#393617,
#393618,#393619,#393620,#393621,#393622,#393623,#393624,#393625,#393626,
#393627,#393628,#393629,#393630,#393631,#393632,#393633,#393634,#393635,
#393636,#393637,#393638,#393639,#393640,#393641,#393642,#393643,#393644),
 .UNSPECIFIED.,.F.,.F.,(4,3,3,3,3,3,3,3,3,3,4),(0.,3.95507910397499E-6,
7.53768426604193E-6,1.1990453333535E-5,1.40475043392585E-5,1.51452104275963E-5,
1.67866272814283E-5,1.69621513005353E-5,1.81338315460707E-5,1.98906334656536E-5,
2.06132424588236E-5),.UNSPECIFIED.);
#25382=B_SPLINE_CURVE_WITH_KNOTS('',3,(#393647,#393648,#393649,#393650),
 .UNSPECIFIED.,.F.,.F.,(4,4),(4.33680868994202E-19,0.00010938435327491),
 .UNSPECIFIED.);
#25383=B_SPLINE_CURVE_WITH_KNOTS('',3,(#393677,#393678,#393679,#393680,
#393681,#393682,#393683,#393684,#393685,#393686,#393687,#393688,#393689,
#393690,#393691,#393692,#393693,#393694,#393695,#393696,#393697,#393698,
#393699,#393700,#393701,#393702,#393703,#393704,#393705,#393706,#393707,
#393708,#393709,#393710),.UNSPECIFIED.,.F.,.F.,(4,3,3,3,3,3,3,3,3,3,3,4),
(2.16840434497101E-19,2.09623992729444E-6,3.17176647120207E-6,4.8263618194376E-6,
5.01000917339953E-6,6.13126454147488E-6,8.60486650288845E-6,9.21144281170475E-6,
1.24722301135761E-5,1.42666454787854E-5,2.04670653756963E-5,2.08026438176801E-5),
 .UNSPECIFIED.);
#25384=B_SPLINE_CURVE_WITH_KNOTS('',3,(#393711,#393712,#393713,#393714),
 .UNSPECIFIED.,.F.,.F.,(4,4),(0.,0.000109384345496908),.UNSPECIFIED.);
#25385=B_SPLINE_CURVE_WITH_KNOTS('',3,(#393819,#393820,#393821,#393822),
 .UNSPECIFIED.,.F.,.F.,(4,4),(0.,9.54361881492176E-5),.UNSPECIFIED.);
#25386=B_SPLINE_CURVE_WITH_KNOTS('',3,(#393827,#393828,#393829,#393830,
#393831,#393832,#393833),.UNSPECIFIED.,.F.,.F.,(4,3,4),(0.,4.41069704323468E-5,
0.000113970027818833),.UNSPECIFIED.);
#25387=B_SPLINE_CURVE_WITH_KNOTS('',3,(#393839,#393840,#393841,#393842),
 .UNSPECIFIED.,.F.,.F.,(4,4),(0.,9.54361881492176E-5),.UNSPECIFIED.);
#25388=B_SPLINE_CURVE_WITH_KNOTS('',3,(#393846,#393847,#393848,#393849,
#393850,#393851,#393852),.UNSPECIFIED.,.F.,.F.,(4,3,4),(0.,6.98630244191492E-5,
0.00011396997403809),.UNSPECIFIED.);
#25389=B_SPLINE_CURVE_WITH_KNOTS('',3,(#393855,#393856,#393857,#393858,
#393859,#393860,#393861,#393862,#393863,#393864,#393865,#393866,#393867,
#393868,#393869,#393870,#393871,#393872,#393873,#393874,#393875,#393876,
#393877,#393878,#393879,#393880,#393881,#393882,#393883,#393884,#393885,
#393886,#393887,#393888,#393889,#393890,#393891,#393892,#393893,#393894,
#393895,#393896,#393897,#393898,#393899,#393900,#393901,#393902,#393903),
 .UNSPECIFIED.,.F.,.F.,(4,3,3,3,3,3,3,3,3,3,3,3,3,3,3,3,4),(0.,1.53100299373406E-6,
4.52554775679239E-6,7.01151246291597E-6,9.26752933799951E-6,1.03084066197172E-5,
1.17138990826861E-5,1.22284894984076E-5,1.30315035324813E-5,1.3836372849781E-5,
1.40464197777494E-5,1.54597749564638E-5,1.62073588704065E-5,1.92092968712532E-5,
1.9523441688255E-5,2.37637844577512E-5,2.61487188977251E-5),
 .UNSPECIFIED.);
#25390=B_SPLINE_CURVE_WITH_KNOTS('',3,(#393918,#393919,#393920,#393921,
#393922,#393923,#393924,#393925,#393926,#393927,#393928,#393929,#393930,
#393931,#393932,#393933,#393934,#393935,#393936,#393937,#393938,#393939,
#393940,#393941,#393942,#393943,#393944,#393945,#393946,#393947,#393948),
 .UNSPECIFIED.,.F.,.F.,(4,3,3,3,3,3,3,3,3,3,4),(0.,3.95507910398327E-6,
7.53768426604179E-6,1.19904533335349E-5,1.40475043392584E-5,1.51452104275965E-5,
1.67866272814327E-5,1.69621513005355E-5,1.8133831546071E-5,1.98906334656535E-5,
2.06132424588242E-5),.UNSPECIFIED.);
#25391=B_SPLINE_CURVE_WITH_KNOTS('',3,(#393951,#393952,#393953,#393954),
 .UNSPECIFIED.,.F.,.F.,(4,4),(4.33680868994202E-19,0.00010938435327491),
 .UNSPECIFIED.);
#25392=B_SPLINE_CURVE_WITH_KNOTS('',3,(#393981,#393982,#393983,#393984,
#393985,#393986,#393987,#393988,#393989,#393990,#393991,#393992,#393993,
#393994,#393995,#393996,#393997,#393998,#393999,#394000,#394001,#394002,
#394003,#394004,#394005,#394006,#394007,#394008,#394009,#394010,#394011,
#394012,#394013,#394014),.UNSPECIFIED.,.F.,.F.,(4,3,3,3,3,3,3,3,3,3,3,4),
(2.16840434497101E-19,2.09623992729472E-6,3.17176647120225E-6,4.82636181943107E-6,
5.01000917339993E-6,6.13126454147534E-6,8.6048665028888E-6,9.21144281170516E-6,
1.24722301135848E-5,1.42666454787862E-5,2.04670653757051E-5,2.08026438176813E-5),
 .UNSPECIFIED.);
#25393=B_SPLINE_CURVE_WITH_KNOTS('',3,(#394015,#394016,#394017,#394018),
 .UNSPECIFIED.,.F.,.F.,(4,4),(0.,0.000109384345496908),.UNSPECIFIED.);
#25394=B_SPLINE_CURVE_WITH_KNOTS('',3,(#394123,#394124,#394125,#394126),
 .UNSPECIFIED.,.F.,.F.,(4,4),(0.,9.54361881492176E-5),.UNSPECIFIED.);
#25395=B_SPLINE_CURVE_WITH_KNOTS('',3,(#394131,#394132,#394133,#394134,
#394135,#394136,#394137),.UNSPECIFIED.,.F.,.F.,(4,3,4),(0.,4.4106970432347E-5,
0.000113970027818834),.UNSPECIFIED.);
#25396=B_SPLINE_CURVE_WITH_KNOTS('',3,(#394143,#394144,#394145,#394146),
 .UNSPECIFIED.,.F.,.F.,(4,4),(0.,9.54361881492175E-5),.UNSPECIFIED.);
#25397=B_SPLINE_CURVE_WITH_KNOTS('',3,(#394150,#394151,#394152,#394153,
#394154,#394155,#394156),.UNSPECIFIED.,.F.,.F.,(4,3,4),(0.,6.9863024419149E-5,
0.000113969974038089),.UNSPECIFIED.);
#25398=B_SPLINE_CURVE_WITH_KNOTS('',3,(#394159,#394160,#394161,#394162,
#394163,#394164,#394165,#394166,#394167,#394168,#394169,#394170,#394171,
#394172,#394173,#394174,#394175,#394176,#394177,#394178,#394179,#394180,
#394181,#394182,#394183,#394184,#394185,#394186,#394187,#394188,#394189,
#394190,#394191,#394192,#394193,#394194,#394195,#394196,#394197,#394198,
#394199,#394200,#394201,#394202,#394203,#394204,#394205,#394206,#394207),
 .UNSPECIFIED.,.F.,.F.,(4,3,3,3,3,3,3,3,3,3,3,3,3,3,3,3,4),(0.,1.53100299373393E-6,
4.52554775679561E-6,7.01151246291605E-6,9.26752933800807E-6,1.03084066197171E-5,
1.17138990826863E-5,1.22284894984075E-5,1.30315035324816E-5,1.38363728497812E-5,
1.40464197777494E-5,1.54597749564639E-5,1.62073588704068E-5,1.92092968713281E-5,
1.95234416882556E-5,2.37637844577602E-5,2.61487188977265E-5),
 .UNSPECIFIED.);
#25399=B_SPLINE_CURVE_WITH_KNOTS('',3,(#394222,#394223,#394224,#394225,
#394226,#394227,#394228,#394229,#394230,#394231,#394232,#394233,#394234,
#394235,#394236,#394237,#394238,#394239,#394240,#394241,#394242,#394243,
#394244,#394245,#394246,#394247,#394248,#394249,#394250,#394251,#394252),
 .UNSPECIFIED.,.F.,.F.,(4,3,3,3,3,3,3,3,3,3,4),(0.,3.95507910397771E-6,
7.53768426604197E-6,1.19904533335349E-5,1.40475043392583E-5,1.51452104275962E-5,
1.67866272814353E-5,1.69621513005356E-5,1.81338315460708E-5,1.98906334656549E-5,
2.06132424588241E-5),.UNSPECIFIED.);
#25400=B_SPLINE_CURVE_WITH_KNOTS('',3,(#394255,#394256,#394257,#394258),
 .UNSPECIFIED.,.F.,.F.,(4,4),(9.69739903612216E-19,0.00010938435327491),
 .UNSPECIFIED.);
#25401=B_SPLINE_CURVE_WITH_KNOTS('',3,(#394285,#394286,#394287,#394288,
#394289,#394290,#394291,#394292,#394293,#394294,#394295,#394296,#394297,
#394298,#394299,#394300,#394301,#394302,#394303,#394304,#394305,#394306,
#394307,#394308,#394309,#394310,#394311,#394312,#394313,#394314,#394315,
#394316,#394317,#394318),.UNSPECIFIED.,.F.,.F.,(4,3,3,3,3,3,3,3,3,3,3,4),
(0.,2.09623992729454E-6,3.17176647120207E-6,4.82636181943974E-6,5.01000917339967E-6,
6.13126454147483E-6,8.60486650288849E-6,9.21144281170483E-6,1.24722301135987E-5,
1.42666454787853E-5,2.04670653757088E-5,2.080264381768E-5),
 .UNSPECIFIED.);
#25402=B_SPLINE_CURVE_WITH_KNOTS('',3,(#394319,#394320,#394321,#394322),
 .UNSPECIFIED.,.F.,.F.,(4,4),(0.,0.000109384345496908),.UNSPECIFIED.);
#25403=B_SPLINE_CURVE_WITH_KNOTS('',3,(#394427,#394428,#394429,#394430),
 .UNSPECIFIED.,.F.,.F.,(4,4),(0.,9.54361881492175E-5),.UNSPECIFIED.);
#25404=B_SPLINE_CURVE_WITH_KNOTS('',3,(#394435,#394436,#394437,#394438,
#394439,#394440,#394441),.UNSPECIFIED.,.F.,.F.,(4,3,4),(0.,4.4106970432347E-5,
0.000113970027818834),.UNSPECIFIED.);
#25405=B_SPLINE_CURVE_WITH_KNOTS('',3,(#394447,#394448,#394449,#394450),
 .UNSPECIFIED.,.F.,.F.,(4,4),(0.,9.54361881492177E-5),.UNSPECIFIED.);
#25406=B_SPLINE_CURVE_WITH_KNOTS('',3,(#394454,#394455,#394456,#394457,
#394458,#394459,#394460),.UNSPECIFIED.,.F.,.F.,(4,3,4),(0.,6.98630244191489E-5,
0.000113969974038089),.UNSPECIFIED.);
#25407=B_SPLINE_CURVE_WITH_KNOTS('',3,(#394463,#394464,#394465,#394466,
#394467,#394468,#394469,#394470,#394471,#394472,#394473,#394474,#394475,
#394476,#394477,#394478,#394479,#394480,#394481,#394482,#394483,#394484,
#394485,#394486,#394487,#394488,#394489,#394490,#394491,#394492,#394493,
#394494,#394495,#394496,#394497,#394498,#394499,#394500,#394501,#394502,
#394503,#394504,#394505,#394506,#394507,#394508,#394509,#394510,#394511),
 .UNSPECIFIED.,.F.,.F.,(4,3,3,3,3,3,3,3,3,3,3,3,3,3,3,3,4),(0.,1.53100299373408E-6,
4.52554775679461E-6,7.01151246291609E-6,9.26752933799773E-6,1.03084066197175E-5,
1.17138990826864E-5,1.22284894984077E-5,1.3031503532482E-5,1.38363728497815E-5,
1.40464197777496E-5,1.54597749564642E-5,1.62073588704071E-5,1.9209296871317E-5,
1.95234416882557E-5,2.37637844577593E-5,2.61487188977264E-5),
 .UNSPECIFIED.);
#25408=B_SPLINE_CURVE_WITH_KNOTS('',3,(#394526,#394527,#394528,#394529,
#394530,#394531,#394532,#394533,#394534,#394535,#394536,#394537,#394538,
#394539,#394540,#394541,#394542,#394543,#394544,#394545,#394546,#394547,
#394548,#394549,#394550,#394551,#394552,#394553,#394554,#394555,#394556),
 .UNSPECIFIED.,.F.,.F.,(4,3,3,3,3,3,3,3,3,3,4),(0.,3.95507910397035E-6,
7.53768426604196E-6,1.1990453333535E-5,1.40475043392584E-5,1.51452104275963E-5,
1.67866272814298E-5,1.69621513005357E-5,1.8133831546071E-5,1.98906334656556E-5,
2.06132424588243E-5),.UNSPECIFIED.);
#25409=B_SPLINE_CURVE_WITH_KNOTS('',3,(#394559,#394560,#394561,#394562),
 .UNSPECIFIED.,.F.,.F.,(4,4),(9.69739903612216E-19,0.00010938435327491),
 .UNSPECIFIED.);
#25410=B_SPLINE_CURVE_WITH_KNOTS('',3,(#394589,#394590,#394591,#394592,
#394593,#394594,#394595,#394596,#394597,#394598,#394599,#394600,#394601,
#394602,#394603,#394604,#394605,#394606,#394607,#394608,#394609,#394610,
#394611,#394612,#394613,#394614,#394615,#394616,#394617,#394618,#394619,
#394620,#394621,#394622),.UNSPECIFIED.,.F.,.F.,(4,3,3,3,3,3,3,3,3,3,3,4),
(0.,2.09623992729433E-6,3.17176647120226E-6,4.82636181944028E-6,5.01000917339988E-6,
6.1312645414751E-6,8.60486650288875E-6,9.21144281170504E-6,1.2472230113614E-5,
1.4266645478786E-5,2.04670653756726E-5,2.0802643817681E-5),
 .UNSPECIFIED.);
#25411=B_SPLINE_CURVE_WITH_KNOTS('',3,(#394623,#394624,#394625,#394626),
 .UNSPECIFIED.,.F.,.F.,(4,4),(0.,0.000109384345496908),.UNSPECIFIED.);
#25412=B_SPLINE_CURVE_WITH_KNOTS('',3,(#394731,#394732,#394733,#394734),
 .UNSPECIFIED.,.F.,.F.,(4,4),(0.,9.54361881492177E-5),.UNSPECIFIED.);
#25413=B_SPLINE_CURVE_WITH_KNOTS('',3,(#394739,#394740,#394741,#394742,
#394743,#394744,#394745),.UNSPECIFIED.,.F.,.F.,(4,3,4),(0.,4.4106970432347E-5,
0.000113970027818834),.UNSPECIFIED.);
#25414=B_SPLINE_CURVE_WITH_KNOTS('',3,(#394751,#394752,#394753,#394754),
 .UNSPECIFIED.,.F.,.F.,(4,4),(4.33680868994202E-19,9.54361881492179E-5),
 .UNSPECIFIED.);
#25415=B_SPLINE_CURVE_WITH_KNOTS('',3,(#394758,#394759,#394760,#394761,
#394762,#394763,#394764),.UNSPECIFIED.,.F.,.F.,(4,3,4),(0.,6.9863024419149E-5,
0.000113969974038089),.UNSPECIFIED.);
#25416=B_SPLINE_CURVE_WITH_KNOTS('',3,(#394767,#394768,#394769,#394770,
#394771,#394772,#394773,#394774,#394775,#394776,#394777,#394778,#394779,
#394780,#394781,#394782,#394783,#394784,#394785,#394786,#394787,#394788,
#394789,#394790,#394791,#394792,#394793,#394794,#394795,#394796,#394797,
#394798,#394799,#394800,#394801,#394802,#394803,#394804,#394805,#394806,
#394807,#394808,#394809,#394810,#394811,#394812,#394813,#394814,#394815),
 .UNSPECIFIED.,.F.,.F.,(4,3,3,3,3,3,3,3,3,3,3,3,3,3,3,3,4),(0.,1.53100299373416E-6,
4.52554775679475E-6,7.01151246291604E-6,9.26752933800239E-6,1.03084066197174E-5,
1.17138990826861E-5,1.22284894984075E-5,1.30315035324821E-5,1.38363728497814E-5,
1.40464197777497E-5,1.54597749564641E-5,1.62073588704072E-5,1.92092968713027E-5,
1.95234416882558E-5,2.37637844577584E-5,2.61487188977266E-5),
 .UNSPECIFIED.);
#25417=B_SPLINE_CURVE_WITH_KNOTS('',3,(#394830,#394831,#394832,#394833,
#394834,#394835,#394836,#394837,#394838,#394839,#394840,#394841,#394842,
#394843,#394844,#394845,#394846,#394847,#394848,#394849,#394850,#394851,
#394852,#394853,#394854,#394855,#394856,#394857,#394858,#394859,#394860),
 .UNSPECIFIED.,.F.,.F.,(4,3,3,3,3,3,3,3,3,3,4),(0.,3.95507910397657E-6,
7.53768426604195E-6,1.1990453333535E-5,1.40475043392586E-5,1.51452104275963E-5,
1.6786627281397E-5,1.69621513005358E-5,1.81338315460709E-5,1.98906334656537E-5,
2.06132424588241E-5),.UNSPECIFIED.);
#25418=B_SPLINE_CURVE_WITH_KNOTS('',3,(#394863,#394864,#394865,#394866),
 .UNSPECIFIED.,.F.,.F.,(4,4),(4.33680868994202E-19,0.00010938435327491),
 .UNSPECIFIED.);
#25419=B_SPLINE_CURVE_WITH_KNOTS('',3,(#394893,#394894,#394895,#394896,
#394897,#394898,#394899,#394900,#394901,#394902,#394903,#394904,#394905,
#394906,#394907,#394908,#394909,#394910,#394911,#394912,#394913,#394914,
#394915,#394916,#394917,#394918,#394919,#394920,#394921,#394922,#394923,
#394924,#394925,#394926),.UNSPECIFIED.,.F.,.F.,(4,3,3,3,3,3,3,3,3,3,3,4),
(2.16840434497101E-19,2.09623992729442E-6,3.17176647120239E-6,4.82636181941647E-6,
5.01000917339955E-6,6.13126454147491E-6,8.60486650288825E-6,9.21144281170468E-6,
1.2472230113594E-5,1.42666454787851E-5,2.0467065375728E-5,2.08026438176793E-5),
 .UNSPECIFIED.);
#25420=B_SPLINE_CURVE_WITH_KNOTS('',3,(#394927,#394928,#394929,#394930),
 .UNSPECIFIED.,.F.,.F.,(4,4),(0.,0.000109384345496908),.UNSPECIFIED.);
#25421=B_SPLINE_CURVE_WITH_KNOTS('',3,(#395035,#395036,#395037,#395038),
 .UNSPECIFIED.,.F.,.F.,(4,4),(0.,9.54361881492175E-5),.UNSPECIFIED.);
#25422=B_SPLINE_CURVE_WITH_KNOTS('',3,(#395043,#395044,#395045,#395046,
#395047,#395048,#395049),.UNSPECIFIED.,.F.,.F.,(4,3,4),(0.,4.4106970432347E-5,
0.000113970027818833),.UNSPECIFIED.);
#25423=B_SPLINE_CURVE_WITH_KNOTS('',3,(#395055,#395056,#395057,#395058),
 .UNSPECIFIED.,.F.,.F.,(4,4),(4.33680868994202E-19,9.54361881492179E-5),
 .UNSPECIFIED.);
#25424=B_SPLINE_CURVE_WITH_KNOTS('',3,(#395062,#395063,#395064,#395065,
#395066,#395067,#395068),.UNSPECIFIED.,.F.,.F.,(4,3,4),(0.,6.98630244191493E-5,
0.00011396997403809),.UNSPECIFIED.);
#25425=B_SPLINE_CURVE_WITH_KNOTS('',3,(#395071,#395072,#395073,#395074,
#395075,#395076,#395077,#395078,#395079,#395080,#395081,#395082,#395083,
#395084,#395085,#395086,#395087,#395088,#395089,#395090,#395091,#395092,
#395093,#395094,#395095,#395096,#395097,#395098,#395099,#395100,#395101,
#395102,#395103,#395104,#395105,#395106,#395107,#395108,#395109,#395110,
#395111,#395112,#395113,#395114,#395115,#395116,#395117,#395118,#395119),
 .UNSPECIFIED.,.F.,.F.,(4,3,3,3,3,3,3,3,3,3,3,3,3,3,3,3,4),(0.,1.53100299373408E-6,
4.52554775678945E-6,7.01151246291589E-6,9.26752933801257E-6,1.03084066197174E-5,
1.17138990826861E-5,1.22284894984071E-5,1.30315035324817E-5,1.3836372849781E-5,
1.40464197777495E-5,1.54597749564638E-5,1.62073588704067E-5,1.92092968712444E-5,
1.95234416882552E-5,2.37637844577596E-5,2.61487188977255E-5),
 .UNSPECIFIED.);
#25426=B_SPLINE_CURVE_WITH_KNOTS('',3,(#395134,#395135,#395136,#395137,
#395138,#395139,#395140,#395141,#395142,#395143,#395144,#395145,#395146,
#395147,#395148,#395149,#395150,#395151,#395152,#395153,#395154,#395155,
#395156,#395157,#395158,#395159,#395160,#395161,#395162,#395163,#395164),
 .UNSPECIFIED.,.F.,.F.,(4,3,3,3,3,3,3,3,3,3,4),(0.,3.95507910398509E-6,
7.53768426604194E-6,1.19904533335351E-5,1.40475043392585E-5,1.51452104275963E-5,
1.67866272814167E-5,1.69621513005357E-5,1.81338315460711E-5,1.98906334656521E-5,
2.06132424588243E-5),.UNSPECIFIED.);
#25427=B_SPLINE_CURVE_WITH_KNOTS('',3,(#395167,#395168,#395169,#395170),
 .UNSPECIFIED.,.F.,.F.,(4,4),(4.33680868994202E-19,0.00010938435327491),
 .UNSPECIFIED.);
#25428=B_SPLINE_CURVE_WITH_KNOTS('',3,(#395197,#395198,#395199,#395200,
#395201,#395202,#395203,#395204,#395205,#395206,#395207,#395208,#395209,
#395210,#395211,#395212,#395213,#395214,#395215,#395216,#395217,#395218,
#395219,#395220,#395221,#395222,#395223,#395224,#395225,#395226,#395227,
#395228,#395229,#395230),.UNSPECIFIED.,.F.,.F.,(4,3,3,3,3,3,3,3,3,3,3,4),
(2.16840434497101E-19,2.09623992729456E-6,3.17176647120226E-6,4.8263618194516E-6,
5.01000917339959E-6,6.13126454147491E-6,8.60486650288858E-6,9.21144281170482E-6,
1.24722301135962E-5,1.42666454787854E-5,2.04670653756933E-5,2.08026438176799E-5),
 .UNSPECIFIED.);
#25429=B_SPLINE_CURVE_WITH_KNOTS('',3,(#395231,#395232,#395233,#395234),
 .UNSPECIFIED.,.F.,.F.,(4,4),(0.,0.000109384345496908),.UNSPECIFIED.);
#25430=B_SPLINE_CURVE_WITH_KNOTS('',3,(#395339,#395340,#395341,#395342),
 .UNSPECIFIED.,.F.,.F.,(4,4),(0.,9.54361881492173E-5),.UNSPECIFIED.);
#25431=B_SPLINE_CURVE_WITH_KNOTS('',3,(#395347,#395348,#395349,#395350,
#395351,#395352,#395353),.UNSPECIFIED.,.F.,.F.,(4,3,4),(0.,4.41069704323469E-5,
0.000113970027818833),.UNSPECIFIED.);
#25432=B_SPLINE_CURVE_WITH_KNOTS('',3,(#395359,#395360,#395361,#395362),
 .UNSPECIFIED.,.F.,.F.,(4,4),(4.47028007668187E-19,9.54361881492177E-5),
 .UNSPECIFIED.);
#25433=B_SPLINE_CURVE_WITH_KNOTS('',3,(#395366,#395367,#395368,#395369,
#395370,#395371,#395372),.UNSPECIFIED.,.F.,.F.,(4,3,4),(0.,6.98630244191491E-5,
0.000113969974038089),.UNSPECIFIED.);
#25434=B_SPLINE_CURVE_WITH_KNOTS('',3,(#395375,#395376,#395377,#395378,
#395379,#395380,#395381,#395382,#395383,#395384,#395385,#395386,#395387,
#395388,#395389,#395390,#395391,#395392,#395393,#395394,#395395,#395396,
#395397,#395398,#395399,#395400,#395401,#395402,#395403,#395404,#395405,
#395406,#395407,#395408,#395409,#395410,#395411,#395412,#395413,#395414,
#395415,#395416,#395417,#395418,#395419,#395420,#395421,#395422,#395423),
 .UNSPECIFIED.,.F.,.F.,(4,3,3,3,3,3,3,3,3,3,3,3,3,3,3,3,4),(0.,1.5310029937341E-6,
4.52554775678762E-6,7.01151246291603E-6,9.26752933800599E-6,1.03084066197174E-5,
1.1713899082686E-5,1.22284894984073E-5,1.30315035324818E-5,1.38363728497812E-5,
1.40464197777493E-5,1.54597749564638E-5,1.62073588704067E-5,1.92092968712513E-5,
1.95234416882552E-5,2.37637844577644E-5,2.61487188977255E-5),
 .UNSPECIFIED.);
#25435=B_SPLINE_CURVE_WITH_KNOTS('',3,(#395438,#395439,#395440,#395441,
#395442,#395443,#395444,#395445,#395446,#395447,#395448,#395449,#395450,
#395451,#395452,#395453,#395454,#395455,#395456,#395457,#395458,#395459,
#395460,#395461,#395462,#395463,#395464,#395465,#395466,#395467,#395468),
 .UNSPECIFIED.,.F.,.F.,(4,3,3,3,3,3,3,3,3,3,4),(0.,3.95507910398144E-6,
7.53768426604199E-6,1.1990453333535E-5,1.40475043392586E-5,1.51452104275965E-5,
1.67866272814099E-5,1.69621513005358E-5,1.81338315460712E-5,1.98906334656528E-5,
2.06132424588245E-5),.UNSPECIFIED.);
#25436=B_SPLINE_CURVE_WITH_KNOTS('',3,(#395471,#395472,#395473,#395474),
 .UNSPECIFIED.,.F.,.F.,(4,4),(4.47028007668187E-19,0.00010938435327491),
 .UNSPECIFIED.);
#25437=B_SPLINE_CURVE_WITH_KNOTS('',3,(#395501,#395502,#395503,#395504,
#395505,#395506,#395507,#395508,#395509,#395510,#395511,#395512,#395513,
#395514,#395515,#395516,#395517,#395518,#395519,#395520,#395521,#395522,
#395523,#395524,#395525,#395526,#395527,#395528,#395529,#395530,#395531,
#395532,#395533,#395534),.UNSPECIFIED.,.F.,.F.,(4,3,3,3,3,3,3,3,3,3,3,4),
(0.,2.09623992729446E-6,3.17176647120222E-6,4.82636181943375E-6,5.0100091733998E-6,
6.13126454147495E-6,8.60486650288865E-6,9.21144281170494E-6,1.24722301135964E-5,
1.42666454787856E-5,2.04670653757012E-5,2.08026438176803E-5),
 .UNSPECIFIED.);
#25438=B_SPLINE_CURVE_WITH_KNOTS('',3,(#395535,#395536,#395537,#395538),
 .UNSPECIFIED.,.F.,.F.,(4,4),(0.,0.000109384345496908),.UNSPECIFIED.);
#25439=B_SPLINE_CURVE_WITH_KNOTS('',3,(#395643,#395644,#395645,#395646),
 .UNSPECIFIED.,.F.,.F.,(4,4),(0.,9.54361881492173E-5),.UNSPECIFIED.);
#25440=B_SPLINE_CURVE_WITH_KNOTS('',3,(#395651,#395652,#395653,#395654,
#395655,#395656,#395657),.UNSPECIFIED.,.F.,.F.,(4,3,4),(0.,4.41069704323467E-5,
0.000113970027818833),.UNSPECIFIED.);
#25441=B_SPLINE_CURVE_WITH_KNOTS('',3,(#395663,#395664,#395665,#395666),
 .UNSPECIFIED.,.F.,.F.,(4,4),(4.33680868994202E-19,9.5436188149218E-5),
 .UNSPECIFIED.);
#25442=B_SPLINE_CURVE_WITH_KNOTS('',3,(#395670,#395671,#395672,#395673,
#395674,#395675,#395676),.UNSPECIFIED.,.F.,.F.,(4,3,4),(0.,6.98630244191495E-5,
0.000113969974038089),.UNSPECIFIED.);
#25443=B_SPLINE_CURVE_WITH_KNOTS('',3,(#395679,#395680,#395681,#395682,
#395683,#395684,#395685,#395686,#395687,#395688,#395689,#395690,#395691,
#395692,#395693,#395694,#395695,#395696,#395697,#395698,#395699,#395700,
#395701,#395702,#395703,#395704,#395705,#395706,#395707,#395708,#395709,
#395710,#395711,#395712,#395713,#395714,#395715,#395716,#395717,#395718,
#395719,#395720,#395721,#395722,#395723,#395724,#395725,#395726,#395727),
 .UNSPECIFIED.,.F.,.F.,(4,3,3,3,3,3,3,3,3,3,3,3,3,3,3,3,4),(0.,1.53100299373412E-6,
4.52554775679016E-6,7.01151246291591E-6,9.26752933800179E-6,1.03084066197171E-5,
1.17138990826861E-5,1.22284894984074E-5,1.30315035324818E-5,1.38363728497813E-5,
1.40464197777495E-5,1.54597749564641E-5,1.62073588704071E-5,1.92092968712855E-5,
1.95234416882559E-5,2.37637844577606E-5,2.6148718897727E-5),
 .UNSPECIFIED.);
#25444=B_SPLINE_CURVE_WITH_KNOTS('',3,(#395742,#395743,#395744,#395745,
#395746,#395747,#395748,#395749,#395750,#395751,#395752,#395753,#395754,
#395755,#395756,#395757,#395758,#395759,#395760,#395761,#395762,#395763,
#395764,#395765,#395766,#395767,#395768,#395769,#395770,#395771,#395772),
 .UNSPECIFIED.,.F.,.F.,(4,3,3,3,3,3,3,3,3,3,4),(0.,3.95507910397768E-6,
7.53768426604198E-6,1.19904533335351E-5,1.40475043392586E-5,1.51452104275964E-5,
1.67866272814183E-5,1.69621513005358E-5,1.81338315460711E-5,1.98906334656542E-5,
2.06132424588245E-5),.UNSPECIFIED.);
#25445=B_SPLINE_CURVE_WITH_KNOTS('',3,(#395775,#395776,#395777,#395778),
 .UNSPECIFIED.,.F.,.F.,(4,4),(4.47028007668187E-19,0.00010938435327491),
 .UNSPECIFIED.);
#25446=B_SPLINE_CURVE_WITH_KNOTS('',3,(#395805,#395806,#395807,#395808,
#395809,#395810,#395811,#395812,#395813,#395814,#395815,#395816,#395817,
#395818,#395819,#395820,#395821,#395822,#395823,#395824,#395825,#395826,
#395827,#395828,#395829,#395830,#395831,#395832,#395833,#395834,#395835,
#395836,#395837,#395838),.UNSPECIFIED.,.F.,.F.,(4,3,3,3,3,3,3,3,3,3,3,4),
(1.0842021724855E-19,2.09623992729441E-6,3.17176647120226E-6,4.82636181944059E-6,
5.01000917339961E-6,6.13126454147497E-6,8.60486650288839E-6,9.21144281170474E-6,
1.24722301136207E-5,1.4266645478785E-5,2.04670653756626E-5,2.08026438176791E-5),
 .UNSPECIFIED.);
#25447=B_SPLINE_CURVE_WITH_KNOTS('',3,(#395839,#395840,#395841,#395842),
 .UNSPECIFIED.,.F.,.F.,(4,4),(0.,0.000109384345496908),.UNSPECIFIED.);
#25448=B_SPLINE_CURVE_WITH_KNOTS('',3,(#395947,#395948,#395949,#395950),
 .UNSPECIFIED.,.F.,.F.,(4,4),(0.,9.54361881492178E-5),.UNSPECIFIED.);
#25449=B_SPLINE_CURVE_WITH_KNOTS('',3,(#395955,#395956,#395957,#395958,
#395959,#395960,#395961),.UNSPECIFIED.,.F.,.F.,(4,3,4),(0.,4.41069704323469E-5,
0.000113970027818833),.UNSPECIFIED.);
#25450=B_SPLINE_CURVE_WITH_KNOTS('',3,(#395967,#395968,#395969,#395970),
 .UNSPECIFIED.,.F.,.F.,(4,4),(4.47028007668187E-19,9.54361881492176E-5),
 .UNSPECIFIED.);
#25451=B_SPLINE_CURVE_WITH_KNOTS('',3,(#395974,#395975,#395976,#395977,
#395978,#395979,#395980),.UNSPECIFIED.,.F.,.F.,(4,3,4),(0.,6.98630244191491E-5,
0.000113969974038089),.UNSPECIFIED.);
#25452=B_SPLINE_CURVE_WITH_KNOTS('',3,(#395983,#395984,#395985,#395986,
#395987,#395988,#395989,#395990,#395991,#395992,#395993,#395994,#395995,
#395996,#395997,#395998,#395999,#396000,#396001,#396002,#396003,#396004,
#396005,#396006,#396007,#396008,#396009,#396010,#396011,#396012,#396013,
#396014,#396015,#396016,#396017,#396018,#396019,#396020,#396021,#396022,
#396023,#396024,#396025,#396026,#396027,#396028,#396029,#396030,#396031),
 .UNSPECIFIED.,.F.,.F.,(4,3,3,3,3,3,3,3,3,3,3,3,3,3,3,3,4),(0.,1.53100299373409E-6,
4.52554775678942E-6,7.01151246291605E-6,9.26752933799663E-6,1.03084066197173E-5,
1.17138990826864E-5,1.22284894984076E-5,1.30315035324818E-5,1.38363728497813E-5,
1.40464197777496E-5,1.5459774956464E-5,1.62073588704069E-5,1.92092968712812E-5,
1.95234416882555E-5,2.3763784457762E-5,2.61487188977261E-5),
 .UNSPECIFIED.);
#25453=B_SPLINE_CURVE_WITH_KNOTS('',3,(#396046,#396047,#396048,#396049,
#396050,#396051,#396052,#396053,#396054,#396055,#396056,#396057,#396058,
#396059,#396060,#396061,#396062,#396063,#396064,#396065,#396066,#396067,
#396068,#396069,#396070,#396071,#396072,#396073,#396074,#396075,#396076),
 .UNSPECIFIED.,.F.,.F.,(4,3,3,3,3,3,3,3,3,3,4),(0.,3.95507910397385E-6,
7.53768426604199E-6,1.19904533335351E-5,1.40475043392587E-5,1.51452104275965E-5,
1.67866272814042E-5,1.69621513005359E-5,1.81338315460712E-5,1.98906334656544E-5,
2.06132424588247E-5),.UNSPECIFIED.);
#25454=B_SPLINE_CURVE_WITH_KNOTS('',3,(#396079,#396080,#396081,#396082),
 .UNSPECIFIED.,.F.,.F.,(4,4),(4.47028007668187E-19,0.00010938435327491),
 .UNSPECIFIED.);
#25455=B_SPLINE_CURVE_WITH_KNOTS('',3,(#396109,#396110,#396111,#396112,
#396113,#396114,#396115,#396116,#396117,#396118,#396119,#396120,#396121,
#396122,#396123,#396124,#396125,#396126,#396127,#396128,#396129,#396130,
#396131,#396132,#396133,#396134,#396135,#396136,#396137,#396138,#396139,
#396140,#396141,#396142),.UNSPECIFIED.,.F.,.F.,(4,3,3,3,3,3,3,3,3,3,3,4),
(1.0842021724855E-19,2.09623992729443E-6,3.17176647120216E-6,4.82636181943593E-6,
5.01000917339959E-6,6.13126454147479E-6,8.60486650288851E-6,9.21144281170492E-6,
1.24722301136026E-5,1.42666454787855E-5,2.04670653756902E-5,2.08026438176802E-5),
 .UNSPECIFIED.);
#25456=B_SPLINE_CURVE_WITH_KNOTS('',3,(#396143,#396144,#396145,#396146),
 .UNSPECIFIED.,.F.,.F.,(4,4),(0.,0.000109384345496908),.UNSPECIFIED.);
#25457=B_SPLINE_CURVE_WITH_KNOTS('',3,(#396251,#396252,#396253,#396254),
 .UNSPECIFIED.,.F.,.F.,(4,4),(0.,9.54361881492174E-5),.UNSPECIFIED.);
#25458=B_SPLINE_CURVE_WITH_KNOTS('',3,(#396259,#396260,#396261,#396262,
#396263,#396264,#396265),.UNSPECIFIED.,.F.,.F.,(4,3,4),(0.,4.41069704323467E-5,
0.000113970027818833),.UNSPECIFIED.);
#25459=B_SPLINE_CURVE_WITH_KNOTS('',3,(#396271,#396272,#396273,#396274),
 .UNSPECIFIED.,.F.,.F.,(4,4),(4.47028007668187E-19,9.54361881492181E-5),
 .UNSPECIFIED.);
#25460=B_SPLINE_CURVE_WITH_KNOTS('',3,(#396278,#396279,#396280,#396281,
#396282,#396283,#396284),.UNSPECIFIED.,.F.,.F.,(4,3,4),(0.,6.98630244191495E-5,
0.000113969974038089),.UNSPECIFIED.);
#25461=B_SPLINE_CURVE_WITH_KNOTS('',3,(#396287,#396288,#396289,#396290,
#396291,#396292,#396293,#396294,#396295,#396296,#396297,#396298,#396299,
#396300,#396301,#396302,#396303,#396304,#396305,#396306,#396307,#396308,
#396309,#396310,#396311,#396312,#396313,#396314,#396315,#396316,#396317,
#396318,#396319,#396320,#396321,#396322,#396323,#396324,#396325,#396326,
#396327,#396328,#396329,#396330,#396331,#396332,#396333,#396334,#396335),
 .UNSPECIFIED.,.F.,.F.,(4,3,3,3,3,3,3,3,3,3,3,3,3,3,3,3,4),(0.,1.53100299373397E-6,
4.52554775678549E-6,7.01151246291585E-6,9.26752933799876E-6,1.03084066197172E-5,
1.17138990826861E-5,1.22284894984074E-5,1.30315035324817E-5,1.38363728497813E-5,
1.40464197777495E-5,1.54597749564641E-5,1.6207358870407E-5,1.92092968712915E-5,
1.95234416882557E-5,2.37637844577633E-5,2.61487188977267E-5),
 .UNSPECIFIED.);
#25462=B_SPLINE_CURVE_WITH_KNOTS('',3,(#396350,#396351,#396352,#396353,
#396354,#396355,#396356,#396357,#396358,#396359,#396360,#396361,#396362,
#396363,#396364,#396365,#396366,#396367,#396368,#396369,#396370,#396371,
#396372,#396373,#396374,#396375,#396376,#396377,#396378,#396379,#396380),
 .UNSPECIFIED.,.F.,.F.,(4,3,3,3,3,3,3,3,3,3,4),(0.,3.95507910397337E-6,
7.53768426604201E-6,1.1990453333535E-5,1.40475043392586E-5,1.51452104275964E-5,
1.67866272814123E-5,1.69621513005357E-5,1.81338315460711E-5,1.98906334656556E-5,
2.06132424588244E-5),.UNSPECIFIED.);
#25463=B_SPLINE_CURVE_WITH_KNOTS('',3,(#396383,#396384,#396385,#396386),
 .UNSPECIFIED.,.F.,.F.,(4,4),(4.63171371119878E-19,0.00010938435327491),
 .UNSPECIFIED.);
#25464=B_SPLINE_CURVE_WITH_KNOTS('',3,(#396413,#396414,#396415,#396416,
#396417,#396418,#396419,#396420,#396421,#396422,#396423,#396424,#396425,
#396426,#396427,#396428,#396429,#396430,#396431,#396432,#396433,#396434,
#396435,#396436,#396437,#396438,#396439,#396440,#396441,#396442,#396443,
#396444,#396445,#396446),.UNSPECIFIED.,.F.,.F.,(4,3,3,3,3,3,3,3,3,3,3,4),
(1.62630325872826E-19,2.0962399272944E-6,3.17176647120221E-6,4.8263618194282E-6,
5.01000917339958E-6,6.1312645414749E-6,8.60486650288834E-6,9.21144281170484E-6,
1.24722301135973E-5,1.42666454787854E-5,2.04670653756913E-5,2.080264381768E-5),
 .UNSPECIFIED.);
#25465=B_SPLINE_CURVE_WITH_KNOTS('',3,(#396447,#396448,#396449,#396450),
 .UNSPECIFIED.,.F.,.F.,(4,4),(0.,0.000109384345496908),.UNSPECIFIED.);
#25466=B_SPLINE_CURVE_WITH_KNOTS('',3,(#396555,#396556,#396557,#396558),
 .UNSPECIFIED.,.F.,.F.,(4,4),(0.,9.54361881492176E-5),.UNSPECIFIED.);
#25467=B_SPLINE_CURVE_WITH_KNOTS('',3,(#396563,#396564,#396565,#396566,
#396567,#396568,#396569),.UNSPECIFIED.,.F.,.F.,(4,3,4),(0.,4.4106970432347E-5,
0.000113970027818834),.UNSPECIFIED.);
#25468=B_SPLINE_CURVE_WITH_KNOTS('',3,(#396575,#396576,#396577,#396578),
 .UNSPECIFIED.,.F.,.F.,(4,4),(4.47028007668187E-19,9.54361881492177E-5),
 .UNSPECIFIED.);
#25469=B_SPLINE_CURVE_WITH_KNOTS('',3,(#396582,#396583,#396584,#396585,
#396586,#396587,#396588),.UNSPECIFIED.,.F.,.F.,(4,3,4),(0.,6.98630244191489E-5,
0.000113969974038089),.UNSPECIFIED.);
#25470=B_SPLINE_CURVE_WITH_KNOTS('',3,(#396591,#396592,#396593,#396594,
#396595,#396596,#396597,#396598,#396599,#396600,#396601,#396602,#396603,
#396604,#396605,#396606,#396607,#396608,#396609,#396610,#396611,#396612,
#396613,#396614,#396615,#396616,#396617,#396618,#396619,#396620,#396621,
#396622,#396623,#396624,#396625,#396626,#396627,#396628,#396629,#396630,
#396631,#396632,#396633,#396634,#396635,#396636,#396637,#396638,#396639),
 .UNSPECIFIED.,.F.,.F.,(4,3,3,3,3,3,3,3,3,3,3,3,3,3,3,3,4),(0.,1.53100299373419E-6,
4.52554775679508E-6,7.01151246291607E-6,9.26752933799554E-6,1.03084066197173E-5,
1.17138990826862E-5,1.22284894984074E-5,1.30315035324817E-5,1.38363728497813E-5,
1.40464197777495E-5,1.54597749564641E-5,1.6207358870407E-5,1.92092968713182E-5,
1.95234416882557E-5,2.37637844577564E-5,2.61487188977266E-5),
 .UNSPECIFIED.);
#25471=B_SPLINE_CURVE_WITH_KNOTS('',3,(#396654,#396655,#396656,#396657,
#396658,#396659,#396660,#396661,#396662,#396663,#396664,#396665,#396666,
#396667,#396668,#396669,#396670,#396671,#396672,#396673,#396674,#396675,
#396676,#396677,#396678,#396679,#396680,#396681,#396682,#396683,#396684),
 .UNSPECIFIED.,.F.,.F.,(4,3,3,3,3,3,3,3,3,3,4),(0.,3.95507910399129E-6,
7.53768426604195E-6,1.19904533335351E-5,1.40475043392585E-5,1.51452104275963E-5,
1.67866272814177E-5,1.69621513005356E-5,1.81338315460709E-5,1.98906334656484E-5,
2.0613242458824E-5),.UNSPECIFIED.);
#25472=B_SPLINE_CURVE_WITH_KNOTS('',3,(#396687,#396688,#396689,#396690),
 .UNSPECIFIED.,.F.,.F.,(4,4),(4.63171371119878E-19,0.00010938435327491),
 .UNSPECIFIED.);
#25473=B_SPLINE_CURVE_WITH_KNOTS('',3,(#396717,#396718,#396719,#396720,
#396721,#396722,#396723,#396724,#396725,#396726,#396727,#396728,#396729,
#396730,#396731,#396732,#396733,#396734,#396735,#396736,#396737,#396738,
#396739,#396740,#396741,#396742,#396743,#396744,#396745,#396746,#396747,
#396748,#396749,#396750),.UNSPECIFIED.,.F.,.F.,(4,3,3,3,3,3,3,3,3,3,3,4),
(1.62630325872826E-19,2.09623992729438E-6,3.17176647120219E-6,4.82636181942821E-6,
5.01000917339952E-6,6.13126454147489E-6,8.6048665028884E-6,9.21144281170481E-6,
1.24722301135895E-5,1.42666454787855E-5,2.04670653756765E-5,2.080264381768E-5),
 .UNSPECIFIED.);
#25474=B_SPLINE_CURVE_WITH_KNOTS('',3,(#396751,#396752,#396753,#396754),
 .UNSPECIFIED.,.F.,.F.,(4,4),(0.,0.000109384345496908),.UNSPECIFIED.);
#25475=B_SPLINE_CURVE_WITH_KNOTS('',3,(#396859,#396860,#396861,#396862),
 .UNSPECIFIED.,.F.,.F.,(4,4),(0.,9.54361881492173E-5),.UNSPECIFIED.);
#25476=B_SPLINE_CURVE_WITH_KNOTS('',3,(#396867,#396868,#396869,#396870,
#396871,#396872,#396873),.UNSPECIFIED.,.F.,.F.,(4,3,4),(0.,4.41069704323472E-5,
0.000113970027818834),.UNSPECIFIED.);
#25477=B_SPLINE_CURVE_WITH_KNOTS('',3,(#396879,#396880,#396881,#396882),
 .UNSPECIFIED.,.F.,.F.,(4,4),(4.48719651148014E-19,9.54361881492176E-5),
 .UNSPECIFIED.);
#25478=B_SPLINE_CURVE_WITH_KNOTS('',3,(#396886,#396887,#396888,#396889,
#396890,#396891,#396892),.UNSPECIFIED.,.F.,.F.,(4,3,4),(0.,6.98630244191491E-5,
0.000113969974038089),.UNSPECIFIED.);
#25479=B_SPLINE_CURVE_WITH_KNOTS('',3,(#396895,#396896,#396897,#396898,
#396899,#396900,#396901,#396902,#396903,#396904,#396905,#396906,#396907,
#396908,#396909,#396910,#396911,#396912,#396913,#396914,#396915,#396916,
#396917,#396918,#396919,#396920,#396921,#396922,#396923,#396924,#396925,
#396926,#396927,#396928,#396929,#396930,#396931,#396932,#396933,#396934,
#396935,#396936,#396937,#396938,#396939,#396940,#396941,#396942,#396943),
 .UNSPECIFIED.,.F.,.F.,(4,3,3,3,3,3,3,3,3,3,3,3,3,3,3,3,4),(0.,1.53100299373413E-6,
4.52554775679464E-6,7.01151246291609E-6,9.26752933800805E-6,1.03084066197173E-5,
1.17138990826862E-5,1.22284894984074E-5,1.30315035324817E-5,1.38363728497812E-5,
1.40464197777494E-5,1.54597749564639E-5,1.62073588704068E-5,1.92092968713364E-5,
1.95234416882556E-5,2.37637844577523E-5,2.61487188977263E-5),
 .UNSPECIFIED.);
#25480=B_SPLINE_CURVE_WITH_KNOTS('',3,(#396958,#396959,#396960,#396961,
#396962,#396963,#396964,#396965,#396966,#396967,#396968,#396969,#396970,
#396971,#396972,#396973,#396974,#396975,#396976,#396977,#396978,#396979,
#396980,#396981,#396982,#396983,#396984,#396985,#396986,#396987,#396988),
 .UNSPECIFIED.,.F.,.F.,(4,3,3,3,3,3,3,3,3,3,4),(0.,3.95507910397758E-6,
7.53768426604201E-6,1.1990453333535E-5,1.40475043392586E-5,1.51452104275964E-5,
1.67866272814164E-5,1.69621513005358E-5,1.81338315460713E-5,1.98906334656549E-5,
2.06132424588247E-5),.UNSPECIFIED.);
#25481=B_SPLINE_CURVE_WITH_KNOTS('',3,(#396991,#396992,#396993,#396994),
 .UNSPECIFIED.,.F.,.F.,(4,4),(4.73369422993816E-19,0.00010938435327491),
 .UNSPECIFIED.);
#25482=B_SPLINE_CURVE_WITH_KNOTS('',3,(#397021,#397022,#397023,#397024,
#397025,#397026,#397027,#397028,#397029,#397030,#397031,#397032,#397033,
#397034,#397035,#397036,#397037,#397038,#397039,#397040,#397041,#397042,
#397043,#397044,#397045,#397046,#397047,#397048,#397049,#397050,#397051,
#397052,#397053,#397054),.UNSPECIFIED.,.F.,.F.,(4,3,3,3,3,3,3,3,3,3,3,4),
(1.62630325872826E-19,2.09623992729438E-6,3.1717664712022E-6,4.82636181943908E-6,
5.01000917339962E-6,6.13126454147497E-6,8.60486650288859E-6,9.21144281170501E-6,
1.24722301136026E-5,1.42666454787856E-5,2.04670653756757E-5,2.08026438176802E-5),
 .UNSPECIFIED.);
#25483=B_SPLINE_CURVE_WITH_KNOTS('',3,(#397055,#397056,#397057,#397058),
 .UNSPECIFIED.,.F.,.F.,(4,4),(0.,0.000109384345496908),.UNSPECIFIED.);
#25484=B_SPLINE_CURVE_WITH_KNOTS('',3,(#397163,#397164,#397165,#397166),
 .UNSPECIFIED.,.F.,.F.,(4,4),(0.,9.54361881492177E-5),.UNSPECIFIED.);
#25485=B_SPLINE_CURVE_WITH_KNOTS('',3,(#397171,#397172,#397173,#397174,
#397175,#397176,#397177),.UNSPECIFIED.,.F.,.F.,(4,3,4),(0.,4.41069704323469E-5,
0.000113970027818834),.UNSPECIFIED.);
#25486=B_SPLINE_CURVE_WITH_KNOTS('',3,(#397183,#397184,#397185,#397186),
 .UNSPECIFIED.,.F.,.F.,(4,4),(4.5436350575631E-19,9.54361881492179E-5),
 .UNSPECIFIED.);
#25487=B_SPLINE_CURVE_WITH_KNOTS('',3,(#397190,#397191,#397192,#397193,
#397194,#397195,#397196),.UNSPECIFIED.,.F.,.F.,(4,3,4),(0.,6.9863024419149E-5,
0.000113969974038089),.UNSPECIFIED.);
#25488=B_SPLINE_CURVE_WITH_KNOTS('',3,(#397199,#397200,#397201,#397202,
#397203,#397204,#397205,#397206,#397207,#397208,#397209,#397210,#397211,
#397212,#397213,#397214,#397215,#397216,#397217,#397218,#397219,#397220,
#397221,#397222,#397223,#397224,#397225,#397226,#397227,#397228,#397229,
#397230,#397231,#397232,#397233,#397234,#397235,#397236,#397237,#397238,
#397239,#397240,#397241,#397242,#397243,#397244,#397245,#397246,#397247),
 .UNSPECIFIED.,.F.,.F.,(4,3,3,3,3,3,3,3,3,3,3,3,3,3,3,3,4),(0.,1.5310029937341E-6,
4.52554775679536E-6,7.01151246291598E-6,9.26752933800322E-6,1.03084066197173E-5,
1.17138990826861E-5,1.22284894984075E-5,1.30315035324817E-5,1.38363728497813E-5,
1.40464197777495E-5,1.54597749564641E-5,1.62073588704069E-5,1.920929687127E-5,
1.95234416882555E-5,2.37637844577578E-5,2.61487188977261E-5),
 .UNSPECIFIED.);
#25489=B_SPLINE_CURVE_WITH_KNOTS('',3,(#397262,#397263,#397264,#397265,
#397266,#397267,#397268,#397269,#397270,#397271,#397272,#397273,#397274,
#397275,#397276,#397277,#397278,#397279,#397280,#397281,#397282,#397283,
#397284,#397285,#397286,#397287,#397288,#397289,#397290,#397291,#397292),
 .UNSPECIFIED.,.F.,.F.,(4,3,3,3,3,3,3,3,3,3,4),(0.,3.95507910396965E-6,
7.53768426604205E-6,1.1990453333535E-5,1.40475043392585E-5,1.51452104275965E-5,
1.6786627281402E-5,1.69621513005358E-5,1.81338315460712E-5,1.98906334656539E-5,
2.06132424588244E-5),.UNSPECIFIED.);
#25490=B_SPLINE_CURVE_WITH_KNOTS('',3,(#397295,#397296,#397297,#397298),
 .UNSPECIFIED.,.F.,.F.,(4,4),(4.84869951806108E-19,0.00010938435327491),
 .UNSPECIFIED.);
#25491=B_SPLINE_CURVE_WITH_KNOTS('',3,(#397325,#397326,#397327,#397328,
#397329,#397330,#397331,#397332,#397333,#397334,#397335,#397336,#397337,
#397338,#397339,#397340,#397341,#397342,#397343,#397344,#397345,#397346,
#397347,#397348,#397349,#397350,#397351,#397352,#397353,#397354,#397355,
#397356,#397357,#397358),.UNSPECIFIED.,.F.,.F.,(4,3,3,3,3,3,3,3,3,3,3,4),
(1.35525271560688E-19,2.09623992729433E-6,3.17176647120218E-6,4.82636181943005E-6,
5.01000917339954E-6,6.13126454147485E-6,8.60486650288841E-6,9.21144281170475E-6,
1.24722301135837E-5,1.42666454787852E-5,2.0467065375683E-5,2.08026438176799E-5),
 .UNSPECIFIED.);
#25492=B_SPLINE_CURVE_WITH_KNOTS('',3,(#397359,#397360,#397361,#397362),
 .UNSPECIFIED.,.F.,.F.,(4,4),(0.,0.000109384345496908),.UNSPECIFIED.);
#25493=B_SPLINE_CURVE_WITH_KNOTS('',3,(#397467,#397468,#397469,#397470),
 .UNSPECIFIED.,.F.,.F.,(4,4),(0.,9.54361881492175E-5),.UNSPECIFIED.);
#25494=B_SPLINE_CURVE_WITH_KNOTS('',3,(#397475,#397476,#397477,#397478,
#397479,#397480,#397481),.UNSPECIFIED.,.F.,.F.,(4,3,4),(0.,4.41069704323468E-5,
0.000113970027818833),.UNSPECIFIED.);
#25495=B_SPLINE_CURVE_WITH_KNOTS('',3,(#397487,#397488,#397489,#397490),
 .UNSPECIFIED.,.F.,.F.,(4,4),(4.63171371119878E-19,9.54361881492178E-5),
 .UNSPECIFIED.);
#25496=B_SPLINE_CURVE_WITH_KNOTS('',3,(#397494,#397495,#397496,#397497,
#397498,#397499,#397500),.UNSPECIFIED.,.F.,.F.,(4,3,4),(0.,6.9863024419149E-5,
0.000113969974038089),.UNSPECIFIED.);
#25497=B_SPLINE_CURVE_WITH_KNOTS('',3,(#397503,#397504,#397505,#397506,
#397507,#397508,#397509,#397510,#397511,#397512,#397513,#397514,#397515,
#397516,#397517,#397518,#397519,#397520,#397521,#397522,#397523,#397524,
#397525,#397526,#397527,#397528,#397529,#397530,#397531,#397532,#397533,
#397534,#397535,#397536,#397537,#397538,#397539,#397540,#397541,#397542,
#397543,#397544,#397545,#397546,#397547,#397548,#397549,#397550,#397551),
 .UNSPECIFIED.,.F.,.F.,(4,3,3,3,3,3,3,3,3,3,3,3,3,3,3,3,4),(0.,1.53100299373415E-6,
4.52554775679159E-6,7.01151246291606E-6,9.26752933801246E-6,1.03084066197173E-5,
1.17138990826861E-5,1.22284894984075E-5,1.30315035324817E-5,1.38363728497813E-5,
1.40464197777495E-5,1.54597749564642E-5,1.62073588704069E-5,1.9209296871264E-5,
1.95234416882557E-5,2.37637844577547E-5,2.61487188977263E-5),
 .UNSPECIFIED.);
#25498=B_SPLINE_CURVE_WITH_KNOTS('',3,(#397566,#397567,#397568,#397569,
#397570,#397571,#397572,#397573,#397574,#397575,#397576,#397577,#397578,
#397579,#397580,#397581,#397582,#397583,#397584,#397585,#397586,#397587,
#397588,#397589,#397590,#397591,#397592,#397593,#397594,#397595,#397596),
 .UNSPECIFIED.,.F.,.F.,(4,3,3,3,3,3,3,3,3,3,4),(0.,3.95507910398452E-6,
7.53768426604194E-6,1.1990453333535E-5,1.40475043392585E-5,1.51452104275964E-5,
1.67866272814187E-5,1.69621513005358E-5,1.81338315460712E-5,1.98906334656524E-5,
2.06132424588246E-5),.UNSPECIFIED.);
#25499=B_SPLINE_CURVE_WITH_KNOTS('',3,(#397599,#397600,#397601,#397602),
 .UNSPECIFIED.,.F.,.F.,(4,4),(5.11417141928151E-19,0.00010938435327491),
 .UNSPECIFIED.);
#25500=B_SPLINE_CURVE_WITH_KNOTS('',3,(#397629,#397630,#397631,#397632,
#397633,#397634,#397635,#397636,#397637,#397638,#397639,#397640,#397641,
#397642,#397643,#397644,#397645,#397646,#397647,#397648,#397649,#397650,
#397651,#397652,#397653,#397654,#397655,#397656,#397657,#397658,#397659,
#397660,#397661,#397662),.UNSPECIFIED.,.F.,.F.,(4,3,3,3,3,3,3,3,3,3,3,4),
(1.0842021724855E-19,2.09623992729446E-6,3.17176647120224E-6,4.8263618194523E-6,
5.01000917339966E-6,6.13126454147504E-6,8.60486650288861E-6,9.21144281170498E-6,
1.24722301135833E-5,1.42666454787858E-5,2.04670653756968E-5,2.08026438176805E-5),
 .UNSPECIFIED.);
#25501=B_SPLINE_CURVE_WITH_KNOTS('',3,(#397663,#397664,#397665,#397666),
 .UNSPECIFIED.,.F.,.F.,(4,4),(0.,0.000109384345496908),.UNSPECIFIED.);
#25502=B_SPLINE_CURVE_WITH_KNOTS('',3,(#397771,#397772,#397773,#397774),
 .UNSPECIFIED.,.F.,.F.,(4,4),(0.,9.54361881492173E-5),.UNSPECIFIED.);
#25503=B_SPLINE_CURVE_WITH_KNOTS('',3,(#397779,#397780,#397781,#397782,
#397783,#397784,#397785),.UNSPECIFIED.,.F.,.F.,(4,3,4),(0.,4.41069704323471E-5,
0.000113970027818833),.UNSPECIFIED.);
#25504=B_SPLINE_CURVE_WITH_KNOTS('',3,(#397791,#397792,#397793,#397794),
 .UNSPECIFIED.,.F.,.F.,(4,4),(4.63171371119878E-19,9.54361881492174E-5),
 .UNSPECIFIED.);
#25505=B_SPLINE_CURVE_WITH_KNOTS('',3,(#397798,#397799,#397800,#397801,
#397802,#397803,#397804),.UNSPECIFIED.,.F.,.F.,(4,3,4),(0.,6.98630244191489E-5,
0.000113969974038089),.UNSPECIFIED.);
#25506=B_SPLINE_CURVE_WITH_KNOTS('',3,(#397807,#397808,#397809,#397810,
#397811,#397812,#397813,#397814,#397815,#397816,#397817,#397818,#397819,
#397820,#397821,#397822,#397823,#397824,#397825,#397826,#397827,#397828,
#397829,#397830,#397831,#397832,#397833,#397834,#397835,#397836,#397837,
#397838,#397839,#397840,#397841,#397842,#397843,#397844,#397845,#397846,
#397847,#397848,#397849,#397850,#397851,#397852,#397853,#397854,#397855),
 .UNSPECIFIED.,.F.,.F.,(4,3,3,3,3,3,3,3,3,3,3,3,3,3,3,3,4),(0.,1.53100299373427E-6,
4.52554775679287E-6,7.01151246291616E-6,9.26752933799541E-6,1.03084066197174E-5,
1.17138990826863E-5,1.22284894984076E-5,1.30315035324818E-5,1.38363728497814E-5,
1.40464197777496E-5,1.54597749564642E-5,1.62073588704071E-5,1.92092968712996E-5,
1.95234416882555E-5,2.376378445776E-5,2.6148718897726E-5),.UNSPECIFIED.);
#25507=B_SPLINE_CURVE_WITH_KNOTS('',3,(#397870,#397871,#397872,#397873,
#397874,#397875,#397876,#397877,#397878,#397879,#397880,#397881,#397882,
#397883,#397884,#397885,#397886,#397887,#397888,#397889,#397890,#397891,
#397892,#397893,#397894,#397895,#397896,#397897,#397898,#397899,#397900),
 .UNSPECIFIED.,.F.,.F.,(4,3,3,3,3,3,3,3,3,3,4),(0.,3.95507910397904E-6,
7.53768426604202E-6,1.19904533335351E-5,1.40475043392587E-5,1.51452104275966E-5,
1.67866272814141E-5,1.6962151300536E-5,1.81338315460713E-5,1.98906334656548E-5,
2.06132424588246E-5),.UNSPECIFIED.);
#25508=B_SPLINE_CURVE_WITH_KNOTS('',3,(#397903,#397904,#397905,#397906),
 .UNSPECIFIED.,.F.,.F.,(4,4),(5.11417141928151E-19,0.00010938435327491),
 .UNSPECIFIED.);
#25509=B_SPLINE_CURVE_WITH_KNOTS('',3,(#397933,#397934,#397935,#397936,
#397937,#397938,#397939,#397940,#397941,#397942,#397943,#397944,#397945,
#397946,#397947,#397948,#397949,#397950,#397951,#397952,#397953,#397954,
#397955,#397956,#397957,#397958,#397959,#397960,#397961,#397962,#397963,
#397964,#397965,#397966),.UNSPECIFIED.,.F.,.F.,(4,3,3,3,3,3,3,3,3,3,3,4),
(1.62630325872826E-19,2.09623992729442E-6,3.17176647120233E-6,4.8263618194495E-6,
5.01000917339967E-6,6.13126454147504E-6,8.60486650288865E-6,9.21144281170504E-6,
1.24722301136077E-5,1.42666454787857E-5,2.04670653756745E-5,2.08026438176805E-5),
 .UNSPECIFIED.);
#25510=B_SPLINE_CURVE_WITH_KNOTS('',3,(#397967,#397968,#397969,#397970),
 .UNSPECIFIED.,.F.,.F.,(4,4),(0.,0.000109384345496908),.UNSPECIFIED.);
#25511=B_SPLINE_CURVE_WITH_KNOTS('',3,(#398075,#398076,#398077,#398078),
 .UNSPECIFIED.,.F.,.F.,(4,4),(0.,9.54361881492172E-5),.UNSPECIFIED.);
#25512=B_SPLINE_CURVE_WITH_KNOTS('',3,(#398083,#398084,#398085,#398086,
#398087,#398088,#398089),.UNSPECIFIED.,.F.,.F.,(4,3,4),(0.,4.4106970432347E-5,
0.000113970027818833),.UNSPECIFIED.);
#25513=B_SPLINE_CURVE_WITH_KNOTS('',3,(#398095,#398096,#398097,#398098),
 .UNSPECIFIED.,.F.,.F.,(4,4),(2.16840434497101E-19,9.54361881492181E-5),
 .UNSPECIFIED.);
#25514=B_SPLINE_CURVE_WITH_KNOTS('',3,(#398102,#398103,#398104,#398105,
#398106,#398107,#398108),.UNSPECIFIED.,.F.,.F.,(4,3,4),(0.,6.98630244191491E-5,
0.000113969974038089),.UNSPECIFIED.);
#25515=B_SPLINE_CURVE_WITH_KNOTS('',3,(#398111,#398112,#398113,#398114,
#398115,#398116,#398117,#398118,#398119,#398120,#398121,#398122,#398123,
#398124,#398125,#398126,#398127,#398128,#398129,#398130,#398131,#398132,
#398133,#398134,#398135,#398136,#398137,#398138,#398139,#398140,#398141,
#398142,#398143,#398144,#398145,#398146,#398147,#398148,#398149,#398150,
#398151,#398152,#398153,#398154,#398155,#398156,#398157,#398158,#398159),
 .UNSPECIFIED.,.F.,.F.,(4,3,3,3,3,3,3,3,3,3,3,3,3,3,3,3,4),(0.,1.53100299373411E-6,
4.52554775679125E-6,7.01151246291595E-6,9.26752933800362E-6,1.03084066197172E-5,
1.17138990826861E-5,1.22284894984074E-5,1.30315035324816E-5,1.3836372849781E-5,
1.40464197777493E-5,1.54597749564638E-5,1.62073588704067E-5,1.9209296871261E-5,
1.95234416882551E-5,2.37637844577578E-5,2.61487188977257E-5),
 .UNSPECIFIED.);
#25516=B_SPLINE_CURVE_WITH_KNOTS('',3,(#398174,#398175,#398176,#398177,
#398178,#398179,#398180,#398181,#398182,#398183,#398184,#398185,#398186,
#398187,#398188,#398189,#398190,#398191,#398192,#398193,#398194,#398195,
#398196,#398197,#398198,#398199,#398200,#398201,#398202,#398203,#398204),
 .UNSPECIFIED.,.F.,.F.,(4,3,3,3,3,3,3,3,3,3,4),(0.,3.95507910398269E-6,
7.53768426604198E-6,1.19904533335351E-5,1.40475043392586E-5,1.51452104275966E-5,
1.67866272814071E-5,1.69621513005359E-5,1.81338315460714E-5,1.98906334656536E-5,
2.06132424588246E-5),.UNSPECIFIED.);
#25517=B_SPLINE_CURVE_WITH_KNOTS('',3,(#398207,#398208,#398209,#398210),
 .UNSPECIFIED.,.F.,.F.,(4,4),(4.84869951806108E-19,0.00010938435327491),
 .UNSPECIFIED.);
#25518=B_SPLINE_CURVE_WITH_KNOTS('',3,(#398237,#398238,#398239,#398240,
#398241,#398242,#398243,#398244,#398245,#398246,#398247,#398248,#398249,
#398250,#398251,#398252,#398253,#398254,#398255,#398256,#398257,#398258,
#398259,#398260,#398261,#398262,#398263,#398264,#398265,#398266,#398267,
#398268,#398269,#398270),.UNSPECIFIED.,.F.,.F.,(4,3,3,3,3,3,3,3,3,3,3,4),
(2.16840434497101E-19,2.09623992729424E-6,3.17176647120196E-6,4.82636181943257E-6,
5.01000917339949E-6,6.1312645414749E-6,8.60486650288852E-6,9.2114428117048E-6,
1.2472230113601E-5,1.42666454787854E-5,2.04670653756909E-5,2.08026438176801E-5),
 .UNSPECIFIED.);
#25519=B_SPLINE_CURVE_WITH_KNOTS('',3,(#398271,#398272,#398273,#398274),
 .UNSPECIFIED.,.F.,.F.,(4,4),(0.,0.000109384345496908),.UNSPECIFIED.);
#25520=B_SPLINE_CURVE_WITH_KNOTS('',3,(#398379,#398380,#398381,#398382),
 .UNSPECIFIED.,.F.,.F.,(4,4),(0.,9.54361881492173E-5),.UNSPECIFIED.);
#25521=B_SPLINE_CURVE_WITH_KNOTS('',3,(#398387,#398388,#398389,#398390,
#398391,#398392,#398393),.UNSPECIFIED.,.F.,.F.,(4,3,4),(0.,4.4106970432347E-5,
0.000113970027818833),.UNSPECIFIED.);
#25522=B_SPLINE_CURVE_WITH_KNOTS('',3,(#398399,#398400,#398401,#398402),
 .UNSPECIFIED.,.F.,.F.,(4,4),(2.16840434497101E-19,9.54361881492179E-5),
 .UNSPECIFIED.);
#25523=B_SPLINE_CURVE_WITH_KNOTS('',3,(#398406,#398407,#398408,#398409,
#398410,#398411,#398412),.UNSPECIFIED.,.F.,.F.,(4,3,4),(0.,6.98630244191488E-5,
0.000113969974038089),.UNSPECIFIED.);
#25524=B_SPLINE_CURVE_WITH_KNOTS('',3,(#398415,#398416,#398417,#398418,
#398419,#398420,#398421,#398422,#398423,#398424,#398425,#398426,#398427,
#398428,#398429,#398430,#398431,#398432,#398433,#398434,#398435,#398436,
#398437,#398438,#398439,#398440,#398441,#398442,#398443,#398444,#398445,
#398446,#398447,#398448,#398449,#398450,#398451,#398452,#398453,#398454,
#398455,#398456,#398457,#398458,#398459,#398460,#398461,#398462,#398463),
 .UNSPECIFIED.,.F.,.F.,(4,3,3,3,3,3,3,3,3,3,3,3,3,3,3,3,4),(0.,1.53100299373426E-6,
4.52554775679122E-6,7.01151246291613E-6,9.26752933800967E-6,1.03084066197174E-5,
1.17138990826863E-5,1.22284894984075E-5,1.30315035324819E-5,1.38363728497814E-5,
1.40464197777496E-5,1.54597749564639E-5,1.62073588704069E-5,1.92092968712659E-5,
1.95234416882553E-5,2.37637844577623E-5,2.61487188977257E-5),
 .UNSPECIFIED.);
#25525=B_SPLINE_CURVE_WITH_KNOTS('',3,(#398478,#398479,#398480,#398481,
#398482,#398483,#398484,#398485,#398486,#398487,#398488,#398489,#398490,
#398491,#398492,#398493,#398494,#398495,#398496,#398497,#398498,#398499,
#398500,#398501,#398502,#398503,#398504,#398505,#398506,#398507,#398508),
 .UNSPECIFIED.,.F.,.F.,(4,3,3,3,3,3,3,3,3,3,4),(0.,3.95507910398825E-6,
7.53768426604196E-6,1.19904533335349E-5,1.40475043392586E-5,1.51452104275964E-5,
1.67866272814144E-5,1.69621513005358E-5,1.81338315460713E-5,1.98906334656502E-5,
2.06132424588246E-5),.UNSPECIFIED.);
#25526=B_SPLINE_CURVE_WITH_KNOTS('',3,(#398511,#398512,#398513,#398514),
 .UNSPECIFIED.,.F.,.F.,(4,4),(5.42101086242752E-19,0.00010938435327491),
 .UNSPECIFIED.);
#25527=B_SPLINE_CURVE_WITH_KNOTS('',3,(#398541,#398542,#398543,#398544,
#398545,#398546,#398547,#398548,#398549,#398550,#398551,#398552,#398553,
#398554,#398555,#398556,#398557,#398558,#398559,#398560,#398561,#398562,
#398563,#398564,#398565,#398566,#398567,#398568,#398569,#398570,#398571,
#398572,#398573,#398574),.UNSPECIFIED.,.F.,.F.,(4,3,3,3,3,3,3,3,3,3,3,4),
(1.0842021724855E-19,2.09623992729444E-6,3.17176647120229E-6,4.82636181943599E-6,
5.01000917339964E-6,6.13126454147494E-6,8.60486650288865E-6,9.21144281170499E-6,
1.24722301135751E-5,1.42666454787858E-5,2.04670653757029E-5,2.08026438176807E-5),
 .UNSPECIFIED.);
#25528=B_SPLINE_CURVE_WITH_KNOTS('',3,(#398575,#398576,#398577,#398578),
 .UNSPECIFIED.,.F.,.F.,(4,4),(0.,0.000109384345496909),.UNSPECIFIED.);
#25529=B_SPLINE_CURVE_WITH_KNOTS('',3,(#398683,#398684,#398685,#398686),
 .UNSPECIFIED.,.F.,.F.,(4,4),(0.,9.54361881492173E-5),.UNSPECIFIED.);
#25530=B_SPLINE_CURVE_WITH_KNOTS('',3,(#398691,#398692,#398693,#398694,
#398695,#398696,#398697),.UNSPECIFIED.,.F.,.F.,(4,3,4),(0.,4.41069704323471E-5,
0.000113970027818833),.UNSPECIFIED.);
#25531=B_SPLINE_CURVE_WITH_KNOTS('',3,(#398703,#398704,#398705,#398706),
 .UNSPECIFIED.,.F.,.F.,(4,4),(4.84869951806108E-19,9.54361881492178E-5),
 .UNSPECIFIED.);
#25532=B_SPLINE_CURVE_WITH_KNOTS('',3,(#398710,#398711,#398712,#398713,
#398714,#398715,#398716),.UNSPECIFIED.,.F.,.F.,(4,3,4),(0.,6.98630244191491E-5,
0.000113969974038089),.UNSPECIFIED.);
#25533=B_SPLINE_CURVE_WITH_KNOTS('',3,(#398719,#398720,#398721,#398722,
#398723,#398724,#398725,#398726,#398727,#398728,#398729,#398730,#398731,
#398732,#398733,#398734,#398735,#398736,#398737,#398738,#398739,#398740,
#398741,#398742,#398743,#398744,#398745,#398746,#398747,#398748,#398749,
#398750,#398751,#398752,#398753,#398754,#398755,#398756,#398757,#398758,
#398759,#398760,#398761,#398762,#398763,#398764,#398765,#398766,#398767),
 .UNSPECIFIED.,.F.,.F.,(4,3,3,3,3,3,3,3,3,3,3,3,3,3,3,3,4),(0.,1.53100299373415E-6,
4.52554775679612E-6,7.01151246291607E-6,9.26752933798826E-6,1.03084066197174E-5,
1.17138990826862E-5,1.22284894984074E-5,1.30315035324818E-5,1.38363728497812E-5,
1.40464197777495E-5,1.5459774956464E-5,1.6207358870407E-5,1.92092968712588E-5,
1.95234416882558E-5,2.37637844577578E-5,2.61487188977265E-5),
 .UNSPECIFIED.);
#25534=B_SPLINE_CURVE_WITH_KNOTS('',3,(#398782,#398783,#398784,#398785,
#398786,#398787,#398788,#398789,#398790,#398791,#398792,#398793,#398794,
#398795,#398796,#398797,#398798,#398799,#398800,#398801,#398802,#398803,
#398804,#398805,#398806,#398807,#398808,#398809,#398810,#398811,#398812),
 .UNSPECIFIED.,.F.,.F.,(4,3,3,3,3,3,3,3,3,3,4),(0.,3.95507910397645E-6,
7.53768426604196E-6,1.19904533335349E-5,1.40475043392584E-5,1.51452104275963E-5,
1.67866272814147E-5,1.69621513005358E-5,1.81338315460712E-5,1.98906334656532E-5,
2.06132424588247E-5),.UNSPECIFIED.);
#25535=B_SPLINE_CURVE_WITH_KNOTS('',3,(#398815,#398816,#398817,#398818),
 .UNSPECIFIED.,.F.,.F.,(4,4),(1.06229684024259E-18,0.00010938435327491),
 .UNSPECIFIED.);
#25536=B_SPLINE_CURVE_WITH_KNOTS('',3,(#398845,#398846,#398847,#398848,
#398849,#398850,#398851,#398852,#398853,#398854,#398855,#398856,#398857,
#398858,#398859,#398860,#398861,#398862,#398863,#398864,#398865,#398866,
#398867,#398868,#398869,#398870,#398871,#398872,#398873,#398874,#398875,
#398876,#398877,#398878),.UNSPECIFIED.,.F.,.F.,(4,3,3,3,3,3,3,3,3,3,3,4),
(1.0842021724855E-19,2.0962399272944E-6,3.17176647120221E-6,4.82636181942624E-6,
5.0100091733996E-6,6.13126454147486E-6,8.60486650288837E-6,9.21144281170471E-6,
1.24722301135842E-5,1.42666454787849E-5,2.04670653756911E-5,2.08026438176791E-5),
 .UNSPECIFIED.);
#25537=B_SPLINE_CURVE_WITH_KNOTS('',3,(#398879,#398880,#398881,#398882),
 .UNSPECIFIED.,.F.,.F.,(4,4),(0.,0.000109384345496908),.UNSPECIFIED.);
#25538=B_SPLINE_CURVE_WITH_KNOTS('',3,(#398987,#398988,#398989,#398990),
 .UNSPECIFIED.,.F.,.F.,(4,4),(0.,9.54361881492175E-5),.UNSPECIFIED.);
#25539=B_SPLINE_CURVE_WITH_KNOTS('',3,(#398995,#398996,#398997,#398998,
#398999,#399000,#399001),.UNSPECIFIED.,.F.,.F.,(4,3,4),(0.,4.41069704323469E-5,
0.000113970027818833),.UNSPECIFIED.);
#25540=B_SPLINE_CURVE_WITH_KNOTS('',3,(#399007,#399008,#399009,#399010),
 .UNSPECIFIED.,.F.,.F.,(4,4),(2.16840434497101E-19,9.54361881492181E-5),
 .UNSPECIFIED.);
#25541=B_SPLINE_CURVE_WITH_KNOTS('',3,(#399014,#399015,#399016,#399017,
#399018,#399019,#399020),.UNSPECIFIED.,.F.,.F.,(4,3,4),(0.,6.98630244191489E-5,
0.000113969974038089),.UNSPECIFIED.);
#25542=B_SPLINE_CURVE_WITH_KNOTS('',3,(#399023,#399024,#399025,#399026,
#399027,#399028,#399029,#399030,#399031,#399032,#399033,#399034,#399035,
#399036,#399037,#399038,#399039,#399040,#399041,#399042,#399043,#399044,
#399045,#399046,#399047,#399048,#399049,#399050,#399051,#399052,#399053,
#399054,#399055,#399056,#399057,#399058,#399059,#399060,#399061,#399062,
#399063,#399064,#399065,#399066,#399067,#399068,#399069,#399070,#399071),
 .UNSPECIFIED.,.F.,.F.,(4,3,3,3,3,3,3,3,3,3,3,3,3,3,3,3,4),(0.,1.53100299373423E-6,
4.52554775678839E-6,7.01151246291621E-6,9.2675293380022E-6,1.03084066197175E-5,
1.17138990826861E-5,1.22284894984073E-5,1.30315035324817E-5,1.3836372849781E-5,
1.40464197777494E-5,1.5459774956464E-5,1.62073588704068E-5,1.92092968713103E-5,
1.95234416882551E-5,2.37637844577638E-5,2.61487188977247E-5),
 .UNSPECIFIED.);
#25543=B_SPLINE_CURVE_WITH_KNOTS('',3,(#399086,#399087,#399088,#399089,
#399090,#399091,#399092,#399093,#399094,#399095,#399096,#399097,#399098,
#399099,#399100,#399101,#399102,#399103,#399104,#399105,#399106,#399107,
#399108,#399109,#399110,#399111,#399112,#399113,#399114,#399115,#399116),
 .UNSPECIFIED.,.F.,.F.,(4,3,3,3,3,3,3,3,3,3,4),(0.,3.95507910396983E-6,
7.53768426604189E-6,1.1990453333535E-5,1.40475043392585E-5,1.51452104275965E-5,
1.67866272814133E-5,1.6962151300536E-5,1.81338315460716E-5,1.98906334656569E-5,
2.06132424588254E-5),.UNSPECIFIED.);
#25544=B_SPLINE_CURVE_WITH_KNOTS('',3,(#399119,#399120,#399121,#399122),
 .UNSPECIFIED.,.F.,.F.,(4,4),(4.84869951806108E-19,0.00010938435327491),
 .UNSPECIFIED.);
#25545=B_SPLINE_CURVE_WITH_KNOTS('',3,(#399149,#399150,#399151,#399152,
#399153,#399154,#399155,#399156,#399157,#399158,#399159,#399160,#399161,
#399162,#399163,#399164,#399165,#399166,#399167,#399168,#399169,#399170,
#399171,#399172,#399173,#399174,#399175,#399176,#399177,#399178,#399179,
#399180,#399181,#399182),.UNSPECIFIED.,.F.,.F.,(4,3,3,3,3,3,3,3,3,3,3,4),
(2.16840434497101E-19,2.09623992729426E-6,3.17176647120219E-6,4.82636181942554E-6,
5.01000917339955E-6,6.13126454147493E-6,8.60486650288818E-6,9.21144281170458E-6,
1.24722301136027E-5,1.42666454787846E-5,2.04670653756731E-5,2.08026438176786E-5),
 .UNSPECIFIED.);
#25546=B_SPLINE_CURVE_WITH_KNOTS('',3,(#399183,#399184,#399185,#399186),
 .UNSPECIFIED.,.F.,.F.,(4,4),(0.,0.000109384345496908),.UNSPECIFIED.);
#25547=B_SPLINE_CURVE_WITH_KNOTS('',3,(#399291,#399292,#399293,#399294),
 .UNSPECIFIED.,.F.,.F.,(4,4),(0.,9.54361881492175E-5),.UNSPECIFIED.);
#25548=B_SPLINE_CURVE_WITH_KNOTS('',3,(#399299,#399300,#399301,#399302,
#399303,#399304,#399305),.UNSPECIFIED.,.F.,.F.,(4,3,4),(0.,4.41069704323471E-5,
0.000113970027818833),.UNSPECIFIED.);
#25549=B_SPLINE_CURVE_WITH_KNOTS('',3,(#399311,#399312,#399313,#399314),
 .UNSPECIFIED.,.F.,.F.,(4,4),(2.16840434497101E-19,9.54361881492182E-5),
 .UNSPECIFIED.);
#25550=B_SPLINE_CURVE_WITH_KNOTS('',3,(#399318,#399319,#399320,#399321,
#399322,#399323,#399324),.UNSPECIFIED.,.F.,.F.,(4,3,4),(0.,6.98630244191493E-5,
0.000113969974038089),.UNSPECIFIED.);
#25551=B_SPLINE_CURVE_WITH_KNOTS('',3,(#399327,#399328,#399329,#399330,
#399331,#399332,#399333,#399334,#399335,#399336,#399337,#399338,#399339,
#399340,#399341,#399342,#399343,#399344,#399345,#399346,#399347,#399348,
#399349,#399350,#399351,#399352,#399353,#399354,#399355,#399356,#399357,
#399358,#399359,#399360,#399361,#399362,#399363,#399364,#399365,#399366,
#399367,#399368,#399369,#399370,#399371,#399372,#399373,#399374,#399375),
 .UNSPECIFIED.,.F.,.F.,(4,3,3,3,3,3,3,3,3,3,3,3,3,3,3,3,4),(0.,1.53100299373411E-6,
4.52554775679371E-6,7.01151246291605E-6,9.26752933799832E-6,1.03084066197173E-5,
1.17138990826861E-5,1.22284894984075E-5,1.3031503532482E-5,1.38363728497812E-5,
1.40464197777496E-5,1.54597749564641E-5,1.6207358870407E-5,1.92092968713185E-5,
1.95234416882556E-5,2.37637844577594E-5,2.61487188977267E-5),
 .UNSPECIFIED.);
#25552=B_SPLINE_CURVE_WITH_KNOTS('',3,(#399390,#399391,#399392,#399393,
#399394,#399395,#399396,#399397,#399398,#399399,#399400,#399401,#399402,
#399403,#399404,#399405,#399406,#399407,#399408,#399409,#399410,#399411,
#399412,#399413,#399414,#399415,#399416,#399417,#399418,#399419,#399420),
 .UNSPECIFIED.,.F.,.F.,(4,3,3,3,3,3,3,3,3,3,4),(0.,3.9550791039821E-6,7.53768426604195E-6,
1.19904533335351E-5,1.40475043392586E-5,1.51452104275965E-5,1.67866272814213E-5,
1.69621513005356E-5,1.81338315460712E-5,1.98906334656531E-5,2.06132424588241E-5),
 .UNSPECIFIED.);
#25553=B_SPLINE_CURVE_WITH_KNOTS('',3,(#399423,#399424,#399425,#399426),
 .UNSPECIFIED.,.F.,.F.,(4,4),(6.1331736667335E-19,0.00010938435327491),
 .UNSPECIFIED.);
#25554=B_SPLINE_CURVE_WITH_KNOTS('',3,(#399453,#399454,#399455,#399456,
#399457,#399458,#399459,#399460,#399461,#399462,#399463,#399464,#399465,
#399466,#399467,#399468,#399469,#399470,#399471,#399472,#399473,#399474,
#399475,#399476,#399477,#399478,#399479,#399480,#399481,#399482,#399483,
#399484,#399485,#399486),.UNSPECIFIED.,.F.,.F.,(4,3,3,3,3,3,3,3,3,3,3,4),
(2.16840434497101E-19,2.09623992729438E-6,3.17176647120215E-6,4.82636181943272E-6,
5.01000917339969E-6,6.13126454147507E-6,8.60486650288861E-6,9.21144281170498E-6,
1.24722301135845E-5,1.42666454787857E-5,2.04670653757436E-5,2.08026438176804E-5),
 .UNSPECIFIED.);
#25555=B_SPLINE_CURVE_WITH_KNOTS('',3,(#399487,#399488,#399489,#399490),
 .UNSPECIFIED.,.F.,.F.,(4,4),(0.,0.000109384345496908),.UNSPECIFIED.);
#25556=B_SPLINE_CURVE_WITH_KNOTS('',3,(#399595,#399596,#399597,#399598),
 .UNSPECIFIED.,.F.,.F.,(4,4),(0.,9.54361881492177E-5),.UNSPECIFIED.);
#25557=B_SPLINE_CURVE_WITH_KNOTS('',3,(#399603,#399604,#399605,#399606,
#399607,#399608,#399609),.UNSPECIFIED.,.F.,.F.,(4,3,4),(0.,4.41069704323472E-5,
0.000113970027818834),.UNSPECIFIED.);
#25558=B_SPLINE_CURVE_WITH_KNOTS('',3,(#399615,#399616,#399617,#399618),
 .UNSPECIFIED.,.F.,.F.,(4,4),(2.16840434497101E-19,9.54361881492179E-5),
 .UNSPECIFIED.);
#25559=B_SPLINE_CURVE_WITH_KNOTS('',3,(#399622,#399623,#399624,#399625,
#399626,#399627,#399628),.UNSPECIFIED.,.F.,.F.,(4,3,4),(0.,6.98630244191492E-5,
0.000113969974038089),.UNSPECIFIED.);
#25560=B_SPLINE_CURVE_WITH_KNOTS('',3,(#399631,#399632,#399633,#399634,
#399635,#399636,#399637,#399638,#399639,#399640,#399641,#399642,#399643,
#399644,#399645,#399646,#399647,#399648,#399649,#399650,#399651,#399652,
#399653,#399654,#399655,#399656,#399657,#399658,#399659,#399660,#399661,
#399662,#399663,#399664,#399665,#399666,#399667,#399668,#399669,#399670,
#399671,#399672,#399673,#399674,#399675,#399676,#399677,#399678,#399679),
 .UNSPECIFIED.,.F.,.F.,(4,3,3,3,3,3,3,3,3,3,3,3,3,3,3,3,4),(0.,1.53100299373409E-6,
4.52554775679162E-6,7.0115124629161E-6,9.26752933800718E-6,1.03084066197173E-5,
1.17138990826861E-5,1.22284894984077E-5,1.30315035324817E-5,1.38363728497814E-5,
1.40464197777495E-5,1.54597749564643E-5,1.62073588704069E-5,1.92092968712789E-5,
1.95234416882557E-5,2.37637844577536E-5,2.61487188977265E-5),
 .UNSPECIFIED.);
#25561=B_SPLINE_CURVE_WITH_KNOTS('',3,(#399694,#399695,#399696,#399697,
#399698,#399699,#399700,#399701,#399702,#399703,#399704,#399705,#399706,
#399707,#399708,#399709,#399710,#399711,#399712,#399713,#399714,#399715,
#399716,#399717,#399718,#399719,#399720,#399721,#399722,#399723,#399724),
 .UNSPECIFIED.,.F.,.F.,(4,3,3,3,3,3,3,3,3,3,4),(0.,3.95507910396712E-6,
7.53768426604191E-6,1.1990453333535E-5,1.40475043392585E-5,1.51452104275962E-5,
1.67866272814315E-5,1.69621513005358E-5,1.81338315460713E-5,1.98906334656587E-5,
2.06132424588245E-5),.UNSPECIFIED.);
#25562=B_SPLINE_CURVE_WITH_KNOTS('',3,(#399727,#399728,#399729,#399730),
 .UNSPECIFIED.,.F.,.F.,(4,4),(6.1331736667335E-19,0.00010938435327491),
 .UNSPECIFIED.);
#25563=B_SPLINE_CURVE_WITH_KNOTS('',3,(#399757,#399758,#399759,#399760,
#399761,#399762,#399763,#399764,#399765,#399766,#399767,#399768,#399769,
#399770,#399771,#399772,#399773,#399774,#399775,#399776,#399777,#399778,
#399779,#399780,#399781,#399782,#399783,#399784,#399785,#399786,#399787,
#399788,#399789,#399790),.UNSPECIFIED.,.F.,.F.,(4,3,3,3,3,3,3,3,3,3,3,4),
(2.16840434497101E-19,2.09623992729449E-6,3.17176647120226E-6,4.82636181944115E-6,
5.01000917339949E-6,6.13126454147491E-6,8.60486650288856E-6,9.21144281170483E-6,
1.24722301135999E-5,1.42666454787852E-5,2.04670653756803E-5,2.08026438176794E-5),
 .UNSPECIFIED.);
#25564=B_SPLINE_CURVE_WITH_KNOTS('',3,(#399791,#399792,#399793,#399794),
 .UNSPECIFIED.,.F.,.F.,(4,4),(0.,0.000109384345496908),.UNSPECIFIED.);
#25565=B_SPLINE_CURVE_WITH_KNOTS('',3,(#399899,#399900,#399901,#399902),
 .UNSPECIFIED.,.F.,.F.,(4,4),(0.,9.54361881492176E-5),.UNSPECIFIED.);
#25566=B_SPLINE_CURVE_WITH_KNOTS('',3,(#399907,#399908,#399909,#399910,
#399911,#399912,#399913),.UNSPECIFIED.,.F.,.F.,(4,3,4),(0.,4.41069704323472E-5,
0.000113970027818833),.UNSPECIFIED.);
#25567=B_SPLINE_CURVE_WITH_KNOTS('',3,(#399919,#399920,#399921,#399922),
 .UNSPECIFIED.,.F.,.F.,(4,4),(2.16840434497101E-19,9.54361881492179E-5),
 .UNSPECIFIED.);
#25568=B_SPLINE_CURVE_WITH_KNOTS('',3,(#399926,#399927,#399928,#399929,
#399930,#399931,#399932),.UNSPECIFIED.,.F.,.F.,(4,3,4),(0.,6.9863024419149E-5,
0.000113969974038089),.UNSPECIFIED.);
#25569=B_SPLINE_CURVE_WITH_KNOTS('',3,(#399935,#399936,#399937,#399938,
#399939,#399940,#399941,#399942,#399943,#399944,#399945,#399946,#399947,
#399948,#399949,#399950,#399951,#399952,#399953,#399954,#399955,#399956,
#399957,#399958,#399959,#399960,#399961,#399962,#399963,#399964,#399965,
#399966,#399967,#399968,#399969,#399970,#399971,#399972,#399973,#399974,
#399975,#399976,#399977,#399978,#399979,#399980,#399981,#399982,#399983),
 .UNSPECIFIED.,.F.,.F.,(4,3,3,3,3,3,3,3,3,3,3,3,3,3,3,3,4),(0.,1.53100299373425E-6,
4.52554775679298E-6,7.01151246291614E-6,9.2675293379928E-6,1.03084066197173E-5,
1.17138990826863E-5,1.22284894984074E-5,1.3031503532482E-5,1.38363728497814E-5,
1.40464197777497E-5,1.54597749564644E-5,1.62073588704073E-5,1.92092968712382E-5,
1.95234416882566E-5,2.37637844577608E-5,2.61487188977282E-5),
 .UNSPECIFIED.);
#25570=B_SPLINE_CURVE_WITH_KNOTS('',3,(#399998,#399999,#400000,#400001,
#400002,#400003,#400004,#400005,#400006,#400007,#400008,#400009,#400010,
#400011,#400012,#400013,#400014,#400015,#400016,#400017,#400018,#400019,
#400020,#400021,#400022,#400023,#400024,#400025,#400026,#400027,#400028),
 .UNSPECIFIED.,.F.,.F.,(4,3,3,3,3,3,3,3,3,3,4),(0.,3.95507910398008E-6,
7.53768426604198E-6,1.1990453333535E-5,1.40475043392586E-5,1.51452104275965E-5,
1.67866272814163E-5,1.69621513005358E-5,1.81338315460713E-5,1.98906334656514E-5,
2.06132424588243E-5),.UNSPECIFIED.);
#25571=B_SPLINE_CURVE_WITH_KNOTS('',3,(#400031,#400032,#400033,#400034),
 .UNSPECIFIED.,.F.,.F.,(4,4),(4.33680868994202E-19,0.00010938435327491),
 .UNSPECIFIED.);
#25572=B_SPLINE_CURVE_WITH_KNOTS('',3,(#400061,#400062,#400063,#400064,
#400065,#400066,#400067,#400068,#400069,#400070,#400071,#400072,#400073,
#400074,#400075,#400076,#400077,#400078,#400079,#400080,#400081,#400082,
#400083,#400084,#400085,#400086,#400087,#400088,#400089,#400090,#400091,
#400092,#400093,#400094),.UNSPECIFIED.,.F.,.F.,(4,3,3,3,3,3,3,3,3,3,3,4),
(2.16840434497101E-19,2.0962399272944E-6,3.17176647120242E-6,4.82636181944529E-6,
5.01000917339975E-6,6.13126454147501E-6,8.6048665028885E-6,9.21144281170502E-6,
1.24722301136151E-5,1.42666454787858E-5,2.04670653756866E-5,2.08026438176806E-5),
 .UNSPECIFIED.);
#25573=B_SPLINE_CURVE_WITH_KNOTS('',3,(#400095,#400096,#400097,#400098),
 .UNSPECIFIED.,.F.,.F.,(4,4),(0.,0.000109384345496908),.UNSPECIFIED.);
#25574=B_SPLINE_CURVE_WITH_KNOTS('',3,(#400203,#400204,#400205,#400206),
 .UNSPECIFIED.,.F.,.F.,(4,4),(0.,9.54361881492176E-5),.UNSPECIFIED.);
#25575=B_SPLINE_CURVE_WITH_KNOTS('',3,(#400211,#400212,#400213,#400214,
#400215,#400216,#400217),.UNSPECIFIED.,.F.,.F.,(4,3,4),(0.,4.41069704323467E-5,
0.000113970027818833),.UNSPECIFIED.);
#25576=B_SPLINE_CURVE_WITH_KNOTS('',3,(#400223,#400224,#400225,#400226),
 .UNSPECIFIED.,.F.,.F.,(4,4),(2.16840434497101E-19,9.54361881492179E-5),
 .UNSPECIFIED.);
#25577=B_SPLINE_CURVE_WITH_KNOTS('',3,(#400230,#400231,#400232,#400233,
#400234,#400235,#400236),.UNSPECIFIED.,.F.,.F.,(4,3,4),(0.,6.98630244191488E-5,
0.000113969974038089),.UNSPECIFIED.);
#25578=B_SPLINE_CURVE_WITH_KNOTS('',3,(#400239,#400240,#400241,#400242,
#400243,#400244,#400245,#400246,#400247,#400248,#400249,#400250,#400251,
#400252,#400253,#400254,#400255,#400256,#400257,#400258,#400259,#400260,
#400261,#400262,#400263,#400264,#400265,#400266,#400267,#400268,#400269,
#400270,#400271,#400272,#400273,#400274,#400275,#400276,#400277,#400278,
#400279,#400280,#400281,#400282,#400283,#400284,#400285,#400286,#400287),
 .UNSPECIFIED.,.F.,.F.,(4,3,3,3,3,3,3,3,3,3,3,3,3,3,3,3,4),(0.,1.53100299373415E-6,
4.52554775679384E-6,7.01151246291613E-6,9.26752933801275E-6,1.03084066197174E-5,
1.17138990826863E-5,1.22284894984077E-5,1.30315035324817E-5,1.38363728497813E-5,
1.40464197777498E-5,1.5459774956464E-5,1.6207358870407E-5,1.92092968713218E-5,
1.95234416882559E-5,2.37637844577589E-5,2.61487188977269E-5),
 .UNSPECIFIED.);
#25579=B_SPLINE_CURVE_WITH_KNOTS('',3,(#400302,#400303,#400304,#400305,
#400306,#400307,#400308,#400309,#400310,#400311,#400312,#400313,#400314,
#400315,#400316,#400317,#400318,#400319,#400320,#400321,#400322,#400323,
#400324,#400325,#400326,#400327,#400328,#400329,#400330,#400331,#400332),
 .UNSPECIFIED.,.F.,.F.,(4,3,3,3,3,3,3,3,3,3,4),(0.,3.95507910398558E-6,
7.53768426604203E-6,1.19904533335348E-5,1.40475043392586E-5,1.51452104275963E-5,
1.67866272814335E-5,1.69621513005358E-5,1.81338315460711E-5,1.98906334656505E-5,
2.06132424588244E-5),.UNSPECIFIED.);
#25580=B_SPLINE_CURVE_WITH_KNOTS('',3,(#400335,#400336,#400337,#400338),
 .UNSPECIFIED.,.F.,.F.,(4,4),(2.16840434497101E-19,0.00010938435327491),
 .UNSPECIFIED.);
#25581=B_SPLINE_CURVE_WITH_KNOTS('',3,(#400365,#400366,#400367,#400368,
#400369,#400370,#400371,#400372,#400373,#400374,#400375,#400376,#400377,
#400378,#400379,#400380,#400381,#400382,#400383,#400384,#400385,#400386,
#400387,#400388,#400389,#400390,#400391,#400392,#400393,#400394,#400395,
#400396,#400397,#400398),.UNSPECIFIED.,.F.,.F.,(4,3,3,3,3,3,3,3,3,3,3,4),
(0.,2.09623992729418E-6,3.171766471202E-6,4.82636181943802E-6,5.01000917339955E-6,
6.13126454147495E-6,8.60486650288841E-6,9.21144281170478E-6,1.24722301136026E-5,
1.42666454787854E-5,2.04670653756955E-5,2.080264381768E-5),
 .UNSPECIFIED.);
#25582=B_SPLINE_CURVE_WITH_KNOTS('',3,(#400399,#400400,#400401,#400402),
 .UNSPECIFIED.,.F.,.F.,(4,4),(0.,0.000109384345496908),.UNSPECIFIED.);
#25583=B_SPLINE_CURVE_WITH_KNOTS('',3,(#400507,#400508,#400509,#400510),
 .UNSPECIFIED.,.F.,.F.,(4,4),(0.,9.54361881492176E-5),.UNSPECIFIED.);
#25584=B_SPLINE_CURVE_WITH_KNOTS('',3,(#400515,#400516,#400517,#400518,
#400519,#400520,#400521),.UNSPECIFIED.,.F.,.F.,(4,3,4),(0.,4.41069704323472E-5,
0.000113970027818833),.UNSPECIFIED.);
#25585=B_SPLINE_CURVE_WITH_KNOTS('',3,(#400527,#400528,#400529,#400530),
 .UNSPECIFIED.,.F.,.F.,(4,4),(2.16840434497101E-19,9.54361881492179E-5),
 .UNSPECIFIED.);
#25586=B_SPLINE_CURVE_WITH_KNOTS('',3,(#400534,#400535,#400536,#400537,
#400538,#400539,#400540),.UNSPECIFIED.,.F.,.F.,(4,3,4),(0.,6.98630244191491E-5,
0.000113969974038089),.UNSPECIFIED.);
#25587=B_SPLINE_CURVE_WITH_KNOTS('',3,(#400543,#400544,#400545,#400546,
#400547,#400548,#400549,#400550,#400551,#400552,#400553,#400554,#400555,
#400556,#400557,#400558,#400559,#400560,#400561,#400562,#400563,#400564,
#400565,#400566,#400567,#400568,#400569,#400570,#400571,#400572,#400573,
#400574,#400575,#400576,#400577,#400578,#400579,#400580,#400581,#400582,
#400583,#400584,#400585,#400586,#400587,#400588,#400589,#400590,#400591),
 .UNSPECIFIED.,.F.,.F.,(4,3,3,3,3,3,3,3,3,3,3,3,3,3,3,3,4),(0.,1.53100299373417E-6,
4.52554775679272E-6,7.01151246291594E-6,9.26752933800003E-6,1.03084066197173E-5,
1.17138990826861E-5,1.22284894984073E-5,1.30315035324815E-5,1.38363728497812E-5,
1.40464197777495E-5,1.54597749564639E-5,1.62073588704069E-5,1.92092968713092E-5,
1.95234416882555E-5,2.37637844577628E-5,2.61487188977262E-5),
 .UNSPECIFIED.);
#25588=B_SPLINE_CURVE_WITH_KNOTS('',3,(#400606,#400607,#400608,#400609,
#400610,#400611,#400612,#400613,#400614,#400615,#400616,#400617,#400618,
#400619,#400620,#400621,#400622,#400623,#400624,#400625,#400626,#400627,
#400628,#400629,#400630,#400631,#400632,#400633,#400634,#400635,#400636),
 .UNSPECIFIED.,.F.,.F.,(4,3,3,3,3,3,3,3,3,3,4),(0.,3.955079103977E-6,7.5376842660419E-6,
1.19904533335349E-5,1.40475043392587E-5,1.51452104275965E-5,1.67866272814353E-5,
1.69621513005359E-5,1.81338315460712E-5,1.9890633465657E-5,2.06132424588247E-5),
 .UNSPECIFIED.);
#25589=B_SPLINE_CURVE_WITH_KNOTS('',3,(#400639,#400640,#400641,#400642),
 .UNSPECIFIED.,.F.,.F.,(4,4),(2.16840434497101E-19,0.00010938435327491),
 .UNSPECIFIED.);
#25590=B_SPLINE_CURVE_WITH_KNOTS('',3,(#400669,#400670,#400671,#400672,
#400673,#400674,#400675,#400676,#400677,#400678,#400679,#400680,#400681,
#400682,#400683,#400684,#400685,#400686,#400687,#400688,#400689,#400690,
#400691,#400692,#400693,#400694,#400695,#400696,#400697,#400698,#400699,
#400700,#400701,#400702),.UNSPECIFIED.,.F.,.F.,(4,3,3,3,3,3,3,3,3,3,3,4),
(0.,2.09623992729445E-6,3.17176647120223E-6,4.82636181943907E-6,5.01000917339951E-6,
6.131264541475E-6,8.60486650288844E-6,9.21144281170483E-6,1.24722301135966E-5,
1.42666454787851E-5,2.0467065375686E-5,2.08026438176793E-5),
 .UNSPECIFIED.);
#25591=B_SPLINE_CURVE_WITH_KNOTS('',3,(#400703,#400704,#400705,#400706),
 .UNSPECIFIED.,.F.,.F.,(4,4),(0.,0.000109384345496908),.UNSPECIFIED.);
#25592=B_SPLINE_CURVE_WITH_KNOTS('',3,(#400811,#400812,#400813,#400814),
 .UNSPECIFIED.,.F.,.F.,(4,4),(0.,9.54361881492176E-5),.UNSPECIFIED.);
#25593=B_SPLINE_CURVE_WITH_KNOTS('',3,(#400819,#400820,#400821,#400822,
#400823,#400824,#400825),.UNSPECIFIED.,.F.,.F.,(4,3,4),(0.,4.41069704323469E-5,
0.000113970027818833),.UNSPECIFIED.);
#25594=B_SPLINE_CURVE_WITH_KNOTS('',3,(#400831,#400832,#400833,#400834),
 .UNSPECIFIED.,.F.,.F.,(4,4),(0.,9.54361881492176E-5),.UNSPECIFIED.);
#25595=B_SPLINE_CURVE_WITH_KNOTS('',3,(#400838,#400839,#400840,#400841,
#400842,#400843,#400844),.UNSPECIFIED.,.F.,.F.,(4,3,4),(0.,6.9863024419149E-5,
0.000113969974038089),.UNSPECIFIED.);
#25596=B_SPLINE_CURVE_WITH_KNOTS('',3,(#400847,#400848,#400849,#400850,
#400851,#400852,#400853,#400854,#400855,#400856,#400857,#400858,#400859,
#400860,#400861,#400862,#400863,#400864,#400865,#400866,#400867,#400868,
#400869,#400870,#400871,#400872,#400873,#400874,#400875,#400876,#400877,
#400878,#400879,#400880,#400881,#400882,#400883,#400884,#400885,#400886,
#400887,#400888,#400889,#400890,#400891,#400892,#400893,#400894,#400895),
 .UNSPECIFIED.,.F.,.F.,(4,3,3,3,3,3,3,3,3,3,3,3,3,3,3,3,4),(0.,1.53100299373414E-6,
4.52554775679455E-6,7.01151246291618E-6,9.26752933800158E-6,1.03084066197174E-5,
1.17138990826862E-5,1.22284894984075E-5,1.30315035324817E-5,1.38363728497811E-5,
1.40464197777495E-5,1.54597749564639E-5,1.62073588704068E-5,1.92092968712879E-5,
1.95234416882552E-5,2.3763784457757E-5,2.61487188977255E-5),
 .UNSPECIFIED.);
#25597=B_SPLINE_CURVE_WITH_KNOTS('',3,(#400910,#400911,#400912,#400913,
#400914,#400915,#400916,#400917,#400918,#400919,#400920,#400921,#400922,
#400923,#400924,#400925,#400926,#400927,#400928,#400929,#400930,#400931,
#400932,#400933,#400934,#400935,#400936,#400937,#400938,#400939,#400940),
 .UNSPECIFIED.,.F.,.F.,(4,3,3,3,3,3,3,3,3,3,4),(0.,3.95507910398038E-6,
7.53768426604196E-6,1.1990453333535E-5,1.40475043392586E-5,1.51452104275967E-5,
1.67866272814212E-5,1.69621513005361E-5,1.81338315460711E-5,1.98906334656552E-5,
2.06132424588246E-5),.UNSPECIFIED.);
#25598=B_SPLINE_CURVE_WITH_KNOTS('',3,(#400943,#400944,#400945,#400946),
 .UNSPECIFIED.,.F.,.F.,(4,4),(4.33680868994202E-19,0.00010938435327491),
 .UNSPECIFIED.);
#25599=B_SPLINE_CURVE_WITH_KNOTS('',3,(#400973,#400974,#400975,#400976,
#400977,#400978,#400979,#400980,#400981,#400982,#400983,#400984,#400985,
#400986,#400987,#400988,#400989,#400990,#400991,#400992,#400993,#400994,
#400995,#400996,#400997,#400998,#400999,#401000,#401001,#401002,#401003,
#401004,#401005,#401006),.UNSPECIFIED.,.F.,.F.,(4,3,3,3,3,3,3,3,3,3,3,4),
(3.06658683336675E-19,2.0962399272942E-6,3.17176647120205E-6,4.82636181942511E-6,
5.01000917339963E-6,6.13126454147484E-6,8.6048665028884E-6,9.21144281170476E-6,
1.24722301135868E-5,1.42666454787856E-5,2.0467065375687E-5,2.08026438176804E-5),
 .UNSPECIFIED.);
#25600=B_SPLINE_CURVE_WITH_KNOTS('',3,(#401007,#401008,#401009,#401010),
 .UNSPECIFIED.,.F.,.F.,(4,4),(0.,0.000109384345496908),.UNSPECIFIED.);
#25601=B_SPLINE_CURVE_WITH_KNOTS('',3,(#401115,#401116,#401117,#401118),
 .UNSPECIFIED.,.F.,.F.,(4,4),(0.,9.54361881492175E-5),.UNSPECIFIED.);
#25602=B_SPLINE_CURVE_WITH_KNOTS('',3,(#401123,#401124,#401125,#401126,
#401127,#401128,#401129),.UNSPECIFIED.,.F.,.F.,(4,3,4),(0.,4.41069704323469E-5,
0.000113970027818833),.UNSPECIFIED.);
#25603=B_SPLINE_CURVE_WITH_KNOTS('',3,(#401135,#401136,#401137,#401138),
 .UNSPECIFIED.,.F.,.F.,(4,4),(4.33680868994202E-19,9.54361881492178E-5),
 .UNSPECIFIED.);
#25604=B_SPLINE_CURVE_WITH_KNOTS('',3,(#401142,#401143,#401144,#401145,
#401146,#401147,#401148),.UNSPECIFIED.,.F.,.F.,(4,3,4),(0.,6.9863024419149E-5,
0.000113969974038089),.UNSPECIFIED.);
#25605=B_SPLINE_CURVE_WITH_KNOTS('',3,(#401151,#401152,#401153,#401154,
#401155,#401156,#401157,#401158,#401159,#401160,#401161,#401162,#401163,
#401164,#401165,#401166,#401167,#401168,#401169,#401170,#401171,#401172,
#401173,#401174,#401175,#401176,#401177,#401178,#401179,#401180,#401181,
#401182,#401183,#401184,#401185,#401186,#401187,#401188,#401189,#401190,
#401191,#401192,#401193,#401194,#401195,#401196,#401197,#401198,#401199),
 .UNSPECIFIED.,.F.,.F.,(4,3,3,3,3,3,3,3,3,3,3,3,3,3,3,3,4),(0.,1.53100299373413E-6,
4.52554775679261E-6,7.01151246291609E-6,9.26752933800109E-6,1.03084066197174E-5,
1.17138990826864E-5,1.22284894984075E-5,1.30315035324817E-5,1.38363728497814E-5,
1.40464197777494E-5,1.54597749564638E-5,1.62073588704068E-5,1.92092968712784E-5,
1.95234416882556E-5,2.37637844577558E-5,2.61487188977267E-5),
 .UNSPECIFIED.);
#25606=B_SPLINE_CURVE_WITH_KNOTS('',3,(#401214,#401215,#401216,#401217,
#401218,#401219,#401220,#401221,#401222,#401223,#401224,#401225,#401226,
#401227,#401228,#401229,#401230,#401231,#401232,#401233,#401234,#401235,
#401236,#401237,#401238,#401239,#401240,#401241,#401242,#401243,#401244),
 .UNSPECIFIED.,.F.,.F.,(4,3,3,3,3,3,3,3,3,3,4),(0.,3.95507910396964E-6,
7.53768426604187E-6,1.19904533335349E-5,1.40475043392586E-5,1.51452104275963E-5,
1.6786627281416E-5,1.69621513005355E-5,1.81338315460709E-5,1.98906334656525E-5,
2.0613242458824E-5),.UNSPECIFIED.);
#25607=B_SPLINE_CURVE_WITH_KNOTS('',3,(#401247,#401248,#401249,#401250),
 .UNSPECIFIED.,.F.,.F.,(4,4),(4.33680868994202E-19,0.00010938435327491),
 .UNSPECIFIED.);
#25608=B_SPLINE_CURVE_WITH_KNOTS('',3,(#401277,#401278,#401279,#401280,
#401281,#401282,#401283,#401284,#401285,#401286,#401287,#401288,#401289,
#401290,#401291,#401292,#401293,#401294,#401295,#401296,#401297,#401298,
#401299,#401300,#401301,#401302,#401303,#401304,#401305,#401306,#401307,
#401308,#401309,#401310),.UNSPECIFIED.,.F.,.F.,(4,3,3,3,3,3,3,3,3,3,3,4),
(2.16840434497101E-19,2.09623992729392E-6,3.17176647120205E-6,4.82636181942159E-6,
5.01000917339932E-6,6.13126454147464E-6,8.60486650288817E-6,9.2114428117045E-6,
1.24722301136082E-5,1.42666454787851E-5,2.04670653757038E-5,2.08026438176795E-5),
 .UNSPECIFIED.);
#25609=B_SPLINE_CURVE_WITH_KNOTS('',3,(#401311,#401312,#401313,#401314),
 .UNSPECIFIED.,.F.,.F.,(4,4),(0.,0.000109384345496908),.UNSPECIFIED.);
#25610=B_SPLINE_CURVE_WITH_KNOTS('',3,(#401419,#401420,#401421,#401422),
 .UNSPECIFIED.,.F.,.F.,(4,4),(0.,9.54361881492175E-5),.UNSPECIFIED.);
#25611=B_SPLINE_CURVE_WITH_KNOTS('',3,(#401427,#401428,#401429,#401430,
#401431,#401432,#401433),.UNSPECIFIED.,.F.,.F.,(4,3,4),(0.,4.41069704323469E-5,
0.000113970027818833),.UNSPECIFIED.);
#25612=B_SPLINE_CURVE_WITH_KNOTS('',3,(#401439,#401440,#401441,#401442),
 .UNSPECIFIED.,.F.,.F.,(4,4),(4.33680868994202E-19,9.54361881492177E-5),
 .UNSPECIFIED.);
#25613=B_SPLINE_CURVE_WITH_KNOTS('',3,(#401446,#401447,#401448,#401449,
#401450,#401451,#401452),.UNSPECIFIED.,.F.,.F.,(4,3,4),(0.,6.98630244191489E-5,
0.000113969974038089),.UNSPECIFIED.);
#25614=B_SPLINE_CURVE_WITH_KNOTS('',3,(#401455,#401456,#401457,#401458,
#401459,#401460,#401461,#401462,#401463,#401464,#401465,#401466,#401467,
#401468,#401469,#401470,#401471,#401472,#401473,#401474,#401475,#401476,
#401477,#401478,#401479,#401480,#401481,#401482,#401483,#401484,#401485,
#401486,#401487,#401488,#401489,#401490,#401491,#401492,#401493,#401494,
#401495,#401496,#401497,#401498,#401499,#401500,#401501,#401502,#401503),
 .UNSPECIFIED.,.F.,.F.,(4,3,3,3,3,3,3,3,3,3,3,3,3,3,3,3,4),(0.,1.53100299373419E-6,
4.52554775679468E-6,7.01151246291595E-6,9.26752933801825E-6,1.03084066197172E-5,
1.17138990826859E-5,1.22284894984072E-5,1.30315035324817E-5,1.38363728497812E-5,
1.40464197777492E-5,1.54597749564638E-5,1.62073588704066E-5,1.92092968712874E-5,
1.95234416882548E-5,2.37637844577601E-5,2.61487188977246E-5),
 .UNSPECIFIED.);
#25615=B_SPLINE_CURVE_WITH_KNOTS('',3,(#401518,#401519,#401520,#401521,
#401522,#401523,#401524,#401525,#401526,#401527,#401528,#401529,#401530,
#401531,#401532,#401533,#401534,#401535,#401536,#401537,#401538,#401539,
#401540,#401541,#401542,#401543,#401544,#401545,#401546,#401547,#401548),
 .UNSPECIFIED.,.F.,.F.,(4,3,3,3,3,3,3,3,3,3,4),(0.,3.95507910396898E-6,
7.537684266042E-6,1.1990453333535E-5,1.40475043392585E-5,1.51452104275964E-5,
1.67866272814168E-5,1.69621513005359E-5,1.81338315460712E-5,1.98906334656556E-5,
2.06132424588245E-5),.UNSPECIFIED.);
#25616=B_SPLINE_CURVE_WITH_KNOTS('',3,(#401551,#401552,#401553,#401554),
 .UNSPECIFIED.,.F.,.F.,(4,4),(4.33680868994202E-19,0.00010938435327491),
 .UNSPECIFIED.);
#25617=B_SPLINE_CURVE_WITH_KNOTS('',3,(#401581,#401582,#401583,#401584,
#401585,#401586,#401587,#401588,#401589,#401590,#401591,#401592,#401593,
#401594,#401595,#401596,#401597,#401598,#401599,#401600,#401601,#401602,
#401603,#401604,#401605,#401606,#401607,#401608,#401609,#401610,#401611,
#401612,#401613,#401614),.UNSPECIFIED.,.F.,.F.,(4,3,3,3,3,3,3,3,3,3,3,4),
(2.16840434497101E-19,2.09623992729436E-6,3.17176647120222E-6,4.82636181944612E-6,
5.01000917339947E-6,6.13126454147495E-6,8.60486650288831E-6,9.21144281170459E-6,
1.24722301136143E-5,1.42666454787854E-5,2.04670653756866E-5,2.08026438176799E-5),
 .UNSPECIFIED.);
#25618=B_SPLINE_CURVE_WITH_KNOTS('',3,(#401615,#401616,#401617,#401618),
 .UNSPECIFIED.,.F.,.F.,(4,4),(0.,0.000109384345496908),.UNSPECIFIED.);
#25619=B_SPLINE_CURVE_WITH_KNOTS('',3,(#401723,#401724,#401725,#401726),
 .UNSPECIFIED.,.F.,.F.,(4,4),(0.,9.54361881492177E-5),.UNSPECIFIED.);
#25620=B_SPLINE_CURVE_WITH_KNOTS('',3,(#401731,#401732,#401733,#401734,
#401735,#401736,#401737),.UNSPECIFIED.,.F.,.F.,(4,3,4),(0.,4.41069704323469E-5,
0.000113970027818833),.UNSPECIFIED.);
#25621=B_SPLINE_CURVE_WITH_KNOTS('',3,(#401743,#401744,#401745,#401746),
 .UNSPECIFIED.,.F.,.F.,(4,4),(4.33680868994202E-19,9.54361881492178E-5),
 .UNSPECIFIED.);
#25622=B_SPLINE_CURVE_WITH_KNOTS('',3,(#401750,#401751,#401752,#401753,
#401754,#401755,#401756),.UNSPECIFIED.,.F.,.F.,(4,3,4),(0.,6.98630244191488E-5,
0.000113969974038089),.UNSPECIFIED.);
#25623=B_SPLINE_CURVE_WITH_KNOTS('',3,(#401759,#401760,#401761,#401762,
#401763,#401764,#401765,#401766,#401767,#401768,#401769,#401770,#401771,
#401772,#401773,#401774,#401775,#401776,#401777,#401778,#401779,#401780,
#401781,#401782,#401783,#401784,#401785,#401786,#401787,#401788,#401789,
#401790,#401791,#401792,#401793,#401794,#401795,#401796,#401797,#401798,
#401799,#401800,#401801,#401802,#401803,#401804,#401805,#401806,#401807),
 .UNSPECIFIED.,.F.,.F.,(4,3,3,3,3,3,3,3,3,3,3,3,3,3,3,3,4),(0.,1.53100299373429E-6,
4.5255477568026E-6,7.01151246291634E-6,9.26752933801703E-6,1.03084066197173E-5,
1.17138990826863E-5,1.22284894984075E-5,1.3031503532482E-5,1.38363728497815E-5,
1.40464197777499E-5,1.54597749564644E-5,1.62073588704075E-5,1.92092968712479E-5,
1.95234416882565E-5,2.37637844577607E-5,2.61487188977278E-5),
 .UNSPECIFIED.);
#25624=B_SPLINE_CURVE_WITH_KNOTS('',3,(#401822,#401823,#401824,#401825,
#401826,#401827,#401828,#401829,#401830,#401831,#401832,#401833,#401834,
#401835,#401836,#401837,#401838,#401839,#401840,#401841,#401842,#401843,
#401844,#401845,#401846,#401847,#401848,#401849,#401850,#401851,#401852),
 .UNSPECIFIED.,.F.,.F.,(4,3,3,3,3,3,3,3,3,3,4),(0.,3.95507910398437E-6,
7.53768426604198E-6,1.1990453333535E-5,1.40475043392586E-5,1.51452104275963E-5,
1.67866272814243E-5,1.69621513005356E-5,1.81338315460712E-5,1.98906334656531E-5,
2.06132424588245E-5),.UNSPECIFIED.);
#25625=B_SPLINE_CURVE_WITH_KNOTS('',3,(#401855,#401856,#401857,#401858),
 .UNSPECIFIED.,.F.,.F.,(4,4),(4.33680868994202E-19,0.00010938435327491),
 .UNSPECIFIED.);
#25626=B_SPLINE_CURVE_WITH_KNOTS('',3,(#401885,#401886,#401887,#401888,
#401889,#401890,#401891,#401892,#401893,#401894,#401895,#401896,#401897,
#401898,#401899,#401900,#401901,#401902,#401903,#401904,#401905,#401906,
#401907,#401908,#401909,#401910,#401911,#401912,#401913,#401914,#401915,
#401916,#401917,#401918),.UNSPECIFIED.,.F.,.F.,(4,3,3,3,3,3,3,3,3,3,3,4),
(2.16840434497101E-19,2.09623992729449E-6,3.17176647120214E-6,4.82636181942187E-6,
5.01000917339954E-6,6.13126454147488E-6,8.60486650288861E-6,9.21144281170478E-6,
1.24722301135873E-5,1.42666454787854E-5,2.04670653756818E-5,2.08026438176801E-5),
 .UNSPECIFIED.);
#25627=B_SPLINE_CURVE_WITH_KNOTS('',3,(#401919,#401920,#401921,#401922),
 .UNSPECIFIED.,.F.,.F.,(4,4),(0.,0.000109384345496908),.UNSPECIFIED.);
#25628=B_SPLINE_CURVE_WITH_KNOTS('',3,(#402027,#402028,#402029,#402030),
 .UNSPECIFIED.,.F.,.F.,(4,4),(0.,9.54361881492177E-5),.UNSPECIFIED.);
#25629=B_SPLINE_CURVE_WITH_KNOTS('',3,(#402035,#402036,#402037,#402038,
#402039,#402040,#402041),.UNSPECIFIED.,.F.,.F.,(4,3,4),(0.,4.4106970432347E-5,
0.000113970027818834),.UNSPECIFIED.);
#25630=B_SPLINE_CURVE_WITH_KNOTS('',3,(#402047,#402048,#402049,#402050),
 .UNSPECIFIED.,.F.,.F.,(4,4),(4.33680868994202E-19,9.54361881492178E-5),
 .UNSPECIFIED.);
#25631=B_SPLINE_CURVE_WITH_KNOTS('',3,(#402054,#402055,#402056,#402057,
#402058,#402059,#402060),.UNSPECIFIED.,.F.,.F.,(4,3,4),(0.,6.9863024419149E-5,
0.000113969974038089),.UNSPECIFIED.);
#25632=B_SPLINE_CURVE_WITH_KNOTS('',3,(#402063,#402064,#402065,#402066,
#402067,#402068,#402069,#402070,#402071,#402072,#402073,#402074,#402075,
#402076,#402077,#402078,#402079,#402080,#402081,#402082,#402083,#402084,
#402085,#402086,#402087,#402088,#402089,#402090,#402091,#402092,#402093,
#402094,#402095,#402096,#402097,#402098,#402099,#402100,#402101,#402102,
#402103,#402104,#402105,#402106,#402107,#402108,#402109,#402110,#402111),
 .UNSPECIFIED.,.F.,.F.,(4,3,3,3,3,3,3,3,3,3,3,3,3,3,3,3,4),(0.,1.53100299373411E-6,
4.52554775679681E-6,7.01151246291603E-6,9.26752933799318E-6,1.03084066197172E-5,
1.1713899082686E-5,1.22284894984074E-5,1.30315035324816E-5,1.38363728497814E-5,
1.40464197777494E-5,1.54597749564641E-5,1.62073588704069E-5,1.920929687127E-5,
1.95234416882557E-5,2.37637844577625E-5,2.61487188977266E-5),
 .UNSPECIFIED.);
#25633=B_SPLINE_CURVE_WITH_KNOTS('',3,(#402126,#402127,#402128,#402129,
#402130,#402131,#402132,#402133,#402134,#402135,#402136,#402137,#402138,
#402139,#402140,#402141,#402142,#402143,#402144,#402145,#402146,#402147,
#402148,#402149,#402150,#402151,#402152,#402153,#402154,#402155,#402156),
 .UNSPECIFIED.,.F.,.F.,(4,3,3,3,3,3,3,3,3,3,4),(0.,3.95507910397755E-6,
7.53768426604204E-6,1.1990453333535E-5,1.40475043392587E-5,1.51452104275965E-5,
1.67866272814177E-5,1.69621513005359E-5,1.81338315460714E-5,1.98906334656546E-5,
2.0613242458825E-5),.UNSPECIFIED.);
#25634=B_SPLINE_CURVE_WITH_KNOTS('',3,(#402159,#402160,#402161,#402162),
 .UNSPECIFIED.,.F.,.F.,(4,4),(9.69739903612216E-19,0.000109384353274909),
 .UNSPECIFIED.);
#25635=B_SPLINE_CURVE_WITH_KNOTS('',3,(#402189,#402190,#402191,#402192,
#402193,#402194,#402195,#402196,#402197,#402198,#402199,#402200,#402201,
#402202,#402203,#402204,#402205,#402206,#402207,#402208,#402209,#402210,
#402211,#402212,#402213,#402214,#402215,#402216,#402217,#402218,#402219,
#402220,#402221,#402222),.UNSPECIFIED.,.F.,.F.,(4,3,3,3,3,3,3,3,3,3,3,4),
(0.,2.09623992729429E-6,3.17176647120231E-6,4.82636181944926E-6,5.01000917339935E-6,
6.13126454147493E-6,8.60486650288825E-6,9.21144281170447E-6,1.24722301135953E-5,
1.4266645478785E-5,2.04670653756821E-5,2.08026438176793E-5),
 .UNSPECIFIED.);
#25636=B_SPLINE_CURVE_WITH_KNOTS('',3,(#402223,#402224,#402225,#402226),
 .UNSPECIFIED.,.F.,.F.,(4,4),(0.,0.000109384345496908),.UNSPECIFIED.);
#25637=B_SPLINE_CURVE_WITH_KNOTS('',3,(#402331,#402332,#402333,#402334),
 .UNSPECIFIED.,.F.,.F.,(4,4),(0.,9.54361881492175E-5),.UNSPECIFIED.);
#25638=B_SPLINE_CURVE_WITH_KNOTS('',3,(#402339,#402340,#402341,#402342,
#402343,#402344,#402345),.UNSPECIFIED.,.F.,.F.,(4,3,4),(0.,4.4106970432347E-5,
0.000113970027818833),.UNSPECIFIED.);
#25639=B_SPLINE_CURVE_WITH_KNOTS('',3,(#402351,#402352,#402353,#402354),
 .UNSPECIFIED.,.F.,.F.,(4,4),(4.33680868994202E-19,9.54361881492175E-5),
 .UNSPECIFIED.);
#25640=B_SPLINE_CURVE_WITH_KNOTS('',3,(#402358,#402359,#402360,#402361,
#402362,#402363,#402364),.UNSPECIFIED.,.F.,.F.,(4,3,4),(0.,6.98630244191489E-5,
0.000113969974038089),.UNSPECIFIED.);
#25641=B_SPLINE_CURVE_WITH_KNOTS('',3,(#402367,#402368,#402369,#402370,
#402371,#402372,#402373,#402374,#402375,#402376,#402377,#402378,#402379,
#402380,#402381,#402382,#402383,#402384,#402385,#402386,#402387,#402388,
#402389,#402390,#402391,#402392,#402393,#402394,#402395,#402396,#402397,
#402398,#402399,#402400,#402401,#402402,#402403,#402404,#402405,#402406,
#402407,#402408,#402409,#402410,#402411,#402412,#402413,#402414,#402415),
 .UNSPECIFIED.,.F.,.F.,(4,3,3,3,3,3,3,3,3,3,3,3,3,3,3,3,4),(0.,1.53100299373417E-6,
4.52554775680002E-6,7.01151246291616E-6,9.26752933800212E-6,1.03084066197174E-5,
1.1713899082686E-5,1.22284894984073E-5,1.30315035324815E-5,1.38363728497811E-5,
1.40464197777491E-5,1.54597749564636E-5,1.62073588704065E-5,1.92092968712526E-5,
1.95234416882551E-5,2.37637844577574E-5,2.61487188977254E-5),
 .UNSPECIFIED.);
#25642=B_SPLINE_CURVE_WITH_KNOTS('',3,(#402430,#402431,#402432,#402433,
#402434,#402435,#402436,#402437,#402438,#402439,#402440,#402441,#402442,
#402443,#402444,#402445,#402446,#402447,#402448,#402449,#402450,#402451,
#402452,#402453,#402454,#402455,#402456,#402457,#402458,#402459,#402460),
 .UNSPECIFIED.,.F.,.F.,(4,3,3,3,3,3,3,3,3,3,4),(0.,3.9550791039745E-6,7.53768426604198E-6,
1.19904533335351E-5,1.40475043392586E-5,1.51452104275967E-5,1.67866272814068E-5,
1.69621513005358E-5,1.81338315460714E-5,1.98906334656572E-5,2.06132424588245E-5),
 .UNSPECIFIED.);
#25643=B_SPLINE_CURVE_WITH_KNOTS('',3,(#402463,#402464,#402465,#402466),
 .UNSPECIFIED.,.F.,.F.,(4,4),(4.33680868994202E-19,0.00010938435327491),
 .UNSPECIFIED.);
#25644=B_SPLINE_CURVE_WITH_KNOTS('',3,(#402493,#402494,#402495,#402496,
#402497,#402498,#402499,#402500,#402501,#402502,#402503,#402504,#402505,
#402506,#402507,#402508,#402509,#402510,#402511,#402512,#402513,#402514,
#402515,#402516,#402517,#402518,#402519,#402520,#402521,#402522,#402523,
#402524,#402525,#402526),.UNSPECIFIED.,.F.,.F.,(4,3,3,3,3,3,3,3,3,3,3,4),
(2.16840434497101E-19,2.09623992729457E-6,3.17176647120237E-6,4.8263618194444E-6,
5.01000917339961E-6,6.13126454147503E-6,8.6048665028887E-6,9.21144281170501E-6,
1.24722301135885E-5,1.42666454787857E-5,2.04670653756818E-5,2.08026438176804E-5),
 .UNSPECIFIED.);
#25645=B_SPLINE_CURVE_WITH_KNOTS('',3,(#402527,#402528,#402529,#402530),
 .UNSPECIFIED.,.F.,.F.,(4,4),(0.,0.000109384345496908),.UNSPECIFIED.);
#25646=B_SPLINE_CURVE_WITH_KNOTS('',3,(#402635,#402636,#402637,#402638),
 .UNSPECIFIED.,.F.,.F.,(4,4),(0.,9.54361881492175E-5),.UNSPECIFIED.);
#25647=B_SPLINE_CURVE_WITH_KNOTS('',3,(#402643,#402644,#402645,#402646,
#402647,#402648,#402649),.UNSPECIFIED.,.F.,.F.,(4,3,4),(0.,4.41069704323469E-5,
0.000113970027818833),.UNSPECIFIED.);
#25648=B_SPLINE_CURVE_WITH_KNOTS('',3,(#402655,#402656,#402657,#402658),
 .UNSPECIFIED.,.F.,.F.,(4,4),(4.33680868994202E-19,9.54361881492175E-5),
 .UNSPECIFIED.);
#25649=B_SPLINE_CURVE_WITH_KNOTS('',3,(#402662,#402663,#402664,#402665,
#402666,#402667,#402668),.UNSPECIFIED.,.F.,.F.,(4,3,4),(0.,6.98630244191489E-5,
0.000113969974038089),.UNSPECIFIED.);
#25650=B_SPLINE_CURVE_WITH_KNOTS('',3,(#402671,#402672,#402673,#402674,
#402675,#402676,#402677,#402678,#402679,#402680,#402681,#402682,#402683,
#402684,#402685,#402686,#402687,#402688,#402689,#402690,#402691,#402692,
#402693,#402694,#402695,#402696,#402697,#402698,#402699,#402700,#402701,
#402702,#402703,#402704,#402705,#402706,#402707,#402708,#402709,#402710,
#402711,#402712,#402713,#402714,#402715,#402716,#402717,#402718,#402719),
 .UNSPECIFIED.,.F.,.F.,(4,3,3,3,3,3,3,3,3,3,3,3,3,3,3,3,4),(0.,1.53100299373418E-6,
4.52554775679361E-6,7.01151246291622E-6,9.26752933800728E-6,1.03084066197175E-5,
1.17138990826863E-5,1.22284894984073E-5,1.30315035324818E-5,1.38363728497812E-5,
1.40464197777495E-5,1.54597749564641E-5,1.62073588704069E-5,1.92092968713019E-5,
1.95234416882557E-5,2.37637844577584E-5,2.61487188977265E-5),
 .UNSPECIFIED.);
#25651=B_SPLINE_CURVE_WITH_KNOTS('',3,(#402734,#402735,#402736,#402737,
#402738,#402739,#402740,#402741,#402742,#402743,#402744,#402745,#402746,
#402747,#402748,#402749,#402750,#402751,#402752,#402753,#402754,#402755,
#402756,#402757,#402758,#402759,#402760,#402761,#402762,#402763,#402764),
 .UNSPECIFIED.,.F.,.F.,(4,3,3,3,3,3,3,3,3,3,4),(0.,3.95507910398474E-6,
7.53768426604196E-6,1.1990453333535E-5,1.40475043392584E-5,1.51452104275962E-5,
1.67866272814233E-5,1.69621513005357E-5,1.8133831546071E-5,1.98906334656502E-5,
2.06132424588241E-5),.UNSPECIFIED.);
#25652=B_SPLINE_CURVE_WITH_KNOTS('',3,(#402767,#402768,#402769,#402770),
 .UNSPECIFIED.,.F.,.F.,(4,4),(4.33680868994202E-19,0.00010938435327491),
 .UNSPECIFIED.);
#25653=B_SPLINE_CURVE_WITH_KNOTS('',3,(#402797,#402798,#402799,#402800,
#402801,#402802,#402803,#402804,#402805,#402806,#402807,#402808,#402809,
#402810,#402811,#402812,#402813,#402814,#402815,#402816,#402817,#402818,
#402819,#402820,#402821,#402822,#402823,#402824,#402825,#402826,#402827,
#402828,#402829,#402830),.UNSPECIFIED.,.F.,.F.,(4,3,3,3,3,3,3,3,3,3,3,4),
(0.,2.09623992729435E-6,3.17176647120212E-6,4.82636181943321E-6,5.01000917339988E-6,
6.13126454147513E-6,8.60486650288861E-6,9.21144281170496E-6,1.24722301136148E-5,
1.4266645478786E-5,2.04670653756914E-5,2.08026438176811E-5),
 .UNSPECIFIED.);
#25654=B_SPLINE_CURVE_WITH_KNOTS('',3,(#402831,#402832,#402833,#402834),
 .UNSPECIFIED.,.F.,.F.,(4,4),(0.,0.000109384345496909),.UNSPECIFIED.);
#25655=B_SPLINE_CURVE_WITH_KNOTS('',3,(#402939,#402940,#402941,#402942),
 .UNSPECIFIED.,.F.,.F.,(4,4),(0.,9.54361881492174E-5),.UNSPECIFIED.);
#25656=B_SPLINE_CURVE_WITH_KNOTS('',3,(#402947,#402948,#402949,#402950,
#402951,#402952,#402953),.UNSPECIFIED.,.F.,.F.,(4,3,4),(0.,4.41069704323467E-5,
0.000113970027818833),.UNSPECIFIED.);
#25657=B_SPLINE_CURVE_WITH_KNOTS('',3,(#402959,#402960,#402961,#402962),
 .UNSPECIFIED.,.F.,.F.,(4,4),(4.33680868994202E-19,9.54361881492178E-5),
 .UNSPECIFIED.);
#25658=B_SPLINE_CURVE_WITH_KNOTS('',3,(#402966,#402967,#402968,#402969,
#402970,#402971,#402972),.UNSPECIFIED.,.F.,.F.,(4,3,4),(0.,6.98630244191492E-5,
0.000113969974038089),.UNSPECIFIED.);
#25659=B_SPLINE_CURVE_WITH_KNOTS('',3,(#402975,#402976,#402977,#402978,
#402979,#402980,#402981,#402982,#402983,#402984,#402985,#402986,#402987,
#402988,#402989,#402990,#402991,#402992,#402993,#402994,#402995,#402996,
#402997,#402998,#402999,#403000,#403001,#403002,#403003,#403004,#403005,
#403006,#403007,#403008,#403009,#403010,#403011,#403012,#403013,#403014,
#403015,#403016,#403017,#403018,#403019,#403020,#403021,#403022,#403023),
 .UNSPECIFIED.,.F.,.F.,(4,3,3,3,3,3,3,3,3,3,3,3,3,3,3,3,4),(0.,1.53100299373391E-6,
4.52554775679138E-6,7.01151246291585E-6,9.2675293380002E-6,1.03084066197173E-5,
1.17138990826862E-5,1.22284894984076E-5,1.30315035324817E-5,1.38363728497813E-5,
1.40464197777495E-5,1.54597749564641E-5,1.6207358870407E-5,1.92092968713447E-5,
1.95234416882558E-5,2.37637844577641E-5,2.61487188977268E-5),
 .UNSPECIFIED.);
#25660=B_SPLINE_CURVE_WITH_KNOTS('',3,(#403038,#403039,#403040,#403041,
#403042,#403043,#403044,#403045,#403046,#403047,#403048,#403049,#403050,
#403051,#403052,#403053,#403054,#403055,#403056,#403057,#403058,#403059,
#403060,#403061,#403062,#403063,#403064,#403065,#403066,#403067,#403068),
 .UNSPECIFIED.,.F.,.F.,(4,3,3,3,3,3,3,3,3,3,4),(0.,3.95507910399186E-6,
7.53768426604196E-6,1.1990453333535E-5,1.40475043392585E-5,1.51452104275965E-5,
1.67866272814145E-5,1.69621513005358E-5,1.81338315460712E-5,1.9890633465651E-5,
2.06132424588246E-5),.UNSPECIFIED.);
#25661=B_SPLINE_CURVE_WITH_KNOTS('',3,(#403071,#403072,#403073,#403074),
 .UNSPECIFIED.,.F.,.F.,(4,4),(4.47028007668187E-19,0.00010938435327491),
 .UNSPECIFIED.);
#25662=B_SPLINE_CURVE_WITH_KNOTS('',3,(#403101,#403102,#403103,#403104,
#403105,#403106,#403107,#403108,#403109,#403110,#403111,#403112,#403113,
#403114,#403115,#403116,#403117,#403118,#403119,#403120,#403121,#403122,
#403123,#403124,#403125,#403126,#403127,#403128,#403129,#403130,#403131,
#403132,#403133,#403134),.UNSPECIFIED.,.F.,.F.,(4,3,3,3,3,3,3,3,3,3,3,4),
(1.0842021724855E-19,2.09623992729434E-6,3.17176647120229E-6,4.82636181944625E-6,
5.01000917339952E-6,6.13126454147493E-6,8.6048665028886E-6,9.2114428117048E-6,
1.24722301135969E-5,1.42666454787854E-5,2.04670653756842E-5,2.08026438176801E-5),
 .UNSPECIFIED.);
#25663=B_SPLINE_CURVE_WITH_KNOTS('',3,(#403135,#403136,#403137,#403138),
 .UNSPECIFIED.,.F.,.F.,(4,4),(0.,0.000109384345496909),.UNSPECIFIED.);
#25664=B_SPLINE_CURVE_WITH_KNOTS('',3,(#403243,#403244,#403245,#403246),
 .UNSPECIFIED.,.F.,.F.,(4,4),(0.,9.54361881492175E-5),.UNSPECIFIED.);
#25665=B_SPLINE_CURVE_WITH_KNOTS('',3,(#403251,#403252,#403253,#403254,
#403255,#403256,#403257),.UNSPECIFIED.,.F.,.F.,(4,3,4),(0.,4.41069704323469E-5,
0.000113970027818833),.UNSPECIFIED.);
#25666=B_SPLINE_CURVE_WITH_KNOTS('',3,(#403263,#403264,#403265,#403266),
 .UNSPECIFIED.,.F.,.F.,(4,4),(4.47028007668187E-19,9.54361881492181E-5),
 .UNSPECIFIED.);
#25667=B_SPLINE_CURVE_WITH_KNOTS('',3,(#403270,#403271,#403272,#403273,
#403274,#403275,#403276),.UNSPECIFIED.,.F.,.F.,(4,3,4),(0.,6.98630244191488E-5,
0.000113969974038089),.UNSPECIFIED.);
#25668=B_SPLINE_CURVE_WITH_KNOTS('',3,(#403279,#403280,#403281,#403282,
#403283,#403284,#403285,#403286,#403287,#403288,#403289,#403290,#403291,
#403292,#403293,#403294,#403295,#403296,#403297,#403298,#403299,#403300,
#403301,#403302,#403303,#403304,#403305,#403306,#403307,#403308,#403309,
#403310,#403311,#403312,#403313,#403314,#403315,#403316,#403317,#403318,
#403319,#403320,#403321,#403322,#403323,#403324,#403325,#403326,#403327),
 .UNSPECIFIED.,.F.,.F.,(4,3,3,3,3,3,3,3,3,3,3,3,3,3,3,3,4),(0.,1.53100299373415E-6,
4.52554775679494E-6,7.01151246291608E-6,9.26752933799504E-6,1.03084066197173E-5,
1.17138990826863E-5,1.22284894984074E-5,1.30315035324818E-5,1.38363728497813E-5,
1.40464197777495E-5,1.5459774956464E-5,1.62073588704069E-5,1.92092968712925E-5,
1.95234416882555E-5,2.37637844577608E-5,2.61487188977261E-5),
 .UNSPECIFIED.);
#25669=B_SPLINE_CURVE_WITH_KNOTS('',3,(#403342,#403343,#403344,#403345,
#403346,#403347,#403348,#403349,#403350,#403351,#403352,#403353,#403354,
#403355,#403356,#403357,#403358,#403359,#403360,#403361,#403362,#403363,
#403364,#403365,#403366,#403367,#403368,#403369,#403370,#403371,#403372),
 .UNSPECIFIED.,.F.,.F.,(4,3,3,3,3,3,3,3,3,3,4),(0.,3.95507910398488E-6,
7.53768426604197E-6,1.19904533335349E-5,1.40475043392583E-5,1.51452104275962E-5,
1.67866272814071E-5,1.69621513005355E-5,1.81338315460707E-5,1.98906334656513E-5,
2.06132424588239E-5),.UNSPECIFIED.);
#25670=B_SPLINE_CURVE_WITH_KNOTS('',3,(#403375,#403376,#403377,#403378),
 .UNSPECIFIED.,.F.,.F.,(4,4),(4.47028007668187E-19,0.00010938435327491),
 .UNSPECIFIED.);
#25671=B_SPLINE_CURVE_WITH_KNOTS('',3,(#403405,#403406,#403407,#403408,
#403409,#403410,#403411,#403412,#403413,#403414,#403415,#403416,#403417,
#403418,#403419,#403420,#403421,#403422,#403423,#403424,#403425,#403426,
#403427,#403428,#403429,#403430,#403431,#403432,#403433,#403434,#403435,
#403436,#403437,#403438),.UNSPECIFIED.,.F.,.F.,(4,3,3,3,3,3,3,3,3,3,3,4),
(1.0842021724855E-19,2.09623992729452E-6,3.17176647120229E-6,4.82636181942986E-6,
5.01000917339994E-6,6.13126454147503E-6,8.60486650288877E-6,9.21144281170519E-6,
1.24722301135898E-5,1.4266645478786E-5,2.04670653756804E-5,2.08026438176811E-5),
 .UNSPECIFIED.);
#25672=B_SPLINE_CURVE_WITH_KNOTS('',3,(#403439,#403440,#403441,#403442),
 .UNSPECIFIED.,.F.,.F.,(4,4),(0.,0.000109384345496908),.UNSPECIFIED.);
#25673=B_SPLINE_CURVE_WITH_KNOTS('',3,(#403547,#403548,#403549,#403550),
 .UNSPECIFIED.,.F.,.F.,(4,4),(0.,9.54361881492177E-5),.UNSPECIFIED.);
#25674=B_SPLINE_CURVE_WITH_KNOTS('',3,(#403555,#403556,#403557,#403558,
#403559,#403560,#403561),.UNSPECIFIED.,.F.,.F.,(4,3,4),(0.,4.4106970432347E-5,
0.000113970027818834),.UNSPECIFIED.);
#25675=B_SPLINE_CURVE_WITH_KNOTS('',3,(#403567,#403568,#403569,#403570),
 .UNSPECIFIED.,.F.,.F.,(4,4),(4.37055868292169E-19,9.54361881492178E-5),
 .UNSPECIFIED.);
#25676=B_SPLINE_CURVE_WITH_KNOTS('',3,(#403574,#403575,#403576,#403577,
#403578,#403579,#403580),.UNSPECIFIED.,.F.,.F.,(4,3,4),(0.,6.98630244191491E-5,
0.000113969974038089),.UNSPECIFIED.);
#25677=B_SPLINE_CURVE_WITH_KNOTS('',3,(#403583,#403584,#403585,#403586,
#403587,#403588,#403589,#403590,#403591,#403592,#403593,#403594,#403595,
#403596,#403597,#403598,#403599,#403600,#403601,#403602,#403603,#403604,
#403605,#403606,#403607,#403608,#403609,#403610,#403611,#403612,#403613,
#403614,#403615,#403616,#403617,#403618,#403619,#403620,#403621,#403622,
#403623,#403624,#403625,#403626,#403627,#403628,#403629,#403630,#403631),
 .UNSPECIFIED.,.F.,.F.,(4,3,3,3,3,3,3,3,3,3,3,3,3,3,3,3,4),(0.,1.53100299373428E-6,
4.52554775678673E-6,7.01151246291611E-6,9.2675293380117E-6,1.03084066197174E-5,
1.17138990826861E-5,1.22284894984074E-5,1.30315035324817E-5,1.38363728497813E-5,
1.40464197777495E-5,1.54597749564639E-5,1.62073588704068E-5,1.92092968713227E-5,
1.95234416882553E-5,2.37637844577601E-5,2.61487188977258E-5),
 .UNSPECIFIED.);
#25678=B_SPLINE_CURVE_WITH_KNOTS('',3,(#403646,#403647,#403648,#403649,
#403650,#403651,#403652,#403653,#403654,#403655,#403656,#403657,#403658,
#403659,#403660,#403661,#403662,#403663,#403664,#403665,#403666,#403667,
#403668,#403669,#403670,#403671,#403672,#403673,#403674,#403675,#403676),
 .UNSPECIFIED.,.F.,.F.,(4,3,3,3,3,3,3,3,3,3,4),(0.,3.95507910397771E-6,
7.53768426604201E-6,1.1990453333535E-5,1.40475043392585E-5,1.51452104275964E-5,
1.67866272814242E-5,1.69621513005359E-5,1.81338315460713E-5,1.98906334656549E-5,
2.06132424588246E-5),.UNSPECIFIED.);
#25679=B_SPLINE_CURVE_WITH_KNOTS('',3,(#403679,#403680,#403681,#403682),
 .UNSPECIFIED.,.F.,.F.,(4,4),(4.47028007668187E-19,0.00010938435327491),
 .UNSPECIFIED.);
#25680=B_SPLINE_CURVE_WITH_KNOTS('',3,(#403709,#403710,#403711,#403712,
#403713,#403714,#403715,#403716,#403717,#403718,#403719,#403720,#403721,
#403722,#403723,#403724,#403725,#403726,#403727,#403728,#403729,#403730,
#403731,#403732,#403733,#403734,#403735,#403736,#403737,#403738,#403739,
#403740,#403741,#403742),.UNSPECIFIED.,.F.,.F.,(4,3,3,3,3,3,3,3,3,3,3,4),
(3.25260651745651E-19,2.09623992729428E-6,3.17176647120214E-6,4.82636181944364E-6,
5.01000917339949E-6,6.13126454147488E-6,8.60486650288841E-6,9.21144281170483E-6,
1.24722301135897E-5,1.42666454787855E-5,2.04670653756992E-5,2.08026438176802E-5),
 .UNSPECIFIED.);
#25681=B_SPLINE_CURVE_WITH_KNOTS('',3,(#403743,#403744,#403745,#403746),
 .UNSPECIFIED.,.F.,.F.,(4,4),(0.,0.000109384345496908),.UNSPECIFIED.);
#25682=B_SPLINE_CURVE_WITH_KNOTS('',3,(#403851,#403852,#403853,#403854),
 .UNSPECIFIED.,.F.,.F.,(4,4),(0.,9.54361881492177E-5),.UNSPECIFIED.);
#25683=B_SPLINE_CURVE_WITH_KNOTS('',3,(#403859,#403860,#403861,#403862,
#403863,#403864,#403865),.UNSPECIFIED.,.F.,.F.,(4,3,4),(0.,4.4106970432347E-5,
0.000113970027818834),.UNSPECIFIED.);
#25684=B_SPLINE_CURVE_WITH_KNOTS('',3,(#403871,#403872,#403873,#403874),
 .UNSPECIFIED.,.F.,.F.,(4,4),(4.47028007668187E-19,9.54361881492176E-5),
 .UNSPECIFIED.);
#25685=B_SPLINE_CURVE_WITH_KNOTS('',3,(#403878,#403879,#403880,#403881,
#403882,#403883,#403884),.UNSPECIFIED.,.F.,.F.,(4,3,4),(0.,6.98630244191491E-5,
0.000113969974038089),.UNSPECIFIED.);
#25686=B_SPLINE_CURVE_WITH_KNOTS('',3,(#403887,#403888,#403889,#403890,
#403891,#403892,#403893,#403894,#403895,#403896,#403897,#403898,#403899,
#403900,#403901,#403902,#403903,#403904,#403905,#403906,#403907,#403908,
#403909,#403910,#403911,#403912,#403913,#403914,#403915,#403916,#403917,
#403918,#403919,#403920,#403921,#403922,#403923,#403924,#403925,#403926,
#403927,#403928,#403929,#403930,#403931,#403932,#403933,#403934,#403935),
 .UNSPECIFIED.,.F.,.F.,(4,3,3,3,3,3,3,3,3,3,3,3,3,3,3,3,4),(0.,1.53100299373417E-6,
4.52554775678891E-6,7.01151246291613E-6,9.26752933800967E-6,1.03084066197174E-5,
1.17138990826861E-5,1.22284894984074E-5,1.30315035324817E-5,1.38363728497813E-5,
1.40464197777495E-5,1.54597749564641E-5,1.6207358870407E-5,1.92092968712626E-5,
1.95234416882557E-5,2.37637844577605E-5,2.61487188977263E-5),
 .UNSPECIFIED.);
#25687=B_SPLINE_CURVE_WITH_KNOTS('',3,(#403950,#403951,#403952,#403953,
#403954,#403955,#403956,#403957,#403958,#403959,#403960,#403961,#403962,
#403963,#403964,#403965,#403966,#403967,#403968,#403969,#403970,#403971,
#403972,#403973,#403974,#403975,#403976,#403977,#403978,#403979,#403980),
 .UNSPECIFIED.,.F.,.F.,(4,3,3,3,3,3,3,3,3,3,4),(0.,3.95507910397136E-6,
7.53768426604194E-6,1.1990453333535E-5,1.40475043392585E-5,1.51452104275964E-5,
1.67866272814088E-5,1.69621513005357E-5,1.81338315460711E-5,1.98906334656549E-5,
2.06132424588245E-5),.UNSPECIFIED.);
#25688=B_SPLINE_CURVE_WITH_KNOTS('',3,(#403983,#403984,#403985,#403986),
 .UNSPECIFIED.,.F.,.F.,(4,4),(4.63171371119878E-19,0.00010938435327491),
 .UNSPECIFIED.);
#25689=B_SPLINE_CURVE_WITH_KNOTS('',3,(#404013,#404014,#404015,#404016,
#404017,#404018,#404019,#404020,#404021,#404022,#404023,#404024,#404025,
#404026,#404027,#404028,#404029,#404030,#404031,#404032,#404033,#404034,
#404035,#404036,#404037,#404038,#404039,#404040,#404041,#404042,#404043,
#404044,#404045,#404046),.UNSPECIFIED.,.F.,.F.,(4,3,3,3,3,3,3,3,3,3,3,4),
(1.0842021724855E-19,2.09623992729439E-6,3.17176647120223E-6,4.82636181943523E-6,
5.01000917339971E-6,6.13126454147506E-6,8.60486650288868E-6,9.21144281170512E-6,
1.24722301135849E-5,1.42666454787859E-5,2.04670653756996E-5,2.08026438176807E-5),
 .UNSPECIFIED.);
#25690=B_SPLINE_CURVE_WITH_KNOTS('',3,(#404047,#404048,#404049,#404050),
 .UNSPECIFIED.,.F.,.F.,(4,4),(0.,0.000109384345496908),.UNSPECIFIED.);
#25691=B_SPLINE_CURVE_WITH_KNOTS('',3,(#404155,#404156,#404157,#404158),
 .UNSPECIFIED.,.F.,.F.,(4,4),(0.,9.54361881492175E-5),.UNSPECIFIED.);
#25692=B_SPLINE_CURVE_WITH_KNOTS('',3,(#404163,#404164,#404165,#404166,
#404167,#404168,#404169),.UNSPECIFIED.,.F.,.F.,(4,3,4),(0.,4.41069704323469E-5,
0.000113970027818833),.UNSPECIFIED.);
#25693=B_SPLINE_CURVE_WITH_KNOTS('',3,(#404175,#404176,#404177,#404178),
 .UNSPECIFIED.,.F.,.F.,(4,4),(4.47028007668187E-19,9.54361881492176E-5),
 .UNSPECIFIED.);
#25694=B_SPLINE_CURVE_WITH_KNOTS('',3,(#404182,#404183,#404184,#404185,
#404186,#404187,#404188),.UNSPECIFIED.,.F.,.F.,(4,3,4),(0.,6.98630244191494E-5,
0.000113969974038089),.UNSPECIFIED.);
#25695=B_SPLINE_CURVE_WITH_KNOTS('',3,(#404191,#404192,#404193,#404194,
#404195,#404196,#404197,#404198,#404199,#404200,#404201,#404202,#404203,
#404204,#404205,#404206,#404207,#404208,#404209,#404210,#404211,#404212,
#404213,#404214,#404215,#404216,#404217,#404218,#404219,#404220,#404221,
#404222,#404223,#404224,#404225,#404226,#404227,#404228,#404229,#404230,
#404231,#404232,#404233,#404234,#404235,#404236,#404237,#404238,#404239),
 .UNSPECIFIED.,.F.,.F.,(4,3,3,3,3,3,3,3,3,3,3,3,3,3,3,3,4),(0.,1.53100299373404E-6,
4.52554775679048E-6,7.01151246291601E-6,9.26752933800589E-6,1.03084066197173E-5,
1.17138990826862E-5,1.22284894984074E-5,1.30315035324817E-5,1.38363728497813E-5,
1.40464197777495E-5,1.5459774956464E-5,1.62073588704068E-5,1.92092968712522E-5,
1.95234416882554E-5,2.37637844577637E-5,2.61487188977262E-5),
 .UNSPECIFIED.);
#25696=B_SPLINE_CURVE_WITH_KNOTS('',3,(#404254,#404255,#404256,#404257,
#404258,#404259,#404260,#404261,#404262,#404263,#404264,#404265,#404266,
#404267,#404268,#404269,#404270,#404271,#404272,#404273,#404274,#404275,
#404276,#404277,#404278,#404279,#404280,#404281,#404282,#404283,#404284),
 .UNSPECIFIED.,.F.,.F.,(4,3,3,3,3,3,3,3,3,3,4),(0.,3.95507910397345E-6,
7.53768426604206E-6,1.19904533335351E-5,1.40475043392586E-5,1.51452104275965E-5,
1.67866272814209E-5,1.69621513005358E-5,1.81338315460712E-5,1.98906334656557E-5,
2.06132424588245E-5),.UNSPECIFIED.);
#25697=B_SPLINE_CURVE_WITH_KNOTS('',3,(#404287,#404288,#404289,#404290),
 .UNSPECIFIED.,.F.,.F.,(4,4),(4.73369422993816E-19,0.00010938435327491),
 .UNSPECIFIED.);
#25698=B_SPLINE_CURVE_WITH_KNOTS('',3,(#404317,#404318,#404319,#404320,
#404321,#404322,#404323,#404324,#404325,#404326,#404327,#404328,#404329,
#404330,#404331,#404332,#404333,#404334,#404335,#404336,#404337,#404338,
#404339,#404340,#404341,#404342,#404343,#404344,#404345,#404346,#404347,
#404348,#404349,#404350),.UNSPECIFIED.,.F.,.F.,(4,3,3,3,3,3,3,3,3,3,3,4),
(1.35525271560688E-19,2.09623992729445E-6,3.17176647120224E-6,4.82636181943226E-6,
5.01000917339961E-6,6.13126454147493E-6,8.6048665028883E-6,9.21144281170468E-6,
1.24722301135904E-5,1.42666454787847E-5,2.04670653757035E-5,2.08026438176787E-5),
 .UNSPECIFIED.);
#25699=B_SPLINE_CURVE_WITH_KNOTS('',3,(#404351,#404352,#404353,#404354),
 .UNSPECIFIED.,.F.,.F.,(4,4),(0.,0.000109384345496908),.UNSPECIFIED.);
#25700=B_SPLINE_CURVE_WITH_KNOTS('',3,(#404459,#404460,#404461,#404462),
 .UNSPECIFIED.,.F.,.F.,(4,4),(0.,9.54361881492174E-5),.UNSPECIFIED.);
#25701=B_SPLINE_CURVE_WITH_KNOTS('',3,(#404467,#404468,#404469,#404470,
#404471,#404472,#404473),.UNSPECIFIED.,.F.,.F.,(4,3,4),(0.,4.41069704323469E-5,
0.000113970027818833),.UNSPECIFIED.);
#25702=B_SPLINE_CURVE_WITH_KNOTS('',3,(#404479,#404480,#404481,#404482),
 .UNSPECIFIED.,.F.,.F.,(4,4),(4.52388553334502E-19,9.54361881492177E-5),
 .UNSPECIFIED.);
#25703=B_SPLINE_CURVE_WITH_KNOTS('',3,(#404486,#404487,#404488,#404489,
#404490,#404491,#404492),.UNSPECIFIED.,.F.,.F.,(4,3,4),(8.470329472543E-22,
6.9863024419149E-5,0.000113969974038089),.UNSPECIFIED.);
#25704=B_SPLINE_CURVE_WITH_KNOTS('',3,(#404495,#404496,#404497,#404498,
#404499,#404500,#404501,#404502,#404503,#404504,#404505,#404506,#404507,
#404508,#404509,#404510,#404511,#404512,#404513,#404514,#404515,#404516,
#404517,#404518,#404519,#404520,#404521,#404522,#404523,#404524,#404525,
#404526,#404527,#404528,#404529,#404530,#404531,#404532,#404533,#404534,
#404535,#404536,#404537,#404538,#404539,#404540,#404541,#404542,#404543),
 .UNSPECIFIED.,.F.,.F.,(4,3,3,3,3,3,3,3,3,3,3,3,3,3,3,3,4),(0.,1.53100299373414E-6,
4.52554775678511E-6,7.01151246291606E-6,9.267529338009E-6,1.03084066197173E-5,
1.17138990826862E-5,1.22284894984074E-5,1.30315035324817E-5,1.38363728497813E-5,
1.40464197777495E-5,1.5459774956464E-5,1.62073588704069E-5,1.92092968712803E-5,
1.95234416882555E-5,2.37637844577586E-5,2.61487188977262E-5),
 .UNSPECIFIED.);
#25705=B_SPLINE_CURVE_WITH_KNOTS('',3,(#404558,#404559,#404560,#404561,
#404562,#404563,#404564,#404565,#404566,#404567,#404568,#404569,#404570,
#404571,#404572,#404573,#404574,#404575,#404576,#404577,#404578,#404579,
#404580,#404581,#404582,#404583,#404584,#404585,#404586,#404587,#404588),
 .UNSPECIFIED.,.F.,.F.,(4,3,3,3,3,3,3,3,3,3,4),(0.,3.9550791039786E-6,7.53768426604197E-6,
1.1990453333535E-5,1.40475043392586E-5,1.51452104275964E-5,1.67866272814111E-5,
1.69621513005358E-5,1.81338315460712E-5,1.98906334656562E-5,2.06132424588244E-5),
 .UNSPECIFIED.);
#25706=B_SPLINE_CURVE_WITH_KNOTS('',3,(#404591,#404592,#404593,#404594),
 .UNSPECIFIED.,.F.,.F.,(4,4),(4.78962492688793E-19,0.00010938435327491),
 .UNSPECIFIED.);
#25707=B_SPLINE_CURVE_WITH_KNOTS('',3,(#404621,#404622,#404623,#404624,
#404625,#404626,#404627,#404628,#404629,#404630,#404631,#404632,#404633,
#404634,#404635,#404636,#404637,#404638,#404639,#404640,#404641,#404642,
#404643,#404644,#404645,#404646,#404647,#404648,#404649,#404650,#404651,
#404652,#404653,#404654),.UNSPECIFIED.,.F.,.F.,(4,3,3,3,3,3,3,3,3,3,3,4),
(1.35525271560688E-19,2.0962399272944E-6,3.17176647120221E-6,4.82636181943873E-6,
5.01000917339963E-6,6.13126454147497E-6,8.6048665028886E-6,9.21144281170497E-6,
1.24722301136065E-5,1.42666454787857E-5,2.04670653756822E-5,2.08026438176805E-5),
 .UNSPECIFIED.);
#25708=B_SPLINE_CURVE_WITH_KNOTS('',3,(#404655,#404656,#404657,#404658),
 .UNSPECIFIED.,.F.,.F.,(4,4),(0.,0.000109384345496908),.UNSPECIFIED.);
#25709=B_SPLINE_CURVE_WITH_KNOTS('',3,(#404763,#404764,#404765,#404766),
 .UNSPECIFIED.,.F.,.F.,(4,4),(0.,9.54361881492175E-5),.UNSPECIFIED.);
#25710=B_SPLINE_CURVE_WITH_KNOTS('',3,(#404771,#404772,#404773,#404774,
#404775,#404776,#404777),.UNSPECIFIED.,.F.,.F.,(4,3,4),(0.,4.41069704323468E-5,
0.000113970027818834),.UNSPECIFIED.);
#25711=B_SPLINE_CURVE_WITH_KNOTS('',3,(#404783,#404784,#404785,#404786),
 .UNSPECIFIED.,.F.,.F.,(4,4),(4.5436350575631E-19,9.54361881492176E-5),
 .UNSPECIFIED.);
#25712=B_SPLINE_CURVE_WITH_KNOTS('',3,(#404790,#404791,#404792,#404793,
#404794,#404795,#404796),.UNSPECIFIED.,.F.,.F.,(4,3,4),(0.,6.9863024419149E-5,
0.000113969974038089),.UNSPECIFIED.);
#25713=B_SPLINE_CURVE_WITH_KNOTS('',3,(#404799,#404800,#404801,#404802,
#404803,#404804,#404805,#404806,#404807,#404808,#404809,#404810,#404811,
#404812,#404813,#404814,#404815,#404816,#404817,#404818,#404819,#404820,
#404821,#404822,#404823,#404824,#404825,#404826,#404827,#404828,#404829,
#404830,#404831,#404832,#404833,#404834,#404835,#404836,#404837,#404838,
#404839,#404840,#404841,#404842,#404843,#404844,#404845,#404846,#404847),
 .UNSPECIFIED.,.F.,.F.,(4,3,3,3,3,3,3,3,3,3,3,3,3,3,3,3,4),(0.,1.53100299373415E-6,
4.52554775679134E-6,7.01151246291607E-6,9.26752933800752E-6,1.03084066197173E-5,
1.17138990826861E-5,1.22284894984074E-5,1.30315035324817E-5,1.38363728497812E-5,
1.40464197777495E-5,1.5459774956464E-5,1.62073588704068E-5,1.92092968713003E-5,
1.95234416882555E-5,2.37637844577607E-5,2.61487188977258E-5),
 .UNSPECIFIED.);
#25714=B_SPLINE_CURVE_WITH_KNOTS('',3,(#404862,#404863,#404864,#404865,
#404866,#404867,#404868,#404869,#404870,#404871,#404872,#404873,#404874,
#404875,#404876,#404877,#404878,#404879,#404880,#404881,#404882,#404883,
#404884,#404885,#404886,#404887,#404888,#404889,#404890,#404891,#404892),
 .UNSPECIFIED.,.F.,.F.,(4,3,3,3,3,3,3,3,3,3,4),(0.,3.95507910399298E-6,
7.53768426604202E-6,1.19904533335351E-5,1.40475043392586E-5,1.51452104275965E-5,
1.67866272814125E-5,1.69621513005359E-5,1.81338315460713E-5,1.9890633465649E-5,
2.06132424588247E-5),.UNSPECIFIED.);
#25715=B_SPLINE_CURVE_WITH_KNOTS('',3,(#404895,#404896,#404897,#404898),
 .UNSPECIFIED.,.F.,.F.,(4,4),(4.84869951806108E-19,0.00010938435327491),
 .UNSPECIFIED.);
#25716=B_SPLINE_CURVE_WITH_KNOTS('',3,(#404925,#404926,#404927,#404928,
#404929,#404930,#404931,#404932,#404933,#404934,#404935,#404936,#404937,
#404938,#404939,#404940,#404941,#404942,#404943,#404944,#404945,#404946,
#404947,#404948,#404949,#404950,#404951,#404952,#404953,#404954,#404955,
#404956,#404957,#404958),.UNSPECIFIED.,.F.,.F.,(4,3,3,3,3,3,3,3,3,3,3,4),
(1.35525271560688E-19,2.09623992729443E-6,3.17176647120225E-6,4.8263618194329E-6,
5.01000917339965E-6,6.13126454147501E-6,8.60486650288862E-6,9.21144281170501E-6,
1.24722301135748E-5,1.42666454787858E-5,2.04670653757036E-5,2.08026438176807E-5),
 .UNSPECIFIED.);
#25717=B_SPLINE_CURVE_WITH_KNOTS('',3,(#404959,#404960,#404961,#404962),
 .UNSPECIFIED.,.F.,.F.,(4,4),(0.,0.000109384345496908),.UNSPECIFIED.);
#25718=B_SPLINE_CURVE_WITH_KNOTS('',3,(#405067,#405068,#405069,#405070),
 .UNSPECIFIED.,.F.,.F.,(4,4),(0.,9.54361881492173E-5),.UNSPECIFIED.);
#25719=B_SPLINE_CURVE_WITH_KNOTS('',3,(#405075,#405076,#405077,#405078,
#405079,#405080,#405081),.UNSPECIFIED.,.F.,.F.,(4,3,4),(0.,4.41069704323472E-5,
0.000113970027818833),.UNSPECIFIED.);
#25720=B_SPLINE_CURVE_WITH_KNOTS('',3,(#405087,#405088,#405089,#405090),
 .UNSPECIFIED.,.F.,.F.,(4,4),(4.63171371119878E-19,9.54361881492176E-5),
 .UNSPECIFIED.);
#25721=B_SPLINE_CURVE_WITH_KNOTS('',3,(#405094,#405095,#405096,#405097,
#405098,#405099,#405100),.UNSPECIFIED.,.F.,.F.,(4,3,4),(0.,6.98630244191491E-5,
0.000113969974038089),.UNSPECIFIED.);
#25722=B_SPLINE_CURVE_WITH_KNOTS('',3,(#405103,#405104,#405105,#405106,
#405107,#405108,#405109,#405110,#405111,#405112,#405113,#405114,#405115,
#405116,#405117,#405118,#405119,#405120,#405121,#405122,#405123,#405124,
#405125,#405126,#405127,#405128,#405129,#405130,#405131,#405132,#405133,
#405134,#405135,#405136,#405137,#405138,#405139,#405140,#405141,#405142,
#405143,#405144,#405145,#405146,#405147,#405148,#405149,#405150,#405151),
 .UNSPECIFIED.,.F.,.F.,(4,3,3,3,3,3,3,3,3,3,3,3,3,3,3,3,4),(0.,1.53100299373408E-6,
4.52554775679546E-6,7.01151246291603E-6,9.26752933800014E-6,1.03084066197173E-5,
1.17138990826862E-5,1.22284894984074E-5,1.30315035324817E-5,1.38363728497812E-5,
1.40464197777494E-5,1.54597749564638E-5,1.62073588704067E-5,1.92092968712711E-5,
1.95234416882554E-5,2.37637844577557E-5,2.6148718897726E-5),
 .UNSPECIFIED.);
#25723=B_SPLINE_CURVE_WITH_KNOTS('',3,(#405166,#405167,#405168,#405169,
#405170,#405171,#405172,#405173,#405174,#405175,#405176,#405177,#405178,
#405179,#405180,#405181,#405182,#405183,#405184,#405185,#405186,#405187,
#405188,#405189,#405190,#405191,#405192,#405193,#405194,#405195,#405196),
 .UNSPECIFIED.,.F.,.F.,(4,3,3,3,3,3,3,3,3,3,4),(0.,3.95507910396783E-6,
7.53768426604193E-6,1.19904533335351E-5,1.40475043392585E-5,1.51452104275963E-5,
1.67866272814202E-5,1.69621513005356E-5,1.8133831546071E-5,1.98906334656567E-5,
2.06132424588241E-5),.UNSPECIFIED.);
#25724=B_SPLINE_CURVE_WITH_KNOTS('',3,(#405199,#405200,#405201,#405202),
 .UNSPECIFIED.,.F.,.F.,(4,4),(1.62630325872826E-19,0.00010938435327491),
 .UNSPECIFIED.);
#25725=B_SPLINE_CURVE_WITH_KNOTS('',3,(#405229,#405230,#405231,#405232,
#405233,#405234,#405235,#405236,#405237,#405238,#405239,#405240,#405241,
#405242,#405243,#405244,#405245,#405246,#405247,#405248,#405249,#405250,
#405251,#405252,#405253,#405254,#405255,#405256,#405257,#405258,#405259,
#405260,#405261,#405262),.UNSPECIFIED.,.F.,.F.,(4,3,3,3,3,3,3,3,3,3,3,4),
(5.42101086242752E-20,2.09623992729448E-6,3.17176647120223E-6,4.82636181942703E-6,
5.0100091733996E-6,6.13126454147494E-6,8.60486650288851E-6,9.21144281170486E-6,
1.24722301136045E-5,1.42666454787856E-5,2.04670653757033E-5,2.08026438176802E-5),
 .UNSPECIFIED.);
#25726=B_SPLINE_CURVE_WITH_KNOTS('',3,(#405263,#405264,#405265,#405266),
 .UNSPECIFIED.,.F.,.F.,(4,4),(0.,0.000109384345496908),.UNSPECIFIED.);
#25727=B_SPLINE_CURVE_WITH_KNOTS('',3,(#405371,#405372,#405373,#405374),
 .UNSPECIFIED.,.F.,.F.,(4,4),(0.,9.54361881492172E-5),.UNSPECIFIED.);
#25728=B_SPLINE_CURVE_WITH_KNOTS('',3,(#405379,#405380,#405381,#405382,
#405383,#405384,#405385),.UNSPECIFIED.,.F.,.F.,(4,3,4),(0.,4.41069704323469E-5,
0.000113970027818833),.UNSPECIFIED.);
#25729=B_SPLINE_CURVE_WITH_KNOTS('',3,(#405391,#405392,#405393,#405394),
 .UNSPECIFIED.,.F.,.F.,(4,4),(4.84869951806108E-19,9.54361881492178E-5),
 .UNSPECIFIED.);
#25730=B_SPLINE_CURVE_WITH_KNOTS('',3,(#405398,#405399,#405400,#405401,
#405402,#405403,#405404),.UNSPECIFIED.,.F.,.F.,(4,3,4),(0.,6.9863024419149E-5,
0.000113969974038089),.UNSPECIFIED.);
#25731=B_SPLINE_CURVE_WITH_KNOTS('',3,(#405407,#405408,#405409,#405410,
#405411,#405412,#405413,#405414,#405415,#405416,#405417,#405418,#405419,
#405420,#405421,#405422,#405423,#405424,#405425,#405426,#405427,#405428,
#405429,#405430,#405431,#405432,#405433,#405434,#405435,#405436,#405437,
#405438,#405439,#405440,#405441,#405442,#405443,#405444,#405445,#405446,
#405447,#405448,#405449,#405450,#405451,#405452,#405453,#405454,#405455),
 .UNSPECIFIED.,.F.,.F.,(4,3,3,3,3,3,3,3,3,3,3,3,3,3,3,3,4),(0.,1.53100299373416E-6,
4.52554775679585E-6,7.01151246291608E-6,9.26752933800778E-6,1.03084066197173E-5,
1.17138990826861E-5,1.22284894984073E-5,1.30315035324816E-5,1.38363728497814E-5,
1.40464197777495E-5,1.54597749564641E-5,1.62073588704069E-5,1.9209296871241E-5,
1.95234416882557E-5,2.37637844577615E-5,2.61487188977267E-5),
 .UNSPECIFIED.);
#25732=B_SPLINE_CURVE_WITH_KNOTS('',3,(#405470,#405471,#405472,#405473,
#405474,#405475,#405476,#405477,#405478,#405479,#405480,#405481,#405482,
#405483,#405484,#405485,#405486,#405487,#405488,#405489,#405490,#405491,
#405492,#405493,#405494,#405495,#405496,#405497,#405498,#405499,#405500),
 .UNSPECIFIED.,.F.,.F.,(4,3,3,3,3,3,3,3,3,3,4),(0.,3.95507910397426E-6,
7.53768426604206E-6,1.19904533335352E-5,1.40475043392587E-5,1.51452104275966E-5,
1.67866272814278E-5,1.6962151300536E-5,1.81338315460714E-5,1.98906334656544E-5,
2.06132424588248E-5),.UNSPECIFIED.);
#25733=B_SPLINE_CURVE_WITH_KNOTS('',3,(#405503,#405504,#405505,#405506),
 .UNSPECIFIED.,.F.,.F.,(4,4),(5.42101086242752E-19,0.00010938435327491),
 .UNSPECIFIED.);
#25734=B_SPLINE_CURVE_WITH_KNOTS('',3,(#405533,#405534,#405535,#405536,
#405537,#405538,#405539,#405540,#405541,#405542,#405543,#405544,#405545,
#405546,#405547,#405548,#405549,#405550,#405551,#405552,#405553,#405554,
#405555,#405556,#405557,#405558,#405559,#405560,#405561,#405562,#405563,
#405564,#405565,#405566),.UNSPECIFIED.,.F.,.F.,(4,3,3,3,3,3,3,3,3,3,3,4),
(1.0842021724855E-19,2.09623992729449E-6,3.17176647120226E-6,4.82636181944126E-6,
5.0100091733997E-6,6.13126454147493E-6,8.6048665028884E-6,9.21144281170475E-6,
1.24722301135929E-5,1.42666454787848E-5,2.04670653756726E-5,2.08026438176789E-5),
 .UNSPECIFIED.);
#25735=B_SPLINE_CURVE_WITH_KNOTS('',3,(#405567,#405568,#405569,#405570),
 .UNSPECIFIED.,.F.,.F.,(4,4),(0.,0.000109384345496908),.UNSPECIFIED.);
#25736=B_SPLINE_CURVE_WITH_KNOTS('',3,(#405675,#405676,#405677,#405678),
 .UNSPECIFIED.,.F.,.F.,(4,4),(0.,9.54361881492173E-5),.UNSPECIFIED.);
#25737=B_SPLINE_CURVE_WITH_KNOTS('',3,(#405683,#405684,#405685,#405686,
#405687,#405688,#405689),.UNSPECIFIED.,.F.,.F.,(4,3,4),(0.,4.41069704323467E-5,
0.000113970027818833),.UNSPECIFIED.);
#25738=B_SPLINE_CURVE_WITH_KNOTS('',3,(#405695,#405696,#405697,#405698),
 .UNSPECIFIED.,.F.,.F.,(4,4),(2.16840434497101E-19,9.54361881492178E-5),
 .UNSPECIFIED.);
#25739=B_SPLINE_CURVE_WITH_KNOTS('',3,(#405702,#405703,#405704,#405705,
#405706,#405707,#405708),.UNSPECIFIED.,.F.,.F.,(4,3,4),(0.,6.98630244191491E-5,
0.000113969974038089),.UNSPECIFIED.);
#25740=B_SPLINE_CURVE_WITH_KNOTS('',3,(#405711,#405712,#405713,#405714,
#405715,#405716,#405717,#405718,#405719,#405720,#405721,#405722,#405723,
#405724,#405725,#405726,#405727,#405728,#405729,#405730,#405731,#405732,
#405733,#405734,#405735,#405736,#405737,#405738,#405739,#405740,#405741,
#405742,#405743,#405744,#405745,#405746,#405747,#405748,#405749,#405750,
#405751,#405752,#405753,#405754,#405755,#405756,#405757,#405758,#405759),
 .UNSPECIFIED.,.F.,.F.,(4,3,3,3,3,3,3,3,3,3,3,3,3,3,3,3,4),(0.,1.53100299373419E-6,
4.52554775679209E-6,7.01151246291602E-6,9.26752933799641E-6,1.03084066197174E-5,
1.17138990826862E-5,1.22284894984075E-5,1.30315035324818E-5,1.38363728497813E-5,
1.40464197777496E-5,1.5459774956464E-5,1.62073588704068E-5,1.92092968712732E-5,
1.95234416882555E-5,2.3763784457757E-5,2.6148718897726E-5),
 .UNSPECIFIED.);
#25741=B_SPLINE_CURVE_WITH_KNOTS('',3,(#405774,#405775,#405776,#405777,
#405778,#405779,#405780,#405781,#405782,#405783,#405784,#405785,#405786,
#405787,#405788,#405789,#405790,#405791,#405792,#405793,#405794,#405795,
#405796,#405797,#405798,#405799,#405800,#405801,#405802,#405803,#405804),
 .UNSPECIFIED.,.F.,.F.,(4,3,3,3,3,3,3,3,3,3,4),(0.,3.95507910397029E-6,
7.53768426604194E-6,1.1990453333535E-5,1.40475043392585E-5,1.51452104275964E-5,
1.67866272814301E-5,1.69621513005357E-5,1.81338315460711E-5,1.98906334656535E-5,
2.06132424588243E-5),.UNSPECIFIED.);
#25742=B_SPLINE_CURVE_WITH_KNOTS('',3,(#405807,#405808,#405809,#405810),
 .UNSPECIFIED.,.F.,.F.,(4,4),(5.42101086242752E-19,0.00010938435327491),
 .UNSPECIFIED.);
#25743=B_SPLINE_CURVE_WITH_KNOTS('',3,(#405837,#405838,#405839,#405840,
#405841,#405842,#405843,#405844,#405845,#405846,#405847,#405848,#405849,
#405850,#405851,#405852,#405853,#405854,#405855,#405856,#405857,#405858,
#405859,#405860,#405861,#405862,#405863,#405864,#405865,#405866,#405867,
#405868,#405869,#405870),.UNSPECIFIED.,.F.,.F.,(4,3,3,3,3,3,3,3,3,3,3,4),
(1.0842021724855E-19,2.09623992729457E-6,3.17176647120225E-6,4.82636181943907E-6,
5.0100091733998E-6,6.13126454147517E-6,8.60486650288879E-6,9.21144281170528E-6,
1.24722301136079E-5,1.42666454787861E-5,2.04670653756915E-5,2.08026438176811E-5),
 .UNSPECIFIED.);
#25744=B_SPLINE_CURVE_WITH_KNOTS('',3,(#405871,#405872,#405873,#405874),
 .UNSPECIFIED.,.F.,.F.,(4,4),(0.,0.000109384345496908),.UNSPECIFIED.);
#25745=B_SPLINE_CURVE_WITH_KNOTS('',3,(#405979,#405980,#405981,#405982),
 .UNSPECIFIED.,.F.,.F.,(4,4),(0.,9.54361881492174E-5),.UNSPECIFIED.);
#25746=B_SPLINE_CURVE_WITH_KNOTS('',3,(#405987,#405988,#405989,#405990,
#405991,#405992,#405993),.UNSPECIFIED.,.F.,.F.,(4,3,4),(0.,4.41069704323467E-5,
0.000113970027818833),.UNSPECIFIED.);
#25747=B_SPLINE_CURVE_WITH_KNOTS('',3,(#405999,#406000,#406001,#406002),
 .UNSPECIFIED.,.F.,.F.,(4,4),(1.0842021724855E-19,9.5436188149218E-5),
 .UNSPECIFIED.);
#25748=B_SPLINE_CURVE_WITH_KNOTS('',3,(#406006,#406007,#406008,#406009,
#406010,#406011,#406012),.UNSPECIFIED.,.F.,.F.,(4,3,4),(0.,6.98630244191491E-5,
0.000113969974038089),.UNSPECIFIED.);
#25749=B_SPLINE_CURVE_WITH_KNOTS('',3,(#406015,#406016,#406017,#406018,
#406019,#406020,#406021,#406022,#406023,#406024,#406025,#406026,#406027,
#406028,#406029,#406030,#406031,#406032,#406033,#406034,#406035,#406036,
#406037,#406038,#406039,#406040,#406041,#406042,#406043,#406044,#406045,
#406046,#406047,#406048,#406049,#406050,#406051,#406052,#406053,#406054,
#406055,#406056,#406057,#406058,#406059,#406060,#406061,#406062,#406063),
 .UNSPECIFIED.,.F.,.F.,(4,3,3,3,3,3,3,3,3,3,3,3,3,3,3,3,4),(0.,1.53100299373407E-6,
4.52554775679091E-6,7.011512462916E-6,9.26752933799658E-6,1.03084066197173E-5,
1.17138990826861E-5,1.22284894984074E-5,1.30315035324817E-5,1.38363728497813E-5,
1.40464197777494E-5,1.54597749564637E-5,1.62073588704067E-5,1.92092968712989E-5,
1.95234416882551E-5,2.37637844577598E-5,2.61487188977256E-5),
 .UNSPECIFIED.);
#25750=B_SPLINE_CURVE_WITH_KNOTS('',3,(#406078,#406079,#406080,#406081,
#406082,#406083,#406084,#406085,#406086,#406087,#406088,#406089,#406090,
#406091,#406092,#406093,#406094,#406095,#406096,#406097,#406098,#406099,
#406100,#406101,#406102,#406103,#406104,#406105,#406106,#406107,#406108),
 .UNSPECIFIED.,.F.,.F.,(4,3,3,3,3,3,3,3,3,3,4),(0.,3.95507910398523E-6,
7.53768426604203E-6,1.1990453333535E-5,1.40475043392585E-5,1.51452104275962E-5,
1.67866272813973E-5,1.69621513005356E-5,1.8133831546071E-5,1.98906334656504E-5,
2.06132424588242E-5),.UNSPECIFIED.);
#25751=B_SPLINE_CURVE_WITH_KNOTS('',3,(#406111,#406112,#406113,#406114),
 .UNSPECIFIED.,.F.,.F.,(4,4),(5.42101086242752E-19,0.00010938435327491),
 .UNSPECIFIED.);
#25752=B_SPLINE_CURVE_WITH_KNOTS('',3,(#406141,#406142,#406143,#406144,
#406145,#406146,#406147,#406148,#406149,#406150,#406151,#406152,#406153,
#406154,#406155,#406156,#406157,#406158,#406159,#406160,#406161,#406162,
#406163,#406164,#406165,#406166,#406167,#406168,#406169,#406170,#406171,
#406172,#406173,#406174),.UNSPECIFIED.,.F.,.F.,(4,3,3,3,3,3,3,3,3,3,3,4),
(1.0842021724855E-19,2.09623992729449E-6,3.17176647120215E-6,4.82636181943874E-6,
5.01000917339961E-6,6.13126454147489E-6,8.60486650288858E-6,9.21144281170495E-6,
1.24722301136101E-5,1.42666454787857E-5,2.04670653756931E-5,2.08026438176806E-5),
 .UNSPECIFIED.);
#25753=B_SPLINE_CURVE_WITH_KNOTS('',3,(#406175,#406176,#406177,#406178),
 .UNSPECIFIED.,.F.,.F.,(4,4),(0.,0.000109384345496908),.UNSPECIFIED.);
#25754=B_SPLINE_CURVE_WITH_KNOTS('',3,(#406283,#406284,#406285,#406286),
 .UNSPECIFIED.,.F.,.F.,(4,4),(0.,9.54361881492175E-5),.UNSPECIFIED.);
#25755=B_SPLINE_CURVE_WITH_KNOTS('',3,(#406291,#406292,#406293,#406294,
#406295,#406296,#406297),.UNSPECIFIED.,.F.,.F.,(4,3,4),(0.,4.4106970432347E-5,
0.000113970027818833),.UNSPECIFIED.);
#25756=B_SPLINE_CURVE_WITH_KNOTS('',3,(#406303,#406304,#406305,#406306),
 .UNSPECIFIED.,.F.,.F.,(4,4),(2.16840434497101E-19,9.54361881492178E-5),
 .UNSPECIFIED.);
#25757=B_SPLINE_CURVE_WITH_KNOTS('',3,(#406310,#406311,#406312,#406313,
#406314,#406315,#406316),.UNSPECIFIED.,.F.,.F.,(4,3,4),(0.,6.9863024419149E-5,
0.000113969974038089),.UNSPECIFIED.);
#25758=B_SPLINE_CURVE_WITH_KNOTS('',3,(#406319,#406320,#406321,#406322,
#406323,#406324,#406325,#406326,#406327,#406328,#406329,#406330,#406331,
#406332,#406333,#406334,#406335,#406336,#406337,#406338,#406339,#406340,
#406341,#406342,#406343,#406344,#406345,#406346,#406347,#406348,#406349,
#406350,#406351,#406352,#406353,#406354,#406355,#406356,#406357,#406358,
#406359,#406360,#406361,#406362,#406363,#406364,#406365,#406366,#406367),
 .UNSPECIFIED.,.F.,.F.,(4,3,3,3,3,3,3,3,3,3,3,3,3,3,3,3,4),(0.,1.53100299373416E-6,
4.52554775679514E-6,7.0115124629161E-6,9.26752933799368E-6,1.03084066197174E-5,
1.17138990826862E-5,1.22284894984073E-5,1.30315035324817E-5,1.38363728497812E-5,
1.40464197777492E-5,1.5459774956464E-5,1.62073588704068E-5,1.92092968713296E-5,
1.95234416882555E-5,2.37637844577558E-5,2.6148718897726E-5),
 .UNSPECIFIED.);
#25759=B_SPLINE_CURVE_WITH_KNOTS('',3,(#406382,#406383,#406384,#406385,
#406386,#406387,#406388,#406389,#406390,#406391,#406392,#406393,#406394,
#406395,#406396,#406397,#406398,#406399,#406400,#406401,#406402,#406403,
#406404,#406405,#406406,#406407,#406408,#406409,#406410,#406411,#406412),
 .UNSPECIFIED.,.F.,.F.,(4,3,3,3,3,3,3,3,3,3,4),(0.,3.95507910397283E-6,
7.53768426604198E-6,1.19904533335351E-5,1.40475043392585E-5,1.51452104275962E-5,
1.67866272814064E-5,1.69621513005357E-5,1.81338315460709E-5,1.98906334656548E-5,
2.06132424588242E-5),.UNSPECIFIED.);
#25760=B_SPLINE_CURVE_WITH_KNOTS('',3,(#406415,#406416,#406417,#406418),
 .UNSPECIFIED.,.F.,.F.,(4,4),(1.06229684024259E-18,0.00010938435327491),
 .UNSPECIFIED.);
#25761=B_SPLINE_CURVE_WITH_KNOTS('',3,(#406445,#406446,#406447,#406448,
#406449,#406450,#406451,#406452,#406453,#406454,#406455,#406456,#406457,
#406458,#406459,#406460,#406461,#406462,#406463,#406464,#406465,#406466,
#406467,#406468,#406469,#406470,#406471,#406472,#406473,#406474,#406475,
#406476,#406477,#406478),.UNSPECIFIED.,.F.,.F.,(4,3,3,3,3,3,3,3,3,3,3,4),
(0.,2.0962399272943E-6,3.17176647120212E-6,4.82636181943056E-6,5.01000917339971E-6,
6.13126454147472E-6,8.60486650288839E-6,9.21144281170468E-6,1.24722301136024E-5,
1.42666454787851E-5,2.04670653756884E-5,2.08026438176793E-5),
 .UNSPECIFIED.);
#25762=B_SPLINE_CURVE_WITH_KNOTS('',3,(#406479,#406480,#406481,#406482),
 .UNSPECIFIED.,.F.,.F.,(4,4),(0.,0.000109384345496908),.UNSPECIFIED.);
#25763=B_SPLINE_CURVE_WITH_KNOTS('',3,(#406587,#406588,#406589,#406590),
 .UNSPECIFIED.,.F.,.F.,(4,4),(0.,9.54361881492172E-5),.UNSPECIFIED.);
#25764=B_SPLINE_CURVE_WITH_KNOTS('',3,(#406595,#406596,#406597,#406598,
#406599,#406600,#406601),.UNSPECIFIED.,.F.,.F.,(4,3,4),(0.,4.41069704323466E-5,
0.000113970027818833),.UNSPECIFIED.);
#25765=B_SPLINE_CURVE_WITH_KNOTS('',3,(#406607,#406608,#406609,#406610),
 .UNSPECIFIED.,.F.,.F.,(4,4),(2.16840434497101E-19,9.54361881492177E-5),
 .UNSPECIFIED.);
#25766=B_SPLINE_CURVE_WITH_KNOTS('',3,(#406614,#406615,#406616,#406617,
#406618,#406619,#406620),.UNSPECIFIED.,.F.,.F.,(4,3,4),(0.,6.98630244191489E-5,
0.000113969974038089),.UNSPECIFIED.);
#25767=B_SPLINE_CURVE_WITH_KNOTS('',3,(#406623,#406624,#406625,#406626,
#406627,#406628,#406629,#406630,#406631,#406632,#406633,#406634,#406635,
#406636,#406637,#406638,#406639,#406640,#406641,#406642,#406643,#406644,
#406645,#406646,#406647,#406648,#406649,#406650,#406651,#406652,#406653,
#406654,#406655,#406656,#406657,#406658,#406659,#406660,#406661,#406662,
#406663,#406664,#406665,#406666,#406667,#406668,#406669,#406670,#406671),
 .UNSPECIFIED.,.F.,.F.,(4,3,3,3,3,3,3,3,3,3,3,3,3,3,3,3,4),(0.,1.53100299373418E-6,
4.52554775678938E-6,7.01151246291608E-6,9.26752933799924E-6,1.03084066197175E-5,
1.17138990826861E-5,1.22284894984077E-5,1.30315035324817E-5,1.38363728497813E-5,
1.40464197777495E-5,1.54597749564642E-5,1.62073588704069E-5,1.9209296871297E-5,
1.95234416882558E-5,2.37637844577571E-5,2.61487188977267E-5),
 .UNSPECIFIED.);
#25768=B_SPLINE_CURVE_WITH_KNOTS('',3,(#406686,#406687,#406688,#406689,
#406690,#406691,#406692,#406693,#406694,#406695,#406696,#406697,#406698,
#406699,#406700,#406701,#406702,#406703,#406704,#406705,#406706,#406707,
#406708,#406709,#406710,#406711,#406712,#406713,#406714,#406715,#406716),
 .UNSPECIFIED.,.F.,.F.,(4,3,3,3,3,3,3,3,3,3,4),(0.,3.95507910397925E-6,
7.53768426604196E-6,1.19904533335351E-5,1.40475043392584E-5,1.51452104275962E-5,
1.67866272814223E-5,1.69621513005356E-5,1.8133831546071E-5,1.98906334656514E-5,
2.06132424588242E-5),.UNSPECIFIED.);
#25769=B_SPLINE_CURVE_WITH_KNOTS('',3,(#406719,#406720,#406721,#406722),
 .UNSPECIFIED.,.F.,.F.,(4,4),(4.84869951806108E-19,0.00010938435327491),
 .UNSPECIFIED.);
#25770=B_SPLINE_CURVE_WITH_KNOTS('',3,(#406749,#406750,#406751,#406752,
#406753,#406754,#406755,#406756,#406757,#406758,#406759,#406760,#406761,
#406762,#406763,#406764,#406765,#406766,#406767,#406768,#406769,#406770,
#406771,#406772,#406773,#406774,#406775,#406776,#406777,#406778,#406779,
#406780,#406781,#406782),.UNSPECIFIED.,.F.,.F.,(4,3,3,3,3,3,3,3,3,3,3,4),
(2.16840434497101E-19,2.0962399272944E-6,3.17176647120198E-6,4.82636181943813E-6,
5.0100091733995E-6,6.13126454147485E-6,8.60486650288839E-6,9.21144281170471E-6,
1.24722301135892E-5,1.42666454787855E-5,2.04670653756988E-5,2.08026438176803E-5),
 .UNSPECIFIED.);
#25771=B_SPLINE_CURVE_WITH_KNOTS('',3,(#406783,#406784,#406785,#406786),
 .UNSPECIFIED.,.F.,.F.,(4,4),(0.,0.000109384345496908),.UNSPECIFIED.);
#25772=B_SPLINE_CURVE_WITH_KNOTS('',3,(#406891,#406892,#406893,#406894),
 .UNSPECIFIED.,.F.,.F.,(4,4),(0.,9.54361881492175E-5),.UNSPECIFIED.);
#25773=B_SPLINE_CURVE_WITH_KNOTS('',3,(#406899,#406900,#406901,#406902,
#406903,#406904,#406905),.UNSPECIFIED.,.F.,.F.,(4,3,4),(0.,4.41069704323467E-5,
0.000113970027818833),.UNSPECIFIED.);
#25774=B_SPLINE_CURVE_WITH_KNOTS('',3,(#406911,#406912,#406913,#406914),
 .UNSPECIFIED.,.F.,.F.,(4,4),(2.16840434497101E-19,9.5436188149218E-5),
 .UNSPECIFIED.);
#25775=B_SPLINE_CURVE_WITH_KNOTS('',3,(#406918,#406919,#406920,#406921,
#406922,#406923,#406924),.UNSPECIFIED.,.F.,.F.,(4,3,4),(0.,6.9863024419149E-5,
0.000113969974038089),.UNSPECIFIED.);
#25776=B_SPLINE_CURVE_WITH_KNOTS('',3,(#406927,#406928,#406929,#406930,
#406931,#406932,#406933,#406934,#406935,#406936,#406937,#406938,#406939,
#406940,#406941,#406942,#406943,#406944,#406945,#406946,#406947,#406948,
#406949,#406950,#406951,#406952,#406953,#406954,#406955,#406956,#406957,
#406958,#406959,#406960,#406961,#406962,#406963,#406964,#406965,#406966,
#406967,#406968,#406969,#406970,#406971,#406972,#406973,#406974,#406975),
 .UNSPECIFIED.,.F.,.F.,(4,3,3,3,3,3,3,3,3,3,3,3,3,3,3,3,4),(0.,1.53100299373417E-6,
4.5255477567939E-6,7.01151246291599E-6,9.26752933800752E-6,1.03084066197173E-5,
1.1713899082686E-5,1.22284894984074E-5,1.30315035324818E-5,1.38363728497814E-5,
1.40464197777495E-5,1.54597749564642E-5,1.62073588704071E-5,1.92092968712427E-5,
1.95234416882558E-5,2.37637844577606E-5,2.61487188977267E-5),
 .UNSPECIFIED.);
#25777=B_SPLINE_CURVE_WITH_KNOTS('',3,(#406990,#406991,#406992,#406993,
#406994,#406995,#406996,#406997,#406998,#406999,#407000,#407001,#407002,
#407003,#407004,#407005,#407006,#407007,#407008,#407009,#407010,#407011,
#407012,#407013,#407014,#407015,#407016,#407017,#407018,#407019,#407020),
 .UNSPECIFIED.,.F.,.F.,(4,3,3,3,3,3,3,3,3,3,4),(0.,3.95507910397345E-6,
7.53768426604203E-6,1.19904533335351E-5,1.40475043392584E-5,1.51452104275961E-5,
1.67866272814359E-5,1.69621513005354E-5,1.81338315460706E-5,1.98906334656507E-5,
2.06132424588236E-5),.UNSPECIFIED.);
#25778=B_SPLINE_CURVE_WITH_KNOTS('',3,(#407023,#407024,#407025,#407026),
 .UNSPECIFIED.,.F.,.F.,(4,4),(6.1331736667335E-19,0.00010938435327491),
 .UNSPECIFIED.);
#25779=B_SPLINE_CURVE_WITH_KNOTS('',3,(#407053,#407054,#407055,#407056,
#407057,#407058,#407059,#407060,#407061,#407062,#407063,#407064,#407065,
#407066,#407067,#407068,#407069,#407070,#407071,#407072,#407073,#407074,
#407075,#407076,#407077,#407078,#407079,#407080,#407081,#407082,#407083,
#407084,#407085,#407086),.UNSPECIFIED.,.F.,.F.,(4,3,3,3,3,3,3,3,3,3,3,4),
(2.16840434497101E-19,2.09623992729424E-6,3.17176647120213E-6,4.82636181944472E-6,
5.01000917339969E-6,6.13126454147474E-6,8.6048665028883E-6,9.21144281170472E-6,
1.2472230113588E-5,1.42666454787853E-5,2.04670653757003E-5,2.08026438176799E-5),
 .UNSPECIFIED.);
#25780=B_SPLINE_CURVE_WITH_KNOTS('',3,(#407087,#407088,#407089,#407090),
 .UNSPECIFIED.,.F.,.F.,(4,4),(0.,0.000109384345496908),.UNSPECIFIED.);
#25781=B_SPLINE_CURVE_WITH_KNOTS('',3,(#407195,#407196,#407197,#407198),
 .UNSPECIFIED.,.F.,.F.,(4,4),(0.,9.54361881492175E-5),.UNSPECIFIED.);
#25782=B_SPLINE_CURVE_WITH_KNOTS('',3,(#407203,#407204,#407205,#407206,
#407207,#407208,#407209),.UNSPECIFIED.,.F.,.F.,(4,3,4),(0.,4.4106970432347E-5,
0.000113970027818833),.UNSPECIFIED.);
#25783=B_SPLINE_CURVE_WITH_KNOTS('',3,(#407215,#407216,#407217,#407218),
 .UNSPECIFIED.,.F.,.F.,(4,4),(2.16840434497101E-19,9.54361881492179E-5),
 .UNSPECIFIED.);
#25784=B_SPLINE_CURVE_WITH_KNOTS('',3,(#407222,#407223,#407224,#407225,
#407226,#407227,#407228),.UNSPECIFIED.,.F.,.F.,(4,3,4),(0.,6.98630244191489E-5,
0.000113969974038089),.UNSPECIFIED.);
#25785=B_SPLINE_CURVE_WITH_KNOTS('',3,(#407231,#407232,#407233,#407234,
#407235,#407236,#407237,#407238,#407239,#407240,#407241,#407242,#407243,
#407244,#407245,#407246,#407247,#407248,#407249,#407250,#407251,#407252,
#407253,#407254,#407255,#407256,#407257,#407258,#407259,#407260,#407261,
#407262,#407263,#407264,#407265,#407266,#407267,#407268,#407269,#407270,
#407271,#407272,#407273,#407274,#407275,#407276,#407277,#407278,#407279),
 .UNSPECIFIED.,.F.,.F.,(4,3,3,3,3,3,3,3,3,3,3,3,3,3,3,3,4),(0.,1.53100299373418E-6,
4.52554775679471E-6,7.0115124629162E-6,9.26752933799194E-6,1.03084066197174E-5,
1.17138990826862E-5,1.22284894984075E-5,1.30315035324818E-5,1.38363728497813E-5,
1.40464197777498E-5,1.54597749564643E-5,1.62073588704074E-5,1.92092968711982E-5,
1.95234416882562E-5,2.37637844577607E-5,2.6148718897727E-5),
 .UNSPECIFIED.);
#25786=B_SPLINE_CURVE_WITH_KNOTS('',3,(#407294,#407295,#407296,#407297,
#407298,#407299,#407300,#407301,#407302,#407303,#407304,#407305,#407306,
#407307,#407308,#407309,#407310,#407311,#407312,#407313,#407314,#407315,
#407316,#407317,#407318,#407319,#407320,#407321,#407322,#407323,#407324),
 .UNSPECIFIED.,.F.,.F.,(4,3,3,3,3,3,3,3,3,3,4),(0.,3.95507910397078E-6,
7.537684266042E-6,1.19904533335351E-5,1.40475043392585E-5,1.51452104275965E-5,
1.67866272814274E-5,1.69621513005358E-5,1.81338315460712E-5,1.98906334656593E-5,
2.06132424588248E-5),.UNSPECIFIED.);
#25787=B_SPLINE_CURVE_WITH_KNOTS('',3,(#407327,#407328,#407329,#407330),
 .UNSPECIFIED.,.F.,.F.,(4,4),(2.16840434497101E-19,0.00010938435327491),
 .UNSPECIFIED.);
#25788=B_SPLINE_CURVE_WITH_KNOTS('',3,(#407357,#407358,#407359,#407360,
#407361,#407362,#407363,#407364,#407365,#407366,#407367,#407368,#407369,
#407370,#407371,#407372,#407373,#407374,#407375,#407376,#407377,#407378,
#407379,#407380,#407381,#407382,#407383,#407384,#407385,#407386,#407387,
#407388,#407389,#407390),.UNSPECIFIED.,.F.,.F.,(4,3,3,3,3,3,3,3,3,3,3,4),
(0.,2.09623992729454E-6,3.17176647120236E-6,4.82636181944207E-6,5.01000917339988E-6,
6.13126454147488E-6,8.60486650288867E-6,9.21144281170499E-6,1.24722301136154E-5,
1.42666454787857E-5,2.04670653757237E-5,2.08026438176804E-5),
 .UNSPECIFIED.);
#25789=B_SPLINE_CURVE_WITH_KNOTS('',3,(#407391,#407392,#407393,#407394),
 .UNSPECIFIED.,.F.,.F.,(4,4),(0.,0.000109384345496908),.UNSPECIFIED.);
#25790=B_SPLINE_CURVE_WITH_KNOTS('',3,(#407499,#407500,#407501,#407502),
 .UNSPECIFIED.,.F.,.F.,(4,4),(0.,9.54361881492175E-5),.UNSPECIFIED.);
#25791=B_SPLINE_CURVE_WITH_KNOTS('',3,(#407507,#407508,#407509,#407510,
#407511,#407512,#407513),.UNSPECIFIED.,.F.,.F.,(4,3,4),(0.,4.41069704323469E-5,
0.000113970027818833),.UNSPECIFIED.);
#25792=B_SPLINE_CURVE_WITH_KNOTS('',3,(#407519,#407520,#407521,#407522),
 .UNSPECIFIED.,.F.,.F.,(4,4),(2.16840434497101E-19,9.54361881492178E-5),
 .UNSPECIFIED.);
#25793=B_SPLINE_CURVE_WITH_KNOTS('',3,(#407526,#407527,#407528,#407529,
#407530,#407531,#407532),.UNSPECIFIED.,.F.,.F.,(4,3,4),(0.,6.98630244191491E-5,
0.000113969974038089),.UNSPECIFIED.);
#25794=B_SPLINE_CURVE_WITH_KNOTS('',3,(#407535,#407536,#407537,#407538,
#407539,#407540,#407541,#407542,#407543,#407544,#407545,#407546,#407547,
#407548,#407549,#407550,#407551,#407552,#407553,#407554,#407555,#407556,
#407557,#407558,#407559,#407560,#407561,#407562,#407563,#407564,#407565,
#407566,#407567,#407568,#407569,#407570,#407571,#407572,#407573,#407574,
#407575,#407576,#407577,#407578,#407579,#407580,#407581,#407582,#407583),
 .UNSPECIFIED.,.F.,.F.,(4,3,3,3,3,3,3,3,3,3,3,3,3,3,3,3,4),(0.,1.53100299373406E-6,
4.52554775679257E-6,7.01151246291608E-6,9.26752933799928E-6,1.03084066197173E-5,
1.17138990826861E-5,1.22284894984075E-5,1.30315035324818E-5,1.38363728497812E-5,
1.40464197777496E-5,1.54597749564643E-5,1.62073588704074E-5,1.92092968712653E-5,
1.95234416882563E-5,2.37637844577625E-5,2.61487188977276E-5),
 .UNSPECIFIED.);
#25795=B_SPLINE_CURVE_WITH_KNOTS('',3,(#407598,#407599,#407600,#407601,
#407602,#407603,#407604,#407605,#407606,#407607,#407608,#407609,#407610,
#407611,#407612,#407613,#407614,#407615,#407616,#407617,#407618,#407619,
#407620,#407621,#407622,#407623,#407624,#407625,#407626,#407627,#407628),
 .UNSPECIFIED.,.F.,.F.,(4,3,3,3,3,3,3,3,3,3,4),(0.,3.9550791039781E-6,7.53768426604216E-6,
1.19904533335351E-5,1.40475043392587E-5,1.51452104275965E-5,1.67866272814076E-5,
1.69621513005362E-5,1.81338315460716E-5,1.98906334656553E-5,2.06132424588251E-5),
 .UNSPECIFIED.);
#25796=B_SPLINE_CURVE_WITH_KNOTS('',3,(#407631,#407632,#407633,#407634),
 .UNSPECIFIED.,.F.,.F.,(4,4),(4.33680868994202E-19,0.00010938435327491),
 .UNSPECIFIED.);
#25797=B_SPLINE_CURVE_WITH_KNOTS('',3,(#407661,#407662,#407663,#407664,
#407665,#407666,#407667,#407668,#407669,#407670,#407671,#407672,#407673,
#407674,#407675,#407676,#407677,#407678,#407679,#407680,#407681,#407682,
#407683,#407684,#407685,#407686,#407687,#407688,#407689,#407690,#407691,
#407692,#407693,#407694),.UNSPECIFIED.,.F.,.F.,(4,3,3,3,3,3,3,3,3,3,3,4),
(4.84869951806108E-19,2.09623992729453E-6,3.17176647120215E-6,4.8263618194302E-6,
5.01000917339957E-6,6.13126454147488E-6,8.60486650288844E-6,9.21144281170473E-6,
1.2472230113588E-5,1.4266645478785E-5,2.04670653756879E-5,2.08026438176792E-5),
 .UNSPECIFIED.);
#25798=B_SPLINE_CURVE_WITH_KNOTS('',3,(#407695,#407696,#407697,#407698),
 .UNSPECIFIED.,.F.,.F.,(4,4),(0.,0.000109384345496908),.UNSPECIFIED.);
#25799=B_SPLINE_CURVE_WITH_KNOTS('',3,(#407803,#407804,#407805,#407806),
 .UNSPECIFIED.,.F.,.F.,(4,4),(0.,9.54361881492177E-5),.UNSPECIFIED.);
#25800=B_SPLINE_CURVE_WITH_KNOTS('',3,(#407811,#407812,#407813,#407814,
#407815,#407816,#407817),.UNSPECIFIED.,.F.,.F.,(4,3,4),(0.,4.41069704323469E-5,
0.000113970027818833),.UNSPECIFIED.);
#25801=B_SPLINE_CURVE_WITH_KNOTS('',3,(#407823,#407824,#407825,#407826),
 .UNSPECIFIED.,.F.,.F.,(4,4),(2.16840434497101E-19,9.5436188149218E-5),
 .UNSPECIFIED.);
#25802=B_SPLINE_CURVE_WITH_KNOTS('',3,(#407830,#407831,#407832,#407833,
#407834,#407835,#407836),.UNSPECIFIED.,.F.,.F.,(4,3,4),(0.,6.98630244191492E-5,
0.000113969974038089),.UNSPECIFIED.);
#25803=B_SPLINE_CURVE_WITH_KNOTS('',3,(#407839,#407840,#407841,#407842,
#407843,#407844,#407845,#407846,#407847,#407848,#407849,#407850,#407851,
#407852,#407853,#407854,#407855,#407856,#407857,#407858,#407859,#407860,
#407861,#407862,#407863,#407864,#407865,#407866,#407867,#407868,#407869,
#407870,#407871,#407872,#407873,#407874,#407875,#407876,#407877,#407878,
#407879,#407880,#407881,#407882,#407883,#407884,#407885,#407886,#407887),
 .UNSPECIFIED.,.F.,.F.,(4,3,3,3,3,3,3,3,3,3,3,3,3,3,3,3,4),(0.,1.53100299373414E-6,
4.52554775679078E-6,7.01151246291599E-6,9.26752933800656E-6,1.03084066197172E-5,
1.17138990826861E-5,1.22284894984074E-5,1.30315035324815E-5,1.38363728497812E-5,
1.40464197777494E-5,1.54597749564641E-5,1.62073588704067E-5,1.92092968712602E-5,
1.95234416882553E-5,2.37637844577585E-5,2.61487188977259E-5),
 .UNSPECIFIED.);
#25804=B_SPLINE_CURVE_WITH_KNOTS('',3,(#407902,#407903,#407904,#407905,
#407906,#407907,#407908,#407909,#407910,#407911,#407912,#407913,#407914,
#407915,#407916,#407917,#407918,#407919,#407920,#407921,#407922,#407923,
#407924,#407925,#407926,#407927,#407928,#407929,#407930,#407931,#407932),
 .UNSPECIFIED.,.F.,.F.,(4,3,3,3,3,3,3,3,3,3,4),(0.,3.95507910397798E-6,
7.53768426604199E-6,1.19904533335349E-5,1.40475043392583E-5,1.51452104275965E-5,
1.67866272814203E-5,1.69621513005356E-5,1.81338315460712E-5,1.98906334656551E-5,
2.0613242458824E-5),.UNSPECIFIED.);
#25805=B_SPLINE_CURVE_WITH_KNOTS('',3,(#407935,#407936,#407937,#407938),
 .UNSPECIFIED.,.F.,.F.,(4,4),(4.33680868994202E-19,0.00010938435327491),
 .UNSPECIFIED.);
#25806=B_SPLINE_CURVE_WITH_KNOTS('',3,(#407965,#407966,#407967,#407968,
#407969,#407970,#407971,#407972,#407973,#407974,#407975,#407976,#407977,
#407978,#407979,#407980,#407981,#407982,#407983,#407984,#407985,#407986,
#407987,#407988,#407989,#407990,#407991,#407992,#407993,#407994,#407995,
#407996,#407997,#407998),.UNSPECIFIED.,.F.,.F.,(4,3,3,3,3,3,3,3,3,3,3,4),
(0.,2.0962399272946E-6,3.1717664712022E-6,4.8263618194285E-6,5.01000917339962E-6,
6.13126454147512E-6,8.60486650288865E-6,9.21144281170501E-6,1.24722301135971E-5,
1.42666454787856E-5,2.04670653756864E-5,2.08026438176801E-5),
 .UNSPECIFIED.);
#25807=B_SPLINE_CURVE_WITH_KNOTS('',3,(#407999,#408000,#408001,#408002),
 .UNSPECIFIED.,.F.,.F.,(4,4),(0.,0.000109384345496908),.UNSPECIFIED.);
#25808=B_SPLINE_CURVE_WITH_KNOTS('',3,(#408107,#408108,#408109,#408110),
 .UNSPECIFIED.,.F.,.F.,(4,4),(0.,9.54361881492175E-5),.UNSPECIFIED.);
#25809=B_SPLINE_CURVE_WITH_KNOTS('',3,(#408115,#408116,#408117,#408118,
#408119,#408120,#408121),.UNSPECIFIED.,.F.,.F.,(4,3,4),(0.,4.41069704323471E-5,
0.000113970027818833),.UNSPECIFIED.);
#25810=B_SPLINE_CURVE_WITH_KNOTS('',3,(#408127,#408128,#408129,#408130),
 .UNSPECIFIED.,.F.,.F.,(4,4),(0.,9.54361881492177E-5),.UNSPECIFIED.);
#25811=B_SPLINE_CURVE_WITH_KNOTS('',3,(#408134,#408135,#408136,#408137,
#408138,#408139,#408140),.UNSPECIFIED.,.F.,.F.,(4,3,4),(0.,6.9863024419149E-5,
0.000113969974038089),.UNSPECIFIED.);
#25812=B_SPLINE_CURVE_WITH_KNOTS('',3,(#408143,#408144,#408145,#408146,
#408147,#408148,#408149,#408150,#408151,#408152,#408153,#408154,#408155,
#408156,#408157,#408158,#408159,#408160,#408161,#408162,#408163,#408164,
#408165,#408166,#408167,#408168,#408169,#408170,#408171,#408172,#408173,
#408174,#408175,#408176,#408177,#408178,#408179,#408180,#408181,#408182,
#408183,#408184,#408185,#408186,#408187,#408188,#408189,#408190,#408191),
 .UNSPECIFIED.,.F.,.F.,(4,3,3,3,3,3,3,3,3,3,3,3,3,3,3,3,4),(0.,1.53100299373409E-6,
4.5255477567909E-6,7.01151246291603E-6,9.26752933800813E-6,1.03084066197175E-5,
1.17138990826863E-5,1.22284894984075E-5,1.30315035324818E-5,1.38363728497814E-5,
1.40464197777496E-5,1.5459774956464E-5,1.6207358870407E-5,1.92092968712736E-5,
1.9523441688256E-5,2.37637844577608E-5,2.61487188977272E-5),
 .UNSPECIFIED.);
#25813=B_SPLINE_CURVE_WITH_KNOTS('',3,(#408206,#408207,#408208,#408209,
#408210,#408211,#408212,#408213,#408214,#408215,#408216,#408217,#408218,
#408219,#408220,#408221,#408222,#408223,#408224,#408225,#408226,#408227,
#408228,#408229,#408230,#408231,#408232,#408233,#408234,#408235,#408236),
 .UNSPECIFIED.,.F.,.F.,(4,3,3,3,3,3,3,3,3,3,4),(0.,3.95507910397288E-6,
7.53768426604196E-6,1.1990453333535E-5,1.40475043392584E-5,1.51452104275964E-5,
1.67866272814138E-5,1.69621513005357E-5,1.8133831546071E-5,1.98906334656539E-5,
2.06132424588241E-5),.UNSPECIFIED.);
#25814=B_SPLINE_CURVE_WITH_KNOTS('',3,(#408239,#408240,#408241,#408242),
 .UNSPECIFIED.,.F.,.F.,(4,4),(4.84869951806108E-19,0.00010938435327491),
 .UNSPECIFIED.);
#25815=B_SPLINE_CURVE_WITH_KNOTS('',3,(#408269,#408270,#408271,#408272,
#408273,#408274,#408275,#408276,#408277,#408278,#408279,#408280,#408281,
#408282,#408283,#408284,#408285,#408286,#408287,#408288,#408289,#408290,
#408291,#408292,#408293,#408294,#408295,#408296,#408297,#408298,#408299,
#408300,#408301,#408302),.UNSPECIFIED.,.F.,.F.,(4,3,3,3,3,3,3,3,3,3,3,4),
(4.84869951806108E-19,2.09623992729411E-6,3.17176647120198E-6,4.82636181942691E-6,
5.01000917339932E-6,6.13126454147457E-6,8.60486650288819E-6,9.21144281170453E-6,
1.24722301135754E-5,1.42666454787853E-5,2.04670653757023E-5,2.080264381768E-5),
 .UNSPECIFIED.);
#25816=B_SPLINE_CURVE_WITH_KNOTS('',3,(#408303,#408304,#408305,#408306),
 .UNSPECIFIED.,.F.,.F.,(4,4),(0.,0.000109384345496908),.UNSPECIFIED.);
#25817=B_SPLINE_CURVE_WITH_KNOTS('',3,(#408411,#408412,#408413,#408414),
 .UNSPECIFIED.,.F.,.F.,(4,4),(0.,9.54361881492177E-5),.UNSPECIFIED.);
#25818=B_SPLINE_CURVE_WITH_KNOTS('',3,(#408419,#408420,#408421,#408422,
#408423,#408424,#408425),.UNSPECIFIED.,.F.,.F.,(4,3,4),(0.,4.4106970432347E-5,
0.000113970027818833),.UNSPECIFIED.);
#25819=B_SPLINE_CURVE_WITH_KNOTS('',3,(#408431,#408432,#408433,#408434),
 .UNSPECIFIED.,.F.,.F.,(4,4),(4.33680868994202E-19,9.54361881492178E-5),
 .UNSPECIFIED.);
#25820=B_SPLINE_CURVE_WITH_KNOTS('',3,(#408438,#408439,#408440,#408441,
#408442,#408443,#408444),.UNSPECIFIED.,.F.,.F.,(4,3,4),(0.,6.98630244191492E-5,
0.000113969974038089),.UNSPECIFIED.);
#25821=B_SPLINE_CURVE_WITH_KNOTS('',3,(#408447,#408448,#408449,#408450,
#408451,#408452,#408453,#408454,#408455,#408456,#408457,#408458,#408459,
#408460,#408461,#408462,#408463,#408464,#408465,#408466,#408467,#408468,
#408469,#408470,#408471,#408472,#408473,#408474,#408475,#408476,#408477,
#408478,#408479,#408480,#408481,#408482,#408483,#408484,#408485,#408486,
#408487,#408488,#408489,#408490,#408491,#408492,#408493,#408494,#408495),
 .UNSPECIFIED.,.F.,.F.,(4,3,3,3,3,3,3,3,3,3,3,3,3,3,3,3,4),(0.,1.53100299373405E-6,
4.52554775679714E-6,7.01151246291601E-6,9.26752933800423E-6,1.03084066197175E-5,
1.17138990826862E-5,1.22284894984072E-5,1.30315035324815E-5,1.3836372849781E-5,
1.40464197777492E-5,1.54597749564635E-5,1.62073588704063E-5,1.920929687128E-5,
1.95234416882546E-5,2.37637844577566E-5,2.61487188977245E-5),
 .UNSPECIFIED.);
#25822=B_SPLINE_CURVE_WITH_KNOTS('',3,(#408510,#408511,#408512,#408513,
#408514,#408515,#408516,#408517,#408518,#408519,#408520,#408521,#408522,
#408523,#408524,#408525,#408526,#408527,#408528,#408529,#408530,#408531,
#408532,#408533,#408534,#408535,#408536,#408537,#408538,#408539,#408540),
 .UNSPECIFIED.,.F.,.F.,(4,3,3,3,3,3,3,3,3,3,4),(0.,3.95507910397667E-6,
7.53768426604193E-6,1.1990453333535E-5,1.40475043392584E-5,1.51452104275964E-5,
1.6786627281433E-5,1.69621513005355E-5,1.81338315460713E-5,1.98906334656521E-5,
2.06132424588243E-5),.UNSPECIFIED.);
#25823=B_SPLINE_CURVE_WITH_KNOTS('',3,(#408543,#408544,#408545,#408546),
 .UNSPECIFIED.,.F.,.F.,(4,4),(4.33680868994202E-19,0.00010938435327491),
 .UNSPECIFIED.);
#25824=B_SPLINE_CURVE_WITH_KNOTS('',3,(#408573,#408574,#408575,#408576,
#408577,#408578,#408579,#408580,#408581,#408582,#408583,#408584,#408585,
#408586,#408587,#408588,#408589,#408590,#408591,#408592,#408593,#408594,
#408595,#408596,#408597,#408598,#408599,#408600,#408601,#408602,#408603,
#408604,#408605,#408606),.UNSPECIFIED.,.F.,.F.,(4,3,3,3,3,3,3,3,3,3,3,4),
(0.,2.09623992729444E-6,3.17176647120251E-6,4.82636181942884E-6,5.01000917339967E-6,
6.131264541475E-6,8.60486650288851E-6,9.21144281170478E-6,1.24722301135965E-5,
1.42666454787855E-5,2.04670653756859E-5,2.08026438176798E-5),
 .UNSPECIFIED.);
#25825=B_SPLINE_CURVE_WITH_KNOTS('',3,(#408607,#408608,#408609,#408610),
 .UNSPECIFIED.,.F.,.F.,(4,4),(0.,0.000109384345496908),.UNSPECIFIED.);
#25826=B_SPLINE_CURVE_WITH_KNOTS('',3,(#408715,#408716,#408717,#408718),
 .UNSPECIFIED.,.F.,.F.,(4,4),(0.,9.54361881492176E-5),.UNSPECIFIED.);
#25827=B_SPLINE_CURVE_WITH_KNOTS('',3,(#408723,#408724,#408725,#408726,
#408727,#408728,#408729),.UNSPECIFIED.,.F.,.F.,(4,3,4),(0.,4.41069704323469E-5,
0.000113970027818834),.UNSPECIFIED.);
#25828=B_SPLINE_CURVE_WITH_KNOTS('',3,(#408735,#408736,#408737,#408738),
 .UNSPECIFIED.,.F.,.F.,(4,4),(4.33680868994202E-19,9.54361881492182E-5),
 .UNSPECIFIED.);
#25829=B_SPLINE_CURVE_WITH_KNOTS('',3,(#408742,#408743,#408744,#408745,
#408746,#408747,#408748),.UNSPECIFIED.,.F.,.F.,(4,3,4),(0.,6.98630244191492E-5,
0.000113969974038089),.UNSPECIFIED.);
#25830=B_SPLINE_CURVE_WITH_KNOTS('',3,(#408751,#408752,#408753,#408754,
#408755,#408756,#408757,#408758,#408759,#408760,#408761,#408762,#408763,
#408764,#408765,#408766,#408767,#408768,#408769,#408770,#408771,#408772,
#408773,#408774,#408775,#408776,#408777,#408778,#408779,#408780,#408781,
#408782,#408783,#408784,#408785,#408786,#408787,#408788,#408789,#408790,
#408791,#408792,#408793,#408794,#408795,#408796,#408797,#408798,#408799),
 .UNSPECIFIED.,.F.,.F.,(4,3,3,3,3,3,3,3,3,3,3,3,3,3,3,3,4),(0.,1.53100299373406E-6,
4.52554775679991E-6,7.01151246291622E-6,9.26752933802365E-6,1.03084066197173E-5,
1.17138990826863E-5,1.22284894984077E-5,1.30315035324818E-5,1.38363728497814E-5,
1.40464197777498E-5,1.54597749564644E-5,1.62073588704074E-5,1.92092968713074E-5,
1.95234416882564E-5,2.37637844577626E-5,2.6148718897728E-5),
 .UNSPECIFIED.);
#25831=B_SPLINE_CURVE_WITH_KNOTS('',3,(#408814,#408815,#408816,#408817,
#408818,#408819,#408820,#408821,#408822,#408823,#408824,#408825,#408826,
#408827,#408828,#408829,#408830,#408831,#408832,#408833,#408834,#408835,
#408836,#408837,#408838,#408839,#408840,#408841,#408842,#408843,#408844),
 .UNSPECIFIED.,.F.,.F.,(4,3,3,3,3,3,3,3,3,3,4),(0.,3.95507910397371E-6,
7.537684266042E-6,1.1990453333535E-5,1.40475043392586E-5,1.51452104275965E-5,
1.67866272814201E-5,1.69621513005358E-5,1.8133831546071E-5,1.98906334656563E-5,
2.0613242458824E-5),.UNSPECIFIED.);
#25832=B_SPLINE_CURVE_WITH_KNOTS('',3,(#408847,#408848,#408849,#408850),
 .UNSPECIFIED.,.F.,.F.,(4,4),(9.69739903612216E-19,0.00010938435327491),
 .UNSPECIFIED.);
#25833=B_SPLINE_CURVE_WITH_KNOTS('',3,(#408877,#408878,#408879,#408880,
#408881,#408882,#408883,#408884,#408885,#408886,#408887,#408888,#408889,
#408890,#408891,#408892,#408893,#408894,#408895,#408896,#408897,#408898,
#408899,#408900,#408901,#408902,#408903,#408904,#408905,#408906,#408907,
#408908,#408909,#408910),.UNSPECIFIED.,.F.,.F.,(4,3,3,3,3,3,3,3,3,3,3,4),
(2.16840434497101E-19,2.09623992729432E-6,3.17176647120227E-6,4.82636181943918E-6,
5.01000917339956E-6,6.13126454147501E-6,8.60486650288879E-6,9.21144281170531E-6,
1.24722301135938E-5,1.4266645478786E-5,2.04670653756976E-5,2.08026438176811E-5),
 .UNSPECIFIED.);
#25834=B_SPLINE_CURVE_WITH_KNOTS('',3,(#408911,#408912,#408913,#408914),
 .UNSPECIFIED.,.F.,.F.,(4,4),(0.,0.000109384345496908),.UNSPECIFIED.);
#25835=B_SPLINE_CURVE_WITH_KNOTS('',3,(#409019,#409020,#409021,#409022),
 .UNSPECIFIED.,.F.,.F.,(4,4),(0.,9.54361881492175E-5),.UNSPECIFIED.);
#25836=B_SPLINE_CURVE_WITH_KNOTS('',3,(#409027,#409028,#409029,#409030,
#409031,#409032,#409033),.UNSPECIFIED.,.F.,.F.,(4,3,4),(0.,4.41069704323468E-5,
0.000113970027818833),.UNSPECIFIED.);
#25837=B_SPLINE_CURVE_WITH_KNOTS('',3,(#409039,#409040,#409041,#409042),
 .UNSPECIFIED.,.F.,.F.,(4,4),(0.,9.54361881492175E-5),.UNSPECIFIED.);
#25838=B_SPLINE_CURVE_WITH_KNOTS('',3,(#409046,#409047,#409048,#409049,
#409050,#409051,#409052),.UNSPECIFIED.,.F.,.F.,(4,3,4),(0.,6.9863024419149E-5,
0.000113969974038089),.UNSPECIFIED.);
#25839=B_SPLINE_CURVE_WITH_KNOTS('',3,(#409055,#409056,#409057,#409058,
#409059,#409060,#409061,#409062,#409063,#409064,#409065,#409066,#409067,
#409068,#409069,#409070,#409071,#409072,#409073,#409074,#409075,#409076,
#409077,#409078,#409079,#409080,#409081,#409082,#409083,#409084,#409085,
#409086,#409087,#409088,#409089,#409090,#409091,#409092,#409093,#409094,
#409095,#409096,#409097,#409098,#409099,#409100,#409101,#409102,#409103),
 .UNSPECIFIED.,.F.,.F.,(4,3,3,3,3,3,3,3,3,3,3,3,3,3,3,3,4),(0.,1.53100299373409E-6,
4.52554775679543E-6,7.0115124629162E-6,9.26752933800661E-6,1.03084066197173E-5,
1.17138990826866E-5,1.22284894984077E-5,1.30315035324818E-5,1.38363728497812E-5,
1.40464197777494E-5,1.54597749564641E-5,1.62073588704069E-5,1.92092968713103E-5,
1.95234416882556E-5,2.37637844577594E-5,2.61487188977262E-5),
 .UNSPECIFIED.);
#25840=B_SPLINE_CURVE_WITH_KNOTS('',3,(#409118,#409119,#409120,#409121,
#409122,#409123,#409124,#409125,#409126,#409127,#409128,#409129,#409130,
#409131,#409132,#409133,#409134,#409135,#409136,#409137,#409138,#409139,
#409140,#409141,#409142,#409143,#409144,#409145,#409146,#409147,#409148),
 .UNSPECIFIED.,.F.,.F.,(4,3,3,3,3,3,3,3,3,3,4),(0.,3.95507910398226E-6,
7.53768426604186E-6,1.19904533335351E-5,1.40475043392585E-5,1.51452104275963E-5,
1.67866272814373E-5,1.69621513005357E-5,1.81338315460711E-5,1.98906334656523E-5,
2.06132424588248E-5),.UNSPECIFIED.);
#25841=B_SPLINE_CURVE_WITH_KNOTS('',3,(#409151,#409152,#409153,#409154),
 .UNSPECIFIED.,.F.,.F.,(4,4),(9.69739903612216E-19,0.00010938435327491),
 .UNSPECIFIED.);
#25842=B_SPLINE_CURVE_WITH_KNOTS('',3,(#409181,#409182,#409183,#409184,
#409185,#409186,#409187,#409188,#409189,#409190,#409191,#409192,#409193,
#409194,#409195,#409196,#409197,#409198,#409199,#409200,#409201,#409202,
#409203,#409204,#409205,#409206,#409207,#409208,#409209,#409210,#409211,
#409212,#409213,#409214),.UNSPECIFIED.,.F.,.F.,(4,3,3,3,3,3,3,3,3,3,3,4),
(0.,2.09623992729454E-6,3.17176647120208E-6,4.82636181943714E-6,5.01000917339954E-6,
6.13126454147485E-6,8.6048665028884E-6,9.21144281170467E-6,1.24722301135978E-5,
1.42666454787854E-5,2.04670653756991E-5,2.08026438176802E-5),
 .UNSPECIFIED.);
#25843=B_SPLINE_CURVE_WITH_KNOTS('',3,(#409215,#409216,#409217,#409218),
 .UNSPECIFIED.,.F.,.F.,(4,4),(0.,0.000109384345496908),.UNSPECIFIED.);
#25844=B_SPLINE_CURVE_WITH_KNOTS('',3,(#409323,#409324,#409325,#409326),
 .UNSPECIFIED.,.F.,.F.,(4,4),(0.,9.54361881492177E-5),.UNSPECIFIED.);
#25845=B_SPLINE_CURVE_WITH_KNOTS('',3,(#409331,#409332,#409333,#409334,
#409335,#409336,#409337),.UNSPECIFIED.,.F.,.F.,(4,3,4),(0.,4.4106970432347E-5,
0.000113970027818833),.UNSPECIFIED.);
#25846=B_SPLINE_CURVE_WITH_KNOTS('',3,(#409343,#409344,#409345,#409346),
 .UNSPECIFIED.,.F.,.F.,(4,4),(4.33680868994202E-19,9.54361881492177E-5),
 .UNSPECIFIED.);
#25847=B_SPLINE_CURVE_WITH_KNOTS('',3,(#409350,#409351,#409352,#409353,
#409354,#409355,#409356),.UNSPECIFIED.,.F.,.F.,(4,3,4),(0.,6.98630244191492E-5,
0.000113969974038089),.UNSPECIFIED.);
#25848=B_SPLINE_CURVE_WITH_KNOTS('',3,(#409359,#409360,#409361,#409362,
#409363,#409364,#409365,#409366,#409367,#409368,#409369,#409370,#409371,
#409372,#409373,#409374,#409375,#409376,#409377,#409378,#409379,#409380,
#409381,#409382,#409383,#409384,#409385,#409386,#409387,#409388,#409389,
#409390,#409391,#409392,#409393,#409394,#409395,#409396,#409397,#409398,
#409399,#409400,#409401,#409402,#409403,#409404,#409405,#409406,#409407),
 .UNSPECIFIED.,.F.,.F.,(4,3,3,3,3,3,3,3,3,3,3,3,3,3,3,3,4),(0.,1.53100299373425E-6,
4.52554775679046E-6,7.01151246291605E-6,9.26752933801314E-6,1.03084066197174E-5,
1.17138990826863E-5,1.22284894984077E-5,1.30315035324819E-5,1.38363728497813E-5,
1.40464197777496E-5,1.54597749564642E-5,1.62073588704071E-5,1.92092968712869E-5,
1.95234416882558E-5,2.37637844577587E-5,2.61487188977268E-5),
 .UNSPECIFIED.);
#25849=B_SPLINE_CURVE_WITH_KNOTS('',3,(#409422,#409423,#409424,#409425,
#409426,#409427,#409428,#409429,#409430,#409431,#409432,#409433,#409434,
#409435,#409436,#409437,#409438,#409439,#409440,#409441,#409442,#409443,
#409444,#409445,#409446,#409447,#409448,#409449,#409450,#409451,#409452),
 .UNSPECIFIED.,.F.,.F.,(4,3,3,3,3,3,3,3,3,3,4),(0.,3.95507910398037E-6,
7.53768426604205E-6,1.1990453333535E-5,1.40475043392586E-5,1.51452104275966E-5,
1.67866272814047E-5,1.69621513005358E-5,1.81338315460714E-5,1.98906334656534E-5,
2.06132424588246E-5),.UNSPECIFIED.);
#25850=B_SPLINE_CURVE_WITH_KNOTS('',3,(#409455,#409456,#409457,#409458),
 .UNSPECIFIED.,.F.,.F.,(4,4),(9.69739903612216E-19,0.00010938435327491),
 .UNSPECIFIED.);
#25851=B_SPLINE_CURVE_WITH_KNOTS('',3,(#409485,#409486,#409487,#409488,
#409489,#409490,#409491,#409492,#409493,#409494,#409495,#409496,#409497,
#409498,#409499,#409500,#409501,#409502,#409503,#409504,#409505,#409506,
#409507,#409508,#409509,#409510,#409511,#409512,#409513,#409514,#409515,
#409516,#409517,#409518),.UNSPECIFIED.,.F.,.F.,(4,3,3,3,3,3,3,3,3,3,3,4),
(0.,2.09623992729449E-6,3.17176647120242E-6,4.8263618194437E-6,5.01000917339965E-6,
6.1312645414752E-6,8.60486650288857E-6,9.21144281170512E-6,1.24722301136084E-5,
1.42666454787857E-5,2.04670653757026E-5,2.08026438176804E-5),
 .UNSPECIFIED.);
#25852=B_SPLINE_CURVE_WITH_KNOTS('',3,(#409519,#409520,#409521,#409522),
 .UNSPECIFIED.,.F.,.F.,(4,4),(0.,0.000109384345496908),.UNSPECIFIED.);
#25853=B_SPLINE_CURVE_WITH_KNOTS('',3,(#410687,#410688,#410689,#410690,
#410691,#410692,#410693,#410694,#410695,#410696,#410697,#410698,#410699,
#410700),.UNSPECIFIED.,.F.,.F.,(4,2,2,2,2,2,4),(9.99952789110385E-7,0.0186719180275584,
0.0311918990740491,0.0543270273300624,0.071245591780139,0.0801745768203788,
0.0885356940042009),.UNSPECIFIED.);
#25854=B_SPLINE_CURVE_WITH_KNOTS('',3,(#410703,#410704,#410705,#410706,
#410707,#410708,#410709,#410710,#410711,#410712),.UNSPECIFIED.,.F.,.F.,
(4,2,2,2,4),(0.,0.0261563177202213,0.0514794122059591,0.0956126325182896,
0.112636617654083),.UNSPECIFIED.);
#25855=B_SPLINE_CURVE_WITH_KNOTS('',3,(#410717,#410718,#410719,#410720,
#410721,#410722,#410723,#410724,#410725,#410726,#410727,#410728,#410729,
#410730,#410731,#410732,#410733,#410734,#410735,#410736),.UNSPECIFIED.,
 .F.,.F.,(4,2,2,2,2,2,2,2,2,4),(-0.318111909131838,-0.302523038044006,-0.254842438467261,
-0.203675597428167,-0.169345881177067,-0.144533555287107,-0.118262221883461,
-0.0861048668116298,-0.0439870055810665,0.),.UNSPECIFIED.);
#25856=B_SPLINE_CURVE_WITH_KNOTS('',3,(#410743,#410744,#410745,#410746,
#410747,#410748,#410749,#410750,#410751,#410752,#410753,#410754,#410755,
#410756,#410757,#410758,#410759,#410760),.UNSPECIFIED.,.F.,.F.,(4,2,2,2,
2,2,2,2,4),(-0.448684784030478,-0.402273095639563,-0.343067075576419,-0.285995793781911,
-0.226278926910573,-0.167718843647999,-0.110407379121187,-0.0552345699471347,
-1.00000016339807E-6),.UNSPECIFIED.);
#25857=B_SPLINE_CURVE_WITH_KNOTS('',3,(#410763,#410764,#410765,#410766,
#410767,#410768,#410769,#410770,#410771,#410772,#410773,#410774,#410775,
#410776,#410777,#410778),.UNSPECIFIED.,.F.,.F.,(4,2,2,2,2,2,2,4),(-29.252097766018,
-29.2214975192493,-29.1900261579108,-29.1309979348172,-29.0708070130408,
-29.0132351605879,-28.9534122905398,-28.9187969711258),.UNSPECIFIED.);
#25858=B_SPLINE_CURVE_WITH_KNOTS('',3,(#410783,#410784,#410785,#410786,
#410787,#410788,#410789,#410790,#410791,#410792,#410793,#410794,#410795,
#410796,#410797,#410798,#410799,#410800,#410801,#410802,#410803,#410804,
#410805,#410806,#410807,#410808,#410809,#410810,#410811,#410812,#410813,
#410814,#410815,#410816,#410817,#410818),.UNSPECIFIED.,.F.,.F.,(4,2,2,2,
2,2,2,2,2,2,2,2,2,2,2,2,2,4),(-1.39493487964975,-1.33933536140023,-1.28047085435749,
-1.22343374849274,-1.16371361805528,-1.10549950745885,-1.04770400873729,
-0.987904720665793,-0.930362048538481,-0.870679137285274,-0.811661333086154,
-0.75465483523098,-0.694950459322707,-0.636580836693497,-0.579072284415414,
-0.51909849981813,-0.461399377221561,-0.448684784030478),.UNSPECIFIED.);
#25859=B_SPLINE_CURVE_WITH_KNOTS('',3,(#410819,#410820,#410821,#410822,
#410823,#410824,#410825,#410826,#410827,#410828,#410829,#410830,#410831,
#410832,#410833,#410834,#410835,#410836,#410837,#410838,#410839,#410840,
#410841,#410842,#410843,#410844,#410845,#410846,#410847,#410848,#410849,
#410850,#410851,#410852,#410853,#410854),.UNSPECIFIED.,.F.,.F.,(4,2,2,2,
2,2,2,2,2,2,2,2,2,2,2,2,2,4),(-28.9187969711258,-28.8952823866813,-28.8370354169342,
-28.7771755690868,-28.7199637678638,-28.6610635136513,-28.6012229559858,
-28.5437786457582,-28.484099470417,-28.4254825927288,-28.3673557383989,
-28.3069171786156,-28.2495271665763,-28.1907246371527,-28.1308478746926,
-28.0735736519825,-28.014124865578,-27.9698505015162),.UNSPECIFIED.);
#25860=B_SPLINE_CURVE_WITH_KNOTS('',3,(#410859,#410860,#410861,#410862,
#410863,#410864,#410865,#410866,#410867,#410868,#410869,#410870,#410871,
#410872,#410873,#410874,#410875,#410876,#410877,#410878,#410879,#410880,
#410881,#410882,#410883,#410884,#410885,#410886,#410887,#410888,#410889,
#410890,#410891,#410892,#410893,#410894,#410895,#410896),.UNSPECIFIED.,
 .F.,.F.,(4,2,2,2,2,2,2,2,2,2,2,2,2,2,2,2,2,2,4),(-2.34124852806073,-2.33690126303019,
-2.27724350495715,-2.21871612127065,-2.16148516986521,-2.10133374186191,
-2.04347846587669,-1.98493722241918,-1.92554377967373,-1.86833924331538,
-1.80863346889893,-1.74988209422244,-1.69273225729192,-1.6329697831651,
-1.57487144052691,-1.51672143261483,-1.45705664513422,-1.39963367235311,
-1.39493487964975),.UNSPECIFIED.);
#25861=B_SPLINE_CURVE_WITH_KNOTS('',3,(#410897,#410898,#410899,#410900,
#410901,#410902,#410903,#410904,#410905,#410906,#410907,#410908,#410909,
#410910,#410911,#410912,#410913,#410914,#410915,#410916,#410917,#410918,
#410919,#410920,#410921,#410922,#410923,#410924,#410925,#410926,#410927,
#410928,#410929,#410930,#410931,#410932),.UNSPECIFIED.,.F.,.F.,(4,2,2,2,
2,2,2,2,2,2,2,2,2,2,2,2,2,4),(-27.9698505015162,-27.955092905267,-27.8971690368431,
-27.8369554028138,-27.7794155920712,-27.720819041241,-27.6609693585283,
-27.603807699935,-27.5445624577898,-27.4850125493338,-27.4272615418296,
-27.367240259664,-27.3094538969521,-27.2510306695638,-27.1911785131228,
-27.1340307959517,-27.0749567020895,-27.0213445386482),.UNSPECIFIED.);
#25862=B_SPLINE_CURVE_WITH_KNOTS('',3,(#410937,#410938,#410939,#410940,
#410941,#410942,#410943,#410944,#410945,#410946,#410947,#410948,#410949,
#410950,#410951,#410952,#410953,#410954,#410955,#410956,#410957,#410958,
#410959,#410960,#410961,#410962,#410963,#410964,#410965,#410966,#410967,
#410968,#410969,#410970,#410971,#410972),.UNSPECIFIED.,.F.,.F.,(4,2,2,2,
2,2,2,2,2,2,2,2,2,2,2,2,2,4),(-3.28643685670557,-3.27350661120751,-3.21586205750387,
-3.15594429548082,-3.098512889948,-3.0401985470805,-2.98056057243175,-2.92361641153634,
-2.86465472519906,-2.8050704439123,-2.74758405487526,-2.68784265002696,
-2.63012907375782,-2.57197212213701,-2.5123199119751,-2.455350141073,-2.39654364425808,
-2.34124852806073),.UNSPECIFIED.);
#25863=B_SPLINE_CURVE_WITH_KNOTS('',3,(#410973,#410974,#410975,#410976,
#410977,#410978,#410979,#410980,#410981,#410982,#410983,#410984,#410985,
#410986,#410987,#410988,#410989,#410990,#410991,#410992,#410993,#410994,
#410995,#410996,#410997,#410998,#410999,#411000,#411001,#411002,#411003,
#411004,#411005,#411006,#411007,#411008,#411009,#411010),.UNSPECIFIED.,
 .F.,.F.,(4,2,2,2,2,2,2,2,2,2,2,2,2,2,2,2,2,2,4),(-27.0213445386482,-27.0148137389868,
-26.9572008257476,-26.8973340689325,-26.8392212916929,-26.7809336352533,
-26.7210515782496,-26.6638279821658,-26.6048870671248,-26.5450228255409,
-26.4875402157774,-26.4278201148169,-26.3692342439642,-26.3110698385162,
-26.2505905031186,-26.1932005595953,-26.1343598543634,-26.0744661565355,
-26.0721220179853),.UNSPECIFIED.);
#25864=B_SPLINE_CURVE_WITH_KNOTS('',3,(#411015,#411016,#411017,#411018,
#411019,#411020,#411021,#411022,#411023,#411024,#411025,#411026,#411027,
#411028,#411029,#411030,#411031,#411032,#411033,#411034,#411035,#411036,
#411037,#411038,#411039,#411040,#411041,#411042,#411043,#411044,#411045,
#411046,#411047,#411048,#411049,#411050),.UNSPECIFIED.,.F.,.F.,(4,2,2,2,
2,2,2,2,2,2,2,2,2,2,2,2,2,4),(-4.23227875089979,-4.19308958251698,-4.15252126808739,
-4.09276835801667,-4.03561843556799,-3.97689033723292,-3.91719298824817,
-3.86001020997198,-3.80063980222867,-3.74206692752785,-3.68423228988271,
-3.62410352474105,-3.56686359207517,-3.50835716243747,-3.44870502120367,
-3.39169065880464,-3.33253914286054,-3.28643685670557),.UNSPECIFIED.);
#25865=B_SPLINE_CURVE_WITH_KNOTS('',3,(#411051,#411052,#411053,#411054,
#411055,#411056,#411057,#411058,#411059,#411060,#411061,#411062,#411063,
#411064,#411065,#411066,#411067,#411068,#411069,#411070,#411071,#411072,
#411073,#411074,#411075,#411076,#411077,#411078,#411079,#411080,#411081,
#411082,#411083,#411084,#411085,#411086),.UNSPECIFIED.,.F.,.F.,(4,2,2,2,
2,2,2,2,2,2,2,2,2,2,2,2,2,4),(-26.0721220179853,-26.017160626507,-25.9576738740858,
-25.8986866001961,-25.8407285543548,-25.7804777660194,-25.7229503409938,
-25.6643192415877,-25.6044563774412,-25.5472754027841,-25.487995756455,
-25.4285015946258,-25.3707203304554,-25.3106661519921,-25.2529032223508,
-25.1944497076039,-25.1345878127328,-25.1233625871879),.UNSPECIFIED.);
#25866=B_SPLINE_CURVE_WITH_KNOTS('',3,(#411091,#411092,#411093,#411094,
#411095,#411096,#411097,#411098,#411099,#411100,#411101,#411102,#411103,
#411104,#411105,#411106,#411107,#411108,#411109,#411110,#411111,#411112,
#411113,#411114,#411115,#411116,#411117,#411118,#411119,#411120,#411121,
#411122,#411123,#411124,#411125,#411126),.UNSPECIFIED.,.F.,.F.,(4,2,2,2,
2,2,2,2,2,2,2,2,2,2,2,2,2,4),(-0.944730488315757,-0.89891383387179,-0.839824556627243,
-0.78287389958975,-0.723293190895891,-0.664848091483223,-0.60768489144294,
-0.547618518959442,-0.489844548217535,-0.431362885084828,-0.372053706579833,
-0.31493020374114,-0.255302759125205,-0.196634951286046,-0.13955662032141,
-0.079873041517757,-0.0392464748727053,-9.99999999806711E-7),
 .UNSPECIFIED.);
#25867=B_SPLINE_CURVE_WITH_KNOTS('',3,(#411127,#411128,#411129,#411130,
#411131,#411132,#411133,#411134,#411135,#411136,#411137,#411138,#411139,
#411140,#411141,#411142,#411143,#411144,#411145,#411146,#411147,#411148,
#411149,#411150,#411151,#411152,#411153,#411154,#411155,#411156,#411157,
#411158,#411159,#411160,#411161,#411162),.UNSPECIFIED.,.F.,.F.,(4,2,2,2,
2,2,2,2,2,2,2,2,2,2,2,2,2,4),(-25.1233625871879,-25.0774324454709,-25.0183282037482,
-24.9582481821066,-24.9006094766757,-24.840714684202,-24.7826335346738,
-24.7243204209327,-24.6644318447055,-24.6072106427378,-24.5482444597356,
-24.4883721594139,-24.4308662178888,-24.3711207220799,-24.3125804351149,
-24.2543935715963,-24.1938891267832,-24.1742281370664),.UNSPECIFIED.);
#25868=B_SPLINE_CURVE_WITH_KNOTS('',3,(#411167,#411168,#411169,#411170,
#411171,#411172,#411173,#411174,#411175,#411176,#411177,#411178,#411179,
#411180,#411181,#411182,#411183,#411184,#411185,#411186,#411187,#411188,
#411189,#411190,#411191,#411192,#411193,#411194,#411195,#411196,#411197,
#411198,#411199,#411200,#411201,#411202),.UNSPECIFIED.,.F.,.F.,(4,2,2,2,
2,2,2,2,2,2,2,2,2,2,2,2,2,4),(-1.88876307323747,-1.83374485867437,-1.77500354530042,
-1.71810670339158,-1.65852871296345,-1.60043603772057,-1.54280856206037,
-1.48313244688252,-1.42570940700207,-1.3662265269564,-1.30732839246978,
-1.25045268050273,-1.19088756813138,-1.13263588100429,-1.07528621171883,
-1.01543214034352,-0.957849461381783,-0.944730488315757),.UNSPECIFIED.);
#25869=B_SPLINE_CURVE_WITH_KNOTS('',3,(#411203,#411204,#411205,#411206,
#411207,#411208,#411209,#411210,#411211,#411212,#411213,#411214,#411215,
#411216,#411217,#411218,#411219,#411220,#411221,#411222,#411223,#411224,
#411225,#411226,#411227,#411228,#411229,#411230,#411231,#411232,#411233,
#411234,#411235,#411236,#411237,#411238),.UNSPECIFIED.,.F.,.F.,(4,2,2,2,
2,2,2,2,2,2,2,2,2,2,2,2,2,4),(-24.1742281370664,-24.1365133939231,-24.0776497602422,
-24.0177548187665,-23.9604318660005,-23.900922584465,-23.8419950479497,
-23.784017836623,-23.7237454632829,-23.6662448206979,-23.6075943276575,
-23.5477340504698,-23.490547683915,-23.431248972548,-23.3718262730906,-23.3140296905872,
-23.2539581003242,-23.2253117019651),.UNSPECIFIED.);
#25870=B_SPLINE_CURVE_WITH_KNOTS('',3,(#411243,#411244,#411245,#411246,
#411247,#411248,#411249,#411250,#411251,#411252,#411253,#411254,#411255,
#411256,#411257,#411258,#411259,#411260,#411261,#411262,#411263,#411264,
#411265,#411266,#411267,#411268,#411269,#411270,#411271,#411272,#411273,
#411274,#411275,#411276,#411277,#411278,#411279,#411280),.UNSPECIFIED.,
 .F.,.F.,(4,2,2,2,2,2,2,2,2,2,2,2,2,2,2,2,2,2,4),(-2.83384756662789,-2.82992577270359,
-2.77028071294861,-2.71174863608066,-2.65454520039306,-2.59438770365034,
-2.53652788636405,-2.47803964435339,-2.41863952240411,-2.3614616687963,
-2.30186610646549,-2.24324200557333,-2.18624034144377,-2.12662278956109,
-2.0686498962575,-2.01067448075632,-1.95113688511984,-1.89383724909564,
-1.88876307323747),.UNSPECIFIED.);
#25871=B_SPLINE_CURVE_WITH_KNOTS('',3,(#411281,#411282,#411283,#411284,
#411285,#411286,#411287,#411288,#411289,#411290,#411291,#411292,#411293,
#411294,#411295,#411296,#411297,#411298,#411299,#411300,#411301,#411302,
#411303,#411304,#411305,#411306,#411307,#411308,#411309,#411310,#411311,
#411312,#411313,#411314,#411315,#411316),.UNSPECIFIED.,.F.,.F.,(4,2,2,2,
2,2,2,2,2,2,2,2,2,2,2,2,2,4),(-23.2253117019651,-23.1962333650746,-23.1377646400003,
-23.07790884712,-23.0207599950722,-22.9616408595193,-22.901640253111,-22.8439906425578,
-22.7840832422152,-22.7260491100111,-22.6677255703613,-22.607846381989,
-22.5506421242094,-22.4916658766836,-22.4318013315578,-22.3742868685931,
-22.3145313196031,-22.2764817495763),.UNSPECIFIED.);
#25872=B_SPLINE_CURVE_WITH_KNOTS('',3,(#411321,#411322,#411323,#411324,
#411325,#411326,#411327,#411328,#411329,#411330,#411331,#411332,#411333,
#411334,#411335,#411336,#411337,#411338,#411339,#411340,#411341,#411342,
#411343,#411344,#411345,#411346,#411347,#411348,#411349,#411350,#411351,
#411352,#411353,#411354,#411355,#411356),.UNSPECIFIED.,.F.,.F.,(4,2,2,2,
2,2,2,2,2,2,2,2,2,2,2,2,2,4),(-3.77882842551939,-3.76608750396215,-3.70645290327603,
-3.64828276634858,-3.59063907211679,-3.53088137745131,-3.47338129154192,
-3.41391599771162,-3.35493498255763,-3.29799778855135,-3.23837239214353,
-3.18003818569917,-3.12266132771161,-3.06272059889875,-3.00505620957078,
-2.94612783742944,-2.88695126997501,-2.83384756662789),.UNSPECIFIED.);
#25873=B_SPLINE_CURVE_WITH_KNOTS('',3,(#411357,#411358,#411359,#411360,
#411361,#411362,#411363,#411364,#411365,#411366,#411367,#411368,#411369,
#411370,#411371,#411372,#411373,#411374,#411375,#411376,#411377,#411378,
#411379,#411380,#411381,#411382,#411383,#411384,#411385,#411386,#411387,
#411388,#411389,#411390,#411391,#411392),.UNSPECIFIED.,.F.,.F.,(4,2,2,2,
2,2,2,2,2,2,2,2,2,2,2,2,2,4),(-22.2764817495763,-22.2560524818532,-22.1978581171903,
-22.1373440487818,-22.0799972717364,-22.0211258149661,-21.9612456561173,
-21.9039190783511,-21.8444025770243,-21.7855514269224,-21.7275699960986,
-21.6672915008503,-21.6098329067871,-21.5511781074627,-21.4913366101491,
-21.4341589326486,-21.3748564408681,-21.3276223997873),.UNSPECIFIED.);
#25874=B_SPLINE_CURVE_WITH_KNOTS('',3,(#411397,#411398,#411399,#411400,
#411401,#411402,#411403,#411404,#411405,#411406,#411407,#411408,#411409,
#411410,#411411,#411412,#411413,#411414,#411415,#411416,#411417,#411418,
#411419,#411420,#411421,#411422,#411423,#411424,#411425,#411426,#411427,
#411428,#411429,#411430,#411431,#411432),.UNSPECIFIED.,.F.,.F.,(4,2,2,2,
2,2,2,2,2,2,2,2,2,2,2,2,2,4),(-4.72451512913708,-4.70335422218615,-4.64312396621101,
-4.58519588309839,-4.52671311480439,-4.46724031581326,-4.40999362694196,
-4.35034348430204,-4.29164723103953,-4.23460643249447,-4.1749357076431,
-4.11689093893578,-4.05890677016987,-3.99929325395434,-3.94192176952015,
-3.88185265443699,-3.82303353231637,-3.77882842551939),.UNSPECIFIED.);
#25875=B_SPLINE_CURVE_WITH_KNOTS('',3,(#411433,#411434,#411435,#411436,
#411437,#411438,#411439,#411440,#411441,#411442,#411443,#411444,#411445,
#411446,#411447,#411448,#411449,#411450,#411451,#411452,#411453,#411454,
#411455,#411456,#411457,#411458,#411459,#411460,#411461,#411462,#411463,
#411464,#411465,#411466,#411467,#411468),.UNSPECIFIED.,.F.,.F.,(4,2,2,2,
2,2,2,2,2,2,2,2,2,2,2,2,2,4),(-21.3276223997873,-21.315522792052,-21.2577258448043,
-21.1976523083246,-21.1399816112249,-21.0815127725348,-21.0216794298315,
-20.9645516701281,-20.905432926813,-20.8455302924166,-20.7878847716901,
-20.7279802727358,-20.6700098901345,-20.6116910755317,-20.5518377670118,
-20.494665655196,-20.4356946787015,-20.3793176857869),.UNSPECIFIED.);
#25876=B_SPLINE_CURVE_WITH_KNOTS('',3,(#411473,#411474,#411475,#411476,
#411477,#411478,#411479,#411480,#411481,#411482,#411483,#411484,#411485,
#411486,#411487,#411488,#411489,#411490,#411491,#411492,#411493,#411494,
#411495,#411496,#411497,#411498,#411499,#411500,#411501,#411502,#411503,
#411504,#411505,#411506,#411507,#411508),.UNSPECIFIED.,.F.,.F.,(4,2,2,2,
2,2,2,2,2,2,2,2,2,2,2,2,2,4),(-5.6703237369621,-5.6401640324469,-5.58034229299679,
-5.52278198432739,-5.46334602502765,-5.40429963955564,-5.34731581221613,
-5.28764667344074,-5.22924728617809,-5.17185644587178,-5.1118469911605,
-5.05411807632568,-4.99520867883528,-4.93596276363503,-4.87887805740263,
-4.81918542463239,-4.76058413611294,-4.72451512913708),.UNSPECIFIED.);
#25877=B_SPLINE_CURVE_WITH_KNOTS('',3,(#411509,#411510,#411511,#411512,
#411513,#411514,#411515,#411516,#411517,#411518,#411519,#411520,#411521,
#411522,#411523,#411524,#411525,#411526,#411527,#411528,#411529,#411530,
#411531,#411532,#411533,#411534,#411535,#411536,#411537,#411538,#411539,
#411540,#411541,#411542,#411543,#411544,#411545,#411546),.UNSPECIFIED.,
 .F.,.F.,(4,2,2,2,2,2,2,2,2,2,2,2,2,2,2,2,2,2,4),(-20.3793176857869,-20.3758542519859,
-20.3183462325325,-20.258596103042,-20.2001962515831,-20.1420095197077,
-20.0815014526744,-20.0241992831074,-19.965335281199,-19.9054866447767,
-19.8481703716897,-19.7886621540349,-19.7299060833526,-19.6719356291545,
-19.6116666905878,-19.5542666265083,-19.4956228575489,-19.4358171532103,
-19.430746292065),.UNSPECIFIED.);
#25878=B_SPLINE_CURVE_WITH_KNOTS('',3,(#411551,#411552,#411553,#411554,
#411555,#411556,#411557,#411558,#411559,#411560,#411561,#411562,#411563,
#411564,#411565,#411566,#411567,#411568,#411569,#411570,#411571,#411572,
#411573,#411574,#411575,#411576,#411577,#411578,#411579,#411580,#411581,
#411582,#411583,#411584,#411585,#411586),.UNSPECIFIED.,.F.,.F.,(4,2,2,2,
2,2,2,2,2,2,2,2,2,2,2,2,2,4),(-6.61638032040915,-6.57683132059212,-6.51730270007273,
-6.46000337416112,-6.40031485620181,-6.3415631731461,-6.28449742901715,
-6.22478976022181,-6.16668968388983,-6.10870989485898,-6.04903759303528,
-5.99161071586561,-5.93157704581943,-5.87269722883836,-5.81571640218553,
-5.75604157196716,-5.69781092401279,-5.6703237369621),.UNSPECIFIED.);
#25879=B_SPLINE_CURVE_WITH_KNOTS('',3,(#411587,#411588,#411589,#411590,
#411591,#411592,#411593,#411594,#411595,#411596,#411597,#411598,#411599,
#411600,#411601,#411602,#411603,#411604,#411605,#411606,#411607,#411608,
#411609,#411610,#411611,#411612,#411613,#411614,#411615,#411616,#411617,
#411618,#411619,#411620,#411621,#411622),.UNSPECIFIED.,.F.,.F.,(4,2,2,2,
2,2,2,2,2,2,2,2,2,2,2,2,2,4),(-19.430746292065,-19.3786626458029,-19.3193719271923,
-19.2601473120078,-19.202365288945,-19.1423055783792,-19.0847064067758,
-19.0262528917624,-18.9664592661961,-18.9093678742006,-18.8502651679771,
-18.7904817479002,-18.7328557461471,-18.6729700713912,-18.6150819830984,
-18.5567834921217,-18.4969735651087,-18.4831085248443),.UNSPECIFIED.);
#25880=B_SPLINE_CURVE_WITH_KNOTS('',3,(#411627,#411628,#411629,#411630,
#411631,#411632,#411633,#411634,#411635,#411636,#411637,#411638,#411639,
#411640,#411641,#411642,#411643,#411644,#411645,#411646,#411647,#411648,
#411649,#411650,#411651,#411652,#411653,#411654,#411655,#411656,#411657,
#411658,#411659,#411660,#411661,#411662),.UNSPECIFIED.,.F.,.F.,(4,2,2,2,
2,2,2,2,2,2,2,2,2,2,2,2,2,4),(-7.56280299453309,-7.51397579813351,-7.45488040556703,
-7.39786421449172,-7.33816724403201,-7.27971887007593,-7.2223274578691,
-7.16226598726619,-7.10448859217055,-7.04561085958982,-6.98631222207624,
-6.92918301214771,-6.86945880028599,-6.81080474940593,-6.75356199202847,
-6.69327594632736,-6.63529587538185,-6.61638032040915),.UNSPECIFIED.);
#25881=B_SPLINE_CURVE_WITH_KNOTS('',3,(#411663,#411664,#411665,#411666,
#411667,#411668,#411669,#411670,#411671,#411672,#411673,#411674,#411675,
#411676,#411677,#411678,#411679,#411680,#411681,#411682,#411683,#411684,
#411685,#411686,#411687,#411688,#411689,#411690,#411691,#411692,#411693,
#411694,#411695,#411696,#411697,#411698),.UNSPECIFIED.,.F.,.F.,(4,2,2,2,
2,2,2,2,2,2,2,2,2,2,2,2,2,4),(-18.4831085248443,-18.4398497946047,-18.380899890151,
-18.3204993686696,-18.2629925038568,-18.2032407246096,-18.1449965661139,
-18.0868132197128,-18.0269603906926,-17.9697223292667,-17.9108849184451,
-17.8510886466108,-17.7938001957988,-17.7343196761421,-17.67568170974,-17.6177412516345,
-17.5575015042724,-17.5352552553618),.UNSPECIFIED.);
#25882=B_SPLINE_CURVE_WITH_KNOTS('',3,(#411703,#411704,#411705,#411706,
#411707,#411708,#411709,#411710,#411711,#411712,#411713,#411714,#411715,
#411716,#411717,#411718,#411719,#411720,#411721,#411722,#411723,#411724,
#411725,#411726,#411727,#411728,#411729,#411730,#411731,#411732,#411733,
#411734,#411735,#411736,#411737,#411738),.UNSPECIFIED.,.F.,.F.,(4,2,2,2,
2,2,2,2,2,2,2,2,2,2,2,2,2,4),(-8.50901833843302,-8.45124527059382,-8.39245399423659,
-8.33537735697918,-8.27564850600765,-8.21750880066048,-8.15954706413863,
-8.09983214948009,-8.04236543464371,-7.98238065207383,-7.92345623462138,
-7.86645466749089,-7.80675544179799,-7.74848021261672,-7.69084355693561,
-7.63097421057873,-7.57336947764254,-7.56280299453309),.UNSPECIFIED.);
#25883=B_SPLINE_CURVE_WITH_KNOTS('',3,(#411739,#411740,#411741,#411742,
#411743,#411744,#411745,#411746,#411747,#411748,#411749,#411750,#411751,
#411752,#411753,#411754,#411755,#411756,#411757,#411758,#411759,#411760,
#411761,#411762,#411763,#411764,#411765,#411766,#411767,#411768,#411769,
#411770,#411771,#411772,#411773,#411774),.UNSPECIFIED.,.F.,.F.,(4,2,2,2,
2,2,2,2,2,2,2,2,2,2,2,2,2,4),(-17.5352552553618,-17.500180410977,-17.4415668719403,
-17.3818181228442,-17.3247049097442,-17.2654454327972,-17.206354372399,
-17.1486063958803,-17.0885802481066,-17.0310741987563,-16.9726553175311,
-16.9129228707841,-16.8558868680907,-16.7968197671686,-16.7371815652351,
-16.6795943612501,-16.6197474148233,-16.5884934184433),.UNSPECIFIED.);
#25884=B_SPLINE_CURVE_WITH_KNOTS('',3,(#411779,#411780,#411781,#411782,
#411783,#411784,#411785,#411786,#411787,#411788,#411789,#411790,#411791,
#411792,#411793,#411794,#411795,#411796,#411797,#411798,#411799,#411800,
#411801,#411802,#411803,#411804,#411805,#411806,#411807,#411808,#411809,
#411810,#411811,#411812,#411813,#411814,#411815,#411816),.UNSPECIFIED.,
 .F.,.F.,(4,2,2,2,2,2,2,2,2,2,2,2,2,2,2,2,2,2,4),(-9.45584958042892,-9.44911444362682,
-9.38940529455709,-9.33092340536227,-9.27354521692587,-9.21344765892337,
-9.155637109888,-9.09680483889744,-9.03746929681846,-8.98030972495833,-8.92056958790122,
-8.86187841179889,-8.8046365842075,-8.74431084730452,-8.68629426447876,
-8.62786150582668,-8.56829303638661,-8.51095644498227,-8.50901833843302),
 .UNSPECIFIED.);
#25885=B_SPLINE_CURVE_WITH_KNOTS('',3,(#411817,#411818,#411819,#411820,
#411821,#411822,#411823,#411824,#411825,#411826,#411827,#411828,#411829,
#411830,#411831,#411832,#411833,#411834,#411835,#411836,#411837,#411838,
#411839,#411840,#411841,#411842,#411843,#411844,#411845,#411846,#411847,
#411848,#411849,#411850,#411851,#411852),.UNSPECIFIED.,.F.,.F.,(4,2,2,2,
2,2,2,2,2,2,2,2,2,2,2,2,2,4),(-16.5884934184433,-16.5619644526248,-16.503705774757,
-16.4439609680891,-16.3869056210481,-16.3279965296225,-16.2677480157603,
-16.2102853322193,-16.1505781319643,-16.0924474020868,-16.0343096714123,
-15.9745257154597,-15.9173667627273,-15.858576053134,-15.7988139394776,
-15.7414738213889,-15.6819049547259,-15.6412631971223),.UNSPECIFIED.);
#25886=B_SPLINE_CURVE_WITH_KNOTS('',3,(#411857,#411858,#411859,#411860,
#411861,#411862,#411863,#411864,#411865,#411866,#411867,#411868,#411869,
#411870,#411871,#411872,#411873,#411874,#411875,#411876,#411877,#411878,
#411879,#411880,#411881,#411882,#411883,#411884,#411885,#411886,#411887,
#411888,#411889,#411890,#411891,#411892),.UNSPECIFIED.,.F.,.F.,(4,2,2,2,
2,2,2,2,2,2,2,2,2,2,2,2,2,4),(-10.4021183806393,-10.386719146917,-10.3269847666313,
-10.2688206008513,-10.2108913298445,-10.151149408754,-10.0936578908522,
-10.0337368539799,-9.97478331397539,-9.91777498482906,-9.85806701687237,
-9.799762515331,-9.7421501230139,-9.68224892850401,-9.62461494536425,-9.56527779334546,
-9.50614904066621,-9.45584958042892),.UNSPECIFIED.);
#25887=B_SPLINE_CURVE_WITH_KNOTS('',3,(#411893,#411894,#411895,#411896,
#411897,#411898,#411899,#411900,#411901,#411902,#411903,#411904,#411905,
#411906,#411907,#411908,#411909,#411910,#411911,#411912,#411913,#411914,
#411915,#411916,#411917,#411918,#411919,#411920,#411921,#411922,#411923,
#411924,#411925,#411926,#411927,#411928),.UNSPECIFIED.,.F.,.F.,(4,2,2,2,
2,2,2,2,2,2,2,2,2,2,2,2,2,4),(-15.6412631971223,-15.6232621654782,-15.5652383608721,
-15.5049100990898,-15.4475507430787,-15.3888527523259,-15.3290420567482,
-15.2718562157653,-15.2125120001521,-15.1534299096715,-15.0956026159645,
-15.0354923063713,-14.9779609251807,-14.9194619385247,-14.859671528249,
-14.7998614516463,-14.7407724105526,-14.6934485066097),.UNSPECIFIED.);
#25888=B_SPLINE_CURVE_WITH_KNOTS('',3,(#411933,#411934,#411935,#411936,
#411937,#411938,#411939,#411940,#411941,#411942,#411943,#411944,#411945,
#411946,#411947,#411948,#411949,#411950,#411951,#411952,#411953,#411954,
#411955,#411956,#411957,#411958,#411959,#411960,#411961,#411962,#411963,
#411964,#411965,#411966,#411967,#411968),.UNSPECIFIED.,.F.,.F.,(4,2,2,2,
2,2,2,2,2,2,2,2,2,2,2,2,2,4),(-11.3489937993946,-11.3249843416779,-11.2648662095898,
-11.2070374667164,-11.1482657581736,-11.0889086914385,-11.0317325945659,
-10.9719921941038,-10.9132790829149,-10.8560523203481,-10.7957024975594,
-10.7376644394895,-10.6792780872413,-10.6196852385539,-10.5623262920233,
-10.5026080478968,-10.4437925103076,-10.4021183806393),.UNSPECIFIED.);
#25889=B_SPLINE_CURVE_WITH_KNOTS('',3,(#411969,#411970,#411971,#411972,
#411973,#411974,#411975,#411976,#411977,#411978,#411979,#411980,#411981,
#411982,#411983,#411984,#411985,#411986,#411987,#411988,#411989,#411990,
#411991,#411992,#411993,#411994,#411995,#411996,#411997,#411998,#411999,
#412000,#412001,#412002,#412003,#412004),.UNSPECIFIED.,.F.,.F.,(4,2,2,2,
2,2,2,2,2,2,2,2,2,2,2,2,2,4),(-14.6934485066097,-14.6836861362662,-14.6238970756216,
-14.5654572878687,-14.5078495561536,-14.4478047028095,-14.3900363319137,
-14.3307889482682,-14.2715136232438,-14.214369456016,-14.1545698698913,
-14.0959415700337,-14.0385380206706,-13.9782856780034,-13.920330482637,
-13.861557025611,-13.8020656366167,-13.7456759924953),.UNSPECIFIED.);
#25890=B_SPLINE_CURVE_WITH_KNOTS('',3,(#412009,#412010,#412011,#412012,
#412013,#412014,#412015,#412016,#412017,#412018,#412019,#412020,#412021,
#412022,#412023,#412024,#412025,#412026,#412027,#412028,#412029,#412030,
#412031,#412032,#412033,#412034,#412035,#412036,#412037,#412038,#412039,
#412040,#412041,#412042,#412043,#412044),.UNSPECIFIED.,.F.,.F.,(4,2,2,2,
2,2,2,2,2,2,2,2,2,2,2,2,2,4),(-12.2951758260951,-12.2622146747337,-12.2024611309874,
-12.1449596563198,-12.0851189116652,-12.0261514566002,-11.9691505120521,
-11.9094496220735,-11.8511308784967,-11.7935575205291,-11.7336399120256,
-11.6759915704143,-11.6167267251397,-11.5575798993392,-11.5005407874677,
-11.4408352033144,-11.3823349014934,-11.3489937993946),.UNSPECIFIED.);
#25891=B_SPLINE_CURVE_WITH_KNOTS('',3,(#412045,#412046,#412047,#412048,
#412049,#412050,#412051,#412052,#412053,#412054,#412055,#412056,#412057,
#412058,#412059,#412060,#412061,#412062,#412063,#412064,#412065,#412066,
#412067,#412068,#412069,#412070,#412071,#412072,#412073,#412074,#412075,
#412076,#412077,#412078,#412079,#412080,#412081,#412082),.UNSPECIFIED.,
 .F.,.F.,(4,2,2,2,2,2,2,2,2,2,2,2,2,2,2,2,2,2,4),(-13.7456759924953,-13.7447648028767,
-13.6849239856238,-13.6260769231875,-13.5687767156984,-13.5082867134724,
-13.4501166203179,-13.3917056147048,-13.33197351399,-13.274482363316,-13.2146526609845,
-13.1556995000451,-13.0985341732067,-13.0386908974151,-12.9803898917325,
-12.9224141846065,-12.8625287398785,-12.8049010444645,-12.7971116521498),
 .UNSPECIFIED.);
#25892=B_SPLINE_CURVE_WITH_KNOTS('',3,(#412087,#412088,#412089,#412090,
#412091,#412092,#412093,#412094,#412095,#412096,#412097,#412098,#412099,
#412100,#412101,#412102,#412103,#412104,#412105,#412106,#412107,#412108,
#412109,#412110,#412111,#412112,#412113,#412114,#412115,#412116,#412117,
#412118,#412119,#412120,#412121,#412122),.UNSPECIFIED.,.F.,.F.,(4,2,2,2,
2,2,2,2,2,2,2,2,2,2,2,2,2,4),(-13.2418576554979,-13.1994627179258,-13.1400993991086,
-13.0829205413793,-13.0231958951588,-12.9644759169146,-12.9072789732011,
-12.8469205098662,-12.7888758968419,-12.7305518663979,-12.6709499395033,
-12.6135834105728,-12.5538738930924,-12.4950492574587,-12.4379937120229,
-12.3782696936795,-12.320096058402,-12.2951758260951),.UNSPECIFIED.);
#25893=B_SPLINE_CURVE_WITH_KNOTS('',3,(#412123,#412124,#412125,#412126,
#412127,#412128,#412129,#412130,#412131,#412132,#412133,#412134,#412135,
#412136,#412137,#412138,#412139,#412140,#412141,#412142,#412143,#412144,
#412145,#412146,#412147,#412148,#412149,#412150,#412151,#412152,#412153,
#412154,#412155,#412156,#412157,#412158),.UNSPECIFIED.,.F.,.F.,(4,2,2,2,
2,2,2,2,2,2,2,2,2,2,2,2,2,4),(-12.7971116521498,-12.7449803461602,-12.6858813644011,
-12.6287647223206,-12.5689427484863,-12.5104936506619,-12.4528213673699,
-12.3927688262555,-12.3349914868138,-12.2756431323407,-12.2163620826767,
-12.1592003952585,-12.0993717077836,-12.0407383394206,-11.9832827998924,
-11.9230269897282,-11.8650667255099,-11.8489689543484),.UNSPECIFIED.);
#25894=B_SPLINE_CURVE_WITH_KNOTS('',3,(#412163,#412164,#412165,#412166,
#412167,#412168,#412169,#412170,#412171,#412172,#412173,#412174,#412175,
#412176,#412177,#412178,#412179,#412180,#412181,#412182,#412183,#412184,
#412185,#412186,#412187,#412188,#412189,#412190,#412191,#412192,#412193,
#412194,#412195,#412196,#412197,#412198),.UNSPECIFIED.,.F.,.F.,(4,2,2,2,
2,2,2,2,2,2,2,2,2,2,2,2,2,4),(-14.1877310170691,-14.135988915634,-14.0770228047692,
-14.0200438189143,-13.960366357188,-13.9020484410295,-13.8445300138478,
-13.7846114265274,-13.7269636528436,-13.6677887881959,-13.6086391417175,
-13.5516095772968,-13.491923747917,-13.4334200881425,-13.376112447951,-13.3159891690372,
-13.2581571460718,-13.2418576554979),.UNSPECIFIED.);
#25895=B_SPLINE_CURVE_WITH_KNOTS('',3,(#412199,#412200,#412201,#412202,
#412203,#412204,#412205,#412206,#412207,#412208,#412209,#412210,#412211,
#412212,#412213,#412214,#412215,#412216,#412217,#412218,#412219,#412220,
#412221,#412222,#412223,#412224,#412225,#412226,#412227,#412228,#412229,
#412230,#412231,#412232,#412233,#412234),.UNSPECIFIED.,.F.,.F.,(4,2,2,2,
2,2,2,2,2,2,2,2,2,2,2,2,2,4),(-11.8489689543484,-11.8062057019271,-11.7467120479489,
-11.6894063080904,-11.6295405390255,-11.5706919501455,-11.5133533098025,
-11.4528633639609,-11.3946915114793,-11.3362085317373,-11.2764770094769,
-11.218985220445,-11.1591378012859,-11.1001853146456,-11.0429938067333,
-10.9831311077197,-10.9248312492268,-10.9000724301687),.UNSPECIFIED.);
#25896=B_SPLINE_CURVE_WITH_KNOTS('',3,(#412239,#412240,#412241,#412242,
#412243,#412244,#412245,#412246,#412247,#412248,#412249,#412250,#412251,
#412252,#412253,#412254,#412255,#412256,#412257,#412258,#412259,#412260,
#412261,#412262,#412263,#412264,#412265,#412266,#412267,#412268,#412269,
#412270,#412271,#412272,#412273,#412274,#412275,#412276),.UNSPECIFIED.,
 .F.,.F.,(4,2,2,2,2,2,2,2,2,2,2,2,2,2,2,2,2,2,4),(-15.1339667326515,-15.1328138533434,
-15.0755472853668,-15.0160533390152,-14.9575818405722,-14.8996342065864,
-14.8393828666999,-14.7811387689155,-14.7215432153836,-14.6641840504559,
-14.6044996275074,-14.5456812087575,-14.4886586947663,-14.4289615372059,
-14.3707935623025,-14.3129768521214,-14.2532271707844,-14.1957307128446,
-14.1877310170691),.UNSPECIFIED.);
#25897=B_SPLINE_CURVE_WITH_KNOTS('',3,(#412277,#412278,#412279,#412280,
#412281,#412282,#412283,#412284,#412285,#412286,#412287,#412288,#412289,
#412290,#412291,#412292,#412293,#412294,#412295,#412296,#412297,#412298,
#412299,#412300,#412301,#412302,#412303,#412304,#412305,#412306,#412307,
#412308,#412309,#412310,#412311,#412312),.UNSPECIFIED.,.F.,.F.,(4,2,2,2,
2,2,2,2,2,2,2,2,2,2,2,2,2,4),(-10.9000724301687,-10.8667984467609,-10.8069161060488,
-10.7492901312385,-10.6892789248494,-10.6301854632589,-10.5730534177407,
-10.5132153838967,-10.4547722371732,-10.3970522395411,-10.3370076193401,
-10.2792364263307,-10.2198060794502,-10.1605347102306,-10.1033697946133,
-10.0435286456608,-9.98490540550661,-9.95172763366354),.UNSPECIFIED.);
#25898=B_SPLINE_CURVE_WITH_KNOTS('',3,(#412317,#412318,#412319,#412320,
#412321,#412322,#412323,#412324,#412325,#412326,#412327,#412328,#412329,
#412330,#412331,#412332,#412333,#412334,#412335,#412336,#412337,#412338,
#412339,#412340,#412341,#412342,#412343,#412344,#412345,#412346,#412347,
#412348,#412349,#412350,#412351,#412352),.UNSPECIFIED.,.F.,.F.,(4,2,2,2,
2,2,2,2,2,2,2,2,2,2,2,2,2,4),(-16.0794051131266,-16.0696407503467,-16.0121174534365,
-15.9523350001075,-15.8946932109278,-15.8364997791912,-15.7768508439869,
-15.7198928362282,-15.6610503748176,-15.6010001801705,-15.5436076054625,
-15.4839716393591,-15.4259926693996,-15.3679268902092,-15.3082432723521,
-15.2511947878248,-15.1924775074701,-15.1339667326515),.UNSPECIFIED.);
#25899=B_SPLINE_CURVE_WITH_KNOTS('',3,(#412353,#412354,#412355,#412356,
#412357,#412358,#412359,#412360,#412361,#412362,#412363,#412364,#412365,
#412366,#412367,#412368,#412369,#412370,#412371,#412372,#412373,#412374,
#412375,#412376,#412377,#412378,#412379,#412380,#412381,#412382,#412383,
#412384,#412385,#412386,#412387,#412388),.UNSPECIFIED.,.F.,.F.,(4,2,2,2,
2,2,2,2,2,2,2,2,2,2,2,2,2,4),(-9.95172763366354,-9.92741383632888,-9.86717010987739,
-9.80921983279747,-9.75028907798721,-9.69080854346615,-9.63351174591108,
-9.57363743547837,-9.51480248845095,-9.4574406720365,-9.39696631029004,
-9.33880772125035,-9.28026960018865,-9.22055403493478,-9.16307647023736,
-9.10322743464804,-9.04429086314863,-9.00274133888152),.UNSPECIFIED.);
#25900=B_SPLINE_CURVE_WITH_KNOTS('',3,(#412393,#412394,#412395,#412396,
#412397,#412398,#412399,#412400,#412401,#412402,#412403,#412404,#412405,
#412406,#412407,#412408,#412409,#412410,#412411,#412412,#412413,#412414,
#412415,#412416,#412417,#412418,#412419,#412420,#412421,#412422,#412423,
#412424,#412425,#412426,#412427,#412428),.UNSPECIFIED.,.F.,.F.,(4,2,2,2,
2,2,2,2,2,2,2,2,2,2,2,2,2,4),(-17.0248696573777,-17.0067626855016,-16.9488761285404,
-16.8886900492831,-16.831478331547,-16.7729191403435,-16.7132565323447,
-16.6562083651293,-16.5970046577124,-16.5380880417454,-16.4803985525618,
-16.4204310100632,-16.3630513473235,-16.3046917953613,-16.2450505258361,
-16.1880961783059,-16.1290897695364,-16.0794051131266),.UNSPECIFIED.);
#25901=B_SPLINE_CURVE_WITH_KNOTS('',3,(#412429,#412430,#412431,#412432,
#412433,#412434,#412435,#412436,#412437,#412438,#412439,#412440,#412441,
#412442,#412443,#412444,#412445,#412446,#412447,#412448,#412449,#412450,
#412451,#412452,#412453,#412454,#412455,#412456,#412457,#412458,#412459,
#412460,#412461,#412462,#412463,#412464),.UNSPECIFIED.,.F.,.F.,(4,2,2,2,
2,2,2,2,2,2,2,2,2,2,2,2,2,4),(-9.00274133888152,-8.98708808222356,-8.92722217436779,
-8.86893852475257,-8.81086478778761,-8.75100098495595,-8.69339164115971,
-8.6333076147785,-8.57423490357275,-8.51710183575562,-8.45726384338693,
-8.39884169405584,-8.34108927130448,-8.28106800117714,-8.22331785961894,
-8.16382232926111,-8.1045759025698,-8.05441325037715),.UNSPECIFIED.);
#25902=B_SPLINE_CURVE_WITH_KNOTS('',3,(#412469,#412470,#412471,#412472,
#412473,#412474,#412475,#412476,#412477,#412478,#412479,#412480,#412481,
#412482,#412483,#412484,#412485,#412486,#412487,#412488,#412489,#412490,
#412491,#412492,#412493,#412494,#412495,#412496,#412497,#412498,#412499,
#412500,#412501,#412502,#412503,#412504),.UNSPECIFIED.,.F.,.F.,(4,2,2,2,
2,2,2,2,2,2,2,2,2,2,2,2,2,4),(-17.9697860632053,-17.9431621937315,-17.8850387122403,
-17.8254391869702,-17.7685240651178,-17.7097518301889,-17.6496732375117,
-17.5923452314049,-17.5327776023798,-17.4748017460718,-17.4168005153958,
-17.3571629468064,-17.3001474078506,-17.2414948860682,-17.1818786968149,
-17.1246738065254,-17.0652450862675,-17.0248696573777),.UNSPECIFIED.);
#25903=B_SPLINE_CURVE_WITH_KNOTS('',3,(#412505,#412506,#412507,#412508,
#412509,#412510,#412511,#412512,#412513,#412514,#412515,#412516,#412517,
#412518,#412519,#412520,#412521,#412522,#412523,#412524,#412525,#412526,
#412527,#412528,#412529,#412530,#412531,#412532,#412533,#412534,#412535,
#412536,#412537,#412538,#412539,#412540,#412541,#412542),.UNSPECIFIED.,
 .F.,.F.,(4,2,2,2,2,2,2,2,2,2,2,2,2,2,2,2,2,2,4),(-8.05441325037715,-8.04742174586969,
-7.98758411506632,-7.92898607371866,-7.87147336403557,-7.81125718161243,
-7.75333182043714,-7.69434731743895,-7.63489521713669,-7.5776211614932,
-7.51775415880984,-7.45894797080115,-7.40157745295303,-7.34113418679424,
-7.28300382792094,-7.22442589013463,-7.1647416525545,-7.1072931406182,-7.10557406287411),
 .UNSPECIFIED.);
#25904=B_SPLINE_CURVE_WITH_KNOTS('',3,(#412547,#412548,#412549,#412550,
#412551,#412552,#412553,#412554,#412555,#412556,#412557,#412558,#412559,
#412560,#412561,#412562,#412563,#412564,#412565,#412566,#412567,#412568,
#412569,#412570,#412571,#412572,#412573,#412574,#412575,#412576,#412577,
#412578,#412579,#412580,#412581,#412582),.UNSPECIFIED.,.F.,.F.,(4,2,2,2,
2,2,2,2,2,2,2,2,2,2,2,2,2,4),(-18.9142706847603,-18.879112817184,-18.8206326702126,
-18.7610269812058,-18.7040467074318,-18.644922279731,-18.5859934242845,
-18.5283780156482,-18.4684891649703,-18.4111309770561,-18.3528462472636,
-18.2932579801719,-18.2363585809717,-18.1774272809653,-18.1179557281923,
-18.0605020205951,-18.0007933709383,-17.9697860632053),.UNSPECIFIED.);
#25905=B_SPLINE_CURVE_WITH_KNOTS('',3,(#412583,#412584,#412585,#412586,
#412587,#412588,#412589,#412590,#412591,#412592,#412593,#412594,#412595,
#412596,#412597,#412598,#412599,#412600,#412601,#412602,#412603,#412604,
#412605,#412606,#412607,#412608,#412609,#412610,#412611,#412612,#412613,
#412614,#412615,#412616,#412617,#412618),.UNSPECIFIED.,.F.,.F.,(4,2,2,2,
2,2,2,2,2,2,2,2,2,2,2,2,2,4),(-7.10557406287411,-7.04745818303111,-6.98855275914176,
-6.93135307843427,-6.87149973761286,-6.81324736108095,-6.75514765506272,
-6.6953178670604,-6.63774007839259,-6.57759901578035,-6.51856237664589,
-6.46144235798614,-6.40162014413745,-6.34323414046294,-6.28546377651572,
-6.22548142888577,-6.16776734990896,-6.15740376012386),.UNSPECIFIED.);
#25906=B_SPLINE_CURVE_WITH_KNOTS('',3,(#412623,#412624,#412625,#412626,
#412627,#412628,#412629,#412630,#412631,#412632,#412633,#412634,#412635,
#412636,#412637,#412638,#412639,#412640,#412641,#412642,#412643,#412644,
#412645,#412646,#412647,#412648,#412649,#412650,#412651,#412652,#412653,
#412654,#412655,#412656,#412657,#412658),.UNSPECIFIED.,.F.,.F.,(4,2,2,2,
2,2,2,2,2,2,2,2,2,2,2,2,2,4),(-19.8584422835686,-19.8152073934546,-19.7565232896875,
-19.6964277594369,-19.6391814863779,-19.5797000820731,-19.5217402307493,
-19.4638208175453,-19.404245965306,-19.3472777488811,-19.2887074085738,
-19.2291553359313,-19.1720289787636,-19.1126830374294,-19.0542020436924,
-18.9963934826294,-18.9362903222569,-18.9142706847603),.UNSPECIFIED.);
#25907=B_SPLINE_CURVE_WITH_KNOTS('',3,(#412659,#412660,#412661,#412662,
#412663,#412664,#412665,#412666,#412667,#412668,#412669,#412670,#412671,
#412672,#412673,#412674,#412675,#412676,#412677,#412678,#412679,#412680,
#412681,#412682,#412683,#412684,#412685,#412686,#412687,#412688,#412689,
#412690,#412691,#412692,#412693,#412694),.UNSPECIFIED.,.F.,.F.,(4,2,2,2,
2,2,2,2,2,2,2,2,2,2,2,2,2,4),(-6.15740376012386,-6.10822172720228,-6.0490156838889,
-5.99188620823853,-5.93206779050262,-5.87351020829041,-5.81599049092837,
-5.75581754399223,-5.69793221518616,-5.63890848208477,-5.57950038364006,
-5.5222630440661,-5.46241899964079,-5.40365695283083,-5.34629170825762,
-5.28589535541311,-5.22780845186964,-5.20907703509223),.UNSPECIFIED.);
#25908=B_SPLINE_CURVE_WITH_KNOTS('',3,(#412699,#412700,#412701,#412702,
#412703,#412704,#412705,#412706,#412707,#412708,#412709,#412710,#412711,
#412712,#412713,#412714,#412715,#412716,#412717,#412718,#412719,#412720,
#412721,#412722,#412723,#412724,#412725,#412726,#412727,#412728,#412729,
#412730,#412731,#412732,#412733,#412734),.UNSPECIFIED.,.F.,.F.,(4,2,2,2,
2,2,2,2,2,2,2,2,2,2,2,2,2,4),(-20.8017161031817,-20.7496789559818,-20.6906526416135,
-20.6317226295974,-20.5741993586506,-20.5144080614634,-20.4570845025018,
-20.3988928086463,-20.3393746294764,-20.282545486662,-20.2237076825146,
-20.1642246610779,-20.1068581592809,-20.0472416921874,-19.9896339732113,
-19.9315981829693,-19.8720649377923,-19.8584422835686),.UNSPECIFIED.);
#25909=B_SPLINE_CURVE_WITH_KNOTS('',3,(#412735,#412736,#412737,#412738,
#412739,#412740,#412741,#412742,#412743,#412744,#412745,#412746,#412747,
#412748,#412749,#412750,#412751,#412752,#412753,#412754,#412755,#412756,
#412757,#412758,#412759,#412760,#412761,#412762,#412763,#412764,#412765,
#412766,#412767,#412768,#412769,#412770),.UNSPECIFIED.,.F.,.F.,(4,2,2,2,
2,2,2,2,2,2,2,2,2,2,2,2,2,4),(-5.20907703509223,-5.16920485068219,-5.10956762673631,
-5.0521632757907,-4.99235803428031,-4.93349930655624,-4.87631684158672,
-4.81649176115974,-4.75828604527994,-4.70017445432352,-4.6403945310797,
-4.58286355547662,-4.52267968715453,-4.46369486316409,-4.40660190807755,
-4.34681119824301,-4.28847691628623,-4.26116841327561),.UNSPECIFIED.);
#25910=B_SPLINE_CURVE_WITH_KNOTS('',3,(#412775,#412776,#412777,#412778,
#412779,#412780,#412781,#412782,#412783,#412784,#412785,#412786,#412787,
#412788,#412789,#412790,#412791,#412792,#412793,#412794,#412795,#412796,
#412797,#412798,#412799,#412800,#412801,#412802,#412803,#412804,#412805,
#412806,#412807,#412808,#412809,#412810,#412811,#412812),.UNSPECIFIED.,
 .F.,.F.,(4,2,2,2,2,2,2,2,2,2,2,2,2,2,2,2,2,2,4),(-21.7459617623565,-21.7423453853052,
-21.6850922827677,-21.6256066051595,-21.5674881210864,-21.5095596509136,
-21.4493195364772,-21.392283120407,-21.3336802984165,-21.2741047422002,
-21.2170434942016,-21.1577995546806,-21.0993315343373,-21.0416194317091,
-20.9816184985961,-20.924489018422,-20.8661065715194,-20.8065751181493,
-20.8017161031817),.UNSPECIFIED.);
#25911=B_SPLINE_CURVE_WITH_KNOTS('',3,(#412813,#412814,#412815,#412816,
#412817,#412818,#412819,#412820,#412821,#412822,#412823,#412824,#412825,
#412826,#412827,#412828,#412829,#412830,#412831,#412832,#412833,#412834,
#412835,#412836,#412837,#412838,#412839,#412840,#412841,#412842,#412843,
#412844,#412845,#412846,#412847,#412848),.UNSPECIFIED.,.F.,.F.,(4,2,2,2,
2,2,2,2,2,2,2,2,2,2,2,2,2,4),(-4.26116841327561,-4.23070237710342,-4.17077500320315,
-4.11311242933797,-4.05353038859324,-3.99438068331312,-3.9372899857969,
-3.87750654045149,-3.81900520002606,-3.7614921033953,-3.70137865717443,
-3.64354899639362,-3.58449934635719,-3.52515141514432,-3.46796518308394,
-3.40815989357924,-3.34945797488407,-3.31355979035892),.UNSPECIFIED.);
#25912=B_SPLINE_CURVE_WITH_KNOTS('',3,(#412853,#412854,#412855,#412856,
#412857,#412858,#412859,#412860,#412861,#412862,#412863,#412864,#412865,
#412866,#412867,#412868,#412869,#412870,#412871,#412872,#412873,#412874,
#412875,#412876,#412877,#412878,#412879,#412880,#412881,#412882,#412883,
#412884,#412885,#412886,#412887,#412888),.UNSPECIFIED.,.F.,.F.,(4,2,2,2,
2,2,2,2,2,2,2,2,2,2,2,2,2,4),(-22.68998065011,-22.6777707860463,-22.6202279402948,
-22.5604180217573,-22.5030176125001,-22.4448059003209,-22.3852427307347,
-22.328372598661,-22.2695139987459,-22.2099052437004,-22.152514528674,-22.0928743951815,
-22.0351787158555,-21.9771178573061,-21.917535881535,-21.8606250794884,
-21.801915096849,-21.7459617623565),.UNSPECIFIED.);
#25913=B_SPLINE_CURVE_WITH_KNOTS('',3,(#412889,#412890,#412891,#412892,
#412893,#412894,#412895,#412896,#412897,#412898,#412899,#412900,#412901,
#412902,#412903,#412904,#412905,#412906,#412907,#412908,#412909,#412910,
#412911,#412912,#412913,#412914,#412915,#412916,#412917,#412918,#412919,
#412920,#412921,#412922,#412923,#412924),.UNSPECIFIED.,.F.,.F.,(4,2,2,2,
2,2,2,2,2,2,2,2,2,2,2,2,2,4),(-3.31355979035892,-3.29211171904543,-3.23177875334416,
-3.17375112630324,-3.11513507891545,-3.05556122121513,-2.99821675833727,
-2.93845715871131,-2.87966134450814,-2.8225102089605,-2.76272934872894,
-2.70458635428677,-2.64647631832303,-2.58676284615983,-2.52929462550545,
-2.46908084307281,-2.4101643664363,-2.36612653176872),.UNSPECIFIED.);
#25914=B_SPLINE_CURVE_WITH_KNOTS('',3,(#412929,#412930,#412931,#412932,
#412933,#412934,#412935,#412936,#412937,#412938,#412939,#412940,#412941,
#412942,#412943,#412944,#412945,#412946,#412947,#412948,#412949,#412950,
#412951,#412952,#412953,#412954,#412955,#412956,#412957,#412958,#412959,
#412960,#412961,#412962,#412963,#412964),.UNSPECIFIED.,.F.,.F.,(4,2,2,2,
2,2,2,2,2,2,2,2,2,2,2,2,2,4),(-23.6345898267855,-23.6140949491887,-23.5561542444433,
-23.4959033790334,-23.4388176101368,-23.3802026881221,-23.320590507054,
-23.2635147517929,-23.2042578136158,-23.1456890151044,-23.0879613142637,
-23.0279460580427,-22.970753042941,-22.912354902148,-22.8527824648407,-22.7958587610358,
-22.736815942826,-22.68998065011),.UNSPECIFIED.);
#25915=B_SPLINE_CURVE_WITH_KNOTS('',3,(#412965,#412966,#412967,#412968,
#412969,#412970,#412971,#412972,#412973,#412974,#412975,#412976,#412977,
#412978,#412979,#412980,#412981,#412982,#412983,#412984,#412985,#412986,
#412987,#412988,#412989,#412990,#412991,#412992,#412993,#412994,#412995,
#412996,#412997,#412998,#412999,#413000),.UNSPECIFIED.,.F.,.F.,(4,2,2,2,
2,2,2,2,2,2,2,2,2,2,2,2,2,4),(-2.36612653176872,-2.35311268006124,-2.29336954071319,
-2.2351033487007,-2.17733789322699,-2.11748240192008,-2.05988757144052,
-2.00028154453617,-1.94120503286711,-1.88416763920247,-1.82443534589591,
-1.76600693231654,-1.70851378499439,-1.64847707345954,-1.59071961453085,
-1.53165630513777,-1.47238570404183,-1.41945372484329),.UNSPECIFIED.);
#25916=B_SPLINE_CURVE_WITH_KNOTS('',3,(#413005,#413006,#413007,#413008,
#413009,#413010,#413011,#413012,#413013,#413014,#413015,#413016,#413017,
#413018,#413019,#413020,#413021,#413022,#413023,#413024,#413025,#413026,
#413027,#413028,#413029,#413030,#413031,#413032,#413033,#413034,#413035,
#413036,#413037,#413038,#413039,#413040),.UNSPECIFIED.,.F.,.F.,(4,2,2,2,
2,2,2,2,2,2,2,2,2,2,2,2,2,4),(-24.5792059929108,-24.5500970949004,-24.4918809036154,
-24.4322903051749,-24.3753946654069,-24.3165310225285,-24.2568186477746,
-24.1994192812253,-24.1397715290208,-24.0820070150704,-24.0239368230827,
-23.964323943516,-23.907376385801,-23.8486564673835,-23.7890576529927,-23.7317935555424,
-23.672297753621,-23.6345898267855),.UNSPECIFIED.);
#25917=B_SPLINE_CURVE_WITH_KNOTS('',3,(#413041,#413042,#413043,#413044,
#413045,#413046,#413047,#413048,#413049,#413050,#413051,#413052,#413053,
#413054,#413055,#413056,#413057,#413058,#413059,#413060,#413061,#413062,
#413063,#413064,#413065,#413066,#413067,#413068,#413069,#413070,#413071,
#413072,#413073,#413074,#413075,#413076,#413077,#413078),.UNSPECIFIED.,
 .F.,.F.,(4,2,2,2,2,2,2,2,2,2,2,2,2,2,2,2,2,2,4),(-1.41945372484329,-1.41526566454244,
-1.35551543195448,-1.29689062832757,-1.23957703033406,-1.17932499202215,
-1.12137345130017,-1.0627573841339,-1.00326432523307,-0.945996493022722,
-0.886299119599774,-0.827583520519354,-0.770478077590893,-0.710758038954895,
-0.652694913124193,-0.594599400688255,-0.53497013529226,-0.477581710315112,
-0.472734891726342),.UNSPECIFIED.);
#25918=B_SPLINE_CURVE_WITH_KNOTS('',3,(#413083,#413084,#413085,#413086,
#413087,#413088,#413089,#413090,#413091,#413092,#413093,#413094,#413095,
#413096,#413097,#413098,#413099,#413100,#413101,#413102,#413103,#413104,
#413105,#413106,#413107,#413108,#413109,#413110,#413111,#413112,#413113,
#413114,#413115,#413116,#413117,#413118),.UNSPECIFIED.,.F.,.F.,(4,2,2,2,
2,2,2,2,2,2,2,2,2,2,2,2,2,4),(-25.5239437797376,-25.4862365841868,-25.4276248886421,
-25.3679930479258,-25.3109167358137,-25.2516623582473,-25.1930121222715,
-25.1352840929817,-25.0752702538568,-25.018030561544,-24.9596321363847,
-24.9000359896044,-24.8430993324249,-24.7840556434341,-24.7249160932499,
-24.667369062466,-24.6075563852897,-24.5792059929108),.UNSPECIFIED.);
#25919=B_SPLINE_CURVE_WITH_KNOTS('',3,(#413120,#413121,#413122,#413123,
#413124,#413125,#413126,#413127,#413128,#413129,#413130,#413131,#413132,
#413133,#413134,#413135,#413136,#413137,#413138,#413139),.UNSPECIFIED.,
 .F.,.F.,(4,2,2,2,2,2,2,2,2,4),(-0.472734891726342,-0.41734976808456,-0.358519527533459,
-0.301523884178399,-0.241845235162269,-0.183664856566032,-0.125921516552503,
-0.0661562618768071,-0.0325226499984521,-1.00000007524637E-6),
 .UNSPECIFIED.);
#25920=B_SPLINE_CURVE_WITH_KNOTS('',3,(#413140,#413141,#413142,#413143,
#413144,#413145,#413146,#413147,#413148,#413149,#413150,#413151,#413152,
#413153,#413154,#413155,#413156,#413157,#413158,#413159),.UNSPECIFIED.,
 .F.,.F.,(4,2,2,2,2,2,2,2,2,4),(-4.25182450433022,-4.21324482415993,-4.17330760656305,
-4.11300975566751,-4.05588823658734,-3.99722796799383,-3.93757504645253,
-3.88045584389487,-3.82115322980259,-3.77909511501224),.UNSPECIFIED.);
#25921=B_SPLINE_CURVE_WITH_KNOTS('',3,(#413164,#413165,#413166,#413167,
#413168,#413169,#413170,#413171,#413172,#413173,#413174,#413175,#413176,
#413177,#413178,#413179,#413180,#413181,#413182,#413183,#413184,#413185,
#413186,#413187,#413188,#413189,#413190,#413191,#413192,#413193,#413194,
#413195,#413196,#413197,#413198,#413199),.UNSPECIFIED.,.F.,.F.,(4,2,2,2,
2,2,2,2,2,2,2,2,2,2,2,2,2,4),(-26.4689340794109,-26.4230444975284,-26.3641911040406,
-26.3043943197107,-26.2470013265531,-26.187361485941,-26.1295452860473,
-26.0714809446919,-26.0118538369996,-25.9548849192215,-25.8961704376275,
-25.8365590552678,-25.7792989717176,-25.719808553885,-25.6615394891026,
-25.6036017340092,-25.5433557799967,-25.5239437797376),.UNSPECIFIED.);
#25922=B_SPLINE_CURVE_WITH_KNOTS('',3,(#413200,#413201,#413202,#413203,
#413204,#413205,#413206,#413207,#413208,#413209,#413210,#413211,#413212,
#413213,#413214,#413215,#413216,#413217,#413218,#413219,#413220,#413221,
#413222,#413223,#413224,#413225,#413226,#413227,#413228,#413229,#413230,
#413231,#413232,#413233,#413234,#413235),.UNSPECIFIED.,.F.,.F.,(4,2,2,2,
2,2,2,2,2,2,2,2,2,2,2,2,2,4),(-3.77909511501224,-3.76255879084929,-3.70478712467392,
-3.64472574486189,-3.58749989775137,-3.52905726514817,-3.46944495073968,
-3.41248069251164,-3.35339303043433,-3.29432488526653,-3.23673911082507,
-3.17688419430657,-3.11945369884331,-3.06119861064818,-3.00159645144949,
-2.94468876957472,-2.88578643339366,-2.83439253495563),.UNSPECIFIED.);
#25923=B_SPLINE_CURVE_WITH_KNOTS('',3,(#413240,#413241,#413242,#413243,
#413244,#413245,#413246,#413247,#413248,#413249,#413250,#413251,#413252,
#413253,#413254,#413255,#413256,#413257,#413258,#413259,#413260,#413261,
#413262,#413263,#413264,#413265,#413266,#413267,#413268,#413269,#413270,
#413271,#413272,#413273,#413274,#413275),.UNSPECIFIED.,.F.,.F.,(4,2,2,2,
2,2,2,2,2,2,2,2,2,2,2,2,2,4),(-27.413585014475,-27.3586963183019,-27.2994597685197,
-27.2407452322649,-27.1830317971469,-27.1230348017685,-27.0657639571981,
-27.0073803107202,-26.9477767793054,-26.8908412827537,-26.8318119875776,
-26.7725962122378,-26.7150599514713,-26.6552599714108,-26.5977580446488,
-26.5395524732983,-26.4799509530169,-26.4689340794109),.UNSPECIFIED.);
#25924=B_SPLINE_CURVE_WITH_KNOTS('',3,(#413276,#413277,#413278,#413279,
#413280,#413281,#413282,#413283,#413284,#413285,#413286,#413287,#413288,
#413289,#413290,#413291,#413292,#413293,#413294,#413295,#413296,#413297,
#413298,#413299,#413300,#413301,#413302,#413303,#413304,#413305,#413306,
#413307,#413308,#413309,#413310,#413311,#413312,#413313),.UNSPECIFIED.,
 .F.,.F.,(4,2,2,2,2,2,2,2,2,2,2,2,2,2,2,2,2,2,4),(-2.83439253495563,-2.8261565099365,
-2.76872402181225,-2.70904015089222,-2.6513165569579,-2.59321356797793,
-2.5335934094535,-2.4766477076658,-2.41789524058402,-2.35828692277368,-2.30099269164597,
-2.24146397083721,-2.18332091803267,-2.12535108784111,-2.06740821026071,
-2.00919870111594,-1.94970082154406,-1.8924346470782,-1.88939598835329),
 .UNSPECIFIED.);
#25925=B_SPLINE_CURVE_WITH_KNOTS('',3,(#413321,#413322,#413323,#413324,
#413325,#413326,#413327,#413328,#413329,#413330,#413331,#413332,#413333,
#413334,#413335,#413336,#413337,#413338,#413339,#413340,#413341,#413342,
#413343,#413344,#413345,#413346,#413347,#413348,#413349,#413350,#413351,
#413352),.UNSPECIFIED.,.F.,.F.,(4,2,2,2,2,2,2,2,2,2,2,2,2,2,2,4),(-29.1863963535123,
-29.1497109670899,-29.1134166088123,-29.055062847062,-28.9954677920218,
-28.9385474105555,-28.8795478027661,-28.8202720404545,-28.7627614641067,
-28.7029896310345,-28.6454600774267,-28.5872801805647,-28.527683695153,
-28.4707806921121,-28.4119527827778,-28.3587334199921),.UNSPECIFIED.);
#25926=B_SPLINE_CURVE_WITH_KNOTS('',3,(#413355,#413356,#413357,#413358,
#413359,#413360,#413361,#413362,#413363,#413364,#413365,#413366,#413367,
#413368,#413369,#413370,#413371,#413372,#413373,#413374,#413375,#413376,
#413377,#413378,#413379,#413380,#413381,#413382,#413383,#413384,#413385,
#413386,#413387,#413388,#413389,#413390),.UNSPECIFIED.,.F.,.F.,(4,2,2,2,
2,2,2,2,2,2,2,2,2,2,2,2,2,4),(-0.944879082372548,-0.897379451402566,-0.838334347307847,
-0.781395526853323,-0.721796519477892,-0.663396730448959,-0.606152751521145,
-0.546137618568464,-0.488408239163712,-0.42975149823817,-0.370495918980581,
-0.313418221859422,-0.253783772254139,-0.195170931018825,-0.138048281270193,
-0.0778012501110445,-0.038228735137851,-1.0000000948418E-6),
 .UNSPECIFIED.);
#25927=B_SPLINE_CURVE_WITH_KNOTS('',3,(#414087,#414088,#414089,#414090,
#414091,#414092,#414093,#414094,#414095,#414096,#414097,#414098,#414099,
#414100,#414101,#414102,#414103,#414104,#414105,#414106,#414107,#414108,
#414109,#414110,#414111,#414112,#414113,#414114,#414115,#414116,#414117,
#414118,#414119,#414120,#414121,#414122,#414123,#414124),.UNSPECIFIED.,
 .F.,.F.,(4,2,2,2,2,2,2,2,2,2,2,2,2,2,2,2,2,2,4),(-28.3587334199921,-28.3520886310235,
-28.2947168329376,-28.2351002552499,-28.1772480545876,-28.1192045326099,
-28.0595791702464,-28.0026035429005,-27.943909641482,-27.8843015620247,
-27.8270602519875,-27.767590499069,-27.7092714269571,-27.6513515336446,
-27.5911259178804,-27.5339882142317,-27.4753948036166,-27.4157594323402,
-27.413585014475),.UNSPECIFIED.);
#25928=B_SPLINE_CURVE_WITH_KNOTS('',3,(#414125,#414126,#414127,#414128,
#414129,#414130,#414131,#414132,#414133,#414134,#414135,#414136,#414137,
#414138,#414139,#414140,#414141,#414142,#414143,#414144,#414145,#414146,
#414147,#414148,#414149,#414150,#414151,#414152,#414153,#414154,#414155,
#414156,#414157,#414158,#414159,#414160),.UNSPECIFIED.,.F.,.F.,(4,2,2,2,
2,2,2,2,2,2,2,2,2,2,2,2,2,4),(-1.88939598835329,-1.83283257048709,-1.77411060750807,
-1.71715934398323,-1.65754309113281,-1.5994709081347,-1.54170066531609,
-1.48205099193883,-1.42464969478967,-1.36492936779628,-1.30606398664382,
-1.24916533957941,-1.18957158552469,-1.13135370679887,-1.07388930634909,
-1.01407501167343,-0.956526329448152,-0.944879082372548),.UNSPECIFIED.);
#25929=B_SPLINE_CURVE_WITH_KNOTS('',3,(#414163,#414164,#414165,#414166,
#414167,#414168,#414169,#414170,#414171,#414172,#414173,#414174),
 .UNSPECIFIED.,.F.,.F.,(4,2,2,2,2,4),(-0.202065267427624,-0.17829348393292,
-0.153313184261408,-0.110608381314549,-0.0554673983154286,-1.00000018307678E-6),
 .UNSPECIFIED.);
#25930=B_SPLINE_CURVE_WITH_KNOTS('',3,(#414175,#414176,#414177,#414178,
#414179,#414180,#414181,#414182,#414183,#414184,#414185,#414186,#414187,
#414188,#414189,#414190,#414191,#414192,#414193,#414194),.UNSPECIFIED.,
 .F.,.F.,(4,2,2,2,2,2,2,2,2,4),(-0.723442842076705,-0.67470994600901,-0.637171178726302,
-0.599047155987729,-0.559110341325991,-0.520318538599342,-0.477726281559118,
-0.416471543823766,-0.3571169726445,-0.318111909131838),.UNSPECIFIED.);
#25931=B_SPLINE_CURVE_WITH_KNOTS('',3,(#414200,#414201,#414202,#414203,
#414204,#414205,#414206,#414207,#414208,#414209,#414210,#414211,#414212,
#414213,#414214,#414215,#414216,#414217,#414218,#414219,#414220,#414221,
#414222,#414223,#414224,#414225,#414226,#414227,#414228,#414229,#414230,
#414231),.UNSPECIFIED.,.F.,.F.,(4,2,2,2,2,2,2,2,2,2,2,2,2,2,2,4),(0.112636617654083,
0.149377717472863,0.209192138323285,0.265054851856284,0.319884610918571,
0.367155139827267,0.416337427526782,0.463897142310362,0.515169975267158,
0.580416230184428,0.669070279346709,0.762049043445549,0.852742975916796,
0.94658012568358,1.02412072733907,1.1048615181955),.UNSPECIFIED.);
#25932=B_SPLINE_CURVE_WITH_KNOTS('',3,(#414271,#414272,#414273,#414274,
#414275,#414276,#414277,#414278,#414279,#414280,#414281,#414282,#414283,
#414284,#414285,#414286),.UNSPECIFIED.,.F.,.F.,(4,3,3,3,3,4),(7.65824322177166E-5,
7.91451746290967E-5,9.26886647076421E-5,0.000106465540579908,0.000127678760140906,
0.000152977955413166),.UNSPECIFIED.);
#25933=B_SPLINE_CURVE_WITH_KNOTS('',3,(#414294,#414295,#414296,#414297,
#414298,#414299,#414300,#414301,#414302,#414303,#414304,#414305,#414306,
#414307,#414308,#414309,#414310,#414311,#414312,#414313,#414314,#414315,
#414316,#414317,#414318),.UNSPECIFIED.,.F.,.F.,(4,3,3,3,3,3,3,3,4),(0.,
2.85550478878829E-5,4.78559032675579E-5,6.34108981925975E-5,7.91451746296059E-5,
9.26886647080578E-5,0.000106465540580229,0.00012767876014108,0.000152977955413166),
 .UNSPECIFIED.);
#25934=B_SPLINE_CURVE_WITH_KNOTS('',3,(#414326,#414327,#414328,#414329,
#414330,#414331,#414332,#414333,#414334,#414335,#414336,#414337,#414338,
#414339,#414340,#414341,#414342,#414343,#414344,#414345,#414346,#414347,
#414348,#414349,#414350),.UNSPECIFIED.,.F.,.F.,(4,3,3,3,3,3,3,3,4),(0.,
2.85550478878828E-5,4.78559032675579E-5,6.34108981925975E-5,7.91451746296059E-5,
9.2688664708058E-5,0.000106465540580229,0.000127678760141081,0.000152977955413166),
 .UNSPECIFIED.);
#25935=B_SPLINE_CURVE_WITH_KNOTS('',3,(#414358,#414359,#414360,#414361,
#414362,#414363,#414364,#414365,#414366,#414367,#414368,#414369,#414370,
#414371,#414372,#414373,#414374,#414375,#414376,#414377,#414378,#414379,
#414380,#414381,#414382),.UNSPECIFIED.,.F.,.F.,(4,3,3,3,3,3,3,3,4),(0.,
2.85550478878827E-5,4.78559032675579E-5,6.34108981925976E-5,7.91451746296058E-5,
9.26886647080579E-5,0.000106465540580229,0.000127678760141081,0.000152977955413166),
 .UNSPECIFIED.);
#25936=B_SPLINE_CURVE_WITH_KNOTS('',3,(#414390,#414391,#414392,#414393,
#414394,#414395,#414396,#414397,#414398,#414399,#414400,#414401,#414402,
#414403,#414404,#414405,#414406,#414407,#414408,#414409,#414410,#414411,
#414412,#414413,#414414),.UNSPECIFIED.,.F.,.F.,(4,3,3,3,3,3,3,3,4),(0.,
2.85550478878826E-5,4.78559032675577E-5,6.34108981925974E-5,7.91451746296057E-5,
9.26886647080577E-5,0.000106465540580228,0.00012767876014108,0.000152977955413165),
 .UNSPECIFIED.);
#25937=B_SPLINE_CURVE_WITH_KNOTS('',3,(#414422,#414423,#414424,#414425,
#414426,#414427,#414428,#414429,#414430,#414431,#414432,#414433,#414434,
#414435,#414436,#414437,#414438,#414439,#414440,#414441,#414442,#414443,
#414444,#414445,#414446),.UNSPECIFIED.,.F.,.F.,(4,3,3,3,3,3,3,3,4),(0.,
2.85550478878828E-5,4.78559032675581E-5,6.34108981925978E-5,7.91451746296063E-5,
9.26886647080584E-5,0.000106465540580229,0.000127678760141081,0.000152977955413167),
 .UNSPECIFIED.);
#25938=B_SPLINE_CURVE_WITH_KNOTS('',3,(#414454,#414455,#414456,#414457,
#414458,#414459,#414460,#414461,#414462,#414463,#414464,#414465,#414466,
#414467,#414468,#414469,#414470,#414471,#414472,#414473,#414474,#414475,
#414476,#414477,#414478),.UNSPECIFIED.,.F.,.F.,(4,3,3,3,3,3,3,3,4),(0.,
2.85550478878825E-5,4.78559032675575E-5,6.34108981925973E-5,7.91451746296055E-5,
9.26886647080577E-5,0.000106465540580229,0.000127678760141081,0.000152977955413166),
 .UNSPECIFIED.);
#25939=B_SPLINE_CURVE_WITH_KNOTS('',3,(#414486,#414487,#414488,#414489,
#414490,#414491,#414492,#414493,#414494,#414495,#414496,#414497,#414498,
#414499,#414500,#414501,#414502,#414503,#414504,#414505,#414506,#414507,
#414508,#414509,#414510),.UNSPECIFIED.,.F.,.F.,(4,3,3,3,3,3,3,3,4),(0.,
2.85550478878825E-5,4.78559032675577E-5,6.34108981925977E-5,7.91451746296061E-5,
9.2688664708058E-5,0.000106465540580229,0.000127678760141081,0.000152977955413166),
 .UNSPECIFIED.);
#25940=B_SPLINE_CURVE_WITH_KNOTS('',3,(#414518,#414519,#414520,#414521,
#414522,#414523,#414524,#414525,#414526,#414527,#414528,#414529,#414530,
#414531,#414532,#414533,#414534,#414535,#414536,#414537,#414538,#414539,
#414540,#414541,#414542),.UNSPECIFIED.,.F.,.F.,(4,3,3,3,3,3,3,3,4),(0.,
2.85550478878828E-5,4.78559032675575E-5,6.34108981925974E-5,7.91451746296058E-5,
9.26886647080578E-5,0.000106465540580229,0.000127678760141081,0.000152977955413166),
 .UNSPECIFIED.);
#25941=B_SPLINE_CURVE_WITH_KNOTS('',3,(#414550,#414551,#414552,#414553,
#414554,#414555,#414556,#414557,#414558,#414559,#414560,#414561,#414562,
#414563,#414564,#414565,#414566,#414567,#414568,#414569,#414570,#414571,
#414572,#414573,#414574),.UNSPECIFIED.,.F.,.F.,(4,3,3,3,3,3,3,3,4),(0.,
2.85550478878827E-5,4.78559032675581E-5,6.34108981925978E-5,7.9145174629606E-5,
9.26886647080583E-5,0.000106465540580229,0.000127678760141081,0.000152977955413166),
 .UNSPECIFIED.);
#25942=B_SPLINE_CURVE_WITH_KNOTS('',3,(#414582,#414583,#414584,#414585,
#414586,#414587,#414588,#414589,#414590,#414591,#414592,#414593,#414594,
#414595,#414596,#414597,#414598,#414599,#414600,#414601,#414602,#414603,
#414604,#414605,#414606),.UNSPECIFIED.,.F.,.F.,(4,3,3,3,3,3,3,3,4),(0.,
2.85550478878827E-5,4.78559032675578E-5,6.34108981925974E-5,7.91451746296058E-5,
9.26886647080578E-5,0.000106465540580229,0.00012767876014108,0.000152977955413166),
 .UNSPECIFIED.);
#25943=B_SPLINE_CURVE_WITH_KNOTS('',3,(#414614,#414615,#414616,#414617,
#414618,#414619,#414620,#414621,#414622,#414623,#414624,#414625,#414626,
#414627,#414628,#414629,#414630,#414631,#414632,#414633,#414634,#414635,
#414636,#414637,#414638),.UNSPECIFIED.,.F.,.F.,(4,3,3,3,3,3,3,3,4),(0.,
2.85550478878825E-5,4.78559032675576E-5,6.34108981925974E-5,7.91451746296056E-5,
9.26886647080575E-5,0.000106465540580228,0.00012767876014108,0.000152977955413165),
 .UNSPECIFIED.);
#25944=B_SPLINE_CURVE_WITH_KNOTS('',3,(#414646,#414647,#414648,#414649,
#414650,#414651,#414652,#414653,#414654,#414655,#414656,#414657,#414658,
#414659,#414660,#414661,#414662,#414663,#414664,#414665,#414666,#414667,
#414668,#414669,#414670),.UNSPECIFIED.,.F.,.F.,(4,3,3,3,3,3,3,3,4),(0.,
2.85550478878826E-5,4.78559032675575E-5,6.34108981925975E-5,7.91451746296052E-5,
9.26886647080576E-5,0.000106465540580228,0.00012767876014108,0.000152977955413165),
 .UNSPECIFIED.);
#25945=B_SPLINE_CURVE_WITH_KNOTS('',3,(#414678,#414679,#414680,#414681,
#414682,#414683,#414684,#414685,#414686,#414687,#414688,#414689,#414690,
#414691,#414692,#414693,#414694,#414695,#414696,#414697,#414698,#414699,
#414700,#414701,#414702),.UNSPECIFIED.,.F.,.F.,(4,3,3,3,3,3,3,3,4),(0.,
2.85550478878826E-5,4.78559032675576E-5,6.34108981925974E-5,7.91451746296057E-5,
9.26886647080577E-5,0.000106465540580229,0.00012767876014108,0.000152977955413165),
 .UNSPECIFIED.);
#25946=B_SPLINE_CURVE_WITH_KNOTS('',3,(#414710,#414711,#414712,#414713,
#414714,#414715,#414716,#414717,#414718,#414719,#414720,#414721,#414722,
#414723,#414724,#414725,#414726,#414727,#414728,#414729,#414730,#414731,
#414732,#414733,#414734),.UNSPECIFIED.,.F.,.F.,(4,3,3,3,3,3,3,3,4),(0.,
2.85550478878829E-5,4.78559032675581E-5,6.34108981925978E-5,7.91451746296064E-5,
9.26886647080586E-5,0.000106465540580229,0.000127678760141081,0.000152977955413166),
 .UNSPECIFIED.);
#25947=B_SPLINE_CURVE_WITH_KNOTS('',3,(#414742,#414743,#414744,#414745,
#414746,#414747,#414748,#414749,#414750,#414751,#414752,#414753,#414754,
#414755,#414756,#414757,#414758,#414759,#414760,#414761,#414762,#414763,
#414764,#414765,#414766),.UNSPECIFIED.,.F.,.F.,(4,3,3,3,3,3,3,3,4),(0.,
2.85550478878828E-5,4.78559032675579E-5,6.34108981925976E-5,7.9145174629606E-5,
9.26886647080582E-5,0.000106465540580229,0.000127678760141081,0.000152977955413167),
 .UNSPECIFIED.);
#25948=B_SPLINE_CURVE_WITH_KNOTS('',3,(#414774,#414775,#414776,#414777,
#414778,#414779,#414780,#414781,#414782,#414783,#414784,#414785,#414786,
#414787,#414788,#414789,#414790,#414791,#414792,#414793,#414794,#414795,
#414796,#414797,#414798),.UNSPECIFIED.,.F.,.F.,(4,3,3,3,3,3,3,3,4),(0.,
2.85550478878827E-5,4.78559032675579E-5,6.34108981925975E-5,7.9145174629606E-5,
9.26886647080579E-5,0.000106465540580229,0.000127678760141081,0.000152977955413166),
 .UNSPECIFIED.);
#25949=B_SPLINE_CURVE_WITH_KNOTS('',3,(#414806,#414807,#414808,#414809,
#414810,#414811,#414812,#414813,#414814,#414815,#414816,#414817,#414818,
#414819,#414820,#414821,#414822,#414823,#414824,#414825,#414826,#414827,
#414828,#414829,#414830),.UNSPECIFIED.,.F.,.F.,(4,3,3,3,3,3,3,3,4),(0.,
2.85550478878826E-5,4.78559032675578E-5,6.34108981925975E-5,7.91451746296059E-5,
9.26886647080579E-5,0.000106465540580229,0.00012767876014108,0.000152977955413166),
 .UNSPECIFIED.);
#25950=B_SPLINE_CURVE_WITH_KNOTS('',3,(#414838,#414839,#414840,#414841,
#414842,#414843,#414844,#414845,#414846,#414847,#414848,#414849,#414850,
#414851,#414852,#414853,#414854,#414855,#414856,#414857,#414858,#414859,
#414860,#414861,#414862),.UNSPECIFIED.,.F.,.F.,(4,3,3,3,3,3,3,3,4),(0.,
2.85550478878826E-5,4.78559032675579E-5,6.34108981925975E-5,7.91451746296058E-5,
9.26886647080578E-5,0.000106465540580229,0.000127678760141081,0.000152977955413166),
 .UNSPECIFIED.);
#25951=B_SPLINE_CURVE_WITH_KNOTS('',3,(#414870,#414871,#414872,#414873,
#414874,#414875,#414876,#414877,#414878,#414879,#414880,#414881,#414882,
#414883,#414884,#414885,#414886,#414887,#414888,#414889,#414890,#414891,
#414892,#414893,#414894),.UNSPECIFIED.,.F.,.F.,(4,3,3,3,3,3,3,3,4),(0.,
2.85550478878828E-5,4.78559032675579E-5,6.34108981925976E-5,7.91451746296061E-5,
9.26886647080581E-5,0.000106465540580229,0.000127678760141081,0.000152977955413166),
 .UNSPECIFIED.);
#25952=B_SPLINE_CURVE_WITH_KNOTS('',3,(#414902,#414903,#414904,#414905,
#414906,#414907,#414908,#414909,#414910,#414911,#414912,#414913,#414914,
#414915,#414916,#414917,#414918,#414919,#414920,#414921,#414922,#414923,
#414924,#414925,#414926),.UNSPECIFIED.,.F.,.F.,(4,3,3,3,3,3,3,3,4),(0.,
2.85550478878828E-5,4.78559032675579E-5,6.34108981925974E-5,7.91451746296058E-5,
9.26886647080578E-5,0.000106465540580229,0.000127678760141081,0.000152977955413166),
 .UNSPECIFIED.);
#25953=B_SPLINE_CURVE_WITH_KNOTS('',3,(#414934,#414935,#414936,#414937,
#414938,#414939,#414940,#414941,#414942,#414943,#414944,#414945,#414946,
#414947,#414948,#414949,#414950,#414951,#414952,#414953,#414954,#414955,
#414956,#414957,#414958),.UNSPECIFIED.,.F.,.F.,(4,3,3,3,3,3,3,3,4),(0.,
2.85550478878826E-5,4.78559032675577E-5,6.34108981925974E-5,7.91451746296057E-5,
9.26886647080578E-5,0.000106465540580229,0.00012767876014108,0.000152977955413166),
 .UNSPECIFIED.);
#25954=B_SPLINE_CURVE_WITH_KNOTS('',3,(#414966,#414967,#414968,#414969,
#414970,#414971,#414972,#414973,#414974,#414975,#414976,#414977,#414978,
#414979,#414980,#414981,#414982,#414983,#414984,#414985,#414986,#414987,
#414988,#414989,#414990),.UNSPECIFIED.,.F.,.F.,(4,3,3,3,3,3,3,3,4),(0.,
2.85550478878827E-5,4.78559032675582E-5,6.34108981925978E-5,7.91451746296061E-5,
9.26886647080581E-5,0.000106465540580229,0.000127678760141081,0.000152977955413166),
 .UNSPECIFIED.);
#25955=B_SPLINE_CURVE_WITH_KNOTS('',3,(#414998,#414999,#415000,#415001,
#415002,#415003,#415004,#415005,#415006,#415007,#415008,#415009,#415010,
#415011,#415012,#415013,#415014,#415015,#415016,#415017,#415018,#415019,
#415020,#415021,#415022),.UNSPECIFIED.,.F.,.F.,(4,3,3,3,3,3,3,3,4),(0.,
2.8555047887883E-5,4.7855903267558E-5,6.34108981925975E-5,7.9145174629606E-5,
9.2688664708058E-5,0.000106465540580229,0.000127678760141081,0.000152977955413166),
 .UNSPECIFIED.);
#25956=B_SPLINE_CURVE_WITH_KNOTS('',3,(#415030,#415031,#415032,#415033,
#415034,#415035,#415036,#415037,#415038,#415039,#415040,#415041,#415042,
#415043,#415044,#415045,#415046,#415047,#415048,#415049,#415050,#415051,
#415052,#415053,#415054),.UNSPECIFIED.,.F.,.F.,(4,3,3,3,3,3,3,3,4),(0.,
2.85550478878827E-5,4.78559032675577E-5,6.34108981925973E-5,7.91451746296059E-5,
9.2688664708058E-5,0.000106465540580229,0.000127678760141081,0.000152977955413166),
 .UNSPECIFIED.);
#25957=B_SPLINE_CURVE_WITH_KNOTS('',3,(#415062,#415063,#415064,#415065,
#415066,#415067,#415068,#415069,#415070,#415071,#415072,#415073,#415074,
#415075,#415076,#415077,#415078,#415079,#415080,#415081,#415082,#415083,
#415084,#415085,#415086),.UNSPECIFIED.,.F.,.F.,(4,3,3,3,3,3,3,3,4),(0.,
2.85550478878828E-5,4.78559032675577E-5,6.34108981925974E-5,7.91451746296058E-5,
9.26886647080579E-5,0.000106465540580229,0.000127678760141081,0.000152977955413166),
 .UNSPECIFIED.);
#25958=B_SPLINE_CURVE_WITH_KNOTS('',3,(#415094,#415095,#415096,#415097,
#415098,#415099,#415100,#415101,#415102,#415103,#415104,#415105,#415106,
#415107,#415108,#415109,#415110,#415111,#415112,#415113,#415114,#415115,
#415116,#415117,#415118),.UNSPECIFIED.,.F.,.F.,(4,3,3,3,3,3,3,3,4),(0.,
2.85550478878826E-5,4.78559032675579E-5,6.34108981925973E-5,7.9145174629606E-5,
9.26886647080578E-5,0.000106465540580229,0.000127678760141081,0.000152977955413166),
 .UNSPECIFIED.);
#25959=B_SPLINE_CURVE_WITH_KNOTS('',3,(#415126,#415127,#415128,#415129,
#415130,#415131,#415132,#415133,#415134,#415135,#415136,#415137,#415138,
#415139,#415140,#415141,#415142,#415143,#415144,#415145,#415146,#415147,
#415148,#415149,#415150),.UNSPECIFIED.,.F.,.F.,(4,3,3,3,3,3,3,3,4),(0.,
2.85550478878826E-5,4.78559032675574E-5,6.3410898192597E-5,7.91451746296055E-5,
9.26886647080575E-5,0.000106465540580229,0.00012767876014108,0.000152977955413165),
 .UNSPECIFIED.);
#25960=B_SPLINE_CURVE_WITH_KNOTS('',3,(#415158,#415159,#415160,#415161,
#415162,#415163,#415164,#415165,#415166,#415167,#415168,#415169,#415170,
#415171,#415172,#415173,#415174,#415175,#415176,#415177,#415178,#415179,
#415180,#415181,#415182),.UNSPECIFIED.,.F.,.F.,(4,3,3,3,3,3,3,3,4),(0.,
2.85550478878822E-5,4.78559032675576E-5,6.34108981925971E-5,7.91451746296059E-5,
9.26886647080578E-5,0.000106465540580228,0.00012767876014108,0.000152977955413165),
 .UNSPECIFIED.);
#25961=B_SPLINE_CURVE_WITH_KNOTS('',3,(#415190,#415191,#415192,#415193,
#415194,#415195,#415196,#415197,#415198,#415199,#415200,#415201,#415202,
#415203,#415204,#415205,#415206,#415207,#415208,#415209,#415210,#415211,
#415212,#415213,#415214),.UNSPECIFIED.,.F.,.F.,(4,3,3,3,3,3,3,3,4),(0.,
2.85550478878825E-5,4.78559032675578E-5,6.34108981925973E-5,7.91451746296057E-5,
9.26886647080579E-5,0.000106465540580229,0.00012767876014108,0.000152977955413165),
 .UNSPECIFIED.);
#25962=B_SPLINE_CURVE_WITH_KNOTS('',3,(#415222,#415223,#415224,#415225,
#415226,#415227,#415228,#415229,#415230,#415231,#415232,#415233,#415234,
#415235,#415236,#415237,#415238,#415239,#415240,#415241,#415242,#415243,
#415244,#415245,#415246),.UNSPECIFIED.,.F.,.F.,(4,3,3,3,3,3,3,3,4),(0.,
2.85550478878828E-5,4.7855903267558E-5,6.34108981925976E-5,7.91451746296062E-5,
9.2688664708058E-5,0.000106465540580229,0.000127678760141081,0.000152977955413166),
 .UNSPECIFIED.);
#25963=B_SPLINE_CURVE_WITH_KNOTS('',3,(#415254,#415255,#415256,#415257,
#415258,#415259,#415260,#415261,#415262,#415263,#415264,#415265,#415266,
#415267,#415268,#415269,#415270,#415271,#415272,#415273,#415274,#415275,
#415276,#415277,#415278),.UNSPECIFIED.,.F.,.F.,(4,3,3,3,3,3,3,3,4),(0.,
2.85550478878827E-5,4.78559032675579E-5,6.34108981925976E-5,7.91451746296059E-5,
9.2688664708058E-5,0.000106465540580229,0.00012767876014108,0.000152977955413165),
 .UNSPECIFIED.);
#25964=B_SPLINE_CURVE_WITH_KNOTS('',3,(#415286,#415287,#415288,#415289,
#415290,#415291,#415292,#415293,#415294,#415295,#415296,#415297,#415298,
#415299,#415300,#415301,#415302,#415303,#415304,#415305,#415306,#415307,
#415308,#415309,#415310),.UNSPECIFIED.,.F.,.F.,(4,3,3,3,3,3,3,3,4),(0.,
2.85550478878827E-5,4.78559032675579E-5,6.34108981925976E-5,7.91451746296062E-5,
9.2688664708058E-5,0.000106465540580229,0.000127678760141081,0.000152977955413166),
 .UNSPECIFIED.);
#25965=B_SPLINE_CURVE_WITH_KNOTS('',3,(#415318,#415319,#415320,#415321,
#415322,#415323,#415324,#415325,#415326,#415327,#415328,#415329,#415330,
#415331,#415332,#415333,#415334,#415335,#415336,#415337,#415338,#415339,
#415340,#415341,#415342),.UNSPECIFIED.,.F.,.F.,(4,3,3,3,3,3,3,3,4),(0.,
2.85550478878825E-5,4.78559032675579E-5,6.34108981925974E-5,7.91451746296058E-5,
9.26886647080579E-5,0.000106465540580229,0.000127678760141081,0.000152977955413166),
 .UNSPECIFIED.);
#25966=B_SPLINE_CURVE_WITH_KNOTS('',3,(#415350,#415351,#415352,#415353,
#415354,#415355,#415356,#415357,#415358,#415359,#415360,#415361,#415362,
#415363,#415364,#415365,#415366,#415367,#415368,#415369,#415370,#415371,
#415372,#415373,#415374),.UNSPECIFIED.,.F.,.F.,(4,3,3,3,3,3,3,3,4),(0.,
2.85550478878828E-5,4.78559032675578E-5,6.34108981925973E-5,7.91451746296057E-5,
9.26886647080578E-5,0.000106465540580228,0.00012767876014108,0.000152977955413166),
 .UNSPECIFIED.);
#25967=B_SPLINE_CURVE_WITH_KNOTS('',3,(#415382,#415383,#415384,#415385,
#415386,#415387,#415388,#415389,#415390,#415391,#415392,#415393,#415394,
#415395,#415396,#415397,#415398,#415399,#415400,#415401,#415402,#415403,
#415404,#415405,#415406),.UNSPECIFIED.,.F.,.F.,(4,3,3,3,3,3,3,3,4),(0.,
2.85550478878823E-5,4.78559032675575E-5,6.34108981925972E-5,7.91451746296055E-5,
9.26886647080575E-5,0.000106465540580228,0.00012767876014108,0.000152977955413165),
 .UNSPECIFIED.);
#25968=B_SPLINE_CURVE_WITH_KNOTS('',3,(#415414,#415415,#415416,#415417,
#415418,#415419,#415420,#415421,#415422,#415423,#415424,#415425,#415426,
#415427,#415428,#415429,#415430,#415431,#415432,#415433,#415434,#415435,
#415436,#415437,#415438),.UNSPECIFIED.,.F.,.F.,(4,3,3,3,3,3,3,3,4),(0.,
2.85550478878827E-5,4.78559032675578E-5,6.34108981925974E-5,7.91451746296058E-5,
9.26886647080577E-5,0.000106465540580229,0.00012767876014108,0.000152977955413165),
 .UNSPECIFIED.);
#25969=B_SPLINE_CURVE_WITH_KNOTS('',3,(#415446,#415447,#415448,#415449,
#415450,#415451,#415452,#415453,#415454,#415455,#415456,#415457,#415458,
#415459,#415460,#415461,#415462,#415463,#415464,#415465,#415466,#415467,
#415468,#415469,#415470),.UNSPECIFIED.,.F.,.F.,(4,3,3,3,3,3,3,3,4),(0.,
2.85550478878824E-5,4.78559032675577E-5,6.34108981925974E-5,7.91451746296058E-5,
9.26886647080578E-5,0.000106465540580229,0.000127678760141081,0.000152977955413166),
 .UNSPECIFIED.);
#25970=B_SPLINE_CURVE_WITH_KNOTS('',3,(#415478,#415479,#415480,#415481,
#415482,#415483,#415484,#415485,#415486,#415487,#415488,#415489,#415490,
#415491,#415492,#415493,#415494,#415495,#415496,#415497,#415498,#415499,
#415500,#415501,#415502),.UNSPECIFIED.,.F.,.F.,(4,3,3,3,3,3,3,3,4),(0.,
2.85550478878823E-5,4.78559032675579E-5,6.34108981925974E-5,7.91451746296058E-5,
9.26886647080579E-5,0.000106465540580229,0.000127678760141081,0.000152977955413166),
 .UNSPECIFIED.);
#25971=B_SPLINE_CURVE_WITH_KNOTS('',3,(#415517,#415518,#415519,#415520,
#415521,#415522,#415523,#415524,#415525,#415526,#415527,#415528,#415529,
#415530,#415531,#415532,#415533,#415534,#415535,#415536,#415537,#415538,
#415539,#415540,#415541),.UNSPECIFIED.,.F.,.F.,(4,3,3,3,3,3,3,3,4),(0.,
2.85550478878826E-5,4.78559032675578E-5,6.34108981925975E-5,7.91451746296059E-5,
9.26886647080581E-5,0.000106465540580229,0.000127678760141081,0.000152977955413166),
 .UNSPECIFIED.);
#25972=B_SPLINE_CURVE_WITH_KNOTS('',3,(#415549,#415550,#415551,#415552,
#415553,#415554,#415555,#415556,#415557,#415558,#415559,#415560,#415561,
#415562,#415563,#415564,#415565,#415566,#415567,#415568,#415569,#415570,
#415571,#415572,#415573),.UNSPECIFIED.,.F.,.F.,(4,3,3,3,3,3,3,3,4),(0.,
2.85550478878824E-5,4.78559032675578E-5,6.34108981925974E-5,7.91451746296058E-5,
9.26886647080579E-5,0.000106465540580229,0.000127678760141081,0.000152977955413166),
 .UNSPECIFIED.);
#25973=B_SPLINE_CURVE_WITH_KNOTS('',3,(#415581,#415582,#415583,#415584,
#415585,#415586,#415587,#415588,#415589,#415590,#415591,#415592,#415593,
#415594,#415595,#415596,#415597,#415598,#415599,#415600,#415601,#415602,
#415603,#415604,#415605),.UNSPECIFIED.,.F.,.F.,(4,3,3,3,3,3,3,3,4),(0.,
2.85550478878827E-5,4.78559032675578E-5,6.34108981925973E-5,7.91451746296058E-5,
9.26886647080578E-5,0.000106465540580229,0.000127678760141081,0.000152977955413166),
 .UNSPECIFIED.);
#25974=B_SPLINE_CURVE_WITH_KNOTS('',3,(#415613,#415614,#415615,#415616,
#415617,#415618,#415619,#415620,#415621,#415622,#415623,#415624,#415625,
#415626,#415627,#415628,#415629,#415630,#415631,#415632,#415633,#415634,
#415635,#415636,#415637),.UNSPECIFIED.,.F.,.F.,(4,3,3,3,3,3,3,3,4),(0.,
2.85550478878828E-5,4.78559032675581E-5,6.34108981925975E-5,7.91451746296059E-5,
9.26886647080578E-5,0.000106465540580229,0.00012767876014108,0.000152977955413165),
 .UNSPECIFIED.);
#25975=B_SPLINE_CURVE_WITH_KNOTS('',3,(#415645,#415646,#415647,#415648,
#415649,#415650,#415651,#415652,#415653,#415654,#415655,#415656,#415657,
#415658,#415659,#415660,#415661,#415662,#415663,#415664,#415665,#415666,
#415667,#415668,#415669),.UNSPECIFIED.,.F.,.F.,(4,3,3,3,3,3,3,3,4),(0.,
2.85550478878827E-5,4.78559032675577E-5,6.34108981925976E-5,7.91451746296059E-5,
9.26886647080578E-5,0.000106465540580229,0.00012767876014108,0.000152977955413166),
 .UNSPECIFIED.);
#25976=B_SPLINE_CURVE_WITH_KNOTS('',3,(#415677,#415678,#415679,#415680,
#415681,#415682,#415683,#415684,#415685,#415686,#415687,#415688,#415689,
#415690,#415691,#415692,#415693,#415694,#415695,#415696,#415697,#415698,
#415699,#415700,#415701),.UNSPECIFIED.,.F.,.F.,(4,3,3,3,3,3,3,3,4),(0.,
2.85550478878825E-5,4.78559032675577E-5,6.34108981925973E-5,7.91451746296055E-5,
9.26886647080577E-5,0.000106465540580229,0.00012767876014108,0.000152977955413165),
 .UNSPECIFIED.);
#25977=B_SPLINE_CURVE_WITH_KNOTS('',3,(#415709,#415710,#415711,#415712,
#415713,#415714,#415715,#415716,#415717,#415718,#415719,#415720,#415721,
#415722,#415723,#415724,#415725,#415726,#415727,#415728,#415729,#415730,
#415731,#415732,#415733),.UNSPECIFIED.,.F.,.F.,(4,3,3,3,3,3,3,3,4),(0.,
2.85550478878829E-5,4.78559032675578E-5,6.34108981925974E-5,7.91451746296059E-5,
9.26886647080576E-5,0.000106465540580228,0.00012767876014108,0.000152977955413165),
 .UNSPECIFIED.);
#25978=B_SPLINE_CURVE_WITH_KNOTS('',3,(#415741,#415742,#415743,#415744,
#415745,#415746,#415747,#415748,#415749,#415750,#415751,#415752,#415753,
#415754,#415755,#415756,#415757,#415758,#415759,#415760,#415761,#415762,
#415763,#415764,#415765),.UNSPECIFIED.,.F.,.F.,(4,3,3,3,3,3,3,3,4),(0.,
2.85550478878826E-5,4.78559032675578E-5,6.34108981925975E-5,7.91451746296058E-5,
9.26886647080576E-5,0.000106465540580229,0.000127678760141081,0.000152977955413166),
 .UNSPECIFIED.);
#25979=B_SPLINE_CURVE_WITH_KNOTS('',3,(#415773,#415774,#415775,#415776,
#415777,#415778,#415779,#415780,#415781,#415782,#415783,#415784,#415785,
#415786,#415787,#415788,#415789,#415790,#415791,#415792,#415793,#415794,
#415795,#415796,#415797),.UNSPECIFIED.,.F.,.F.,(4,3,3,3,3,3,3,3,4),(0.,
2.85550478878825E-5,4.78559032675576E-5,6.34108981925972E-5,7.91451746296057E-5,
9.26886647080577E-5,0.000106465540580229,0.000127678760141081,0.000152977955413166),
 .UNSPECIFIED.);
#25980=B_SPLINE_CURVE_WITH_KNOTS('',3,(#415805,#415806,#415807,#415808,
#415809,#415810,#415811,#415812,#415813,#415814,#415815,#415816,#415817,
#415818,#415819,#415820,#415821,#415822,#415823,#415824,#415825,#415826,
#415827,#415828,#415829),.UNSPECIFIED.,.F.,.F.,(4,3,3,3,3,3,3,3,4),(0.,
2.85550478878827E-5,4.7855903267558E-5,6.34108981925976E-5,7.9145174629606E-5,
9.26886647080582E-5,0.000106465540580229,0.000127678760141081,0.000152977955413166),
 .UNSPECIFIED.);
#25981=B_SPLINE_CURVE_WITH_KNOTS('',3,(#415837,#415838,#415839,#415840,
#415841,#415842,#415843,#415844,#415845,#415846,#415847,#415848,#415849,
#415850,#415851,#415852,#415853,#415854,#415855,#415856,#415857,#415858,
#415859,#415860,#415861),.UNSPECIFIED.,.F.,.F.,(4,3,3,3,3,3,3,3,4),(0.,
2.85550478878827E-5,4.78559032675578E-5,6.34108981925974E-5,7.9145174629606E-5,
9.26886647080581E-5,0.000106465540580229,0.000127678760141081,0.000152977955413166),
 .UNSPECIFIED.);
#25982=B_SPLINE_CURVE_WITH_KNOTS('',3,(#415869,#415870,#415871,#415872,
#415873,#415874,#415875,#415876,#415877,#415878,#415879,#415880,#415881,
#415882,#415883,#415884,#415885,#415886,#415887,#415888,#415889,#415890,
#415891,#415892,#415893),.UNSPECIFIED.,.F.,.F.,(4,3,3,3,3,3,3,3,4),(0.,
2.85550478878826E-5,4.78559032675578E-5,6.34108981925974E-5,7.91451746296056E-5,
9.26886647080576E-5,0.000106465540580228,0.000127678760141081,0.000152977955413165),
 .UNSPECIFIED.);
#25983=B_SPLINE_CURVE_WITH_KNOTS('',3,(#415901,#415902,#415903,#415904,
#415905,#415906,#415907,#415908,#415909,#415910,#415911,#415912,#415913,
#415914,#415915,#415916,#415917,#415918,#415919,#415920,#415921,#415922,
#415923,#415924,#415925),.UNSPECIFIED.,.F.,.F.,(4,3,3,3,3,3,3,3,4),(0.,
2.85550478878827E-5,4.7855903267558E-5,6.34108981925976E-5,7.91451746296059E-5,
9.26886647080581E-5,0.000106465540580229,0.000127678760141081,0.000152977955413166),
 .UNSPECIFIED.);
#25984=B_SPLINE_CURVE_WITH_KNOTS('',3,(#415933,#415934,#415935,#415936,
#415937,#415938,#415939,#415940,#415941,#415942,#415943,#415944,#415945,
#415946,#415947,#415948,#415949,#415950,#415951,#415952,#415953,#415954,
#415955,#415956,#415957),.UNSPECIFIED.,.F.,.F.,(4,3,3,3,3,3,3,3,4),(0.,
2.85550478878827E-5,4.78559032675581E-5,6.34108981925976E-5,7.91451746296061E-5,
9.2688664708058E-5,0.000106465540580229,0.000127678760141081,0.000152977955413166),
 .UNSPECIFIED.);
#25985=B_SPLINE_CURVE_WITH_KNOTS('',3,(#415965,#415966,#415967,#415968,
#415969,#415970,#415971,#415972,#415973,#415974,#415975,#415976,#415977,
#415978,#415979,#415980,#415981,#415982,#415983,#415984,#415985,#415986,
#415987,#415988,#415989),.UNSPECIFIED.,.F.,.F.,(4,3,3,3,3,3,3,3,4),(0.,
2.85550478878826E-5,4.7855903267558E-5,6.34108981925975E-5,7.91451746296057E-5,
9.26886647080582E-5,0.000106465540580229,0.000127678760141081,0.000152977955413166),
 .UNSPECIFIED.);
#25986=B_SPLINE_CURVE_WITH_KNOTS('',3,(#415997,#415998,#415999,#416000,
#416001,#416002,#416003,#416004,#416005,#416006,#416007,#416008,#416009,
#416010,#416011,#416012,#416013,#416014,#416015,#416016,#416017,#416018,
#416019,#416020,#416021),.UNSPECIFIED.,.F.,.F.,(4,3,3,3,3,3,3,3,4),(0.,
2.85550478878828E-5,4.78559032675581E-5,6.34108981925976E-5,7.91451746296059E-5,
9.26886647080581E-5,0.000106465540580229,0.000127678760141081,0.000152977955413166),
 .UNSPECIFIED.);
#25987=B_SPLINE_CURVE_WITH_KNOTS('',3,(#416029,#416030,#416031,#416032,
#416033,#416034,#416035,#416036,#416037,#416038,#416039,#416040,#416041,
#416042,#416043,#416044,#416045,#416046,#416047,#416048,#416049,#416050,
#416051,#416052,#416053),.UNSPECIFIED.,.F.,.F.,(4,3,3,3,3,3,3,3,4),(0.,
2.85550478878829E-5,4.7855903267558E-5,6.34108981925976E-5,7.91451746296061E-5,
9.26886647080581E-5,0.000106465540580229,0.000127678760141081,0.000152977955413166),
 .UNSPECIFIED.);
#25988=B_SPLINE_CURVE_WITH_KNOTS('',3,(#416061,#416062,#416063,#416064,
#416065,#416066,#416067,#416068,#416069,#416070,#416071,#416072,#416073,
#416074,#416075,#416076,#416077,#416078,#416079,#416080,#416081,#416082,
#416083,#416084,#416085),.UNSPECIFIED.,.F.,.F.,(4,3,3,3,3,3,3,3,4),(0.,
2.85550478878825E-5,4.78559032675577E-5,6.34108981925974E-5,7.91451746296058E-5,
9.26886647080578E-5,0.000106465540580228,0.000127678760141081,0.000152977955413166),
 .UNSPECIFIED.);
#25989=B_SPLINE_CURVE_WITH_KNOTS('',3,(#416093,#416094,#416095,#416096,
#416097,#416098,#416099,#416100,#416101,#416102,#416103,#416104,#416105,
#416106,#416107,#416108,#416109,#416110,#416111,#416112,#416113,#416114,
#416115,#416116,#416117),.UNSPECIFIED.,.F.,.F.,(4,3,3,3,3,3,3,3,4),(0.,
2.85550478878829E-5,4.7855903267558E-5,6.34108981925975E-5,7.91451746296059E-5,
9.26886647080578E-5,0.000106465540580229,0.000127678760141081,0.000152977955413166),
 .UNSPECIFIED.);
#25990=B_SPLINE_CURVE_WITH_KNOTS('',3,(#416125,#416126,#416127,#416128,
#416129,#416130,#416131,#416132,#416133,#416134,#416135,#416136,#416137,
#416138,#416139,#416140,#416141,#416142,#416143,#416144,#416145,#416146,
#416147,#416148,#416149),.UNSPECIFIED.,.F.,.F.,(4,3,3,3,3,3,3,3,4),(0.,
2.85550478878826E-5,4.78559032675579E-5,6.34108981925974E-5,7.91451746296059E-5,
9.2688664708058E-5,0.000106465540580229,0.000127678760141081,0.000152977955413166),
 .UNSPECIFIED.);
#25991=B_SPLINE_CURVE_WITH_KNOTS('',3,(#416157,#416158,#416159,#416160,
#416161,#416162,#416163,#416164,#416165,#416166,#416167,#416168,#416169,
#416170,#416171,#416172,#416173,#416174,#416175,#416176,#416177,#416178,
#416179,#416180,#416181),.UNSPECIFIED.,.F.,.F.,(4,3,3,3,3,3,3,3,4),(0.,
2.85550478878828E-5,4.78559032675581E-5,6.34108981925976E-5,7.91451746296059E-5,
9.2688664708058E-5,0.000106465540580229,0.000127678760141081,0.000152977955413166),
 .UNSPECIFIED.);
#25992=B_SPLINE_CURVE_WITH_KNOTS('',3,(#416189,#416190,#416191,#416192,
#416193,#416194,#416195,#416196,#416197,#416198,#416199,#416200,#416201,
#416202,#416203,#416204,#416205,#416206,#416207,#416208,#416209,#416210,
#416211,#416212,#416213),.UNSPECIFIED.,.F.,.F.,(4,3,3,3,3,3,3,3,4),(0.,
2.85550478878829E-5,4.7855903267558E-5,6.34108981925977E-5,7.9145174629606E-5,
9.26886647080579E-5,0.000106465540580229,0.000127678760141081,0.000152977955413166),
 .UNSPECIFIED.);
#25993=B_SPLINE_CURVE_WITH_KNOTS('',3,(#416221,#416222,#416223,#416224,
#416225,#416226,#416227,#416228,#416229,#416230,#416231,#416232,#416233,
#416234,#416235,#416236,#416237,#416238,#416239,#416240,#416241,#416242,
#416243,#416244,#416245),.UNSPECIFIED.,.F.,.F.,(4,3,3,3,3,3,3,3,4),(0.,
2.85550478878826E-5,4.78559032675575E-5,6.34108981925974E-5,7.9145174629606E-5,
9.26886647080579E-5,0.000106465540580229,0.000127678760141081,0.000152977955413166),
 .UNSPECIFIED.);
#25994=B_SPLINE_CURVE_WITH_KNOTS('',3,(#416253,#416254,#416255,#416256,
#416257,#416258,#416259,#416260,#416261,#416262,#416263,#416264,#416265,
#416266,#416267,#416268,#416269,#416270,#416271,#416272,#416273,#416274,
#416275,#416276,#416277),.UNSPECIFIED.,.F.,.F.,(4,3,3,3,3,3,3,3,4),(0.,
2.85550478878826E-5,4.78559032675579E-5,6.34108981925973E-5,7.91451746296058E-5,
9.26886647080579E-5,0.000106465540580229,0.000127678760141081,0.000152977955413166),
 .UNSPECIFIED.);
#25995=B_SPLINE_CURVE_WITH_KNOTS('',3,(#416285,#416286,#416287,#416288,
#416289,#416290,#416291,#416292,#416293,#416294,#416295,#416296,#416297,
#416298,#416299,#416300,#416301,#416302,#416303,#416304,#416305,#416306,
#416307,#416308,#416309),.UNSPECIFIED.,.F.,.F.,(4,3,3,3,3,3,3,3,4),(0.,
2.85550478878825E-5,4.78559032675578E-5,6.34108981925975E-5,7.9145174629606E-5,
9.2688664708058E-5,0.000106465540580229,0.000127678760141081,0.000152977955413166),
 .UNSPECIFIED.);
#25996=B_SPLINE_CURVE_WITH_KNOTS('',3,(#416317,#416318,#416319,#416320,
#416321,#416322,#416323,#416324,#416325,#416326,#416327,#416328,#416329,
#416330,#416331,#416332,#416333,#416334,#416335,#416336,#416337,#416338,
#416339,#416340,#416341),.UNSPECIFIED.,.F.,.F.,(4,3,3,3,3,3,3,3,4),(0.,
2.85550478878826E-5,4.7855903267558E-5,6.34108981925976E-5,7.91451746296062E-5,
9.26886647080583E-5,0.000106465540580229,0.000127678760141081,0.000152977955413167),
 .UNSPECIFIED.);
#25997=B_SPLINE_CURVE_WITH_KNOTS('',3,(#416349,#416350,#416351,#416352,
#416353,#416354,#416355,#416356,#416357,#416358,#416359,#416360,#416361,
#416362,#416363,#416364,#416365,#416366,#416367,#416368,#416369,#416370,
#416371,#416372,#416373),.UNSPECIFIED.,.F.,.F.,(4,3,3,3,3,3,3,3,4),(0.,
2.85550478878827E-5,4.78559032675575E-5,6.34108981925974E-5,7.91451746296055E-5,
9.26886647080577E-5,0.000106465540580228,0.00012767876014108,0.000152977955413165),
 .UNSPECIFIED.);
#25998=B_SPLINE_CURVE_WITH_KNOTS('',3,(#416381,#416382,#416383,#416384,
#416385,#416386,#416387,#416388,#416389,#416390,#416391,#416392,#416393,
#416394,#416395,#416396,#416397,#416398,#416399,#416400,#416401,#416402,
#416403,#416404,#416405),.UNSPECIFIED.,.F.,.F.,(4,3,3,3,3,3,3,3,4),(0.,
2.85550478878827E-5,4.78559032675578E-5,6.34108981925978E-5,7.91451746296065E-5,
9.26886647080582E-5,0.000106465540580229,0.000127678760141082,0.000152977955413167),
 .UNSPECIFIED.);
#25999=B_SPLINE_CURVE_WITH_KNOTS('',3,(#416413,#416414,#416415,#416416,
#416417,#416418,#416419,#416420,#416421,#416422,#416423,#416424,#416425,
#416426,#416427,#416428,#416429,#416430,#416431,#416432,#416433,#416434,
#416435,#416436,#416437),.UNSPECIFIED.,.F.,.F.,(4,3,3,3,3,3,3,3,4),(0.,
2.85550478878827E-5,4.78559032675576E-5,6.34108981925972E-5,7.91451746296057E-5,
9.26886647080576E-5,0.000106465540580229,0.00012767876014108,0.000152977955413166),
 .UNSPECIFIED.);
#26000=B_SPLINE_CURVE_WITH_KNOTS('',3,(#416445,#416446,#416447,#416448,
#416449,#416450,#416451,#416452,#416453,#416454,#416455,#416456,#416457,
#416458,#416459,#416460,#416461,#416462,#416463,#416464,#416465,#416466,
#416467,#416468,#416469),.UNSPECIFIED.,.F.,.F.,(4,3,3,3,3,3,3,3,4),(0.,
2.85550478878827E-5,4.78559032675579E-5,6.34108981925976E-5,7.9145174629606E-5,
9.26886647080581E-5,0.000106465540580229,0.000127678760141081,0.000152977955413166),
 .UNSPECIFIED.);
#26001=B_SPLINE_CURVE_WITH_KNOTS('',3,(#416477,#416478,#416479,#416480,
#416481,#416482,#416483,#416484,#416485,#416486,#416487,#416488,#416489,
#416490,#416491,#416492,#416493,#416494,#416495,#416496,#416497,#416498,
#416499,#416500,#416501),.UNSPECIFIED.,.F.,.F.,(4,3,3,3,3,3,3,3,4),(0.,
2.85550478878828E-5,4.78559032675579E-5,6.34108981925975E-5,7.91451746296059E-5,
9.2688664708058E-5,0.000106465540580229,0.00012767876014108,0.000152977955413165),
 .UNSPECIFIED.);
#26002=B_SPLINE_CURVE_WITH_KNOTS('',3,(#416509,#416510,#416511,#416512,
#416513,#416514,#416515,#416516,#416517,#416518,#416519,#416520,#416521,
#416522,#416523,#416524,#416525,#416526,#416527,#416528,#416529,#416530,
#416531,#416532,#416533),.UNSPECIFIED.,.F.,.F.,(4,3,3,3,3,3,3,3,4),(0.,
2.85550478878826E-5,4.78559032675578E-5,6.34108981925975E-5,7.91451746296059E-5,
9.2688664708058E-5,0.000106465540580229,0.000127678760141081,0.000152977955413166),
 .UNSPECIFIED.);
#26003=B_SPLINE_CURVE_WITH_KNOTS('',3,(#416541,#416542,#416543,#416544,
#416545,#416546,#416547,#416548,#416549,#416550,#416551,#416552,#416553,
#416554,#416555,#416556,#416557,#416558,#416559,#416560,#416561,#416562,
#416563,#416564,#416565),.UNSPECIFIED.,.F.,.F.,(4,3,3,3,3,3,3,3,4),(0.,
2.85550478878828E-5,4.78559032675578E-5,6.34108981925975E-5,7.9145174629606E-5,
9.26886647080578E-5,0.000106465540580229,0.000127678760141081,0.000152977955413166),
 .UNSPECIFIED.);
#26004=B_SPLINE_CURVE_WITH_KNOTS('',3,(#416573,#416574,#416575,#416576,
#416577,#416578,#416579,#416580,#416581,#416582,#416583,#416584,#416585,
#416586,#416587,#416588,#416589,#416590,#416591,#416592,#416593,#416594,
#416595,#416596,#416597),.UNSPECIFIED.,.F.,.F.,(4,3,3,3,3,3,3,3,4),(0.,
2.85550478878824E-5,4.78559032675577E-5,6.34108981925973E-5,7.91451746296057E-5,
9.26886647080576E-5,0.000106465540580228,0.00012767876014108,0.000152977955413165),
 .UNSPECIFIED.);
#26005=B_SPLINE_CURVE_WITH_KNOTS('',3,(#416605,#416606,#416607,#416608,
#416609,#416610,#416611,#416612,#416613,#416614,#416615,#416616,#416617,
#416618,#416619,#416620,#416621,#416622,#416623,#416624,#416625,#416626,
#416627,#416628,#416629),.UNSPECIFIED.,.F.,.F.,(4,3,3,3,3,3,3,3,4),(0.,
2.85550478878829E-5,4.7855903267558E-5,6.34108981925977E-5,7.91451746296061E-5,
9.26886647080582E-5,0.000106465540580229,0.000127678760141081,0.000152977955413166),
 .UNSPECIFIED.);
#26006=B_SPLINE_CURVE_WITH_KNOTS('',3,(#416637,#416638,#416639,#416640,
#416641,#416642,#416643,#416644,#416645,#416646,#416647,#416648,#416649,
#416650,#416651,#416652,#416653,#416654,#416655,#416656,#416657,#416658,
#416659,#416660,#416661),.UNSPECIFIED.,.F.,.F.,(4,3,3,3,3,3,3,3,4),(0.,
2.85550478878826E-5,4.78559032675577E-5,6.34108981925972E-5,7.91451746296056E-5,
9.26886647080577E-5,0.000106465540580228,0.000127678760141081,0.000152977955413165),
 .UNSPECIFIED.);
#26007=B_SPLINE_CURVE_WITH_KNOTS('',3,(#416669,#416670,#416671,#416672,
#416673,#416674,#416675,#416676,#416677,#416678,#416679,#416680,#416681,
#416682,#416683,#416684,#416685,#416686,#416687,#416688,#416689,#416690,
#416691,#416692,#416693),.UNSPECIFIED.,.F.,.F.,(4,3,3,3,3,3,3,3,4),(0.,
2.85550478878825E-5,4.78559032675577E-5,6.34108981925973E-5,7.91451746296057E-5,
9.26886647080579E-5,0.000106465540580228,0.000127678760141081,0.000152977955413166),
 .UNSPECIFIED.);
#26008=B_SPLINE_CURVE_WITH_KNOTS('',3,(#416701,#416702,#416703,#416704,
#416705,#416706,#416707,#416708,#416709,#416710,#416711,#416712,#416713,
#416714,#416715,#416716,#416717,#416718,#416719,#416720,#416721,#416722,
#416723,#416724,#416725),.UNSPECIFIED.,.F.,.F.,(4,3,3,3,3,3,3,3,4),(0.,
2.85550478878828E-5,4.78559032675579E-5,6.34108981925977E-5,7.9145174629606E-5,
9.26886647080581E-5,0.000106465540580229,0.000127678760141081,0.000152977955413166),
 .UNSPECIFIED.);
#26009=B_SPLINE_CURVE_WITH_KNOTS('',3,(#416732,#416733,#416734,#416735,
#416736,#416737,#416738,#416739,#416740,#416741,#416742,#416743,#416744),
 .UNSPECIFIED.,.F.,.F.,(4,3,3,3,4),(0.,2.85550478876862E-5,4.78559032672286E-5,
6.34108981921613E-5,7.65824322177166E-5),.UNSPECIFIED.);
#26010=B_SPLINE_CURVE_WITH_KNOTS('',3,(#416755,#416756,#416757,#416758,
#416759,#416760,#416761,#416762,#416763,#416764,#416765,#416766,#416767,
#416768,#416769,#416770),.UNSPECIFIED.,.F.,.F.,(4,3,3,3,3,4),(0.,6.54397980774373E-6,
1.78746088883289E-5,2.90961555784964E-5,4.25056718483935E-5,6.52023395140211E-5),
 .UNSPECIFIED.);
#26011=B_SPLINE_CURVE_WITH_KNOTS('',3,(#416772,#416773,#416774,#416775,
#416776,#416777,#416778,#416779,#416780,#416781,#416782,#416783,#416784,
#416785,#416786,#416787),.UNSPECIFIED.,.F.,.F.,(4,3,3,3,3,4),(2.71050543121376E-20,
1.81271519801731E-5,3.33528222530966E-5,4.35246196643646E-5,5.39830173117273E-5,
6.44389677343626E-5),.UNSPECIFIED.);
#26012=B_SPLINE_CURVE_WITH_KNOTS('',3,(#416794,#416795,#416796,#416797,
#416798,#416799,#416800,#416801,#416802,#416803,#416804,#416805,#416806,
#416807,#416808,#416809),.UNSPECIFIED.,.F.,.F.,(4,3,3,3,3,4),(0.,6.54397980774379E-6,
1.78746088883289E-5,2.90961555784964E-5,4.25056718483935E-5,6.52023395140209E-5),
 .UNSPECIFIED.);
#26013=B_SPLINE_CURVE_WITH_KNOTS('',3,(#416811,#416812,#416813,#416814,
#416815,#416816,#416817,#416818,#416819,#416820,#416821,#416822,#416823,
#416824,#416825,#416826),.UNSPECIFIED.,.F.,.F.,(4,3,3,3,3,4),(5.42101086242752E-20,
1.81271519801731E-5,3.33528222530966E-5,4.35246196643646E-5,5.39830173117273E-5,
6.44389677343626E-5),.UNSPECIFIED.);
#26014=B_SPLINE_CURVE_WITH_KNOTS('',3,(#416833,#416834,#416835,#416836,
#416837,#416838,#416839,#416840,#416841,#416842,#416843,#416844,#416845,
#416846,#416847,#416848),.UNSPECIFIED.,.F.,.F.,(4,3,3,3,3,4),(0.,6.5439798077437E-6,
1.78746088883288E-5,2.90961555784963E-5,4.25056718483934E-5,6.52023395140209E-5),
 .UNSPECIFIED.);
#26015=B_SPLINE_CURVE_WITH_KNOTS('',3,(#416850,#416851,#416852,#416853,
#416854,#416855,#416856,#416857,#416858,#416859,#416860,#416861,#416862,
#416863,#416864,#416865),.UNSPECIFIED.,.F.,.F.,(4,3,3,3,3,4),(0.,1.81271519801731E-5,
3.33528222530966E-5,4.35246196643646E-5,5.39830173117273E-5,6.44389677343627E-5),
 .UNSPECIFIED.);
#26016=B_SPLINE_CURVE_WITH_KNOTS('',3,(#416872,#416873,#416874,#416875,
#416876,#416877,#416878,#416879,#416880,#416881,#416882,#416883,#416884,
#416885,#416886,#416887),.UNSPECIFIED.,.F.,.F.,(4,3,3,3,3,4),(0.,6.54397980774353E-6,
1.78746088883287E-5,2.90961555784963E-5,4.25056718483933E-5,6.52023395140208E-5),
 .UNSPECIFIED.);
#26017=B_SPLINE_CURVE_WITH_KNOTS('',3,(#416889,#416890,#416891,#416892,
#416893,#416894,#416895,#416896,#416897,#416898,#416899,#416900,#416901,
#416902,#416903,#416904),.UNSPECIFIED.,.F.,.F.,(4,3,3,3,3,4),(0.,1.81271519801731E-5,
3.33528222530967E-5,4.35246196643647E-5,5.39830173117274E-5,6.44389677343627E-5),
 .UNSPECIFIED.);
#26018=B_SPLINE_CURVE_WITH_KNOTS('',3,(#416911,#416912,#416913,#416914,
#416915,#416916,#416917,#416918,#416919,#416920,#416921,#416922,#416923,
#416924,#416925,#416926),.UNSPECIFIED.,.F.,.F.,(4,3,3,3,3,4),(0.,6.54397980774348E-6,
1.78746088883288E-5,2.90961555784961E-5,4.25056718483932E-5,6.52023395140207E-5),
 .UNSPECIFIED.);
#26019=B_SPLINE_CURVE_WITH_KNOTS('',3,(#416928,#416929,#416930,#416931,
#416932,#416933,#416934,#416935,#416936,#416937,#416938,#416939,#416940,
#416941,#416942,#416943),.UNSPECIFIED.,.F.,.F.,(4,3,3,3,3,4),(0.,1.81271519801731E-5,
3.33528222530967E-5,4.35246196643646E-5,5.39830173117275E-5,6.44389677343628E-5),
 .UNSPECIFIED.);
#26020=B_SPLINE_CURVE_WITH_KNOTS('',3,(#416950,#416951,#416952,#416953,
#416954,#416955,#416956,#416957,#416958,#416959,#416960,#416961,#416962,
#416963,#416964,#416965),.UNSPECIFIED.,.F.,.F.,(4,3,3,3,3,4),(0.,6.54397980774384E-6,
1.78746088883289E-5,2.90961555784964E-5,4.25056718483935E-5,6.5202339514021E-5),
 .UNSPECIFIED.);
#26021=B_SPLINE_CURVE_WITH_KNOTS('',3,(#416967,#416968,#416969,#416970,
#416971,#416972,#416973,#416974,#416975,#416976,#416977,#416978,#416979,
#416980,#416981,#416982),.UNSPECIFIED.,.F.,.F.,(4,3,3,3,3,4),(0.,1.81271519801731E-5,
3.33528222530965E-5,4.35246196643645E-5,5.39830173117272E-5,6.44389677343626E-5),
 .UNSPECIFIED.);
#26022=B_SPLINE_CURVE_WITH_KNOTS('',3,(#416989,#416990,#416991,#416992,
#416993,#416994,#416995,#416996,#416997,#416998,#416999,#417000,#417001,
#417002,#417003,#417004),.UNSPECIFIED.,.F.,.F.,(4,3,3,3,3,4),(0.,6.54397980774374E-6,
1.78746088883286E-5,2.90961555784963E-5,4.25056718483934E-5,6.5202339514021E-5),
 .UNSPECIFIED.);
#26023=B_SPLINE_CURVE_WITH_KNOTS('',3,(#417006,#417007,#417008,#417009,
#417010,#417011,#417012,#417013,#417014,#417015,#417016,#417017,#417018,
#417019,#417020,#417021),.UNSPECIFIED.,.F.,.F.,(4,3,3,3,3,4),(0.,1.81271519801732E-5,
3.33528222530967E-5,4.35246196643648E-5,5.39830173117271E-5,6.44389677343624E-5),
 .UNSPECIFIED.);
#26024=B_SPLINE_CURVE_WITH_KNOTS('',3,(#417028,#417029,#417030,#417031,
#417032,#417033,#417034,#417035,#417036,#417037,#417038,#417039,#417040,
#417041,#417042,#417043),.UNSPECIFIED.,.F.,.F.,(4,3,3,3,3,4),(0.,6.54397980774362E-6,
1.78746088883288E-5,2.90961555784963E-5,4.25056718483934E-5,6.52023395140209E-5),
 .UNSPECIFIED.);
#26025=B_SPLINE_CURVE_WITH_KNOTS('',3,(#417045,#417046,#417047,#417048,
#417049,#417050,#417051,#417052,#417053,#417054,#417055,#417056,#417057,
#417058,#417059,#417060),.UNSPECIFIED.,.F.,.F.,(4,3,3,3,3,4),(0.,1.81271519801732E-5,
3.33528222530965E-5,4.35246196643646E-5,5.39830173117272E-5,6.44389677343625E-5),
 .UNSPECIFIED.);
#26026=B_SPLINE_CURVE_WITH_KNOTS('',3,(#417067,#417068,#417069,#417070,
#417071,#417072,#417073,#417074,#417075,#417076,#417077,#417078,#417079,
#417080,#417081,#417082),.UNSPECIFIED.,.F.,.F.,(4,3,3,3,3,4),(0.,6.54397980774392E-6,
1.78746088883292E-5,2.90961555784966E-5,4.25056718483937E-5,6.52023395140214E-5),
 .UNSPECIFIED.);
#26027=B_SPLINE_CURVE_WITH_KNOTS('',3,(#417084,#417085,#417086,#417087,
#417088,#417089,#417090,#417091,#417092,#417093,#417094,#417095,#417096,
#417097,#417098,#417099),.UNSPECIFIED.,.F.,.F.,(4,3,3,3,3,4),(0.,1.81271519801731E-5,
3.33528222530967E-5,4.35246196643647E-5,5.39830173117272E-5,6.44389677343625E-5),
 .UNSPECIFIED.);
#26028=B_SPLINE_CURVE_WITH_KNOTS('',3,(#417106,#417107,#417108,#417109,
#417110,#417111,#417112,#417113,#417114,#417115,#417116,#417117,#417118,
#417119,#417120,#417121),.UNSPECIFIED.,.F.,.F.,(4,3,3,3,3,4),(0.,6.54397980774367E-6,
1.78746088883289E-5,2.90961555784963E-5,4.25056718483934E-5,6.52023395140208E-5),
 .UNSPECIFIED.);
#26029=B_SPLINE_CURVE_WITH_KNOTS('',3,(#417123,#417124,#417125,#417126,
#417127,#417128,#417129,#417130,#417131,#417132,#417133,#417134,#417135,
#417136,#417137,#417138),.UNSPECIFIED.,.F.,.F.,(4,3,3,3,3,4),(0.,1.81271519801731E-5,
3.33528222530965E-5,4.35246196643647E-5,5.39830173117273E-5,6.44389677343627E-5),
 .UNSPECIFIED.);
#26030=B_SPLINE_CURVE_WITH_KNOTS('',3,(#417145,#417146,#417147,#417148,
#417149,#417150,#417151,#417152,#417153,#417154,#417155,#417156,#417157,
#417158,#417159,#417160),.UNSPECIFIED.,.F.,.F.,(4,3,3,3,3,4),(0.,6.54397980774391E-6,
1.7874608888329E-5,2.90961555784965E-5,4.25056718483936E-5,6.52023395140211E-5),
 .UNSPECIFIED.);
#26031=B_SPLINE_CURVE_WITH_KNOTS('',3,(#417162,#417163,#417164,#417165,
#417166,#417167,#417168,#417169,#417170,#417171,#417172,#417173,#417174,
#417175,#417176,#417177),.UNSPECIFIED.,.F.,.F.,(4,3,3,3,3,4),(0.,1.8127151980173E-5,
3.33528222530963E-5,4.35246196643646E-5,5.39830173117274E-5,6.44389677343629E-5),
 .UNSPECIFIED.);
#26032=B_SPLINE_CURVE_WITH_KNOTS('',3,(#417184,#417185,#417186,#417187,
#417188,#417189,#417190,#417191,#417192,#417193,#417194,#417195,#417196,
#417197,#417198,#417199),.UNSPECIFIED.,.F.,.F.,(4,3,3,3,3,4),(0.,6.54397980774351E-6,
1.78746088883289E-5,2.90961555784962E-5,4.25056718483934E-5,6.52023395140209E-5),
 .UNSPECIFIED.);
#26033=B_SPLINE_CURVE_WITH_KNOTS('',3,(#417201,#417202,#417203,#417204,
#417205,#417206,#417207,#417208,#417209,#417210,#417211,#417212,#417213,
#417214,#417215,#417216),.UNSPECIFIED.,.F.,.F.,(4,3,3,3,3,4),(0.,1.81271519801732E-5,
3.33528222530968E-5,4.35246196643648E-5,5.39830173117279E-5,6.44389677343633E-5),
 .UNSPECIFIED.);
#26034=B_SPLINE_CURVE_WITH_KNOTS('',3,(#417223,#417224,#417225,#417226,
#417227,#417228,#417229,#417230,#417231,#417232,#417233,#417234,#417235,
#417236,#417237,#417238),.UNSPECIFIED.,.F.,.F.,(4,3,3,3,3,4),(0.,6.5439798077437E-6,
1.78746088883288E-5,2.90961555784963E-5,4.25056718483932E-5,6.52023395140205E-5),
 .UNSPECIFIED.);
#26035=B_SPLINE_CURVE_WITH_KNOTS('',3,(#417240,#417241,#417242,#417243,
#417244,#417245,#417246,#417247,#417248,#417249,#417250,#417251,#417252,
#417253,#417254,#417255),.UNSPECIFIED.,.F.,.F.,(4,3,3,3,3,4),(0.,1.81271519801731E-5,
3.33528222530966E-5,4.35246196643646E-5,5.39830173117274E-5,6.44389677343625E-5),
 .UNSPECIFIED.);
#26036=B_SPLINE_CURVE_WITH_KNOTS('',3,(#417262,#417263,#417264,#417265,
#417266,#417267,#417268,#417269,#417270,#417271,#417272,#417273,#417274,
#417275,#417276,#417277),.UNSPECIFIED.,.F.,.F.,(4,3,3,3,3,4),(0.,6.54397980774372E-6,
1.78746088883288E-5,2.90961555784962E-5,4.25056718483931E-5,6.52023395140206E-5),
 .UNSPECIFIED.);
#26037=B_SPLINE_CURVE_WITH_KNOTS('',3,(#417279,#417280,#417281,#417282,
#417283,#417284,#417285,#417286,#417287,#417288,#417289,#417290,#417291,
#417292,#417293,#417294),.UNSPECIFIED.,.F.,.F.,(4,3,3,3,3,4),(0.,1.81271519801731E-5,
3.33528222530966E-5,4.35246196643646E-5,5.39830173117274E-5,6.4438967734363E-5),
 .UNSPECIFIED.);
#26038=B_SPLINE_CURVE_WITH_KNOTS('',3,(#417301,#417302,#417303,#417304,
#417305,#417306,#417307,#417308,#417309,#417310,#417311,#417312,#417313,
#417314,#417315,#417316),.UNSPECIFIED.,.F.,.F.,(4,3,3,3,3,4),(0.,6.54397980774378E-6,
1.78746088883289E-5,2.90961555784965E-5,4.25056718483935E-5,6.52023395140212E-5),
 .UNSPECIFIED.);
#26039=B_SPLINE_CURVE_WITH_KNOTS('',3,(#417318,#417319,#417320,#417321,
#417322,#417323,#417324,#417325,#417326,#417327,#417328,#417329,#417330,
#417331,#417332,#417333),.UNSPECIFIED.,.F.,.F.,(4,3,3,3,3,4),(0.,1.81271519801731E-5,
3.33528222530964E-5,4.35246196643642E-5,5.39830173117271E-5,6.44389677343626E-5),
 .UNSPECIFIED.);
#26040=B_SPLINE_CURVE_WITH_KNOTS('',3,(#417340,#417341,#417342,#417343,
#417344,#417345,#417346,#417347,#417348,#417349,#417350,#417351,#417352,
#417353,#417354,#417355),.UNSPECIFIED.,.F.,.F.,(4,3,3,3,3,4),(0.,6.54397980774373E-6,
1.78746088883289E-5,2.90961555784964E-5,4.25056718483935E-5,6.52023395140208E-5),
 .UNSPECIFIED.);
#26041=B_SPLINE_CURVE_WITH_KNOTS('',3,(#417357,#417358,#417359,#417360,
#417361,#417362,#417363,#417364,#417365,#417366,#417367,#417368,#417369,
#417370,#417371,#417372),.UNSPECIFIED.,.F.,.F.,(4,3,3,3,3,4),(0.,1.81271519801731E-5,
3.33528222530966E-5,4.35246196643646E-5,5.39830173117274E-5,6.44389677343629E-5),
 .UNSPECIFIED.);
#26042=B_SPLINE_CURVE_WITH_KNOTS('',3,(#417379,#417380,#417381,#417382,
#417383,#417384,#417385,#417386,#417387,#417388,#417389,#417390,#417391,
#417392,#417393,#417394),.UNSPECIFIED.,.F.,.F.,(4,3,3,3,3,4),(0.,6.54397980774365E-6,
1.78746088883288E-5,2.90961555784964E-5,4.25056718483935E-5,6.52023395140211E-5),
 .UNSPECIFIED.);
#26043=B_SPLINE_CURVE_WITH_KNOTS('',3,(#417396,#417397,#417398,#417399,
#417400,#417401,#417402,#417403,#417404,#417405,#417406,#417407,#417408,
#417409,#417410,#417411),.UNSPECIFIED.,.F.,.F.,(4,3,3,3,3,4),(0.,1.81271519801731E-5,
3.33528222530965E-5,4.35246196643645E-5,5.39830173117272E-5,6.44389677343626E-5),
 .UNSPECIFIED.);
#26044=B_SPLINE_CURVE_WITH_KNOTS('',3,(#417418,#417419,#417420,#417421,
#417422,#417423,#417424,#417425,#417426,#417427,#417428,#417429,#417430,
#417431,#417432,#417433),.UNSPECIFIED.,.F.,.F.,(4,3,3,3,3,4),(0.,6.54397980774371E-6,
1.78746088883289E-5,2.90961555784963E-5,4.25056718483935E-5,6.52023395140209E-5),
 .UNSPECIFIED.);
#26045=B_SPLINE_CURVE_WITH_KNOTS('',3,(#417435,#417436,#417437,#417438,
#417439,#417440,#417441,#417442,#417443,#417444,#417445,#417446,#417447,
#417448,#417449,#417450),.UNSPECIFIED.,.F.,.F.,(4,3,3,3,3,4),(5.42101086242752E-20,
1.81271519801731E-5,3.33528222530966E-5,4.35246196643646E-5,5.39830173117274E-5,
6.44389677343628E-5),.UNSPECIFIED.);
#26046=B_SPLINE_CURVE_WITH_KNOTS('',3,(#417457,#417458,#417459,#417460,
#417461,#417462,#417463,#417464,#417465,#417466,#417467,#417468,#417469,
#417470,#417471,#417472),.UNSPECIFIED.,.F.,.F.,(4,3,3,3,3,4),(0.,6.54397980774374E-6,
1.78746088883289E-5,2.90961555784964E-5,4.25056718483934E-5,6.52023395140209E-5),
 .UNSPECIFIED.);
#26047=B_SPLINE_CURVE_WITH_KNOTS('',3,(#417474,#417475,#417476,#417477,
#417478,#417479,#417480,#417481,#417482,#417483,#417484,#417485,#417486,
#417487,#417488,#417489),.UNSPECIFIED.,.F.,.F.,(4,3,3,3,3,4),(2.71050543121376E-20,
1.81271519801731E-5,3.33528222530966E-5,4.35246196643646E-5,5.39830173117273E-5,
6.44389677343626E-5),.UNSPECIFIED.);
#26048=B_SPLINE_CURVE_WITH_KNOTS('',3,(#417496,#417497,#417498,#417499,
#417500,#417501,#417502,#417503,#417504,#417505,#417506,#417507,#417508,
#417509,#417510,#417511),.UNSPECIFIED.,.F.,.F.,(4,3,3,3,3,4),(0.,6.54397980774373E-6,
1.78746088883289E-5,2.90961555784963E-5,4.25056718483934E-5,6.52023395140208E-5),
 .UNSPECIFIED.);
#26049=B_SPLINE_CURVE_WITH_KNOTS('',3,(#417513,#417514,#417515,#417516,
#417517,#417518,#417519,#417520,#417521,#417522,#417523,#417524,#417525,
#417526,#417527,#417528),.UNSPECIFIED.,.F.,.F.,(4,3,3,3,3,4),(2.71050543121376E-20,
1.81271519801731E-5,3.33528222530966E-5,4.35246196643646E-5,5.39830173117273E-5,
6.44389677343626E-5),.UNSPECIFIED.);
#26050=B_SPLINE_CURVE_WITH_KNOTS('',3,(#417535,#417536,#417537,#417538,
#417539,#417540,#417541,#417542,#417543,#417544,#417545,#417546,#417547,
#417548,#417549,#417550),.UNSPECIFIED.,.F.,.F.,(4,3,3,3,3,4),(0.,6.54397980774376E-6,
1.78746088883289E-5,2.90961555784964E-5,4.25056718483935E-5,6.5202339514021E-5),
 .UNSPECIFIED.);
#26051=B_SPLINE_CURVE_WITH_KNOTS('',3,(#417552,#417553,#417554,#417555,
#417556,#417557,#417558,#417559,#417560,#417561,#417562,#417563,#417564,
#417565,#417566,#417567),.UNSPECIFIED.,.F.,.F.,(4,3,3,3,3,4),(5.42101086242752E-20,
1.81271519801731E-5,3.33528222530966E-5,4.35246196643646E-5,5.39830173117273E-5,
6.44389677343626E-5),.UNSPECIFIED.);
#26052=B_SPLINE_CURVE_WITH_KNOTS('',3,(#417574,#417575,#417576,#417577,
#417578,#417579,#417580,#417581,#417582,#417583,#417584,#417585,#417586,
#417587,#417588,#417589),.UNSPECIFIED.,.F.,.F.,(4,3,3,3,3,4),(0.,6.54397980774373E-6,
1.78746088883289E-5,2.90961555784964E-5,4.25056718483934E-5,6.52023395140209E-5),
 .UNSPECIFIED.);
#26053=B_SPLINE_CURVE_WITH_KNOTS('',3,(#417591,#417592,#417593,#417594,
#417595,#417596,#417597,#417598,#417599,#417600,#417601,#417602,#417603,
#417604,#417605,#417606),.UNSPECIFIED.,.F.,.F.,(4,3,3,3,3,4),(0.,1.81271519801731E-5,
3.33528222530965E-5,4.35246196643645E-5,5.39830173117274E-5,6.44389677343627E-5),
 .UNSPECIFIED.);
#26054=B_SPLINE_CURVE_WITH_KNOTS('',3,(#417613,#417614,#417615,#417616,
#417617,#417618,#417619,#417620,#417621,#417622,#417623,#417624,#417625,
#417626,#417627,#417628),.UNSPECIFIED.,.F.,.F.,(4,3,3,3,3,4),(0.,6.54397980774377E-6,
1.78746088883288E-5,2.90961555784963E-5,4.25056718483935E-5,6.52023395140211E-5),
 .UNSPECIFIED.);
#26055=B_SPLINE_CURVE_WITH_KNOTS('',3,(#417630,#417631,#417632,#417633,
#417634,#417635,#417636,#417637,#417638,#417639,#417640,#417641,#417642,
#417643,#417644,#417645),.UNSPECIFIED.,.F.,.F.,(4,3,3,3,3,4),(0.,1.81271519801731E-5,
3.33528222530966E-5,4.35246196643646E-5,5.39830173117272E-5,6.44389677343625E-5),
 .UNSPECIFIED.);
#26056=B_SPLINE_CURVE_WITH_KNOTS('',3,(#417652,#417653,#417654,#417655,
#417656,#417657,#417658,#417659,#417660,#417661,#417662,#417663,#417664,
#417665,#417666,#417667),.UNSPECIFIED.,.F.,.F.,(4,3,3,3,3,4),(0.,6.54397980774367E-6,
1.78746088883288E-5,2.90961555784963E-5,4.25056718483934E-5,6.52023395140209E-5),
 .UNSPECIFIED.);
#26057=B_SPLINE_CURVE_WITH_KNOTS('',3,(#417669,#417670,#417671,#417672,
#417673,#417674,#417675,#417676,#417677,#417678,#417679,#417680,#417681,
#417682,#417683,#417684),.UNSPECIFIED.,.F.,.F.,(4,3,3,3,3,4),(0.,1.81271519801731E-5,
3.33528222530967E-5,4.35246196643647E-5,5.39830173117276E-5,6.4438967734363E-5),
 .UNSPECIFIED.);
#26058=B_SPLINE_CURVE_WITH_KNOTS('',3,(#417691,#417692,#417693,#417694,
#417695,#417696,#417697,#417698,#417699,#417700,#417701,#417702,#417703,
#417704,#417705,#417706),.UNSPECIFIED.,.F.,.F.,(4,3,3,3,3,4),(0.,6.54397980774349E-6,
1.78746088883288E-5,2.90961555784963E-5,4.25056718483933E-5,6.52023395140206E-5),
 .UNSPECIFIED.);
#26059=B_SPLINE_CURVE_WITH_KNOTS('',3,(#417708,#417709,#417710,#417711,
#417712,#417713,#417714,#417715,#417716,#417717,#417718,#417719,#417720,
#417721,#417722,#417723),.UNSPECIFIED.,.F.,.F.,(4,3,3,3,3,4),(0.,1.81271519801732E-5,
3.33528222530966E-5,4.35246196643646E-5,5.39830173117274E-5,6.4438967734363E-5),
 .UNSPECIFIED.);
#26060=B_SPLINE_CURVE_WITH_KNOTS('',3,(#417730,#417731,#417732,#417733,
#417734,#417735,#417736,#417737,#417738,#417739,#417740,#417741,#417742,
#417743,#417744,#417745),.UNSPECIFIED.,.F.,.F.,(4,3,3,3,3,4),(0.,6.5439798077438E-6,
1.78746088883289E-5,2.90961555784962E-5,4.25056718483932E-5,6.52023395140206E-5),
 .UNSPECIFIED.);
#26061=B_SPLINE_CURVE_WITH_KNOTS('',3,(#417747,#417748,#417749,#417750,
#417751,#417752,#417753,#417754,#417755,#417756,#417757,#417758,#417759,
#417760,#417761,#417762),.UNSPECIFIED.,.F.,.F.,(4,3,3,3,3,4),(0.,1.81271519801732E-5,
3.33528222530965E-5,4.35246196643647E-5,5.39830173117274E-5,6.44389677343628E-5),
 .UNSPECIFIED.);
#26062=B_SPLINE_CURVE_WITH_KNOTS('',3,(#417769,#417770,#417771,#417772,
#417773,#417774,#417775,#417776,#417777,#417778,#417779,#417780,#417781,
#417782,#417783,#417784),.UNSPECIFIED.,.F.,.F.,(4,3,3,3,3,4),(0.,6.54397980774388E-6,
1.78746088883289E-5,2.90961555784964E-5,4.25056718483935E-5,6.52023395140211E-5),
 .UNSPECIFIED.);
#26063=B_SPLINE_CURVE_WITH_KNOTS('',3,(#417786,#417787,#417788,#417789,
#417790,#417791,#417792,#417793,#417794,#417795,#417796,#417797,#417798,
#417799,#417800,#417801),.UNSPECIFIED.,.F.,.F.,(4,3,3,3,3,4),(0.,1.8127151980173E-5,
3.33528222530964E-5,4.35246196643643E-5,5.39830173117268E-5,6.44389677343624E-5),
 .UNSPECIFIED.);
#26064=B_SPLINE_CURVE_WITH_KNOTS('',3,(#417808,#417809,#417810,#417811,
#417812,#417813,#417814,#417815,#417816,#417817,#417818,#417819,#417820,
#417821,#417822,#417823),.UNSPECIFIED.,.F.,.F.,(4,3,3,3,3,4),(0.,6.54397980774362E-6,
1.78746088883289E-5,2.90961555784964E-5,4.25056718483934E-5,6.52023395140208E-5),
 .UNSPECIFIED.);
#26065=B_SPLINE_CURVE_WITH_KNOTS('',3,(#417825,#417826,#417827,#417828,
#417829,#417830,#417831,#417832,#417833,#417834,#417835,#417836,#417837,
#417838,#417839,#417840),.UNSPECIFIED.,.F.,.F.,(4,3,3,3,3,4),(0.,1.81271519801731E-5,
3.33528222530967E-5,4.35246196643645E-5,5.39830173117272E-5,6.44389677343627E-5),
 .UNSPECIFIED.);
#26066=B_SPLINE_CURVE_WITH_KNOTS('',3,(#417847,#417848,#417849,#417850,
#417851,#417852,#417853,#417854,#417855,#417856,#417857,#417858,#417859,
#417860,#417861,#417862),.UNSPECIFIED.,.F.,.F.,(4,3,3,3,3,4),(0.,6.54397980774398E-6,
1.7874608888329E-5,2.90961555784965E-5,4.25056718483937E-5,6.52023395140213E-5),
 .UNSPECIFIED.);
#26067=B_SPLINE_CURVE_WITH_KNOTS('',3,(#417864,#417865,#417866,#417867,
#417868,#417869,#417870,#417871,#417872,#417873,#417874,#417875,#417876,
#417877,#417878,#417879),.UNSPECIFIED.,.F.,.F.,(4,3,3,3,3,4),(0.,1.81271519801732E-5,
3.33528222530968E-5,4.35246196643646E-5,5.39830173117275E-5,6.44389677343627E-5),
 .UNSPECIFIED.);
#26068=B_SPLINE_CURVE_WITH_KNOTS('',3,(#417886,#417887,#417888,#417889,
#417890,#417891,#417892,#417893,#417894,#417895,#417896,#417897,#417898,
#417899,#417900,#417901),.UNSPECIFIED.,.F.,.F.,(4,3,3,3,3,4),(0.,6.54397980774373E-6,
1.78746088883286E-5,2.90961555784964E-5,4.25056718483933E-5,6.52023395140207E-5),
 .UNSPECIFIED.);
#26069=B_SPLINE_CURVE_WITH_KNOTS('',3,(#417903,#417904,#417905,#417906,
#417907,#417908,#417909,#417910,#417911,#417912,#417913,#417914,#417915,
#417916,#417917,#417918),.UNSPECIFIED.,.F.,.F.,(4,3,3,3,3,4),(0.,1.81271519801732E-5,
3.33528222530965E-5,4.35246196643643E-5,5.39830173117273E-5,6.44389677343627E-5),
 .UNSPECIFIED.);
#26070=B_SPLINE_CURVE_WITH_KNOTS('',3,(#417925,#417926,#417927,#417928,
#417929,#417930,#417931,#417932,#417933,#417934,#417935,#417936,#417937,
#417938,#417939,#417940),.UNSPECIFIED.,.F.,.F.,(4,3,3,3,3,4),(0.,6.54397980774373E-6,
1.78746088883289E-5,2.90961555784966E-5,4.25056718483937E-5,6.52023395140213E-5),
 .UNSPECIFIED.);
#26071=B_SPLINE_CURVE_WITH_KNOTS('',3,(#417942,#417943,#417944,#417945,
#417946,#417947,#417948,#417949,#417950,#417951,#417952,#417953,#417954,
#417955,#417956,#417957),.UNSPECIFIED.,.F.,.F.,(4,3,3,3,3,4),(0.,1.81271519801731E-5,
3.33528222530965E-5,4.35246196643644E-5,5.39830173117273E-5,6.44389677343629E-5),
 .UNSPECIFIED.);
#26072=B_SPLINE_CURVE_WITH_KNOTS('',3,(#417964,#417965,#417966,#417967,
#417968,#417969,#417970,#417971,#417972,#417973,#417974,#417975,#417976,
#417977,#417978,#417979),.UNSPECIFIED.,.F.,.F.,(4,3,3,3,3,4),(0.,6.54397980774386E-6,
1.78746088883289E-5,2.90961555784964E-5,4.25056718483936E-5,6.52023395140211E-5),
 .UNSPECIFIED.);
#26073=B_SPLINE_CURVE_WITH_KNOTS('',3,(#417981,#417982,#417983,#417984,
#417985,#417986,#417987,#417988,#417989,#417990,#417991,#417992,#417993,
#417994,#417995,#417996),.UNSPECIFIED.,.F.,.F.,(4,3,3,3,3,4),(0.,1.81271519801731E-5,
3.33528222530964E-5,4.35246196643646E-5,5.39830173117272E-5,6.44389677343629E-5),
 .UNSPECIFIED.);
#26074=B_SPLINE_CURVE_WITH_KNOTS('',3,(#418003,#418004,#418005,#418006,
#418007,#418008,#418009,#418010,#418011,#418012,#418013,#418014,#418015,
#418016,#418017,#418018),.UNSPECIFIED.,.F.,.F.,(4,3,3,3,3,4),(0.,6.5439798077436E-6,
1.78746088883289E-5,2.90961555784965E-5,4.25056718483935E-5,6.52023395140211E-5),
 .UNSPECIFIED.);
#26075=B_SPLINE_CURVE_WITH_KNOTS('',3,(#418020,#418021,#418022,#418023,
#418024,#418025,#418026,#418027,#418028,#418029,#418030,#418031,#418032,
#418033,#418034,#418035),.UNSPECIFIED.,.F.,.F.,(4,3,3,3,3,4),(0.,1.81271519801731E-5,
3.33528222530965E-5,4.35246196643644E-5,5.39830173117273E-5,6.44389677343625E-5),
 .UNSPECIFIED.);
#26076=B_SPLINE_CURVE_WITH_KNOTS('',3,(#418042,#418043,#418044,#418045,
#418046,#418047,#418048,#418049,#418050,#418051,#418052,#418053,#418054,
#418055,#418056,#418057),.UNSPECIFIED.,.F.,.F.,(4,3,3,3,3,4),(0.,6.54397980774372E-6,
1.78746088883287E-5,2.90961555784964E-5,4.25056718483934E-5,6.52023395140209E-5),
 .UNSPECIFIED.);
#26077=B_SPLINE_CURVE_WITH_KNOTS('',3,(#418059,#418060,#418061,#418062,
#418063,#418064,#418065,#418066,#418067,#418068,#418069,#418070,#418071,
#418072,#418073,#418074),.UNSPECIFIED.,.F.,.F.,(4,3,3,3,3,4),(0.,1.8127151980173E-5,
3.33528222530966E-5,4.35246196643645E-5,5.39830173117273E-5,6.44389677343627E-5),
 .UNSPECIFIED.);
#26078=B_SPLINE_CURVE_WITH_KNOTS('',3,(#418081,#418082,#418083,#418084,
#418085,#418086,#418087,#418088,#418089,#418090,#418091,#418092,#418093,
#418094,#418095,#418096),.UNSPECIFIED.,.F.,.F.,(4,3,3,3,3,4),(0.,6.54397980774384E-6,
1.7874608888329E-5,2.90961555784964E-5,4.25056718483935E-5,6.52023395140211E-5),
 .UNSPECIFIED.);
#26079=B_SPLINE_CURVE_WITH_KNOTS('',3,(#418098,#418099,#418100,#418101,
#418102,#418103,#418104,#418105,#418106,#418107,#418108,#418109,#418110,
#418111,#418112,#418113),.UNSPECIFIED.,.F.,.F.,(4,3,3,3,3,4),(0.,1.81271519801731E-5,
3.33528222530964E-5,4.35246196643645E-5,5.39830173117271E-5,6.44389677343624E-5),
 .UNSPECIFIED.);
#26080=B_SPLINE_CURVE_WITH_KNOTS('',3,(#418120,#418121,#418122,#418123,
#418124,#418125,#418126,#418127,#418128,#418129,#418130,#418131,#418132,
#418133,#418134,#418135),.UNSPECIFIED.,.F.,.F.,(4,3,3,3,3,4),(0.,6.54397980774382E-6,
1.78746088883289E-5,2.90961555784965E-5,4.25056718483936E-5,6.52023395140212E-5),
 .UNSPECIFIED.);
#26081=B_SPLINE_CURVE_WITH_KNOTS('',3,(#418137,#418138,#418139,#418140,
#418141,#418142,#418143,#418144,#418145,#418146,#418147,#418148,#418149,
#418150,#418151,#418152),.UNSPECIFIED.,.F.,.F.,(4,3,3,3,3,4),(0.,1.81271519801731E-5,
3.33528222530966E-5,4.35246196643645E-5,5.39830173117275E-5,6.44389677343628E-5),
 .UNSPECIFIED.);
#26082=B_SPLINE_CURVE_WITH_KNOTS('',3,(#418159,#418160,#418161,#418162,
#418163,#418164,#418165,#418166,#418167,#418168,#418169,#418170,#418171,
#418172,#418173,#418174),.UNSPECIFIED.,.F.,.F.,(4,3,3,3,3,4),(0.,6.54397980774367E-6,
1.78746088883288E-5,2.90961555784963E-5,4.25056718483933E-5,6.52023395140207E-5),
 .UNSPECIFIED.);
#26083=B_SPLINE_CURVE_WITH_KNOTS('',3,(#418176,#418177,#418178,#418179,
#418180,#418181,#418182,#418183,#418184,#418185,#418186,#418187,#418188,
#418189,#418190,#418191),.UNSPECIFIED.,.F.,.F.,(4,3,3,3,3,4),(5.42101086242752E-20,
1.81271519801731E-5,3.33528222530966E-5,4.35246196643646E-5,5.39830173117274E-5,
6.44389677343627E-5),.UNSPECIFIED.);
#26084=B_SPLINE_CURVE_WITH_KNOTS('',3,(#418198,#418199,#418200,#418201,
#418202,#418203,#418204,#418205,#418206,#418207,#418208,#418209,#418210,
#418211,#418212,#418213),.UNSPECIFIED.,.F.,.F.,(4,3,3,3,3,4),(0.,6.54397980774372E-6,
1.78746088883289E-5,2.90961555784964E-5,4.25056718483934E-5,6.5202339514021E-5),
 .UNSPECIFIED.);
#26085=B_SPLINE_CURVE_WITH_KNOTS('',3,(#418215,#418216,#418217,#418218,
#418219,#418220,#418221,#418222,#418223,#418224,#418225,#418226,#418227,
#418228,#418229,#418230),.UNSPECIFIED.,.F.,.F.,(4,3,3,3,3,4),(2.71050543121376E-20,
1.81271519801731E-5,3.33528222530966E-5,4.35246196643646E-5,5.39830173117273E-5,
6.44389677343625E-5),.UNSPECIFIED.);
#26086=B_SPLINE_CURVE_WITH_KNOTS('',3,(#418237,#418238,#418239,#418240,
#418241,#418242,#418243,#418244,#418245,#418246,#418247,#418248,#418249,
#418250,#418251,#418252),.UNSPECIFIED.,.F.,.F.,(4,3,3,3,3,4),(0.,6.54397980774373E-6,
1.78746088883289E-5,2.90961555784964E-5,4.25056718483934E-5,6.52023395140209E-5),
 .UNSPECIFIED.);
#26087=B_SPLINE_CURVE_WITH_KNOTS('',3,(#418255,#418256,#418257,#418258,
#418259,#418260,#418261,#418262,#418263,#418264,#418265,#418266,#418267,
#418268,#418269,#418270),.UNSPECIFIED.,.F.,.F.,(4,3,3,3,3,4),(0.,1.81271519801731E-5,
3.33528222530966E-5,4.35246196643646E-5,5.39830173117274E-5,6.44389677343629E-5),
 .UNSPECIFIED.);
#26088=B_SPLINE_CURVE_WITH_KNOTS('',3,(#418277,#418278,#418279,#418280,
#418281,#418282,#418283,#418284,#418285,#418286,#418287,#418288,#418289,
#418290,#418291,#418292),.UNSPECIFIED.,.F.,.F.,(4,3,3,3,3,4),(0.,6.54397980774374E-6,
1.78746088883289E-5,2.90961555784964E-5,4.25056718483934E-5,6.52023395140209E-5),
 .UNSPECIFIED.);
#26089=B_SPLINE_CURVE_WITH_KNOTS('',3,(#418294,#418295,#418296,#418297,
#418298,#418299,#418300,#418301,#418302,#418303,#418304,#418305,#418306,
#418307,#418308,#418309),.UNSPECIFIED.,.F.,.F.,(4,3,3,3,3,4),(5.42101086242752E-20,
1.81271519801731E-5,3.33528222530966E-5,4.35246196643646E-5,5.39830173117273E-5,
6.44389677343625E-5),.UNSPECIFIED.);
#26090=B_SPLINE_CURVE_WITH_KNOTS('',3,(#418316,#418317,#418318,#418319,
#418320,#418321,#418322,#418323,#418324,#418325,#418326,#418327,#418328,
#418329,#418330,#418331),.UNSPECIFIED.,.F.,.F.,(4,3,3,3,3,4),(0.,6.54397980774378E-6,
1.78746088883288E-5,2.90961555784963E-5,4.25056718483934E-5,6.52023395140208E-5),
 .UNSPECIFIED.);
#26091=B_SPLINE_CURVE_WITH_KNOTS('',3,(#418333,#418334,#418335,#418336,
#418337,#418338,#418339,#418340,#418341,#418342,#418343,#418344,#418345,
#418346,#418347,#418348),.UNSPECIFIED.,.F.,.F.,(4,3,3,3,3,4),(0.,1.81271519801731E-5,
3.33528222530966E-5,4.35246196643645E-5,5.39830173117272E-5,6.44389677343625E-5),
 .UNSPECIFIED.);
#26092=B_SPLINE_CURVE_WITH_KNOTS('',3,(#418355,#418356,#418357,#418358,
#418359,#418360,#418361,#418362,#418363,#418364,#418365,#418366,#418367,
#418368,#418369,#418370),.UNSPECIFIED.,.F.,.F.,(4,3,3,3,3,4),(0.,6.54397980774369E-6,
1.78746088883288E-5,2.90961555784963E-5,4.25056718483934E-5,6.52023395140209E-5),
 .UNSPECIFIED.);
#26093=B_SPLINE_CURVE_WITH_KNOTS('',3,(#418372,#418373,#418374,#418375,
#418376,#418377,#418378,#418379,#418380,#418381,#418382,#418383,#418384,
#418385,#418386,#418387),.UNSPECIFIED.,.F.,.F.,(4,3,3,3,3,4),(0.,1.81271519801732E-5,
3.33528222530966E-5,4.35246196643647E-5,5.39830173117272E-5,6.44389677343626E-5),
 .UNSPECIFIED.);
#26094=B_SPLINE_CURVE_WITH_KNOTS('',3,(#418394,#418395,#418396,#418397,
#418398,#418399,#418400,#418401,#418402,#418403,#418404,#418405,#418406,
#418407,#418408,#418409),.UNSPECIFIED.,.F.,.F.,(4,3,3,3,3,4),(0.,6.5439798077436E-6,
1.78746088883288E-5,2.90961555784963E-5,4.25056718483933E-5,6.52023395140209E-5),
 .UNSPECIFIED.);
#26095=B_SPLINE_CURVE_WITH_KNOTS('',3,(#418411,#418412,#418413,#418414,
#418415,#418416,#418417,#418418,#418419,#418420,#418421,#418422,#418423,
#418424,#418425,#418426),.UNSPECIFIED.,.F.,.F.,(4,3,3,3,3,4),(0.,1.81271519801731E-5,
3.33528222530967E-5,4.35246196643647E-5,5.39830173117274E-5,6.4438967734363E-5),
 .UNSPECIFIED.);
#26096=B_SPLINE_CURVE_WITH_KNOTS('',3,(#418433,#418434,#418435,#418436,
#418437,#418438,#418439,#418440,#418441,#418442,#418443,#418444,#418445,
#418446,#418447,#418448),.UNSPECIFIED.,.F.,.F.,(4,3,3,3,3,4),(0.,6.54397980774359E-6,
1.78746088883289E-5,2.90961555784964E-5,4.25056718483934E-5,6.52023395140208E-5),
 .UNSPECIFIED.);
#26097=B_SPLINE_CURVE_WITH_KNOTS('',3,(#418450,#418451,#418452,#418453,
#418454,#418455,#418456,#418457,#418458,#418459,#418460,#418461,#418462,
#418463,#418464,#418465),.UNSPECIFIED.,.F.,.F.,(4,3,3,3,3,4),(0.,1.81271519801731E-5,
3.33528222530964E-5,4.35246196643645E-5,5.39830173117274E-5,6.44389677343629E-5),
 .UNSPECIFIED.);
#26098=B_SPLINE_CURVE_WITH_KNOTS('',3,(#418472,#418473,#418474,#418475,
#418476,#418477,#418478,#418479,#418480,#418481,#418482,#418483,#418484,
#418485,#418486,#418487),.UNSPECIFIED.,.F.,.F.,(4,3,3,3,3,4),(0.,6.54397980774364E-6,
1.7874608888329E-5,2.90961555784965E-5,4.25056718483936E-5,6.52023395140211E-5),
 .UNSPECIFIED.);
#26099=B_SPLINE_CURVE_WITH_KNOTS('',3,(#418489,#418490,#418491,#418492,
#418493,#418494,#418495,#418496,#418497,#418498,#418499,#418500,#418501,
#418502,#418503,#418504),.UNSPECIFIED.,.F.,.F.,(4,3,3,3,3,4),(0.,1.81271519801731E-5,
3.33528222530965E-5,4.35246196643648E-5,5.39830173117276E-5,6.44389677343631E-5),
 .UNSPECIFIED.);
#26100=B_SPLINE_CURVE_WITH_KNOTS('',3,(#418511,#418512,#418513,#418514,
#418515,#418516,#418517,#418518,#418519,#418520,#418521,#418522,#418523,
#418524,#418525,#418526),.UNSPECIFIED.,.F.,.F.,(4,3,3,3,3,4),(0.,6.5439798077437E-6,
1.78746088883287E-5,2.90961555784963E-5,4.25056718483934E-5,6.52023395140209E-5),
 .UNSPECIFIED.);
#26101=B_SPLINE_CURVE_WITH_KNOTS('',3,(#418528,#418529,#418530,#418531,
#418532,#418533,#418534,#418535,#418536,#418537,#418538,#418539,#418540,
#418541,#418542,#418543),.UNSPECIFIED.,.F.,.F.,(4,3,3,3,3,4),(0.,1.81271519801732E-5,
3.33528222530966E-5,4.35246196643647E-5,5.39830173117273E-5,6.44389677343626E-5),
 .UNSPECIFIED.);
#26102=B_SPLINE_CURVE_WITH_KNOTS('',3,(#418550,#418551,#418552,#418553,
#418554,#418555,#418556,#418557,#418558,#418559,#418560,#418561,#418562,
#418563,#418564,#418565),.UNSPECIFIED.,.F.,.F.,(4,3,3,3,3,4),(0.,6.54397980774401E-6,
1.78746088883291E-5,2.90961555784967E-5,4.25056718483938E-5,6.52023395140214E-5),
 .UNSPECIFIED.);
#26103=B_SPLINE_CURVE_WITH_KNOTS('',3,(#418567,#418568,#418569,#418570,
#418571,#418572,#418573,#418574,#418575,#418576,#418577,#418578,#418579,
#418580,#418581,#418582),.UNSPECIFIED.,.F.,.F.,(4,3,3,3,3,4),(0.,1.81271519801731E-5,
3.33528222530967E-5,4.35246196643648E-5,5.39830173117277E-5,6.44389677343627E-5),
 .UNSPECIFIED.);
#26104=B_SPLINE_CURVE_WITH_KNOTS('',3,(#418589,#418590,#418591,#418592,
#418593,#418594,#418595,#418596,#418597,#418598,#418599,#418600,#418601,
#418602,#418603,#418604),.UNSPECIFIED.,.F.,.F.,(4,3,3,3,3,4),(0.,6.54397980774356E-6,
1.7874608888329E-5,2.90961555784964E-5,4.25056718483936E-5,6.52023395140211E-5),
 .UNSPECIFIED.);
#26105=B_SPLINE_CURVE_WITH_KNOTS('',3,(#418606,#418607,#418608,#418609,
#418610,#418611,#418612,#418613,#418614,#418615,#418616,#418617,#418618,
#418619,#418620,#418621),.UNSPECIFIED.,.F.,.F.,(4,3,3,3,3,4),(0.,1.8127151980173E-5,
3.33528222530964E-5,4.35246196643645E-5,5.3983017311727E-5,6.44389677343624E-5),
 .UNSPECIFIED.);
#26106=B_SPLINE_CURVE_WITH_KNOTS('',3,(#418628,#418629,#418630,#418631,
#418632,#418633,#418634,#418635,#418636,#418637,#418638,#418639,#418640,
#418641,#418642,#418643),.UNSPECIFIED.,.F.,.F.,(4,3,3,3,3,4),(0.,6.54397980774394E-6,
1.78746088883292E-5,2.90961555784967E-5,4.25056718483935E-5,6.52023395140211E-5),
 .UNSPECIFIED.);
#26107=B_SPLINE_CURVE_WITH_KNOTS('',3,(#418645,#418646,#418647,#418648,
#418649,#418650,#418651,#418652,#418653,#418654,#418655,#418656,#418657,
#418658,#418659,#418660),.UNSPECIFIED.,.F.,.F.,(4,3,3,3,3,4),(0.,1.81271519801731E-5,
3.33528222530967E-5,4.35246196643646E-5,5.39830173117274E-5,6.44389677343627E-5),
 .UNSPECIFIED.);
#26108=B_SPLINE_CURVE_WITH_KNOTS('',3,(#418667,#418668,#418669,#418670,
#418671,#418672,#418673,#418674,#418675,#418676,#418677,#418678,#418679,
#418680,#418681,#418682),.UNSPECIFIED.,.F.,.F.,(4,3,3,3,3,4),(0.,6.54397980774397E-6,
1.78746088883291E-5,2.90961555784962E-5,4.25056718483934E-5,6.52023395140212E-5),
 .UNSPECIFIED.);
#26109=B_SPLINE_CURVE_WITH_KNOTS('',3,(#418684,#418685,#418686,#418687,
#418688,#418689,#418690,#418691,#418692,#418693,#418694,#418695,#418696,
#418697,#418698,#418699),.UNSPECIFIED.,.F.,.F.,(4,3,3,3,3,4),(0.,1.81271519801731E-5,
3.33528222530966E-5,4.35246196643644E-5,5.39830173117273E-5,6.44389677343626E-5),
 .UNSPECIFIED.);
#26110=B_SPLINE_CURVE_WITH_KNOTS('',3,(#418706,#418707,#418708,#418709,
#418710,#418711,#418712,#418713,#418714,#418715,#418716,#418717,#418718,
#418719,#418720,#418721),.UNSPECIFIED.,.F.,.F.,(4,3,3,3,3,4),(0.,6.54397980774329E-6,
1.78746088883288E-5,2.90961555784961E-5,4.25056718483933E-5,6.52023395140208E-5),
 .UNSPECIFIED.);
#26111=B_SPLINE_CURVE_WITH_KNOTS('',3,(#418723,#418724,#418725,#418726,
#418727,#418728,#418729,#418730,#418731,#418732,#418733,#418734,#418735,
#418736,#418737,#418738),.UNSPECIFIED.,.F.,.F.,(4,3,3,3,3,4),(0.,1.81271519801731E-5,
3.33528222530966E-5,4.35246196643647E-5,5.39830173117277E-5,6.44389677343631E-5),
 .UNSPECIFIED.);
#26112=B_SPLINE_CURVE_WITH_KNOTS('',3,(#418745,#418746,#418747,#418748,
#418749,#418750,#418751,#418752,#418753,#418754,#418755,#418756,#418757,
#418758,#418759,#418760),.UNSPECIFIED.,.F.,.F.,(4,3,3,3,3,4),(0.,6.54397980774385E-6,
1.78746088883287E-5,2.90961555784962E-5,4.25056718483931E-5,6.52023395140203E-5),
 .UNSPECIFIED.);
#26113=B_SPLINE_CURVE_WITH_KNOTS('',3,(#418762,#418763,#418764,#418765,
#418766,#418767,#418768,#418769,#418770,#418771,#418772,#418773,#418774,
#418775,#418776,#418777),.UNSPECIFIED.,.F.,.F.,(4,3,3,3,3,4),(0.,1.81271519801732E-5,
3.33528222530966E-5,4.35246196643644E-5,5.39830173117271E-5,6.44389677343623E-5),
 .UNSPECIFIED.);
#26114=B_SPLINE_CURVE_WITH_KNOTS('',3,(#418784,#418785,#418786,#418787,
#418788,#418789,#418790,#418791,#418792,#418793,#418794,#418795,#418796,
#418797,#418798,#418799),.UNSPECIFIED.,.F.,.F.,(4,3,3,3,3,4),(0.,6.54397980774368E-6,
1.78746088883288E-5,2.90961555784964E-5,4.25056718483934E-5,6.5202339514021E-5),
 .UNSPECIFIED.);
#26115=B_SPLINE_CURVE_WITH_KNOTS('',3,(#418801,#418802,#418803,#418804,
#418805,#418806,#418807,#418808,#418809,#418810,#418811,#418812,#418813,
#418814,#418815,#418816),.UNSPECIFIED.,.F.,.F.,(4,3,3,3,3,4),(0.,1.81271519801731E-5,
3.33528222530967E-5,4.35246196643647E-5,5.39830173117274E-5,6.44389677343628E-5),
 .UNSPECIFIED.);
#26116=B_SPLINE_CURVE_WITH_KNOTS('',3,(#418823,#418824,#418825,#418826,
#418827,#418828,#418829,#418830,#418831,#418832,#418833,#418834,#418835,
#418836,#418837,#418838),.UNSPECIFIED.,.F.,.F.,(4,3,3,3,3,4),(0.,6.54397980774364E-6,
1.78746088883288E-5,2.90961555784963E-5,4.25056718483933E-5,6.52023395140208E-5),
 .UNSPECIFIED.);
#26117=B_SPLINE_CURVE_WITH_KNOTS('',3,(#418840,#418841,#418842,#418843,
#418844,#418845,#418846,#418847,#418848,#418849,#418850,#418851,#418852,
#418853,#418854,#418855),.UNSPECIFIED.,.F.,.F.,(4,3,3,3,3,4),(0.,1.8127151980173E-5,
3.33528222530965E-5,4.35246196643644E-5,5.39830173117271E-5,6.44389677343624E-5),
 .UNSPECIFIED.);
#26118=B_SPLINE_CURVE_WITH_KNOTS('',3,(#418862,#418863,#418864,#418865,
#418866,#418867,#418868,#418869,#418870,#418871,#418872,#418873,#418874,
#418875,#418876,#418877),.UNSPECIFIED.,.F.,.F.,(4,3,3,3,3,4),(0.,6.54397980774372E-6,
1.78746088883289E-5,2.90961555784963E-5,4.25056718483934E-5,6.52023395140209E-5),
 .UNSPECIFIED.);
#26119=B_SPLINE_CURVE_WITH_KNOTS('',3,(#418879,#418880,#418881,#418882,
#418883,#418884,#418885,#418886,#418887,#418888,#418889,#418890,#418891,
#418892,#418893,#418894),.UNSPECIFIED.,.F.,.F.,(4,3,3,3,3,4),(0.,1.81271519801731E-5,
3.33528222530967E-5,4.35246196643646E-5,5.39830173117274E-5,6.44389677343626E-5),
 .UNSPECIFIED.);
#26120=B_SPLINE_CURVE_WITH_KNOTS('',3,(#418901,#418902,#418903,#418904,
#418905,#418906,#418907,#418908,#418909,#418910,#418911,#418912,#418913,
#418914,#418915,#418916),.UNSPECIFIED.,.F.,.F.,(4,3,3,3,3,4),(0.,6.54397980774376E-6,
1.78746088883289E-5,2.90961555784963E-5,4.25056718483934E-5,6.52023395140209E-5),
 .UNSPECIFIED.);
#26121=B_SPLINE_CURVE_WITH_KNOTS('',3,(#418918,#418919,#418920,#418921,
#418922,#418923,#418924,#418925,#418926,#418927,#418928,#418929,#418930,
#418931,#418932,#418933),.UNSPECIFIED.,.F.,.F.,(4,3,3,3,3,4),(5.42101086242752E-20,
1.81271519801732E-5,3.33528222530966E-5,4.35246196643646E-5,5.39830173117274E-5,
6.44389677343629E-5),.UNSPECIFIED.);
#26122=B_SPLINE_CURVE_WITH_KNOTS('',3,(#418940,#418941,#418942,#418943,
#418944,#418945,#418946,#418947,#418948,#418949,#418950,#418951,#418952,
#418953,#418954,#418955),.UNSPECIFIED.,.F.,.F.,(4,3,3,3,3,4),(0.,6.54397980774381E-6,
1.78746088883288E-5,2.90961555784963E-5,4.25056718483934E-5,6.52023395140208E-5),
 .UNSPECIFIED.);
#26123=B_SPLINE_CURVE_WITH_KNOTS('',3,(#418957,#418958,#418959,#418960,
#418961,#418962,#418963,#418964,#418965,#418966,#418967,#418968,#418969,
#418970,#418971,#418972),.UNSPECIFIED.,.F.,.F.,(4,3,3,3,3,4),(2.71050543121376E-20,
1.81271519801731E-5,3.33528222530966E-5,4.35246196643646E-5,5.39830173117273E-5,
6.44389677343626E-5),.UNSPECIFIED.);
#26124=B_SPLINE_CURVE_WITH_KNOTS('',3,(#418979,#418980,#418981,#418982,
#418983,#418984,#418985,#418986,#418987,#418988,#418989,#418990,#418991,
#418992,#418993,#418994),.UNSPECIFIED.,.F.,.F.,(4,3,3,3,3,4),(0.,6.54397980774374E-6,
1.78746088883289E-5,2.90961555784963E-5,4.25056718483934E-5,6.52023395140209E-5),
 .UNSPECIFIED.);
#26125=B_SPLINE_CURVE_WITH_KNOTS('',3,(#418996,#418997,#418998,#418999,
#419000,#419001,#419002,#419003,#419004,#419005,#419006,#419007,#419008,
#419009,#419010,#419011),.UNSPECIFIED.,.F.,.F.,(4,3,3,3,3,4),(3.04931861011548E-20,
1.81271519801731E-5,3.33528222530966E-5,4.35246196643646E-5,5.39830173117273E-5,
6.44389677343626E-5),.UNSPECIFIED.);
#26126=B_SPLINE_CURVE_WITH_KNOTS('',3,(#419018,#419019,#419020,#419021,
#419022,#419023,#419024,#419025,#419026,#419027,#419028,#419029,#419030,
#419031,#419032,#419033),.UNSPECIFIED.,.F.,.F.,(4,3,3,3,3,4),(0.,6.54397980774372E-6,
1.78746088883289E-5,2.90961555784964E-5,4.25056718483934E-5,6.52023395140209E-5),
 .UNSPECIFIED.);
#26127=B_SPLINE_CURVE_WITH_KNOTS('',3,(#419035,#419036,#419037,#419038,
#419039,#419040,#419041,#419042,#419043,#419044,#419045,#419046,#419047,
#419048,#419049,#419050),.UNSPECIFIED.,.F.,.F.,(4,3,3,3,3,4),(2.71050543121376E-20,
1.81271519801731E-5,3.33528222530966E-5,4.35246196643646E-5,5.39830173117274E-5,
6.44389677343626E-5),.UNSPECIFIED.);
#26128=B_SPLINE_CURVE_WITH_KNOTS('',3,(#419057,#419058,#419059,#419060,
#419061,#419062,#419063,#419064,#419065,#419066,#419067,#419068,#419069,
#419070,#419071,#419072),.UNSPECIFIED.,.F.,.F.,(4,3,3,3,3,4),(0.,6.5439798077437E-6,
1.78746088883288E-5,2.90961555784964E-5,4.25056718483934E-5,6.52023395140209E-5),
 .UNSPECIFIED.);
#26129=B_SPLINE_CURVE_WITH_KNOTS('',3,(#419074,#419075,#419076,#419077,
#419078,#419079,#419080,#419081,#419082,#419083,#419084,#419085,#419086,
#419087,#419088,#419089),.UNSPECIFIED.,.F.,.F.,(4,3,3,3,3,4),(5.42101086242752E-20,
1.81271519801731E-5,3.33528222530966E-5,4.35246196643646E-5,5.39830173117275E-5,
6.44389677343629E-5),.UNSPECIFIED.);
#26130=B_SPLINE_CURVE_WITH_KNOTS('',3,(#419096,#419097,#419098,#419099,
#419100,#419101,#419102,#419103,#419104,#419105,#419106,#419107,#419108,
#419109,#419110,#419111),.UNSPECIFIED.,.F.,.F.,(4,3,3,3,3,4),(0.,6.54397980774373E-6,
1.78746088883289E-5,2.90961555784964E-5,4.25056718483935E-5,6.52023395140211E-5),
 .UNSPECIFIED.);
#26131=B_SPLINE_CURVE_WITH_KNOTS('',3,(#419113,#419114,#419115,#419116,
#419117,#419118,#419119,#419120,#419121,#419122,#419123,#419124,#419125,
#419126,#419127,#419128),.UNSPECIFIED.,.F.,.F.,(4,3,3,3,3,4),(0.,1.81271519801731E-5,
3.33528222530966E-5,4.35246196643647E-5,5.39830173117275E-5,6.44389677343629E-5),
 .UNSPECIFIED.);
#26132=B_SPLINE_CURVE_WITH_KNOTS('',3,(#419135,#419136,#419137,#419138,
#419139,#419140,#419141,#419142,#419143,#419144,#419145,#419146,#419147,
#419148,#419149,#419150),.UNSPECIFIED.,.F.,.F.,(4,3,3,3,3,4),(0.,6.54397980774369E-6,
1.78746088883289E-5,2.90961555784963E-5,4.25056718483934E-5,6.52023395140208E-5),
 .UNSPECIFIED.);
#26133=B_SPLINE_CURVE_WITH_KNOTS('',3,(#419152,#419153,#419154,#419155,
#419156,#419157,#419158,#419159,#419160,#419161,#419162,#419163,#419164,
#419165,#419166,#419167),.UNSPECIFIED.,.F.,.F.,(4,3,3,3,3,4),(0.,1.81271519801732E-5,
3.33528222530967E-5,4.35246196643647E-5,5.39830173117272E-5,6.44389677343624E-5),
 .UNSPECIFIED.);
#26134=B_SPLINE_CURVE_WITH_KNOTS('',3,(#419174,#419175,#419176,#419177,
#419178,#419179,#419180,#419181,#419182,#419183,#419184,#419185,#419186,
#419187,#419188,#419189),.UNSPECIFIED.,.F.,.F.,(4,3,3,3,3,4),(0.,6.54397980774364E-6,
1.78746088883289E-5,2.90961555784963E-5,4.25056718483934E-5,6.52023395140209E-5),
 .UNSPECIFIED.);
#26135=B_SPLINE_CURVE_WITH_KNOTS('',3,(#419191,#419192,#419193,#419194,
#419195,#419196,#419197,#419198,#419199,#419200,#419201,#419202,#419203,
#419204,#419205,#419206),.UNSPECIFIED.,.F.,.F.,(4,3,3,3,3,4),(0.,1.81271519801732E-5,
3.33528222530968E-5,4.35246196643649E-5,5.39830173117278E-5,6.4438967734363E-5),
 .UNSPECIFIED.);
#26136=B_SPLINE_CURVE_WITH_KNOTS('',3,(#419213,#419214,#419215,#419216,
#419217,#419218,#419219,#419220,#419221,#419222,#419223,#419224,#419225,
#419226,#419227,#419228),.UNSPECIFIED.,.F.,.F.,(4,3,3,3,3,4),(0.,6.54397980774374E-6,
1.78746088883289E-5,2.90961555784962E-5,4.25056718483933E-5,6.52023395140208E-5),
 .UNSPECIFIED.);
#26137=B_SPLINE_CURVE_WITH_KNOTS('',3,(#419230,#419231,#419232,#419233,
#419234,#419235,#419236,#419237,#419238,#419239,#419240,#419241,#419242,
#419243,#419244,#419245),.UNSPECIFIED.,.F.,.F.,(4,3,3,3,3,4),(0.,1.81271519801732E-5,
3.33528222530967E-5,4.35246196643645E-5,5.39830173117275E-5,6.4438967734363E-5),
 .UNSPECIFIED.);
#26138=B_SPLINE_CURVE_WITH_KNOTS('',3,(#419252,#419253,#419254,#419255,
#419256,#419257,#419258,#419259,#419260,#419261,#419262,#419263,#419264,
#419265,#419266,#419267),.UNSPECIFIED.,.F.,.F.,(4,3,3,3,3,4),(0.,6.54397980774345E-6,
1.78746088883287E-5,2.90961555784962E-5,4.25056718483933E-5,6.52023395140207E-5),
 .UNSPECIFIED.);
#26139=B_SPLINE_CURVE_WITH_KNOTS('',3,(#419269,#419270,#419271,#419272,
#419273,#419274,#419275,#419276,#419277,#419278,#419279,#419280,#419281,
#419282,#419283,#419284),.UNSPECIFIED.,.F.,.F.,(4,3,3,3,3,4),(0.,1.81271519801731E-5,
3.33528222530967E-5,4.35246196643646E-5,5.39830173117276E-5,6.44389677343627E-5),
 .UNSPECIFIED.);
#26140=B_SPLINE_CURVE_WITH_KNOTS('',3,(#419291,#419292,#419293,#419294,
#419295,#419296,#419297,#419298,#419299,#419300,#419301,#419302,#419303,
#419304,#419305,#419306),.UNSPECIFIED.,.F.,.F.,(4,3,3,3,3,4),(0.,6.5439798077436E-6,
1.78746088883289E-5,2.90961555784961E-5,4.25056718483932E-5,6.52023395140208E-5),
 .UNSPECIFIED.);
#26141=B_SPLINE_CURVE_WITH_KNOTS('',3,(#419308,#419309,#419310,#419311,
#419312,#419313,#419314,#419315,#419316,#419317,#419318,#419319,#419320,
#419321,#419322,#419323),.UNSPECIFIED.,.F.,.F.,(4,3,3,3,3,4),(0.,1.81271519801732E-5,
3.33528222530966E-5,4.35246196643646E-5,5.39830173117277E-5,6.44389677343631E-5),
 .UNSPECIFIED.);
#26142=B_SPLINE_CURVE_WITH_KNOTS('',3,(#419330,#419331,#419332,#419333,
#419334,#419335,#419336,#419337,#419338,#419339,#419340,#419341,#419342,
#419343,#419344,#419345),.UNSPECIFIED.,.F.,.F.,(4,3,3,3,3,4),(0.,6.54397980774355E-6,
1.78746088883288E-5,2.90961555784961E-5,4.25056718483933E-5,6.52023395140206E-5),
 .UNSPECIFIED.);
#26143=B_SPLINE_CURVE_WITH_KNOTS('',3,(#419347,#419348,#419349,#419350,
#419351,#419352,#419353,#419354,#419355,#419356,#419357,#419358,#419359,
#419360,#419361,#419362),.UNSPECIFIED.,.F.,.F.,(4,3,3,3,3,4),(0.,1.81271519801731E-5,
3.33528222530965E-5,4.35246196643647E-5,5.39830173117274E-5,6.44389677343627E-5),
 .UNSPECIFIED.);
#26144=B_SPLINE_CURVE_WITH_KNOTS('',3,(#419369,#419370,#419371,#419372,
#419373,#419374,#419375,#419376,#419377,#419378,#419379,#419380,#419381,
#419382,#419383,#419384),.UNSPECIFIED.,.F.,.F.,(4,3,3,3,3,4),(0.,6.54397980774366E-6,
1.78746088883287E-5,2.90961555784963E-5,4.25056718483933E-5,6.52023395140209E-5),
 .UNSPECIFIED.);
#26145=B_SPLINE_CURVE_WITH_KNOTS('',3,(#419386,#419387,#419388,#419389,
#419390,#419391,#419392,#419393,#419394,#419395,#419396,#419397,#419398,
#419399,#419400,#419401),.UNSPECIFIED.,.F.,.F.,(4,3,3,3,3,4),(0.,1.81271519801732E-5,
3.33528222530969E-5,4.3524619664365E-5,5.39830173117279E-5,6.44389677343629E-5),
 .UNSPECIFIED.);
#26146=B_SPLINE_CURVE_WITH_KNOTS('',3,(#419408,#419409,#419410,#419411,
#419412,#419413,#419414,#419415,#419416,#419417,#419418,#419419,#419420,
#419421,#419422,#419423),.UNSPECIFIED.,.F.,.F.,(4,3,3,3,3,4),(0.,6.54397980774377E-6,
1.78746088883288E-5,2.90961555784961E-5,4.25056718483931E-5,6.52023395140207E-5),
 .UNSPECIFIED.);
#26147=B_SPLINE_CURVE_WITH_KNOTS('',3,(#419425,#419426,#419427,#419428,
#419429,#419430,#419431,#419432,#419433,#419434,#419435,#419436,#419437,
#419438,#419439,#419440),.UNSPECIFIED.,.F.,.F.,(4,3,3,3,3,4),(0.,1.81271519801731E-5,
3.33528222530965E-5,4.35246196643647E-5,5.39830173117273E-5,6.44389677343631E-5),
 .UNSPECIFIED.);
#26148=B_SPLINE_CURVE_WITH_KNOTS('',3,(#419447,#419448,#419449,#419450,
#419451,#419452,#419453,#419454,#419455,#419456,#419457,#419458,#419459,
#419460,#419461,#419462),.UNSPECIFIED.,.F.,.F.,(4,3,3,3,3,4),(0.,6.54397980774363E-6,
1.78746088883288E-5,2.90961555784963E-5,4.25056718483932E-5,6.52023395140206E-5),
 .UNSPECIFIED.);
#26149=B_SPLINE_CURVE_WITH_KNOTS('',3,(#419464,#419465,#419466,#419467,
#419468,#419469,#419470,#419471,#419472,#419473,#419474,#419475,#419476,
#419477,#419478,#419479),.UNSPECIFIED.,.F.,.F.,(4,3,3,3,3,4),(0.,1.81271519801732E-5,
3.33528222530967E-5,4.35246196643648E-5,5.39830173117274E-5,6.44389677343624E-5),
 .UNSPECIFIED.);
#26150=B_SPLINE_CURVE_WITH_KNOTS('',3,(#419486,#419487,#419488,#419489,
#419490,#419491,#419492,#419493,#419494,#419495,#419496,#419497,#419498,
#419499,#419500,#419501),.UNSPECIFIED.,.F.,.F.,(4,3,3,3,3,4),(0.,6.5439798077438E-6,
1.78746088883289E-5,2.90961555784965E-5,4.25056718483936E-5,6.52023395140211E-5),
 .UNSPECIFIED.);
#26151=B_SPLINE_CURVE_WITH_KNOTS('',3,(#419503,#419504,#419505,#419506,
#419507,#419508,#419509,#419510,#419511,#419512,#419513,#419514,#419515,
#419516,#419517,#419518),.UNSPECIFIED.,.F.,.F.,(4,3,3,3,3,4),(0.,1.81271519801732E-5,
3.33528222530968E-5,4.35246196643648E-5,5.39830173117278E-5,6.44389677343629E-5),
 .UNSPECIFIED.);
#26152=B_SPLINE_CURVE_WITH_KNOTS('',3,(#419525,#419526,#419527,#419528,
#419529,#419530,#419531,#419532,#419533,#419534,#419535,#419536,#419537,
#419538,#419539,#419540),.UNSPECIFIED.,.F.,.F.,(4,3,3,3,3,4),(0.,6.54397980774342E-6,
1.78746088883288E-5,2.90961555784962E-5,4.25056718483932E-5,6.52023395140207E-5),
 .UNSPECIFIED.);
#26153=B_SPLINE_CURVE_WITH_KNOTS('',3,(#419542,#419543,#419544,#419545,
#419546,#419547,#419548,#419549,#419550,#419551,#419552,#419553,#419554,
#419555,#419556,#419557),.UNSPECIFIED.,.F.,.F.,(4,3,3,3,3,4),(0.,1.81271519801731E-5,
3.33528222530964E-5,4.35246196643644E-5,5.39830173117272E-5,6.44389677343626E-5),
 .UNSPECIFIED.);
#26154=B_SPLINE_CURVE_WITH_KNOTS('',3,(#419564,#419565,#419566,#419567,
#419568,#419569,#419570,#419571,#419572,#419573,#419574,#419575,#419576,
#419577,#419578,#419579),.UNSPECIFIED.,.F.,.F.,(4,3,3,3,3,4),(0.,6.54397980774389E-6,
1.7874608888329E-5,2.90961555784964E-5,4.25056718483935E-5,6.5202339514021E-5),
 .UNSPECIFIED.);
#26155=B_SPLINE_CURVE_WITH_KNOTS('',3,(#419581,#419582,#419583,#419584,
#419585,#419586,#419587,#419588,#419589,#419590,#419591,#419592,#419593,
#419594,#419595,#419596),.UNSPECIFIED.,.F.,.F.,(4,3,3,3,3,4),(0.,1.81271519801731E-5,
3.33528222530965E-5,4.35246196643644E-5,5.39830173117275E-5,6.44389677343631E-5),
 .UNSPECIFIED.);
#26156=B_SPLINE_CURVE_WITH_KNOTS('',3,(#419603,#419604,#419605,#419606,
#419607,#419608,#419609,#419610,#419611,#419612,#419613,#419614,#419615,
#419616,#419617,#419618),.UNSPECIFIED.,.F.,.F.,(4,3,3,3,3,4),(0.,6.54397980774396E-6,
1.7874608888329E-5,2.90961555784966E-5,4.25056718483937E-5,6.52023395140212E-5),
 .UNSPECIFIED.);
#26157=B_SPLINE_CURVE_WITH_KNOTS('',3,(#419620,#419621,#419622,#419623,
#419624,#419625,#419626,#419627,#419628,#419629,#419630,#419631,#419632,
#419633,#419634,#419635),.UNSPECIFIED.,.F.,.F.,(4,3,3,3,3,4),(0.,1.81271519801731E-5,
3.33528222530966E-5,4.35246196643646E-5,5.39830173117271E-5,6.44389677343625E-5),
 .UNSPECIFIED.);
#26158=B_SPLINE_CURVE_WITH_KNOTS('',3,(#419642,#419643,#419644,#419645,
#419646,#419647,#419648,#419649,#419650,#419651,#419652,#419653,#419654,
#419655,#419656,#419657),.UNSPECIFIED.,.F.,.F.,(4,3,3,3,3,4),(0.,6.54397980774352E-6,
1.78746088883288E-5,2.90961555784962E-5,4.25056718483933E-5,6.52023395140208E-5),
 .UNSPECIFIED.);
#26159=B_SPLINE_CURVE_WITH_KNOTS('',3,(#419659,#419660,#419661,#419662,
#419663,#419664,#419665,#419666,#419667,#419668,#419669,#419670,#419671,
#419672,#419673,#419674),.UNSPECIFIED.,.F.,.F.,(4,3,3,3,3,4),(5.42101086242752E-20,
1.81271519801732E-5,3.33528222530967E-5,4.35246196643647E-5,5.39830173117276E-5,
6.4438967734363E-5),.UNSPECIFIED.);
#26160=B_SPLINE_CURVE_WITH_KNOTS('',3,(#419681,#419682,#419683,#419684,
#419685,#419686,#419687,#419688,#419689,#419690,#419691,#419692,#419693,
#419694,#419695,#419696),.UNSPECIFIED.,.F.,.F.,(4,3,3,3,3,4),(0.,6.54397980774381E-6,
1.7874608888329E-5,2.90961555784965E-5,4.25056718483935E-5,6.52023395140209E-5),
 .UNSPECIFIED.);
#26161=B_SPLINE_CURVE_WITH_KNOTS('',3,(#419698,#419699,#419700,#419701,
#419702,#419703,#419704,#419705,#419706,#419707,#419708,#419709,#419710,
#419711,#419712,#419713),.UNSPECIFIED.,.F.,.F.,(4,3,3,3,3,4),(5.42101086242752E-20,
1.81271519801731E-5,3.33528222530966E-5,4.35246196643646E-5,5.39830173117274E-5,
6.44389677343628E-5),.UNSPECIFIED.);
#26162=B_SPLINE_CURVE_WITH_KNOTS('',3,(#419720,#419721,#419722,#419723,
#419724,#419725,#419726,#419727,#419728,#419729,#419730,#419731,#419732,
#419733,#419734,#419735),.UNSPECIFIED.,.F.,.F.,(4,3,3,3,3,4),(0.,6.54397980774374E-6,
1.78746088883289E-5,2.90961555784964E-5,4.25056718483934E-5,6.52023395140209E-5),
 .UNSPECIFIED.);
#26163=B_SPLINE_CURVE_WITH_KNOTS('',3,(#419737,#419738,#419739,#419740,
#419741,#419742,#419743,#419744,#419745,#419746,#419747,#419748,#419749,
#419750,#419751,#419752),.UNSPECIFIED.,.F.,.F.,(4,3,3,3,3,4),(2.71050543121376E-20,
1.81271519801731E-5,3.33528222530966E-5,4.35246196643646E-5,5.39830173117275E-5,
6.44389677343629E-5),.UNSPECIFIED.);
#26164=B_SPLINE_CURVE_WITH_KNOTS('',3,(#419987,#419988,#419989,#419990,
#419991,#419992,#419993,#419994,#419995,#419996,#419997,#419998,#419999,
#420000,#420001,#420002,#420003,#420004,#420005,#420006,#420007,#420008,
#420009,#420010,#420011,#420012,#420013,#420014,#420015,#420016,#420017,
#420018,#420019,#420020,#420021,#420022,#420023),.UNSPECIFIED.,.F.,.F.,
(4,3,3,3,3,3,3,3,3,3,3,3,4),(0.,9.59031527198933E-6,1.94769411222704E-5,
2.02405092183152E-5,3.21374138577714E-5,3.60302195070439E-5,4.42640648818668E-5,
4.53660204229443E-5,5.03633762302166E-5,5.17708036292896E-5,5.37928993851989E-5,
5.541037554602E-5,5.64557889510063E-5),.UNSPECIFIED.);
#26165=B_SPLINE_CURVE_WITH_KNOTS('',3,(#420025,#420026,#420027,#420028,
#420029,#420030,#420031,#420032,#420033,#420034,#420035,#420036,#420037,
#420038,#420039,#420040,#420041,#420042,#420043,#420044,#420045,#420046,
#420047,#420048,#420049,#420050,#420051,#420052),.UNSPECIFIED.,.F.,.F.,
(4,3,3,3,3,3,3,3,3,4),(5.64557889510063E-5,5.98940966493751E-5,6.3421400387338E-5,
7.22241476085188E-5,7.38322796533364E-5,8.36529189331468E-5,8.80714278222499E-5,
9.84837568501108E-5,0.000108624704079211,0.000110823272382853),
 .UNSPECIFIED.);
#26166=B_SPLINE_CURVE_WITH_KNOTS('',3,(#420064,#420065,#420066,#420067),
 .UNSPECIFIED.,.F.,.F.,(4,4),(4.43935777737106E-19,7.70025630629237E-5),
 .UNSPECIFIED.);
#26167=B_SPLINE_CURVE_WITH_KNOTS('',3,(#420076,#420077,#420078,#420079),
 .UNSPECIFIED.,.F.,.F.,(4,4),(0.,7.7002563062924E-5),.UNSPECIFIED.);
#26168=B_SPLINE_CURVE_WITH_KNOTS('',3,(#422619,#422620,#422621,#422622,
#422623,#422624,#422625,#422626,#422627,#422628,#422629,#422630,#422631,
#422632,#422633,#422634,#422635,#422636,#422637,#422638,#422639,#422640,
#422641,#422642,#422643,#422644,#422645,#422646,#422647,#422648,#422649,
#422650,#422651,#422652),.UNSPECIFIED.,.F.,.F.,(4,3,3,3,3,3,3,3,3,3,3,4),
(0.,4.2915783730415E-6,5.42772623795336E-6,1.00901698482348E-5,1.31279195068639E-5,
1.57383542265889E-5,1.61011507492104E-5,1.67166789291755E-5,1.95343262811359E-5,
2.29377234674649E-5,2.71556047620058E-5,3.34407099942658E-5),
 .UNSPECIFIED.);
#26169=B_SPLINE_CURVE_WITH_KNOTS('',3,(#422654,#422655,#422656,#422657,
#422658,#422659,#422660),.UNSPECIFIED.,.F.,.F.,(4,3,4),(0.,4.40000041065376E-5,
9.89910850773113E-5),.UNSPECIFIED.);
#26170=B_SPLINE_CURVE_WITH_KNOTS('',3,(#422673,#422674,#422675,#422676,
#422677,#422678,#422679,#422680,#422681,#422682,#422683,#422684,#422685,
#422686,#422687,#422688,#422689,#422690,#422691,#422692,#422693,#422694,
#422695,#422696,#422697,#422698,#422699,#422700),.UNSPECIFIED.,.F.,.F.,
(4,3,3,3,3,3,3,3,3,4),(0.,8.6603962858312E-6,1.64707715200666E-5,2.24502894132279E-5,
2.49975961757824E-5,2.88526003690281E-5,3.10661348995016E-5,3.4305354351696E-5,
3.66410545653559E-5,4.00504537627887E-5),.UNSPECIFIED.);
#26171=B_SPLINE_CURVE_WITH_KNOTS('',3,(#422761,#422762,#422763,#422764,
#422765,#422766,#422767,#422768,#422769,#422770,#422771,#422772,#422773,
#422774,#422775,#422776,#422777,#422778,#422779,#422780,#422781,#422782,
#422783,#422784,#422785,#422786,#422787,#422788,#422789,#422790,#422791,
#422792,#422793,#422794),.UNSPECIFIED.,.F.,.F.,(4,3,3,3,3,3,3,3,3,3,3,4),
(8.80914265144472E-20,3.71309426656646E-6,5.39981071559417E-6,8.78933289332424E-6,
9.0027235706752E-6,1.07143984504149E-5,1.60780299679549E-5,1.65806081157686E-5,
2.30369726850657E-5,2.67819200416086E-5,3.59736924187689E-5,4.03862783807E-5),
 .UNSPECIFIED.);
#26172=B_SPLINE_CURVE_WITH_KNOTS('',3,(#422877,#422878,#422879,#422880),
 .UNSPECIFIED.,.F.,.F.,(4,4),(0.,7.7002563062924E-5),.UNSPECIFIED.);
#26173=B_SPLINE_CURVE_WITH_KNOTS('',3,(#422890,#422891,#422892,#422893),
 .UNSPECIFIED.,.F.,.F.,(4,4),(4.47028007668187E-19,7.70025630629238E-5),
 .UNSPECIFIED.);
#26174=B_SPLINE_CURVE_WITH_KNOTS('',3,(#422897,#422898,#422899,#422900,
#422901,#422902,#422903,#422904,#422905,#422906,#422907,#422908,#422909,
#422910,#422911,#422912,#422913,#422914,#422915,#422916,#422917,#422918,
#422919,#422920,#422921,#422922,#422923,#422924,#422925,#422926,#422927,
#422928,#422929,#422930,#422931,#422932,#422933),.UNSPECIFIED.,.F.,.F.,
(4,3,3,3,3,3,3,3,3,3,3,3,4),(0.,9.59031527200574E-6,1.94769411222917E-5,
2.02405092183154E-5,3.21374138577699E-5,3.6030219507044E-5,4.42640648818861E-5,
4.53660204229444E-5,5.03633762302092E-5,5.17708036292896E-5,5.37928993851989E-5,
5.541037554602E-5,5.64557889507966E-5),.UNSPECIFIED.);
#26175=B_SPLINE_CURVE_WITH_KNOTS('',3,(#422934,#422935,#422936,#422937,
#422938,#422939,#422940,#422941,#422942,#422943,#422944,#422945,#422946,
#422947,#422948,#422949,#422950,#422951,#422952,#422953,#422954,#422955,
#422956,#422957,#422958,#422959,#422960,#422961),.UNSPECIFIED.,.F.,.F.,
(4,3,3,3,3,3,3,3,3,4),(5.64557889507966E-5,5.98940966493751E-5,6.34214003873381E-5,
7.22241476085334E-5,7.38322796533363E-5,8.3652918933141E-5,8.80714278222501E-5,
9.8483756850102E-5,0.000108624704079186,0.000110823272382853),
 .UNSPECIFIED.);
#26176=B_SPLINE_CURVE_WITH_KNOTS('',3,(#422977,#422978,#422979,#422980,
#422981,#422982,#422983,#422984,#422985,#422986,#422987,#422988,#422989,
#422990,#422991,#422992,#422993,#422994,#422995,#422996,#422997,#422998,
#422999,#423000,#423001,#423002,#423003,#423004),.UNSPECIFIED.,.F.,.F.,
(4,3,3,3,3,3,3,3,3,4),(0.,8.6603962857854E-6,1.64707715200666E-5,2.24502894132548E-5,
2.49975961757822E-5,2.8852600369028E-5,3.10661348995016E-5,3.43053543516959E-5,
3.66410545653558E-5,4.00504537627886E-5),.UNSPECIFIED.);
#26177=B_SPLINE_CURVE_WITH_KNOTS('',3,(#423007,#423008,#423009,#423010,
#423011,#423012,#423013),.UNSPECIFIED.,.F.,.F.,(4,3,4),(0.,4.40000041065377E-5,
9.89910850773114E-5),.UNSPECIFIED.);
#26178=B_SPLINE_CURVE_WITH_KNOTS('',3,(#423034,#423035,#423036,#423037,
#423038,#423039,#423040,#423041,#423042,#423043,#423044,#423045,#423046,
#423047,#423048,#423049,#423050,#423051,#423052,#423053,#423054,#423055,
#423056,#423057,#423058,#423059,#423060,#423061,#423062,#423063,#423064,
#423065,#423066,#423067),.UNSPECIFIED.,.F.,.F.,(4,3,3,3,3,3,3,3,3,3,3,4),
(0.,4.29157837303072E-6,5.42772623795326E-6,1.00901698482348E-5,1.31279195068639E-5,
1.57383542265865E-5,1.61011507492105E-5,1.67166789291757E-5,1.9534326281136E-5,
2.29377234674651E-5,2.7155604762006E-5,3.34407099942659E-5),
 .UNSPECIFIED.);
#26179=B_SPLINE_CURVE_WITH_KNOTS('',3,(#423080,#423081,#423082,#423083,
#423084,#423085,#423086,#423087,#423088,#423089,#423090,#423091,#423092,
#423093,#423094,#423095,#423096,#423097,#423098,#423099,#423100,#423101,
#423102,#423103,#423104,#423105,#423106,#423107,#423108,#423109,#423110,
#423111,#423112,#423113),.UNSPECIFIED.,.F.,.F.,(4,3,3,3,3,3,3,3,3,3,3,4),
(5.42101086242752E-20,3.71309426656642E-6,5.39981071559419E-6,8.78933289366534E-6,
9.00272357067523E-6,1.0714398450415E-5,1.60780299679576E-5,1.65806081157688E-5,
2.30369726850415E-5,2.67819200416087E-5,3.59736924187938E-5,4.03862783807003E-5),
 .UNSPECIFIED.);
#26180=B_SPLINE_CURVE_WITH_KNOTS('',3,(#423226,#423227,#423228,#423229),
 .UNSPECIFIED.,.F.,.F.,(4,4),(0.,7.70025630629239E-5),.UNSPECIFIED.);
#26181=B_SPLINE_CURVE_WITH_KNOTS('',3,(#423239,#423240,#423241,#423242),
 .UNSPECIFIED.,.F.,.F.,(4,4),(4.41238316394827E-19,7.70025630629238E-5),
 .UNSPECIFIED.);
#26182=B_SPLINE_CURVE_WITH_KNOTS('',3,(#423246,#423247,#423248,#423249,
#423250,#423251,#423252,#423253,#423254,#423255,#423256,#423257,#423258,
#423259,#423260,#423261,#423262,#423263,#423264,#423265,#423266,#423267,
#423268,#423269,#423270,#423271,#423272,#423273,#423274,#423275,#423276,
#423277,#423278,#423279,#423280,#423281,#423282),.UNSPECIFIED.,.F.,.F.,
(4,3,3,3,3,3,3,3,3,3,3,3,4),(0.,9.59031527201346E-6,1.94769411223158E-5,
2.02405092183153E-5,3.21374138577746E-5,3.6030219507044E-5,4.42640648818315E-5,
4.53660204229444E-5,5.03633762302215E-5,5.17708036292896E-5,5.37928993851989E-5,
5.54103755460195E-5,5.64557889513096E-5),.UNSPECIFIED.);
#26183=B_SPLINE_CURVE_WITH_KNOTS('',3,(#423283,#423284,#423285,#423286,
#423287,#423288,#423289,#423290,#423291,#423292,#423293,#423294,#423295,
#423296,#423297,#423298,#423299,#423300,#423301,#423302,#423303,#423304,
#423305,#423306,#423307,#423308,#423309,#423310),.UNSPECIFIED.,.F.,.F.,
(4,3,3,3,3,3,3,3,3,4),(5.64557889513096E-5,5.98940966493751E-5,6.3421400387338E-5,
7.22241476084388E-5,7.38322796533364E-5,8.36529189331415E-5,8.807142782225E-5,
9.84837568500727E-5,0.000108624704079135,0.000110823272382853),
 .UNSPECIFIED.);
#26184=B_SPLINE_CURVE_WITH_KNOTS('',3,(#423326,#423327,#423328,#423329,
#423330,#423331,#423332,#423333,#423334,#423335,#423336,#423337,#423338,
#423339,#423340,#423341,#423342,#423343,#423344,#423345,#423346,#423347,
#423348,#423349,#423350,#423351,#423352,#423353),.UNSPECIFIED.,.F.,.F.,
(4,3,3,3,3,3,3,3,3,4),(0.,8.66039628581207E-6,1.64707715200665E-5,2.24502894132646E-5,
2.49975961757823E-5,2.8852600369028E-5,3.10661348995016E-5,3.43053543516961E-5,
3.66410545653561E-5,4.00504537627889E-5),.UNSPECIFIED.);
#26185=B_SPLINE_CURVE_WITH_KNOTS('',3,(#423356,#423357,#423358,#423359,
#423360,#423361,#423362),.UNSPECIFIED.,.F.,.F.,(4,3,4),(0.,4.40000041065374E-5,
9.89910850773114E-5),.UNSPECIFIED.);
#26186=B_SPLINE_CURVE_WITH_KNOTS('',3,(#423383,#423384,#423385,#423386,
#423387,#423388,#423389,#423390,#423391,#423392,#423393,#423394,#423395,
#423396,#423397,#423398,#423399,#423400,#423401,#423402,#423403,#423404,
#423405,#423406,#423407,#423408,#423409,#423410,#423411,#423412,#423413,
#423414,#423415,#423416),.UNSPECIFIED.,.F.,.F.,(4,3,3,3,3,3,3,3,3,3,3,4),
(0.,4.29157837302144E-6,5.4277262379533E-6,1.00901698482348E-5,1.3127919506864E-5,
1.57383542265789E-5,1.61011507492104E-5,1.67166789291755E-5,1.95343262811359E-5,
2.29377234674649E-5,2.71556047620059E-5,3.34407099942658E-5),
 .UNSPECIFIED.);
#26187=B_SPLINE_CURVE_WITH_KNOTS('',3,(#423429,#423430,#423431,#423432,
#423433,#423434,#423435,#423436,#423437,#423438,#423439,#423440,#423441,
#423442,#423443,#423444,#423445,#423446,#423447,#423448,#423449,#423450,
#423451,#423452,#423453,#423454,#423455,#423456,#423457,#423458,#423459,
#423460,#423461,#423462),.UNSPECIFIED.,.F.,.F.,(4,3,3,3,3,3,3,3,3,3,3,4),
(5.42101086242752E-20,3.71309426656648E-6,5.39981071559418E-6,8.78933289330926E-6,
9.0027235706753E-6,1.0714398450415E-5,1.60780299679585E-5,1.65806081157688E-5,
2.3036972685038E-5,2.67819200416088E-5,3.59736924188206E-5,4.03862783807005E-5),
 .UNSPECIFIED.);
#26188=B_SPLINE_CURVE_WITH_KNOTS('',3,(#423575,#423576,#423577,#423578),
 .UNSPECIFIED.,.F.,.F.,(4,4),(0.,7.70025630629239E-5),.UNSPECIFIED.);
#26189=B_SPLINE_CURVE_WITH_KNOTS('',3,(#423588,#423589,#423590,#423591),
 .UNSPECIFIED.,.F.,.F.,(4,4),(4.37055868292169E-19,7.70025630629239E-5),
 .UNSPECIFIED.);
#26190=B_SPLINE_CURVE_WITH_KNOTS('',3,(#423595,#423596,#423597,#423598,
#423599,#423600,#423601,#423602,#423603,#423604,#423605,#423606,#423607,
#423608,#423609,#423610,#423611,#423612,#423613,#423614,#423615,#423616,
#423617,#423618,#423619,#423620,#423621,#423622,#423623,#423624,#423625,
#423626,#423627,#423628,#423629,#423630,#423631),.UNSPECIFIED.,.F.,.F.,
(4,3,3,3,3,3,3,3,3,3,3,3,4),(0.,9.59031527200032E-6,1.94769411222912E-5,
2.02405092183152E-5,3.21374138577754E-5,3.60302195070438E-5,4.42640648818326E-5,
4.53660204229441E-5,5.03633762302261E-5,5.17708036292895E-5,5.37928993851988E-5,
5.54103755460196E-5,5.64557889505696E-5),.UNSPECIFIED.);
#26191=B_SPLINE_CURVE_WITH_KNOTS('',3,(#423632,#423633,#423634,#423635,
#423636,#423637,#423638,#423639,#423640,#423641,#423642,#423643,#423644,
#423645,#423646,#423647,#423648,#423649,#423650,#423651,#423652,#423653,
#423654,#423655,#423656,#423657,#423658,#423659),.UNSPECIFIED.,.F.,.F.,
(4,3,3,3,3,3,3,3,3,4),(5.64557889505696E-5,5.98940966493749E-5,6.34214003873378E-5,
7.22241476084911E-5,7.38322796533361E-5,8.3652918933132E-5,8.80714278222497E-5,
9.84837568500572E-5,0.000108624704079099,0.000110823272382853),
 .UNSPECIFIED.);
#26192=B_SPLINE_CURVE_WITH_KNOTS('',3,(#423675,#423676,#423677,#423678,
#423679,#423680,#423681,#423682,#423683,#423684,#423685,#423686,#423687,
#423688,#423689,#423690,#423691,#423692,#423693,#423694,#423695,#423696,
#423697,#423698,#423699,#423700,#423701,#423702),.UNSPECIFIED.,.F.,.F.,
(4,3,3,3,3,3,3,3,3,4),(0.,8.6603962858033E-6,1.64707715200666E-5,2.24502894132316E-5,
2.49975961757823E-5,2.8852600369028E-5,3.10661348995016E-5,3.43053543516961E-5,
3.6641054565356E-5,4.00504537627889E-5),.UNSPECIFIED.);
#26193=B_SPLINE_CURVE_WITH_KNOTS('',3,(#423705,#423706,#423707,#423708,
#423709,#423710,#423711),.UNSPECIFIED.,.F.,.F.,(4,3,4),(0.,4.40000041065376E-5,
9.89910850773116E-5),.UNSPECIFIED.);
#26194=B_SPLINE_CURVE_WITH_KNOTS('',3,(#423732,#423733,#423734,#423735,
#423736,#423737,#423738,#423739,#423740,#423741,#423742,#423743,#423744,
#423745,#423746,#423747,#423748,#423749,#423750,#423751,#423752,#423753,
#423754,#423755,#423756,#423757,#423758,#423759,#423760,#423761,#423762,
#423763,#423764,#423765),.UNSPECIFIED.,.F.,.F.,(4,3,3,3,3,3,3,3,3,3,3,4),
(0.,4.29157837303003E-6,5.42772623795338E-6,1.00901698482344E-5,1.31279195068639E-5,
1.57383542265823E-5,1.61011507492103E-5,1.67166789291752E-5,1.95343262811357E-5,
2.29377234674648E-5,2.71556047620056E-5,3.34407099942655E-5),
 .UNSPECIFIED.);
#26195=B_SPLINE_CURVE_WITH_KNOTS('',3,(#423778,#423779,#423780,#423781,
#423782,#423783,#423784,#423785,#423786,#423787,#423788,#423789,#423790,
#423791,#423792,#423793,#423794,#423795,#423796,#423797,#423798,#423799,
#423800,#423801,#423802,#423803,#423804,#423805,#423806,#423807,#423808,
#423809,#423810,#423811),.UNSPECIFIED.,.F.,.F.,(4,3,3,3,3,3,3,3,3,3,3,4),
(5.42101086242752E-20,3.71309426656649E-6,5.39981071559419E-6,8.78933289329362E-6,
9.00272357067532E-6,1.0714398450415E-5,1.60780299679622E-5,1.65806081157688E-5,
2.30369726850379E-5,2.67819200416089E-5,3.59736924187726E-5,4.03862783807006E-5),
 .UNSPECIFIED.);
#26196=B_SPLINE_CURVE_WITH_KNOTS('',3,(#423924,#423925,#423926,#423927),
 .UNSPECIFIED.,.F.,.F.,(4,4),(0.,7.70025630629241E-5),.UNSPECIFIED.);
#26197=B_SPLINE_CURVE_WITH_KNOTS('',3,(#423937,#423938,#423939,#423940),
 .UNSPECIFIED.,.F.,.F.,(4,4),(4.33680868994202E-19,7.70025630629239E-5),
 .UNSPECIFIED.);
#26198=B_SPLINE_CURVE_WITH_KNOTS('',3,(#423944,#423945,#423946,#423947,
#423948,#423949,#423950,#423951,#423952,#423953,#423954,#423955,#423956,
#423957,#423958,#423959,#423960,#423961,#423962,#423963,#423964,#423965,
#423966,#423967,#423968,#423969,#423970,#423971,#423972,#423973,#423974,
#423975,#423976,#423977,#423978,#423979,#423980),.UNSPECIFIED.,.F.,.F.,
(4,3,3,3,3,3,3,3,3,3,3,3,4),(0.,9.5903152720106E-6,1.94769411223126E-5,
2.02405092183153E-5,3.21374138577666E-5,3.60302195070438E-5,4.42640648818143E-5,
4.53660204229444E-5,5.0363376230216E-5,5.17708036292896E-5,5.37928993851988E-5,
5.54103755460201E-5,5.64557889507744E-5),.UNSPECIFIED.);
#26199=B_SPLINE_CURVE_WITH_KNOTS('',3,(#423981,#423982,#423983,#423984,
#423985,#423986,#423987,#423988,#423989,#423990,#423991,#423992,#423993,
#423994,#423995,#423996,#423997,#423998,#423999,#424000,#424001,#424002,
#424003,#424004,#424005,#424006,#424007,#424008),.UNSPECIFIED.,.F.,.F.,
(4,3,3,3,3,3,3,3,3,4),(5.64557889507744E-5,5.98940966493751E-5,6.34214003873379E-5,
7.22241476084577E-5,7.38322796533363E-5,8.36529189331507E-5,8.80714278222499E-5,
9.84837568500952E-5,0.000108624704079183,0.000110823272382853),
 .UNSPECIFIED.);
#26200=B_SPLINE_CURVE_WITH_KNOTS('',3,(#424024,#424025,#424026,#424027,
#424028,#424029,#424030,#424031,#424032,#424033,#424034,#424035,#424036,
#424037,#424038,#424039,#424040,#424041,#424042,#424043,#424044,#424045,
#424046,#424047,#424048,#424049,#424050,#424051),.UNSPECIFIED.,.F.,.F.,
(4,3,3,3,3,3,3,3,3,4),(0.,8.66039628581227E-6,1.64707715200666E-5,2.24502894132344E-5,
2.49975961757823E-5,2.8852600369028E-5,3.10661348995015E-5,3.4305354351696E-5,
3.66410545653559E-5,4.00504537627887E-5),.UNSPECIFIED.);
#26201=B_SPLINE_CURVE_WITH_KNOTS('',3,(#424054,#424055,#424056,#424057,
#424058,#424059,#424060),.UNSPECIFIED.,.F.,.F.,(4,3,4),(0.,4.40000041065374E-5,
9.8991085077311E-5),.UNSPECIFIED.);
#26202=B_SPLINE_CURVE_WITH_KNOTS('',3,(#424081,#424082,#424083,#424084,
#424085,#424086,#424087,#424088,#424089,#424090,#424091,#424092,#424093,
#424094,#424095,#424096,#424097,#424098,#424099,#424100,#424101,#424102,
#424103,#424104,#424105,#424106,#424107,#424108,#424109,#424110,#424111,
#424112,#424113,#424114),.UNSPECIFIED.,.F.,.F.,(4,3,3,3,3,3,3,3,3,3,3,4),
(0.,4.29157837303544E-6,5.42772623795348E-6,1.0090169848235E-5,1.31279195068642E-5,
1.5738354226584E-5,1.61011507492107E-5,1.67166789291759E-5,1.95343262811362E-5,
2.29377234674651E-5,2.71556047620061E-5,3.34407099942662E-5),
 .UNSPECIFIED.);
#26203=B_SPLINE_CURVE_WITH_KNOTS('',3,(#424127,#424128,#424129,#424130,
#424131,#424132,#424133,#424134,#424135,#424136,#424137,#424138,#424139,
#424140,#424141,#424142,#424143,#424144,#424145,#424146,#424147,#424148,
#424149,#424150,#424151,#424152,#424153,#424154,#424155,#424156,#424157,
#424158,#424159,#424160),.UNSPECIFIED.,.F.,.F.,(4,3,3,3,3,3,3,3,3,3,3,4),
(1.0842021724855E-19,3.71309426656642E-6,5.39981071559425E-6,8.78933289331666E-6,
9.00272357067523E-6,1.07143984504148E-5,1.60780299679651E-5,1.65806081157685E-5,
2.30369726850497E-5,2.67819200416083E-5,3.59736924187557E-5,4.03862783806994E-5),
 .UNSPECIFIED.);
#26204=B_SPLINE_CURVE_WITH_KNOTS('',3,(#424273,#424274,#424275,#424276),
 .UNSPECIFIED.,.F.,.F.,(4,4),(0.,7.70025630629238E-5),.UNSPECIFIED.);
#26205=B_SPLINE_CURVE_WITH_KNOTS('',3,(#424286,#424287,#424288,#424289),
 .UNSPECIFIED.,.F.,.F.,(4,4),(4.33680868994202E-19,7.70025630629238E-5),
 .UNSPECIFIED.);
#26206=B_SPLINE_CURVE_WITH_KNOTS('',3,(#424293,#424294,#424295,#424296,
#424297,#424298,#424299,#424300,#424301,#424302,#424303,#424304,#424305,
#424306,#424307,#424308,#424309,#424310,#424311,#424312,#424313,#424314,
#424315,#424316,#424317,#424318,#424319,#424320,#424321,#424322,#424323,
#424324,#424325,#424326,#424327,#424328,#424329),.UNSPECIFIED.,.F.,.F.,
(4,3,3,3,3,3,3,3,3,3,3,3,4),(0.,9.5903152719965E-6,1.94769411222866E-5,
2.02405092183151E-5,3.21374138577523E-5,3.60302195070439E-5,4.42640648818848E-5,
4.53660204229442E-5,5.03633762302146E-5,5.17708036292897E-5,5.3792899385199E-5,
5.54103755460205E-5,5.64557889509545E-5),.UNSPECIFIED.);
#26207=B_SPLINE_CURVE_WITH_KNOTS('',3,(#424330,#424331,#424332,#424333,
#424334,#424335,#424336,#424337,#424338,#424339,#424340,#424341,#424342,
#424343,#424344,#424345,#424346,#424347,#424348,#424349,#424350,#424351,
#424352,#424353,#424354,#424355,#424356,#424357),.UNSPECIFIED.,.F.,.F.,
(4,3,3,3,3,3,3,3,3,4),(5.64557889509545E-5,5.98940966493752E-5,6.34214003873382E-5,
7.22241476085202E-5,7.38322796533367E-5,8.36529189331274E-5,8.80714278222504E-5,
9.84837568500655E-5,0.000108624704079124,0.000110823272382854),
 .UNSPECIFIED.);
#26208=B_SPLINE_CURVE_WITH_KNOTS('',3,(#424373,#424374,#424375,#424376,
#424377,#424378,#424379,#424380,#424381,#424382,#424383,#424384,#424385,
#424386,#424387,#424388,#424389,#424390,#424391,#424392,#424393,#424394,
#424395,#424396,#424397,#424398,#424399,#424400),.UNSPECIFIED.,.F.,.F.,
(4,3,3,3,3,3,3,3,3,4),(0.,8.66039628584811E-6,1.64707715200668E-5,2.24502894132374E-5,
2.49975961757828E-5,2.88526003690285E-5,3.10661348995021E-5,3.43053543516967E-5,
3.66410545653568E-5,4.00504537627891E-5),.UNSPECIFIED.);
#26209=B_SPLINE_CURVE_WITH_KNOTS('',3,(#424403,#424404,#424405,#424406,
#424407,#424408,#424409),.UNSPECIFIED.,.F.,.F.,(4,3,4),(0.,4.40000041065375E-5,
9.89910850773109E-5),.UNSPECIFIED.);
#26210=B_SPLINE_CURVE_WITH_KNOTS('',3,(#424430,#424431,#424432,#424433,
#424434,#424435,#424436,#424437,#424438,#424439,#424440,#424441,#424442,
#424443,#424444,#424445,#424446,#424447,#424448,#424449,#424450,#424451,
#424452,#424453,#424454,#424455,#424456,#424457,#424458,#424459,#424460,
#424461,#424462,#424463),.UNSPECIFIED.,.F.,.F.,(4,3,3,3,3,3,3,3,3,3,3,4),
(0.,4.29157837303359E-6,5.42772623795353E-6,1.00901698482349E-5,1.31279195068641E-5,
1.57383542265853E-5,1.61011507492106E-5,1.67166789291759E-5,1.95343262811364E-5,
2.29377234674653E-5,2.71556047620062E-5,3.34407099942664E-5),
 .UNSPECIFIED.);
#26211=B_SPLINE_CURVE_WITH_KNOTS('',3,(#424476,#424477,#424478,#424479,
#424480,#424481,#424482,#424483,#424484,#424485,#424486,#424487,#424488,
#424489,#424490,#424491,#424492,#424493,#424494,#424495,#424496,#424497,
#424498,#424499,#424500,#424501,#424502,#424503,#424504,#424505,#424506,
#424507,#424508,#424509),.UNSPECIFIED.,.F.,.F.,(4,3,3,3,3,3,3,3,3,3,3,4),
(0.,3.71309426656636E-6,5.39981071559408E-6,8.78933289330066E-6,9.00272357067524E-6,
1.07143984504147E-5,1.60780299679589E-5,1.65806081157685E-5,2.30369726850456E-5,
2.67819200416083E-5,3.59736924187622E-5,4.03862783806998E-5),
 .UNSPECIFIED.);
#26212=B_SPLINE_CURVE_WITH_KNOTS('',3,(#424622,#424623,#424624,#424625),
 .UNSPECIFIED.,.F.,.F.,(4,4),(0.,7.70025630629239E-5),.UNSPECIFIED.);
#26213=B_SPLINE_CURVE_WITH_KNOTS('',3,(#424635,#424636,#424637,#424638),
 .UNSPECIFIED.,.F.,.F.,(4,4),(4.33680868994202E-19,7.70025630629237E-5),
 .UNSPECIFIED.);
#26214=B_SPLINE_CURVE_WITH_KNOTS('',3,(#424642,#424643,#424644,#424645,
#424646,#424647,#424648,#424649,#424650,#424651,#424652,#424653,#424654,
#424655,#424656,#424657,#424658,#424659,#424660,#424661,#424662,#424663,
#424664,#424665,#424666,#424667,#424668,#424669,#424670,#424671,#424672,
#424673,#424674,#424675,#424676,#424677,#424678),.UNSPECIFIED.,.F.,.F.,
(4,3,3,3,3,3,3,3,3,3,3,3,4),(0.,9.59031527199588E-6,1.94769411222848E-5,
2.02405092183153E-5,3.21374138577599E-5,3.60302195070438E-5,4.42640648819043E-5,
4.53660204229442E-5,5.03633762301906E-5,5.17708036292898E-5,5.37928993851988E-5,
5.54103755460198E-5,5.64557889507646E-5),.UNSPECIFIED.);
#26215=B_SPLINE_CURVE_WITH_KNOTS('',3,(#424679,#424680,#424681,#424682,
#424683,#424684,#424685,#424686,#424687,#424688,#424689,#424690,#424691,
#424692,#424693,#424694,#424695,#424696,#424697,#424698,#424699,#424700,
#424701,#424702,#424703,#424704,#424705,#424706),.UNSPECIFIED.,.F.,.F.,
(4,3,3,3,3,3,3,3,3,4),(5.64557889507646E-5,5.98940966493748E-5,6.3421400387338E-5,
7.22241476084039E-5,7.38322796533363E-5,8.36529189331441E-5,8.80714278222497E-5,
9.84837568500709E-5,0.000108624704079132,0.000110823272382853),
 .UNSPECIFIED.);
#26216=B_SPLINE_CURVE_WITH_KNOTS('',3,(#424722,#424723,#424724,#424725,
#424726,#424727,#424728,#424729,#424730,#424731,#424732,#424733,#424734,
#424735,#424736,#424737,#424738,#424739,#424740,#424741,#424742,#424743,
#424744,#424745,#424746,#424747,#424748,#424749),.UNSPECIFIED.,.F.,.F.,
(4,3,3,3,3,3,3,3,3,4),(0.,8.66039628583738E-6,1.6470771520067E-5,2.2450289413233E-5,
2.49975961757828E-5,2.88526003690285E-5,3.10661348995021E-5,3.43053543516966E-5,
3.66410545653567E-5,4.00504537627891E-5),.UNSPECIFIED.);
#26217=B_SPLINE_CURVE_WITH_KNOTS('',3,(#424752,#424753,#424754,#424755,
#424756,#424757,#424758),.UNSPECIFIED.,.F.,.F.,(4,3,4),(0.,4.40000041065374E-5,
9.89910850773109E-5),.UNSPECIFIED.);
#26218=B_SPLINE_CURVE_WITH_KNOTS('',3,(#424779,#424780,#424781,#424782,
#424783,#424784,#424785,#424786,#424787,#424788,#424789,#424790,#424791,
#424792,#424793,#424794,#424795,#424796,#424797,#424798,#424799,#424800,
#424801,#424802,#424803,#424804,#424805,#424806,#424807,#424808,#424809,
#424810,#424811,#424812),.UNSPECIFIED.,.F.,.F.,(4,3,3,3,3,3,3,3,3,3,3,4),
(0.,4.29157837302829E-6,5.42772623795352E-6,1.0090169848235E-5,1.31279195068643E-5,
1.57383542265904E-5,1.61011507492108E-5,1.67166789291759E-5,1.9534326281136E-5,
2.29377234674649E-5,2.71556047620058E-5,3.34407099942657E-5),
 .UNSPECIFIED.);
#26219=B_SPLINE_CURVE_WITH_KNOTS('',3,(#424825,#424826,#424827,#424828,
#424829,#424830,#424831,#424832,#424833,#424834,#424835,#424836,#424837,
#424838,#424839,#424840,#424841,#424842,#424843,#424844,#424845,#424846,
#424847,#424848,#424849,#424850,#424851,#424852,#424853,#424854,#424855,
#424856,#424857,#424858),.UNSPECIFIED.,.F.,.F.,(4,3,3,3,3,3,3,3,3,3,3,4),
(2.16840434497101E-19,3.71309426656633E-6,5.39981071559424E-6,8.78933289369172E-6,
9.00272357067502E-6,1.07143984504147E-5,1.6078029967956E-5,1.65806081157685E-5,
2.30369726850514E-5,2.67819200416083E-5,3.59736924187967E-5,4.03862783806995E-5),
 .UNSPECIFIED.);
#26220=B_SPLINE_CURVE_WITH_KNOTS('',3,(#424971,#424972,#424973,#424974),
 .UNSPECIFIED.,.F.,.F.,(4,4),(0.,7.70025630629238E-5),.UNSPECIFIED.);
#26221=B_SPLINE_CURVE_WITH_KNOTS('',3,(#424984,#424985,#424986,#424987),
 .UNSPECIFIED.,.F.,.F.,(4,4),(4.33680868994202E-19,7.70025630629236E-5),
 .UNSPECIFIED.);
#26222=B_SPLINE_CURVE_WITH_KNOTS('',3,(#424991,#424992,#424993,#424994,
#424995,#424996,#424997,#424998,#424999,#425000,#425001,#425002,#425003,
#425004,#425005,#425006,#425007,#425008,#425009,#425010,#425011,#425012,
#425013,#425014,#425015,#425016,#425017,#425018,#425019,#425020,#425021,
#425022,#425023,#425024,#425025,#425026,#425027),.UNSPECIFIED.,.F.,.F.,
(4,3,3,3,3,3,3,3,3,3,3,3,4),(0.,9.59031527196868E-6,1.94769411222495E-5,
2.02405092183152E-5,3.21374138577699E-5,3.60302195070441E-5,4.42640648818247E-5,
4.53660204229442E-5,5.03633762302055E-5,5.17708036292895E-5,5.37928993851988E-5,
5.54103755460197E-5,5.64557889510261E-5),.UNSPECIFIED.);
#26223=B_SPLINE_CURVE_WITH_KNOTS('',3,(#425028,#425029,#425030,#425031,
#425032,#425033,#425034,#425035,#425036,#425037,#425038,#425039,#425040,
#425041,#425042,#425043,#425044,#425045,#425046,#425047,#425048,#425049,
#425050,#425051,#425052,#425053,#425054,#425055),.UNSPECIFIED.,.F.,.F.,
(4,3,3,3,3,3,3,3,3,4),(5.64557889510261E-5,5.98940966493748E-5,6.34214003873378E-5,
7.22241476084834E-5,7.38322796533361E-5,8.36529189331444E-5,8.80714278222496E-5,
9.84837568500701E-5,0.000108624704079139,0.000110823272382853),
 .UNSPECIFIED.);
#26224=B_SPLINE_CURVE_WITH_KNOTS('',3,(#425071,#425072,#425073,#425074,
#425075,#425076,#425077,#425078,#425079,#425080,#425081,#425082,#425083,
#425084,#425085,#425086,#425087,#425088,#425089,#425090,#425091,#425092,
#425093,#425094,#425095,#425096,#425097,#425098),.UNSPECIFIED.,.F.,.F.,
(4,3,3,3,3,3,3,3,3,4),(0.,8.66039628582221E-6,1.64707715200666E-5,2.24502894132205E-5,
2.49975961757824E-5,2.88526003690279E-5,3.10661348995017E-5,3.43053543516962E-5,
3.66410545653564E-5,4.00504537627889E-5),.UNSPECIFIED.);
#26225=B_SPLINE_CURVE_WITH_KNOTS('',3,(#425101,#425102,#425103,#425104,
#425105,#425106,#425107),.UNSPECIFIED.,.F.,.F.,(4,3,4),(0.,4.40000041065378E-5,
9.89910850773116E-5),.UNSPECIFIED.);
#26226=B_SPLINE_CURVE_WITH_KNOTS('',3,(#425128,#425129,#425130,#425131,
#425132,#425133,#425134,#425135,#425136,#425137,#425138,#425139,#425140,
#425141,#425142,#425143,#425144,#425145,#425146,#425147,#425148,#425149,
#425150,#425151,#425152,#425153,#425154,#425155,#425156,#425157,#425158,
#425159,#425160,#425161),.UNSPECIFIED.,.F.,.F.,(4,3,3,3,3,3,3,3,3,3,3,4),
(0.,4.29157837302005E-6,5.42772623795335E-6,1.00901698482347E-5,1.31279195068638E-5,
1.57383542265804E-5,1.61011507492102E-5,1.67166789291744E-5,1.95343262811357E-5,
2.29377234674647E-5,2.71556047620055E-5,3.34407099942655E-5),
 .UNSPECIFIED.);
#26227=B_SPLINE_CURVE_WITH_KNOTS('',3,(#425174,#425175,#425176,#425177,
#425178,#425179,#425180,#425181,#425182,#425183,#425184,#425185,#425186,
#425187,#425188,#425189,#425190,#425191,#425192,#425193,#425194,#425195,
#425196,#425197,#425198,#425199,#425200,#425201,#425202,#425203,#425204,
#425205,#425206,#425207),.UNSPECIFIED.,.F.,.F.,(4,3,3,3,3,3,3,3,3,3,3,4),
(0.,3.7130942665666E-6,5.39981071559435E-6,8.78933289368458E-6,9.0027235706753E-6,
1.0714398450415E-5,1.60780299679457E-5,1.65806081157687E-5,2.30369726850392E-5,
2.67819200416082E-5,3.59736924188217E-5,4.03862783806992E-5),
 .UNSPECIFIED.);
#26228=B_SPLINE_CURVE_WITH_KNOTS('',3,(#425320,#425321,#425322,#425323),
 .UNSPECIFIED.,.F.,.F.,(4,4),(0.,7.70025630629239E-5),.UNSPECIFIED.);
#26229=B_SPLINE_CURVE_WITH_KNOTS('',3,(#425333,#425334,#425335,#425336),
 .UNSPECIFIED.,.F.,.F.,(4,4),(4.33680868994202E-19,7.70025630629233E-5),
 .UNSPECIFIED.);
#26230=B_SPLINE_CURVE_WITH_KNOTS('',3,(#425340,#425341,#425342,#425343,
#425344,#425345,#425346,#425347,#425348,#425349,#425350,#425351,#425352,
#425353,#425354,#425355,#425356,#425357,#425358,#425359,#425360,#425361,
#425362,#425363,#425364,#425365,#425366,#425367,#425368,#425369,#425370,
#425371,#425372,#425373,#425374,#425375,#425376),.UNSPECIFIED.,.F.,.F.,
(4,3,3,3,3,3,3,3,3,3,3,3,4),(0.,9.59031527199996E-6,1.94769411222853E-5,
2.02405092183151E-5,3.2137413857757E-5,3.60302195070436E-5,4.42640648819028E-5,
4.53660204229443E-5,5.03633762301884E-5,5.17708036292894E-5,5.37928993851986E-5,
5.54103755460202E-5,5.64557889513433E-5),.UNSPECIFIED.);
#26231=B_SPLINE_CURVE_WITH_KNOTS('',3,(#425377,#425378,#425379,#425380,
#425381,#425382,#425383,#425384,#425385,#425386,#425387,#425388,#425389,
#425390,#425391,#425392,#425393,#425394,#425395,#425396,#425397,#425398,
#425399,#425400,#425401,#425402,#425403,#425404),.UNSPECIFIED.,.F.,.F.,
(4,3,3,3,3,3,3,3,3,4),(5.64557889513433E-5,5.9894096649375E-5,6.3421400387338E-5,
7.22241476084518E-5,7.38322796533362E-5,8.3652918933141E-5,8.80714278222498E-5,
9.84837568500725E-5,0.000108624704079137,0.000110823272382853),
 .UNSPECIFIED.);
#26232=B_SPLINE_CURVE_WITH_KNOTS('',3,(#425420,#425421,#425422,#425423,
#425424,#425425,#425426,#425427,#425428,#425429,#425430,#425431,#425432,
#425433,#425434,#425435,#425436,#425437,#425438,#425439,#425440,#425441,
#425442,#425443,#425444,#425445,#425446,#425447),.UNSPECIFIED.,.F.,.F.,
(4,3,3,3,3,3,3,3,3,4),(0.,8.66039628581385E-6,1.64707715200667E-5,2.2450289413247E-5,
2.49975961757824E-5,2.88526003690282E-5,3.10661348995018E-5,3.43053543516961E-5,
3.66410545653561E-5,4.00504537627887E-5),.UNSPECIFIED.);
#26233=B_SPLINE_CURVE_WITH_KNOTS('',3,(#425450,#425451,#425452,#425453,
#425454,#425455,#425456),.UNSPECIFIED.,.F.,.F.,(4,3,4),(0.,4.40000041065375E-5,
9.89910850773115E-5),.UNSPECIFIED.);
#26234=B_SPLINE_CURVE_WITH_KNOTS('',3,(#425477,#425478,#425479,#425480,
#425481,#425482,#425483,#425484,#425485,#425486,#425487,#425488,#425489,
#425490,#425491,#425492,#425493,#425494,#425495,#425496,#425497,#425498,
#425499,#425500,#425501,#425502,#425503,#425504,#425505,#425506,#425507,
#425508,#425509,#425510),.UNSPECIFIED.,.F.,.F.,(4,3,3,3,3,3,3,3,3,3,3,4),
(0.,4.29157837304995E-6,5.42772623795321E-6,1.00901698482345E-5,1.31279195068636E-5,
1.57383542265953E-5,1.61011507492102E-5,1.67166789291755E-5,1.95343262811355E-5,
2.29377234674644E-5,2.71556047620056E-5,3.34407099942655E-5),
 .UNSPECIFIED.);
#26235=B_SPLINE_CURVE_WITH_KNOTS('',3,(#425523,#425524,#425525,#425526,
#425527,#425528,#425529,#425530,#425531,#425532,#425533,#425534,#425535,
#425536,#425537,#425538,#425539,#425540,#425541,#425542,#425543,#425544,
#425545,#425546,#425547,#425548,#425549,#425550,#425551,#425552,#425553,
#425554,#425555,#425556),.UNSPECIFIED.,.F.,.F.,(4,3,3,3,3,3,3,3,3,3,3,4),
(0.,3.71309426656671E-6,5.39981071559432E-6,8.78933289371078E-6,9.00272357067543E-6,
1.07143984504152E-5,1.60780299679494E-5,1.65806081157689E-5,2.30369726850434E-5,
2.67819200416089E-5,3.59736924188055E-5,4.03862783807004E-5),
 .UNSPECIFIED.);
#26236=B_SPLINE_CURVE_WITH_KNOTS('',3,(#425669,#425670,#425671,#425672),
 .UNSPECIFIED.,.F.,.F.,(4,4),(0.,7.7002563062924E-5),.UNSPECIFIED.);
#26237=B_SPLINE_CURVE_WITH_KNOTS('',3,(#425682,#425683,#425684,#425685),
 .UNSPECIFIED.,.F.,.F.,(4,4),(4.84869951806108E-19,7.70025630629238E-5),
 .UNSPECIFIED.);
#26238=B_SPLINE_CURVE_WITH_KNOTS('',3,(#425689,#425690,#425691,#425692,
#425693,#425694,#425695,#425696,#425697,#425698,#425699,#425700,#425701,
#425702,#425703,#425704,#425705,#425706,#425707,#425708,#425709,#425710,
#425711,#425712,#425713,#425714,#425715,#425716,#425717,#425718,#425719,
#425720,#425721,#425722,#425723,#425724,#425725),.UNSPECIFIED.,.F.,.F.,
(4,3,3,3,3,3,3,3,3,3,3,3,4),(0.,9.59031527201029E-6,1.94769411223069E-5,
2.0240509218315E-5,3.21374138577701E-5,3.60302195070435E-5,4.42640648818496E-5,
4.53660204229439E-5,5.03633762302282E-5,5.17708036292892E-5,5.37928993851987E-5,
5.54103755460199E-5,5.64557889512175E-5),.UNSPECIFIED.);
#26239=B_SPLINE_CURVE_WITH_KNOTS('',3,(#425726,#425727,#425728,#425729,
#425730,#425731,#425732,#425733,#425734,#425735,#425736,#425737,#425738,
#425739,#425740,#425741,#425742,#425743,#425744,#425745,#425746,#425747,
#425748,#425749,#425750,#425751,#425752,#425753),.UNSPECIFIED.,.F.,.F.,
(4,3,3,3,3,3,3,3,3,4),(5.64557889512175E-5,5.98940966493747E-5,6.34214003873375E-5,
7.22241476083973E-5,7.38322796533362E-5,8.36529189331593E-5,8.80714278222496E-5,
9.84837568501165E-5,0.000108624704079233,0.000110823272382853),
 .UNSPECIFIED.);
#26240=B_SPLINE_CURVE_WITH_KNOTS('',3,(#425769,#425770,#425771,#425772,
#425773,#425774,#425775,#425776,#425777,#425778,#425779,#425780,#425781,
#425782,#425783,#425784,#425785,#425786,#425787,#425788,#425789,#425790,
#425791,#425792,#425793,#425794,#425795,#425796),.UNSPECIFIED.,.F.,.F.,
(4,3,3,3,3,3,3,3,3,4),(0.,8.66039628584176E-6,1.64707715200667E-5,2.24502894132358E-5,
2.49975961757823E-5,2.88526003690282E-5,3.10661348995017E-5,3.4305354351696E-5,
3.6641054565356E-5,4.00504537627888E-5),.UNSPECIFIED.);
#26241=B_SPLINE_CURVE_WITH_KNOTS('',3,(#425799,#425800,#425801,#425802,
#425803,#425804,#425805),.UNSPECIFIED.,.F.,.F.,(4,3,4),(0.,4.40000041065377E-5,
9.89910850773114E-5),.UNSPECIFIED.);
#26242=B_SPLINE_CURVE_WITH_KNOTS('',3,(#425826,#425827,#425828,#425829,
#425830,#425831,#425832,#425833,#425834,#425835,#425836,#425837,#425838,
#425839,#425840,#425841,#425842,#425843,#425844,#425845,#425846,#425847,
#425848,#425849,#425850,#425851,#425852,#425853,#425854,#425855,#425856,
#425857,#425858,#425859),.UNSPECIFIED.,.F.,.F.,(4,3,3,3,3,3,3,3,3,3,3,4),
(0.,4.29157837302334E-6,5.42772623795342E-6,1.00901698482347E-5,1.3127919506864E-5,
1.57383542265795E-5,1.61011507492107E-5,1.67166789291751E-5,1.95343262811362E-5,
2.29377234674651E-5,2.71556047620059E-5,3.34407099942661E-5),
 .UNSPECIFIED.);
#26243=B_SPLINE_CURVE_WITH_KNOTS('',3,(#425872,#425873,#425874,#425875,
#425876,#425877,#425878,#425879,#425880,#425881,#425882,#425883,#425884,
#425885,#425886,#425887,#425888,#425889,#425890,#425891,#425892,#425893,
#425894,#425895,#425896,#425897,#425898,#425899,#425900,#425901,#425902,
#425903,#425904,#425905),.UNSPECIFIED.,.F.,.F.,(4,3,3,3,3,3,3,3,3,3,3,4),
(0.,3.7130942665666E-6,5.39981071559416E-6,8.78933289328906E-6,9.0027235706754E-6,
1.07143984504151E-5,1.60780299679608E-5,1.65806081157689E-5,2.30369726850439E-5,
2.67819200416086E-5,3.59736924187639E-5,4.03862783807002E-5),
 .UNSPECIFIED.);
#26244=B_SPLINE_CURVE_WITH_KNOTS('',3,(#426018,#426019,#426020,#426021),
 .UNSPECIFIED.,.F.,.F.,(4,4),(0.,7.70025630629238E-5),.UNSPECIFIED.);
#26245=B_SPLINE_CURVE_WITH_KNOTS('',3,(#426031,#426032,#426033,#426034),
 .UNSPECIFIED.,.F.,.F.,(4,4),(0.,7.70025630629238E-5),.UNSPECIFIED.);
#26246=B_SPLINE_CURVE_WITH_KNOTS('',3,(#426038,#426039,#426040,#426041,
#426042,#426043,#426044,#426045,#426046,#426047,#426048,#426049,#426050,
#426051,#426052,#426053,#426054,#426055,#426056,#426057,#426058,#426059,
#426060,#426061,#426062,#426063,#426064,#426065,#426066,#426067,#426068,
#426069,#426070,#426071,#426072,#426073,#426074),.UNSPECIFIED.,.F.,.F.,
(4,3,3,3,3,3,3,3,3,3,3,3,4),(0.,9.5903152720036E-6,1.94769411222964E-5,
2.02405092183154E-5,3.21374138577761E-5,3.60302195070438E-5,4.4264064881776E-5,
4.53660204229443E-5,5.03633762302123E-5,5.17708036292897E-5,5.37928993851989E-5,
5.54103755460199E-5,5.64557889509958E-5),.UNSPECIFIED.);
#26247=B_SPLINE_CURVE_WITH_KNOTS('',3,(#426075,#426076,#426077,#426078,
#426079,#426080,#426081,#426082,#426083,#426084,#426085,#426086,#426087,
#426088,#426089,#426090,#426091,#426092,#426093,#426094,#426095,#426096,
#426097,#426098,#426099,#426100,#426101,#426102),.UNSPECIFIED.,.F.,.F.,
(4,3,3,3,3,3,3,3,3,4),(5.64557889509958E-5,5.98940966493749E-5,6.3421400387338E-5,
7.22241476085281E-5,7.38322796533361E-5,8.3652918933147E-5,8.80714278222493E-5,
9.84837568501112E-5,0.000108624704079221,0.000110823272382852),
 .UNSPECIFIED.);
#26248=B_SPLINE_CURVE_WITH_KNOTS('',3,(#426118,#426119,#426120,#426121,
#426122,#426123,#426124,#426125,#426126,#426127,#426128,#426129,#426130,
#426131,#426132,#426133,#426134,#426135,#426136,#426137,#426138,#426139,
#426140,#426141,#426142,#426143,#426144,#426145),.UNSPECIFIED.,.F.,.F.,
(4,3,3,3,3,3,3,3,3,4),(0.,8.66039628579918E-6,1.64707715200669E-5,2.2450289413237E-5,
2.49975961757828E-5,2.88526003690285E-5,3.10661348995021E-5,3.43053543516965E-5,
3.66410545653566E-5,4.00504537627887E-5),.UNSPECIFIED.);
#26249=B_SPLINE_CURVE_WITH_KNOTS('',3,(#426148,#426149,#426150,#426151,
#426152,#426153,#426154),.UNSPECIFIED.,.F.,.F.,(4,3,4),(0.,4.40000041065375E-5,
9.8991085077311E-5),.UNSPECIFIED.);
#26250=B_SPLINE_CURVE_WITH_KNOTS('',3,(#426175,#426176,#426177,#426178,
#426179,#426180,#426181,#426182,#426183,#426184,#426185,#426186,#426187,
#426188,#426189,#426190,#426191,#426192,#426193,#426194,#426195,#426196,
#426197,#426198,#426199,#426200,#426201,#426202,#426203,#426204,#426205,
#426206,#426207,#426208),.UNSPECIFIED.,.F.,.F.,(4,3,3,3,3,3,3,3,3,3,3,4),
(0.,4.29157837302442E-6,5.42772623795322E-6,1.00901698482346E-5,1.31279195068638E-5,
1.57383542265859E-5,1.61011507492107E-5,1.67166789291753E-5,1.9534326281136E-5,
2.29377234674649E-5,2.71556047620057E-5,3.34407099942659E-5),
 .UNSPECIFIED.);
#26251=B_SPLINE_CURVE_WITH_KNOTS('',3,(#426221,#426222,#426223,#426224,
#426225,#426226,#426227,#426228,#426229,#426230,#426231,#426232,#426233,
#426234,#426235,#426236,#426237,#426238,#426239,#426240,#426241,#426242,
#426243,#426244,#426245,#426246,#426247,#426248,#426249,#426250,#426251,
#426252,#426253,#426254),.UNSPECIFIED.,.F.,.F.,(4,3,3,3,3,3,3,3,3,3,3,4),
(0.,3.71309426656662E-6,5.39981071559435E-6,8.78933289332053E-6,9.00272357067553E-6,
1.07143984504153E-5,1.60780299679585E-5,1.6580608115769E-5,2.30369726850372E-5,
2.67819200416089E-5,3.59736924188161E-5,4.03862783807003E-5),
 .UNSPECIFIED.);
#26252=B_SPLINE_CURVE_WITH_KNOTS('',3,(#426367,#426368,#426369,#426370),
 .UNSPECIFIED.,.F.,.F.,(4,4),(0.,7.70025630629237E-5),.UNSPECIFIED.);
#26253=B_SPLINE_CURVE_WITH_KNOTS('',3,(#426380,#426381,#426382,#426383),
 .UNSPECIFIED.,.F.,.F.,(4,4),(0.,7.70025630629238E-5),.UNSPECIFIED.);
#26254=B_SPLINE_CURVE_WITH_KNOTS('',3,(#426387,#426388,#426389,#426390,
#426391,#426392,#426393,#426394,#426395,#426396,#426397,#426398,#426399,
#426400,#426401,#426402,#426403,#426404,#426405,#426406,#426407,#426408,
#426409,#426410,#426411,#426412,#426413,#426414,#426415,#426416,#426417,
#426418,#426419,#426420,#426421,#426422,#426423),.UNSPECIFIED.,.F.,.F.,
(4,3,3,3,3,3,3,3,3,3,3,3,4),(0.,9.59031527200642E-6,1.94769411222944E-5,
2.02405092183152E-5,3.21374138577678E-5,3.6030219507044E-5,4.42640648819271E-5,
4.53660204229444E-5,5.03633762302186E-5,5.17708036292897E-5,5.37928993851991E-5,
5.54103755460196E-5,5.64557889512567E-5),.UNSPECIFIED.);
#26255=B_SPLINE_CURVE_WITH_KNOTS('',3,(#426424,#426425,#426426,#426427,
#426428,#426429,#426430,#426431,#426432,#426433,#426434,#426435,#426436,
#426437,#426438,#426439,#426440,#426441,#426442,#426443,#426444,#426445,
#426446,#426447,#426448,#426449,#426450,#426451),.UNSPECIFIED.,.F.,.F.,
(4,3,3,3,3,3,3,3,3,4),(5.64557889512567E-5,5.9894096649375E-5,6.34214003873379E-5,
7.22241476083888E-5,7.38322796533364E-5,8.36529189331357E-5,8.807142782225E-5,
9.84837568500544E-5,0.000108624704079104,0.000110823272382853),
 .UNSPECIFIED.);
#26256=B_SPLINE_CURVE_WITH_KNOTS('',3,(#426467,#426468,#426469,#426470,
#426471,#426472,#426473,#426474,#426475,#426476,#426477,#426478,#426479,
#426480,#426481,#426482,#426483,#426484,#426485,#426486,#426487,#426488,
#426489,#426490,#426491,#426492,#426493,#426494),.UNSPECIFIED.,.F.,.F.,
(4,3,3,3,3,3,3,3,3,4),(0.,8.66039628580946E-6,1.64707715200666E-5,2.24502894132521E-5,
2.49975961757823E-5,2.88526003690281E-5,3.10661348995017E-5,3.43053543516962E-5,
3.66410545653556E-5,4.00504537627888E-5),.UNSPECIFIED.);
#26257=B_SPLINE_CURVE_WITH_KNOTS('',3,(#426497,#426498,#426499,#426500,
#426501,#426502,#426503),.UNSPECIFIED.,.F.,.F.,(4,3,4),(0.,4.40000041065375E-5,
9.89910850773113E-5),.UNSPECIFIED.);
#26258=B_SPLINE_CURVE_WITH_KNOTS('',3,(#426524,#426525,#426526,#426527,
#426528,#426529,#426530,#426531,#426532,#426533,#426534,#426535,#426536,
#426537,#426538,#426539,#426540,#426541,#426542,#426543,#426544,#426545,
#426546,#426547,#426548,#426549,#426550,#426551,#426552,#426553,#426554,
#426555,#426556,#426557),.UNSPECIFIED.,.F.,.F.,(4,3,3,3,3,3,3,3,3,3,3,4),
(0.,4.29157837303971E-6,5.4277262379535E-6,1.00901698482348E-5,1.3127919506864E-5,
1.57383542265878E-5,1.61011507492106E-5,1.67166789291757E-5,1.9534326281136E-5,
2.29377234674647E-5,2.71556047620058E-5,3.34407099942659E-5),
 .UNSPECIFIED.);
#26259=B_SPLINE_CURVE_WITH_KNOTS('',3,(#426570,#426571,#426572,#426573,
#426574,#426575,#426576,#426577,#426578,#426579,#426580,#426581,#426582,
#426583,#426584,#426585,#426586,#426587,#426588,#426589,#426590,#426591,
#426592,#426593,#426594,#426595,#426596,#426597,#426598,#426599,#426600,
#426601,#426602,#426603),.UNSPECIFIED.,.F.,.F.,(4,3,3,3,3,3,3,3,3,3,3,4),
(6.1331736667335E-19,3.71309426656605E-6,5.399810715594E-6,8.78933289331522E-6,
9.00272357067485E-6,1.07143984504146E-5,1.60780299679516E-5,1.65806081157683E-5,
2.3036972685016E-5,2.6781920041608E-5,3.59736924187877E-5,4.03862783806992E-5),
 .UNSPECIFIED.);
#26260=B_SPLINE_CURVE_WITH_KNOTS('',3,(#426716,#426717,#426718,#426719),
 .UNSPECIFIED.,.F.,.F.,(4,4),(0.,7.70025630629241E-5),.UNSPECIFIED.);
#26261=B_SPLINE_CURVE_WITH_KNOTS('',3,(#426729,#426730,#426731,#426732),
 .UNSPECIFIED.,.F.,.F.,(4,4),(2.16840434497101E-19,7.70025630629238E-5),
 .UNSPECIFIED.);
#26262=B_SPLINE_CURVE_WITH_KNOTS('',3,(#426736,#426737,#426738,#426739,
#426740,#426741,#426742,#426743,#426744,#426745,#426746,#426747,#426748,
#426749,#426750,#426751,#426752,#426753,#426754,#426755,#426756,#426757,
#426758,#426759,#426760,#426761,#426762,#426763,#426764,#426765,#426766,
#426767,#426768,#426769,#426770,#426771,#426772),.UNSPECIFIED.,.F.,.F.,
(4,3,3,3,3,3,3,3,3,3,3,3,4),(0.,9.590315272008E-6,1.94769411222952E-5,2.02405092183151E-5,
3.21374138577707E-5,3.60302195070438E-5,4.42640648818693E-5,4.53660204229443E-5,
5.03633762301991E-5,5.17708036292894E-5,5.37928993851986E-5,5.54103755460196E-5,
5.64557889511543E-5),.UNSPECIFIED.);
#26263=B_SPLINE_CURVE_WITH_KNOTS('',3,(#426773,#426774,#426775,#426776,
#426777,#426778,#426779,#426780,#426781,#426782,#426783,#426784,#426785,
#426786,#426787,#426788,#426789,#426790,#426791,#426792,#426793,#426794,
#426795,#426796,#426797,#426798,#426799,#426800),.UNSPECIFIED.,.F.,.F.,
(4,3,3,3,3,3,3,3,3,4),(5.64557889511543E-5,5.98940966493751E-5,6.34214003873378E-5,
7.22241476084624E-5,7.3832279653336E-5,8.36529189331399E-5,8.80714278222494E-5,
9.8483756850071E-5,0.000108624704079142,0.000110823272382852),
 .UNSPECIFIED.);
#26264=B_SPLINE_CURVE_WITH_KNOTS('',3,(#426816,#426817,#426818,#426819,
#426820,#426821,#426822,#426823,#426824,#426825,#426826,#426827,#426828,
#426829,#426830,#426831,#426832,#426833,#426834,#426835,#426836,#426837,
#426838,#426839,#426840,#426841,#426842,#426843),.UNSPECIFIED.,.F.,.F.,
(4,3,3,3,3,3,3,3,3,4),(0.,8.66039628583704E-6,1.64707715200666E-5,2.24502894132115E-5,
2.49975961757823E-5,2.8852600369028E-5,3.10661348995016E-5,3.4305354351696E-5,
3.66410545653559E-5,4.00504537627888E-5),.UNSPECIFIED.);
#26265=B_SPLINE_CURVE_WITH_KNOTS('',3,(#426846,#426847,#426848,#426849,
#426850,#426851,#426852),.UNSPECIFIED.,.F.,.F.,(4,3,4),(0.,4.40000041065373E-5,
9.89910850773113E-5),.UNSPECIFIED.);
#26266=B_SPLINE_CURVE_WITH_KNOTS('',3,(#426873,#426874,#426875,#426876,
#426877,#426878,#426879,#426880,#426881,#426882,#426883,#426884,#426885,
#426886,#426887,#426888,#426889,#426890,#426891,#426892,#426893,#426894,
#426895,#426896,#426897,#426898,#426899,#426900,#426901,#426902,#426903,
#426904,#426905,#426906),.UNSPECIFIED.,.F.,.F.,(4,3,3,3,3,3,3,3,3,3,3,4),
(0.,4.29157837303212E-6,5.4277262379533E-6,1.00901698482348E-5,1.31279195068639E-5,
1.57383542265859E-5,1.61011507492106E-5,1.67166789291755E-5,1.95343262811357E-5,
2.2937723467465E-5,2.71556047620056E-5,3.34407099942654E-5),
 .UNSPECIFIED.);
#26267=B_SPLINE_CURVE_WITH_KNOTS('',3,(#426919,#426920,#426921,#426922,
#426923,#426924,#426925,#426926,#426927,#426928,#426929,#426930,#426931,
#426932,#426933,#426934,#426935,#426936,#426937,#426938,#426939,#426940,
#426941,#426942,#426943,#426944,#426945,#426946,#426947,#426948,#426949,
#426950,#426951,#426952),.UNSPECIFIED.,.F.,.F.,(4,3,3,3,3,3,3,3,3,3,3,4),
(0.,3.71309426656661E-6,5.39981071559432E-6,8.78933289364816E-6,9.00272357067536E-6,
1.07143984504151E-5,1.60780299679642E-5,1.65806081157689E-5,2.30369726850498E-5,
2.6781920041609E-5,3.59736924187643E-5,4.03862783807005E-5),
 .UNSPECIFIED.);
#26268=B_SPLINE_CURVE_WITH_KNOTS('',3,(#427065,#427066,#427067,#427068),
 .UNSPECIFIED.,.F.,.F.,(4,4),(0.,7.70025630629238E-5),.UNSPECIFIED.);
#26269=B_SPLINE_CURVE_WITH_KNOTS('',3,(#427078,#427079,#427080,#427081),
 .UNSPECIFIED.,.F.,.F.,(4,4),(4.63171371119878E-19,7.70025630629236E-5),
 .UNSPECIFIED.);
#26270=B_SPLINE_CURVE_WITH_KNOTS('',3,(#427085,#427086,#427087,#427088,
#427089,#427090,#427091,#427092,#427093,#427094,#427095,#427096,#427097,
#427098,#427099,#427100,#427101,#427102,#427103,#427104,#427105,#427106,
#427107,#427108,#427109,#427110,#427111,#427112,#427113,#427114,#427115,
#427116,#427117,#427118,#427119,#427120,#427121),.UNSPECIFIED.,.F.,.F.,
(4,3,3,3,3,3,3,3,3,3,3,3,4),(0.,9.59031527200658E-6,1.94769411222967E-5,
2.02405092183153E-5,3.21374138577672E-5,3.60302195070438E-5,4.42640648818944E-5,
4.53660204229444E-5,5.03633762302181E-5,5.17708036292896E-5,5.37928993851989E-5,
5.54103755460198E-5,5.64557889511992E-5),.UNSPECIFIED.);
#26271=B_SPLINE_CURVE_WITH_KNOTS('',3,(#427122,#427123,#427124,#427125,
#427126,#427127,#427128,#427129,#427130,#427131,#427132,#427133,#427134,
#427135,#427136,#427137,#427138,#427139,#427140,#427141,#427142,#427143,
#427144,#427145,#427146,#427147,#427148,#427149),.UNSPECIFIED.,.F.,.F.,
(4,3,3,3,3,3,3,3,3,4),(5.64557889511992E-5,5.98940966493751E-5,6.34214003873379E-5,
7.22241476084401E-5,7.38322796533362E-5,8.36529189331593E-5,8.80714278222498E-5,
9.8483756850112E-5,0.000108624704079221,0.000110823272382853),
 .UNSPECIFIED.);
#26272=B_SPLINE_CURVE_WITH_KNOTS('',3,(#427165,#427166,#427167,#427168,
#427169,#427170,#427171,#427172,#427173,#427174,#427175,#427176,#427177,
#427178,#427179,#427180,#427181,#427182,#427183,#427184,#427185,#427186,
#427187,#427188,#427189,#427190,#427191,#427192),.UNSPECIFIED.,.F.,.F.,
(4,3,3,3,3,3,3,3,3,4),(0.,8.66039628577747E-6,1.64707715200665E-5,2.24502894132765E-5,
2.49975961757823E-5,2.88526003690281E-5,3.10661348995017E-5,3.43053543516961E-5,
3.66410545653561E-5,4.00504537627891E-5),.UNSPECIFIED.);
#26273=B_SPLINE_CURVE_WITH_KNOTS('',3,(#427195,#427196,#427197,#427198,
#427199,#427200,#427201),.UNSPECIFIED.,.F.,.F.,(4,3,4),(0.,4.40000041065372E-5,
9.89910850773113E-5),.UNSPECIFIED.);
#26274=B_SPLINE_CURVE_WITH_KNOTS('',3,(#427222,#427223,#427224,#427225,
#427226,#427227,#427228,#427229,#427230,#427231,#427232,#427233,#427234,
#427235,#427236,#427237,#427238,#427239,#427240,#427241,#427242,#427243,
#427244,#427245,#427246,#427247,#427248,#427249,#427250,#427251,#427252,
#427253,#427254,#427255),.UNSPECIFIED.,.F.,.F.,(4,3,3,3,3,3,3,3,3,3,3,4),
(0.,4.29157837302174E-6,5.42772623795324E-6,1.00901698482348E-5,1.31279195068638E-5,
1.57383542265879E-5,1.61011507492104E-5,1.67166789291754E-5,1.95343262811358E-5,
2.2937723467465E-5,2.71556047620057E-5,3.34407099942658E-5),
 .UNSPECIFIED.);
#26275=B_SPLINE_CURVE_WITH_KNOTS('',3,(#427268,#427269,#427270,#427271,
#427272,#427273,#427274,#427275,#427276,#427277,#427278,#427279,#427280,
#427281,#427282,#427283,#427284,#427285,#427286,#427287,#427288,#427289,
#427290,#427291,#427292,#427293,#427294,#427295,#427296,#427297,#427298,
#427299,#427300,#427301),.UNSPECIFIED.,.F.,.F.,(4,3,3,3,3,3,3,3,3,3,3,4),
(5.42101086242752E-20,3.71309426656656E-6,5.39981071559424E-6,8.78933289329387E-6,
9.00272357067524E-6,1.0714398450415E-5,1.60780299679569E-5,1.65806081157688E-5,
2.30369726850531E-5,2.67819200416085E-5,3.59736924187559E-5,4.03862783807002E-5),
 .UNSPECIFIED.);
#26276=B_SPLINE_CURVE_WITH_KNOTS('',3,(#427414,#427415,#427416,#427417),
 .UNSPECIFIED.,.F.,.F.,(4,4),(0.,7.70025630629241E-5),.UNSPECIFIED.);
#26277=B_SPLINE_CURVE_WITH_KNOTS('',3,(#427427,#427428,#427429,#427430),
 .UNSPECIFIED.,.F.,.F.,(4,4),(1.0842021724855E-19,7.70025630629236E-5),
 .UNSPECIFIED.);
#26278=B_SPLINE_CURVE_WITH_KNOTS('',3,(#427434,#427435,#427436,#427437,
#427438,#427439,#427440,#427441,#427442,#427443,#427444,#427445,#427446,
#427447,#427448,#427449,#427450,#427451,#427452,#427453,#427454,#427455,
#427456,#427457,#427458,#427459,#427460,#427461,#427462,#427463,#427464,
#427465,#427466,#427467,#427468,#427469,#427470),.UNSPECIFIED.,.F.,.F.,
(4,3,3,3,3,3,3,3,3,3,3,3,4),(0.,9.59031527199611E-6,1.9476941122284E-5,
2.02405092183151E-5,3.21374138577688E-5,3.60302195070439E-5,4.42640648818978E-5,
4.53660204229444E-5,5.03633762302136E-5,5.17708036292894E-5,5.37928993851988E-5,
5.54103755460199E-5,5.64557889511083E-5),.UNSPECIFIED.);
#26279=B_SPLINE_CURVE_WITH_KNOTS('',3,(#427471,#427472,#427473,#427474,
#427475,#427476,#427477,#427478,#427479,#427480,#427481,#427482,#427483,
#427484,#427485,#427486,#427487,#427488,#427489,#427490,#427491,#427492,
#427493,#427494,#427495,#427496,#427497,#427498),.UNSPECIFIED.,.F.,.F.,
(4,3,3,3,3,3,3,3,3,4),(5.64557889511083E-5,5.98940966493748E-5,6.34214003873378E-5,
7.22241476084839E-5,7.38322796533364E-5,8.36529189331476E-5,8.80714278222498E-5,
9.84837568500776E-5,0.000108624704079139,0.000110823272382853),
 .UNSPECIFIED.);
#26280=B_SPLINE_CURVE_WITH_KNOTS('',3,(#427514,#427515,#427516,#427517,
#427518,#427519,#427520,#427521,#427522,#427523,#427524,#427525,#427526,
#427527,#427528,#427529,#427530,#427531,#427532,#427533,#427534,#427535,
#427536,#427537,#427538,#427539,#427540,#427541),.UNSPECIFIED.,.F.,.F.,
(4,3,3,3,3,3,3,3,3,4),(0.,8.66039628580465E-6,1.64707715200667E-5,2.24502894132612E-5,
2.49975961757825E-5,2.88526003690282E-5,3.10661348995018E-5,3.43053543516961E-5,
3.66410545653559E-5,4.00504537627886E-5),.UNSPECIFIED.);
#26281=B_SPLINE_CURVE_WITH_KNOTS('',3,(#427544,#427545,#427546,#427547,
#427548,#427549,#427550),.UNSPECIFIED.,.F.,.F.,(4,3,4),(0.,4.40000041065375E-5,
9.89910850773114E-5),.UNSPECIFIED.);
#26282=B_SPLINE_CURVE_WITH_KNOTS('',3,(#427571,#427572,#427573,#427574,
#427575,#427576,#427577,#427578,#427579,#427580,#427581,#427582,#427583,
#427584,#427585,#427586,#427587,#427588,#427589,#427590,#427591,#427592,
#427593,#427594,#427595,#427596,#427597,#427598,#427599,#427600,#427601,
#427602,#427603,#427604),.UNSPECIFIED.,.F.,.F.,(4,3,3,3,3,3,3,3,3,3,3,4),
(0.,4.29157837304268E-6,5.42772623795342E-6,1.00901698482348E-5,1.31279195068639E-5,
1.57383542265942E-5,1.61011507492105E-5,1.67166789291756E-5,1.95343262811359E-5,
2.29377234674649E-5,2.71556047620056E-5,3.3440709994266E-5),
 .UNSPECIFIED.);
#26283=B_SPLINE_CURVE_WITH_KNOTS('',3,(#427617,#427618,#427619,#427620,
#427621,#427622,#427623,#427624,#427625,#427626,#427627,#427628,#427629,
#427630,#427631,#427632,#427633,#427634,#427635,#427636,#427637,#427638,
#427639,#427640,#427641,#427642,#427643,#427644,#427645,#427646,#427647,
#427648,#427649,#427650),.UNSPECIFIED.,.F.,.F.,(4,3,3,3,3,3,3,3,3,3,3,4),
(1.0842021724855E-19,3.71309426656654E-6,5.39981071559418E-6,8.7893328933137E-6,
9.00272357067519E-6,1.0714398450415E-5,1.6078029967963E-5,1.65806081157686E-5,
2.30369726850455E-5,2.67819200416086E-5,3.59736924187525E-5,4.03862783806999E-5),
 .UNSPECIFIED.);
#26284=B_SPLINE_CURVE_WITH_KNOTS('',3,(#427763,#427764,#427765,#427766),
 .UNSPECIFIED.,.F.,.F.,(4,4),(0.,7.70025630629241E-5),.UNSPECIFIED.);
#26285=B_SPLINE_CURVE_WITH_KNOTS('',3,(#427776,#427777,#427778,#427779),
 .UNSPECIFIED.,.F.,.F.,(4,4),(2.16840434497101E-19,7.70025630629238E-5),
 .UNSPECIFIED.);
#26286=B_SPLINE_CURVE_WITH_KNOTS('',3,(#427783,#427784,#427785,#427786,
#427787,#427788,#427789,#427790,#427791,#427792,#427793,#427794,#427795,
#427796,#427797,#427798,#427799,#427800,#427801,#427802,#427803,#427804,
#427805,#427806,#427807,#427808,#427809,#427810,#427811,#427812,#427813,
#427814,#427815,#427816,#427817,#427818,#427819),.UNSPECIFIED.,.F.,.F.,
(4,3,3,3,3,3,3,3,3,3,3,3,4),(0.,9.59031527200811E-6,1.94769411222919E-5,
2.0240509218315E-5,3.2137413857773E-5,3.60302195070438E-5,4.42640648818379E-5,
4.53660204229443E-5,5.03633762302087E-5,5.17708036292895E-5,5.37928993851988E-5,
5.54103755460197E-5,5.64557889512956E-5),.UNSPECIFIED.);
#26287=B_SPLINE_CURVE_WITH_KNOTS('',3,(#427820,#427821,#427822,#427823,
#427824,#427825,#427826,#427827,#427828,#427829,#427830,#427831,#427832,
#427833,#427834,#427835,#427836,#427837,#427838,#427839,#427840,#427841,
#427842,#427843,#427844,#427845,#427846,#427847),.UNSPECIFIED.,.F.,.F.,
(4,3,3,3,3,3,3,3,3,4),(5.64557889512956E-5,5.98940966493751E-5,6.34214003873378E-5,
7.22241476084982E-5,7.38322796533364E-5,8.36529189331437E-5,8.80714278222499E-5,
9.8483756850066E-5,0.000108624704079128,0.000110823272382853),
 .UNSPECIFIED.);
#26288=B_SPLINE_CURVE_WITH_KNOTS('',3,(#427863,#427864,#427865,#427866,
#427867,#427868,#427869,#427870,#427871,#427872,#427873,#427874,#427875,
#427876,#427877,#427878,#427879,#427880,#427881,#427882,#427883,#427884,
#427885,#427886,#427887,#427888,#427889,#427890),.UNSPECIFIED.,.F.,.F.,
(4,3,3,3,3,3,3,3,3,4),(0.,8.66039628578402E-6,1.64707715200666E-5,2.24502894132383E-5,
2.49975961757825E-5,2.8852600369028E-5,3.10661348995017E-5,3.43053543516961E-5,
3.66410545653559E-5,4.00504537627886E-5),.UNSPECIFIED.);
#26289=B_SPLINE_CURVE_WITH_KNOTS('',3,(#427893,#427894,#427895,#427896,
#427897,#427898,#427899),.UNSPECIFIED.,.F.,.F.,(4,3,4),(0.,4.40000041065375E-5,
9.89910850773112E-5),.UNSPECIFIED.);
#26290=B_SPLINE_CURVE_WITH_KNOTS('',3,(#427920,#427921,#427922,#427923,
#427924,#427925,#427926,#427927,#427928,#427929,#427930,#427931,#427932,
#427933,#427934,#427935,#427936,#427937,#427938,#427939,#427940,#427941,
#427942,#427943,#427944,#427945,#427946,#427947,#427948,#427949,#427950,
#427951,#427952,#427953),.UNSPECIFIED.,.F.,.F.,(4,3,3,3,3,3,3,3,3,3,3,4),
(0.,4.29157837303304E-6,5.42772623795324E-6,1.00901698482347E-5,1.31279195068638E-5,
1.57383542265858E-5,1.61011507492102E-5,1.67166789291752E-5,1.95343262811359E-5,
2.29377234674647E-5,2.71556047620056E-5,3.34407099942656E-5),
 .UNSPECIFIED.);
#26291=B_SPLINE_CURVE_WITH_KNOTS('',3,(#427966,#427967,#427968,#427969,
#427970,#427971,#427972,#427973,#427974,#427975,#427976,#427977,#427978,
#427979,#427980,#427981,#427982,#427983,#427984,#427985,#427986,#427987,
#427988,#427989,#427990,#427991,#427992,#427993,#427994,#427995,#427996,
#427997,#427998,#427999),.UNSPECIFIED.,.F.,.F.,(4,3,3,3,3,3,3,3,3,3,3,4),
(0.,3.71309426656663E-6,5.39981071559434E-6,8.78933289329627E-6,9.00272357067523E-6,
1.0714398450415E-5,1.6078029967947E-5,1.65806081157688E-5,2.30369726850588E-5,
2.67819200416087E-5,3.59736924187837E-5,4.03862783807003E-5),
 .UNSPECIFIED.);
#26292=B_SPLINE_CURVE_WITH_KNOTS('',3,(#428112,#428113,#428114,#428115),
 .UNSPECIFIED.,.F.,.F.,(4,4),(0.,7.70025630629237E-5),.UNSPECIFIED.);
#26293=B_SPLINE_CURVE_WITH_KNOTS('',3,(#428125,#428126,#428127,#428128),
 .UNSPECIFIED.,.F.,.F.,(4,4),(0.,7.70025630629239E-5),.UNSPECIFIED.);
#26294=B_SPLINE_CURVE_WITH_KNOTS('',3,(#428132,#428133,#428134,#428135,
#428136,#428137,#428138,#428139,#428140,#428141,#428142,#428143,#428144,
#428145,#428146,#428147,#428148,#428149,#428150,#428151,#428152,#428153,
#428154,#428155,#428156,#428157,#428158,#428159,#428160,#428161,#428162,
#428163,#428164,#428165,#428166,#428167,#428168),.UNSPECIFIED.,.F.,.F.,
(4,3,3,3,3,3,3,3,3,3,3,3,4),(0.,9.59031527200666E-6,1.94769411223038E-5,
2.02405092183152E-5,3.21374138577607E-5,3.60302195070441E-5,4.42640648818939E-5,
4.53660204229446E-5,5.03633762302108E-5,5.177080362929E-5,5.3792899385199E-5,
5.54103755460199E-5,5.6455788950677E-5),.UNSPECIFIED.);
#26295=B_SPLINE_CURVE_WITH_KNOTS('',3,(#428169,#428170,#428171,#428172,
#428173,#428174,#428175,#428176,#428177,#428178,#428179,#428180,#428181,
#428182,#428183,#428184,#428185,#428186,#428187,#428188,#428189,#428190,
#428191,#428192,#428193,#428194,#428195,#428196),.UNSPECIFIED.,.F.,.F.,
(4,3,3,3,3,3,3,3,3,4),(5.6455788950677E-5,5.98940966493752E-5,6.34214003873382E-5,
7.2224147608401E-5,7.38322796533364E-5,8.36529189331423E-5,8.807142782225E-5,
9.84837568500578E-5,0.000108624704079111,0.000110823272382853),
 .UNSPECIFIED.);
#26296=B_SPLINE_CURVE_WITH_KNOTS('',3,(#428212,#428213,#428214,#428215,
#428216,#428217,#428218,#428219,#428220,#428221,#428222,#428223,#428224,
#428225,#428226,#428227,#428228,#428229,#428230,#428231,#428232,#428233,
#428234,#428235,#428236,#428237,#428238,#428239),.UNSPECIFIED.,.F.,.F.,
(4,3,3,3,3,3,3,3,3,4),(0.,8.66039628583575E-6,1.64707715200666E-5,2.24502894132503E-5,
2.49975961757824E-5,2.88526003690281E-5,3.10661348995017E-5,3.4305354351696E-5,
3.66410545653561E-5,4.00504537627891E-5),.UNSPECIFIED.);
#26297=B_SPLINE_CURVE_WITH_KNOTS('',3,(#428242,#428243,#428244,#428245,
#428246,#428247,#428248),.UNSPECIFIED.,.F.,.F.,(4,3,4),(0.,4.40000041065376E-5,
9.89910850773114E-5),.UNSPECIFIED.);
#26298=B_SPLINE_CURVE_WITH_KNOTS('',3,(#428269,#428270,#428271,#428272,
#428273,#428274,#428275,#428276,#428277,#428278,#428279,#428280,#428281,
#428282,#428283,#428284,#428285,#428286,#428287,#428288,#428289,#428290,
#428291,#428292,#428293,#428294,#428295,#428296,#428297,#428298,#428299,
#428300,#428301,#428302),.UNSPECIFIED.,.F.,.F.,(4,3,3,3,3,3,3,3,3,3,3,4),
(0.,4.29157837305384E-6,5.42772623795331E-6,1.00901698482348E-5,1.31279195068639E-5,
1.57383542265921E-5,1.61011507492104E-5,1.67166789291754E-5,1.95343262811356E-5,
2.29377234674648E-5,2.71556047620052E-5,3.34407099942653E-5),
 .UNSPECIFIED.);
#26299=B_SPLINE_CURVE_WITH_KNOTS('',3,(#428315,#428316,#428317,#428318,
#428319,#428320,#428321,#428322,#428323,#428324,#428325,#428326,#428327,
#428328,#428329,#428330,#428331,#428332,#428333,#428334,#428335,#428336,
#428337,#428338,#428339,#428340,#428341,#428342,#428343,#428344,#428345,
#428346,#428347,#428348),.UNSPECIFIED.,.F.,.F.,(4,3,3,3,3,3,3,3,3,3,3,4),
(2.16840434497101E-19,3.71309426656624E-6,5.39981071559413E-6,8.78933289330621E-6,
9.00272357067499E-6,1.07143984504148E-5,1.60780299679538E-5,1.65806081157682E-5,
2.30369726850502E-5,2.67819200416079E-5,3.59736924187975E-5,4.03862783806988E-5),
 .UNSPECIFIED.);
#26300=B_SPLINE_CURVE_WITH_KNOTS('',3,(#428461,#428462,#428463,#428464),
 .UNSPECIFIED.,.F.,.F.,(4,4),(0.,7.70025630629237E-5),.UNSPECIFIED.);
#26301=B_SPLINE_CURVE_WITH_KNOTS('',3,(#428474,#428475,#428476,#428477),
 .UNSPECIFIED.,.F.,.F.,(4,4),(2.16840434497101E-19,7.70025630629237E-5),
 .UNSPECIFIED.);
#26302=B_SPLINE_CURVE_WITH_KNOTS('',3,(#428481,#428482,#428483,#428484,
#428485,#428486,#428487,#428488,#428489,#428490,#428491,#428492,#428493,
#428494,#428495,#428496,#428497,#428498,#428499,#428500,#428501,#428502,
#428503,#428504,#428505,#428506,#428507,#428508,#428509,#428510,#428511,
#428512,#428513,#428514,#428515,#428516,#428517),.UNSPECIFIED.,.F.,.F.,
(4,3,3,3,3,3,3,3,3,3,3,3,4),(0.,9.59031527199202E-6,1.94769411222766E-5,
2.02405092183153E-5,3.21374138577703E-5,3.60302195070439E-5,4.42640648818995E-5,
4.53660204229444E-5,5.03633762302019E-5,5.17708036292897E-5,5.37928993851988E-5,
5.54103755460197E-5,5.64557889509303E-5),.UNSPECIFIED.);
#26303=B_SPLINE_CURVE_WITH_KNOTS('',3,(#428518,#428519,#428520,#428521,
#428522,#428523,#428524,#428525,#428526,#428527,#428528,#428529,#428530,
#428531,#428532,#428533,#428534,#428535,#428536,#428537,#428538,#428539,
#428540,#428541,#428542,#428543,#428544,#428545),.UNSPECIFIED.,.F.,.F.,
(4,3,3,3,3,3,3,3,3,4),(5.64557889509303E-5,5.98940966493749E-5,6.34214003873378E-5,
7.22241476083715E-5,7.38322796533363E-5,8.36529189331431E-5,8.80714278222498E-5,
9.84837568500731E-5,0.000108624704079147,0.000110823272382853),
 .UNSPECIFIED.);
#26304=B_SPLINE_CURVE_WITH_KNOTS('',3,(#428561,#428562,#428563,#428564,
#428565,#428566,#428567,#428568,#428569,#428570,#428571,#428572,#428573,
#428574,#428575,#428576,#428577,#428578,#428579,#428580,#428581,#428582,
#428583,#428584,#428585,#428586,#428587,#428588),.UNSPECIFIED.,.F.,.F.,
(4,3,3,3,3,3,3,3,3,4),(0.,8.66039628583168E-6,1.64707715200665E-5,2.24502894132335E-5,
2.49975961757824E-5,2.8852600369028E-5,3.10661348995016E-5,3.4305354351696E-5,
3.66410545653561E-5,4.00504537627882E-5),.UNSPECIFIED.);
#26305=B_SPLINE_CURVE_WITH_KNOTS('',3,(#428591,#428592,#428593,#428594,
#428595,#428596,#428597),.UNSPECIFIED.,.F.,.F.,(4,3,4),(0.,4.40000041065375E-5,
9.89910850773113E-5),.UNSPECIFIED.);
#26306=B_SPLINE_CURVE_WITH_KNOTS('',3,(#428618,#428619,#428620,#428621,
#428622,#428623,#428624,#428625,#428626,#428627,#428628,#428629,#428630,
#428631,#428632,#428633,#428634,#428635,#428636,#428637,#428638,#428639,
#428640,#428641,#428642,#428643,#428644,#428645,#428646,#428647,#428648,
#428649,#428650,#428651),.UNSPECIFIED.,.F.,.F.,(4,3,3,3,3,3,3,3,3,3,3,4),
(0.,4.29157837304218E-6,5.42772623795328E-6,1.00901698482345E-5,1.31279195068639E-5,
1.57383542265798E-5,1.61011507492105E-5,1.67166789291752E-5,1.9534326281136E-5,
2.29377234674652E-5,2.71556047620059E-5,3.34407099942656E-5),
 .UNSPECIFIED.);
#26307=B_SPLINE_CURVE_WITH_KNOTS('',3,(#428664,#428665,#428666,#428667,
#428668,#428669,#428670,#428671,#428672,#428673,#428674,#428675,#428676,
#428677,#428678,#428679,#428680,#428681,#428682,#428683,#428684,#428685,
#428686,#428687,#428688,#428689,#428690,#428691,#428692,#428693,#428694,
#428695,#428696,#428697),.UNSPECIFIED.,.F.,.F.,(4,3,3,3,3,3,3,3,3,3,3,4),
(0.,3.71309426656666E-6,5.39981071559459E-6,8.78933289334293E-6,9.00272357067531E-6,
1.0714398450415E-5,1.60780299679529E-5,1.65806081157687E-5,2.30369726850411E-5,
2.67819200416086E-5,3.59736924188054E-5,4.03862783806999E-5),
 .UNSPECIFIED.);
#26308=B_SPLINE_CURVE_WITH_KNOTS('',3,(#428810,#428811,#428812,#428813),
 .UNSPECIFIED.,.F.,.F.,(4,4),(0.,7.7002563062924E-5),.UNSPECIFIED.);
#26309=B_SPLINE_CURVE_WITH_KNOTS('',3,(#428823,#428824,#428825,#428826),
 .UNSPECIFIED.,.F.,.F.,(4,4),(6.1331736667335E-19,7.70025630629235E-5),
 .UNSPECIFIED.);
#26310=B_SPLINE_CURVE_WITH_KNOTS('',3,(#428830,#428831,#428832,#428833,
#428834,#428835,#428836,#428837,#428838,#428839,#428840,#428841,#428842,
#428843,#428844,#428845,#428846,#428847,#428848,#428849,#428850,#428851,
#428852,#428853,#428854,#428855,#428856,#428857,#428858,#428859,#428860,
#428861,#428862,#428863,#428864,#428865,#428866),.UNSPECIFIED.,.F.,.F.,
(4,3,3,3,3,3,3,3,3,3,3,3,4),(0.,9.59031527201265E-6,1.94769411223105E-5,
2.02405092183152E-5,3.2137413857766E-5,3.60302195070438E-5,4.42640648818916E-5,
4.53660204229442E-5,5.03633762302019E-5,5.17708036292896E-5,5.37928993851987E-5,
5.54103755460202E-5,5.64557889510335E-5),.UNSPECIFIED.);
#26311=B_SPLINE_CURVE_WITH_KNOTS('',3,(#428867,#428868,#428869,#428870,
#428871,#428872,#428873,#428874,#428875,#428876,#428877,#428878,#428879,
#428880,#428881,#428882,#428883,#428884,#428885,#428886,#428887,#428888,
#428889,#428890,#428891,#428892,#428893,#428894),.UNSPECIFIED.,.F.,.F.,
(4,3,3,3,3,3,3,3,3,4),(5.64557889510335E-5,5.98940966493751E-5,6.34214003873383E-5,
7.22241476084741E-5,7.38322796533365E-5,8.36529189331344E-5,8.80714278222503E-5,
9.8483756850067E-5,0.000108624704079123,0.000110823272382854),
 .UNSPECIFIED.);
#26312=B_SPLINE_CURVE_WITH_KNOTS('',3,(#428910,#428911,#428912,#428913,
#428914,#428915,#428916,#428917,#428918,#428919,#428920,#428921,#428922,
#428923,#428924,#428925,#428926,#428927,#428928,#428929,#428930,#428931,
#428932,#428933,#428934,#428935,#428936,#428937),.UNSPECIFIED.,.F.,.F.,
(4,3,3,3,3,3,3,3,3,4),(0.,8.66039628579893E-6,1.64707715200667E-5,2.24502894132494E-5,
2.49975961757824E-5,2.88526003690281E-5,3.10661348995014E-5,3.43053543516958E-5,
3.66410545653558E-5,4.00504537627883E-5),.UNSPECIFIED.);
#26313=B_SPLINE_CURVE_WITH_KNOTS('',3,(#428940,#428941,#428942,#428943,
#428944,#428945,#428946),.UNSPECIFIED.,.F.,.F.,(4,3,4),(0.,4.40000041065374E-5,
9.89910850773111E-5),.UNSPECIFIED.);
#26314=B_SPLINE_CURVE_WITH_KNOTS('',3,(#428967,#428968,#428969,#428970,
#428971,#428972,#428973,#428974,#428975,#428976,#428977,#428978,#428979,
#428980,#428981,#428982,#428983,#428984,#428985,#428986,#428987,#428988,
#428989,#428990,#428991,#428992,#428993,#428994,#428995,#428996,#428997,
#428998,#428999,#429000),.UNSPECIFIED.,.F.,.F.,(4,3,3,3,3,3,3,3,3,3,3,4),
(0.,4.29157837304618E-6,5.42772623795343E-6,1.0090169848235E-5,1.31279195068639E-5,
1.57383542265892E-5,1.61011507492107E-5,1.6716678929176E-5,1.95343262811359E-5,
2.29377234674647E-5,2.71556047620057E-5,3.34407099942664E-5),
 .UNSPECIFIED.);
#26315=B_SPLINE_CURVE_WITH_KNOTS('',3,(#429013,#429014,#429015,#429016,
#429017,#429018,#429019,#429020,#429021,#429022,#429023,#429024,#429025,
#429026,#429027,#429028,#429029,#429030,#429031,#429032,#429033,#429034,
#429035,#429036,#429037,#429038,#429039,#429040,#429041,#429042,#429043,
#429044,#429045,#429046),.UNSPECIFIED.,.F.,.F.,(4,3,3,3,3,3,3,3,3,3,3,4),
(0.,3.71309426656647E-6,5.39981071559407E-6,8.7893328936682E-6,9.00272357067528E-6,
1.07143984504149E-5,1.60780299679635E-5,1.65806081157687E-5,2.30369726850325E-5,
2.67819200416084E-5,3.59736924187732E-5,4.03862783806996E-5),
 .UNSPECIFIED.);
#26316=B_SPLINE_CURVE_WITH_KNOTS('',3,(#429159,#429160,#429161,#429162),
 .UNSPECIFIED.,.F.,.F.,(4,4),(0.,7.70025630629237E-5),.UNSPECIFIED.);
#26317=B_SPLINE_CURVE_WITH_KNOTS('',3,(#429172,#429173,#429174,#429175),
 .UNSPECIFIED.,.F.,.F.,(4,4),(2.16840434497101E-19,7.70025630629237E-5),
 .UNSPECIFIED.);
#26318=B_SPLINE_CURVE_WITH_KNOTS('',3,(#429179,#429180,#429181,#429182,
#429183,#429184,#429185,#429186,#429187,#429188,#429189,#429190,#429191,
#429192,#429193,#429194,#429195,#429196,#429197,#429198,#429199,#429200,
#429201,#429202,#429203,#429204,#429205,#429206,#429207,#429208,#429209,
#429210,#429211,#429212,#429213,#429214,#429215),.UNSPECIFIED.,.F.,.F.,
(4,3,3,3,3,3,3,3,3,3,3,3,4),(0.,9.59031527200831E-6,1.94769411222969E-5,
2.02405092183152E-5,3.21374138577705E-5,3.60302195070437E-5,4.4264064881883E-5,
4.53660204229444E-5,5.03633762301811E-5,5.17708036292893E-5,5.37928993851988E-5,
5.54103755460199E-5,5.64557889510115E-5),.UNSPECIFIED.);
#26319=B_SPLINE_CURVE_WITH_KNOTS('',3,(#429216,#429217,#429218,#429219,
#429220,#429221,#429222,#429223,#429224,#429225,#429226,#429227,#429228,
#429229,#429230,#429231,#429232,#429233,#429234,#429235,#429236,#429237,
#429238,#429239,#429240,#429241,#429242,#429243),.UNSPECIFIED.,.F.,.F.,
(4,3,3,3,3,3,3,3,3,4),(5.64557889510115E-5,5.98940966493751E-5,6.34214003873379E-5,
7.22241476084954E-5,7.38322796533364E-5,8.36529189331411E-5,8.80714278222498E-5,
9.84837568500968E-5,0.000108624704079193,0.000110823272382853),
 .UNSPECIFIED.);
#26320=B_SPLINE_CURVE_WITH_KNOTS('',3,(#429259,#429260,#429261,#429262,
#429263,#429264,#429265,#429266,#429267,#429268,#429269,#429270,#429271,
#429272,#429273,#429274,#429275,#429276,#429277,#429278,#429279,#429280,
#429281,#429282,#429283,#429284,#429285,#429286),.UNSPECIFIED.,.F.,.F.,
(4,3,3,3,3,3,3,3,3,4),(0.,8.66039628577601E-6,1.64707715200666E-5,2.24502894132603E-5,
2.49975961757822E-5,2.88526003690279E-5,3.10661348995017E-5,3.43053543516959E-5,
3.66410545653557E-5,4.00504537627883E-5),.UNSPECIFIED.);
#26321=B_SPLINE_CURVE_WITH_KNOTS('',3,(#429289,#429290,#429291,#429292,
#429293,#429294,#429295),.UNSPECIFIED.,.F.,.F.,(4,3,4),(0.,4.40000041065374E-5,
9.89910850773112E-5),.UNSPECIFIED.);
#26322=B_SPLINE_CURVE_WITH_KNOTS('',3,(#429316,#429317,#429318,#429319,
#429320,#429321,#429322,#429323,#429324,#429325,#429326,#429327,#429328,
#429329,#429330,#429331,#429332,#429333,#429334,#429335,#429336,#429337,
#429338,#429339,#429340,#429341,#429342,#429343,#429344,#429345,#429346,
#429347,#429348,#429349),.UNSPECIFIED.,.F.,.F.,(4,3,3,3,3,3,3,3,3,3,3,4),
(0.,4.29157837305213E-6,5.42772623795348E-6,1.0090169848235E-5,1.31279195068641E-5,
1.57383542265938E-5,1.61011507492108E-5,1.67166789291762E-5,1.95343262811361E-5,
2.29377234674651E-5,2.71556047620057E-5,3.34407099942658E-5),
 .UNSPECIFIED.);
#26323=B_SPLINE_CURVE_WITH_KNOTS('',3,(#429362,#429363,#429364,#429365,
#429366,#429367,#429368,#429369,#429370,#429371,#429372,#429373,#429374,
#429375,#429376,#429377,#429378,#429379,#429380,#429381,#429382,#429383,
#429384,#429385,#429386,#429387,#429388,#429389,#429390,#429391,#429392,
#429393,#429394,#429395),.UNSPECIFIED.,.F.,.F.,(4,3,3,3,3,3,3,3,3,3,3,4),
(2.16840434497101E-19,3.71309426656637E-6,5.39981071559423E-6,8.78933289368051E-6,
9.00272357067532E-6,1.0714398450415E-5,1.60780299679574E-5,1.65806081157687E-5,
2.30369726850297E-5,2.67819200416087E-5,3.59736924188118E-5,4.03862783807003E-5),
 .UNSPECIFIED.);
#26324=B_SPLINE_CURVE_WITH_KNOTS('',3,(#429508,#429509,#429510,#429511),
 .UNSPECIFIED.,.F.,.F.,(4,4),(0.,7.70025630629237E-5),.UNSPECIFIED.);
#26325=B_SPLINE_CURVE_WITH_KNOTS('',3,(#429521,#429522,#429523,#429524),
 .UNSPECIFIED.,.F.,.F.,(4,4),(0.,7.70025630629238E-5),.UNSPECIFIED.);
#26326=B_SPLINE_CURVE_WITH_KNOTS('',3,(#429528,#429529,#429530,#429531,
#429532,#429533,#429534,#429535,#429536,#429537,#429538,#429539,#429540,
#429541,#429542,#429543,#429544,#429545,#429546,#429547,#429548,#429549,
#429550,#429551,#429552,#429553,#429554,#429555,#429556,#429557,#429558,
#429559,#429560,#429561,#429562,#429563,#429564),.UNSPECIFIED.,.F.,.F.,
(4,3,3,3,3,3,3,3,3,3,3,3,4),(0.,9.59031527201064E-6,1.94769411223038E-5,
2.02405092183152E-5,3.21374138577706E-5,3.6030219507044E-5,4.42640648818172E-5,
4.53660204229447E-5,5.03633762302194E-5,5.17708036292895E-5,5.37928993851989E-5,
5.54103755460194E-5,5.64557889514687E-5),.UNSPECIFIED.);
#26327=B_SPLINE_CURVE_WITH_KNOTS('',3,(#429565,#429566,#429567,#429568,
#429569,#429570,#429571,#429572,#429573,#429574,#429575,#429576,#429577,
#429578,#429579,#429580,#429581,#429582,#429583,#429584,#429585,#429586,
#429587,#429588,#429589,#429590,#429591,#429592),.UNSPECIFIED.,.F.,.F.,
(4,3,3,3,3,3,3,3,3,4),(5.64557889514687E-5,5.98940966493748E-5,6.34214003873379E-5,
7.22241476084777E-5,7.38322796533365E-5,8.36529189331359E-5,8.80714278222495E-5,
9.84837568500667E-5,0.000108624704079124,0.000110823272382853),
 .UNSPECIFIED.);
#26328=B_SPLINE_CURVE_WITH_KNOTS('',3,(#429608,#429609,#429610,#429611,
#429612,#429613,#429614,#429615,#429616,#429617,#429618,#429619,#429620,
#429621,#429622,#429623,#429624,#429625,#429626,#429627,#429628,#429629,
#429630,#429631,#429632,#429633,#429634,#429635),.UNSPECIFIED.,.F.,.F.,
(4,3,3,3,3,3,3,3,3,4),(0.,8.66039628581978E-6,1.64707715200666E-5,2.24502894132339E-5,
2.49975961757823E-5,2.88526003690281E-5,3.10661348995017E-5,3.43053543516961E-5,
3.66410545653563E-5,4.00504537627894E-5),.UNSPECIFIED.);
#26329=B_SPLINE_CURVE_WITH_KNOTS('',3,(#429638,#429639,#429640,#429641,
#429642,#429643,#429644),.UNSPECIFIED.,.F.,.F.,(4,3,4),(0.,4.40000041065377E-5,
9.89910850773114E-5),.UNSPECIFIED.);
#26330=B_SPLINE_CURVE_WITH_KNOTS('',3,(#429665,#429666,#429667,#429668,
#429669,#429670,#429671,#429672,#429673,#429674,#429675,#429676,#429677,
#429678,#429679,#429680,#429681,#429682,#429683,#429684,#429685,#429686,
#429687,#429688,#429689,#429690,#429691,#429692,#429693,#429694,#429695,
#429696,#429697,#429698),.UNSPECIFIED.,.F.,.F.,(4,3,3,3,3,3,3,3,3,3,3,4),
(0.,4.29157837304062E-6,5.42772623795341E-6,1.00901698482346E-5,1.31279195068639E-5,
1.57383542265844E-5,1.61011507492103E-5,1.6716678929175E-5,1.95343262811355E-5,
2.29377234674645E-5,2.71556047620055E-5,3.34407099942655E-5),
 .UNSPECIFIED.);
#26331=B_SPLINE_CURVE_WITH_KNOTS('',3,(#429711,#429712,#429713,#429714,
#429715,#429716,#429717,#429718,#429719,#429720,#429721,#429722,#429723,
#429724,#429725,#429726,#429727,#429728,#429729,#429730,#429731,#429732,
#429733,#429734,#429735,#429736,#429737,#429738,#429739,#429740,#429741,
#429742,#429743,#429744),.UNSPECIFIED.,.F.,.F.,(4,3,3,3,3,3,3,3,3,3,3,4),
(2.16840434497101E-19,3.71309426656627E-6,5.39981071559405E-6,8.78933289328103E-6,
9.00272357067521E-6,1.0714398450415E-5,1.60780299679534E-5,1.65806081157689E-5,
2.30369726850297E-5,2.6781920041609E-5,3.59736924188219E-5,4.03862783807006E-5),
 .UNSPECIFIED.);
#26332=B_SPLINE_CURVE_WITH_KNOTS('',3,(#429857,#429858,#429859,#429860),
 .UNSPECIFIED.,.F.,.F.,(4,4),(0.,7.70025630629241E-5),.UNSPECIFIED.);
#26333=B_SPLINE_CURVE_WITH_KNOTS('',3,(#429870,#429871,#429872,#429873),
 .UNSPECIFIED.,.F.,.F.,(4,4),(4.33680868994202E-19,7.70025630629237E-5),
 .UNSPECIFIED.);
#26334=B_SPLINE_CURVE_WITH_KNOTS('',3,(#429877,#429878,#429879,#429880,
#429881,#429882,#429883,#429884,#429885,#429886,#429887,#429888,#429889,
#429890,#429891,#429892,#429893,#429894,#429895,#429896,#429897,#429898,
#429899,#429900,#429901,#429902,#429903,#429904,#429905,#429906,#429907,
#429908,#429909,#429910,#429911,#429912,#429913),.UNSPECIFIED.,.F.,.F.,
(4,3,3,3,3,3,3,3,3,3,3,3,4),(0.,9.5903152720102E-6,1.94769411223118E-5,
2.02405092183152E-5,3.21374138577704E-5,3.6030219507044E-5,4.42640648818753E-5,
4.53660204229444E-5,5.03633762302121E-5,5.17708036292897E-5,5.3792899385199E-5,
5.541037554602E-5,5.645578895115E-5),.UNSPECIFIED.);
#26335=B_SPLINE_CURVE_WITH_KNOTS('',3,(#429914,#429915,#429916,#429917,
#429918,#429919,#429920,#429921,#429922,#429923,#429924,#429925,#429926,
#429927,#429928,#429929,#429930,#429931,#429932,#429933,#429934,#429935,
#429936,#429937,#429938,#429939,#429940,#429941),.UNSPECIFIED.,.F.,.F.,
(4,3,3,3,3,3,3,3,3,4),(5.645578895115E-5,5.9894096649375E-5,6.34214003873382E-5,
7.22241476084637E-5,7.38322796533365E-5,8.36529189331475E-5,8.80714278222503E-5,
9.84837568500771E-5,0.000108624704079148,0.000110823272382854),
 .UNSPECIFIED.);
#26336=B_SPLINE_CURVE_WITH_KNOTS('',3,(#429957,#429958,#429959,#429960,
#429961,#429962,#429963,#429964,#429965,#429966,#429967,#429968,#429969,
#429970,#429971,#429972,#429973,#429974,#429975,#429976,#429977,#429978,
#429979,#429980,#429981,#429982,#429983,#429984),.UNSPECIFIED.,.F.,.F.,
(4,3,3,3,3,3,3,3,3,4),(0.,8.66039628582388E-6,1.64707715200666E-5,2.24502894132161E-5,
2.49975961757823E-5,2.8852600369028E-5,3.10661348995018E-5,3.43053543516958E-5,
3.6641054565356E-5,4.00504537627889E-5),.UNSPECIFIED.);
#26337=B_SPLINE_CURVE_WITH_KNOTS('',3,(#429987,#429988,#429989,#429990,
#429991,#429992,#429993),.UNSPECIFIED.,.F.,.F.,(4,3,4),(0.,4.40000041065375E-5,
9.89910850773112E-5),.UNSPECIFIED.);
#26338=B_SPLINE_CURVE_WITH_KNOTS('',3,(#430014,#430015,#430016,#430017,
#430018,#430019,#430020,#430021,#430022,#430023,#430024,#430025,#430026,
#430027,#430028,#430029,#430030,#430031,#430032,#430033,#430034,#430035,
#430036,#430037,#430038,#430039,#430040,#430041,#430042,#430043,#430044,
#430045,#430046,#430047),.UNSPECIFIED.,.F.,.F.,(4,3,3,3,3,3,3,3,3,3,3,4),
(0.,4.29157837304584E-6,5.42772623795323E-6,1.00901698482347E-5,1.31279195068638E-5,
1.57383542265883E-5,1.61011507492104E-5,1.67166789291758E-5,1.95343262811358E-5,
2.29377234674649E-5,2.71556047620058E-5,3.3440709994266E-5),
 .UNSPECIFIED.);
#26339=B_SPLINE_CURVE_WITH_KNOTS('',3,(#430060,#430061,#430062,#430063,
#430064,#430065,#430066,#430067,#430068,#430069,#430070,#430071,#430072,
#430073,#430074,#430075,#430076,#430077,#430078,#430079,#430080,#430081,
#430082,#430083,#430084,#430085,#430086,#430087,#430088,#430089,#430090,
#430091,#430092,#430093),.UNSPECIFIED.,.F.,.F.,(4,3,3,3,3,3,3,3,3,3,3,4),
(0.,3.71309426656669E-6,5.39981071559425E-6,8.78933289330839E-6,9.00272357067503E-6,
1.07143984504149E-5,1.6078029967955E-5,1.65806081157685E-5,2.30369726850441E-5,
2.67819200416079E-5,3.59736924187609E-5,4.03862783806989E-5),
 .UNSPECIFIED.);
#26340=B_SPLINE_CURVE_WITH_KNOTS('',3,(#430206,#430207,#430208,#430209),
 .UNSPECIFIED.,.F.,.F.,(4,4),(0.,7.70025630629237E-5),.UNSPECIFIED.);
#26341=B_SPLINE_CURVE_WITH_KNOTS('',3,(#430219,#430220,#430221,#430222),
 .UNSPECIFIED.,.F.,.F.,(4,4),(0.,7.70025630629239E-5),.UNSPECIFIED.);
#26342=B_SPLINE_CURVE_WITH_KNOTS('',3,(#430226,#430227,#430228,#430229,
#430230,#430231,#430232,#430233,#430234,#430235,#430236,#430237,#430238,
#430239,#430240,#430241,#430242,#430243,#430244,#430245,#430246,#430247,
#430248,#430249,#430250,#430251,#430252,#430253,#430254,#430255,#430256,
#430257,#430258,#430259,#430260,#430261,#430262),.UNSPECIFIED.,.F.,.F.,
(4,3,3,3,3,3,3,3,3,3,3,3,4),(0.,9.59031527199471E-6,1.94769411222829E-5,
2.02405092183151E-5,3.21374138577656E-5,3.60302195070439E-5,4.42640648818787E-5,
4.53660204229443E-5,5.03633762302059E-5,5.17708036292899E-5,5.37928993851987E-5,
5.54103755460193E-5,5.64557889511556E-5),.UNSPECIFIED.);
#26343=B_SPLINE_CURVE_WITH_KNOTS('',3,(#430263,#430264,#430265,#430266,
#430267,#430268,#430269,#430270,#430271,#430272,#430273,#430274,#430275,
#430276,#430277,#430278,#430279,#430280,#430281,#430282,#430283,#430284,
#430285,#430286,#430287,#430288,#430289,#430290),.UNSPECIFIED.,.F.,.F.,
(4,3,3,3,3,3,3,3,3,4),(5.64557889511556E-5,5.98940966493751E-5,6.34214003873379E-5,
7.22241476084211E-5,7.38322796533363E-5,8.3652918933143E-5,8.807142782225E-5,
9.84837568500654E-5,0.000108624704079118,0.000110823272382854),
 .UNSPECIFIED.);
#26344=B_SPLINE_CURVE_WITH_KNOTS('',3,(#430306,#430307,#430308,#430309,
#430310,#430311,#430312,#430313,#430314,#430315,#430316,#430317,#430318,
#430319,#430320,#430321,#430322,#430323,#430324,#430325,#430326,#430327,
#430328,#430329,#430330,#430331,#430332,#430333),.UNSPECIFIED.,.F.,.F.,
(4,3,3,3,3,3,3,3,3,4),(0.,8.660396285831E-6,1.64707715200666E-5,2.24502894132403E-5,
2.49975961757823E-5,2.8852600369028E-5,3.10661348995015E-5,3.43053543516961E-5,
3.66410545653561E-5,4.00504537627889E-5),.UNSPECIFIED.);
#26345=B_SPLINE_CURVE_WITH_KNOTS('',3,(#430336,#430337,#430338,#430339,
#430340,#430341,#430342),.UNSPECIFIED.,.F.,.F.,(4,3,4),(0.,4.40000041065374E-5,
9.89910850773116E-5),.UNSPECIFIED.);
#26346=B_SPLINE_CURVE_WITH_KNOTS('',3,(#430363,#430364,#430365,#430366,
#430367,#430368,#430369,#430370,#430371,#430372,#430373,#430374,#430375,
#430376,#430377,#430378,#430379,#430380,#430381,#430382,#430383,#430384,
#430385,#430386,#430387,#430388,#430389,#430390,#430391,#430392,#430393,
#430394,#430395,#430396),.UNSPECIFIED.,.F.,.F.,(4,3,3,3,3,3,3,3,3,3,3,4),
(0.,4.29157837303028E-6,5.42772623795317E-6,1.00901698482344E-5,1.31279195068634E-5,
1.57383542265872E-5,1.61011507492103E-5,1.67166789291751E-5,1.95343262811353E-5,
2.29377234674644E-5,2.71556047620053E-5,3.34407099942653E-5),
 .UNSPECIFIED.);
#26347=B_SPLINE_CURVE_WITH_KNOTS('',3,(#430409,#430410,#430411,#430412,
#430413,#430414,#430415,#430416,#430417,#430418,#430419,#430420,#430421,
#430422,#430423,#430424,#430425,#430426,#430427,#430428,#430429,#430430,
#430431,#430432,#430433,#430434,#430435,#430436,#430437,#430438,#430439,
#430440,#430441,#430442),.UNSPECIFIED.,.F.,.F.,(4,3,3,3,3,3,3,3,3,3,3,4),
(2.16840434497101E-19,3.71309426656678E-6,5.39981071559421E-6,8.78933289368528E-6,
9.00272357067521E-6,1.07143984504151E-5,1.60780299679553E-5,1.65806081157686E-5,
2.30369726850255E-5,2.67819200416087E-5,3.59736924188074E-5,4.03862783807002E-5),
 .UNSPECIFIED.);
#26348=B_SPLINE_CURVE_WITH_KNOTS('',3,(#430555,#430556,#430557,#430558),
 .UNSPECIFIED.,.F.,.F.,(4,4),(0.,7.7002563062924E-5),.UNSPECIFIED.);
#26349=B_SPLINE_CURVE_WITH_KNOTS('',3,(#430568,#430569,#430570,#430571),
 .UNSPECIFIED.,.F.,.F.,(4,4),(4.33680868994202E-19,7.70025630629234E-5),
 .UNSPECIFIED.);
#26350=B_SPLINE_CURVE_WITH_KNOTS('',3,(#430575,#430576,#430577,#430578,
#430579,#430580,#430581,#430582,#430583,#430584,#430585,#430586,#430587,
#430588,#430589,#430590,#430591,#430592,#430593,#430594,#430595,#430596,
#430597,#430598,#430599,#430600,#430601,#430602,#430603,#430604,#430605,
#430606,#430607,#430608,#430609,#430610,#430611),.UNSPECIFIED.,.F.,.F.,
(4,3,3,3,3,3,3,3,3,3,3,3,4),(0.,9.59031527198726E-6,1.94769411222748E-5,
2.0240509218315E-5,3.2137413857772E-5,3.60302195070436E-5,4.42640648818736E-5,
4.53660204229444E-5,5.03633762302037E-5,5.17708036292896E-5,5.3792899385199E-5,
5.54103755460196E-5,5.64557889513675E-5),.UNSPECIFIED.);
#26351=B_SPLINE_CURVE_WITH_KNOTS('',3,(#430612,#430613,#430614,#430615,
#430616,#430617,#430618,#430619,#430620,#430621,#430622,#430623,#430624,
#430625,#430626,#430627,#430628,#430629,#430630,#430631,#430632,#430633,
#430634,#430635,#430636,#430637,#430638,#430639),.UNSPECIFIED.,.F.,.F.,
(4,3,3,3,3,3,3,3,3,4),(5.64557889513675E-5,5.98940966493752E-5,6.34214003873379E-5,
7.22241476085083E-5,7.38322796533366E-5,8.36529189331453E-5,8.80714278222503E-5,
9.84837568500839E-5,0.000108624704079163,0.000110823272382854),
 .UNSPECIFIED.);
#26352=B_SPLINE_CURVE_WITH_KNOTS('',3,(#430655,#430656,#430657,#430658,
#430659,#430660,#430661,#430662,#430663,#430664,#430665,#430666,#430667,
#430668,#430669,#430670,#430671,#430672,#430673,#430674,#430675,#430676,
#430677,#430678,#430679,#430680,#430681,#430682),.UNSPECIFIED.,.F.,.F.,
(4,3,3,3,3,3,3,3,3,4),(0.,8.66039628583618E-6,1.64707715200666E-5,2.24502894132307E-5,
2.49975961757824E-5,2.88526003690281E-5,3.10661348995016E-5,3.43053543516959E-5,
3.66410545653561E-5,4.00504537627889E-5),.UNSPECIFIED.);
#26353=B_SPLINE_CURVE_WITH_KNOTS('',3,(#430685,#430686,#430687,#430688,
#430689,#430690,#430691),.UNSPECIFIED.,.F.,.F.,(4,3,4),(0.,4.40000041065375E-5,
9.89910850773113E-5),.UNSPECIFIED.);
#26354=B_SPLINE_CURVE_WITH_KNOTS('',3,(#430712,#430713,#430714,#430715,
#430716,#430717,#430718,#430719,#430720,#430721,#430722,#430723,#430724,
#430725,#430726,#430727,#430728,#430729,#430730,#430731,#430732,#430733,
#430734,#430735,#430736,#430737,#430738,#430739,#430740,#430741,#430742,
#430743,#430744,#430745),.UNSPECIFIED.,.F.,.F.,(4,3,3,3,3,3,3,3,3,3,3,4),
(0.,4.29157837303874E-6,5.42772623795334E-6,1.0090169848235E-5,1.31279195068638E-5,
1.57383542265808E-5,1.61011507492107E-5,1.67166789291761E-5,1.95343262811359E-5,
2.29377234674652E-5,2.71556047620062E-5,3.34407099942662E-5),
 .UNSPECIFIED.);
#26355=B_SPLINE_CURVE_WITH_KNOTS('',3,(#430758,#430759,#430760,#430761,
#430762,#430763,#430764,#430765,#430766,#430767,#430768,#430769,#430770,
#430771,#430772,#430773,#430774,#430775,#430776,#430777,#430778,#430779,
#430780,#430781,#430782,#430783,#430784,#430785,#430786,#430787,#430788,
#430789,#430790,#430791),.UNSPECIFIED.,.F.,.F.,(4,3,3,3,3,3,3,3,3,3,3,4),
(0.,3.71309426656648E-6,5.39981071559433E-6,8.78933289366858E-6,9.00272357067512E-6,
1.0714398450415E-5,1.60780299679577E-5,1.65806081157687E-5,2.3036972685043E-5,
2.67819200416086E-5,3.59736924187824E-5,4.03862783807001E-5),
 .UNSPECIFIED.);
#26356=B_SPLINE_CURVE_WITH_KNOTS('',3,(#430904,#430905,#430906,#430907),
 .UNSPECIFIED.,.F.,.F.,(4,4),(0.,7.70025630629237E-5),.UNSPECIFIED.);
#26357=B_SPLINE_CURVE_WITH_KNOTS('',3,(#430917,#430918,#430919,#430920),
 .UNSPECIFIED.,.F.,.F.,(4,4),(4.33680868994202E-19,7.70025630629238E-5),
 .UNSPECIFIED.);
#26358=B_SPLINE_CURVE_WITH_KNOTS('',3,(#430924,#430925,#430926,#430927,
#430928,#430929,#430930,#430931,#430932,#430933,#430934,#430935,#430936,
#430937,#430938,#430939,#430940,#430941,#430942,#430943,#430944,#430945,
#430946,#430947,#430948,#430949,#430950,#430951,#430952,#430953,#430954,
#430955,#430956,#430957,#430958,#430959,#430960),.UNSPECIFIED.,.F.,.F.,
(4,3,3,3,3,3,3,3,3,3,3,3,4),(0.,9.59031527200496E-6,1.94769411222924E-5,
2.02405092183151E-5,3.2137413857772E-5,3.6030219507044E-5,4.42640648817857E-5,
4.53660204229446E-5,5.03633762302157E-5,5.17708036292896E-5,5.37928993851989E-5,
5.54103755460198E-5,5.64557889510994E-5),.UNSPECIFIED.);
#26359=B_SPLINE_CURVE_WITH_KNOTS('',3,(#430961,#430962,#430963,#430964,
#430965,#430966,#430967,#430968,#430969,#430970,#430971,#430972,#430973,
#430974,#430975,#430976,#430977,#430978,#430979,#430980,#430981,#430982,
#430983,#430984,#430985,#430986,#430987,#430988),.UNSPECIFIED.,.F.,.F.,
(4,3,3,3,3,3,3,3,3,4),(5.64557889510994E-5,5.98940966493752E-5,6.34214003873382E-5,
7.22241476084606E-5,7.38322796533366E-5,8.36529189331425E-5,8.80714278222502E-5,
9.84837568500645E-5,0.000108624704079118,0.000110823272382854),
 .UNSPECIFIED.);
#26360=B_SPLINE_CURVE_WITH_KNOTS('',3,(#431004,#431005,#431006,#431007,
#431008,#431009,#431010,#431011,#431012,#431013,#431014,#431015,#431016,
#431017,#431018,#431019,#431020,#431021,#431022,#431023,#431024,#431025,
#431026,#431027,#431028,#431029,#431030,#431031),.UNSPECIFIED.,.F.,.F.,
(4,3,3,3,3,3,3,3,3,4),(0.,8.66039628580277E-6,1.6470771520067E-5,2.24502894132263E-5,
2.49975961757828E-5,2.88526003690287E-5,3.10661348995023E-5,3.43053543516968E-5,
3.66410545653568E-5,4.0050453762789E-5),.UNSPECIFIED.);
#26361=B_SPLINE_CURVE_WITH_KNOTS('',3,(#431034,#431035,#431036,#431037,
#431038,#431039,#431040),.UNSPECIFIED.,.F.,.F.,(4,3,4),(0.,4.40000041065373E-5,
9.89910850773113E-5),.UNSPECIFIED.);
#26362=B_SPLINE_CURVE_WITH_KNOTS('',3,(#431061,#431062,#431063,#431064,
#431065,#431066,#431067,#431068,#431069,#431070,#431071,#431072,#431073,
#431074,#431075,#431076,#431077,#431078,#431079,#431080,#431081,#431082,
#431083,#431084,#431085,#431086,#431087,#431088,#431089,#431090,#431091,
#431092,#431093,#431094),.UNSPECIFIED.,.F.,.F.,(4,3,3,3,3,3,3,3,3,3,3,4),
(0.,4.29157837304175E-6,5.42772623795323E-6,1.00901698482348E-5,1.31279195068639E-5,
1.57383542265785E-5,1.61011507492102E-5,1.67166789291755E-5,1.95343262811357E-5,
2.29377234674649E-5,2.71556047620058E-5,3.34407099942656E-5),
 .UNSPECIFIED.);
#26363=B_SPLINE_CURVE_WITH_KNOTS('',3,(#431107,#431108,#431109,#431110,
#431111,#431112,#431113,#431114,#431115,#431116,#431117,#431118,#431119,
#431120,#431121,#431122,#431123,#431124,#431125,#431126,#431127,#431128,
#431129,#431130,#431131,#431132,#431133,#431134,#431135,#431136,#431137,
#431138,#431139,#431140),.UNSPECIFIED.,.F.,.F.,(4,3,3,3,3,3,3,3,3,3,3,4),
(0.,3.71309426656655E-6,5.39981071559422E-6,8.7893328936629E-6,9.00272357067514E-6,
1.07143984504147E-5,1.60780299679635E-5,1.65806081157687E-5,2.30369726850508E-5,
2.67819200416086E-5,3.59736924187397E-5,4.03862783806999E-5),
 .UNSPECIFIED.);
#26364=B_SPLINE_CURVE_WITH_KNOTS('',3,(#431253,#431254,#431255,#431256),
 .UNSPECIFIED.,.F.,.F.,(4,4),(0.,7.70025630629239E-5),.UNSPECIFIED.);
#26365=B_SPLINE_CURVE_WITH_KNOTS('',3,(#431266,#431267,#431268,#431269),
 .UNSPECIFIED.,.F.,.F.,(4,4),(4.33680868994202E-19,7.70025630629236E-5),
 .UNSPECIFIED.);
#26366=B_SPLINE_CURVE_WITH_KNOTS('',3,(#431273,#431274,#431275,#431276,
#431277,#431278,#431279,#431280,#431281,#431282,#431283,#431284,#431285,
#431286,#431287,#431288,#431289,#431290,#431291,#431292,#431293,#431294,
#431295,#431296,#431297,#431298,#431299,#431300,#431301,#431302,#431303,
#431304,#431305,#431306,#431307,#431308,#431309),.UNSPECIFIED.,.F.,.F.,
(4,3,3,3,3,3,3,3,3,3,3,3,4),(0.,9.5903152720047E-6,1.94769411222842E-5,
2.0240509218315E-5,3.21374138577764E-5,3.6030219507044E-5,4.42640648818235E-5,
4.53660204229444E-5,5.0363376230219E-5,5.17708036292897E-5,5.37928993851989E-5,
5.54103755460197E-5,5.64557889508719E-5),.UNSPECIFIED.);
#26367=B_SPLINE_CURVE_WITH_KNOTS('',3,(#431310,#431311,#431312,#431313,
#431314,#431315,#431316,#431317,#431318,#431319,#431320,#431321,#431322,
#431323,#431324,#431325,#431326,#431327,#431328,#431329,#431330,#431331,
#431332,#431333,#431334,#431335,#431336,#431337),.UNSPECIFIED.,.F.,.F.,
(4,3,3,3,3,3,3,3,3,4),(5.64557889508719E-5,5.98940966493751E-5,6.3421400387338E-5,
7.22241476084641E-5,7.38322796533365E-5,8.36529189331414E-5,8.80714278222502E-5,
9.848375685006E-5,0.000108624704079087,0.000110823272382854),
 .UNSPECIFIED.);
#26368=B_SPLINE_CURVE_WITH_KNOTS('',3,(#431353,#431354,#431355,#431356,
#431357,#431358,#431359,#431360,#431361,#431362,#431363,#431364,#431365,
#431366,#431367,#431368,#431369,#431370,#431371,#431372,#431373,#431374,
#431375,#431376,#431377,#431378,#431379,#431380),.UNSPECIFIED.,.F.,.F.,
(4,3,3,3,3,3,3,3,3,4),(0.,8.66039628582158E-6,1.64707715200665E-5,2.24502894132426E-5,
2.49975961757824E-5,2.88526003690279E-5,3.10661348995016E-5,3.43053543516961E-5,
3.66410545653559E-5,4.00504537627885E-5),.UNSPECIFIED.);
#26369=B_SPLINE_CURVE_WITH_KNOTS('',3,(#431383,#431384,#431385,#431386,
#431387,#431388,#431389),.UNSPECIFIED.,.F.,.F.,(4,3,4),(0.,4.40000041065374E-5,
9.89910850773113E-5),.UNSPECIFIED.);
#26370=B_SPLINE_CURVE_WITH_KNOTS('',3,(#431410,#431411,#431412,#431413,
#431414,#431415,#431416,#431417,#431418,#431419,#431420,#431421,#431422,
#431423,#431424,#431425,#431426,#431427,#431428,#431429,#431430,#431431,
#431432,#431433,#431434,#431435,#431436,#431437,#431438,#431439,#431440,
#431441,#431442,#431443),.UNSPECIFIED.,.F.,.F.,(4,3,3,3,3,3,3,3,3,3,3,4),
(0.,4.29157837304048E-6,5.42772623795318E-6,1.00901698482346E-5,1.31279195068639E-5,
1.57383542265845E-5,1.61011507492104E-5,1.67166789291754E-5,1.95343262811357E-5,
2.29377234674649E-5,2.7155604762006E-5,3.34407099942659E-5),
 .UNSPECIFIED.);
#26371=B_SPLINE_CURVE_WITH_KNOTS('',3,(#431456,#431457,#431458,#431459,
#431460,#431461,#431462,#431463,#431464,#431465,#431466,#431467,#431468,
#431469,#431470,#431471,#431472,#431473,#431474,#431475,#431476,#431477,
#431478,#431479,#431480,#431481,#431482,#431483,#431484,#431485,#431486,
#431487,#431488,#431489),.UNSPECIFIED.,.F.,.F.,(4,3,3,3,3,3,3,3,3,3,3,4),
(0.,3.71309426656658E-6,5.39981071559416E-6,8.78933289367644E-6,9.00272357067511E-6,
1.07143984504147E-5,1.6078029967954E-5,1.65806081157684E-5,2.30369726850593E-5,
2.67819200416081E-5,3.59736924187712E-5,4.03862783806992E-5),
 .UNSPECIFIED.);
#26372=B_SPLINE_CURVE_WITH_KNOTS('',3,(#431602,#431603,#431604,#431605),
 .UNSPECIFIED.,.F.,.F.,(4,4),(0.,7.7002563062924E-5),.UNSPECIFIED.);
#26373=B_SPLINE_CURVE_WITH_KNOTS('',3,(#431615,#431616,#431617,#431618),
 .UNSPECIFIED.,.F.,.F.,(4,4),(4.33680868994202E-19,7.70025630629234E-5),
 .UNSPECIFIED.);
#26374=B_SPLINE_CURVE_WITH_KNOTS('',3,(#431622,#431623,#431624,#431625,
#431626,#431627,#431628,#431629,#431630,#431631,#431632,#431633,#431634,
#431635,#431636,#431637,#431638,#431639,#431640,#431641,#431642,#431643,
#431644,#431645,#431646,#431647,#431648,#431649,#431650,#431651,#431652,
#431653,#431654,#431655,#431656,#431657,#431658),.UNSPECIFIED.,.F.,.F.,
(4,3,3,3,3,3,3,3,3,3,3,3,4),(0.,9.59031527200327E-6,1.94769411222958E-5,
2.02405092183153E-5,3.21374138577732E-5,3.60302195070438E-5,4.42640648818343E-5,
4.53660204229444E-5,5.03633762302119E-5,5.17708036292895E-5,5.37928993851989E-5,
5.54103755460195E-5,5.64557889510178E-5),.UNSPECIFIED.);
#26375=B_SPLINE_CURVE_WITH_KNOTS('',3,(#431659,#431660,#431661,#431662,
#431663,#431664,#431665,#431666,#431667,#431668,#431669,#431670,#431671,
#431672,#431673,#431674,#431675,#431676,#431677,#431678,#431679,#431680,
#431681,#431682,#431683,#431684,#431685,#431686),.UNSPECIFIED.,.F.,.F.,
(4,3,3,3,3,3,3,3,3,4),(5.64557889510178E-5,5.9894096649375E-5,6.34214003873379E-5,
7.22241476083772E-5,7.38322796533363E-5,8.36529189331363E-5,8.80714278222497E-5,
9.84837568500626E-5,0.000108624704079122,0.000110823272382853),
 .UNSPECIFIED.);
#26376=B_SPLINE_CURVE_WITH_KNOTS('',3,(#431702,#431703,#431704,#431705,
#431706,#431707,#431708,#431709,#431710,#431711,#431712,#431713,#431714,
#431715,#431716,#431717,#431718,#431719,#431720,#431721,#431722,#431723,
#431724,#431725,#431726,#431727,#431728,#431729),.UNSPECIFIED.,.F.,.F.,
(4,3,3,3,3,3,3,3,3,4),(0.,8.66039628581431E-6,1.64707715200667E-5,2.24502894132164E-5,
2.49975961757824E-5,2.88526003690281E-5,3.10661348995016E-5,3.4305354351696E-5,
3.6641054565356E-5,4.00504537627885E-5),.UNSPECIFIED.);
#26377=B_SPLINE_CURVE_WITH_KNOTS('',3,(#431732,#431733,#431734,#431735,
#431736,#431737,#431738),.UNSPECIFIED.,.F.,.F.,(4,3,4),(0.,4.4000004106538E-5,
9.89910850773115E-5),.UNSPECIFIED.);
#26378=B_SPLINE_CURVE_WITH_KNOTS('',3,(#431759,#431760,#431761,#431762,
#431763,#431764,#431765,#431766,#431767,#431768,#431769,#431770,#431771,
#431772,#431773,#431774,#431775,#431776,#431777,#431778,#431779,#431780,
#431781,#431782,#431783,#431784,#431785,#431786,#431787,#431788,#431789,
#431790,#431791,#431792),.UNSPECIFIED.,.F.,.F.,(4,3,3,3,3,3,3,3,3,3,3,4),
(0.,4.29157837304129E-6,5.42772623795345E-6,1.00901698482348E-5,1.3127919506864E-5,
1.57383542265835E-5,1.61011507492105E-5,1.67166789291752E-5,1.95343262811359E-5,
2.2937723467465E-5,2.71556047620058E-5,3.34407099942656E-5),
 .UNSPECIFIED.);
#26379=B_SPLINE_CURVE_WITH_KNOTS('',3,(#431805,#431806,#431807,#431808,
#431809,#431810,#431811,#431812,#431813,#431814,#431815,#431816,#431817,
#431818,#431819,#431820,#431821,#431822,#431823,#431824,#431825,#431826,
#431827,#431828,#431829,#431830,#431831,#431832,#431833,#431834,#431835,
#431836,#431837,#431838),.UNSPECIFIED.,.F.,.F.,(4,3,3,3,3,3,3,3,3,3,3,4),
(0.,3.71309426656657E-6,5.3998107155942E-6,8.78933289368234E-6,9.00272357067517E-6,
1.07143984504149E-5,1.60780299679592E-5,1.65806081157687E-5,2.30369726850617E-5,
2.67819200416084E-5,3.59736924187323E-5,4.03862783806997E-5),
 .UNSPECIFIED.);
#26380=B_SPLINE_CURVE_WITH_KNOTS('',3,(#431951,#431952,#431953,#431954),
 .UNSPECIFIED.,.F.,.F.,(4,4),(0.,7.7002563062924E-5),.UNSPECIFIED.);
#26381=B_SPLINE_CURVE_WITH_KNOTS('',3,(#431964,#431965,#431966,#431967),
 .UNSPECIFIED.,.F.,.F.,(4,4),(4.33680868994202E-19,7.70025630629234E-5),
 .UNSPECIFIED.);
#26382=B_SPLINE_CURVE_WITH_KNOTS('',3,(#431971,#431972,#431973,#431974,
#431975,#431976,#431977,#431978,#431979,#431980,#431981,#431982,#431983,
#431984,#431985,#431986,#431987,#431988,#431989,#431990,#431991,#431992,
#431993,#431994,#431995,#431996,#431997,#431998,#431999,#432000,#432001,
#432002,#432003,#432004,#432005,#432006,#432007),.UNSPECIFIED.,.F.,.F.,
(4,3,3,3,3,3,3,3,3,3,3,3,4),(0.,9.5903152720082E-6,1.94769411223113E-5,
2.02405092183154E-5,3.21374138577727E-5,3.60302195070441E-5,4.42640648818362E-5,
4.53660204229446E-5,5.03633762302027E-5,5.17708036292899E-5,5.37928993851991E-5,
5.54103755460203E-5,5.64557889513793E-5),.UNSPECIFIED.);
#26383=B_SPLINE_CURVE_WITH_KNOTS('',3,(#432008,#432009,#432010,#432011,
#432012,#432013,#432014,#432015,#432016,#432017,#432018,#432019,#432020,
#432021,#432022,#432023,#432024,#432025,#432026,#432027,#432028,#432029,
#432030,#432031,#432032,#432033,#432034,#432035),.UNSPECIFIED.,.F.,.F.,
(4,3,3,3,3,3,3,3,3,4),(5.64557889513793E-5,5.98940966493753E-5,6.34214003873382E-5,
7.22241476083956E-5,7.38322796533367E-5,8.36529189331575E-5,8.80714278222504E-5,
9.84837568501053E-5,0.000108624704079197,0.000110823272382854),
 .UNSPECIFIED.);
#26384=B_SPLINE_CURVE_WITH_KNOTS('',3,(#432051,#432052,#432053,#432054,
#432055,#432056,#432057,#432058,#432059,#432060,#432061,#432062,#432063,
#432064,#432065,#432066,#432067,#432068,#432069,#432070,#432071,#432072,
#432073,#432074,#432075,#432076,#432077,#432078),.UNSPECIFIED.,.F.,.F.,
(4,3,3,3,3,3,3,3,3,4),(0.,8.66039628578029E-6,1.64707715200667E-5,2.24502894132172E-5,
2.49975961757824E-5,2.8852600369028E-5,3.10661348995016E-5,3.4305354351696E-5,
3.66410545653558E-5,4.00504537627886E-5),.UNSPECIFIED.);
#26385=B_SPLINE_CURVE_WITH_KNOTS('',3,(#432081,#432082,#432083,#432084,
#432085,#432086,#432087),.UNSPECIFIED.,.F.,.F.,(4,3,4),(0.,4.40000041065376E-5,
9.8991085077311E-5),.UNSPECIFIED.);
#26386=B_SPLINE_CURVE_WITH_KNOTS('',3,(#432108,#432109,#432110,#432111,
#432112,#432113,#432114,#432115,#432116,#432117,#432118,#432119,#432120,
#432121,#432122,#432123,#432124,#432125,#432126,#432127,#432128,#432129,
#432130,#432131,#432132,#432133,#432134,#432135,#432136,#432137,#432138,
#432139,#432140,#432141),.UNSPECIFIED.,.F.,.F.,(4,3,3,3,3,3,3,3,3,3,3,4),
(0.,4.29157837303255E-6,5.42772623795373E-6,1.00901698482351E-5,1.31279195068643E-5,
1.57383542265874E-5,1.61011507492108E-5,1.67166789291762E-5,1.95343262811362E-5,
2.29377234674652E-5,2.71556047620063E-5,3.34407099942663E-5),
 .UNSPECIFIED.);
#26387=B_SPLINE_CURVE_WITH_KNOTS('',3,(#432154,#432155,#432156,#432157,
#432158,#432159,#432160,#432161,#432162,#432163,#432164,#432165,#432166,
#432167,#432168,#432169,#432170,#432171,#432172,#432173,#432174,#432175,
#432176,#432177,#432178,#432179,#432180,#432181,#432182,#432183,#432184,
#432185,#432186,#432187),.UNSPECIFIED.,.F.,.F.,(4,3,3,3,3,3,3,3,3,3,3,4),
(1.0842021724855E-19,3.71309426656634E-6,5.39981071559413E-6,8.78933289367088E-6,
9.00272357067501E-6,1.07143984504148E-5,1.60780299679518E-5,1.65806081157686E-5,
2.30369726850616E-5,2.67819200416086E-5,3.59736924187708E-5,4.03862783807001E-5),
 .UNSPECIFIED.);
#26388=B_SPLINE_CURVE_WITH_KNOTS('',3,(#432300,#432301,#432302,#432303),
 .UNSPECIFIED.,.F.,.F.,(4,4),(0.,7.70025630629239E-5),.UNSPECIFIED.);
#26389=B_SPLINE_CURVE_WITH_KNOTS('',3,(#432313,#432314,#432315,#432316),
 .UNSPECIFIED.,.F.,.F.,(4,4),(4.37055868292169E-19,7.70025630629237E-5),
 .UNSPECIFIED.);
#26390=B_SPLINE_CURVE_WITH_KNOTS('',3,(#432320,#432321,#432322,#432323,
#432324,#432325,#432326,#432327,#432328,#432329,#432330,#432331,#432332,
#432333,#432334,#432335,#432336,#432337,#432338,#432339,#432340,#432341,
#432342,#432343,#432344,#432345,#432346,#432347,#432348,#432349,#432350,
#432351,#432352,#432353,#432354,#432355,#432356),.UNSPECIFIED.,.F.,.F.,
(4,3,3,3,3,3,3,3,3,3,3,3,4),(0.,9.59031527200674E-6,1.94769411222978E-5,
2.02405092183151E-5,3.21374138577751E-5,3.60302195070439E-5,4.42640648818341E-5,
4.53660204229443E-5,5.03633762302115E-5,5.17708036292897E-5,5.37928993851989E-5,
5.54103755460201E-5,5.64557889514343E-5),.UNSPECIFIED.);
#26391=B_SPLINE_CURVE_WITH_KNOTS('',3,(#432357,#432358,#432359,#432360,
#432361,#432362,#432363,#432364,#432365,#432366,#432367,#432368,#432369,
#432370,#432371,#432372,#432373,#432374,#432375,#432376,#432377,#432378,
#432379,#432380,#432381,#432382,#432383,#432384),.UNSPECIFIED.,.F.,.F.,
(4,3,3,3,3,3,3,3,3,4),(5.64557889514343E-5,5.98940966493752E-5,6.34214003873381E-5,
7.22241476084827E-5,7.38322796533365E-5,8.36529189331353E-5,8.80714278222501E-5,
9.84837568500637E-5,0.00010862470407912,0.000110823272382854),
 .UNSPECIFIED.);
#26392=B_SPLINE_CURVE_WITH_KNOTS('',3,(#432400,#432401,#432402,#432403,
#432404,#432405,#432406,#432407,#432408,#432409,#432410,#432411,#432412,
#432413,#432414,#432415,#432416,#432417,#432418,#432419,#432420,#432421,
#432422,#432423,#432424,#432425,#432426,#432427),.UNSPECIFIED.,.F.,.F.,
(4,3,3,3,3,3,3,3,3,4),(0.,8.66039628582544E-6,1.64707715200667E-5,2.24502894132273E-5,
2.49975961757824E-5,2.88526003690281E-5,3.10661348995017E-5,3.43053543516961E-5,
3.66410545653561E-5,4.0050453762789E-5),.UNSPECIFIED.);
#26393=B_SPLINE_CURVE_WITH_KNOTS('',3,(#432430,#432431,#432432,#432433,
#432434,#432435,#432436),.UNSPECIFIED.,.F.,.F.,(4,3,4),(0.,4.40000041065379E-5,
9.89910850773112E-5),.UNSPECIFIED.);
#26394=B_SPLINE_CURVE_WITH_KNOTS('',3,(#432457,#432458,#432459,#432460,
#432461,#432462,#432463,#432464,#432465,#432466,#432467,#432468,#432469,
#432470,#432471,#432472,#432473,#432474,#432475,#432476,#432477,#432478,
#432479,#432480,#432481,#432482,#432483,#432484,#432485,#432486,#432487,
#432488,#432489,#432490),.UNSPECIFIED.,.F.,.F.,(4,3,3,3,3,3,3,3,3,3,3,4),
(0.,4.29157837302454E-6,5.4277262379536E-6,1.0090169848235E-5,1.31279195068642E-5,
1.57383542265848E-5,1.61011507492107E-5,1.6716678929176E-5,1.95343262811362E-5,
2.29377234674653E-5,2.71556047620063E-5,3.34407099942665E-5),
 .UNSPECIFIED.);
#26395=B_SPLINE_CURVE_WITH_KNOTS('',3,(#432503,#432504,#432505,#432506,
#432507,#432508,#432509,#432510,#432511,#432512,#432513,#432514,#432515,
#432516,#432517,#432518,#432519,#432520,#432521,#432522,#432523,#432524,
#432525,#432526,#432527,#432528,#432529,#432530,#432531,#432532,#432533,
#432534,#432535,#432536),.UNSPECIFIED.,.F.,.F.,(4,3,3,3,3,3,3,3,3,3,3,4),
(1.0842021724855E-19,3.71309426656643E-6,5.3998107155941E-6,8.78933289366509E-6,
9.00272357067505E-6,1.07143984504149E-5,1.60780299679579E-5,1.65806081157687E-5,
2.30369726850607E-5,2.67819200416085E-5,3.59736924187652E-5,4.03862783807E-5),
 .UNSPECIFIED.);
#26396=B_SPLINE_CURVE_WITH_KNOTS('',3,(#432649,#432650,#432651,#432652),
 .UNSPECIFIED.,.F.,.F.,(4,4),(0.,7.70025630629241E-5),.UNSPECIFIED.);
#26397=B_SPLINE_CURVE_WITH_KNOTS('',3,(#432662,#432663,#432664,#432665),
 .UNSPECIFIED.,.F.,.F.,(4,4),(4.41238316394827E-19,7.70025630629235E-5),
 .UNSPECIFIED.);
#26398=B_SPLINE_CURVE_WITH_KNOTS('',3,(#432669,#432670,#432671,#432672,
#432673,#432674,#432675,#432676,#432677,#432678,#432679,#432680,#432681,
#432682,#432683,#432684,#432685,#432686,#432687,#432688,#432689,#432690,
#432691,#432692,#432693,#432694,#432695,#432696,#432697,#432698,#432699,
#432700,#432701,#432702,#432703,#432704,#432705),.UNSPECIFIED.,.F.,.F.,
(4,3,3,3,3,3,3,3,3,3,3,3,4),(0.,9.59031527197544E-6,1.94769411222578E-5,
2.02405092183153E-5,3.21374138577708E-5,3.6030219507044E-5,4.42640648818711E-5,
4.53660204229444E-5,5.03633762302043E-5,5.17708036292896E-5,5.37928993851989E-5,
5.54103755460198E-5,5.64557889511408E-5),.UNSPECIFIED.);
#26399=B_SPLINE_CURVE_WITH_KNOTS('',3,(#432706,#432707,#432708,#432709,
#432710,#432711,#432712,#432713,#432714,#432715,#432716,#432717,#432718,
#432719,#432720,#432721,#432722,#432723,#432724,#432725,#432726,#432727,
#432728,#432729,#432730,#432731,#432732,#432733),.UNSPECIFIED.,.F.,.F.,
(4,3,3,3,3,3,3,3,3,4),(5.64557889511408E-5,5.98940966493751E-5,6.3421400387338E-5,
7.22241476085115E-5,7.38322796533365E-5,8.36529189331405E-5,8.807142782225E-5,
9.84837568500711E-5,0.00010862470407914,0.000110823272382853),
 .UNSPECIFIED.);
#26400=B_SPLINE_CURVE_WITH_KNOTS('',3,(#432749,#432750,#432751,#432752,
#432753,#432754,#432755,#432756,#432757,#432758,#432759,#432760,#432761,
#432762,#432763,#432764,#432765,#432766,#432767,#432768,#432769,#432770,
#432771,#432772,#432773,#432774,#432775,#432776),.UNSPECIFIED.,.F.,.F.,
(4,3,3,3,3,3,3,3,3,4),(0.,8.66039628581856E-6,1.64707715200667E-5,2.24502894132393E-5,
2.49975961757824E-5,2.88526003690281E-5,3.10661348995016E-5,3.43053543516961E-5,
3.6641054565356E-5,4.0050453762789E-5),.UNSPECIFIED.);
#26401=B_SPLINE_CURVE_WITH_KNOTS('',3,(#432779,#432780,#432781,#432782,
#432783,#432784,#432785),.UNSPECIFIED.,.F.,.F.,(4,3,4),(0.,4.40000041065371E-5,
9.89910850773111E-5),.UNSPECIFIED.);
#26402=B_SPLINE_CURVE_WITH_KNOTS('',3,(#432806,#432807,#432808,#432809,
#432810,#432811,#432812,#432813,#432814,#432815,#432816,#432817,#432818,
#432819,#432820,#432821,#432822,#432823,#432824,#432825,#432826,#432827,
#432828,#432829,#432830,#432831,#432832,#432833,#432834,#432835,#432836,
#432837,#432838,#432839),.UNSPECIFIED.,.F.,.F.,(4,3,3,3,3,3,3,3,3,3,3,4),
(0.,4.29157837305563E-6,5.4277262379533E-6,1.00901698482349E-5,1.3127919506864E-5,
1.57383542265875E-5,1.61011507492106E-5,1.67166789291755E-5,1.9534326281136E-5,
2.29377234674649E-5,2.7155604762006E-5,3.34407099942659E-5),
 .UNSPECIFIED.);
#26403=B_SPLINE_CURVE_WITH_KNOTS('',3,(#432852,#432853,#432854,#432855,
#432856,#432857,#432858,#432859,#432860,#432861,#432862,#432863,#432864,
#432865,#432866,#432867,#432868,#432869,#432870,#432871,#432872,#432873,
#432874,#432875,#432876,#432877,#432878,#432879,#432880,#432881,#432882,
#432883,#432884,#432885),.UNSPECIFIED.,.F.,.F.,(4,3,3,3,3,3,3,3,3,3,3,4),
(1.0842021724855E-19,3.71309426656642E-6,5.39981071559414E-6,8.78933289363548E-6,
9.00272357067524E-6,1.0714398450415E-5,1.60780299679622E-5,1.65806081157688E-5,
2.30369726850369E-5,2.67819200416088E-5,3.59736924187517E-5,4.03862783807003E-5),
 .UNSPECIFIED.);
#26404=B_SPLINE_CURVE_WITH_KNOTS('',3,(#432998,#432999,#433000,#433001),
 .UNSPECIFIED.,.F.,.F.,(4,4),(0.,7.70025630629241E-5),.UNSPECIFIED.);
#26405=B_SPLINE_CURVE_WITH_KNOTS('',3,(#433011,#433012,#433013,#433014),
 .UNSPECIFIED.,.F.,.F.,(4,4),(4.42537225052217E-19,7.70025630629237E-5),
 .UNSPECIFIED.);
#26406=B_SPLINE_CURVE_WITH_KNOTS('',3,(#433018,#433019,#433020,#433021,
#433022,#433023,#433024,#433025,#433026,#433027,#433028,#433029,#433030,
#433031,#433032,#433033,#433034,#433035,#433036,#433037,#433038,#433039,
#433040,#433041,#433042,#433043,#433044,#433045,#433046,#433047,#433048,
#433049,#433050,#433051,#433052,#433053,#433054),.UNSPECIFIED.,.F.,.F.,
(4,3,3,3,3,3,3,3,3,3,3,3,4),(0.,9.59031527200432E-6,1.94769411222929E-5,
2.02405092183153E-5,3.21374138577673E-5,3.6030219507044E-5,4.42640648819217E-5,
4.53660204229445E-5,5.0363376230212E-5,5.17708036292897E-5,5.3792899385199E-5,
5.541037554602E-5,5.64557889509114E-5),.UNSPECIFIED.);
#26407=B_SPLINE_CURVE_WITH_KNOTS('',3,(#433055,#433056,#433057,#433058,
#433059,#433060,#433061,#433062,#433063,#433064,#433065,#433066,#433067,
#433068,#433069,#433070,#433071,#433072,#433073,#433074,#433075,#433076,
#433077,#433078,#433079,#433080,#433081,#433082),.UNSPECIFIED.,.F.,.F.,
(4,3,3,3,3,3,3,3,3,4),(5.64557889509114E-5,5.98940966493752E-5,6.34214003873381E-5,
7.22241476084362E-5,7.38322796533365E-5,8.36529189331371E-5,8.80714278222501E-5,
9.84837568500736E-5,0.000108624704079148,0.000110823272382854),
 .UNSPECIFIED.);
#26408=B_SPLINE_CURVE_WITH_KNOTS('',3,(#433098,#433099,#433100,#433101,
#433102,#433103,#433104,#433105,#433106,#433107,#433108,#433109,#433110,
#433111,#433112,#433113,#433114,#433115,#433116,#433117,#433118,#433119,
#433120,#433121,#433122,#433123,#433124,#433125),.UNSPECIFIED.,.F.,.F.,
(4,3,3,3,3,3,3,3,3,4),(0.,8.66039628583388E-6,1.64707715200667E-5,2.24502894132186E-5,
2.49975961757824E-5,2.88526003690281E-5,3.10661348995016E-5,3.4305354351696E-5,
3.6641054565356E-5,4.00504537627888E-5),.UNSPECIFIED.);
#26409=B_SPLINE_CURVE_WITH_KNOTS('',3,(#433128,#433129,#433130,#433131,
#433132,#433133,#433134),.UNSPECIFIED.,.F.,.F.,(4,3,4),(0.,4.40000041065376E-5,
9.89910850773113E-5),.UNSPECIFIED.);
#26410=B_SPLINE_CURVE_WITH_KNOTS('',3,(#433155,#433156,#433157,#433158,
#433159,#433160,#433161,#433162,#433163,#433164,#433165,#433166,#433167,
#433168,#433169,#433170,#433171,#433172,#433173,#433174,#433175,#433176,
#433177,#433178,#433179,#433180,#433181,#433182,#433183,#433184,#433185,
#433186,#433187,#433188),.UNSPECIFIED.,.F.,.F.,(4,3,3,3,3,3,3,3,3,3,3,4),
(0.,4.2915783730512E-6,5.42772623795345E-6,1.00901698482349E-5,1.31279195068639E-5,
1.57383542265821E-5,1.61011507492105E-5,1.67166789291757E-5,1.9534326281136E-5,
2.2937723467465E-5,2.71556047620059E-5,3.3440709994266E-5),
 .UNSPECIFIED.);
#26411=B_SPLINE_CURVE_WITH_KNOTS('',3,(#433201,#433202,#433203,#433204,
#433205,#433206,#433207,#433208,#433209,#433210,#433211,#433212,#433213,
#433214,#433215,#433216,#433217,#433218,#433219,#433220,#433221,#433222,
#433223,#433224,#433225,#433226,#433227,#433228,#433229,#433230,#433231,
#433232,#433233,#433234),.UNSPECIFIED.,.F.,.F.,(4,3,3,3,3,3,3,3,3,3,3,4),
(9.48676900924816E-20,3.71309426656646E-6,5.39981071559417E-6,8.78933289365053E-6,
9.00272357067522E-6,1.07143984504149E-5,1.60780299679672E-5,1.65806081157687E-5,
2.30369726850437E-5,2.67819200416084E-5,3.59736924187517E-5,4.03862783806997E-5),
 .UNSPECIFIED.);
#26412=B_SPLINE_CURVE_WITH_KNOTS('',3,(#433347,#433348,#433349,#433350),
 .UNSPECIFIED.,.F.,.F.,(4,4),(0.,7.70025630629241E-5),.UNSPECIFIED.);
#26413=B_SPLINE_CURVE_WITH_KNOTS('',3,(#433360,#433361,#433362,#433363),
 .UNSPECIFIED.,.F.,.F.,(4,4),(4.47028007668187E-19,7.70025630629238E-5),
 .UNSPECIFIED.);
#26414=B_SPLINE_CURVE_WITH_KNOTS('',3,(#433367,#433368,#433369,#433370,
#433371,#433372,#433373,#433374,#433375,#433376,#433377,#433378,#433379,
#433380,#433381,#433382,#433383,#433384,#433385,#433386,#433387,#433388,
#433389,#433390,#433391,#433392,#433393,#433394,#433395,#433396,#433397,
#433398,#433399,#433400,#433401,#433402,#433403),.UNSPECIFIED.,.F.,.F.,
(4,3,3,3,3,3,3,3,3,3,3,3,4),(0.,9.59031527200568E-6,1.94769411222974E-5,
2.02405092183153E-5,3.21374138577626E-5,3.60302195070439E-5,4.42640648818366E-5,
4.53660204229444E-5,5.03633762302246E-5,5.17708036292896E-5,5.37928993851989E-5,
5.54103755460199E-5,5.64557889511924E-5),.UNSPECIFIED.);
#26415=B_SPLINE_CURVE_WITH_KNOTS('',3,(#433404,#433405,#433406,#433407,
#433408,#433409,#433410,#433411,#433412,#433413,#433414,#433415,#433416,
#433417,#433418,#433419,#433420,#433421,#433422,#433423,#433424,#433425,
#433426,#433427,#433428,#433429,#433430,#433431),.UNSPECIFIED.,.F.,.F.,
(4,3,3,3,3,3,3,3,3,4),(5.64557889511924E-5,5.98940966493751E-5,6.34214003873381E-5,
7.22241476084559E-5,7.38322796533365E-5,8.36529189331304E-5,8.80714278222502E-5,
9.84837568500671E-5,0.000108624704079125,0.000110823272382854),
 .UNSPECIFIED.);
#26416=B_SPLINE_CURVE_WITH_KNOTS('',3,(#433447,#433448,#433449,#433450,
#433451,#433452,#433453,#433454,#433455,#433456,#433457,#433458,#433459,
#433460,#433461,#433462,#433463,#433464,#433465,#433466,#433467,#433468,
#433469,#433470,#433471,#433472,#433473,#433474),.UNSPECIFIED.,.F.,.F.,
(4,3,3,3,3,3,3,3,3,4),(0.,8.66039628579021E-6,1.64707715200667E-5,2.2450289413231E-5,
2.49975961757823E-5,2.8852600369028E-5,3.10661348995015E-5,3.4305354351696E-5,
3.66410545653559E-5,4.00504537627887E-5),.UNSPECIFIED.);
#26417=B_SPLINE_CURVE_WITH_KNOTS('',3,(#433477,#433478,#433479,#433480,
#433481,#433482,#433483),.UNSPECIFIED.,.F.,.F.,(4,3,4),(0.,4.40000041065377E-5,
9.89910850773116E-5),.UNSPECIFIED.);
#26418=B_SPLINE_CURVE_WITH_KNOTS('',3,(#433504,#433505,#433506,#433507,
#433508,#433509,#433510,#433511,#433512,#433513,#433514,#433515,#433516,
#433517,#433518,#433519,#433520,#433521,#433522,#433523,#433524,#433525,
#433526,#433527,#433528,#433529,#433530,#433531,#433532,#433533,#433534,
#433535,#433536,#433537),.UNSPECIFIED.,.F.,.F.,(4,3,3,3,3,3,3,3,3,3,3,4),
(0.,4.29157837303811E-6,5.42772623795339E-6,1.00901698482347E-5,1.31279195068639E-5,
1.57383542265873E-5,1.61011507492103E-5,1.67166789291758E-5,1.95343262811359E-5,
2.29377234674646E-5,2.71556047620056E-5,3.34407099942658E-5),
 .UNSPECIFIED.);
#26419=B_SPLINE_CURVE_WITH_KNOTS('',3,(#433550,#433551,#433552,#433553,
#433554,#433555,#433556,#433557,#433558,#433559,#433560,#433561,#433562,
#433563,#433564,#433565,#433566,#433567,#433568,#433569,#433570,#433571,
#433572,#433573,#433574,#433575,#433576,#433577,#433578,#433579,#433580,
#433581,#433582,#433583),.UNSPECIFIED.,.F.,.F.,(4,3,3,3,3,3,3,3,3,3,3,4),
(8.13151629364128E-20,3.71309426656637E-6,5.3998107155941E-6,8.78933289331537E-6,
9.00272357067515E-6,1.07143984504149E-5,1.60780299679551E-5,1.65806081157687E-5,
2.30369726850453E-5,2.67819200416086E-5,3.59736924188064E-5,4.03862783807001E-5),
 .UNSPECIFIED.);
#26420=B_SPLINE_CURVE_WITH_KNOTS('',3,(#433696,#433697,#433698,#433699),
 .UNSPECIFIED.,.F.,.F.,(4,4),(0.,7.7002563062924E-5),.UNSPECIFIED.);
#26421=B_SPLINE_CURVE_WITH_KNOTS('',3,(#433709,#433710,#433711,#433712),
 .UNSPECIFIED.,.F.,.F.,(4,4),(4.47028007668187E-19,7.70025630629235E-5),
 .UNSPECIFIED.);
#26422=B_SPLINE_CURVE_WITH_KNOTS('',3,(#433716,#433717,#433718,#433719,
#433720,#433721,#433722,#433723,#433724,#433725,#433726,#433727,#433728,
#433729,#433730,#433731,#433732,#433733,#433734,#433735,#433736,#433737,
#433738,#433739,#433740,#433741,#433742,#433743,#433744,#433745,#433746,
#433747,#433748,#433749,#433750,#433751,#433752),.UNSPECIFIED.,.F.,.F.,
(4,3,3,3,3,3,3,3,3,3,3,3,4),(0.,9.59031527200619E-6,1.94769411222942E-5,
2.02405092183152E-5,3.21374138577641E-5,3.60302195070439E-5,4.4264064881794E-5,
4.53660204229443E-5,5.03633762302236E-5,5.17708036292896E-5,5.37928993851988E-5,
5.54103755460197E-5,5.64557889511151E-5),.UNSPECIFIED.);
#26423=B_SPLINE_CURVE_WITH_KNOTS('',3,(#433753,#433754,#433755,#433756,
#433757,#433758,#433759,#433760,#433761,#433762,#433763,#433764,#433765,
#433766,#433767,#433768,#433769,#433770,#433771,#433772,#433773,#433774,
#433775,#433776,#433777,#433778,#433779,#433780),.UNSPECIFIED.,.F.,.F.,
(4,3,3,3,3,3,3,3,3,4),(5.64557889511151E-5,5.9894096649375E-5,6.3421400387338E-5,
7.22241476084724E-5,7.38322796533362E-5,8.36529189331358E-5,8.80714278222499E-5,
9.84837568500631E-5,0.000108624704079119,0.000110823272382853),
 .UNSPECIFIED.);
#26424=B_SPLINE_CURVE_WITH_KNOTS('',3,(#433796,#433797,#433798,#433799,
#433800,#433801,#433802,#433803,#433804,#433805,#433806,#433807,#433808,
#433809,#433810,#433811,#433812,#433813,#433814,#433815,#433816,#433817,
#433818,#433819,#433820,#433821,#433822,#433823),.UNSPECIFIED.,.F.,.F.,
(4,3,3,3,3,3,3,3,3,4),(0.,8.66039628580801E-6,1.64707715200666E-5,2.24502894132537E-5,
2.49975961757824E-5,2.88526003690281E-5,3.10661348995017E-5,3.4305354351696E-5,
3.66410545653559E-5,4.00504537627886E-5),.UNSPECIFIED.);
#26425=B_SPLINE_CURVE_WITH_KNOTS('',3,(#433826,#433827,#433828,#433829,
#433830,#433831,#433832),.UNSPECIFIED.,.F.,.F.,(4,3,4),(0.,4.40000041065374E-5,
9.89910850773113E-5),.UNSPECIFIED.);
#26426=B_SPLINE_CURVE_WITH_KNOTS('',3,(#433853,#433854,#433855,#433856,
#433857,#433858,#433859,#433860,#433861,#433862,#433863,#433864,#433865,
#433866,#433867,#433868,#433869,#433870,#433871,#433872,#433873,#433874,
#433875,#433876,#433877,#433878,#433879,#433880,#433881,#433882,#433883,
#433884,#433885,#433886),.UNSPECIFIED.,.F.,.F.,(4,3,3,3,3,3,3,3,3,3,3,4),
(0.,4.29157837303002E-6,5.42772623795338E-6,1.00901698482348E-5,1.3127919506864E-5,
1.57383542265799E-5,1.61011507492105E-5,1.67166789291756E-5,1.95343262811359E-5,
2.29377234674648E-5,2.71556047620057E-5,3.34407099942657E-5),
 .UNSPECIFIED.);
#26427=B_SPLINE_CURVE_WITH_KNOTS('',3,(#433899,#433900,#433901,#433902,
#433903,#433904,#433905,#433906,#433907,#433908,#433909,#433910,#433911,
#433912,#433913,#433914,#433915,#433916,#433917,#433918,#433919,#433920,
#433921,#433922,#433923,#433924,#433925,#433926,#433927,#433928,#433929,
#433930,#433931,#433932),.UNSPECIFIED.,.F.,.F.,(4,3,3,3,3,3,3,3,3,3,3,4),
(1.0842021724855E-19,3.71309426656652E-6,5.39981071559414E-6,8.7893328936642E-6,
9.00272357067527E-6,1.0714398450415E-5,1.60780299679545E-5,1.65806081157689E-5,
2.30369726850333E-5,2.67819200416089E-5,3.59736924188076E-5,4.03862783807005E-5),
 .UNSPECIFIED.);
#26428=B_SPLINE_CURVE_WITH_KNOTS('',3,(#434045,#434046,#434047,#434048),
 .UNSPECIFIED.,.F.,.F.,(4,4),(0.,7.70025630629239E-5),.UNSPECIFIED.);
#26429=B_SPLINE_CURVE_WITH_KNOTS('',3,(#434058,#434059,#434060,#434061),
 .UNSPECIFIED.,.F.,.F.,(4,4),(1.0842021724855E-19,7.70025630629237E-5),
 .UNSPECIFIED.);
#26430=B_SPLINE_CURVE_WITH_KNOTS('',3,(#434065,#434066,#434067,#434068,
#434069,#434070,#434071,#434072,#434073,#434074,#434075,#434076,#434077,
#434078,#434079,#434080,#434081,#434082,#434083,#434084,#434085,#434086,
#434087,#434088,#434089,#434090,#434091,#434092,#434093,#434094,#434095,
#434096,#434097,#434098,#434099,#434100,#434101),.UNSPECIFIED.,.F.,.F.,
(4,3,3,3,3,3,3,3,3,3,3,3,4),(0.,9.59031527200469E-6,1.94769411222819E-5,
2.02405092183153E-5,3.21374138577713E-5,3.60302195070438E-5,4.42640648818814E-5,
4.53660204229444E-5,5.03633762302024E-5,5.17708036292895E-5,5.37928993851988E-5,
5.54103755460199E-5,5.64557889509706E-5),.UNSPECIFIED.);
#26431=B_SPLINE_CURVE_WITH_KNOTS('',3,(#434102,#434103,#434104,#434105,
#434106,#434107,#434108,#434109,#434110,#434111,#434112,#434113,#434114,
#434115,#434116,#434117,#434118,#434119,#434120,#434121,#434122,#434123,
#434124,#434125,#434126,#434127,#434128,#434129),.UNSPECIFIED.,.F.,.F.,
(4,3,3,3,3,3,3,3,3,4),(5.64557889509706E-5,5.9894096649375E-5,6.34214003873379E-5,
7.222414760851E-5,7.38322796533364E-5,8.36529189331486E-5,8.80714278222499E-5,
9.84837568501126E-5,0.000108624704079219,0.000110823272382853),
 .UNSPECIFIED.);
#26432=B_SPLINE_CURVE_WITH_KNOTS('',3,(#434145,#434146,#434147,#434148,
#434149,#434150,#434151,#434152,#434153,#434154,#434155,#434156,#434157,
#434158,#434159,#434160,#434161,#434162,#434163,#434164,#434165,#434166,
#434167,#434168,#434169,#434170,#434171,#434172),.UNSPECIFIED.,.F.,.F.,
(4,3,3,3,3,3,3,3,3,4),(0.,8.6603962858081E-6,1.64707715200666E-5,2.24502894132384E-5,
2.49975961757823E-5,2.8852600369028E-5,3.10661348995015E-5,3.4305354351696E-5,
3.66410545653559E-5,4.00504537627885E-5),.UNSPECIFIED.);
#26433=B_SPLINE_CURVE_WITH_KNOTS('',3,(#434175,#434176,#434177,#434178,
#434179,#434180,#434181),.UNSPECIFIED.,.F.,.F.,(4,3,4),(0.,4.40000041065376E-5,
9.89910850773114E-5),.UNSPECIFIED.);
#26434=B_SPLINE_CURVE_WITH_KNOTS('',3,(#434202,#434203,#434204,#434205,
#434206,#434207,#434208,#434209,#434210,#434211,#434212,#434213,#434214,
#434215,#434216,#434217,#434218,#434219,#434220,#434221,#434222,#434223,
#434224,#434225,#434226,#434227,#434228,#434229,#434230,#434231,#434232,
#434233,#434234,#434235),.UNSPECIFIED.,.F.,.F.,(4,3,3,3,3,3,3,3,3,3,3,4),
(0.,4.29157837305019E-6,5.4277262379532E-6,1.00901698482347E-5,1.31279195068639E-5,
1.57383542265796E-5,1.61011507492104E-5,1.67166789291757E-5,1.95343262811361E-5,
2.2937723467465E-5,2.7155604762006E-5,3.34407099942661E-5),
 .UNSPECIFIED.);
#26435=B_SPLINE_CURVE_WITH_KNOTS('',3,(#434248,#434249,#434250,#434251,
#434252,#434253,#434254,#434255,#434256,#434257,#434258,#434259,#434260,
#434261,#434262,#434263,#434264,#434265,#434266,#434267,#434268,#434269,
#434270,#434271,#434272,#434273,#434274,#434275,#434276,#434277,#434278,
#434279,#434280,#434281),.UNSPECIFIED.,.F.,.F.,(4,3,3,3,3,3,3,3,3,3,3,4),
(1.0842021724855E-19,3.71309426656629E-6,5.3998107155941E-6,8.78933289329952E-6,
9.00272357067513E-6,1.07143984504149E-5,1.6078029967954E-5,1.65806081157686E-5,
2.30369726850589E-5,2.67819200416085E-5,3.59736924188033E-5,4.03862783807E-5),
 .UNSPECIFIED.);
#26436=B_SPLINE_CURVE_WITH_KNOTS('',3,(#434394,#434395,#434396,#434397),
 .UNSPECIFIED.,.F.,.F.,(4,4),(0.,7.70025630629243E-5),.UNSPECIFIED.);
#26437=B_SPLINE_CURVE_WITH_KNOTS('',3,(#434407,#434408,#434409,#434410),
 .UNSPECIFIED.,.F.,.F.,(4,4),(2.16840434497101E-19,7.70025630629238E-5),
 .UNSPECIFIED.);
#26438=B_SPLINE_CURVE_WITH_KNOTS('',3,(#434414,#434415,#434416,#434417,
#434418,#434419,#434420,#434421,#434422,#434423,#434424,#434425,#434426,
#434427,#434428,#434429,#434430,#434431,#434432,#434433,#434434,#434435,
#434436,#434437,#434438,#434439,#434440,#434441,#434442,#434443,#434444,
#434445,#434446,#434447,#434448,#434449,#434450),.UNSPECIFIED.,.F.,.F.,
(4,3,3,3,3,3,3,3,3,3,3,3,4),(0.,9.59031527197168E-6,1.94769411222557E-5,
2.02405092183152E-5,3.21374138577623E-5,3.60302195070439E-5,4.42640648819179E-5,
4.53660204229443E-5,5.03633762301952E-5,5.17708036292895E-5,5.37928993851988E-5,
5.54103755460205E-5,5.64557889511527E-5),.UNSPECIFIED.);
#26439=B_SPLINE_CURVE_WITH_KNOTS('',3,(#434451,#434452,#434453,#434454,
#434455,#434456,#434457,#434458,#434459,#434460,#434461,#434462,#434463,
#434464,#434465,#434466,#434467,#434468,#434469,#434470,#434471,#434472,
#434473,#434474,#434475,#434476,#434477,#434478),.UNSPECIFIED.,.F.,.F.,
(4,3,3,3,3,3,3,3,3,4),(5.64557889511527E-5,5.98940966493751E-5,6.3421400387338E-5,
7.22241476084597E-5,7.38322796533364E-5,8.36529189331495E-5,8.807142782225E-5,
9.84837568501151E-5,0.000108624704079247,0.000110823272382854),
 .UNSPECIFIED.);
#26440=B_SPLINE_CURVE_WITH_KNOTS('',3,(#434494,#434495,#434496,#434497,
#434498,#434499,#434500,#434501,#434502,#434503,#434504,#434505,#434506,
#434507,#434508,#434509,#434510,#434511,#434512,#434513,#434514,#434515,
#434516,#434517,#434518,#434519,#434520,#434521),.UNSPECIFIED.,.F.,.F.,
(4,3,3,3,3,3,3,3,3,4),(0.,8.6603962858347E-6,1.64707715200667E-5,2.2450289413261E-5,
2.49975961757823E-5,2.88526003690281E-5,3.10661348995018E-5,3.43053543516962E-5,
3.66410545653562E-5,4.00504537627892E-5),.UNSPECIFIED.);
#26441=B_SPLINE_CURVE_WITH_KNOTS('',3,(#434524,#434525,#434526,#434527,
#434528,#434529,#434530),.UNSPECIFIED.,.F.,.F.,(4,3,4),(0.,4.40000041065378E-5,
9.89910850773116E-5),.UNSPECIFIED.);
#26442=B_SPLINE_CURVE_WITH_KNOTS('',3,(#434551,#434552,#434553,#434554,
#434555,#434556,#434557,#434558,#434559,#434560,#434561,#434562,#434563,
#434564,#434565,#434566,#434567,#434568,#434569,#434570,#434571,#434572,
#434573,#434574,#434575,#434576,#434577,#434578,#434579,#434580,#434581,
#434582,#434583,#434584),.UNSPECIFIED.,.F.,.F.,(4,3,3,3,3,3,3,3,3,3,3,4),
(0.,4.29157837303538E-6,5.42772623795322E-6,1.00901698482348E-5,1.31279195068638E-5,
1.57383542265853E-5,1.61011507492106E-5,1.67166789291757E-5,1.95343262811361E-5,
2.2937723467465E-5,2.7155604762006E-5,3.3440709994266E-5),.UNSPECIFIED.);
#26443=B_SPLINE_CURVE_WITH_KNOTS('',3,(#434597,#434598,#434599,#434600,
#434601,#434602,#434603,#434604,#434605,#434606,#434607,#434608,#434609,
#434610,#434611,#434612,#434613,#434614,#434615,#434616,#434617,#434618,
#434619,#434620,#434621,#434622,#434623,#434624,#434625,#434626,#434627,
#434628,#434629,#434630),.UNSPECIFIED.,.F.,.F.,(4,3,3,3,3,3,3,3,3,3,3,4),
(2.16840434497101E-19,3.71309426656641E-6,5.39981071559398E-6,8.78933289365255E-6,
9.002723570675E-6,1.07143984504147E-5,1.60780299679668E-5,1.65806081157686E-5,
2.30369726850311E-5,2.67819200416086E-5,3.59736924187738E-5,4.03862783807001E-5),
 .UNSPECIFIED.);
#26444=B_SPLINE_CURVE_WITH_KNOTS('',3,(#434743,#434744,#434745,#434746),
 .UNSPECIFIED.,.F.,.F.,(4,4),(0.,7.70025630629239E-5),.UNSPECIFIED.);
#26445=B_SPLINE_CURVE_WITH_KNOTS('',3,(#434756,#434757,#434758,#434759),
 .UNSPECIFIED.,.F.,.F.,(4,4),(2.16840434497101E-19,7.7002563062924E-5),
 .UNSPECIFIED.);
#26446=B_SPLINE_CURVE_WITH_KNOTS('',3,(#434763,#434764,#434765,#434766,
#434767,#434768,#434769,#434770,#434771,#434772,#434773,#434774,#434775,
#434776,#434777,#434778,#434779,#434780,#434781,#434782,#434783,#434784,
#434785,#434786,#434787,#434788,#434789,#434790,#434791,#434792,#434793,
#434794,#434795,#434796,#434797,#434798,#434799),.UNSPECIFIED.,.F.,.F.,
(4,3,3,3,3,3,3,3,3,3,3,3,4),(0.,9.59031527200526E-6,1.94769411222901E-5,
2.02405092183153E-5,3.21374138577741E-5,3.60302195070439E-5,4.42640648818246E-5,
4.53660204229444E-5,5.03633762301999E-5,5.17708036292895E-5,5.37928993851987E-5,
5.54103755460196E-5,5.64557889512458E-5),.UNSPECIFIED.);
#26447=B_SPLINE_CURVE_WITH_KNOTS('',3,(#434800,#434801,#434802,#434803,
#434804,#434805,#434806,#434807,#434808,#434809,#434810,#434811,#434812,
#434813,#434814,#434815,#434816,#434817,#434818,#434819,#434820,#434821,
#434822,#434823,#434824,#434825,#434826,#434827),.UNSPECIFIED.,.F.,.F.,
(4,3,3,3,3,3,3,3,3,4),(5.64557889512458E-5,5.98940966493751E-5,6.34214003873378E-5,
7.22241476084449E-5,7.38322796533364E-5,8.36529189331453E-5,8.80714278222498E-5,
9.84837568500673E-5,0.000108624704079133,0.000110823272382853),
 .UNSPECIFIED.);
#26448=B_SPLINE_CURVE_WITH_KNOTS('',3,(#434843,#434844,#434845,#434846,
#434847,#434848,#434849,#434850,#434851,#434852,#434853,#434854,#434855,
#434856,#434857,#434858,#434859,#434860,#434861,#434862,#434863,#434864,
#434865,#434866,#434867,#434868,#434869,#434870),.UNSPECIFIED.,.F.,.F.,
(4,3,3,3,3,3,3,3,3,4),(0.,8.66039628585016E-6,1.64707715200665E-5,2.24502894132343E-5,
2.49975961757822E-5,2.88526003690281E-5,3.10661348995015E-5,3.4305354351696E-5,
3.66410545653557E-5,4.00504537627886E-5),.UNSPECIFIED.);
#26449=B_SPLINE_CURVE_WITH_KNOTS('',3,(#434873,#434874,#434875,#434876,
#434877,#434878,#434879),.UNSPECIFIED.,.F.,.F.,(4,3,4),(0.,4.40000041065375E-5,
9.89910850773113E-5),.UNSPECIFIED.);
#26450=B_SPLINE_CURVE_WITH_KNOTS('',3,(#434900,#434901,#434902,#434903,
#434904,#434905,#434906,#434907,#434908,#434909,#434910,#434911,#434912,
#434913,#434914,#434915,#434916,#434917,#434918,#434919,#434920,#434921,
#434922,#434923,#434924,#434925,#434926,#434927,#434928,#434929,#434930,
#434931,#434932,#434933),.UNSPECIFIED.,.F.,.F.,(4,3,3,3,3,3,3,3,3,3,3,4),
(0.,4.29157837302687E-6,5.42772623795313E-6,1.00901698482347E-5,1.31279195068639E-5,
1.57383542265806E-5,1.61011507492103E-5,1.6716678929175E-5,1.95343262811356E-5,
2.29377234674646E-5,2.71556047620055E-5,3.34407099942656E-5),
 .UNSPECIFIED.);
#26451=B_SPLINE_CURVE_WITH_KNOTS('',3,(#434946,#434947,#434948,#434949,
#434950,#434951,#434952,#434953,#434954,#434955,#434956,#434957,#434958,
#434959,#434960,#434961,#434962,#434963,#434964,#434965,#434966,#434967,
#434968,#434969,#434970,#434971,#434972,#434973,#434974,#434975,#434976,
#434977,#434978,#434979),.UNSPECIFIED.,.F.,.F.,(4,3,3,3,3,3,3,3,3,3,3,4),
(0.,3.71309426656649E-6,5.3998107155942E-6,8.78933289370609E-6,9.00272357067532E-6,
1.07143984504151E-5,1.60780299679492E-5,1.6580608115769E-5,2.3036972685064E-5,
2.6781920041609E-5,3.59736924188123E-5,4.03862783807007E-5),
 .UNSPECIFIED.);
#26452=B_SPLINE_CURVE_WITH_KNOTS('',3,(#435092,#435093,#435094,#435095),
 .UNSPECIFIED.,.F.,.F.,(4,4),(0.,7.7002563062924E-5),.UNSPECIFIED.);
#26453=B_SPLINE_CURVE_WITH_KNOTS('',3,(#435105,#435106,#435107,#435108),
 .UNSPECIFIED.,.F.,.F.,(4,4),(2.16840434497101E-19,7.70025630629234E-5),
 .UNSPECIFIED.);
#26454=B_SPLINE_CURVE_WITH_KNOTS('',3,(#435112,#435113,#435114,#435115,
#435116,#435117,#435118,#435119,#435120,#435121,#435122,#435123,#435124,
#435125,#435126,#435127,#435128,#435129,#435130,#435131,#435132,#435133,
#435134,#435135,#435136,#435137,#435138,#435139,#435140,#435141,#435142,
#435143,#435144,#435145,#435146,#435147,#435148),.UNSPECIFIED.,.F.,.F.,
(4,3,3,3,3,3,3,3,3,3,3,3,4),(0.,9.59031527199155E-6,1.94769411222748E-5,
2.02405092183152E-5,3.21374138577728E-5,3.60302195070438E-5,4.42640648818854E-5,
4.53660204229444E-5,5.036337623021E-5,5.17708036292895E-5,5.37928993851989E-5,
5.54103755460202E-5,5.64557889511684E-5),.UNSPECIFIED.);
#26455=B_SPLINE_CURVE_WITH_KNOTS('',3,(#435149,#435150,#435151,#435152,
#435153,#435154,#435155,#435156,#435157,#435158,#435159,#435160,#435161,
#435162,#435163,#435164,#435165,#435166,#435167,#435168,#435169,#435170,
#435171,#435172,#435173,#435174,#435175,#435176),.UNSPECIFIED.,.F.,.F.,
(4,3,3,3,3,3,3,3,3,4),(5.64557889511684E-5,5.9894096649375E-5,6.34214003873381E-5,
7.22241476084239E-5,7.38322796533365E-5,8.36529189331425E-5,8.807142782225E-5,
9.84837568500588E-5,0.000108624704079108,0.000110823272382854),
 .UNSPECIFIED.);
#26456=B_SPLINE_CURVE_WITH_KNOTS('',3,(#435192,#435193,#435194,#435195,
#435196,#435197,#435198,#435199,#435200,#435201,#435202,#435203,#435204,
#435205,#435206,#435207,#435208,#435209,#435210,#435211,#435212,#435213,
#435214,#435215,#435216,#435217,#435218,#435219),.UNSPECIFIED.,.F.,.F.,
(4,3,3,3,3,3,3,3,3,4),(0.,8.66039628582568E-6,1.6470771520067E-5,2.24502894132484E-5,
2.4997596175783E-5,2.88526003690286E-5,3.10661348995021E-5,3.43053543516964E-5,
3.66410545653567E-5,4.00504537627889E-5),.UNSPECIFIED.);
#26457=B_SPLINE_CURVE_WITH_KNOTS('',3,(#435222,#435223,#435224,#435225,
#435226,#435227,#435228),.UNSPECIFIED.,.F.,.F.,(4,3,4),(0.,4.40000041065377E-5,
9.89910850773115E-5),.UNSPECIFIED.);
#26458=B_SPLINE_CURVE_WITH_KNOTS('',3,(#435249,#435250,#435251,#435252,
#435253,#435254,#435255,#435256,#435257,#435258,#435259,#435260,#435261,
#435262,#435263,#435264,#435265,#435266,#435267,#435268,#435269,#435270,
#435271,#435272,#435273,#435274,#435275,#435276,#435277,#435278,#435279,
#435280,#435281,#435282),.UNSPECIFIED.,.F.,.F.,(4,3,3,3,3,3,3,3,3,3,3,4),
(0.,4.2915783730306E-6,5.42772623795349E-6,1.00901698482348E-5,1.31279195068639E-5,
1.57383542265897E-5,1.61011507492107E-5,1.6716678929176E-5,1.95343262811361E-5,
2.29377234674652E-5,2.71556047620063E-5,3.34407099942664E-5),
 .UNSPECIFIED.);
#26459=B_SPLINE_CURVE_WITH_KNOTS('',3,(#435295,#435296,#435297,#435298,
#435299,#435300,#435301,#435302,#435303,#435304,#435305,#435306,#435307,
#435308,#435309,#435310,#435311,#435312,#435313,#435314,#435315,#435316,
#435317,#435318,#435319,#435320,#435321,#435322,#435323,#435324,#435325,
#435326,#435327,#435328),.UNSPECIFIED.,.F.,.F.,(4,3,3,3,3,3,3,3,3,3,3,4),
(0.,3.71309426656607E-6,5.39981071559398E-6,8.78933289328321E-6,9.00272357067504E-6,
1.07143984504148E-5,1.60780299679388E-5,1.65806081157685E-5,2.30369726850487E-5,
2.67819200416084E-5,3.59736924188455E-5,4.03862783806998E-5),
 .UNSPECIFIED.);
#26460=B_SPLINE_CURVE_WITH_KNOTS('',3,(#435441,#435442,#435443,#435444),
 .UNSPECIFIED.,.F.,.F.,(4,4),(0.,7.70025630629241E-5),.UNSPECIFIED.);
#26461=B_SPLINE_CURVE_WITH_KNOTS('',3,(#435454,#435455,#435456,#435457),
 .UNSPECIFIED.,.F.,.F.,(4,4),(2.16840434497101E-19,7.70025630629236E-5),
 .UNSPECIFIED.);
#26462=B_SPLINE_CURVE_WITH_KNOTS('',3,(#435461,#435462,#435463,#435464,
#435465,#435466,#435467,#435468,#435469,#435470,#435471,#435472,#435473,
#435474,#435475,#435476,#435477,#435478,#435479,#435480,#435481,#435482,
#435483,#435484,#435485,#435486,#435487,#435488,#435489,#435490,#435491,
#435492,#435493,#435494,#435495,#435496,#435497),.UNSPECIFIED.,.F.,.F.,
(4,3,3,3,3,3,3,3,3,3,3,3,4),(0.,9.59031527199796E-6,1.94769411222854E-5,
2.02405092183152E-5,3.21374138577684E-5,3.60302195070438E-5,4.42640648819319E-5,
4.53660204229443E-5,5.03633762301984E-5,5.17708036292895E-5,5.37928993851986E-5,
5.54103755460199E-5,5.6455788950753E-5),.UNSPECIFIED.);
#26463=B_SPLINE_CURVE_WITH_KNOTS('',3,(#435498,#435499,#435500,#435501,
#435502,#435503,#435504,#435505,#435506,#435507,#435508,#435509,#435510,
#435511,#435512,#435513,#435514,#435515,#435516,#435517,#435518,#435519,
#435520,#435521,#435522,#435523,#435524,#435525),.UNSPECIFIED.,.F.,.F.,
(4,3,3,3,3,3,3,3,3,4),(5.6455788950753E-5,5.98940966493747E-5,6.34214003873378E-5,
7.2224147608461E-5,7.38322796533361E-5,8.36529189331474E-5,8.80714278222495E-5,
9.84837568500782E-5,0.000108624704079145,0.000110823272382853),
 .UNSPECIFIED.);
#26464=B_SPLINE_CURVE_WITH_KNOTS('',3,(#435541,#435542,#435543,#435544,
#435545,#435546,#435547,#435548,#435549,#435550,#435551,#435552,#435553,
#435554,#435555,#435556,#435557,#435558,#435559,#435560,#435561,#435562,
#435563,#435564,#435565,#435566,#435567,#435568),.UNSPECIFIED.,.F.,.F.,
(4,3,3,3,3,3,3,3,3,4),(0.,8.66039628586018E-6,1.64707715200669E-5,2.24502894132357E-5,
2.49975961757829E-5,2.88526003690289E-5,3.10661348995023E-5,3.43053543516968E-5,
3.66410545653568E-5,4.00504537627889E-5),.UNSPECIFIED.);
#26465=B_SPLINE_CURVE_WITH_KNOTS('',3,(#435571,#435572,#435573,#435574,
#435575,#435576,#435577),.UNSPECIFIED.,.F.,.F.,(4,3,4),(0.,4.40000041065378E-5,
9.89910850773116E-5),.UNSPECIFIED.);
#26466=B_SPLINE_CURVE_WITH_KNOTS('',3,(#435598,#435599,#435600,#435601,
#435602,#435603,#435604,#435605,#435606,#435607,#435608,#435609,#435610,
#435611,#435612,#435613,#435614,#435615,#435616,#435617,#435618,#435619,
#435620,#435621,#435622,#435623,#435624,#435625,#435626,#435627,#435628,
#435629,#435630,#435631),.UNSPECIFIED.,.F.,.F.,(4,3,3,3,3,3,3,3,3,3,3,4),
(0.,4.29157837302937E-6,5.42772623795306E-6,1.00901698482347E-5,1.31279195068637E-5,
1.57383542265839E-5,1.61011507492102E-5,1.67166789291754E-5,1.95343262811358E-5,
2.29377234674648E-5,2.71556047620055E-5,3.34407099942653E-5),
 .UNSPECIFIED.);
#26467=B_SPLINE_CURVE_WITH_KNOTS('',3,(#435644,#435645,#435646,#435647,
#435648,#435649,#435650,#435651,#435652,#435653,#435654,#435655,#435656,
#435657,#435658,#435659,#435660,#435661,#435662,#435663,#435664,#435665,
#435666,#435667,#435668,#435669,#435670,#435671,#435672,#435673,#435674,
#435675,#435676,#435677),.UNSPECIFIED.,.F.,.F.,(4,3,3,3,3,3,3,3,3,3,3,4),
(0.,3.71309426656662E-6,5.39981071559464E-6,8.78933289368124E-6,9.00272357067546E-6,
1.07143984504151E-5,1.60780299679529E-5,1.6580608115769E-5,2.303697268505E-5,
2.67819200416091E-5,3.59736924187716E-5,4.03862783807006E-5),
 .UNSPECIFIED.);
#26468=B_SPLINE_CURVE_WITH_KNOTS('',3,(#435790,#435791,#435792,#435793),
 .UNSPECIFIED.,.F.,.F.,(4,4),(0.,7.70025630629239E-5),.UNSPECIFIED.);
#26469=B_SPLINE_CURVE_WITH_KNOTS('',3,(#435803,#435804,#435805,#435806),
 .UNSPECIFIED.,.F.,.F.,(4,4),(0.,7.70025630629238E-5),.UNSPECIFIED.);
#26470=B_SPLINE_CURVE_WITH_KNOTS('',3,(#435810,#435811,#435812,#435813,
#435814,#435815,#435816,#435817,#435818,#435819,#435820,#435821,#435822,
#435823,#435824,#435825,#435826,#435827,#435828,#435829,#435830,#435831,
#435832,#435833,#435834,#435835,#435836,#435837,#435838,#435839,#435840,
#435841,#435842,#435843,#435844,#435845,#435846),.UNSPECIFIED.,.F.,.F.,
(4,3,3,3,3,3,3,3,3,3,3,3,4),(0.,9.59031527203606E-6,1.94769411223574E-5,
2.02405092183154E-5,3.21374138577652E-5,3.60302195070439E-5,4.42640648818479E-5,
4.53660204229445E-5,5.03633762302319E-5,5.17708036292895E-5,5.37928993851989E-5,
5.54103755460196E-5,5.64557889509337E-5),.UNSPECIFIED.);
#26471=B_SPLINE_CURVE_WITH_KNOTS('',3,(#435847,#435848,#435849,#435850,
#435851,#435852,#435853,#435854,#435855,#435856,#435857,#435858,#435859,
#435860,#435861,#435862,#435863,#435864,#435865,#435866,#435867,#435868,
#435869,#435870,#435871,#435872,#435873,#435874),.UNSPECIFIED.,.F.,.F.,
(4,3,3,3,3,3,3,3,3,4),(5.64557889509337E-5,5.98940966493753E-5,6.34214003873381E-5,
7.2224147608401E-5,7.38322796533362E-5,8.36529189331597E-5,8.80714278222501E-5,
9.84837568501059E-5,0.000108624704079191,0.000110823272382853),
 .UNSPECIFIED.);
#26472=B_SPLINE_CURVE_WITH_KNOTS('',3,(#435890,#435891,#435892,#435893,
#435894,#435895,#435896,#435897,#435898,#435899,#435900,#435901,#435902,
#435903,#435904,#435905,#435906,#435907,#435908,#435909,#435910,#435911,
#435912,#435913,#435914,#435915,#435916,#435917),.UNSPECIFIED.,.F.,.F.,
(4,3,3,3,3,3,3,3,3,4),(0.,8.66039628578931E-6,1.6470771520067E-5,2.24502894132249E-5,
2.49975961757829E-5,2.88526003690286E-5,3.10661348995018E-5,3.43053543516963E-5,
3.66410545653567E-5,4.00504537627888E-5),.UNSPECIFIED.);
#26473=B_SPLINE_CURVE_WITH_KNOTS('',3,(#435920,#435921,#435922,#435923,
#435924,#435925,#435926),.UNSPECIFIED.,.F.,.F.,(4,3,4),(0.,4.40000041065377E-5,
9.89910850773112E-5),.UNSPECIFIED.);
#26474=B_SPLINE_CURVE_WITH_KNOTS('',3,(#435947,#435948,#435949,#435950,
#435951,#435952,#435953,#435954,#435955,#435956,#435957,#435958,#435959,
#435960,#435961,#435962,#435963,#435964,#435965,#435966,#435967,#435968,
#435969,#435970,#435971,#435972,#435973,#435974,#435975,#435976,#435977,
#435978,#435979,#435980),.UNSPECIFIED.,.F.,.F.,(4,3,3,3,3,3,3,3,3,3,3,4),
(0.,4.29157837304789E-6,5.42772623795347E-6,1.0090169848235E-5,1.31279195068639E-5,
1.57383542265994E-5,1.61011507492107E-5,1.67166789291758E-5,1.95343262811364E-5,
2.29377234674653E-5,2.71556047620062E-5,3.3440709994266E-5),
 .UNSPECIFIED.);
#26475=B_SPLINE_CURVE_WITH_KNOTS('',3,(#435993,#435994,#435995,#435996,
#435997,#435998,#435999,#436000,#436001,#436002,#436003,#436004,#436005,
#436006,#436007,#436008,#436009,#436010,#436011,#436012,#436013,#436014,
#436015,#436016,#436017,#436018,#436019,#436020,#436021,#436022,#436023,
#436024,#436025,#436026),.UNSPECIFIED.,.F.,.F.,(4,3,3,3,3,3,3,3,3,3,3,4),
(2.16840434497101E-19,3.7130942665664E-6,5.39981071559413E-6,8.78933289330628E-6,
9.0027235706752E-6,1.07143984504148E-5,1.60780299679502E-5,1.65806081157688E-5,
2.30369726850799E-5,2.67819200416088E-5,3.59736924187541E-5,4.03862783807006E-5),
 .UNSPECIFIED.);
#26476=B_SPLINE_CURVE_WITH_KNOTS('',3,(#436139,#436140,#436141,#436142),
 .UNSPECIFIED.,.F.,.F.,(4,4),(0.,7.70025630629239E-5),.UNSPECIFIED.);
#26477=B_SPLINE_CURVE_WITH_KNOTS('',3,(#436152,#436153,#436154,#436155),
 .UNSPECIFIED.,.F.,.F.,(4,4),(2.16840434497101E-19,7.70025630629238E-5),
 .UNSPECIFIED.);
#26478=B_SPLINE_CURVE_WITH_KNOTS('',3,(#436159,#436160,#436161,#436162,
#436163,#436164,#436165,#436166,#436167,#436168,#436169,#436170,#436171,
#436172,#436173,#436174,#436175,#436176,#436177,#436178,#436179,#436180,
#436181,#436182,#436183,#436184,#436185,#436186,#436187,#436188,#436189,
#436190,#436191,#436192,#436193,#436194,#436195),.UNSPECIFIED.,.F.,.F.,
(4,3,3,3,3,3,3,3,3,3,3,3,4),(0.,9.5903152719825E-6,1.94769411222625E-5,
2.02405092183152E-5,3.21374138577704E-5,3.60302195070439E-5,4.42640648818249E-5,
4.53660204229442E-5,5.03633762302113E-5,5.17708036292899E-5,5.37928993851988E-5,
5.54103755460209E-5,5.64557889509965E-5),.UNSPECIFIED.);
#26479=B_SPLINE_CURVE_WITH_KNOTS('',3,(#436196,#436197,#436198,#436199,
#436200,#436201,#436202,#436203,#436204,#436205,#436206,#436207,#436208,
#436209,#436210,#436211,#436212,#436213,#436214,#436215,#436216,#436217,
#436218,#436219,#436220,#436221,#436222,#436223),.UNSPECIFIED.,.F.,.F.,
(4,3,3,3,3,3,3,3,3,4),(5.64557889509965E-5,5.98940966493753E-5,6.34214003873383E-5,
7.22241476084711E-5,7.38322796533366E-5,8.3652918933141E-5,8.80714278222504E-5,
9.84837568500915E-5,0.000108624704079173,0.000110823272382854),
 .UNSPECIFIED.);
#26480=B_SPLINE_CURVE_WITH_KNOTS('',3,(#436239,#436240,#436241,#436242,
#436243,#436244,#436245,#436246,#436247,#436248,#436249,#436250,#436251,
#436252,#436253,#436254,#436255,#436256,#436257,#436258,#436259,#436260,
#436261,#436262,#436263,#436264,#436265,#436266),.UNSPECIFIED.,.F.,.F.,
(4,3,3,3,3,3,3,3,3,4),(0.,8.66039628579659E-6,1.64707715200667E-5,2.24502894132511E-5,
2.49975961757824E-5,2.8852600369028E-5,3.10661348995018E-5,3.4305354351696E-5,
3.66410545653558E-5,4.00504537627887E-5),.UNSPECIFIED.);
#26481=B_SPLINE_CURVE_WITH_KNOTS('',3,(#436269,#436270,#436271,#436272,
#436273,#436274,#436275),.UNSPECIFIED.,.F.,.F.,(4,3,4),(0.,4.40000041065376E-5,
9.89910850773112E-5),.UNSPECIFIED.);
#26482=B_SPLINE_CURVE_WITH_KNOTS('',3,(#436296,#436297,#436298,#436299,
#436300,#436301,#436302,#436303,#436304,#436305,#436306,#436307,#436308,
#436309,#436310,#436311,#436312,#436313,#436314,#436315,#436316,#436317,
#436318,#436319,#436320,#436321,#436322,#436323,#436324,#436325,#436326,
#436327,#436328,#436329),.UNSPECIFIED.,.F.,.F.,(4,3,3,3,3,3,3,3,3,3,3,4),
(0.,4.29157837303514E-6,5.42772623795343E-6,1.00901698482349E-5,1.31279195068641E-5,
1.57383542265741E-5,1.61011507492106E-5,1.67166789291761E-5,1.95343262811359E-5,
2.29377234674652E-5,2.71556047620062E-5,3.34407099942666E-5),
 .UNSPECIFIED.);
#26483=B_SPLINE_CURVE_WITH_KNOTS('',3,(#436342,#436343,#436344,#436345,
#436346,#436347,#436348,#436349,#436350,#436351,#436352,#436353,#436354,
#436355,#436356,#436357,#436358,#436359,#436360,#436361,#436362,#436363,
#436364,#436365,#436366,#436367,#436368,#436369,#436370,#436371,#436372,
#436373,#436374,#436375),.UNSPECIFIED.,.F.,.F.,(4,3,3,3,3,3,3,3,3,3,3,4),
(0.,3.71309426656653E-6,5.39981071559412E-6,8.78933289366921E-6,9.00272357067533E-6,
1.0714398450415E-5,1.607802996795E-5,1.65806081157687E-5,2.30369726850199E-5,
2.67819200416086E-5,3.59736924188143E-5,4.03862783806999E-5),
 .UNSPECIFIED.);
#26484=B_SPLINE_CURVE_WITH_KNOTS('',3,(#436488,#436489,#436490,#436491),
 .UNSPECIFIED.,.F.,.F.,(4,4),(0.,7.70025630629239E-5),.UNSPECIFIED.);
#26485=B_SPLINE_CURVE_WITH_KNOTS('',3,(#436501,#436502,#436503,#436504),
 .UNSPECIFIED.,.F.,.F.,(4,4),(2.16840434497101E-19,7.70025630629238E-5),
 .UNSPECIFIED.);
#26486=B_SPLINE_CURVE_WITH_KNOTS('',3,(#436508,#436509,#436510,#436511,
#436512,#436513,#436514,#436515,#436516,#436517,#436518,#436519,#436520,
#436521,#436522,#436523,#436524,#436525,#436526,#436527,#436528,#436529,
#436530,#436531,#436532,#436533,#436534,#436535,#436536,#436537,#436538,
#436539,#436540,#436541,#436542,#436543,#436544),.UNSPECIFIED.,.F.,.F.,
(4,3,3,3,3,3,3,3,3,3,3,3,4),(0.,9.59031527201526E-6,1.94769411223018E-5,
2.02405092183151E-5,3.21374138577733E-5,3.6030219507044E-5,4.42640648818702E-5,
4.53660204229444E-5,5.0363376230214E-5,5.17708036292896E-5,5.37928993851991E-5,
5.54103755460203E-5,5.64557889511334E-5),.UNSPECIFIED.);
#26487=B_SPLINE_CURVE_WITH_KNOTS('',3,(#436545,#436546,#436547,#436548,
#436549,#436550,#436551,#436552,#436553,#436554,#436555,#436556,#436557,
#436558,#436559,#436560,#436561,#436562,#436563,#436564,#436565,#436566,
#436567,#436568,#436569,#436570,#436571,#436572),.UNSPECIFIED.,.F.,.F.,
(4,3,3,3,3,3,3,3,3,4),(5.64557889511334E-5,5.98940966493753E-5,6.34214003873383E-5,
7.22241476084157E-5,7.38322796533368E-5,8.36529189331239E-5,8.80714278222506E-5,
9.84837568500551E-5,0.000108624704079119,0.000110823272382854),
 .UNSPECIFIED.);
#26488=B_SPLINE_CURVE_WITH_KNOTS('',3,(#436588,#436589,#436590,#436591,
#436592,#436593,#436594,#436595,#436596,#436597,#436598,#436599,#436600,
#436601,#436602,#436603,#436604,#436605,#436606,#436607,#436608,#436609,
#436610,#436611,#436612,#436613,#436614,#436615),.UNSPECIFIED.,.F.,.F.,
(4,3,3,3,3,3,3,3,3,4),(0.,8.66039628579537E-6,1.64707715200666E-5,2.24502894132562E-5,
2.49975961757822E-5,2.8852600369028E-5,3.10661348995016E-5,3.43053543516961E-5,
3.66410545653559E-5,4.00504537627884E-5),.UNSPECIFIED.);
#26489=B_SPLINE_CURVE_WITH_KNOTS('',3,(#436618,#436619,#436620,#436621,
#436622,#436623,#436624),.UNSPECIFIED.,.F.,.F.,(4,3,4),(0.,4.40000041065378E-5,
9.89910850773114E-5),.UNSPECIFIED.);
#26490=B_SPLINE_CURVE_WITH_KNOTS('',3,(#436645,#436646,#436647,#436648,
#436649,#436650,#436651,#436652,#436653,#436654,#436655,#436656,#436657,
#436658,#436659,#436660,#436661,#436662,#436663,#436664,#436665,#436666,
#436667,#436668,#436669,#436670,#436671,#436672,#436673,#436674,#436675,
#436676,#436677,#436678),.UNSPECIFIED.,.F.,.F.,(4,3,3,3,3,3,3,3,3,3,3,4),
(0.,4.29157837302742E-6,5.42772623795344E-6,1.00901698482348E-5,1.31279195068639E-5,
1.57383542265895E-5,1.61011507492104E-5,1.6716678929176E-5,1.95343262811361E-5,
2.2937723467465E-5,2.7155604762006E-5,3.34407099942662E-5),
 .UNSPECIFIED.);
#26491=B_SPLINE_CURVE_WITH_KNOTS('',3,(#436691,#436692,#436693,#436694,
#436695,#436696,#436697,#436698,#436699,#436700,#436701,#436702,#436703,
#436704,#436705,#436706,#436707,#436708,#436709,#436710,#436711,#436712,
#436713,#436714,#436715,#436716,#436717,#436718,#436719,#436720,#436721,
#436722,#436723,#436724),.UNSPECIFIED.,.F.,.F.,(4,3,3,3,3,3,3,3,3,3,3,4),
(0.,3.71309426656648E-6,5.39981071559424E-6,8.78933289368692E-6,9.00272357067524E-6,
1.07143984504148E-5,1.60780299679589E-5,1.65806081157688E-5,2.3036972685045E-5,
2.67819200416088E-5,3.59736924188061E-5,4.03862783807006E-5),
 .UNSPECIFIED.);
#26492=B_SPLINE_CURVE_WITH_KNOTS('',3,(#436837,#436838,#436839,#436840),
 .UNSPECIFIED.,.F.,.F.,(4,4),(0.,7.70025630629238E-5),.UNSPECIFIED.);
#26493=B_SPLINE_CURVE_WITH_KNOTS('',3,(#436850,#436851,#436852,#436853),
 .UNSPECIFIED.,.F.,.F.,(4,4),(0.,7.70025630629235E-5),.UNSPECIFIED.);
#26494=B_SPLINE_CURVE_WITH_KNOTS('',3,(#436857,#436858,#436859,#436860,
#436861,#436862,#436863,#436864,#436865,#436866,#436867,#436868,#436869,
#436870,#436871,#436872,#436873,#436874,#436875,#436876,#436877,#436878,
#436879,#436880,#436881,#436882,#436883,#436884,#436885,#436886,#436887,
#436888,#436889,#436890,#436891,#436892,#436893),.UNSPECIFIED.,.F.,.F.,
(4,3,3,3,3,3,3,3,3,3,3,3,4),(0.,9.59031527202043E-6,1.94769411223311E-5,
2.02405092183154E-5,3.21374138577703E-5,3.60302195070436E-5,4.42640648819417E-5,
4.53660204229441E-5,5.03633762302143E-5,5.17708036292897E-5,5.37928993851988E-5,
5.54103755460199E-5,5.64557889509022E-5),.UNSPECIFIED.);
#26495=B_SPLINE_CURVE_WITH_KNOTS('',3,(#436894,#436895,#436896,#436897,
#436898,#436899,#436900,#436901,#436902,#436903,#436904,#436905,#436906,
#436907,#436908,#436909,#436910,#436911,#436912,#436913,#436914,#436915,
#436916,#436917,#436918,#436919,#436920,#436921),.UNSPECIFIED.,.F.,.F.,
(4,3,3,3,3,3,3,3,3,4),(5.64557889509022E-5,5.98940966493751E-5,6.34214003873379E-5,
7.22241476086138E-5,7.38322796533362E-5,8.36529189331517E-5,8.80714278222496E-5,
9.84837568501121E-5,0.000108624704079202,0.000110823272382853),
 .UNSPECIFIED.);
#26496=B_SPLINE_CURVE_WITH_KNOTS('',3,(#436937,#436938,#436939,#436940,
#436941,#436942,#436943,#436944,#436945,#436946,#436947,#436948,#436949,
#436950,#436951,#436952,#436953,#436954,#436955,#436956,#436957,#436958,
#436959,#436960,#436961,#436962,#436963,#436964),.UNSPECIFIED.,.F.,.F.,
(4,3,3,3,3,3,3,3,3,4),(0.,8.660396285838E-6,1.64707715200667E-5,2.24502894129291E-5,
2.49975961757824E-5,2.88526003690282E-5,3.10661348995017E-5,3.43053543516958E-5,
3.6641054565356E-5,4.00504537627886E-5),.UNSPECIFIED.);
#26497=B_SPLINE_CURVE_WITH_KNOTS('',3,(#436967,#436968,#436969,#436970,
#436971,#436972,#436973),.UNSPECIFIED.,.F.,.F.,(4,3,4),(0.,4.40000041065374E-5,
9.89910850773111E-5),.UNSPECIFIED.);
#26498=B_SPLINE_CURVE_WITH_KNOTS('',3,(#436994,#436995,#436996,#436997,
#436998,#436999,#437000,#437001,#437002,#437003,#437004,#437005,#437006,
#437007,#437008,#437009,#437010,#437011,#437012,#437013,#437014,#437015,
#437016,#437017,#437018,#437019,#437020,#437021,#437022,#437023,#437024,
#437025,#437026,#437027),.UNSPECIFIED.,.F.,.F.,(4,3,3,3,3,3,3,3,3,3,3,4),
(0.,4.29157837302125E-6,5.42772623795363E-6,1.00901698482349E-5,1.31279195068643E-5,
1.57383542265817E-5,1.61011507492105E-5,1.67166789291761E-5,1.95343262811362E-5,
2.29377234674653E-5,2.71556047620061E-5,3.34407099942659E-5),
 .UNSPECIFIED.);
#26499=B_SPLINE_CURVE_WITH_KNOTS('',3,(#437040,#437041,#437042,#437043,
#437044,#437045,#437046,#437047,#437048,#437049,#437050,#437051,#437052,
#437053,#437054,#437055,#437056,#437057,#437058,#437059,#437060,#437061,
#437062,#437063,#437064,#437065,#437066,#437067,#437068,#437069,#437070,
#437071,#437072,#437073),.UNSPECIFIED.,.F.,.F.,(4,3,3,3,3,3,3,3,3,3,3,4),
(2.16840434497101E-19,3.71309426656617E-6,5.39981071559392E-6,8.78933289364865E-6,
9.00272357067512E-6,1.07143984504147E-5,1.60780299679705E-5,1.65806081157687E-5,
2.30369726850335E-5,2.67819200416085E-5,3.59736924188345E-5,4.03862783806998E-5),
 .UNSPECIFIED.);
#26500=B_SPLINE_CURVE_WITH_KNOTS('',3,(#437186,#437187,#437188,#437189),
 .UNSPECIFIED.,.F.,.F.,(4,4),(0.,7.70025630629236E-5),.UNSPECIFIED.);
#26501=B_SPLINE_CURVE_WITH_KNOTS('',3,(#437199,#437200,#437201,#437202),
 .UNSPECIFIED.,.F.,.F.,(4,4),(4.33680868994202E-19,7.70025630629238E-5),
 .UNSPECIFIED.);
#26502=B_SPLINE_CURVE_WITH_KNOTS('',3,(#437206,#437207,#437208,#437209,
#437210,#437211,#437212,#437213,#437214,#437215,#437216,#437217,#437218,
#437219,#437220,#437221,#437222,#437223,#437224,#437225,#437226,#437227,
#437228,#437229,#437230,#437231,#437232,#437233,#437234,#437235,#437236,
#437237,#437238,#437239,#437240,#437241,#437242),.UNSPECIFIED.,.F.,.F.,
(4,3,3,3,3,3,3,3,3,3,3,3,4),(0.,9.5903152720398E-6,1.94769411223548E-5,
2.02405092183152E-5,3.21374138577692E-5,3.60302195070439E-5,4.42640648818201E-5,
4.53660204229444E-5,5.03633762302064E-5,5.17708036292898E-5,5.37928993851991E-5,
5.54103755460198E-5,5.64557889508151E-5),.UNSPECIFIED.);
#26503=B_SPLINE_CURVE_WITH_KNOTS('',3,(#437243,#437244,#437245,#437246,
#437247,#437248,#437249,#437250,#437251,#437252,#437253,#437254,#437255,
#437256,#437257,#437258,#437259,#437260,#437261,#437262,#437263,#437264,
#437265,#437266,#437267,#437268,#437269,#437270),.UNSPECIFIED.,.F.,.F.,
(4,3,3,3,3,3,3,3,3,4),(5.64557889508151E-5,5.98940966493754E-5,6.34214003873384E-5,
7.22241476084689E-5,7.38322796533367E-5,8.36529189331414E-5,8.80714278222504E-5,
9.84837568500745E-5,0.00010862470407914,0.000110823272382854),
 .UNSPECIFIED.);
#26504=B_SPLINE_CURVE_WITH_KNOTS('',3,(#437286,#437287,#437288,#437289,
#437290,#437291,#437292,#437293,#437294,#437295,#437296,#437297,#437298,
#437299,#437300,#437301,#437302,#437303,#437304,#437305,#437306,#437307,
#437308,#437309,#437310,#437311,#437312,#437313),.UNSPECIFIED.,.F.,.F.,
(4,3,3,3,3,3,3,3,3,4),(0.,8.6603962858034E-6,1.64707715200669E-5,2.2450289413248E-5,
2.49975961757828E-5,2.88526003690285E-5,3.1066134899502E-5,3.43053543516968E-5,
3.66410545653566E-5,4.00504537627889E-5),.UNSPECIFIED.);
#26505=B_SPLINE_CURVE_WITH_KNOTS('',3,(#437316,#437317,#437318,#437319,
#437320,#437321,#437322),.UNSPECIFIED.,.F.,.F.,(4,3,4),(0.,4.40000041065376E-5,
9.89910850773112E-5),.UNSPECIFIED.);
#26506=B_SPLINE_CURVE_WITH_KNOTS('',3,(#437343,#437344,#437345,#437346,
#437347,#437348,#437349,#437350,#437351,#437352,#437353,#437354,#437355,
#437356,#437357,#437358,#437359,#437360,#437361,#437362,#437363,#437364,
#437365,#437366,#437367,#437368,#437369,#437370,#437371,#437372,#437373,
#437374,#437375,#437376),.UNSPECIFIED.,.F.,.F.,(4,3,3,3,3,3,3,3,3,3,3,4),
(0.,4.29157837305506E-6,5.42772623795337E-6,1.00901698482351E-5,1.31279195068642E-5,
1.57383542265671E-5,1.61011507492106E-5,1.67166789291762E-5,1.95343262811363E-5,
2.29377234674653E-5,2.71556047620063E-5,3.34407099942663E-5),
 .UNSPECIFIED.);
#26507=B_SPLINE_CURVE_WITH_KNOTS('',3,(#437389,#437390,#437391,#437392,
#437393,#437394,#437395,#437396,#437397,#437398,#437399,#437400,#437401,
#437402,#437403,#437404,#437405,#437406,#437407,#437408,#437409,#437410,
#437411,#437412,#437413,#437414,#437415,#437416,#437417,#437418,#437419,
#437420,#437421,#437422),.UNSPECIFIED.,.F.,.F.,(4,3,3,3,3,3,3,3,3,3,3,4),
(0.,3.71309426656638E-6,5.3998107155941E-6,8.78933289365815E-6,9.00272357067497E-6,
1.07143984504149E-5,1.60780299679781E-5,1.65806081157684E-5,2.30369726850169E-5,
2.67819200416079E-5,3.59736924188327E-5,4.03862783806989E-5),
 .UNSPECIFIED.);
#26508=B_SPLINE_CURVE_WITH_KNOTS('',3,(#437535,#437536,#437537,#437538),
 .UNSPECIFIED.,.F.,.F.,(4,4),(0.,7.70025630629239E-5),.UNSPECIFIED.);
#26509=B_SPLINE_CURVE_WITH_KNOTS('',3,(#437548,#437549,#437550,#437551),
 .UNSPECIFIED.,.F.,.F.,(4,4),(4.33680868994202E-19,7.70025630629238E-5),
 .UNSPECIFIED.);
#26510=B_SPLINE_CURVE_WITH_KNOTS('',3,(#437555,#437556,#437557,#437558,
#437559,#437560,#437561,#437562,#437563,#437564,#437565,#437566,#437567,
#437568,#437569,#437570,#437571,#437572,#437573,#437574,#437575,#437576,
#437577,#437578,#437579,#437580,#437581,#437582,#437583,#437584,#437585,
#437586,#437587,#437588,#437589,#437590,#437591),.UNSPECIFIED.,.F.,.F.,
(4,3,3,3,3,3,3,3,3,3,3,3,4),(0.,9.59031527200714E-6,1.94769411223042E-5,
2.02405092183152E-5,3.21374138577778E-5,3.60302195070437E-5,4.42640648818082E-5,
4.53660204229444E-5,5.03633762302091E-5,5.17708036292898E-5,5.37928993851988E-5,
5.54103755460199E-5,5.64557889513718E-5),.UNSPECIFIED.);
#26511=B_SPLINE_CURVE_WITH_KNOTS('',3,(#437592,#437593,#437594,#437595,
#437596,#437597,#437598,#437599,#437600,#437601,#437602,#437603,#437604,
#437605,#437606,#437607,#437608,#437609,#437610,#437611,#437612,#437613,
#437614,#437615,#437616,#437617,#437618,#437619),.UNSPECIFIED.,.F.,.F.,
(4,3,3,3,3,3,3,3,3,4),(5.64557889513718E-5,5.98940966493751E-5,6.3421400387338E-5,
7.22241476084119E-5,7.38322796533366E-5,8.36529189331453E-5,8.80714278222501E-5,
9.84837568500711E-5,0.000108624704079126,0.000110823272382854),
 .UNSPECIFIED.);
#26512=B_SPLINE_CURVE_WITH_KNOTS('',3,(#437635,#437636,#437637,#437638,
#437639,#437640,#437641,#437642,#437643,#437644,#437645,#437646,#437647,
#437648,#437649,#437650,#437651,#437652,#437653,#437654,#437655,#437656,
#437657,#437658,#437659,#437660,#437661,#437662),.UNSPECIFIED.,.F.,.F.,
(4,3,3,3,3,3,3,3,3,4),(0.,8.66039628577752E-6,1.64707715200667E-5,2.24502894132132E-5,
2.49975961757823E-5,2.8852600369028E-5,3.10661348995015E-5,3.4305354351696E-5,
3.66410545653558E-5,4.00504537627882E-5),.UNSPECIFIED.);
#26513=B_SPLINE_CURVE_WITH_KNOTS('',3,(#437665,#437666,#437667,#437668,
#437669,#437670,#437671),.UNSPECIFIED.,.F.,.F.,(4,3,4),(0.,4.4000004106538E-5,
9.89910850773116E-5),.UNSPECIFIED.);
#26514=B_SPLINE_CURVE_WITH_KNOTS('',3,(#437692,#437693,#437694,#437695,
#437696,#437697,#437698,#437699,#437700,#437701,#437702,#437703,#437704,
#437705,#437706,#437707,#437708,#437709,#437710,#437711,#437712,#437713,
#437714,#437715,#437716,#437717,#437718,#437719,#437720,#437721,#437722,
#437723,#437724,#437725),.UNSPECIFIED.,.F.,.F.,(4,3,3,3,3,3,3,3,3,3,3,4),
(0.,4.29157837303885E-6,5.42772623795332E-6,1.00901698482349E-5,1.31279195068638E-5,
1.5738354226589E-5,1.61011507492106E-5,1.67166789291754E-5,1.95343262811361E-5,
2.29377234674651E-5,2.71556047620061E-5,3.34407099942664E-5),
 .UNSPECIFIED.);
#26515=B_SPLINE_CURVE_WITH_KNOTS('',3,(#437738,#437739,#437740,#437741,
#437742,#437743,#437744,#437745,#437746,#437747,#437748,#437749,#437750,
#437751,#437752,#437753,#437754,#437755,#437756,#437757,#437758,#437759,
#437760,#437761,#437762,#437763,#437764,#437765,#437766,#437767,#437768,
#437769,#437770,#437771),.UNSPECIFIED.,.F.,.F.,(4,3,3,3,3,3,3,3,3,3,3,4),
(0.,3.7130942665663E-6,5.39981071559403E-6,8.78933289330991E-6,9.00272357067504E-6,
1.07143984504147E-5,1.60780299679603E-5,1.65806081157687E-5,2.30369726850442E-5,
2.67819200416087E-5,3.59736924187731E-5,4.03862783807004E-5),
 .UNSPECIFIED.);
#26516=B_SPLINE_CURVE_WITH_KNOTS('',3,(#437884,#437885,#437886,#437887),
 .UNSPECIFIED.,.F.,.F.,(4,4),(0.,7.70025630629238E-5),.UNSPECIFIED.);
#26517=B_SPLINE_CURVE_WITH_KNOTS('',3,(#437897,#437898,#437899,#437900),
 .UNSPECIFIED.,.F.,.F.,(4,4),(0.,7.70025630629239E-5),.UNSPECIFIED.);
#26518=B_SPLINE_CURVE_WITH_KNOTS('',3,(#437904,#437905,#437906,#437907,
#437908,#437909,#437910,#437911,#437912,#437913,#437914,#437915,#437916,
#437917,#437918,#437919,#437920,#437921,#437922,#437923,#437924,#437925,
#437926,#437927,#437928,#437929,#437930,#437931,#437932,#437933,#437934,
#437935,#437936,#437937,#437938,#437939,#437940),.UNSPECIFIED.,.F.,.F.,
(4,3,3,3,3,3,3,3,3,3,3,3,4),(0.,9.59031527202011E-6,1.94769411223197E-5,
2.02405092183154E-5,3.21374138577635E-5,3.60302195070441E-5,4.4264064881854E-5,
4.53660204229442E-5,5.03633762302141E-5,5.17708036292897E-5,5.37928993851989E-5,
5.54103755460195E-5,5.64557889512644E-5),.UNSPECIFIED.);
#26519=B_SPLINE_CURVE_WITH_KNOTS('',3,(#437941,#437942,#437943,#437944,
#437945,#437946,#437947,#437948,#437949,#437950,#437951,#437952,#437953,
#437954,#437955,#437956,#437957,#437958,#437959,#437960,#437961,#437962,
#437963,#437964,#437965,#437966,#437967,#437968),.UNSPECIFIED.,.F.,.F.,
(4,3,3,3,3,3,3,3,3,4),(5.64557889512644E-5,5.98940966493748E-5,6.34214003873378E-5,
7.22241476084218E-5,7.38322796533363E-5,8.36529189331423E-5,8.80714278222497E-5,
9.84837568500604E-5,0.000108624704079115,0.000110823272382853),
 .UNSPECIFIED.);
#26520=B_SPLINE_CURVE_WITH_KNOTS('',3,(#437984,#437985,#437986,#437987,
#437988,#437989,#437990,#437991,#437992,#437993,#437994,#437995,#437996,
#437997,#437998,#437999,#438000,#438001,#438002,#438003,#438004,#438005,
#438006,#438007,#438008,#438009,#438010,#438011),.UNSPECIFIED.,.F.,.F.,
(4,3,3,3,3,3,3,3,3,4),(0.,8.66039628578128E-6,1.64707715200666E-5,2.24502894132383E-5,
2.49975961757824E-5,2.8852600369028E-5,3.10661348995017E-5,3.43053543516959E-5,
3.66410545653557E-5,4.00504537627889E-5),.UNSPECIFIED.);
#26521=B_SPLINE_CURVE_WITH_KNOTS('',3,(#438014,#438015,#438016,#438017,
#438018,#438019,#438020),.UNSPECIFIED.,.F.,.F.,(4,3,4),(0.,4.40000041065373E-5,
9.89910850773111E-5),.UNSPECIFIED.);
#26522=B_SPLINE_CURVE_WITH_KNOTS('',3,(#438041,#438042,#438043,#438044,
#438045,#438046,#438047,#438048,#438049,#438050,#438051,#438052,#438053,
#438054,#438055,#438056,#438057,#438058,#438059,#438060,#438061,#438062,
#438063,#438064,#438065,#438066,#438067,#438068,#438069,#438070,#438071,
#438072,#438073,#438074),.UNSPECIFIED.,.F.,.F.,(4,3,3,3,3,3,3,3,3,3,3,4),
(0.,4.2915783730307E-6,5.42772623795346E-6,1.00901698482348E-5,1.31279195068641E-5,
1.57383542265829E-5,1.61011507492106E-5,1.67166789291753E-5,1.9534326281136E-5,
2.2937723467465E-5,2.71556047620057E-5,3.34407099942656E-5),
 .UNSPECIFIED.);
#26523=B_SPLINE_CURVE_WITH_KNOTS('',3,(#438087,#438088,#438089,#438090,
#438091,#438092,#438093,#438094,#438095,#438096,#438097,#438098,#438099,
#438100,#438101,#438102,#438103,#438104,#438105,#438106,#438107,#438108,
#438109,#438110,#438111,#438112,#438113,#438114,#438115,#438116,#438117,
#438118,#438119,#438120),.UNSPECIFIED.,.F.,.F.,(4,3,3,3,3,3,3,3,3,3,3,4),
(0.,3.71309426656622E-6,5.39981071559398E-6,8.78933289327679E-6,9.00272357067504E-6,
1.07143984504148E-5,1.60780299679623E-5,1.65806081157686E-5,2.30369726850495E-5,
2.67819200416084E-5,3.5973692418755E-5,4.03862783806997E-5),
 .UNSPECIFIED.);
#26524=B_SPLINE_CURVE_WITH_KNOTS('',3,(#438233,#438234,#438235,#438236),
 .UNSPECIFIED.,.F.,.F.,(4,4),(0.,7.70025630629241E-5),.UNSPECIFIED.);
#26525=B_SPLINE_CURVE_WITH_KNOTS('',3,(#438246,#438247,#438248,#438249),
 .UNSPECIFIED.,.F.,.F.,(4,4),(4.33680868994202E-19,7.70025630629239E-5),
 .UNSPECIFIED.);
#26526=B_SPLINE_CURVE_WITH_KNOTS('',3,(#438253,#438254,#438255,#438256,
#438257,#438258,#438259,#438260,#438261,#438262,#438263,#438264,#438265,
#438266,#438267,#438268,#438269,#438270,#438271,#438272,#438273,#438274,
#438275,#438276,#438277,#438278,#438279,#438280,#438281,#438282,#438283,
#438284,#438285,#438286,#438287,#438288,#438289),.UNSPECIFIED.,.F.,.F.,
(4,3,3,3,3,3,3,3,3,3,3,3,4),(0.,9.59031527198475E-6,1.94769411222611E-5,
2.02405092183153E-5,3.21374138577742E-5,3.60302195070439E-5,4.4264064881873E-5,
4.53660204229443E-5,5.0363376230202E-5,5.17708036292894E-5,5.37928993851989E-5,
5.54103755460197E-5,5.6455788951275E-5),.UNSPECIFIED.);
#26527=B_SPLINE_CURVE_WITH_KNOTS('',3,(#438290,#438291,#438292,#438293,
#438294,#438295,#438296,#438297,#438298,#438299,#438300,#438301,#438302,
#438303,#438304,#438305,#438306,#438307,#438308,#438309,#438310,#438311,
#438312,#438313,#438314,#438315,#438316,#438317),.UNSPECIFIED.,.F.,.F.,
(4,3,3,3,3,3,3,3,3,4),(5.6455788951275E-5,5.9894096649375E-5,6.3421400387338E-5,
7.22241476084665E-5,7.38322796533363E-5,8.36529189331418E-5,8.80714278222499E-5,
9.84837568500648E-5,0.000108624704079118,0.000110823272382853),
 .UNSPECIFIED.);
#26528=B_SPLINE_CURVE_WITH_KNOTS('',3,(#438333,#438334,#438335,#438336,
#438337,#438338,#438339,#438340,#438341,#438342,#438343,#438344,#438345,
#438346,#438347,#438348,#438349,#438350,#438351,#438352,#438353,#438354,
#438355,#438356,#438357,#438358,#438359,#438360),.UNSPECIFIED.,.F.,.F.,
(4,3,3,3,3,3,3,3,3,4),(0.,8.6603962858341E-6,1.64707715200666E-5,2.24502894132345E-5,
2.49975961757823E-5,2.8852600369028E-5,3.10661348995015E-5,3.4305354351696E-5,
3.66410545653559E-5,4.00504537627888E-5),.UNSPECIFIED.);
#26529=B_SPLINE_CURVE_WITH_KNOTS('',3,(#438363,#438364,#438365,#438366,
#438367,#438368,#438369),.UNSPECIFIED.,.F.,.F.,(4,3,4),(0.,4.40000041065375E-5,
9.89910850773111E-5),.UNSPECIFIED.);
#26530=B_SPLINE_CURVE_WITH_KNOTS('',3,(#438390,#438391,#438392,#438393,
#438394,#438395,#438396,#438397,#438398,#438399,#438400,#438401,#438402,
#438403,#438404,#438405,#438406,#438407,#438408,#438409,#438410,#438411,
#438412,#438413,#438414,#438415,#438416,#438417,#438418,#438419,#438420,
#438421,#438422,#438423),.UNSPECIFIED.,.F.,.F.,(4,3,3,3,3,3,3,3,3,3,3,4),
(0.,4.29157837305459E-6,5.42772623795334E-6,1.0090169848235E-5,1.3127919506864E-5,
1.57383542265921E-5,1.61011507492108E-5,1.67166789291756E-5,1.9534326281136E-5,
2.29377234674651E-5,2.71556047620062E-5,3.34407099942664E-5),
 .UNSPECIFIED.);
#26531=B_SPLINE_CURVE_WITH_KNOTS('',3,(#438436,#438437,#438438,#438439,
#438440,#438441,#438442,#438443,#438444,#438445,#438446,#438447,#438448,
#438449,#438450,#438451,#438452,#438453,#438454,#438455,#438456,#438457,
#438458,#438459,#438460,#438461,#438462,#438463,#438464,#438465,#438466,
#438467,#438468,#438469),.UNSPECIFIED.,.F.,.F.,(4,3,3,3,3,3,3,3,3,3,3,4),
(2.16840434497101E-19,3.71309426656658E-6,5.39981071559397E-6,8.78933289368793E-6,
9.00272357067522E-6,1.0714398450415E-5,1.60780299679471E-5,1.65806081157687E-5,
2.30369726850326E-5,2.67819200416086E-5,3.59736924188203E-5,4.03862783807E-5),
 .UNSPECIFIED.);
#26532=B_SPLINE_CURVE_WITH_KNOTS('',3,(#438582,#438583,#438584,#438585),
 .UNSPECIFIED.,.F.,.F.,(4,4),(0.,7.7002563062924E-5),.UNSPECIFIED.);
#26533=B_SPLINE_CURVE_WITH_KNOTS('',3,(#438595,#438596,#438597,#438598),
 .UNSPECIFIED.,.F.,.F.,(4,4),(4.33680868994202E-19,7.70025630629233E-5),
 .UNSPECIFIED.);
#26534=B_SPLINE_CURVE_WITH_KNOTS('',3,(#438602,#438603,#438604,#438605,
#438606,#438607,#438608,#438609,#438610,#438611,#438612,#438613,#438614,
#438615,#438616,#438617,#438618,#438619,#438620,#438621,#438622,#438623,
#438624,#438625,#438626,#438627,#438628,#438629,#438630,#438631,#438632,
#438633,#438634,#438635,#438636,#438637,#438638),.UNSPECIFIED.,.F.,.F.,
(4,3,3,3,3,3,3,3,3,3,3,3,4),(0.,9.59031527199921E-6,1.94769411222901E-5,
2.02405092183154E-5,3.21374138577632E-5,3.60302195070441E-5,4.42640648818578E-5,
4.53660204229444E-5,5.03633762302122E-5,5.17708036292897E-5,5.37928993851991E-5,
5.541037554602E-5,5.64557889513533E-5),.UNSPECIFIED.);
#26535=B_SPLINE_CURVE_WITH_KNOTS('',3,(#438639,#438640,#438641,#438642,
#438643,#438644,#438645,#438646,#438647,#438648,#438649,#438650,#438651,
#438652,#438653,#438654,#438655,#438656,#438657,#438658,#438659,#438660,
#438661,#438662,#438663,#438664,#438665,#438666),.UNSPECIFIED.,.F.,.F.,
(4,3,3,3,3,3,3,3,3,4),(5.64557889513533E-5,5.98940966493752E-5,6.34214003873381E-5,
7.2224147608471E-5,7.38322796533365E-5,8.36529189331559E-5,8.807142782225E-5,
9.84837568501025E-5,0.000108624704079196,0.000110823272382853),
 .UNSPECIFIED.);
#26536=B_SPLINE_CURVE_WITH_KNOTS('',3,(#438682,#438683,#438684,#438685,
#438686,#438687,#438688,#438689,#438690,#438691,#438692,#438693,#438694,
#438695,#438696,#438697,#438698,#438699,#438700,#438701,#438702,#438703,
#438704,#438705,#438706,#438707,#438708,#438709),.UNSPECIFIED.,.F.,.F.,
(4,3,3,3,3,3,3,3,3,4),(0.,8.66039628578054E-6,1.64707715200668E-5,2.24502894132268E-5,
2.49975961757825E-5,2.88526003690282E-5,3.10661348995018E-5,3.43053543516961E-5,
3.66410545653559E-5,4.00504537627886E-5),.UNSPECIFIED.);
#26537=B_SPLINE_CURVE_WITH_KNOTS('',3,(#438712,#438713,#438714,#438715,
#438716,#438717,#438718),.UNSPECIFIED.,.F.,.F.,(4,3,4),(0.,4.4000004106538E-5,
9.89910850773115E-5),.UNSPECIFIED.);
#26538=B_SPLINE_CURVE_WITH_KNOTS('',3,(#438739,#438740,#438741,#438742,
#438743,#438744,#438745,#438746,#438747,#438748,#438749,#438750,#438751,
#438752,#438753,#438754,#438755,#438756,#438757,#438758,#438759,#438760,
#438761,#438762,#438763,#438764,#438765,#438766,#438767,#438768,#438769,
#438770,#438771,#438772),.UNSPECIFIED.,.F.,.F.,(4,3,3,3,3,3,3,3,3,3,3,4),
(0.,4.29157837304534E-6,5.42772623795311E-6,1.00901698482347E-5,1.31279195068639E-5,
1.57383542265917E-5,1.61011507492105E-5,1.67166789291755E-5,1.95343262811359E-5,
2.29377234674649E-5,2.71556047620057E-5,3.34407099942656E-5),
 .UNSPECIFIED.);
#26539=B_SPLINE_CURVE_WITH_KNOTS('',3,(#438785,#438786,#438787,#438788,
#438789,#438790,#438791,#438792,#438793,#438794,#438795,#438796,#438797,
#438798,#438799,#438800,#438801,#438802,#438803,#438804,#438805,#438806,
#438807,#438808,#438809,#438810,#438811,#438812,#438813,#438814,#438815,
#438816,#438817,#438818),.UNSPECIFIED.,.F.,.F.,(4,3,3,3,3,3,3,3,3,3,3,4),
(3.25260651745651E-19,3.71309426656627E-6,5.39981071559409E-6,8.78933289367001E-6,
9.00272357067521E-6,1.07143984504148E-5,1.60780299679545E-5,1.65806081157686E-5,
2.30369726850601E-5,2.67819200416085E-5,3.59736924187893E-5,4.03862783807E-5),
 .UNSPECIFIED.);
#26540=B_SPLINE_CURVE_WITH_KNOTS('',3,(#438931,#438932,#438933,#438934),
 .UNSPECIFIED.,.F.,.F.,(4,4),(0.,7.70025630629238E-5),.UNSPECIFIED.);
#26541=B_SPLINE_CURVE_WITH_KNOTS('',3,(#438944,#438945,#438946,#438947),
 .UNSPECIFIED.,.F.,.F.,(4,4),(4.47028007668187E-19,7.70025630629238E-5),
 .UNSPECIFIED.);
#26542=B_SPLINE_CURVE_WITH_KNOTS('',3,(#438951,#438952,#438953,#438954,
#438955,#438956,#438957,#438958,#438959,#438960,#438961,#438962,#438963,
#438964,#438965,#438966,#438967,#438968,#438969,#438970,#438971,#438972,
#438973,#438974,#438975,#438976,#438977,#438978,#438979,#438980,#438981,
#438982,#438983,#438984,#438985,#438986,#438987),.UNSPECIFIED.,.F.,.F.,
(4,3,3,3,3,3,3,3,3,3,3,3,4),(0.,9.59031527198971E-6,1.94769411222721E-5,
2.02405092183151E-5,3.2137413857768E-5,3.60302195070439E-5,4.42640648818942E-5,
4.53660204229443E-5,5.03633762302038E-5,5.17708036292894E-5,5.37928993851986E-5,
5.54103755460195E-5,5.64557889510681E-5),.UNSPECIFIED.);
#26543=B_SPLINE_CURVE_WITH_KNOTS('',3,(#438988,#438989,#438990,#438991,
#438992,#438993,#438994,#438995,#438996,#438997,#438998,#438999,#439000,
#439001,#439002,#439003,#439004,#439005,#439006,#439007,#439008,#439009,
#439010,#439011,#439012,#439013,#439014,#439015),.UNSPECIFIED.,.F.,.F.,
(4,3,3,3,3,3,3,3,3,4),(5.64557889510681E-5,5.98940966493749E-5,6.34214003873378E-5,
7.22241476084715E-5,7.38322796533362E-5,8.36529189331469E-5,8.80714278222497E-5,
9.84837568500673E-5,0.000108624704079129,0.000110823272382853),
 .UNSPECIFIED.);
#26544=B_SPLINE_CURVE_WITH_KNOTS('',3,(#439031,#439032,#439033,#439034,
#439035,#439036,#439037,#439038,#439039,#439040,#439041,#439042,#439043,
#439044,#439045,#439046,#439047,#439048,#439049,#439050,#439051,#439052,
#439053,#439054,#439055,#439056,#439057,#439058),.UNSPECIFIED.,.F.,.F.,
(4,3,3,3,3,3,3,3,3,4),(0.,8.66039628580409E-6,1.64707715200665E-5,2.24502894132433E-5,
2.49975961757824E-5,2.8852600369028E-5,3.10661348995016E-5,3.4305354351696E-5,
3.66410545653558E-5,4.00504537627886E-5),.UNSPECIFIED.);
#26545=B_SPLINE_CURVE_WITH_KNOTS('',3,(#439061,#439062,#439063,#439064,
#439065,#439066,#439067),.UNSPECIFIED.,.F.,.F.,(4,3,4),(0.,4.40000041065376E-5,
9.89910850773111E-5),.UNSPECIFIED.);
#26546=B_SPLINE_CURVE_WITH_KNOTS('',3,(#439088,#439089,#439090,#439091,
#439092,#439093,#439094,#439095,#439096,#439097,#439098,#439099,#439100,
#439101,#439102,#439103,#439104,#439105,#439106,#439107,#439108,#439109,
#439110,#439111,#439112,#439113,#439114,#439115,#439116,#439117,#439118,
#439119,#439120,#439121),.UNSPECIFIED.,.F.,.F.,(4,3,3,3,3,3,3,3,3,3,3,4),
(0.,4.2915783730258E-6,5.42772623795346E-6,1.00901698482349E-5,1.31279195068641E-5,
1.57383542265877E-5,1.61011507492107E-5,1.67166789291757E-5,1.9534326281136E-5,
2.29377234674651E-5,2.7155604762006E-5,3.34407099942659E-5),
 .UNSPECIFIED.);
#26547=B_SPLINE_CURVE_WITH_KNOTS('',3,(#439134,#439135,#439136,#439137,
#439138,#439139,#439140,#439141,#439142,#439143,#439144,#439145,#439146,
#439147,#439148,#439149,#439150,#439151,#439152,#439153,#439154,#439155,
#439156,#439157,#439158,#439159,#439160,#439161,#439162,#439163,#439164,
#439165,#439166,#439167),.UNSPECIFIED.,.F.,.F.,(4,3,3,3,3,3,3,3,3,3,3,4),
(1.0842021724855E-19,3.7130942665664E-6,5.39981071559421E-6,8.78933289366966E-6,
9.00272357067517E-6,1.07143984504149E-5,1.60780299679564E-5,1.65806081157687E-5,
2.30369726850369E-5,2.67819200416086E-5,3.59736924188085E-5,4.03862783807002E-5),
 .UNSPECIFIED.);
#26548=B_SPLINE_CURVE_WITH_KNOTS('',3,(#439280,#439281,#439282,#439283),
 .UNSPECIFIED.,.F.,.F.,(4,4),(0.,7.70025630629239E-5),.UNSPECIFIED.);
#26549=B_SPLINE_CURVE_WITH_KNOTS('',3,(#439293,#439294,#439295,#439296),
 .UNSPECIFIED.,.F.,.F.,(4,4),(4.37055868292169E-19,7.70025630629235E-5),
 .UNSPECIFIED.);
#26550=B_SPLINE_CURVE_WITH_KNOTS('',3,(#439300,#439301,#439302,#439303,
#439304,#439305,#439306,#439307,#439308,#439309,#439310,#439311,#439312,
#439313,#439314,#439315,#439316,#439317,#439318,#439319,#439320,#439321,
#439322,#439323,#439324,#439325,#439326,#439327,#439328,#439329,#439330,
#439331,#439332,#439333,#439334,#439335,#439336),.UNSPECIFIED.,.F.,.F.,
(4,3,3,3,3,3,3,3,3,3,3,3,4),(0.,9.59031527199935E-6,1.94769411222823E-5,
2.02405092183153E-5,3.21374138577703E-5,3.60302195070441E-5,4.4264064881889E-5,
4.53660204229445E-5,5.03633762302015E-5,5.17708036292898E-5,5.3792899385199E-5,
5.541037554602E-5,5.64557889510303E-5),.UNSPECIFIED.);
#26551=B_SPLINE_CURVE_WITH_KNOTS('',3,(#439337,#439338,#439339,#439340,
#439341,#439342,#439343,#439344,#439345,#439346,#439347,#439348,#439349,
#439350,#439351,#439352,#439353,#439354,#439355,#439356,#439357,#439358,
#439359,#439360,#439361,#439362,#439363,#439364),.UNSPECIFIED.,.F.,.F.,
(4,3,3,3,3,3,3,3,3,4),(5.64557889510303E-5,5.98940966493752E-5,6.34214003873382E-5,
7.22241476084422E-5,7.38322796533368E-5,8.36529189331455E-5,8.80714278222503E-5,
9.8483756850078E-5,0.000108624704079147,0.000110823272382854),
 .UNSPECIFIED.);
#26552=B_SPLINE_CURVE_WITH_KNOTS('',3,(#439380,#439381,#439382,#439383,
#439384,#439385,#439386,#439387,#439388,#439389,#439390,#439391,#439392,
#439393,#439394,#439395,#439396,#439397,#439398,#439399,#439400,#439401,
#439402,#439403,#439404,#439405,#439406,#439407),.UNSPECIFIED.,.F.,.F.,
(4,3,3,3,3,3,3,3,3,4),(0.,8.66039628584726E-6,1.64707715200667E-5,2.2450289413223E-5,
2.49975961757824E-5,2.88526003690281E-5,3.10661348995017E-5,3.43053543516961E-5,
3.66410545653559E-5,4.00504537627887E-5),.UNSPECIFIED.);
#26553=B_SPLINE_CURVE_WITH_KNOTS('',3,(#439410,#439411,#439412,#439413,
#439414,#439415,#439416),.UNSPECIFIED.,.F.,.F.,(4,3,4),(0.,4.40000041065376E-5,
9.89910850773114E-5),.UNSPECIFIED.);
#26554=B_SPLINE_CURVE_WITH_KNOTS('',3,(#439437,#439438,#439439,#439440,
#439441,#439442,#439443,#439444,#439445,#439446,#439447,#439448,#439449,
#439450,#439451,#439452,#439453,#439454,#439455,#439456,#439457,#439458,
#439459,#439460,#439461,#439462,#439463,#439464,#439465,#439466,#439467,
#439468,#439469,#439470),.UNSPECIFIED.,.F.,.F.,(4,3,3,3,3,3,3,3,3,3,3,4),
(0.,4.29157837304442E-6,5.42772623795332E-6,1.00901698482346E-5,1.31279195068639E-5,
1.57383542265886E-5,1.61011507492104E-5,1.67166789291752E-5,1.95343262811359E-5,
2.29377234674649E-5,2.71556047620057E-5,3.34407099942661E-5),
 .UNSPECIFIED.);
#26555=B_SPLINE_CURVE_WITH_KNOTS('',3,(#439483,#439484,#439485,#439486,
#439487,#439488,#439489,#439490,#439491,#439492,#439493,#439494,#439495,
#439496,#439497,#439498,#439499,#439500,#439501,#439502,#439503,#439504,
#439505,#439506,#439507,#439508,#439509,#439510,#439511,#439512,#439513,
#439514,#439515,#439516),.UNSPECIFIED.,.F.,.F.,(4,3,3,3,3,3,3,3,3,3,3,4),
(1.0842021724855E-19,3.71309426656646E-6,5.39981071559411E-6,8.78933289331216E-6,
9.00272357067517E-6,1.07143984504148E-5,1.60780299679535E-5,1.65806081157685E-5,
2.30369726850261E-5,2.67819200416085E-5,3.59736924187453E-5,4.03862783806999E-5),
 .UNSPECIFIED.);
#26556=B_SPLINE_CURVE_WITH_KNOTS('',3,(#439629,#439630,#439631,#439632),
 .UNSPECIFIED.,.F.,.F.,(4,4),(0.,7.7002563062924E-5),.UNSPECIFIED.);
#26557=B_SPLINE_CURVE_WITH_KNOTS('',3,(#439642,#439643,#439644,#439645),
 .UNSPECIFIED.,.F.,.F.,(4,4),(4.41238316394827E-19,7.70025630629232E-5),
 .UNSPECIFIED.);
#26558=B_SPLINE_CURVE_WITH_KNOTS('',3,(#439649,#439650,#439651,#439652,
#439653,#439654,#439655,#439656,#439657,#439658,#439659,#439660,#439661,
#439662,#439663,#439664,#439665,#439666,#439667,#439668,#439669,#439670,
#439671,#439672,#439673,#439674,#439675,#439676,#439677,#439678,#439679,
#439680,#439681,#439682,#439683,#439684,#439685),.UNSPECIFIED.,.F.,.F.,
(4,3,3,3,3,3,3,3,3,3,3,3,4),(0.,9.59031527201392E-6,1.94769411223066E-5,
2.02405092183155E-5,3.2137413857776E-5,3.60302195070442E-5,4.42640648817747E-5,
4.53660204229446E-5,5.03633762302201E-5,5.17708036292898E-5,5.37928993851991E-5,
5.54103755460201E-5,5.64557889513918E-5),.UNSPECIFIED.);
#26559=B_SPLINE_CURVE_WITH_KNOTS('',3,(#439686,#439687,#439688,#439689,
#439690,#439691,#439692,#439693,#439694,#439695,#439696,#439697,#439698,
#439699,#439700,#439701,#439702,#439703,#439704,#439705,#439706,#439707,
#439708,#439709,#439710,#439711,#439712,#439713),.UNSPECIFIED.,.F.,.F.,
(4,3,3,3,3,3,3,3,3,4),(5.64557889513918E-5,5.98940966493753E-5,6.34214003873382E-5,
7.22241476084647E-5,7.38322796533367E-5,8.36529189331493E-5,8.80714278222502E-5,
9.84837568500753E-5,0.000108624704079138,0.000110823272382854),
 .UNSPECIFIED.);
#26560=B_SPLINE_CURVE_WITH_KNOTS('',3,(#439729,#439730,#439731,#439732,
#439733,#439734,#439735,#439736,#439737,#439738,#439739,#439740,#439741,
#439742,#439743,#439744,#439745,#439746,#439747,#439748,#439749,#439750,
#439751,#439752,#439753,#439754,#439755,#439756),.UNSPECIFIED.,.F.,.F.,
(4,3,3,3,3,3,3,3,3,4),(0.,8.6603962857847E-6,1.64707715200667E-5,2.24502894132614E-5,
2.49975961757825E-5,2.88526003690281E-5,3.10661348995017E-5,3.43053543516961E-5,
3.66410545653559E-5,4.00504537627886E-5),.UNSPECIFIED.);
#26561=B_SPLINE_CURVE_WITH_KNOTS('',3,(#439759,#439760,#439761,#439762,
#439763,#439764,#439765),.UNSPECIFIED.,.F.,.F.,(4,3,4),(0.,4.40000041065375E-5,
9.89910850773112E-5),.UNSPECIFIED.);
#26562=B_SPLINE_CURVE_WITH_KNOTS('',3,(#439786,#439787,#439788,#439789,
#439790,#439791,#439792,#439793,#439794,#439795,#439796,#439797,#439798,
#439799,#439800,#439801,#439802,#439803,#439804,#439805,#439806,#439807,
#439808,#439809,#439810,#439811,#439812,#439813,#439814,#439815,#439816,
#439817,#439818,#439819),.UNSPECIFIED.,.F.,.F.,(4,3,3,3,3,3,3,3,3,3,3,4),
(0.,4.29157837304389E-6,5.42772623795354E-6,1.0090169848235E-5,1.31279195068641E-5,
1.57383542265878E-5,1.61011507492106E-5,1.67166789291757E-5,1.9534326281136E-5,
2.2937723467465E-5,2.71556047620059E-5,3.3440709994266E-5),
 .UNSPECIFIED.);
#26563=B_SPLINE_CURVE_WITH_KNOTS('',3,(#439832,#439833,#439834,#439835,
#439836,#439837,#439838,#439839,#439840,#439841,#439842,#439843,#439844,
#439845,#439846,#439847,#439848,#439849,#439850,#439851,#439852,#439853,
#439854,#439855,#439856,#439857,#439858,#439859,#439860,#439861,#439862,
#439863,#439864,#439865),.UNSPECIFIED.,.F.,.F.,(4,3,3,3,3,3,3,3,3,3,3,4),
(8.13151629364128E-20,3.71309426656647E-6,5.39981071559418E-6,8.78933289332817E-6,
9.0027235706752E-6,1.07143984504149E-5,1.60780299679466E-5,1.65806081157687E-5,
2.30369726850553E-5,2.67819200416087E-5,3.59736924187626E-5,4.03862783807002E-5),
 .UNSPECIFIED.);
#26564=B_SPLINE_CURVE_WITH_KNOTS('',3,(#439978,#439979,#439980,#439981),
 .UNSPECIFIED.,.F.,.F.,(4,4),(0.,7.70025630629236E-5),.UNSPECIFIED.);
#26565=B_SPLINE_CURVE_WITH_KNOTS('',3,(#439991,#439992,#439993,#439994),
 .UNSPECIFIED.,.F.,.F.,(4,4),(4.47028007668187E-19,7.70025630629236E-5),
 .UNSPECIFIED.);
#26566=B_SPLINE_CURVE_WITH_KNOTS('',3,(#439998,#439999,#440000,#440001,
#440002,#440003,#440004,#440005,#440006,#440007,#440008,#440009,#440010,
#440011,#440012,#440013,#440014,#440015,#440016,#440017,#440018,#440019,
#440020,#440021,#440022,#440023,#440024,#440025,#440026,#440027,#440028,
#440029,#440030,#440031,#440032,#440033,#440034),.UNSPECIFIED.,.F.,.F.,
(4,3,3,3,3,3,3,3,3,3,3,3,4),(0.,9.59031527201329E-6,1.94769411223138E-5,
2.02405092183152E-5,3.21374138577644E-5,3.6030219507044E-5,4.42640648818663E-5,
4.53660204229444E-5,5.03633762301941E-5,5.17708036292896E-5,5.37928993851989E-5,
5.54103755460198E-5,5.64557889511221E-5),.UNSPECIFIED.);
#26567=B_SPLINE_CURVE_WITH_KNOTS('',3,(#440035,#440036,#440037,#440038,
#440039,#440040,#440041,#440042,#440043,#440044,#440045,#440046,#440047,
#440048,#440049,#440050,#440051,#440052,#440053,#440054,#440055,#440056,
#440057,#440058,#440059,#440060,#440061,#440062),.UNSPECIFIED.,.F.,.F.,
(4,3,3,3,3,3,3,3,3,4),(5.64557889511221E-5,5.98940966493751E-5,6.34214003873381E-5,
7.22241476084529E-5,7.38322796533365E-5,8.36529189331292E-5,8.807142782225E-5,
9.84837568500623E-5,0.000108624704079134,0.000110823272382854),
 .UNSPECIFIED.);
#26568=B_SPLINE_CURVE_WITH_KNOTS('',3,(#440078,#440079,#440080,#440081,
#440082,#440083,#440084,#440085,#440086,#440087,#440088,#440089,#440090,
#440091,#440092,#440093,#440094,#440095,#440096,#440097,#440098,#440099,
#440100,#440101,#440102,#440103,#440104,#440105),.UNSPECIFIED.,.F.,.F.,
(4,3,3,3,3,3,3,3,3,4),(0.,8.66039628583239E-6,1.64707715200667E-5,2.24502894132358E-5,
2.49975961757824E-5,2.88526003690281E-5,3.10661348995017E-5,3.43053543516961E-5,
3.66410545653561E-5,4.00504537627891E-5),.UNSPECIFIED.);
#26569=B_SPLINE_CURVE_WITH_KNOTS('',3,(#440108,#440109,#440110,#440111,
#440112,#440113,#440114),.UNSPECIFIED.,.F.,.F.,(4,3,4),(0.,4.40000041065376E-5,
9.89910850773112E-5),.UNSPECIFIED.);
#26570=B_SPLINE_CURVE_WITH_KNOTS('',3,(#440135,#440136,#440137,#440138,
#440139,#440140,#440141,#440142,#440143,#440144,#440145,#440146,#440147,
#440148,#440149,#440150,#440151,#440152,#440153,#440154,#440155,#440156,
#440157,#440158,#440159,#440160,#440161,#440162,#440163,#440164,#440165,
#440166,#440167,#440168),.UNSPECIFIED.,.F.,.F.,(4,3,3,3,3,3,3,3,3,3,3,4),
(0.,4.2915783730137E-6,5.42772623795345E-6,1.00901698482348E-5,1.31279195068639E-5,
1.57383542265848E-5,1.61011507492105E-5,1.67166789291754E-5,1.95343262811359E-5,
2.29377234674649E-5,2.71556047620058E-5,3.34407099942659E-5),
 .UNSPECIFIED.);
#26571=B_SPLINE_CURVE_WITH_KNOTS('',3,(#440181,#440182,#440183,#440184,
#440185,#440186,#440187,#440188,#440189,#440190,#440191,#440192,#440193,
#440194,#440195,#440196,#440197,#440198,#440199,#440200,#440201,#440202,
#440203,#440204,#440205,#440206,#440207,#440208,#440209,#440210,#440211,
#440212,#440213,#440214),.UNSPECIFIED.,.F.,.F.,(4,3,3,3,3,3,3,3,3,3,3,4),
(8.13151629364128E-20,3.71309426656648E-6,5.39981071559416E-6,8.78933289331532E-6,
9.00272357067522E-6,1.07143984504149E-5,1.60780299679582E-5,1.65806081157687E-5,
2.30369726850442E-5,2.67819200416087E-5,3.5973692418805E-5,4.03862783807002E-5),
 .UNSPECIFIED.);
#26572=B_SPLINE_CURVE_WITH_KNOTS('',3,(#440327,#440328,#440329,#440330),
 .UNSPECIFIED.,.F.,.F.,(4,4),(0.,7.70025630629243E-5),.UNSPECIFIED.);
#26573=B_SPLINE_CURVE_WITH_KNOTS('',3,(#440340,#440341,#440342,#440343),
 .UNSPECIFIED.,.F.,.F.,(4,4),(1.0842021724855E-19,7.70025630629239E-5),
 .UNSPECIFIED.);
#26574=B_SPLINE_CURVE_WITH_KNOTS('',3,(#440347,#440348,#440349,#440350,
#440351,#440352,#440353,#440354,#440355,#440356,#440357,#440358,#440359,
#440360,#440361,#440362,#440363,#440364,#440365,#440366,#440367,#440368,
#440369,#440370,#440371,#440372,#440373,#440374,#440375,#440376,#440377,
#440378,#440379,#440380,#440381,#440382,#440383),.UNSPECIFIED.,.F.,.F.,
(4,3,3,3,3,3,3,3,3,3,3,3,4),(0.,9.59031527198821E-6,1.94769411222708E-5,
2.0240509218315E-5,3.21374138577731E-5,3.60302195070438E-5,4.42640648818033E-5,
4.53660204229442E-5,5.03633762302213E-5,5.17708036292894E-5,5.37928993851987E-5,
5.54103755460196E-5,5.64557889510612E-5),.UNSPECIFIED.);
#26575=B_SPLINE_CURVE_WITH_KNOTS('',3,(#440384,#440385,#440386,#440387,
#440388,#440389,#440390,#440391,#440392,#440393,#440394,#440395,#440396,
#440397,#440398,#440399,#440400,#440401,#440402,#440403,#440404,#440405,
#440406,#440407,#440408,#440409,#440410,#440411),.UNSPECIFIED.,.F.,.F.,
(4,3,3,3,3,3,3,3,3,4),(5.64557889510612E-5,5.9894096649375E-5,6.34214003873378E-5,
7.22241476084378E-5,7.38322796533361E-5,8.36529189331501E-5,8.80714278222497E-5,
9.84837568500782E-5,0.00010862470407915,0.000110823272382853),
 .UNSPECIFIED.);
#26576=B_SPLINE_CURVE_WITH_KNOTS('',3,(#440427,#440428,#440429,#440430,
#440431,#440432,#440433,#440434,#440435,#440436,#440437,#440438,#440439,
#440440,#440441,#440442,#440443,#440444,#440445,#440446,#440447,#440448,
#440449,#440450,#440451,#440452,#440453,#440454),.UNSPECIFIED.,.F.,.F.,
(4,3,3,3,3,3,3,3,3,4),(0.,8.66039628581255E-6,1.64707715200667E-5,2.24502894132374E-5,
2.49975961757822E-5,2.8852600369028E-5,3.10661348995016E-5,3.43053543516961E-5,
3.6641054565356E-5,4.00504537627891E-5),.UNSPECIFIED.);
#26577=B_SPLINE_CURVE_WITH_KNOTS('',3,(#440457,#440458,#440459,#440460,
#440461,#440462,#440463),.UNSPECIFIED.,.F.,.F.,(4,3,4),(0.,4.40000041065373E-5,
9.89910850773114E-5),.UNSPECIFIED.);
#26578=B_SPLINE_CURVE_WITH_KNOTS('',3,(#440484,#440485,#440486,#440487,
#440488,#440489,#440490,#440491,#440492,#440493,#440494,#440495,#440496,
#440497,#440498,#440499,#440500,#440501,#440502,#440503,#440504,#440505,
#440506,#440507,#440508,#440509,#440510,#440511,#440512,#440513,#440514,
#440515,#440516,#440517),.UNSPECIFIED.,.F.,.F.,(4,3,3,3,3,3,3,3,3,3,3,4),
(0.,4.2915783730491E-6,5.42772623795335E-6,1.00901698482346E-5,1.31279195068638E-5,
1.57383542265797E-5,1.61011507492104E-5,1.67166789291761E-5,1.95343262811359E-5,
2.2937723467465E-5,2.71556047620059E-5,3.34407099942659E-5),
 .UNSPECIFIED.);
#26579=B_SPLINE_CURVE_WITH_KNOTS('',3,(#440530,#440531,#440532,#440533,
#440534,#440535,#440536,#440537,#440538,#440539,#440540,#440541,#440542,
#440543,#440544,#440545,#440546,#440547,#440548,#440549,#440550,#440551,
#440552,#440553,#440554,#440555,#440556,#440557,#440558,#440559,#440560,
#440561,#440562,#440563),.UNSPECIFIED.,.F.,.F.,(4,3,3,3,3,3,3,3,3,3,3,4),
(1.0842021724855E-19,3.71309426656638E-6,5.39981071559417E-6,8.78933289369073E-6,
9.00272357067512E-6,1.07143984504148E-5,1.6078029967961E-5,1.65806081157686E-5,
2.30369726850332E-5,2.67819200416086E-5,3.5973692418783E-5,4.03862783806998E-5),
 .UNSPECIFIED.);
#26580=B_SPLINE_CURVE_WITH_KNOTS('',3,(#440676,#440677,#440678,#440679),
 .UNSPECIFIED.,.F.,.F.,(4,4),(0.,7.70025630629237E-5),.UNSPECIFIED.);
#26581=B_SPLINE_CURVE_WITH_KNOTS('',3,(#440689,#440690,#440691,#440692),
 .UNSPECIFIED.,.F.,.F.,(4,4),(1.0842021724855E-19,7.70025630629236E-5),
 .UNSPECIFIED.);
#26582=B_SPLINE_CURVE_WITH_KNOTS('',3,(#440696,#440697,#440698,#440699,
#440700,#440701,#440702,#440703,#440704,#440705,#440706,#440707,#440708,
#440709,#440710,#440711,#440712,#440713,#440714,#440715,#440716,#440717,
#440718,#440719,#440720,#440721,#440722,#440723,#440724,#440725,#440726,
#440727,#440728,#440729,#440730,#440731,#440732),.UNSPECIFIED.,.F.,.F.,
(4,3,3,3,3,3,3,3,3,3,3,3,4),(0.,9.59031527199807E-6,1.94769411222929E-5,
2.02405092183153E-5,3.21374138577713E-5,3.60302195070441E-5,4.42640648819238E-5,
4.53660204229445E-5,5.03633762301965E-5,5.17708036292898E-5,5.37928993851992E-5,
5.54103755460202E-5,5.64557889512322E-5),.UNSPECIFIED.);
#26583=B_SPLINE_CURVE_WITH_KNOTS('',3,(#440733,#440734,#440735,#440736,
#440737,#440738,#440739,#440740,#440741,#440742,#440743,#440744,#440745,
#440746,#440747,#440748,#440749,#440750,#440751,#440752,#440753,#440754,
#440755,#440756,#440757,#440758,#440759,#440760),.UNSPECIFIED.,.F.,.F.,
(4,3,3,3,3,3,3,3,3,4),(5.64557889512322E-5,5.98940966493754E-5,6.34214003873382E-5,
7.22241476084645E-5,7.38322796533368E-5,8.36529189331482E-5,8.80714278222504E-5,
9.84837568500693E-5,0.000108624704079132,0.000110823272382854),
 .UNSPECIFIED.);
#26584=B_SPLINE_CURVE_WITH_KNOTS('',3,(#440776,#440777,#440778,#440779,
#440780,#440781,#440782,#440783,#440784,#440785,#440786,#440787,#440788,
#440789,#440790,#440791,#440792,#440793,#440794,#440795,#440796,#440797,
#440798,#440799,#440800,#440801,#440802,#440803),.UNSPECIFIED.,.F.,.F.,
(4,3,3,3,3,3,3,3,3,4),(0.,8.66039628580622E-6,1.64707715200666E-5,2.24502894132216E-5,
2.49975961757823E-5,2.8852600369028E-5,3.10661348995015E-5,3.43053543516959E-5,
3.66410545653559E-5,4.00504537627886E-5),.UNSPECIFIED.);
#26585=B_SPLINE_CURVE_WITH_KNOTS('',3,(#440806,#440807,#440808,#440809,
#440810,#440811,#440812),.UNSPECIFIED.,.F.,.F.,(4,3,4),(0.,4.40000041065376E-5,
9.89910850773115E-5),.UNSPECIFIED.);
#26586=B_SPLINE_CURVE_WITH_KNOTS('',3,(#440833,#440834,#440835,#440836,
#440837,#440838,#440839,#440840,#440841,#440842,#440843,#440844,#440845,
#440846,#440847,#440848,#440849,#440850,#440851,#440852,#440853,#440854,
#440855,#440856,#440857,#440858,#440859,#440860,#440861,#440862,#440863,
#440864,#440865,#440866),.UNSPECIFIED.,.F.,.F.,(4,3,3,3,3,3,3,3,3,3,3,4),
(0.,4.29157837304607E-6,5.4277262379532E-6,1.00901698482346E-5,1.31279195068638E-5,
1.57383542265904E-5,1.61011507492105E-5,1.67166789291756E-5,1.95343262811358E-5,
2.29377234674647E-5,2.71556047620058E-5,3.34407099942655E-5),
 .UNSPECIFIED.);
#26587=B_SPLINE_CURVE_WITH_KNOTS('',3,(#440879,#440880,#440881,#440882,
#440883,#440884,#440885,#440886,#440887,#440888,#440889,#440890,#440891,
#440892,#440893,#440894,#440895,#440896,#440897,#440898,#440899,#440900,
#440901,#440902,#440903,#440904,#440905,#440906,#440907,#440908,#440909,
#440910,#440911,#440912),.UNSPECIFIED.,.F.,.F.,(4,3,3,3,3,3,3,3,3,3,3,4),
(1.0842021724855E-19,3.71309426656633E-6,5.39981071559412E-6,8.78933289368465E-6,
9.00272357067514E-6,1.07143984504148E-5,1.60780299679548E-5,1.65806081157686E-5,
2.30369726850478E-5,2.67819200416084E-5,3.59736924187961E-5,4.03862783806998E-5),
 .UNSPECIFIED.);
#26588=B_SPLINE_CURVE_WITH_KNOTS('',3,(#441025,#441026,#441027,#441028),
 .UNSPECIFIED.,.F.,.F.,(4,4),(0.,7.70025630629242E-5),.UNSPECIFIED.);
#26589=B_SPLINE_CURVE_WITH_KNOTS('',3,(#441038,#441039,#441040,#441041),
 .UNSPECIFIED.,.F.,.F.,(4,4),(1.0842021724855E-19,7.7002563062924E-5),
 .UNSPECIFIED.);
#26590=B_SPLINE_CURVE_WITH_KNOTS('',3,(#441045,#441046,#441047,#441048,
#441049,#441050,#441051,#441052,#441053,#441054,#441055,#441056,#441057,
#441058,#441059,#441060,#441061,#441062,#441063,#441064,#441065,#441066,
#441067,#441068,#441069,#441070,#441071,#441072,#441073,#441074,#441075,
#441076,#441077,#441078,#441079,#441080,#441081),.UNSPECIFIED.,.F.,.F.,
(4,3,3,3,3,3,3,3,3,3,3,3,4),(0.,9.59031527199008E-6,1.94769411222735E-5,
2.02405092183149E-5,3.21374138577699E-5,3.60302195070437E-5,4.42640648818485E-5,
4.53660204229443E-5,5.03633762302068E-5,5.17708036292895E-5,5.37928993851988E-5,
5.54103755460198E-5,5.64557889509075E-5),.UNSPECIFIED.);
#26591=B_SPLINE_CURVE_WITH_KNOTS('',3,(#441082,#441083,#441084,#441085,
#441086,#441087,#441088,#441089,#441090,#441091,#441092,#441093,#441094,
#441095,#441096,#441097,#441098,#441099,#441100,#441101,#441102,#441103,
#441104,#441105,#441106,#441107,#441108,#441109),.UNSPECIFIED.,.F.,.F.,
(4,3,3,3,3,3,3,3,3,4),(5.64557889509075E-5,5.98940966493748E-5,6.34214003873379E-5,
7.22241476084888E-5,7.38322796533363E-5,8.36529189331411E-5,8.807142782225E-5,
9.84837568500729E-5,0.000108624704079144,0.000110823272382854),
 .UNSPECIFIED.);
#26592=B_SPLINE_CURVE_WITH_KNOTS('',3,(#441125,#441126,#441127,#441128,
#441129,#441130,#441131,#441132,#441133,#441134,#441135,#441136,#441137,
#441138,#441139,#441140,#441141,#441142,#441143,#441144,#441145,#441146,
#441147,#441148,#441149,#441150,#441151,#441152),.UNSPECIFIED.,.F.,.F.,
(4,3,3,3,3,3,3,3,3,4),(0.,8.66039628583705E-6,1.64707715200666E-5,2.24502894132194E-5,
2.49975961757824E-5,2.8852600369028E-5,3.10661348995015E-5,3.4305354351696E-5,
3.66410545653558E-5,4.00504537627885E-5),.UNSPECIFIED.);
#26593=B_SPLINE_CURVE_WITH_KNOTS('',3,(#441155,#441156,#441157,#441158,
#441159,#441160,#441161),.UNSPECIFIED.,.F.,.F.,(4,3,4),(0.,4.40000041065375E-5,
9.89910850773112E-5),.UNSPECIFIED.);
#26594=B_SPLINE_CURVE_WITH_KNOTS('',3,(#441182,#441183,#441184,#441185,
#441186,#441187,#441188,#441189,#441190,#441191,#441192,#441193,#441194,
#441195,#441196,#441197,#441198,#441199,#441200,#441201,#441202,#441203,
#441204,#441205,#441206,#441207,#441208,#441209,#441210,#441211,#441212,
#441213,#441214,#441215),.UNSPECIFIED.,.F.,.F.,(4,3,3,3,3,3,3,3,3,3,3,4),
(0.,4.29157837302068E-6,5.42772623795361E-6,1.00901698482348E-5,1.31279195068639E-5,
1.57383542265845E-5,1.61011507492104E-5,1.67166789291762E-5,1.95343262811359E-5,
2.29377234674648E-5,2.71556047620061E-5,3.34407099942661E-5),
 .UNSPECIFIED.);
#26595=B_SPLINE_CURVE_WITH_KNOTS('',3,(#441228,#441229,#441230,#441231,
#441232,#441233,#441234,#441235,#441236,#441237,#441238,#441239,#441240,
#441241,#441242,#441243,#441244,#441245,#441246,#441247,#441248,#441249,
#441250,#441251,#441252,#441253,#441254,#441255,#441256,#441257,#441258,
#441259,#441260,#441261),.UNSPECIFIED.,.F.,.F.,(4,3,3,3,3,3,3,3,3,3,3,4),
(1.0842021724855E-19,3.71309426656657E-6,5.3998107155941E-6,8.7893328936576E-6,
9.00272357067521E-6,1.0714398450415E-5,1.60780299679475E-5,1.65806081157686E-5,
2.30369726850495E-5,2.67819200416085E-5,3.59736924187832E-5,4.03862783806998E-5),
 .UNSPECIFIED.);
#26596=B_SPLINE_CURVE_WITH_KNOTS('',3,(#441374,#441375,#441376,#441377),
 .UNSPECIFIED.,.F.,.F.,(4,4),(0.,7.70025630629242E-5),.UNSPECIFIED.);
#26597=B_SPLINE_CURVE_WITH_KNOTS('',3,(#441387,#441388,#441389,#441390),
 .UNSPECIFIED.,.F.,.F.,(4,4),(2.16840434497101E-19,7.70025630629237E-5),
 .UNSPECIFIED.);
#26598=B_SPLINE_CURVE_WITH_KNOTS('',3,(#441394,#441395,#441396,#441397,
#441398,#441399,#441400,#441401,#441402,#441403,#441404,#441405,#441406,
#441407,#441408,#441409,#441410,#441411,#441412,#441413,#441414,#441415,
#441416,#441417,#441418,#441419,#441420,#441421,#441422,#441423,#441424,
#441425,#441426,#441427,#441428,#441429,#441430),.UNSPECIFIED.,.F.,.F.,
(4,3,3,3,3,3,3,3,3,3,3,3,4),(0.,9.59031527197619E-6,1.94769411222538E-5,
2.02405092183151E-5,3.21374138577715E-5,3.60302195070438E-5,4.42640648818347E-5,
4.53660204229442E-5,5.03633762302098E-5,5.17708036292895E-5,5.37928993851989E-5,
5.54103755460198E-5,5.64557889502042E-5),.UNSPECIFIED.);
#26599=B_SPLINE_CURVE_WITH_KNOTS('',3,(#441431,#441432,#441433,#441434,
#441435,#441436,#441437,#441438,#441439,#441440,#441441,#441442,#441443,
#441444,#441445,#441446,#441447,#441448,#441449,#441450,#441451,#441452,
#441453,#441454,#441455,#441456,#441457,#441458),.UNSPECIFIED.,.F.,.F.,
(4,3,3,3,3,3,3,3,3,4),(5.64557889502042E-5,5.9894096649375E-5,6.3421400387338E-5,
7.22241476084978E-5,7.38322796533364E-5,8.36529189331515E-5,8.80714278222499E-5,
9.84837568500678E-5,0.00010862470407913,0.000110823272382853),
 .UNSPECIFIED.);
#26600=B_SPLINE_CURVE_WITH_KNOTS('',3,(#441474,#441475,#441476,#441477,
#441478,#441479,#441480,#441481,#441482,#441483,#441484,#441485,#441486,
#441487,#441488,#441489,#441490,#441491,#441492,#441493,#441494,#441495,
#441496,#441497,#441498,#441499,#441500,#441501),.UNSPECIFIED.,.F.,.F.,
(4,3,3,3,3,3,3,3,3,4),(0.,8.66039628578315E-6,1.64707715200666E-5,2.24502894132418E-5,
2.49975961757825E-5,2.88526003690282E-5,3.10661348995018E-5,3.43053543516961E-5,
3.66410545653561E-5,4.00504537627891E-5),.UNSPECIFIED.);
#26601=B_SPLINE_CURVE_WITH_KNOTS('',3,(#441504,#441505,#441506,#441507,
#441508,#441509,#441510),.UNSPECIFIED.,.F.,.F.,(4,3,4),(0.,4.40000041065374E-5,
9.89910850773113E-5),.UNSPECIFIED.);
#26602=B_SPLINE_CURVE_WITH_KNOTS('',3,(#441531,#441532,#441533,#441534,
#441535,#441536,#441537,#441538,#441539,#441540,#441541,#441542,#441543,
#441544,#441545,#441546,#441547,#441548,#441549,#441550,#441551,#441552,
#441553,#441554,#441555,#441556,#441557,#441558,#441559,#441560,#441561,
#441562,#441563,#441564),.UNSPECIFIED.,.F.,.F.,(4,3,3,3,3,3,3,3,3,3,3,4),
(0.,4.29157837302783E-6,5.42772623795327E-6,1.00901698482347E-5,1.31279195068638E-5,
1.57383542265772E-5,1.61011507492103E-5,1.67166789291755E-5,1.95343262811356E-5,
2.29377234674647E-5,2.71556047620059E-5,3.34407099942655E-5),
 .UNSPECIFIED.);
#26603=B_SPLINE_CURVE_WITH_KNOTS('',3,(#441577,#441578,#441579,#441580,
#441581,#441582,#441583,#441584,#441585,#441586,#441587,#441588,#441589,
#441590,#441591,#441592,#441593,#441594,#441595,#441596,#441597,#441598,
#441599,#441600,#441601,#441602,#441603,#441604,#441605,#441606,#441607,
#441608,#441609,#441610),.UNSPECIFIED.,.F.,.F.,(4,3,3,3,3,3,3,3,3,3,3,4),
(0.,3.71309426656659E-6,5.39981071559433E-6,8.78933289366048E-6,9.00272357067536E-6,
1.0714398450415E-5,1.60780299679548E-5,1.65806081157688E-5,2.3036972685049E-5,
2.67819200416087E-5,3.59736924187513E-5,4.03862783807003E-5),
 .UNSPECIFIED.);
#26604=B_SPLINE_CURVE_WITH_KNOTS('',3,(#441723,#441724,#441725,#441726),
 .UNSPECIFIED.,.F.,.F.,(4,4),(0.,7.70025630629239E-5),.UNSPECIFIED.);
#26605=B_SPLINE_CURVE_WITH_KNOTS('',3,(#441736,#441737,#441738,#441739),
 .UNSPECIFIED.,.F.,.F.,(4,4),(2.16840434497101E-19,7.70025630629239E-5),
 .UNSPECIFIED.);
#26606=B_SPLINE_CURVE_WITH_KNOTS('',3,(#441743,#441744,#441745,#441746,
#441747,#441748,#441749,#441750,#441751,#441752,#441753,#441754,#441755,
#441756,#441757,#441758,#441759,#441760,#441761,#441762,#441763,#441764,
#441765,#441766,#441767,#441768,#441769,#441770,#441771,#441772,#441773,
#441774,#441775,#441776,#441777,#441778,#441779),.UNSPECIFIED.,.F.,.F.,
(4,3,3,3,3,3,3,3,3,3,3,3,4),(0.,9.59031527200763E-6,1.94769411223023E-5,
2.02405092183151E-5,3.21374138577724E-5,3.60302195070439E-5,4.4264064881911E-5,
4.53660204229445E-5,5.03633762301955E-5,5.17708036292899E-5,5.37928993851988E-5,
5.541037554602E-5,5.64557889510721E-5),.UNSPECIFIED.);
#26607=B_SPLINE_CURVE_WITH_KNOTS('',3,(#441780,#441781,#441782,#441783,
#441784,#441785,#441786,#441787,#441788,#441789,#441790,#441791,#441792,
#441793,#441794,#441795,#441796,#441797,#441798,#441799,#441800,#441801,
#441802,#441803,#441804,#441805,#441806,#441807),.UNSPECIFIED.,.F.,.F.,
(4,3,3,3,3,3,3,3,3,4),(5.64557889510721E-5,5.98940966493751E-5,6.34214003873383E-5,
7.2224147608454E-5,7.38322796533366E-5,8.36529189331437E-5,8.80714278222502E-5,
9.84837568500657E-5,0.000108624704079128,0.000110823272382854),
 .UNSPECIFIED.);
#26608=B_SPLINE_CURVE_WITH_KNOTS('',3,(#441823,#441824,#441825,#441826,
#441827,#441828,#441829,#441830,#441831,#441832,#441833,#441834,#441835,
#441836,#441837,#441838,#441839,#441840,#441841,#441842,#441843,#441844,
#441845,#441846,#441847,#441848,#441849,#441850),.UNSPECIFIED.,.F.,.F.,
(4,3,3,3,3,3,3,3,3,4),(0.,8.66039628584837E-6,1.64707715200667E-5,2.24502894132287E-5,
2.49975961757824E-5,2.8852600369028E-5,3.10661348995016E-5,3.4305354351696E-5,
3.6641054565356E-5,4.00504537627888E-5),.UNSPECIFIED.);
#26609=B_SPLINE_CURVE_WITH_KNOTS('',3,(#441853,#441854,#441855,#441856,
#441857,#441858,#441859),.UNSPECIFIED.,.F.,.F.,(4,3,4),(0.,4.40000041065375E-5,
9.89910850773113E-5),.UNSPECIFIED.);
#26610=B_SPLINE_CURVE_WITH_KNOTS('',3,(#441880,#441881,#441882,#441883,
#441884,#441885,#441886,#441887,#441888,#441889,#441890,#441891,#441892,
#441893,#441894,#441895,#441896,#441897,#441898,#441899,#441900,#441901,
#441902,#441903,#441904,#441905,#441906,#441907,#441908,#441909,#441910,
#441911,#441912,#441913),.UNSPECIFIED.,.F.,.F.,(4,3,3,3,3,3,3,3,3,3,3,4),
(0.,4.29157837302178E-6,5.42772623795343E-6,1.00901698482349E-5,1.31279195068641E-5,
1.5738354226582E-5,1.61011507492108E-5,1.67166789291758E-5,1.95343262811362E-5,
2.29377234674655E-5,2.71556047620061E-5,3.34407099942666E-5),
 .UNSPECIFIED.);
#26611=B_SPLINE_CURVE_WITH_KNOTS('',3,(#441926,#441927,#441928,#441929,
#441930,#441931,#441932,#441933,#441934,#441935,#441936,#441937,#441938,
#441939,#441940,#441941,#441942,#441943,#441944,#441945,#441946,#441947,
#441948,#441949,#441950,#441951,#441952,#441953,#441954,#441955,#441956,
#441957,#441958,#441959),.UNSPECIFIED.,.F.,.F.,(4,3,3,3,3,3,3,3,3,3,3,4),
(0.,3.71309426656663E-6,5.39981071559421E-6,8.78933289334327E-6,9.00272357067522E-6,
1.07143984504149E-5,1.60780299679527E-5,1.65806081157686E-5,2.30369726850418E-5,
2.67819200416087E-5,3.59736924188099E-5,4.03862783807004E-5),
 .UNSPECIFIED.);
#26612=B_SPLINE_CURVE_WITH_KNOTS('',3,(#442072,#442073,#442074,#442075),
 .UNSPECIFIED.,.F.,.F.,(4,4),(0.,7.70025630629239E-5),.UNSPECIFIED.);
#26613=B_SPLINE_CURVE_WITH_KNOTS('',3,(#442085,#442086,#442087,#442088),
 .UNSPECIFIED.,.F.,.F.,(4,4),(2.16840434497101E-19,7.70025630629236E-5),
 .UNSPECIFIED.);
#26614=B_SPLINE_CURVE_WITH_KNOTS('',3,(#442092,#442093,#442094,#442095,
#442096,#442097,#442098,#442099,#442100,#442101,#442102,#442103,#442104,
#442105,#442106,#442107,#442108,#442109,#442110,#442111,#442112,#442113,
#442114,#442115,#442116,#442117,#442118,#442119,#442120,#442121,#442122,
#442123,#442124,#442125,#442126,#442127,#442128),.UNSPECIFIED.,.F.,.F.,
(4,3,3,3,3,3,3,3,3,3,3,3,4),(0.,9.59031527201911E-6,1.94769411223113E-5,
2.02405092183152E-5,3.21374138577674E-5,3.6030219507044E-5,4.42640648818895E-5,
4.53660204229443E-5,5.03633762302114E-5,5.17708036292897E-5,5.37928993851987E-5,
5.54103755460198E-5,5.64557889512061E-5),.UNSPECIFIED.);
#26615=B_SPLINE_CURVE_WITH_KNOTS('',3,(#442129,#442130,#442131,#442132,
#442133,#442134,#442135,#442136,#442137,#442138,#442139,#442140,#442141,
#442142,#442143,#442144,#442145,#442146,#442147,#442148,#442149,#442150,
#442151,#442152,#442153,#442154,#442155,#442156),.UNSPECIFIED.,.F.,.F.,
(4,3,3,3,3,3,3,3,3,4),(5.64557889512061E-5,5.98940966493753E-5,6.3421400387338E-5,
7.22241476084492E-5,7.38322796533364E-5,8.3652918933154E-5,8.807142782225E-5,
9.84837568500723E-5,0.000108624704079135,0.000110823272382854),
 .UNSPECIFIED.);
#26616=B_SPLINE_CURVE_WITH_KNOTS('',3,(#442172,#442173,#442174,#442175,
#442176,#442177,#442178,#442179,#442180,#442181,#442182,#442183,#442184,
#442185,#442186,#442187,#442188,#442189,#442190,#442191,#442192,#442193,
#442194,#442195,#442196,#442197,#442198,#442199),.UNSPECIFIED.,.F.,.F.,
(4,3,3,3,3,3,3,3,3,4),(0.,8.66039628581202E-6,1.64707715200667E-5,2.2450289413238E-5,
2.49975961757824E-5,2.88526003690279E-5,3.10661348995017E-5,3.43053543516958E-5,
3.66410545653558E-5,4.00504537627888E-5),.UNSPECIFIED.);
#26617=B_SPLINE_CURVE_WITH_KNOTS('',3,(#442202,#442203,#442204,#442205,
#442206,#442207,#442208),.UNSPECIFIED.,.F.,.F.,(4,3,4),(0.,4.40000041065374E-5,
9.89910850773111E-5),.UNSPECIFIED.);
#26618=B_SPLINE_CURVE_WITH_KNOTS('',3,(#442229,#442230,#442231,#442232,
#442233,#442234,#442235,#442236,#442237,#442238,#442239,#442240,#442241,
#442242,#442243,#442244,#442245,#442246,#442247,#442248,#442249,#442250,
#442251,#442252,#442253,#442254,#442255,#442256,#442257,#442258,#442259,
#442260,#442261,#442262),.UNSPECIFIED.,.F.,.F.,(4,3,3,3,3,3,3,3,3,3,3,4),
(0.,4.29157837304528E-6,5.42772623795349E-6,1.00901698482351E-5,1.31279195068643E-5,
1.5738354226576E-5,1.61011507492107E-5,1.67166789291759E-5,1.95343262811362E-5,
2.29377234674653E-5,2.71556047620063E-5,3.34407099942664E-5),
 .UNSPECIFIED.);
#26619=B_SPLINE_CURVE_WITH_KNOTS('',3,(#442275,#442276,#442277,#442278,
#442279,#442280,#442281,#442282,#442283,#442284,#442285,#442286,#442287,
#442288,#442289,#442290,#442291,#442292,#442293,#442294,#442295,#442296,
#442297,#442298,#442299,#442300,#442301,#442302,#442303,#442304,#442305,
#442306,#442307,#442308),.UNSPECIFIED.,.F.,.F.,(4,3,3,3,3,3,3,3,3,3,3,4),
(0.,3.7130942665664E-6,5.39981071559395E-6,8.78933289368984E-6,9.00272357067498E-6,
1.07143984504148E-5,1.6078029967946E-5,1.65806081157686E-5,2.30369726850543E-5,
2.67819200416085E-5,3.59736924187727E-5,4.03862783807E-5),.UNSPECIFIED.);
#26620=B_SPLINE_CURVE_WITH_KNOTS('',3,(#442421,#442422,#442423,#442424),
 .UNSPECIFIED.,.F.,.F.,(4,4),(0.,7.7002563062924E-5),.UNSPECIFIED.);
#26621=B_SPLINE_CURVE_WITH_KNOTS('',3,(#442434,#442435,#442436,#442437),
 .UNSPECIFIED.,.F.,.F.,(4,4),(2.16840434497101E-19,7.70025630629238E-5),
 .UNSPECIFIED.);
#26622=B_SPLINE_CURVE_WITH_KNOTS('',3,(#442441,#442442,#442443,#442444,
#442445,#442446,#442447,#442448,#442449,#442450,#442451,#442452,#442453,
#442454,#442455,#442456,#442457,#442458,#442459,#442460,#442461,#442462,
#442463,#442464,#442465,#442466,#442467,#442468,#442469,#442470,#442471,
#442472,#442473,#442474,#442475,#442476,#442477),.UNSPECIFIED.,.F.,.F.,
(4,3,3,3,3,3,3,3,3,3,3,3,4),(0.,9.59031527200278E-6,1.94769411222902E-5,
2.02405092183151E-5,3.21374138577676E-5,3.60302195070439E-5,4.426406488193E-5,
4.53660204229443E-5,5.03633762301989E-5,5.17708036292895E-5,5.37928993851989E-5,
5.54103755460197E-5,5.64557889509049E-5),.UNSPECIFIED.);
#26623=B_SPLINE_CURVE_WITH_KNOTS('',3,(#442478,#442479,#442480,#442481,
#442482,#442483,#442484,#442485,#442486,#442487,#442488,#442489,#442490,
#442491,#442492,#442493,#442494,#442495,#442496,#442497,#442498,#442499,
#442500,#442501,#442502,#442503,#442504,#442505),.UNSPECIFIED.,.F.,.F.,
(4,3,3,3,3,3,3,3,3,4),(5.64557889509049E-5,5.98940966493752E-5,6.3421400387338E-5,
7.22241476084301E-5,7.38322796533361E-5,8.36529189331512E-5,8.80714278222498E-5,
9.84837568500755E-5,0.000108624704079146,0.000110823272382853),
 .UNSPECIFIED.);
#26624=B_SPLINE_CURVE_WITH_KNOTS('',3,(#442521,#442522,#442523,#442524,
#442525,#442526,#442527,#442528,#442529,#442530,#442531,#442532,#442533,
#442534,#442535,#442536,#442537,#442538,#442539,#442540,#442541,#442542,
#442543,#442544,#442545,#442546,#442547,#442548),.UNSPECIFIED.,.F.,.F.,
(4,3,3,3,3,3,3,3,3,4),(0.,8.66039628582242E-6,1.6470771520067E-5,2.24502894132491E-5,
2.4997596175783E-5,2.88526003690286E-5,3.10661348995021E-5,3.43053543516965E-5,
3.66410545653568E-5,4.00504537627891E-5),.UNSPECIFIED.);
#26625=B_SPLINE_CURVE_WITH_KNOTS('',3,(#442551,#442552,#442553,#442554,
#442555,#442556,#442557),.UNSPECIFIED.,.F.,.F.,(4,3,4),(0.,4.40000041065377E-5,
9.89910850773113E-5),.UNSPECIFIED.);
#26626=B_SPLINE_CURVE_WITH_KNOTS('',3,(#442578,#442579,#442580,#442581,
#442582,#442583,#442584,#442585,#442586,#442587,#442588,#442589,#442590,
#442591,#442592,#442593,#442594,#442595,#442596,#442597,#442598,#442599,
#442600,#442601,#442602,#442603,#442604,#442605,#442606,#442607,#442608,
#442609,#442610,#442611),.UNSPECIFIED.,.F.,.F.,(4,3,3,3,3,3,3,3,3,3,3,4),
(0.,4.29157837302455E-6,5.4277262379531E-6,1.00901698482347E-5,1.31279195068636E-5,
1.57383542265912E-5,1.61011507492101E-5,1.67166789291748E-5,1.95343262811356E-5,
2.29377234674644E-5,2.7155604762005E-5,3.34407099942654E-5),
 .UNSPECIFIED.);
#26627=B_SPLINE_CURVE_WITH_KNOTS('',3,(#442624,#442625,#442626,#442627,
#442628,#442629,#442630,#442631,#442632,#442633,#442634,#442635,#442636,
#442637,#442638,#442639,#442640,#442641,#442642,#442643,#442644,#442645,
#442646,#442647,#442648,#442649,#442650,#442651,#442652,#442653,#442654,
#442655,#442656,#442657),.UNSPECIFIED.,.F.,.F.,(4,3,3,3,3,3,3,3,3,3,3,4),
(2.16840434497101E-19,3.71309426656645E-6,5.39981071559426E-6,8.78933289330928E-6,
9.00272357067514E-6,1.07143984504149E-5,1.60780299679444E-5,1.65806081157686E-5,
2.30369726850413E-5,2.67819200416083E-5,3.59736924187559E-5,4.03862783806996E-5),
 .UNSPECIFIED.);
#26628=B_SPLINE_CURVE_WITH_KNOTS('',3,(#442770,#442771,#442772,#442773),
 .UNSPECIFIED.,.F.,.F.,(4,4),(0.,7.7002563062924E-5),.UNSPECIFIED.);
#26629=B_SPLINE_CURVE_WITH_KNOTS('',3,(#442783,#442784,#442785,#442786),
 .UNSPECIFIED.,.F.,.F.,(4,4),(2.16840434497101E-19,7.70025630629236E-5),
 .UNSPECIFIED.);
#26630=B_SPLINE_CURVE_WITH_KNOTS('',3,(#442790,#442791,#442792,#442793,
#442794,#442795,#442796,#442797,#442798,#442799,#442800,#442801,#442802,
#442803,#442804,#442805,#442806,#442807,#442808,#442809,#442810,#442811,
#442812,#442813,#442814,#442815,#442816,#442817,#442818,#442819,#442820,
#442821,#442822,#442823,#442824,#442825,#442826),.UNSPECIFIED.,.F.,.F.,
(4,3,3,3,3,3,3,3,3,3,3,3,4),(0.,9.59031527199893E-6,1.94769411222929E-5,
2.02405092183152E-5,3.21374138577771E-5,3.60302195070439E-5,4.4264064881834E-5,
4.53660204229443E-5,5.03633762302013E-5,5.17708036292894E-5,5.37928993851988E-5,
5.54103755460194E-5,5.64557889511955E-5),.UNSPECIFIED.);
#26631=B_SPLINE_CURVE_WITH_KNOTS('',3,(#442827,#442828,#442829,#442830,
#442831,#442832,#442833,#442834,#442835,#442836,#442837,#442838,#442839,
#442840,#442841,#442842,#442843,#442844,#442845,#442846,#442847,#442848,
#442849,#442850,#442851,#442852,#442853,#442854),.UNSPECIFIED.,.F.,.F.,
(4,3,3,3,3,3,3,3,3,4),(5.64557889511955E-5,5.9894096649375E-5,6.34214003873381E-5,
7.22241476084563E-5,7.38322796533359E-5,8.36529189331489E-5,8.80714278222495E-5,
9.8483756850075E-5,0.000108624704079149,0.000110823272382853),
 .UNSPECIFIED.);
#26632=B_SPLINE_CURVE_WITH_KNOTS('',3,(#442870,#442871,#442872,#442873,
#442874,#442875,#442876,#442877,#442878,#442879,#442880,#442881,#442882,
#442883,#442884,#442885,#442886,#442887,#442888,#442889,#442890,#442891,
#442892,#442893,#442894,#442895,#442896,#442897),.UNSPECIFIED.,.F.,.F.,
(4,3,3,3,3,3,3,3,3,4),(0.,8.66039628581672E-6,1.64707715200666E-5,2.24502894132125E-5,
2.49975961757825E-5,2.88526003690281E-5,3.10661348995016E-5,3.43053543516959E-5,
3.66410545653562E-5,4.00504537627891E-5),.UNSPECIFIED.);
#26633=B_SPLINE_CURVE_WITH_KNOTS('',3,(#442900,#442901,#442902,#442903,
#442904,#442905,#442906),.UNSPECIFIED.,.F.,.F.,(4,3,4),(0.,4.40000041065376E-5,
9.89910850773114E-5),.UNSPECIFIED.);
#26634=B_SPLINE_CURVE_WITH_KNOTS('',3,(#442927,#442928,#442929,#442930,
#442931,#442932,#442933,#442934,#442935,#442936,#442937,#442938,#442939,
#442940,#442941,#442942,#442943,#442944,#442945,#442946,#442947,#442948,
#442949,#442950,#442951,#442952,#442953,#442954,#442955,#442956,#442957,
#442958,#442959,#442960),.UNSPECIFIED.,.F.,.F.,(4,3,3,3,3,3,3,3,3,3,3,4),
(0.,4.29157837303576E-6,5.42772623795327E-6,1.00901698482347E-5,1.31279195068638E-5,
1.57383542265823E-5,1.61011507492104E-5,1.67166789291752E-5,1.95343262811356E-5,
2.29377234674646E-5,2.71556047620055E-5,3.34407099942653E-5),
 .UNSPECIFIED.);
#26635=B_SPLINE_CURVE_WITH_KNOTS('',3,(#442973,#442974,#442975,#442976,
#442977,#442978,#442979,#442980,#442981,#442982,#442983,#442984,#442985,
#442986,#442987,#442988,#442989,#442990,#442991,#442992,#442993,#442994,
#442995,#442996,#442997,#442998,#442999,#443000,#443001,#443002,#443003,
#443004,#443005,#443006),.UNSPECIFIED.,.F.,.F.,(4,3,3,3,3,3,3,3,3,3,3,4),
(2.16840434497101E-19,3.71309426656623E-6,5.39981071559397E-6,8.78933289330331E-6,
9.00272357067499E-6,1.07143984504146E-5,1.6078029967947E-5,1.65806081157683E-5,
2.30369726850555E-5,2.6781920041608E-5,3.59736924187373E-5,4.03862783806993E-5),
 .UNSPECIFIED.);
#26636=B_SPLINE_CURVE_WITH_KNOTS('',3,(#443119,#443120,#443121,#443122),
 .UNSPECIFIED.,.F.,.F.,(4,4),(0.,7.70025630629239E-5),.UNSPECIFIED.);
#26637=B_SPLINE_CURVE_WITH_KNOTS('',3,(#443132,#443133,#443134,#443135),
 .UNSPECIFIED.,.F.,.F.,(4,4),(2.16840434497101E-19,7.70025630629237E-5),
 .UNSPECIFIED.);
#26638=B_SPLINE_CURVE_WITH_KNOTS('',3,(#443139,#443140,#443141,#443142,
#443143,#443144,#443145,#443146,#443147,#443148,#443149,#443150,#443151,
#443152,#443153,#443154,#443155,#443156,#443157,#443158,#443159,#443160,
#443161,#443162,#443163,#443164,#443165,#443166,#443167,#443168,#443169,
#443170,#443171,#443172,#443173,#443174,#443175),.UNSPECIFIED.,.F.,.F.,
(4,3,3,3,3,3,3,3,3,3,3,3,4),(0.,9.59031527200983E-6,1.94769411222978E-5,
2.02405092183153E-5,3.21374138577654E-5,3.60302195070439E-5,4.42640648818711E-5,
4.53660204229442E-5,5.03633762302079E-5,5.17708036292895E-5,5.37928993851986E-5,
5.54103755460198E-5,5.64557889512199E-5),.UNSPECIFIED.);
#26639=B_SPLINE_CURVE_WITH_KNOTS('',3,(#443176,#443177,#443178,#443179,
#443180,#443181,#443182,#443183,#443184,#443185,#443186,#443187,#443188,
#443189,#443190,#443191,#443192,#443193,#443194,#443195,#443196,#443197,
#443198,#443199,#443200,#443201,#443202,#443203),.UNSPECIFIED.,.F.,.F.,
(4,3,3,3,3,3,3,3,3,4),(5.64557889512199E-5,5.98940966493751E-5,6.34214003873378E-5,
7.22241476084778E-5,7.38322796533363E-5,8.36529189331535E-5,8.80714278222497E-5,
9.84837568501019E-5,0.000108624704079195,0.000110823272382853),
 .UNSPECIFIED.);
#26640=B_SPLINE_CURVE_WITH_KNOTS('',3,(#443219,#443220,#443221,#443222,
#443223,#443224,#443225,#443226,#443227,#443228,#443229,#443230,#443231,
#443232,#443233,#443234,#443235,#443236,#443237,#443238,#443239,#443240,
#443241,#443242,#443243,#443244,#443245,#443246),.UNSPECIFIED.,.F.,.F.,
(4,3,3,3,3,3,3,3,3,4),(0.,8.66039628582605E-6,1.64707715200667E-5,2.24502894132618E-5,
2.49975961757822E-5,2.8852600369028E-5,3.10661348995017E-5,3.43053543516961E-5,
3.66410545653558E-5,4.00504537627885E-5),.UNSPECIFIED.);
#26641=B_SPLINE_CURVE_WITH_KNOTS('',3,(#443249,#443250,#443251,#443252,
#443253,#443254,#443255),.UNSPECIFIED.,.F.,.F.,(4,3,4),(0.,4.40000041065376E-5,
9.89910850773113E-5),.UNSPECIFIED.);
#26642=B_SPLINE_CURVE_WITH_KNOTS('',3,(#443276,#443277,#443278,#443279,
#443280,#443281,#443282,#443283,#443284,#443285,#443286,#443287,#443288,
#443289,#443290,#443291,#443292,#443293,#443294,#443295,#443296,#443297,
#443298,#443299,#443300,#443301,#443302,#443303,#443304,#443305,#443306,
#443307,#443308,#443309),.UNSPECIFIED.,.F.,.F.,(4,3,3,3,3,3,3,3,3,3,3,4),
(0.,4.29157837304045E-6,5.42772623795319E-6,1.00901698482347E-5,1.31279195068639E-5,
1.57383542265809E-5,1.61011507492103E-5,1.67166789291753E-5,1.95343262811357E-5,
2.29377234674648E-5,2.71556047620057E-5,3.34407099942658E-5),
 .UNSPECIFIED.);
#26643=B_SPLINE_CURVE_WITH_KNOTS('',3,(#443322,#443323,#443324,#443325,
#443326,#443327,#443328,#443329,#443330,#443331,#443332,#443333,#443334,
#443335,#443336,#443337,#443338,#443339,#443340,#443341,#443342,#443343,
#443344,#443345,#443346,#443347,#443348,#443349,#443350,#443351,#443352,
#443353,#443354,#443355),.UNSPECIFIED.,.F.,.F.,(4,3,3,3,3,3,3,3,3,3,3,4),
(2.16840434497101E-19,3.71309426656637E-6,5.39981071559423E-6,8.78933289369147E-6,
9.00272357067518E-6,1.0714398450415E-5,1.60780299679611E-5,1.65806081157689E-5,
2.30369726850217E-5,2.6781920041609E-5,3.59736924188261E-5,4.03862783807009E-5),
 .UNSPECIFIED.);
#26644=B_SPLINE_CURVE_WITH_KNOTS('',3,(#443468,#443469,#443470,#443471),
 .UNSPECIFIED.,.F.,.F.,(4,4),(0.,7.70025630629238E-5),.UNSPECIFIED.);
#26645=B_SPLINE_CURVE_WITH_KNOTS('',3,(#443481,#443482,#443483,#443484),
 .UNSPECIFIED.,.F.,.F.,(4,4),(0.,7.7002563062924E-5),.UNSPECIFIED.);
#26646=B_SPLINE_CURVE_WITH_KNOTS('',3,(#443488,#443489,#443490,#443491,
#443492,#443493,#443494,#443495,#443496,#443497,#443498,#443499,#443500,
#443501,#443502,#443503,#443504,#443505,#443506,#443507,#443508,#443509,
#443510,#443511,#443512,#443513,#443514,#443515,#443516,#443517,#443518,
#443519,#443520,#443521,#443522,#443523,#443524),.UNSPECIFIED.,.F.,.F.,
(4,3,3,3,3,3,3,3,3,3,3,3,4),(0.,9.59031527200099E-6,1.94769411222849E-5,
2.02405092183154E-5,3.21374138577703E-5,3.60302195070439E-5,4.42640648818483E-5,
4.53660204229446E-5,5.03633762302092E-5,5.17708036292899E-5,5.37928993851989E-5,
5.54103755460196E-5,5.64557889512858E-5),.UNSPECIFIED.);
#26647=B_SPLINE_CURVE_WITH_KNOTS('',3,(#443525,#443526,#443527,#443528,
#443529,#443530,#443531,#443532,#443533,#443534,#443535,#443536,#443537,
#443538,#443539,#443540,#443541,#443542,#443543,#443544,#443545,#443546,
#443547,#443548,#443549,#443550,#443551,#443552),.UNSPECIFIED.,.F.,.F.,
(4,3,3,3,3,3,3,3,3,4),(5.64557889512858E-5,5.9894096649375E-5,6.34214003873377E-5,
7.22241476084027E-5,7.38322796533363E-5,8.36529189331388E-5,8.80714278222497E-5,
9.84837568500627E-5,0.000108624704079124,0.000110823272382853),
 .UNSPECIFIED.);
#26648=B_SPLINE_CURVE_WITH_KNOTS('',3,(#443568,#443569,#443570,#443571,
#443572,#443573,#443574,#443575,#443576,#443577,#443578,#443579,#443580,
#443581,#443582,#443583,#443584,#443585,#443586,#443587,#443588,#443589,
#443590,#443591,#443592,#443593,#443594,#443595),.UNSPECIFIED.,.F.,.F.,
(4,3,3,3,3,3,3,3,3,4),(0.,8.66039628583908E-6,1.64707715200666E-5,2.24502894132304E-5,
2.49975961757823E-5,2.88526003690279E-5,3.10661348995015E-5,3.43053543516958E-5,
3.66410545653561E-5,4.00504537627889E-5),.UNSPECIFIED.);
#26649=B_SPLINE_CURVE_WITH_KNOTS('',3,(#443598,#443599,#443600,#443601,
#443602,#443603,#443604),.UNSPECIFIED.,.F.,.F.,(4,3,4),(0.,4.40000041065374E-5,
9.89910850773112E-5),.UNSPECIFIED.);
#26650=B_SPLINE_CURVE_WITH_KNOTS('',3,(#443625,#443626,#443627,#443628,
#443629,#443630,#443631,#443632,#443633,#443634,#443635,#443636,#443637,
#443638,#443639,#443640,#443641,#443642,#443643,#443644,#443645,#443646,
#443647,#443648,#443649,#443650,#443651,#443652,#443653,#443654,#443655,
#443656,#443657,#443658),.UNSPECIFIED.,.F.,.F.,(4,3,3,3,3,3,3,3,3,3,3,4),
(0.,4.29157837303037E-6,5.42772623795304E-6,1.00901698482347E-5,1.31279195068637E-5,
1.57383542265969E-5,1.61011507492103E-5,1.67166789291754E-5,1.95343262811355E-5,
2.29377234674647E-5,2.71556047620054E-5,3.34407099942654E-5),
 .UNSPECIFIED.);
#26651=B_SPLINE_CURVE_WITH_KNOTS('',3,(#443671,#443672,#443673,#443674,
#443675,#443676,#443677,#443678,#443679,#443680,#443681,#443682,#443683,
#443684,#443685,#443686,#443687,#443688,#443689,#443690,#443691,#443692,
#443693,#443694,#443695,#443696,#443697,#443698,#443699,#443700,#443701,
#443702,#443703,#443704),.UNSPECIFIED.,.F.,.F.,(4,3,3,3,3,3,3,3,3,3,3,4),
(0.,3.71309426656671E-6,5.39981071559412E-6,8.78933289331451E-6,9.00272357067549E-6,
1.07143984504153E-5,1.60780299679558E-5,1.65806081157689E-5,2.30369726850571E-5,
2.67819200416092E-5,3.59736924187926E-5,4.0386278380701E-5),
 .UNSPECIFIED.);
#26652=B_SPLINE_CURVE_WITH_KNOTS('',3,(#443817,#443818,#443819,#443820),
 .UNSPECIFIED.,.F.,.F.,(4,4),(0.,7.70025630629237E-5),.UNSPECIFIED.);
#26653=B_SPLINE_CURVE_WITH_KNOTS('',3,(#443830,#443831,#443832,#443833),
 .UNSPECIFIED.,.F.,.F.,(4,4),(4.33680868994202E-19,7.70025630629238E-5),
 .UNSPECIFIED.);
#26654=B_SPLINE_CURVE_WITH_KNOTS('',3,(#443837,#443838,#443839,#443840,
#443841,#443842,#443843,#443844,#443845,#443846,#443847,#443848,#443849,
#443850,#443851,#443852,#443853,#443854,#443855,#443856,#443857,#443858,
#443859,#443860,#443861,#443862,#443863,#443864,#443865,#443866,#443867,
#443868,#443869,#443870,#443871,#443872,#443873),.UNSPECIFIED.,.F.,.F.,
(4,3,3,3,3,3,3,3,3,3,3,3,4),(0.,9.59031527199245E-6,1.94769411222787E-5,
2.02405092183153E-5,3.2137413857778E-5,3.60302195070441E-5,4.42640648819171E-5,
4.53660204229442E-5,5.03633762302015E-5,5.17708036292896E-5,5.37928993851988E-5,
5.54103755460206E-5,5.64557889511081E-5),.UNSPECIFIED.);
#26655=B_SPLINE_CURVE_WITH_KNOTS('',3,(#443874,#443875,#443876,#443877,
#443878,#443879,#443880,#443881,#443882,#443883,#443884,#443885,#443886,
#443887,#443888,#443889,#443890,#443891,#443892,#443893,#443894,#443895,
#443896,#443897,#443898,#443899,#443900,#443901),.UNSPECIFIED.,.F.,.F.,
(4,3,3,3,3,3,3,3,3,4),(5.64557889511081E-5,5.98940966493752E-5,6.34214003873379E-5,
7.22241476085193E-5,7.38322796533365E-5,8.36529189331587E-5,8.80714278222504E-5,
9.84837568501169E-5,0.00010862470407922,0.000110823272382854),
 .UNSPECIFIED.);
#26656=B_SPLINE_CURVE_WITH_KNOTS('',3,(#443917,#443918,#443919,#443920,
#443921,#443922,#443923,#443924,#443925,#443926,#443927,#443928,#443929,
#443930,#443931,#443932,#443933,#443934,#443935,#443936,#443937,#443938,
#443939,#443940,#443941,#443942,#443943,#443944),.UNSPECIFIED.,.F.,.F.,
(4,3,3,3,3,3,3,3,3,4),(0.,8.6603962858496E-6,1.64707715200666E-5,2.24502894132311E-5,
2.49975961757824E-5,2.8852600369028E-5,3.10661348995016E-5,3.4305354351696E-5,
3.6641054565356E-5,4.00504537627891E-5),.UNSPECIFIED.);
#26657=B_SPLINE_CURVE_WITH_KNOTS('',3,(#443947,#443948,#443949,#443950,
#443951,#443952,#443953),.UNSPECIFIED.,.F.,.F.,(4,3,4),(0.,4.40000041065375E-5,
9.89910850773112E-5),.UNSPECIFIED.);
#26658=B_SPLINE_CURVE_WITH_KNOTS('',3,(#443974,#443975,#443976,#443977,
#443978,#443979,#443980,#443981,#443982,#443983,#443984,#443985,#443986,
#443987,#443988,#443989,#443990,#443991,#443992,#443993,#443994,#443995,
#443996,#443997,#443998,#443999,#444000,#444001,#444002,#444003,#444004,
#444005,#444006,#444007),.UNSPECIFIED.,.F.,.F.,(4,3,3,3,3,3,3,3,3,3,3,4),
(0.,4.29157837301968E-6,5.42772623795346E-6,1.00901698482351E-5,1.31279195068641E-5,
1.57383542265875E-5,1.6101150749211E-5,1.67166789291759E-5,1.95343262811362E-5,
2.29377234674654E-5,2.71556047620065E-5,3.34407099942667E-5),
 .UNSPECIFIED.);
#26659=B_SPLINE_CURVE_WITH_KNOTS('',3,(#444020,#444021,#444022,#444023,
#444024,#444025,#444026,#444027,#444028,#444029,#444030,#444031,#444032,
#444033,#444034,#444035,#444036,#444037,#444038,#444039,#444040,#444041,
#444042,#444043,#444044,#444045,#444046,#444047,#444048,#444049,#444050,
#444051,#444052,#444053),.UNSPECIFIED.,.F.,.F.,(4,3,3,3,3,3,3,3,3,3,3,4),
(2.16840434497101E-19,3.71309426656662E-6,5.39981071559424E-6,8.78933289331598E-6,
9.00272357067511E-6,1.07143984504147E-5,1.60780299679598E-5,1.65806081157684E-5,
2.30369726850327E-5,2.67819200416082E-5,3.59736924188149E-5,4.03862783806993E-5),
 .UNSPECIFIED.);
#26660=B_SPLINE_CURVE_WITH_KNOTS('',3,(#444166,#444167,#444168,#444169),
 .UNSPECIFIED.,.F.,.F.,(4,4),(0.,7.70025630629239E-5),.UNSPECIFIED.);
#26661=B_SPLINE_CURVE_WITH_KNOTS('',3,(#444179,#444180,#444181,#444182),
 .UNSPECIFIED.,.F.,.F.,(4,4),(4.33680868994202E-19,7.7002563062924E-5),
 .UNSPECIFIED.);
#26662=B_SPLINE_CURVE_WITH_KNOTS('',3,(#444186,#444187,#444188,#444189,
#444190,#444191,#444192,#444193,#444194,#444195,#444196,#444197,#444198,
#444199,#444200,#444201,#444202,#444203,#444204,#444205,#444206,#444207,
#444208,#444209,#444210,#444211,#444212,#444213,#444214,#444215,#444216,
#444217,#444218,#444219,#444220,#444221,#444222),.UNSPECIFIED.,.F.,.F.,
(4,3,3,3,3,3,3,3,3,3,3,3,4),(0.,9.59031527200592E-6,1.94769411222996E-5,
2.02405092183151E-5,3.21374138577715E-5,3.60302195070437E-5,4.42640648819735E-5,
4.5366020422944E-5,5.03633762301883E-5,5.17708036292892E-5,5.37928993851985E-5,
5.5410375546019E-5,5.64557889516034E-5),.UNSPECIFIED.);
#26663=B_SPLINE_CURVE_WITH_KNOTS('',3,(#444223,#444224,#444225,#444226,
#444227,#444228,#444229,#444230,#444231,#444232,#444233,#444234,#444235,
#444236,#444237,#444238,#444239,#444240,#444241,#444242,#444243,#444244,
#444245,#444246,#444247,#444248,#444249,#444250),.UNSPECIFIED.,.F.,.F.,
(4,3,3,3,3,3,3,3,3,4),(5.64557889516034E-5,5.98940966493748E-5,6.34214003873374E-5,
7.22241476085106E-5,7.38322796533359E-5,8.36529189331493E-5,8.8071427822249E-5,
9.84837568500857E-5,0.000108624704079163,0.000110823272382852),
 .UNSPECIFIED.);
#26664=B_SPLINE_CURVE_WITH_KNOTS('',3,(#444266,#444267,#444268,#444269,
#444270,#444271,#444272,#444273,#444274,#444275,#444276,#444277,#444278,
#444279,#444280,#444281,#444282,#444283,#444284,#444285,#444286,#444287,
#444288,#444289,#444290,#444291,#444292,#444293),.UNSPECIFIED.,.F.,.F.,
(4,3,3,3,3,3,3,3,3,4),(0.,8.66039628580049E-6,1.64707715200665E-5,2.24502894132241E-5,
2.49975961757822E-5,2.8852600369028E-5,3.10661348995015E-5,3.43053543516958E-5,
3.6641054565356E-5,4.0050453762789E-5),.UNSPECIFIED.);
#26665=B_SPLINE_CURVE_WITH_KNOTS('',3,(#444296,#444297,#444298,#444299,
#444300,#444301,#444302),.UNSPECIFIED.,.F.,.F.,(4,3,4),(0.,4.40000041065373E-5,
9.89910850773112E-5),.UNSPECIFIED.);
#26666=B_SPLINE_CURVE_WITH_KNOTS('',3,(#444323,#444324,#444325,#444326,
#444327,#444328,#444329,#444330,#444331,#444332,#444333,#444334,#444335,
#444336,#444337,#444338,#444339,#444340,#444341,#444342,#444343,#444344,
#444345,#444346,#444347,#444348,#444349,#444350,#444351,#444352,#444353,
#444354,#444355,#444356),.UNSPECIFIED.,.F.,.F.,(4,3,3,3,3,3,3,3,3,3,3,4),
(0.,4.29157837306035E-6,5.42772623795318E-6,1.00901698482348E-5,1.3127919506864E-5,
1.57383542265774E-5,1.61011507492105E-5,1.67166789291753E-5,1.95343262811357E-5,
2.29377234674649E-5,2.71556047620058E-5,3.34407099942658E-5),
 .UNSPECIFIED.);
#26667=B_SPLINE_CURVE_WITH_KNOTS('',3,(#444369,#444370,#444371,#444372,
#444373,#444374,#444375,#444376,#444377,#444378,#444379,#444380,#444381,
#444382,#444383,#444384,#444385,#444386,#444387,#444388,#444389,#444390,
#444391,#444392,#444393,#444394,#444395,#444396,#444397,#444398,#444399,
#444400,#444401,#444402),.UNSPECIFIED.,.F.,.F.,(4,3,3,3,3,3,3,3,3,3,3,4),
(0.,3.71309426656633E-6,5.39981071559413E-6,8.78933289330927E-6,9.00272357067526E-6,
1.0714398450415E-5,1.60780299679556E-5,1.65806081157687E-5,2.30369726850343E-5,
2.67819200416086E-5,3.59736924187825E-5,4.03862783807002E-5),
 .UNSPECIFIED.);
#26668=B_SPLINE_CURVE_WITH_KNOTS('',3,(#444515,#444516,#444517,#444518),
 .UNSPECIFIED.,.F.,.F.,(4,4),(0.,7.70025630629237E-5),.UNSPECIFIED.);
#26669=B_SPLINE_CURVE_WITH_KNOTS('',3,(#444528,#444529,#444530,#444531),
 .UNSPECIFIED.,.F.,.F.,(4,4),(4.33680868994202E-19,7.70025630629236E-5),
 .UNSPECIFIED.);
#26670=B_SPLINE_CURVE_WITH_KNOTS('',3,(#444535,#444536,#444537,#444538,
#444539,#444540,#444541,#444542,#444543,#444544,#444545,#444546,#444547,
#444548,#444549,#444550,#444551,#444552,#444553,#444554,#444555,#444556,
#444557,#444558,#444559,#444560,#444561,#444562,#444563,#444564,#444565,
#444566,#444567,#444568,#444569,#444570,#444571),.UNSPECIFIED.,.F.,.F.,
(4,3,3,3,3,3,3,3,3,3,3,3,4),(0.,9.59031527198161E-6,1.94769411222625E-5,
2.02405092183153E-5,3.21374138577781E-5,3.60302195070436E-5,4.42640648818272E-5,
4.53660204229445E-5,5.03633762301973E-5,5.17708036292894E-5,5.37928993851988E-5,
5.54103755460195E-5,5.64557889510153E-5),.UNSPECIFIED.);
#26671=B_SPLINE_CURVE_WITH_KNOTS('',3,(#444572,#444573,#444574,#444575,
#444576,#444577,#444578,#444579,#444580,#444581,#444582,#444583,#444584,
#444585,#444586,#444587,#444588,#444589,#444590,#444591,#444592,#444593,
#444594,#444595,#444596,#444597,#444598,#444599),.UNSPECIFIED.,.F.,.F.,
(4,3,3,3,3,3,3,3,3,4),(5.64557889510153E-5,5.98940966493749E-5,6.34214003873379E-5,
7.22241476084258E-5,7.38322796533363E-5,8.36529189331488E-5,8.80714278222499E-5,
9.84837568500756E-5,0.000108624704079134,0.000110823272382853),
 .UNSPECIFIED.);
#26672=B_SPLINE_CURVE_WITH_KNOTS('',3,(#444615,#444616,#444617,#444618,
#444619,#444620,#444621,#444622,#444623,#444624,#444625,#444626,#444627,
#444628,#444629,#444630,#444631,#444632,#444633,#444634,#444635,#444636,
#444637,#444638,#444639,#444640,#444641,#444642),.UNSPECIFIED.,.F.,.F.,
(4,3,3,3,3,3,3,3,3,4),(0.,8.66039628579394E-6,1.64707715200667E-5,2.24502894132511E-5,
2.49975961757824E-5,2.88526003690281E-5,3.10661348995017E-5,3.43053543516961E-5,
3.66410545653561E-5,4.0050453762789E-5),.UNSPECIFIED.);
#26673=B_SPLINE_CURVE_WITH_KNOTS('',3,(#444645,#444646,#444647,#444648,
#444649,#444650,#444651),.UNSPECIFIED.,.F.,.F.,(4,3,4),(0.,4.40000041065371E-5,
9.89910850773111E-5),.UNSPECIFIED.);
#26674=B_SPLINE_CURVE_WITH_KNOTS('',3,(#444672,#444673,#444674,#444675,
#444676,#444677,#444678,#444679,#444680,#444681,#444682,#444683,#444684,
#444685,#444686,#444687,#444688,#444689,#444690,#444691,#444692,#444693,
#444694,#444695,#444696,#444697,#444698,#444699,#444700,#444701,#444702,
#444703,#444704,#444705),.UNSPECIFIED.,.F.,.F.,(4,3,3,3,3,3,3,3,3,3,3,4),
(0.,4.2915783730184E-6,5.42772623795351E-6,1.00901698482345E-5,1.31279195068638E-5,
1.57383542265793E-5,1.61011507492105E-5,1.67166789291754E-5,1.95343262811357E-5,
2.29377234674648E-5,2.71556047620057E-5,3.34407099942656E-5),
 .UNSPECIFIED.);
#26675=B_SPLINE_CURVE_WITH_KNOTS('',3,(#444718,#444719,#444720,#444721,
#444722,#444723,#444724,#444725,#444726,#444727,#444728,#444729,#444730,
#444731,#444732,#444733,#444734,#444735,#444736,#444737,#444738,#444739,
#444740,#444741,#444742,#444743,#444744,#444745,#444746,#444747,#444748,
#444749,#444750,#444751),.UNSPECIFIED.,.F.,.F.,(4,3,3,3,3,3,3,3,3,3,3,4),
(0.,3.71309426656649E-6,5.3998107155939E-6,8.78933289327122E-6,9.00272357067513E-6,
1.07143984504147E-5,1.60780299679589E-5,1.65806081157686E-5,2.30369726850634E-5,
2.67819200416087E-5,3.59736924187455E-5,4.03862783807006E-5),
 .UNSPECIFIED.);
#26676=B_SPLINE_CURVE_WITH_KNOTS('',3,(#444864,#444865,#444866,#444867),
 .UNSPECIFIED.,.F.,.F.,(4,4),(0.,7.70025630629237E-5),.UNSPECIFIED.);
#26677=B_SPLINE_CURVE_WITH_KNOTS('',3,(#444877,#444878,#444879,#444880),
 .UNSPECIFIED.,.F.,.F.,(4,4),(4.33680868994202E-19,7.70025630629236E-5),
 .UNSPECIFIED.);
#26678=B_SPLINE_CURVE_WITH_KNOTS('',3,(#444884,#444885,#444886,#444887,
#444888,#444889,#444890,#444891,#444892,#444893,#444894,#444895,#444896,
#444897,#444898,#444899,#444900,#444901,#444902,#444903,#444904,#444905,
#444906,#444907,#444908,#444909,#444910,#444911,#444912,#444913,#444914,
#444915,#444916,#444917,#444918,#444919,#444920),.UNSPECIFIED.,.F.,.F.,
(4,3,3,3,3,3,3,3,3,3,3,3,4),(0.,9.59031527201753E-6,1.9476941122308E-5,
2.02405092183154E-5,3.21374138577773E-5,3.60302195070444E-5,4.42640648819026E-5,
4.53660204229445E-5,5.03633762302112E-5,5.17708036292897E-5,5.37928993851987E-5,
5.54103755460199E-5,5.64557889514577E-5),.UNSPECIFIED.);
#26679=B_SPLINE_CURVE_WITH_KNOTS('',3,(#444921,#444922,#444923,#444924,
#444925,#444926,#444927,#444928,#444929,#444930,#444931,#444932,#444933,
#444934,#444935,#444936,#444937,#444938,#444939,#444940,#444941,#444942,
#444943,#444944,#444945,#444946,#444947,#444948),.UNSPECIFIED.,.F.,.F.,
(4,3,3,3,3,3,3,3,3,4),(5.64557889514577E-5,5.98940966493751E-5,6.34214003873383E-5,
7.22241476084398E-5,7.38322796533365E-5,8.36529189331448E-5,8.80714278222499E-5,
9.84837568500812E-5,0.000108624704079154,0.000110823272382853),
 .UNSPECIFIED.);
#26680=B_SPLINE_CURVE_WITH_KNOTS('',3,(#444964,#444965,#444966,#444967,
#444968,#444969,#444970,#444971,#444972,#444973,#444974,#444975,#444976,
#444977,#444978,#444979,#444980,#444981,#444982,#444983,#444984,#444985,
#444986,#444987,#444988,#444989,#444990,#444991),.UNSPECIFIED.,.F.,.F.,
(4,3,3,3,3,3,3,3,3,4),(0.,8.66039628577846E-6,1.64707715200669E-5,2.24502894132539E-5,
2.49975961757828E-5,2.88526003690286E-5,3.10661348995021E-5,3.43053543516966E-5,
3.66410545653563E-5,4.00504537627887E-5),.UNSPECIFIED.);
#26681=B_SPLINE_CURVE_WITH_KNOTS('',3,(#444994,#444995,#444996,#444997,
#444998,#444999,#445000),.UNSPECIFIED.,.F.,.F.,(4,3,4),(0.,4.40000041065374E-5,
9.89910850773111E-5),.UNSPECIFIED.);
#26682=B_SPLINE_CURVE_WITH_KNOTS('',3,(#445021,#445022,#445023,#445024,
#445025,#445026,#445027,#445028,#445029,#445030,#445031,#445032,#445033,
#445034,#445035,#445036,#445037,#445038,#445039,#445040,#445041,#445042,
#445043,#445044,#445045,#445046,#445047,#445048,#445049,#445050,#445051,
#445052,#445053,#445054),.UNSPECIFIED.,.F.,.F.,(4,3,3,3,3,3,3,3,3,3,3,4),
(0.,4.29157837305176E-6,5.42772623795343E-6,1.00901698482347E-5,1.31279195068639E-5,
1.57383542265907E-5,1.61011507492105E-5,1.67166789291758E-5,1.95343262811358E-5,
2.2937723467465E-5,2.71556047620059E-5,3.3440709994266E-5),
 .UNSPECIFIED.);
#26683=B_SPLINE_CURVE_WITH_KNOTS('',3,(#445067,#445068,#445069,#445070,
#445071,#445072,#445073,#445074,#445075,#445076,#445077,#445078,#445079,
#445080,#445081,#445082,#445083,#445084,#445085,#445086,#445087,#445088,
#445089,#445090,#445091,#445092,#445093,#445094,#445095,#445096,#445097,
#445098,#445099,#445100),.UNSPECIFIED.,.F.,.F.,(4,3,3,3,3,3,3,3,3,3,3,4),
(2.16840434497101E-19,3.7130942665665E-6,5.39981071559408E-6,8.78933289365784E-6,
9.00272357067535E-6,1.07143984504151E-5,1.60780299679626E-5,1.65806081157688E-5,
2.30369726850283E-5,2.67819200416088E-5,3.59736924187693E-5,4.03862783807004E-5),
 .UNSPECIFIED.);
#26684=B_SPLINE_CURVE_WITH_KNOTS('',3,(#445213,#445214,#445215,#445216),
 .UNSPECIFIED.,.F.,.F.,(4,4),(0.,7.70025630629241E-5),.UNSPECIFIED.);
#26685=B_SPLINE_CURVE_WITH_KNOTS('',3,(#445226,#445227,#445228,#445229),
 .UNSPECIFIED.,.F.,.F.,(4,4),(4.33680868994202E-19,7.70025630629237E-5),
 .UNSPECIFIED.);
#26686=B_SPLINE_CURVE_WITH_KNOTS('',3,(#445233,#445234,#445235,#445236,
#445237,#445238,#445239,#445240,#445241,#445242,#445243,#445244,#445245,
#445246,#445247,#445248,#445249,#445250,#445251,#445252,#445253,#445254,
#445255,#445256,#445257,#445258,#445259,#445260,#445261,#445262,#445263,
#445264,#445265,#445266,#445267,#445268,#445269),.UNSPECIFIED.,.F.,.F.,
(4,3,3,3,3,3,3,3,3,3,3,3,4),(0.,9.59031527200409E-6,1.9476941122299E-5,
2.02405092183152E-5,3.21374138577639E-5,3.60302195070437E-5,4.42640648818624E-5,
4.53660204229444E-5,5.03633762302181E-5,5.17708036292895E-5,5.37928993851987E-5,
5.54103755460196E-5,5.64557889508704E-5),.UNSPECIFIED.);
#26687=B_SPLINE_CURVE_WITH_KNOTS('',3,(#445270,#445271,#445272,#445273,
#445274,#445275,#445276,#445277,#445278,#445279,#445280,#445281,#445282,
#445283,#445284,#445285,#445286,#445287,#445288,#445289,#445290,#445291,
#445292,#445293,#445294,#445295,#445296,#445297),.UNSPECIFIED.,.F.,.F.,
(4,3,3,3,3,3,3,3,3,4),(5.64557889508704E-5,5.98940966493747E-5,6.34214003873377E-5,
7.22241476084951E-5,7.3832279653336E-5,8.36529189331591E-5,8.80714278222496E-5,
9.84837568501187E-5,0.000108624704079221,0.000110823272382853),
 .UNSPECIFIED.);
#26688=B_SPLINE_CURVE_WITH_KNOTS('',3,(#445313,#445314,#445315,#445316,
#445317,#445318,#445319,#445320,#445321,#445322,#445323,#445324,#445325,
#445326,#445327,#445328,#445329,#445330,#445331,#445332,#445333,#445334,
#445335,#445336,#445337,#445338,#445339,#445340),.UNSPECIFIED.,.F.,.F.,
(4,3,3,3,3,3,3,3,3,4),(0.,8.66039628579246E-6,1.64707715200667E-5,2.24502894129346E-5,
2.49975961757824E-5,2.88526003690281E-5,3.10661348995016E-5,3.43053543516961E-5,
3.66410545653559E-5,4.00504537627887E-5),.UNSPECIFIED.);
#26689=B_SPLINE_CURVE_WITH_KNOTS('',3,(#445343,#445344,#445345,#445346,
#445347,#445348,#445349),.UNSPECIFIED.,.F.,.F.,(4,3,4),(0.,4.40000041065373E-5,
9.89910850773112E-5),.UNSPECIFIED.);
#26690=B_SPLINE_CURVE_WITH_KNOTS('',3,(#445370,#445371,#445372,#445373,
#445374,#445375,#445376,#445377,#445378,#445379,#445380,#445381,#445382,
#445383,#445384,#445385,#445386,#445387,#445388,#445389,#445390,#445391,
#445392,#445393,#445394,#445395,#445396,#445397,#445398,#445399,#445400,
#445401,#445402,#445403),.UNSPECIFIED.,.F.,.F.,(4,3,3,3,3,3,3,3,3,3,3,4),
(0.,4.29157837305078E-6,5.4277262379532E-6,1.00901698482344E-5,1.31279195068637E-5,
1.57383542265852E-5,1.61011507492101E-5,1.67166789291755E-5,1.95343262811355E-5,
2.29377234674645E-5,2.71556047620054E-5,3.34407099942652E-5),
 .UNSPECIFIED.);
#26691=B_SPLINE_CURVE_WITH_KNOTS('',3,(#445416,#445417,#445418,#445419,
#445420,#445421,#445422,#445423,#445424,#445425,#445426,#445427,#445428,
#445429,#445430,#445431,#445432,#445433,#445434,#445435,#445436,#445437,
#445438,#445439,#445440,#445441,#445442,#445443,#445444,#445445,#445446,
#445447,#445448,#445449),.UNSPECIFIED.,.F.,.F.,(4,3,3,3,3,3,3,3,3,3,3,4),
(1.0842021724855E-19,3.71309426656644E-6,5.39981071559416E-6,8.78933289330016E-6,
9.00272357067517E-6,1.07143984504149E-5,1.60780299679582E-5,1.65806081157687E-5,
2.30369726850505E-5,2.67819200416087E-5,3.59736924187412E-5,4.03862783807004E-5),
 .UNSPECIFIED.);
#26692=B_SPLINE_CURVE_WITH_KNOTS('',3,(#445562,#445563,#445564,#445565),
 .UNSPECIFIED.,.F.,.F.,(4,4),(0.,7.70025630629238E-5),.UNSPECIFIED.);
#26693=B_SPLINE_CURVE_WITH_KNOTS('',3,(#445575,#445576,#445577,#445578),
 .UNSPECIFIED.,.F.,.F.,(4,4),(4.33680868994202E-19,7.70025630629236E-5),
 .UNSPECIFIED.);
#26694=B_SPLINE_CURVE_WITH_KNOTS('',3,(#445582,#445583,#445584,#445585,
#445586,#445587,#445588,#445589,#445590,#445591,#445592,#445593,#445594,
#445595,#445596,#445597,#445598,#445599,#445600,#445601,#445602,#445603,
#445604,#445605,#445606,#445607,#445608,#445609,#445610,#445611,#445612,
#445613,#445614,#445615,#445616,#445617,#445618),.UNSPECIFIED.,.F.,.F.,
(4,3,3,3,3,3,3,3,3,3,3,3,4),(0.,9.59031527199521E-6,1.9476941122276E-5,
2.02405092183153E-5,3.21374138577658E-5,3.6030219507044E-5,4.4264064881821E-5,
4.53660204229446E-5,5.03633762302175E-5,5.17708036292897E-5,5.37928993851991E-5,
5.54103755460206E-5,5.64557889515007E-5),.UNSPECIFIED.);
#26695=B_SPLINE_CURVE_WITH_KNOTS('',3,(#445619,#445620,#445621,#445622,
#445623,#445624,#445625,#445626,#445627,#445628,#445629,#445630,#445631,
#445632,#445633,#445634,#445635,#445636,#445637,#445638,#445639,#445640,
#445641,#445642,#445643,#445644,#445645,#445646),.UNSPECIFIED.,.F.,.F.,
(4,3,3,3,3,3,3,3,3,4),(5.64557889515007E-5,5.98940966493753E-5,6.34214003873382E-5,
7.22241476085262E-5,7.38322796533366E-5,8.365291893315E-5,8.80714278222501E-5,
9.84837568501103E-5,0.000108624704079207,0.000110823272382854),
 .UNSPECIFIED.);
#26696=B_SPLINE_CURVE_WITH_KNOTS('',3,(#445662,#445663,#445664,#445665,
#445666,#445667,#445668,#445669,#445670,#445671,#445672,#445673,#445674,
#445675,#445676,#445677,#445678,#445679,#445680,#445681,#445682,#445683,
#445684,#445685,#445686,#445687,#445688,#445689),.UNSPECIFIED.,.F.,.F.,
(4,3,3,3,3,3,3,3,3,4),(0.,8.66039628580631E-6,1.64707715200667E-5,2.24502894132641E-5,
2.49975961757823E-5,2.88526003690281E-5,3.10661348995016E-5,3.4305354351696E-5,
3.66410545653559E-5,4.00504537627885E-5),.UNSPECIFIED.);
#26697=B_SPLINE_CURVE_WITH_KNOTS('',3,(#445692,#445693,#445694,#445695,
#445696,#445697,#445698),.UNSPECIFIED.,.F.,.F.,(4,3,4),(0.,4.40000041065376E-5,
9.89910850773112E-5),.UNSPECIFIED.);
#26698=B_SPLINE_CURVE_WITH_KNOTS('',3,(#445719,#445720,#445721,#445722,
#445723,#445724,#445725,#445726,#445727,#445728,#445729,#445730,#445731,
#445732,#445733,#445734,#445735,#445736,#445737,#445738,#445739,#445740,
#445741,#445742,#445743,#445744,#445745,#445746,#445747,#445748,#445749,
#445750,#445751,#445752),.UNSPECIFIED.,.F.,.F.,(4,3,3,3,3,3,3,3,3,3,3,4),
(0.,4.29157837303616E-6,5.42772623795344E-6,1.00901698482348E-5,1.3127919506864E-5,
1.57383542265838E-5,1.61011507492106E-5,1.67166789291761E-5,1.95343262811362E-5,
2.29377234674651E-5,2.71556047620063E-5,3.34407099942663E-5),
 .UNSPECIFIED.);
#26699=B_SPLINE_CURVE_WITH_KNOTS('',3,(#445765,#445766,#445767,#445768,
#445769,#445770,#445771,#445772,#445773,#445774,#445775,#445776,#445777,
#445778,#445779,#445780,#445781,#445782,#445783,#445784,#445785,#445786,
#445787,#445788,#445789,#445790,#445791,#445792,#445793,#445794,#445795,
#445796,#445797,#445798),.UNSPECIFIED.,.F.,.F.,(4,3,3,3,3,3,3,3,3,3,3,4),
(0.,3.71309426656651E-6,5.39981071559418E-6,8.78933289368936E-6,9.00272357067521E-6,
1.0714398450415E-5,1.60780299679545E-5,1.65806081157686E-5,2.30369726850577E-5,
2.67819200416086E-5,3.59736924187482E-5,4.03862783806999E-5),
 .UNSPECIFIED.);
#26700=B_SPLINE_CURVE_WITH_KNOTS('',3,(#445911,#445912,#445913,#445914),
 .UNSPECIFIED.,.F.,.F.,(4,4),(0.,7.70025630629238E-5),.UNSPECIFIED.);
#26701=B_SPLINE_CURVE_WITH_KNOTS('',3,(#445924,#445925,#445926,#445927),
 .UNSPECIFIED.,.F.,.F.,(4,4),(4.47028007668187E-19,7.70025630629235E-5),
 .UNSPECIFIED.);
#26702=B_SPLINE_CURVE_WITH_KNOTS('',3,(#445931,#445932,#445933,#445934,
#445935,#445936,#445937,#445938,#445939,#445940,#445941,#445942,#445943,
#445944,#445945,#445946,#445947,#445948,#445949,#445950,#445951,#445952,
#445953,#445954,#445955,#445956,#445957,#445958,#445959,#445960,#445961,
#445962,#445963,#445964,#445965,#445966,#445967),.UNSPECIFIED.,.F.,.F.,
(4,3,3,3,3,3,3,3,3,3,3,3,4),(0.,9.59031527203696E-6,1.9476941122349E-5,
2.02405092183153E-5,3.21374138577552E-5,3.60302195070438E-5,4.42640648819458E-5,
4.53660204229443E-5,5.03633762301987E-5,5.17708036292895E-5,5.37928993851987E-5,
5.54103755460198E-5,5.64557889512956E-5),.UNSPECIFIED.);
#26703=B_SPLINE_CURVE_WITH_KNOTS('',3,(#445968,#445969,#445970,#445971,
#445972,#445973,#445974,#445975,#445976,#445977,#445978,#445979,#445980,
#445981,#445982,#445983,#445984,#445985,#445986,#445987,#445988,#445989,
#445990,#445991,#445992,#445993,#445994,#445995),.UNSPECIFIED.,.F.,.F.,
(4,3,3,3,3,3,3,3,3,4),(5.64557889512956E-5,5.98940966493749E-5,6.34214003873378E-5,
7.22241476084465E-5,7.38322796533362E-5,8.36529189331447E-5,8.80714278222496E-5,
9.84837568500728E-5,0.000108624704079131,0.000110823272382853),
 .UNSPECIFIED.);
#26704=B_SPLINE_CURVE_WITH_KNOTS('',3,(#446011,#446012,#446013,#446014,
#446015,#446016,#446017,#446018,#446019,#446020,#446021,#446022,#446023,
#446024,#446025,#446026,#446027,#446028,#446029,#446030,#446031,#446032,
#446033,#446034,#446035,#446036,#446037,#446038),.UNSPECIFIED.,.F.,.F.,
(4,3,3,3,3,3,3,3,3,4),(0.,8.6603962858097E-6,1.64707715200665E-5,2.24502894132422E-5,
2.49975961757823E-5,2.8852600369028E-5,3.10661348995016E-5,3.4305354351696E-5,
3.66410545653558E-5,4.00504537627886E-5),.UNSPECIFIED.);
#26705=B_SPLINE_CURVE_WITH_KNOTS('',3,(#446041,#446042,#446043,#446044,
#446045,#446046,#446047),.UNSPECIFIED.,.F.,.F.,(4,3,4),(0.,4.40000041065374E-5,
9.89910850773112E-5),.UNSPECIFIED.);
#26706=B_SPLINE_CURVE_WITH_KNOTS('',3,(#446068,#446069,#446070,#446071,
#446072,#446073,#446074,#446075,#446076,#446077,#446078,#446079,#446080,
#446081,#446082,#446083,#446084,#446085,#446086,#446087,#446088,#446089,
#446090,#446091,#446092,#446093,#446094,#446095,#446096,#446097,#446098,
#446099,#446100,#446101),.UNSPECIFIED.,.F.,.F.,(4,3,3,3,3,3,3,3,3,3,3,4),
(0.,4.29157837303425E-6,5.42772623795356E-6,1.00901698482349E-5,1.3127919506864E-5,
1.57383542265805E-5,1.61011507492106E-5,1.67166789291759E-5,1.9534326281136E-5,
2.29377234674651E-5,2.71556047620061E-5,3.34407099942661E-5),
 .UNSPECIFIED.);
#26707=B_SPLINE_CURVE_WITH_KNOTS('',3,(#446114,#446115,#446116,#446117,
#446118,#446119,#446120,#446121,#446122,#446123,#446124,#446125,#446126,
#446127,#446128,#446129,#446130,#446131,#446132,#446133,#446134,#446135,
#446136,#446137,#446138,#446139,#446140,#446141,#446142,#446143,#446144,
#446145,#446146,#446147),.UNSPECIFIED.,.F.,.F.,(4,3,3,3,3,3,3,3,3,3,3,4),
(5.42101086242752E-20,3.71309426656648E-6,5.3998107155943E-6,8.78933289365762E-6,
9.00272357067529E-6,1.0714398450415E-5,1.60780299679587E-5,1.65806081157689E-5,
2.3036972685055E-5,2.67819200416088E-5,3.59736924187735E-5,4.03862783807004E-5),
 .UNSPECIFIED.);
#26708=B_SPLINE_CURVE_WITH_KNOTS('',3,(#446260,#446261,#446262,#446263),
 .UNSPECIFIED.,.F.,.F.,(4,4),(0.,7.70025630629241E-5),.UNSPECIFIED.);
#26709=B_SPLINE_CURVE_WITH_KNOTS('',3,(#446273,#446274,#446275,#446276),
 .UNSPECIFIED.,.F.,.F.,(4,4),(4.41238316394827E-19,7.70025630629236E-5),
 .UNSPECIFIED.);
#26710=B_SPLINE_CURVE_WITH_KNOTS('',3,(#446280,#446281,#446282,#446283,
#446284,#446285,#446286,#446287,#446288,#446289,#446290,#446291,#446292,
#446293,#446294,#446295,#446296,#446297,#446298,#446299,#446300,#446301,
#446302,#446303,#446304,#446305,#446306,#446307,#446308,#446309,#446310,
#446311,#446312,#446313,#446314,#446315,#446316),.UNSPECIFIED.,.F.,.F.,
(4,3,3,3,3,3,3,3,3,3,3,3,4),(0.,9.59031527199735E-6,1.94769411222785E-5,
2.02405092183151E-5,3.2137413857779E-5,3.60302195070439E-5,4.42640648818236E-5,
4.53660204229444E-5,5.03633762302106E-5,5.17708036292896E-5,5.37928993851989E-5,
5.54103755460201E-5,5.64557889507886E-5),.UNSPECIFIED.);
#26711=B_SPLINE_CURVE_WITH_KNOTS('',3,(#446317,#446318,#446319,#446320,
#446321,#446322,#446323,#446324,#446325,#446326,#446327,#446328,#446329,
#446330,#446331,#446332,#446333,#446334,#446335,#446336,#446337,#446338,
#446339,#446340,#446341,#446342,#446343,#446344),.UNSPECIFIED.,.F.,.F.,
(4,3,3,3,3,3,3,3,3,4),(5.64557889507886E-5,5.98940966493751E-5,6.3421400387338E-5,
7.22241476084905E-5,7.38322796533365E-5,8.36529189331635E-5,8.807142782225E-5,
9.8483756850128E-5,0.000108624704079255,0.000110823272382854),
 .UNSPECIFIED.);
#26712=B_SPLINE_CURVE_WITH_KNOTS('',3,(#446360,#446361,#446362,#446363,
#446364,#446365,#446366,#446367,#446368,#446369,#446370,#446371,#446372,
#446373,#446374,#446375,#446376,#446377,#446378,#446379,#446380,#446381,
#446382,#446383,#446384,#446385,#446386,#446387),.UNSPECIFIED.,.F.,.F.,
(4,3,3,3,3,3,3,3,3,4),(0.,8.6603962857781E-6,1.64707715200667E-5,2.2450289413243E-5,
2.49975961757824E-5,2.88526003690281E-5,3.10661348995016E-5,3.43053543516961E-5,
3.66410545653559E-5,4.00504537627887E-5),.UNSPECIFIED.);
#26713=B_SPLINE_CURVE_WITH_KNOTS('',3,(#446390,#446391,#446392,#446393,
#446394,#446395,#446396),.UNSPECIFIED.,.F.,.F.,(4,3,4),(0.,4.40000041065377E-5,
9.89910850773114E-5),.UNSPECIFIED.);
#26714=B_SPLINE_CURVE_WITH_KNOTS('',3,(#446417,#446418,#446419,#446420,
#446421,#446422,#446423,#446424,#446425,#446426,#446427,#446428,#446429,
#446430,#446431,#446432,#446433,#446434,#446435,#446436,#446437,#446438,
#446439,#446440,#446441,#446442,#446443,#446444,#446445,#446446,#446447,
#446448,#446449,#446450),.UNSPECIFIED.,.F.,.F.,(4,3,3,3,3,3,3,3,3,3,3,4),
(0.,4.29157837302368E-6,5.42772623795337E-6,1.00901698482347E-5,1.31279195068638E-5,
1.57383542265853E-5,1.61011507492103E-5,1.67166789291756E-5,1.95343262811357E-5,
2.29377234674647E-5,2.71556047620056E-5,3.34407099942657E-5),
 .UNSPECIFIED.);
#26715=B_SPLINE_CURVE_WITH_KNOTS('',3,(#446463,#446464,#446465,#446466,
#446467,#446468,#446469,#446470,#446471,#446472,#446473,#446474,#446475,
#446476,#446477,#446478,#446479,#446480,#446481,#446482,#446483,#446484,
#446485,#446486,#446487,#446488,#446489,#446490,#446491,#446492,#446493,
#446494,#446495,#446496),.UNSPECIFIED.,.F.,.F.,(4,3,3,3,3,3,3,3,3,3,3,4),
(8.13151629364128E-20,3.71309426656643E-6,5.39981071559413E-6,8.78933289367591E-6,
9.00272357067522E-6,1.07143984504149E-5,1.60780299679527E-5,1.65806081157687E-5,
2.30369726850458E-5,2.67819200416086E-5,3.59736924188039E-5,4.03862783807E-5),
 .UNSPECIFIED.);
#26716=B_SPLINE_CURVE_WITH_KNOTS('',3,(#446609,#446610,#446611,#446612),
 .UNSPECIFIED.,.F.,.F.,(4,4),(4.2351647362715E-22,7.70025630629241E-5),
 .UNSPECIFIED.);
#26717=B_SPLINE_CURVE_WITH_KNOTS('',3,(#446622,#446623,#446624,#446625),
 .UNSPECIFIED.,.F.,.F.,(4,4),(4.43935777737106E-19,7.70025630629237E-5),
 .UNSPECIFIED.);
#26718=B_SPLINE_CURVE_WITH_KNOTS('',3,(#446629,#446630,#446631,#446632,
#446633,#446634,#446635,#446636,#446637,#446638,#446639,#446640,#446641,
#446642,#446643,#446644,#446645,#446646,#446647,#446648,#446649,#446650,
#446651,#446652,#446653,#446654,#446655,#446656,#446657,#446658,#446659,
#446660,#446661,#446662,#446663,#446664,#446665),.UNSPECIFIED.,.F.,.F.,
(4,3,3,3,3,3,3,3,3,3,3,3,4),(0.,9.59031527199033E-6,1.94769411222786E-5,
2.02405092183153E-5,3.21374138577756E-5,3.6030219507044E-5,4.42640648817823E-5,
4.53660204229445E-5,5.03633762302121E-5,5.17708036292897E-5,5.3792899385199E-5,
5.54103755460201E-5,5.64557889509772E-5),.UNSPECIFIED.);
#26719=B_SPLINE_CURVE_WITH_KNOTS('',3,(#446666,#446667,#446668,#446669,
#446670,#446671,#446672,#446673,#446674,#446675,#446676,#446677,#446678,
#446679,#446680,#446681,#446682,#446683,#446684,#446685,#446686,#446687,
#446688,#446689,#446690,#446691,#446692,#446693),.UNSPECIFIED.,.F.,.F.,
(4,3,3,3,3,3,3,3,3,4),(5.64557889509772E-5,5.98940966493752E-5,6.34214003873381E-5,
7.22241476084702E-5,7.38322796533365E-5,8.36529189331638E-5,8.80714278222502E-5,
9.84837568501129E-5,0.000108624704079212,0.000110823272382854),
 .UNSPECIFIED.);
#26720=B_SPLINE_CURVE_WITH_KNOTS('',3,(#446709,#446710,#446711,#446712,
#446713,#446714,#446715,#446716,#446717,#446718,#446719,#446720,#446721,
#446722,#446723,#446724,#446725,#446726,#446727,#446728,#446729,#446730,
#446731,#446732,#446733,#446734,#446735,#446736),.UNSPECIFIED.,.F.,.F.,
(4,3,3,3,3,3,3,3,3,4),(0.,8.66039628577415E-6,1.64707715200667E-5,2.24502894129709E-5,
2.49975961757824E-5,2.8852600369028E-5,3.10661348995016E-5,3.4305354351696E-5,
3.66410545653559E-5,4.00504537627886E-5),.UNSPECIFIED.);
#26721=B_SPLINE_CURVE_WITH_KNOTS('',3,(#446739,#446740,#446741,#446742,
#446743,#446744,#446745),.UNSPECIFIED.,.F.,.F.,(4,3,4),(0.,4.40000041065374E-5,
9.89910850773113E-5),.UNSPECIFIED.);
#26722=B_SPLINE_CURVE_WITH_KNOTS('',3,(#446766,#446767,#446768,#446769,
#446770,#446771,#446772,#446773,#446774,#446775,#446776,#446777,#446778,
#446779,#446780,#446781,#446782,#446783,#446784,#446785,#446786,#446787,
#446788,#446789,#446790,#446791,#446792,#446793,#446794,#446795,#446796,
#446797,#446798,#446799),.UNSPECIFIED.,.F.,.F.,(4,3,3,3,3,3,3,3,3,3,3,4),
(0.,4.29157837305466E-6,5.42772623795305E-6,1.00901698482346E-5,1.31279195068638E-5,
1.57383542265818E-5,1.61011507492103E-5,1.67166789291756E-5,1.95343262811358E-5,
2.29377234674649E-5,2.71556047620057E-5,3.34407099942656E-5),
 .UNSPECIFIED.);
#26723=B_SPLINE_CURVE_WITH_KNOTS('',3,(#446812,#446813,#446814,#446815,
#446816,#446817,#446818,#446819,#446820,#446821,#446822,#446823,#446824,
#446825,#446826,#446827,#446828,#446829,#446830,#446831,#446832,#446833,
#446834,#446835,#446836,#446837,#446838,#446839,#446840,#446841,#446842,
#446843,#446844,#446845),.UNSPECIFIED.,.F.,.F.,(4,3,3,3,3,3,3,3,3,3,3,4),
(9.14795583034644E-20,3.71309426656653E-6,5.39981071559422E-6,8.78933289365931E-6,
9.00272357067526E-6,1.07143984504149E-5,1.60780299679613E-5,1.65806081157687E-5,
2.30369726850558E-5,2.67819200416085E-5,3.5973692418903E-5,4.03862783806968E-5),
 .UNSPECIFIED.);
#26724=B_SPLINE_CURVE_WITH_KNOTS('',3,(#446958,#446959,#446960,#446961),
 .UNSPECIFIED.,.F.,.F.,(4,4),(0.,7.7002563062924E-5),.UNSPECIFIED.);
#26725=B_SPLINE_CURVE_WITH_KNOTS('',3,(#446971,#446972,#446973,#446974),
 .UNSPECIFIED.,.F.,.F.,(4,4),(4.47028007668187E-19,7.70025630629237E-5),
 .UNSPECIFIED.);
#26726=B_SPLINE_CURVE_WITH_KNOTS('',3,(#446978,#446979,#446980,#446981,
#446982,#446983,#446984,#446985,#446986,#446987,#446988,#446989,#446990,
#446991,#446992,#446993,#446994,#446995,#446996,#446997,#446998,#446999,
#447000,#447001,#447002,#447003,#447004,#447005,#447006,#447007,#447008,
#447009,#447010,#447011,#447012,#447013,#447014),.UNSPECIFIED.,.F.,.F.,
(4,3,3,3,3,3,3,3,3,3,3,3,4),(0.,9.5903152720076E-6,1.94769411223003E-5,
2.02405092183152E-5,3.21374138577718E-5,3.60302195070439E-5,4.4264064881891E-5,
4.53660204229443E-5,5.03633762301953E-5,5.17708036292895E-5,5.37928993851988E-5,
5.54103755460199E-5,5.64557889511778E-5),.UNSPECIFIED.);
#26727=B_SPLINE_CURVE_WITH_KNOTS('',3,(#447015,#447016,#447017,#447018,
#447019,#447020,#447021,#447022,#447023,#447024,#447025,#447026,#447027,
#447028,#447029,#447030,#447031,#447032,#447033,#447034,#447035,#447036,
#447037,#447038,#447039,#447040,#447041,#447042),.UNSPECIFIED.,.F.,.F.,
(4,3,3,3,3,3,3,3,3,4),(5.64557889511778E-5,5.9894096649375E-5,6.34214003873379E-5,
7.2224147608466E-5,7.38322796533362E-5,8.36529189331405E-5,8.80714278222499E-5,
9.8483756850072E-5,0.000108624704079137,0.000110823272382853),
 .UNSPECIFIED.);
#26728=B_SPLINE_CURVE_WITH_KNOTS('',3,(#447058,#447059,#447060,#447061,
#447062,#447063,#447064,#447065,#447066,#447067,#447068,#447069,#447070,
#447071,#447072,#447073,#447074,#447075,#447076,#447077,#447078,#447079,
#447080,#447081,#447082,#447083,#447084,#447085),.UNSPECIFIED.,.F.,.F.,
(4,3,3,3,3,3,3,3,3,4),(0.,8.66039628582417E-6,1.64707715200666E-5,2.24502894132344E-5,
2.49975961757823E-5,2.8852600369028E-5,3.10661348995016E-5,3.4305354351696E-5,
3.66410545653559E-5,4.00504537627888E-5),.UNSPECIFIED.);
#26729=B_SPLINE_CURVE_WITH_KNOTS('',3,(#447088,#447089,#447090,#447091,
#447092,#447093,#447094),.UNSPECIFIED.,.F.,.F.,(4,3,4),(0.,4.40000041065374E-5,
9.8991085077311E-5),.UNSPECIFIED.);
#26730=B_SPLINE_CURVE_WITH_KNOTS('',3,(#447115,#447116,#447117,#447118,
#447119,#447120,#447121,#447122,#447123,#447124,#447125,#447126,#447127,
#447128,#447129,#447130,#447131,#447132,#447133,#447134,#447135,#447136,
#447137,#447138,#447139,#447140,#447141,#447142,#447143,#447144,#447145,
#447146,#447147,#447148),.UNSPECIFIED.,.F.,.F.,(4,3,3,3,3,3,3,3,3,3,3,4),
(0.,4.29157837303296E-6,5.4277262379535E-6,1.00901698482348E-5,1.3127919506864E-5,
1.57383542265895E-5,1.61011507492105E-5,1.67166789291755E-5,1.95343262811359E-5,
2.29377234674648E-5,2.71556047620056E-5,3.34407099942656E-5),
 .UNSPECIFIED.);
#26731=B_SPLINE_CURVE_WITH_KNOTS('',3,(#447161,#447162,#447163,#447164,
#447165,#447166,#447167,#447168,#447169,#447170,#447171,#447172,#447173,
#447174,#447175,#447176,#447177,#447178,#447179,#447180,#447181,#447182,
#447183,#447184,#447185,#447186,#447187,#447188,#447189,#447190,#447191,
#447192,#447193,#447194),.UNSPECIFIED.,.F.,.F.,(4,3,3,3,3,3,3,3,3,3,3,4),
(8.13151629364128E-20,3.71309426656644E-6,5.39981071559418E-6,8.78933289368667E-6,
9.00272357067519E-6,1.07143984504149E-5,1.60780299679507E-5,1.65806081157687E-5,
2.30369726850405E-5,2.67819200416087E-5,3.59736924188187E-5,4.03862783807001E-5),
 .UNSPECIFIED.);
#26732=B_SPLINE_CURVE_WITH_KNOTS('',3,(#447307,#447308,#447309,#447310),
 .UNSPECIFIED.,.F.,.F.,(4,4),(0.,7.70025630629242E-5),.UNSPECIFIED.);
#26733=B_SPLINE_CURVE_WITH_KNOTS('',3,(#447320,#447321,#447322,#447323),
 .UNSPECIFIED.,.F.,.F.,(4,4),(4.47028007668187E-19,7.70025630629237E-5),
 .UNSPECIFIED.);
#26734=B_SPLINE_CURVE_WITH_KNOTS('',3,(#447327,#447328,#447329,#447330,
#447331,#447332,#447333,#447334,#447335,#447336,#447337,#447338,#447339,
#447340,#447341,#447342,#447343,#447344,#447345,#447346,#447347,#447348,
#447349,#447350,#447351,#447352,#447353,#447354,#447355,#447356,#447357,
#447358,#447359,#447360,#447361,#447362,#447363),.UNSPECIFIED.,.F.,.F.,
(4,3,3,3,3,3,3,3,3,3,3,3,4),(0.,9.59031527201221E-6,1.94769411223092E-5,
2.02405092183152E-5,3.21374138577726E-5,3.60302195070438E-5,4.42640648819218E-5,
4.53660204229443E-5,5.03633762302023E-5,5.17708036292896E-5,5.37928993851988E-5,
5.54103755460198E-5,5.64557889509462E-5),.UNSPECIFIED.);
#26735=B_SPLINE_CURVE_WITH_KNOTS('',3,(#447364,#447365,#447366,#447367,
#447368,#447369,#447370,#447371,#447372,#447373,#447374,#447375,#447376,
#447377,#447378,#447379,#447380,#447381,#447382,#447383,#447384,#447385,
#447386,#447387,#447388,#447389,#447390,#447391),.UNSPECIFIED.,.F.,.F.,
(4,3,3,3,3,3,3,3,3,4),(5.64557889509462E-5,5.98940966493749E-5,6.34214003873379E-5,
7.22241476084611E-5,7.38322796533362E-5,8.36529189331336E-5,8.80714278222497E-5,
9.84837568500736E-5,0.000108624704079139,0.000110823272382853),
 .UNSPECIFIED.);
#26736=B_SPLINE_CURVE_WITH_KNOTS('',3,(#447407,#447408,#447409,#447410,
#447411,#447412,#447413,#447414,#447415,#447416,#447417,#447418,#447419,
#447420,#447421,#447422,#447423,#447424,#447425,#447426,#447427,#447428,
#447429,#447430,#447431,#447432,#447433,#447434),.UNSPECIFIED.,.F.,.F.,
(4,3,3,3,3,3,3,3,3,4),(0.,8.66039628584135E-6,1.64707715200667E-5,2.24502894132571E-5,
2.49975961757824E-5,2.88526003690282E-5,3.10661348995016E-5,3.43053543516961E-5,
3.6641054565356E-5,4.00504537627888E-5),.UNSPECIFIED.);
#26737=B_SPLINE_CURVE_WITH_KNOTS('',3,(#447437,#447438,#447439,#447440,
#447441,#447442,#447443),.UNSPECIFIED.,.F.,.F.,(4,3,4),(0.,4.40000041065373E-5,
9.89910850773113E-5),.UNSPECIFIED.);
#26738=B_SPLINE_CURVE_WITH_KNOTS('',3,(#447464,#447465,#447466,#447467,
#447468,#447469,#447470,#447471,#447472,#447473,#447474,#447475,#447476,
#447477,#447478,#447479,#447480,#447481,#447482,#447483,#447484,#447485,
#447486,#447487,#447488,#447489,#447490,#447491,#447492,#447493,#447494,
#447495,#447496,#447497),.UNSPECIFIED.,.F.,.F.,(4,3,3,3,3,3,3,3,3,3,3,4),
(0.,4.29157837302508E-6,5.42772623795343E-6,1.00901698482347E-5,1.31279195068639E-5,
1.57383542265875E-5,1.61011507492105E-5,1.67166789291755E-5,1.9534326281136E-5,
2.29377234674652E-5,2.71556047620059E-5,3.3440709994266E-5),
 .UNSPECIFIED.);
#26739=B_SPLINE_CURVE_WITH_KNOTS('',3,(#447510,#447511,#447512,#447513,
#447514,#447515,#447516,#447517,#447518,#447519,#447520,#447521,#447522,
#447523,#447524,#447525,#447526,#447527,#447528,#447529,#447530,#447531,
#447532,#447533,#447534,#447535,#447536,#447537,#447538,#447539,#447540,
#447541,#447542,#447543),.UNSPECIFIED.,.F.,.F.,(4,3,3,3,3,3,3,3,3,3,3,4),
(5.42101086242752E-20,3.71309426656648E-6,5.39981071559421E-6,8.78933289331524E-6,
9.00272357067526E-6,1.0714398450415E-5,1.60780299679625E-5,1.65806081157688E-5,
2.30369726850327E-5,2.67819200416088E-5,3.59736924187896E-5,4.03862783807003E-5),
 .UNSPECIFIED.);
#26740=B_SPLINE_CURVE_WITH_KNOTS('',3,(#447656,#447657,#447658,#447659),
 .UNSPECIFIED.,.F.,.F.,(4,4),(0.,7.70025630629239E-5),.UNSPECIFIED.);
#26741=B_SPLINE_CURVE_WITH_KNOTS('',3,(#447669,#447670,#447671,#447672),
 .UNSPECIFIED.,.F.,.F.,(4,4),(1.0842021724855E-19,7.70025630629237E-5),
 .UNSPECIFIED.);
#26742=B_SPLINE_CURVE_WITH_KNOTS('',3,(#447676,#447677,#447678,#447679,
#447680,#447681,#447682,#447683,#447684,#447685,#447686,#447687,#447688,
#447689,#447690,#447691,#447692,#447693,#447694,#447695,#447696,#447697,
#447698,#447699,#447700,#447701,#447702,#447703,#447704,#447705,#447706,
#447707,#447708,#447709,#447710,#447711,#447712),.UNSPECIFIED.,.F.,.F.,
(4,3,3,3,3,3,3,3,3,3,3,3,4),(0.,9.59031527200873E-6,1.94769411223043E-5,
2.02405092183151E-5,3.21374138577679E-5,3.60302195070439E-5,4.42640648818551E-5,
4.53660204229443E-5,5.0363376230211E-5,5.17708036292896E-5,5.37928993851988E-5,
5.54103755460199E-5,5.64557889511168E-5),.UNSPECIFIED.);
#26743=B_SPLINE_CURVE_WITH_KNOTS('',3,(#447713,#447714,#447715,#447716,
#447717,#447718,#447719,#447720,#447721,#447722,#447723,#447724,#447725,
#447726,#447727,#447728,#447729,#447730,#447731,#447732,#447733,#447734,
#447735,#447736,#447737,#447738,#447739,#447740),.UNSPECIFIED.,.F.,.F.,
(4,3,3,3,3,3,3,3,3,4),(5.64557889511168E-5,5.9894096649375E-5,6.34214003873379E-5,
7.22241476083523E-5,7.38322796533361E-5,8.36529189331479E-5,8.80714278222499E-5,
9.8483756850077E-5,0.000108624704079147,0.000110823272382853),
 .UNSPECIFIED.);
#26744=B_SPLINE_CURVE_WITH_KNOTS('',3,(#447756,#447757,#447758,#447759,
#447760,#447761,#447762,#447763,#447764,#447765,#447766,#447767,#447768,
#447769,#447770,#447771,#447772,#447773,#447774,#447775,#447776,#447777,
#447778,#447779,#447780,#447781,#447782,#447783),.UNSPECIFIED.,.F.,.F.,
(4,3,3,3,3,3,3,3,3,4),(0.,8.66039628581661E-6,1.64707715200667E-5,2.24502894132545E-5,
2.49975961757824E-5,2.8852600369028E-5,3.10661348995016E-5,3.4305354351696E-5,
3.66410545653559E-5,4.00504537627887E-5),.UNSPECIFIED.);
#26745=B_SPLINE_CURVE_WITH_KNOTS('',3,(#447786,#447787,#447788,#447789,
#447790,#447791,#447792),.UNSPECIFIED.,.F.,.F.,(4,3,4),(0.,4.40000041065374E-5,
9.8991085077311E-5),.UNSPECIFIED.);
#26746=B_SPLINE_CURVE_WITH_KNOTS('',3,(#447813,#447814,#447815,#447816,
#447817,#447818,#447819,#447820,#447821,#447822,#447823,#447824,#447825,
#447826,#447827,#447828,#447829,#447830,#447831,#447832,#447833,#447834,
#447835,#447836,#447837,#447838,#447839,#447840,#447841,#447842,#447843,
#447844,#447845,#447846),.UNSPECIFIED.,.F.,.F.,(4,3,3,3,3,3,3,3,3,3,3,4),
(0.,4.2915783730183E-6,5.42772623795347E-6,1.00901698482349E-5,1.31279195068642E-5,
1.57383542265885E-5,1.61011507492107E-5,1.67166789291759E-5,1.95343262811362E-5,
2.29377234674653E-5,2.71556047620063E-5,3.34407099942661E-5),
 .UNSPECIFIED.);
#26747=B_SPLINE_CURVE_WITH_KNOTS('',3,(#447859,#447860,#447861,#447862,
#447863,#447864,#447865,#447866,#447867,#447868,#447869,#447870,#447871,
#447872,#447873,#447874,#447875,#447876,#447877,#447878,#447879,#447880,
#447881,#447882,#447883,#447884,#447885,#447886,#447887,#447888,#447889,
#447890,#447891,#447892),.UNSPECIFIED.,.F.,.F.,(4,3,3,3,3,3,3,3,3,3,3,4),
(2.16840434497101E-19,3.71309426656641E-6,5.39981071559409E-6,8.78933289329756E-6,
9.00272357067517E-6,1.07143984504149E-5,1.60780299679583E-5,1.65806081157685E-5,
2.30369726850452E-5,2.67819200416083E-5,3.59736924187826E-5,4.03862783806996E-5),
 .UNSPECIFIED.);
#26748=B_SPLINE_CURVE_WITH_KNOTS('',3,(#448005,#448006,#448007,#448008),
 .UNSPECIFIED.,.F.,.F.,(4,4),(0.,7.7002563062924E-5),.UNSPECIFIED.);
#26749=B_SPLINE_CURVE_WITH_KNOTS('',3,(#448018,#448019,#448020,#448021),
 .UNSPECIFIED.,.F.,.F.,(4,4),(2.16840434497101E-19,7.70025630629238E-5),
 .UNSPECIFIED.);
#26750=B_SPLINE_CURVE_WITH_KNOTS('',3,(#448025,#448026,#448027,#448028,
#448029,#448030,#448031,#448032,#448033,#448034,#448035,#448036,#448037,
#448038,#448039,#448040,#448041,#448042,#448043,#448044,#448045,#448046,
#448047,#448048,#448049,#448050,#448051,#448052,#448053,#448054,#448055,
#448056,#448057,#448058,#448059,#448060,#448061),.UNSPECIFIED.,.F.,.F.,
(4,3,3,3,3,3,3,3,3,3,3,3,4),(0.,9.59031527198866E-6,1.94769411222687E-5,
2.02405092183153E-5,3.21374138577716E-5,3.60302195070438E-5,4.42640648818875E-5,
4.53660204229444E-5,5.0363376230206E-5,5.17708036292895E-5,5.37928993851989E-5,
5.54103755460199E-5,5.64557889511988E-5),.UNSPECIFIED.);
#26751=B_SPLINE_CURVE_WITH_KNOTS('',3,(#448062,#448063,#448064,#448065,
#448066,#448067,#448068,#448069,#448070,#448071,#448072,#448073,#448074,
#448075,#448076,#448077,#448078,#448079,#448080,#448081,#448082,#448083,
#448084,#448085,#448086,#448087,#448088,#448089),.UNSPECIFIED.,.F.,.F.,
(4,3,3,3,3,3,3,3,3,4),(5.64557889511988E-5,5.9894096649375E-5,6.34214003873379E-5,
7.22241476083957E-5,7.38322796533361E-5,8.36529189331633E-5,8.80714278222497E-5,
9.84837568501205E-5,0.000108624704079235,0.000110823272382853),
 .UNSPECIFIED.);
#26752=B_SPLINE_CURVE_WITH_KNOTS('',3,(#448105,#448106,#448107,#448108,
#448109,#448110,#448111,#448112,#448113,#448114,#448115,#448116,#448117,
#448118,#448119,#448120,#448121,#448122,#448123,#448124,#448125,#448126,
#448127,#448128,#448129,#448130,#448131,#448132),.UNSPECIFIED.,.F.,.F.,
(4,3,3,3,3,3,3,3,3,4),(0.,8.66039628578604E-6,1.64707715200665E-5,2.24502894132191E-5,
2.49975961757823E-5,2.8852600369028E-5,3.10661348995016E-5,3.4305354351696E-5,
3.66410545653559E-5,4.00504537627889E-5),.UNSPECIFIED.);
#26753=B_SPLINE_CURVE_WITH_KNOTS('',3,(#448135,#448136,#448137,#448138,
#448139,#448140,#448141),.UNSPECIFIED.,.F.,.F.,(4,3,4),(0.,4.40000041065374E-5,
9.89910850773112E-5),.UNSPECIFIED.);
#26754=B_SPLINE_CURVE_WITH_KNOTS('',3,(#448162,#448163,#448164,#448165,
#448166,#448167,#448168,#448169,#448170,#448171,#448172,#448173,#448174,
#448175,#448176,#448177,#448178,#448179,#448180,#448181,#448182,#448183,
#448184,#448185,#448186,#448187,#448188,#448189,#448190,#448191,#448192,
#448193,#448194,#448195),.UNSPECIFIED.,.F.,.F.,(4,3,3,3,3,3,3,3,3,3,3,4),
(0.,4.29157837303585E-6,5.42772623795341E-6,1.00901698482348E-5,1.3127919506864E-5,
1.5738354226579E-5,1.61011507492105E-5,1.67166789291754E-5,1.95343262811359E-5,
2.29377234674646E-5,2.71556047620056E-5,3.34407099942653E-5),
 .UNSPECIFIED.);
#26755=B_SPLINE_CURVE_WITH_KNOTS('',3,(#448208,#448209,#448210,#448211,
#448212,#448213,#448214,#448215,#448216,#448217,#448218,#448219,#448220,
#448221,#448222,#448223,#448224,#448225,#448226,#448227,#448228,#448229,
#448230,#448231,#448232,#448233,#448234,#448235,#448236,#448237,#448238,
#448239,#448240,#448241),.UNSPECIFIED.,.F.,.F.,(4,3,3,3,3,3,3,3,3,3,3,4),
(1.0842021724855E-19,3.7130942665665E-6,5.39981071559421E-6,8.78933289329038E-6,
9.00272357067531E-6,1.0714398450415E-5,1.60780299679534E-5,1.65806081157688E-5,
2.30369726850481E-5,2.67819200416089E-5,3.59736924187636E-5,4.03862783807004E-5),
 .UNSPECIFIED.);
#26756=B_SPLINE_CURVE_WITH_KNOTS('',3,(#448354,#448355,#448356,#448357),
 .UNSPECIFIED.,.F.,.F.,(4,4),(0.,7.70025630629239E-5),.UNSPECIFIED.);
#26757=B_SPLINE_CURVE_WITH_KNOTS('',3,(#448367,#448368,#448369,#448370),
 .UNSPECIFIED.,.F.,.F.,(4,4),(0.,7.70025630629241E-5),.UNSPECIFIED.);
#26758=B_SPLINE_CURVE_WITH_KNOTS('',3,(#448374,#448375,#448376,#448377,
#448378,#448379,#448380,#448381,#448382,#448383,#448384,#448385,#448386,
#448387,#448388,#448389,#448390,#448391,#448392,#448393,#448394,#448395,
#448396,#448397,#448398,#448399,#448400,#448401,#448402,#448403,#448404,
#448405,#448406,#448407,#448408,#448409,#448410),.UNSPECIFIED.,.F.,.F.,
(4,3,3,3,3,3,3,3,3,3,3,3,4),(0.,9.59031527198869E-6,1.94769411222726E-5,
2.02405092183153E-5,3.21374138577653E-5,3.60302195070441E-5,4.42640648818868E-5,
4.53660204229444E-5,5.03633762302017E-5,5.17708036292897E-5,5.37928993851991E-5,
5.54103755460197E-5,5.64557889511107E-5),.UNSPECIFIED.);
#26759=B_SPLINE_CURVE_WITH_KNOTS('',3,(#448411,#448412,#448413,#448414,
#448415,#448416,#448417,#448418,#448419,#448420,#448421,#448422,#448423,
#448424,#448425,#448426,#448427,#448428,#448429,#448430,#448431,#448432,
#448433,#448434,#448435,#448436,#448437,#448438),.UNSPECIFIED.,.F.,.F.,
(4,3,3,3,3,3,3,3,3,4),(5.64557889511107E-5,5.98940966493752E-5,6.34214003873379E-5,
7.22241476084464E-5,7.38322796533364E-5,8.36529189331498E-5,8.807142782225E-5,
9.84837568500754E-5,0.000108624704079144,0.000110823272382853),
 .UNSPECIFIED.);
#26760=B_SPLINE_CURVE_WITH_KNOTS('',3,(#448454,#448455,#448456,#448457,
#448458,#448459,#448460,#448461,#448462,#448463,#448464,#448465,#448466,
#448467,#448468,#448469,#448470,#448471,#448472,#448473,#448474,#448475,
#448476,#448477,#448478,#448479,#448480,#448481),.UNSPECIFIED.,.F.,.F.,
(4,3,3,3,3,3,3,3,3,4),(0.,8.66039628580875E-6,1.64707715200666E-5,2.24502894132507E-5,
2.49975961757822E-5,2.8852600369028E-5,3.10661348995017E-5,3.43053543516959E-5,
3.66410545653558E-5,4.00504537627884E-5),.UNSPECIFIED.);
#26761=B_SPLINE_CURVE_WITH_KNOTS('',3,(#448484,#448485,#448486,#448487,
#448488,#448489,#448490),.UNSPECIFIED.,.F.,.F.,(4,3,4),(0.,4.40000041065377E-5,
9.89910850773113E-5),.UNSPECIFIED.);
#26762=B_SPLINE_CURVE_WITH_KNOTS('',3,(#448511,#448512,#448513,#448514,
#448515,#448516,#448517,#448518,#448519,#448520,#448521,#448522,#448523,
#448524,#448525,#448526,#448527,#448528,#448529,#448530,#448531,#448532,
#448533,#448534,#448535,#448536,#448537,#448538,#448539,#448540,#448541,
#448542,#448543,#448544),.UNSPECIFIED.,.F.,.F.,(4,3,3,3,3,3,3,3,3,3,3,4),
(0.,4.29157837305611E-6,5.42772623795344E-6,1.00901698482349E-5,1.3127919506864E-5,
1.5738354226584E-5,1.61011507492106E-5,1.6716678929175E-5,1.95343262811357E-5,
2.29377234674646E-5,2.71556047620054E-5,3.34407099942654E-5),
 .UNSPECIFIED.);
#26763=B_SPLINE_CURVE_WITH_KNOTS('',3,(#448557,#448558,#448559,#448560,
#448561,#448562,#448563,#448564,#448565,#448566,#448567,#448568,#448569,
#448570,#448571,#448572,#448573,#448574,#448575,#448576,#448577,#448578,
#448579,#448580,#448581,#448582,#448583,#448584,#448585,#448586,#448587,
#448588,#448589,#448590),.UNSPECIFIED.,.F.,.F.,(4,3,3,3,3,3,3,3,3,3,3,4),
(0.,3.71309426656648E-6,5.3998107155944E-6,8.78933289331138E-6,9.00272357067539E-6,
1.0714398450415E-5,1.60780299679542E-5,1.65806081157689E-5,2.30369726850623E-5,
2.67819200416089E-5,3.5973692418722E-5,4.03862783807005E-5),
 .UNSPECIFIED.);
#26764=B_SPLINE_CURVE_WITH_KNOTS('',3,(#448703,#448704,#448705,#448706),
 .UNSPECIFIED.,.F.,.F.,(4,4),(0.,7.70025630629239E-5),.UNSPECIFIED.);
#26765=B_SPLINE_CURVE_WITH_KNOTS('',3,(#448716,#448717,#448718,#448719),
 .UNSPECIFIED.,.F.,.F.,(4,4),(2.16840434497101E-19,7.70025630629239E-5),
 .UNSPECIFIED.);
#26766=B_SPLINE_CURVE_WITH_KNOTS('',3,(#448723,#448724,#448725,#448726,
#448727,#448728,#448729,#448730,#448731,#448732,#448733,#448734,#448735,
#448736,#448737,#448738,#448739,#448740,#448741,#448742,#448743,#448744,
#448745,#448746,#448747,#448748,#448749,#448750,#448751,#448752,#448753,
#448754,#448755,#448756,#448757,#448758,#448759),.UNSPECIFIED.,.F.,.F.,
(4,3,3,3,3,3,3,3,3,3,3,3,4),(0.,9.59031527201032E-6,1.94769411223074E-5,
2.02405092183152E-5,3.21374138577751E-5,3.60302195070438E-5,4.42640648818425E-5,
4.53660204229442E-5,5.03633762302174E-5,5.17708036292895E-5,5.37928993851987E-5,
5.54103755460198E-5,5.64557889512764E-5),.UNSPECIFIED.);
#26767=B_SPLINE_CURVE_WITH_KNOTS('',3,(#448760,#448761,#448762,#448763,
#448764,#448765,#448766,#448767,#448768,#448769,#448770,#448771,#448772,
#448773,#448774,#448775,#448776,#448777,#448778,#448779,#448780,#448781,
#448782,#448783,#448784,#448785,#448786,#448787),.UNSPECIFIED.,.F.,.F.,
(4,3,3,3,3,3,3,3,3,4),(5.64557889512764E-5,5.9894096649375E-5,6.34214003873378E-5,
7.22241476084241E-5,7.38322796533363E-5,8.36529189331436E-5,8.80714278222494E-5,
9.8483756850073E-5,0.000108624704079142,0.000110823272382853),
 .UNSPECIFIED.);
#26768=B_SPLINE_CURVE_WITH_KNOTS('',3,(#448803,#448804,#448805,#448806,
#448807,#448808,#448809,#448810,#448811,#448812,#448813,#448814,#448815,
#448816,#448817,#448818,#448819,#448820,#448821,#448822,#448823,#448824,
#448825,#448826,#448827,#448828,#448829,#448830),.UNSPECIFIED.,.F.,.F.,
(4,3,3,3,3,3,3,3,3,4),(0.,8.66039628580909E-6,1.64707715200669E-5,2.24502894132356E-5,
2.49975961757829E-5,2.88526003690284E-5,3.10661348995019E-5,3.43053543516966E-5,
3.66410545653565E-5,4.0050453762789E-5),.UNSPECIFIED.);
#26769=B_SPLINE_CURVE_WITH_KNOTS('',3,(#448833,#448834,#448835,#448836,
#448837,#448838,#448839),.UNSPECIFIED.,.F.,.F.,(4,3,4),(0.,4.40000041065376E-5,
9.89910850773114E-5),.UNSPECIFIED.);
#26770=B_SPLINE_CURVE_WITH_KNOTS('',3,(#448860,#448861,#448862,#448863,
#448864,#448865,#448866,#448867,#448868,#448869,#448870,#448871,#448872,
#448873,#448874,#448875,#448876,#448877,#448878,#448879,#448880,#448881,
#448882,#448883,#448884,#448885,#448886,#448887,#448888,#448889,#448890,
#448891,#448892,#448893),.UNSPECIFIED.,.F.,.F.,(4,3,3,3,3,3,3,3,3,3,3,4),
(0.,4.29157837305915E-6,5.42772623795332E-6,1.00901698482347E-5,1.31279195068641E-5,
1.57383542265863E-5,1.61011507492104E-5,1.67166789291754E-5,1.95343262811356E-5,
2.29377234674649E-5,2.71556047620056E-5,3.34407099942654E-5),
 .UNSPECIFIED.);
#26771=B_SPLINE_CURVE_WITH_KNOTS('',3,(#448906,#448907,#448908,#448909,
#448910,#448911,#448912,#448913,#448914,#448915,#448916,#448917,#448918,
#448919,#448920,#448921,#448922,#448923,#448924,#448925,#448926,#448927,
#448928,#448929,#448930,#448931,#448932,#448933,#448934,#448935,#448936,
#448937,#448938,#448939),.UNSPECIFIED.,.F.,.F.,(4,3,3,3,3,3,3,3,3,3,3,4),
(0.,3.71309426656643E-6,5.39981071559402E-6,8.7893328936724E-6,9.00272357067533E-6,
1.07143984504149E-5,1.60780299679559E-5,1.6580608115769E-5,2.30369726850549E-5,
2.67819200416093E-5,3.59736924187847E-5,4.03862783807012E-5),
 .UNSPECIFIED.);
#26772=B_SPLINE_CURVE_WITH_KNOTS('',3,(#449052,#449053,#449054,#449055),
 .UNSPECIFIED.,.F.,.F.,(4,4),(0.,7.70025630629241E-5),.UNSPECIFIED.);
#26773=B_SPLINE_CURVE_WITH_KNOTS('',3,(#449065,#449066,#449067,#449068),
 .UNSPECIFIED.,.F.,.F.,(4,4),(2.16840434497101E-19,7.70025630629236E-5),
 .UNSPECIFIED.);
#26774=B_SPLINE_CURVE_WITH_KNOTS('',3,(#449072,#449073,#449074,#449075,
#449076,#449077,#449078,#449079,#449080,#449081,#449082,#449083,#449084,
#449085,#449086,#449087,#449088,#449089,#449090,#449091,#449092,#449093,
#449094,#449095,#449096,#449097,#449098,#449099,#449100,#449101,#449102,
#449103,#449104,#449105,#449106,#449107,#449108),.UNSPECIFIED.,.F.,.F.,
(4,3,3,3,3,3,3,3,3,3,3,3,4),(0.,9.59031527202431E-6,1.94769411223246E-5,
2.02405092183152E-5,3.21374138577649E-5,3.6030219507044E-5,4.42640648818395E-5,
4.53660204229444E-5,5.03633762301883E-5,5.17708036292894E-5,5.37928993851986E-5,
5.54103755460197E-5,5.64557889512117E-5),.UNSPECIFIED.);
#26775=B_SPLINE_CURVE_WITH_KNOTS('',3,(#449109,#449110,#449111,#449112,
#449113,#449114,#449115,#449116,#449117,#449118,#449119,#449120,#449121,
#449122,#449123,#449124,#449125,#449126,#449127,#449128,#449129,#449130,
#449131,#449132,#449133,#449134,#449135,#449136),.UNSPECIFIED.,.F.,.F.,
(4,3,3,3,3,3,3,3,3,4),(5.64557889512117E-5,5.9894096649375E-5,6.34214003873379E-5,
7.22241476084387E-5,7.38322796533362E-5,8.36529189331548E-5,8.80714278222501E-5,
9.8483756850112E-5,0.000108624704079212,0.000110823272382853),
 .UNSPECIFIED.);
#26776=B_SPLINE_CURVE_WITH_KNOTS('',3,(#449152,#449153,#449154,#449155,
#449156,#449157,#449158,#449159,#449160,#449161,#449162,#449163,#449164,
#449165,#449166,#449167,#449168,#449169,#449170,#449171,#449172,#449173,
#449174,#449175,#449176,#449177,#449178,#449179),.UNSPECIFIED.,.F.,.F.,
(4,3,3,3,3,3,3,3,3,4),(0.,8.66039628580669E-6,1.64707715200667E-5,2.24502894132311E-5,
2.49975961757824E-5,2.88526003690281E-5,3.10661348995017E-5,3.4305354351696E-5,
3.66410545653558E-5,4.00504537627885E-5),.UNSPECIFIED.);
#26777=B_SPLINE_CURVE_WITH_KNOTS('',3,(#449182,#449183,#449184,#449185,
#449186,#449187,#449188),.UNSPECIFIED.,.F.,.F.,(4,3,4),(0.,4.40000041065373E-5,
9.89910850773112E-5),.UNSPECIFIED.);
#26778=B_SPLINE_CURVE_WITH_KNOTS('',3,(#449209,#449210,#449211,#449212,
#449213,#449214,#449215,#449216,#449217,#449218,#449219,#449220,#449221,
#449222,#449223,#449224,#449225,#449226,#449227,#449228,#449229,#449230,
#449231,#449232,#449233,#449234,#449235,#449236,#449237,#449238,#449239,
#449240,#449241,#449242),.UNSPECIFIED.,.F.,.F.,(4,3,3,3,3,3,3,3,3,3,3,4),
(0.,4.2915783730327E-6,5.42772623795325E-6,1.00901698482348E-5,1.31279195068637E-5,
1.57383542265831E-5,1.61011507492103E-5,1.67166789291759E-5,1.9534326281136E-5,
2.29377234674645E-5,2.71556047620059E-5,3.3440709994266E-5),
 .UNSPECIFIED.);
#26779=B_SPLINE_CURVE_WITH_KNOTS('',3,(#449255,#449256,#449257,#449258,
#449259,#449260,#449261,#449262,#449263,#449264,#449265,#449266,#449267,
#449268,#449269,#449270,#449271,#449272,#449273,#449274,#449275,#449276,
#449277,#449278,#449279,#449280,#449281,#449282,#449283,#449284,#449285,
#449286,#449287,#449288),.UNSPECIFIED.,.F.,.F.,(4,3,3,3,3,3,3,3,3,3,3,4),
(2.16840434497101E-19,3.71309426656647E-6,5.39981071559407E-6,8.78933289331909E-6,
9.00272357067532E-6,1.0714398450415E-5,1.60780299679462E-5,1.65806081157688E-5,
2.30369726850435E-5,2.67819200416086E-5,3.59736924187839E-5,4.03862783807001E-5),
 .UNSPECIFIED.);
#26780=B_SPLINE_CURVE_WITH_KNOTS('',3,(#449399,#449400,#449401,#449402,
#449403,#449404,#449405),.UNSPECIFIED.,.F.,.F.,(4,3,4),(-48.8692190558412,
-47.9084138130922,-47.8494095495406),.UNSPECIFIED.);
#26781=B_SPLINE_CURVE_WITH_KNOTS('',3,(#449411,#449412,#449413,#449414,
#449415,#449416,#449417,#449418,#449419,#449420,#449421,#449422,#449423,
#449424,#449425,#449426,#449427,#449428,#449429),.UNSPECIFIED.,.F.,.F.,
(4,3,3,3,3,3,4),(45.2902480251326,45.9122299042133,46.9103218586527,47.9084138130921,
48.9065057675316,49.904597721971,50.9026896764104),.UNSPECIFIED.);
#26782=B_SPLINE_CURVE_WITH_KNOTS('',3,(#449431,#449432,#449433,#449434,
#449435,#449436,#449437,#449438,#449439,#449440,#449441,#449442,#449443,
#449444,#449445,#449446,#449447,#449448,#449449,#449450,#449451,#449452),
 .UNSPECIFIED.,.F.,.F.,(4,3,3,3,3,3,3,4),(-47.8494095495406,-46.9103218586527,
-45.9122299042133,-44.9141379497739,-43.9160459953345,-42.9179540408951,
-41.9198620864556,-41.5662242423611),.UNSPECIFIED.);
#26783=B_SPLINE_CURVE_WITH_KNOTS('',3,(#449457,#449458,#449459,#449460,
#449461,#449462,#449463,#449464,#449465,#449466,#449467,#449468,#449469,
#449470,#449471,#449472,#449473,#449474,#449475,#449476,#449477,#449478),
 .UNSPECIFIED.,.F.,.F.,(4,3,3,3,3,3,3,4),(39.007062717953,39.9236781775768,
40.9217701320162,41.9198620864556,42.917954040895,43.9160459953345,44.9141379497739,
45.2902480251326),.UNSPECIFIED.);
#26784=B_SPLINE_CURVE_WITH_KNOTS('',3,(#449479,#449480,#449481,#449482,
#449483,#449484,#449485,#449486,#449487,#449488,#449489,#449490,#449491,
#449492,#449493,#449494,#449495,#449496,#449497,#449498,#449499,#449500),
 .UNSPECIFIED.,.F.,.F.,(4,3,3,3,3,3,3,4),(-41.5662242423611,-40.9217701320162,
-39.9236781775768,-38.9255862231374,-37.927494268698,-36.9294023142585,
-35.9313103598191,-35.2830389351814),.UNSPECIFIED.);
#26785=B_SPLINE_CURVE_WITH_KNOTS('',3,(#449505,#449506,#449507,#449508,
#449509,#449510,#449511,#449512,#449513,#449514,#449515,#449516,#449517,
#449518,#449519,#449520,#449521,#449522,#449523,#449524,#449525,#449526,
#449527,#449528,#449529),.UNSPECIFIED.,.F.,.F.,(4,3,3,3,3,3,3,3,4),(32.7238774107735,
32.9370344965008,33.9351264509403,34.9332184053797,35.9313103598191,36.9294023142585,
37.9274942686979,38.9255862231374,39.007062717953),.UNSPECIFIED.);
#26786=B_SPLINE_CURVE_WITH_KNOTS('',3,(#449530,#449531,#449532,#449533,
#449534,#449535,#449536,#449537,#449538,#449539,#449540,#449541,#449542,
#449543,#449544,#449545,#449546,#449547,#449548,#449549,#449550,#449551),
 .UNSPECIFIED.,.F.,.F.,(4,3,3,3,3,3,3,4),(-35.2830389351814,-34.9332184053797,
-33.9351264509403,-32.9370344965009,-31.9389425420614,-30.940850587622,
-29.9427586331826,-28.9998536280018),.UNSPECIFIED.);
#26787=B_SPLINE_CURVE_WITH_KNOTS('',3,(#449556,#449557,#449558,#449559,
#449560,#449561,#449562,#449563,#449564,#449565,#449566,#449567,#449568,
#449569,#449570,#449571,#449572,#449573,#449574,#449575,#449576,#449577),
 .UNSPECIFIED.,.F.,.F.,(4,3,3,3,3,3,3,4),(26.4406921035939,26.9484827698643,
27.9465747243037,28.9446666787432,29.9427586331826,30.940850587622,31.9389425420614,
32.7238774107735),.UNSPECIFIED.);
#26788=B_SPLINE_CURVE_WITH_KNOTS('',3,(#449578,#449579,#449580,#449581,
#449582,#449583,#449584,#449585,#449586,#449587,#449588,#449589,#449590,
#449591,#449592,#449593,#449594,#449595,#449596,#449597,#449598,#449599,
#449600,#449601,#449602),.UNSPECIFIED.,.F.,.F.,(4,3,3,3,3,3,3,3,4),(-28.9998536280018,
-28.9446666787432,-27.9465747243038,-26.9484827698643,-25.9503908154249,
-24.9522988609855,-23.9542069065461,-22.9561149521067,-22.7166683208223),
 .UNSPECIFIED.);
#26789=B_SPLINE_CURVE_WITH_KNOTS('',3,(#449607,#449608,#449609,#449610,
#449611,#449612,#449613,#449614,#449615,#449616,#449617,#449618,#449619,
#449620,#449621,#449622,#449623,#449624,#449625,#449626,#449627,#449628),
 .UNSPECIFIED.,.F.,.F.,(4,3,3,3,3,3,3,4),(20.1575067964143,20.9599310432278,
21.9580229976672,22.9561149521067,23.9542069065461,24.9522988609855,25.9503908154249,
26.4406921035939),.UNSPECIFIED.);
#26790=B_SPLINE_CURVE_WITH_KNOTS('',3,(#449629,#449630,#449631,#449632,
#449633,#449634,#449635,#449636,#449637,#449638,#449639,#449640,#449641,
#449642,#449643,#449644,#449645,#449646,#449647,#449648,#449649,#449650),
 .UNSPECIFIED.,.F.,.F.,(4,3,3,3,3,3,3,4),(-22.7166683208223,-21.9580229976672,
-20.9599310432278,-19.9618390887884,-18.963747134349,-17.9656551799096,
-16.9675632254701,-16.4334830136427),.UNSPECIFIED.);
#26791=B_SPLINE_CURVE_WITH_KNOTS('',3,(#449655,#449656,#449657,#449658,
#449659,#449660,#449661,#449662,#449663,#449664,#449665,#449666,#449667,
#449668,#449669,#449670,#449671,#449672,#449673,#449674,#449675,#449676,
#449677,#449678,#449679),.UNSPECIFIED.,.F.,.F.,(4,3,3,3,3,3,3,3,4),(13.8743214892347,
13.9732873621519,14.9713793165913,15.9694712710307,16.9675632254701,17.9656551799096,
18.963747134349,19.9618390887884,20.1575067964143),.UNSPECIFIED.);
#26792=B_SPLINE_CURVE_WITH_KNOTS('',3,(#449680,#449681,#449682,#449683,
#449684,#449685,#449686,#449687,#449688,#449689,#449690,#449691,#449692,
#449693,#449694,#449695,#449696,#449697,#449698,#449699,#449700,#449701),
 .UNSPECIFIED.,.F.,.F.,(4,3,3,3,3,3,3,4),(-16.4334830136427,-15.9694712710307,
-14.9713793165913,-13.9732873621519,-12.9751954077125,-11.977103453273,
-10.9790114988336,-10.1502977064631),.UNSPECIFIED.);
#26793=B_SPLINE_CURVE_WITH_KNOTS('',3,(#449707,#449708,#449709,#449710,
#449711,#449712,#449713,#449714,#449715,#449716,#449717,#449718,#449719),
 .UNSPECIFIED.,.F.,.F.,(4,3,3,3,4),(-3.86711239928348,-2.99427586331826,
-1.99618390887884,-0.998091954439421,0.),.UNSPECIFIED.);
#26794=B_SPLINE_CURVE_WITH_KNOTS('',3,(#449722,#449723,#449724,#449725,
#449726,#449727,#449728,#449729,#449730,#449731,#449732,#449733,#449734,
#449735,#449736,#449737,#449738,#449739,#449740),.UNSPECIFIED.,.F.,.F.,
(4,3,3,3,3,3,4),(2.03347062056922,2.99427586331826,3.99236781775768,4.9904597721971,
5.98855172663652,6.98664368107594,7.59113618205511),.UNSPECIFIED.);
#26795=B_SPLINE_CURVE_WITH_KNOTS('',3,(#449746,#449747,#449748,#449749,
#449750,#449751,#449752),.UNSPECIFIED.,.F.,.F.,(4,1,1,1,4),(59.6902604182061,
59.7492646817576,60.747356636197,61.7454485906364,62.7435405450759),
 .UNSPECIFIED.);
#26796=B_SPLINE_CURVE_WITH_KNOTS('',3,(#449755,#449756,#449757,#449758,
#449759,#449760,#449761),.UNSPECIFIED.,.F.,.F.,(4,1,1,1,4),(59.6902604182061,
60.3122422972867,61.3103342517261,62.3084262061655,63.2692314489146),
 .UNSPECIFIED.);
#26797=B_SPLINE_CURVE_WITH_KNOTS('',3,(#449766,#449767,#449768,#449769,
#449770,#449771,#449772,#449773,#449774,#449775),.UNSPECIFIED.,.F.,.F.,
(4,1,1,1,1,1,1,4),(53.4070751110265,53.7607129551211,54.7588049095605,55.7568968639999,
56.7549888184393,57.7530807728788,58.7511727273182,59.6902604182061),
 .UNSPECIFIED.);
#26798=B_SPLINE_CURVE_WITH_KNOTS('',3,(#449776,#449777,#449778,#449779,
#449780,#449781,#449782,#449783,#449784,#449785),.UNSPECIFIED.,.F.,.F.,
(4,1,1,1,1,1,1,4),(53.4070751110265,54.3236905706502,55.3217825250896,56.319874479529,
57.3179664339684,58.3160583884079,59.3141503428473,59.6902604182061),
 .UNSPECIFIED.);
#26799=B_SPLINE_CURVE_WITH_KNOTS('',3,(#449790,#449791,#449792,#449793,
#449794,#449795,#449796,#449797,#449798,#449799),.UNSPECIFIED.,.F.,.F.,
(4,1,1,1,1,1,1,4),(47.1238898038469,47.7721612284846,48.770253182924,49.7683451373634,
50.7664370918028,51.7645290462422,52.7626210006817,53.4070751110265),
 .UNSPECIFIED.);
#26800=B_SPLINE_CURVE_WITH_KNOTS('',3,(#449800,#449801,#449802,#449803,
#449804,#449805,#449806,#449807,#449808,#449809,#449810),.UNSPECIFIED.,
 .F.,.F.,(4,1,1,1,1,1,1,1,4),(47.1238898038469,47.3370468895742,48.3351388440137,
49.3332307984531,50.3313227528925,51.3294147073319,52.3275066617713,53.3255986162108,
53.4070751110265),.UNSPECIFIED.);
#26801=B_SPLINE_CURVE_WITH_KNOTS('',3,(#449815,#449816,#449817,#449818,
#449819,#449820,#449821,#449822,#449823,#449824),.UNSPECIFIED.,.F.,.F.,
(4,1,1,1,1,1,1,4),(40.8407044966673,41.783609501848,42.7817014562875,43.7797934107269,
44.7778853651663,45.7759773196057,46.7740692740451,47.1238898038469),
 .UNSPECIFIED.);
#26802=B_SPLINE_CURVE_WITH_KNOTS('',3,(#449825,#449826,#449827,#449828,
#449829,#449830,#449831,#449832,#449833,#449834),.UNSPECIFIED.,.F.,.F.,
(4,1,1,1,1,1,1,4),(40.8407044966673,41.3484951629377,42.3465871173771,43.3446790718166,
44.342771026256,45.3408629806954,46.3389549351348,47.1238898038469),
 .UNSPECIFIED.);
#26803=B_SPLINE_CURVE_WITH_KNOTS('',3,(#449839,#449840,#449841,#449842,
#449843,#449844,#449845,#449846,#449847,#449848,#449849),.UNSPECIFIED.,
 .F.,.F.,(4,1,1,1,1,1,1,1,4),(34.5575191894877,34.7969658207721,35.7950577752115,
36.7931497296509,37.7912416840904,38.7893336385298,39.7874255929692,40.7855175474086,
40.8407044966673),.UNSPECIFIED.);
#26804=B_SPLINE_CURVE_WITH_KNOTS('',3,(#449850,#449851,#449852,#449853,
#449854,#449855,#449856,#449857,#449858,#449859),.UNSPECIFIED.,.F.,.F.,
(4,1,1,1,1,1,1,4),(34.5575191894877,35.3599434363012,36.3580353907406,37.35612734518,
38.3542192996195,39.3523112540589,40.3504032084983,40.8407044966673),
 .UNSPECIFIED.);
#26805=B_SPLINE_CURVE_WITH_KNOTS('',3,(#449864,#449865,#449866,#449867,
#449868,#449869,#449870,#449871,#449872,#449873),.UNSPECIFIED.,.F.,.F.,
(4,1,1,1,1,1,1,4),(28.2743338823081,28.8084140941356,29.806506048575,30.8045980030144,
31.8026899574538,32.8007819118933,33.7988738663327,34.5575191894877),
 .UNSPECIFIED.);
#26806=B_SPLINE_CURVE_WITH_KNOTS('',3,(#449874,#449875,#449876,#449877,
#449878,#449879,#449880,#449881,#449882,#449883,#449884),.UNSPECIFIED.,
 .F.,.F.,(4,1,1,1,1,1,1,1,4),(28.2743338823081,28.3732997552253,29.3713917096647,
30.3694836641041,31.3675756185435,32.3656675729829,33.3637595274224,34.3618514818618,
34.5575191894877),.UNSPECIFIED.);
#26807=B_SPLINE_CURVE_WITH_KNOTS('',3,(#449889,#449890,#449891,#449892,
#449893,#449894,#449895,#449896,#449897,#449898),.UNSPECIFIED.,.F.,.F.,
(4,1,1,1,1,1,1,4),(21.9911485751285,22.8198623674991,23.8179543219385,24.8160462763779,
25.8141382308173,26.8122301852567,27.8103221396962,28.2743338823081),
 .UNSPECIFIED.);
#26808=B_SPLINE_CURVE_WITH_KNOTS('',3,(#449899,#449900,#449901,#449902,
#449903,#449904,#449905,#449906,#449907,#449908),.UNSPECIFIED.,.F.,.F.,
(4,1,1,1,1,1,1,4),(21.9911485751285,22.3847480285887,23.3828399830282,24.3809319374676,
25.379023891907,26.3771158463464,27.3752078007858,28.2743338823081),
 .UNSPECIFIED.);
#26809=B_SPLINE_CURVE_WITH_KNOTS('',3,(#449914,#449915,#449916,#449917,
#449918),.UNSPECIFIED.,.F.,.F.,(4,1,4),(14.4000123930734,15.3981043475128,
15.7079632679489),.UNSPECIFIED.);
#26810=B_SPLINE_CURVE_WITH_KNOTS('',3,(#449921,#449922,#449923,#449924,
#449925),.UNSPECIFIED.,.F.,.F.,(4,1,4),(13.8743214892347,14.8351267319837,
15.7079632679489),.UNSPECIFIED.);
#26811=B_SPLINE_CURVE_WITH_KNOTS('',3,(#449932,#449933,#449934,#449935,
#449936,#449937,#449938),.UNSPECIFIED.,.F.,.F.,(4,3,4),(-48.8692190558412,
-47.9084138130922,-47.8494095495406),.UNSPECIFIED.);
#26812=B_SPLINE_CURVE_WITH_KNOTS('',3,(#449944,#449945,#449946,#449947,
#449948,#449949,#449950,#449951,#449952,#449953,#449954,#449955,#449956,
#449957,#449958,#449959,#449960,#449961,#449962),.UNSPECIFIED.,.F.,.F.,
(4,3,3,3,3,3,4),(45.2902480251326,45.9122299042133,46.9103218586527,47.9084138130921,
48.9065057675316,49.904597721971,50.9026896764104),.UNSPECIFIED.);
#26813=B_SPLINE_CURVE_WITH_KNOTS('',3,(#449964,#449965,#449966,#449967,
#449968,#449969,#449970,#449971,#449972,#449973,#449974,#449975,#449976,
#449977,#449978,#449979,#449980,#449981,#449982,#449983,#449984,#449985),
 .UNSPECIFIED.,.F.,.F.,(4,3,3,3,3,3,3,4),(-47.8494095495406,-46.9103218586527,
-45.9122299042133,-44.9141379497739,-43.9160459953345,-42.9179540408951,
-41.9198620864556,-41.5662242423611),.UNSPECIFIED.);
#26814=B_SPLINE_CURVE_WITH_KNOTS('',3,(#449990,#449991,#449992,#449993,
#449994,#449995,#449996,#449997,#449998,#449999,#450000,#450001,#450002,
#450003,#450004,#450005,#450006,#450007,#450008,#450009,#450010,#450011),
 .UNSPECIFIED.,.F.,.F.,(4,3,3,3,3,3,3,4),(39.007062717953,39.9236781775768,
40.9217701320162,41.9198620864556,42.917954040895,43.9160459953345,44.9141379497739,
45.2902480251326),.UNSPECIFIED.);
#26815=B_SPLINE_CURVE_WITH_KNOTS('',3,(#450012,#450013,#450014,#450015,
#450016,#450017,#450018,#450019,#450020,#450021,#450022,#450023,#450024,
#450025,#450026,#450027,#450028,#450029,#450030,#450031,#450032,#450033),
 .UNSPECIFIED.,.F.,.F.,(4,3,3,3,3,3,3,4),(-41.5662242423611,-40.9217701320162,
-39.9236781775768,-38.9255862231374,-37.927494268698,-36.9294023142585,
-35.9313103598191,-35.2830389351814),.UNSPECIFIED.);
#26816=B_SPLINE_CURVE_WITH_KNOTS('',3,(#450038,#450039,#450040,#450041,
#450042,#450043,#450044,#450045,#450046,#450047,#450048,#450049,#450050,
#450051,#450052,#450053,#450054,#450055,#450056,#450057,#450058,#450059,
#450060,#450061,#450062),.UNSPECIFIED.,.F.,.F.,(4,3,3,3,3,3,3,3,4),(32.7238774107735,
32.9370344965008,33.9351264509403,34.9332184053797,35.9313103598191,36.9294023142585,
37.9274942686979,38.9255862231374,39.007062717953),.UNSPECIFIED.);
#26817=B_SPLINE_CURVE_WITH_KNOTS('',3,(#450063,#450064,#450065,#450066,
#450067,#450068,#450069,#450070,#450071,#450072,#450073,#450074,#450075,
#450076,#450077,#450078,#450079,#450080,#450081,#450082,#450083,#450084),
 .UNSPECIFIED.,.F.,.F.,(4,3,3,3,3,3,3,4),(-35.2830389351814,-34.9332184053797,
-33.9351264509403,-32.9370344965009,-31.9389425420614,-30.940850587622,
-29.9427586331826,-28.9998536280018),.UNSPECIFIED.);
#26818=B_SPLINE_CURVE_WITH_KNOTS('',3,(#450089,#450090,#450091,#450092,
#450093,#450094,#450095,#450096,#450097,#450098,#450099,#450100,#450101,
#450102,#450103,#450104,#450105,#450106,#450107,#450108,#450109,#450110),
 .UNSPECIFIED.,.F.,.F.,(4,3,3,3,3,3,3,4),(26.4406921035939,26.9484827698643,
27.9465747243037,28.9446666787432,29.9427586331826,30.940850587622,31.9389425420614,
32.7238774107735),.UNSPECIFIED.);
#26819=B_SPLINE_CURVE_WITH_KNOTS('',3,(#450111,#450112,#450113,#450114,
#450115,#450116,#450117,#450118,#450119,#450120,#450121,#450122,#450123,
#450124,#450125,#450126,#450127,#450128,#450129,#450130,#450131,#450132,
#450133,#450134,#450135),.UNSPECIFIED.,.F.,.F.,(4,3,3,3,3,3,3,3,4),(-28.9998536280018,
-28.9446666787432,-27.9465747243038,-26.9484827698643,-25.9503908154249,
-24.9522988609855,-23.9542069065461,-22.9561149521067,-22.7166683208223),
 .UNSPECIFIED.);
#26820=B_SPLINE_CURVE_WITH_KNOTS('',3,(#450140,#450141,#450142,#450143,
#450144,#450145,#450146,#450147,#450148,#450149,#450150,#450151,#450152,
#450153,#450154,#450155,#450156,#450157,#450158,#450159,#450160,#450161),
 .UNSPECIFIED.,.F.,.F.,(4,3,3,3,3,3,3,4),(20.1575067964143,20.9599310432278,
21.9580229976672,22.9561149521067,23.9542069065461,24.9522988609855,25.9503908154249,
26.4406921035939),.UNSPECIFIED.);
#26821=B_SPLINE_CURVE_WITH_KNOTS('',3,(#450162,#450163,#450164,#450165,
#450166,#450167,#450168,#450169,#450170,#450171,#450172,#450173,#450174,
#450175,#450176,#450177,#450178,#450179,#450180,#450181,#450182,#450183),
 .UNSPECIFIED.,.F.,.F.,(4,3,3,3,3,3,3,4),(-22.7166683208223,-21.9580229976672,
-20.9599310432278,-19.9618390887884,-18.963747134349,-17.9656551799096,
-16.9675632254701,-16.4334830136427),.UNSPECIFIED.);
#26822=B_SPLINE_CURVE_WITH_KNOTS('',3,(#450188,#450189,#450190,#450191,
#450192,#450193,#450194,#450195,#450196,#450197,#450198,#450199,#450200,
#450201,#450202,#450203,#450204,#450205,#450206,#450207,#450208,#450209,
#450210,#450211,#450212),.UNSPECIFIED.,.F.,.F.,(4,3,3,3,3,3,3,3,4),(13.8743214892347,
13.9732873621519,14.9713793165913,15.9694712710307,16.9675632254701,17.9656551799096,
18.963747134349,19.9618390887884,20.1575067964143),.UNSPECIFIED.);
#26823=B_SPLINE_CURVE_WITH_KNOTS('',3,(#450213,#450214,#450215,#450216,
#450217,#450218,#450219,#450220,#450221,#450222,#450223,#450224,#450225,
#450226,#450227,#450228,#450229,#450230,#450231,#450232,#450233,#450234),
 .UNSPECIFIED.,.F.,.F.,(4,3,3,3,3,3,3,4),(-16.4334830136427,-15.9694712710307,
-14.9713793165913,-13.9732873621519,-12.9751954077125,-11.977103453273,
-10.9790114988336,-10.1502977064631),.UNSPECIFIED.);
#26824=B_SPLINE_CURVE_WITH_KNOTS('',3,(#450240,#450241,#450242,#450243,
#450244,#450245,#450246,#450247,#450248,#450249,#450250,#450251,#450252),
 .UNSPECIFIED.,.F.,.F.,(4,3,3,3,4),(-3.86711239928348,-2.99427586331826,
-1.99618390887884,-0.998091954439421,0.),.UNSPECIFIED.);
#26825=B_SPLINE_CURVE_WITH_KNOTS('',3,(#450255,#450256,#450257,#450258,
#450259,#450260,#450261,#450262,#450263,#450264,#450265,#450266,#450267,
#450268,#450269,#450270,#450271,#450272,#450273),.UNSPECIFIED.,.F.,.F.,
(4,3,3,3,3,3,4),(2.03347062056922,2.99427586331826,3.99236781775768,4.9904597721971,
5.98855172663652,6.98664368107594,7.59113618205511),.UNSPECIFIED.);
#26826=B_SPLINE_CURVE_WITH_KNOTS('',3,(#450279,#450280,#450281,#450282,
#450283,#450284,#450285),.UNSPECIFIED.,.F.,.F.,(4,1,1,1,4),(59.6902604182061,
59.7492646817576,60.747356636197,61.7454485906364,62.7435405450759),
 .UNSPECIFIED.);
#26827=B_SPLINE_CURVE_WITH_KNOTS('',3,(#450288,#450289,#450290,#450291,
#450292,#450293,#450294),.UNSPECIFIED.,.F.,.F.,(4,1,1,1,4),(59.6902604182061,
60.3122422972867,61.3103342517261,62.3084262061655,63.2692314489146),
 .UNSPECIFIED.);
#26828=B_SPLINE_CURVE_WITH_KNOTS('',3,(#450299,#450300,#450301,#450302,
#450303,#450304,#450305,#450306,#450307,#450308),.UNSPECIFIED.,.F.,.F.,
(4,1,1,1,1,1,1,4),(53.4070751110265,53.7607129551211,54.7588049095605,55.7568968639999,
56.7549888184393,57.7530807728788,58.7511727273182,59.6902604182061),
 .UNSPECIFIED.);
#26829=B_SPLINE_CURVE_WITH_KNOTS('',3,(#450309,#450310,#450311,#450312,
#450313,#450314,#450315,#450316,#450317,#450318),.UNSPECIFIED.,.F.,.F.,
(4,1,1,1,1,1,1,4),(53.4070751110265,54.3236905706502,55.3217825250896,56.319874479529,
57.3179664339684,58.3160583884079,59.3141503428473,59.6902604182061),
 .UNSPECIFIED.);
#26830=B_SPLINE_CURVE_WITH_KNOTS('',3,(#450323,#450324,#450325,#450326,
#450327,#450328,#450329,#450330,#450331,#450332),.UNSPECIFIED.,.F.,.F.,
(4,1,1,1,1,1,1,4),(47.1238898038469,47.7721612284846,48.770253182924,49.7683451373634,
50.7664370918028,51.7645290462422,52.7626210006817,53.4070751110265),
 .UNSPECIFIED.);
#26831=B_SPLINE_CURVE_WITH_KNOTS('',3,(#450333,#450334,#450335,#450336,
#450337,#450338,#450339,#450340,#450341,#450342,#450343),.UNSPECIFIED.,
 .F.,.F.,(4,1,1,1,1,1,1,1,4),(47.1238898038469,47.3370468895742,48.3351388440137,
49.3332307984531,50.3313227528925,51.3294147073319,52.3275066617713,53.3255986162108,
53.4070751110265),.UNSPECIFIED.);
#26832=B_SPLINE_CURVE_WITH_KNOTS('',3,(#450348,#450349,#450350,#450351,
#450352,#450353,#450354,#450355,#450356,#450357),.UNSPECIFIED.,.F.,.F.,
(4,1,1,1,1,1,1,4),(40.8407044966673,41.783609501848,42.7817014562875,43.7797934107269,
44.7778853651663,45.7759773196057,46.7740692740451,47.1238898038469),
 .UNSPECIFIED.);
#26833=B_SPLINE_CURVE_WITH_KNOTS('',3,(#450358,#450359,#450360,#450361,
#450362,#450363,#450364,#450365,#450366,#450367),.UNSPECIFIED.,.F.,.F.,
(4,1,1,1,1,1,1,4),(40.8407044966673,41.3484951629377,42.3465871173771,43.3446790718166,
44.342771026256,45.3408629806954,46.3389549351348,47.1238898038469),
 .UNSPECIFIED.);
#26834=B_SPLINE_CURVE_WITH_KNOTS('',3,(#450372,#450373,#450374,#450375,
#450376,#450377,#450378,#450379,#450380,#450381,#450382),.UNSPECIFIED.,
 .F.,.F.,(4,1,1,1,1,1,1,1,4),(34.5575191894877,34.7969658207721,35.7950577752115,
36.7931497296509,37.7912416840904,38.7893336385298,39.7874255929692,40.7855175474086,
40.8407044966673),.UNSPECIFIED.);
#26835=B_SPLINE_CURVE_WITH_KNOTS('',3,(#450383,#450384,#450385,#450386,
#450387,#450388,#450389,#450390,#450391,#450392),.UNSPECIFIED.,.F.,.F.,
(4,1,1,1,1,1,1,4),(34.5575191894877,35.3599434363012,36.3580353907406,37.35612734518,
38.3542192996195,39.3523112540589,40.3504032084983,40.8407044966673),
 .UNSPECIFIED.);
#26836=B_SPLINE_CURVE_WITH_KNOTS('',3,(#450397,#450398,#450399,#450400,
#450401,#450402,#450403,#450404,#450405,#450406),.UNSPECIFIED.,.F.,.F.,
(4,1,1,1,1,1,1,4),(28.2743338823081,28.8084140941356,29.806506048575,30.8045980030144,
31.8026899574538,32.8007819118933,33.7988738663327,34.5575191894877),
 .UNSPECIFIED.);
#26837=B_SPLINE_CURVE_WITH_KNOTS('',3,(#450407,#450408,#450409,#450410,
#450411,#450412,#450413,#450414,#450415,#450416,#450417),.UNSPECIFIED.,
 .F.,.F.,(4,1,1,1,1,1,1,1,4),(28.2743338823081,28.3732997552253,29.3713917096647,
30.3694836641041,31.3675756185435,32.3656675729829,33.3637595274224,34.3618514818618,
34.5575191894877),.UNSPECIFIED.);
#26838=B_SPLINE_CURVE_WITH_KNOTS('',3,(#450422,#450423,#450424,#450425,
#450426,#450427,#450428,#450429,#450430,#450431),.UNSPECIFIED.,.F.,.F.,
(4,1,1,1,1,1,1,4),(21.9911485751285,22.8198623674991,23.8179543219385,24.8160462763779,
25.8141382308173,26.8122301852567,27.8103221396962,28.2743338823081),
 .UNSPECIFIED.);
#26839=B_SPLINE_CURVE_WITH_KNOTS('',3,(#450432,#450433,#450434,#450435,
#450436,#450437,#450438,#450439,#450440,#450441),.UNSPECIFIED.,.F.,.F.,
(4,1,1,1,1,1,1,4),(21.9911485751285,22.3847480285887,23.3828399830282,24.3809319374676,
25.379023891907,26.3771158463464,27.3752078007858,28.2743338823081),
 .UNSPECIFIED.);
#26840=B_SPLINE_CURVE_WITH_KNOTS('',3,(#450447,#450448,#450449,#450450,
#450451),.UNSPECIFIED.,.F.,.F.,(4,1,4),(14.4000123930734,15.3981043475128,
15.7079632679489),.UNSPECIFIED.);
#26841=B_SPLINE_CURVE_WITH_KNOTS('',3,(#450454,#450455,#450456,#450457,
#450458),.UNSPECIFIED.,.F.,.F.,(4,1,4),(13.8743214892347,14.8351267319837,
15.7079632679489),.UNSPECIFIED.);
#26842=B_SPLINE_CURVE_WITH_KNOTS('',3,(#450465,#450466,#450467,#450468,
#450469,#450470,#450471),.UNSPECIFIED.,.F.,.F.,(4,3,4),(-48.8692190558412,
-47.9084138130922,-47.8494095495406),.UNSPECIFIED.);
#26843=B_SPLINE_CURVE_WITH_KNOTS('',3,(#450477,#450478,#450479,#450480,
#450481,#450482,#450483,#450484,#450485,#450486,#450487,#450488,#450489,
#450490,#450491,#450492,#450493,#450494,#450495),.UNSPECIFIED.,.F.,.F.,
(4,3,3,3,3,3,4),(45.2902480251326,45.9122299042133,46.9103218586527,47.9084138130921,
48.9065057675316,49.904597721971,50.9026896764104),.UNSPECIFIED.);
#26844=B_SPLINE_CURVE_WITH_KNOTS('',3,(#450497,#450498,#450499,#450500,
#450501,#450502,#450503,#450504,#450505,#450506,#450507,#450508,#450509,
#450510,#450511,#450512,#450513,#450514,#450515,#450516,#450517,#450518),
 .UNSPECIFIED.,.F.,.F.,(4,3,3,3,3,3,3,4),(-47.8494095495406,-46.9103218586527,
-45.9122299042133,-44.9141379497739,-43.9160459953345,-42.9179540408951,
-41.9198620864556,-41.5662242423611),.UNSPECIFIED.);
#26845=B_SPLINE_CURVE_WITH_KNOTS('',3,(#450523,#450524,#450525,#450526,
#450527,#450528,#450529,#450530,#450531,#450532,#450533,#450534,#450535,
#450536,#450537,#450538,#450539,#450540,#450541,#450542,#450543,#450544),
 .UNSPECIFIED.,.F.,.F.,(4,3,3,3,3,3,3,4),(39.007062717953,39.9236781775768,
40.9217701320162,41.9198620864556,42.917954040895,43.9160459953345,44.9141379497739,
45.2902480251326),.UNSPECIFIED.);
#26846=B_SPLINE_CURVE_WITH_KNOTS('',3,(#450545,#450546,#450547,#450548,
#450549,#450550,#450551,#450552,#450553,#450554,#450555,#450556,#450557,
#450558,#450559,#450560,#450561,#450562,#450563,#450564,#450565,#450566),
 .UNSPECIFIED.,.F.,.F.,(4,3,3,3,3,3,3,4),(-41.5662242423611,-40.9217701320162,
-39.9236781775768,-38.9255862231374,-37.927494268698,-36.9294023142585,
-35.9313103598191,-35.2830389351814),.UNSPECIFIED.);
#26847=B_SPLINE_CURVE_WITH_KNOTS('',3,(#450571,#450572,#450573,#450574,
#450575,#450576,#450577,#450578,#450579,#450580,#450581,#450582,#450583,
#450584,#450585,#450586,#450587,#450588,#450589,#450590,#450591,#450592,
#450593,#450594,#450595),.UNSPECIFIED.,.F.,.F.,(4,3,3,3,3,3,3,3,4),(32.7238774107735,
32.9370344965008,33.9351264509403,34.9332184053797,35.9313103598191,36.9294023142585,
37.9274942686979,38.9255862231374,39.007062717953),.UNSPECIFIED.);
#26848=B_SPLINE_CURVE_WITH_KNOTS('',3,(#450596,#450597,#450598,#450599,
#450600,#450601,#450602,#450603,#450604,#450605,#450606,#450607,#450608,
#450609,#450610,#450611,#450612,#450613,#450614,#450615,#450616,#450617),
 .UNSPECIFIED.,.F.,.F.,(4,3,3,3,3,3,3,4),(-35.2830389351814,-34.9332184053797,
-33.9351264509403,-32.9370344965009,-31.9389425420614,-30.940850587622,
-29.9427586331826,-28.9998536280018),.UNSPECIFIED.);
#26849=B_SPLINE_CURVE_WITH_KNOTS('',3,(#450622,#450623,#450624,#450625,
#450626,#450627,#450628,#450629,#450630,#450631,#450632,#450633,#450634,
#450635,#450636,#450637,#450638,#450639,#450640,#450641,#450642,#450643),
 .UNSPECIFIED.,.F.,.F.,(4,3,3,3,3,3,3,4),(26.4406921035939,26.9484827698643,
27.9465747243037,28.9446666787432,29.9427586331826,30.940850587622,31.9389425420614,
32.7238774107735),.UNSPECIFIED.);
#26850=B_SPLINE_CURVE_WITH_KNOTS('',3,(#450644,#450645,#450646,#450647,
#450648,#450649,#450650,#450651,#450652,#450653,#450654,#450655,#450656,
#450657,#450658,#450659,#450660,#450661,#450662,#450663,#450664,#450665,
#450666,#450667,#450668),.UNSPECIFIED.,.F.,.F.,(4,3,3,3,3,3,3,3,4),(-28.9998536280018,
-28.9446666787432,-27.9465747243038,-26.9484827698643,-25.9503908154249,
-24.9522988609855,-23.9542069065461,-22.9561149521067,-22.7166683208223),
 .UNSPECIFIED.);
#26851=B_SPLINE_CURVE_WITH_KNOTS('',3,(#450673,#450674,#450675,#450676,
#450677,#450678,#450679,#450680,#450681,#450682,#450683,#450684,#450685,
#450686,#450687,#450688,#450689,#450690,#450691,#450692,#450693,#450694),
 .UNSPECIFIED.,.F.,.F.,(4,3,3,3,3,3,3,4),(20.1575067964143,20.9599310432278,
21.9580229976672,22.9561149521067,23.9542069065461,24.9522988609855,25.9503908154249,
26.4406921035939),.UNSPECIFIED.);
#26852=B_SPLINE_CURVE_WITH_KNOTS('',3,(#450695,#450696,#450697,#450698,
#450699,#450700,#450701,#450702,#450703,#450704,#450705,#450706,#450707,
#450708,#450709,#450710,#450711,#450712,#450713,#450714,#450715,#450716),
 .UNSPECIFIED.,.F.,.F.,(4,3,3,3,3,3,3,4),(-22.7166683208223,-21.9580229976672,
-20.9599310432278,-19.9618390887884,-18.963747134349,-17.9656551799096,
-16.9675632254701,-16.4334830136427),.UNSPECIFIED.);
#26853=B_SPLINE_CURVE_WITH_KNOTS('',3,(#450721,#450722,#450723,#450724,
#450725,#450726,#450727,#450728,#450729,#450730,#450731,#450732,#450733,
#450734,#450735,#450736,#450737,#450738,#450739,#450740,#450741,#450742,
#450743,#450744,#450745),.UNSPECIFIED.,.F.,.F.,(4,3,3,3,3,3,3,3,4),(13.8743214892347,
13.9732873621519,14.9713793165913,15.9694712710307,16.9675632254701,17.9656551799096,
18.963747134349,19.9618390887884,20.1575067964143),.UNSPECIFIED.);
#26854=B_SPLINE_CURVE_WITH_KNOTS('',3,(#450746,#450747,#450748,#450749,
#450750,#450751,#450752,#450753,#450754,#450755,#450756,#450757,#450758,
#450759,#450760,#450761,#450762,#450763,#450764,#450765,#450766,#450767),
 .UNSPECIFIED.,.F.,.F.,(4,3,3,3,3,3,3,4),(-16.4334830136427,-15.9694712710307,
-14.9713793165913,-13.9732873621519,-12.9751954077125,-11.977103453273,
-10.9790114988336,-10.1502977064631),.UNSPECIFIED.);
#26855=B_SPLINE_CURVE_WITH_KNOTS('',3,(#450773,#450774,#450775,#450776,
#450777,#450778,#450779,#450780,#450781,#450782,#450783,#450784,#450785),
 .UNSPECIFIED.,.F.,.F.,(4,3,3,3,4),(-3.86711239928348,-2.99427586331826,
-1.99618390887884,-0.998091954439421,0.),.UNSPECIFIED.);
#26856=B_SPLINE_CURVE_WITH_KNOTS('',3,(#450788,#450789,#450790,#450791,
#450792,#450793,#450794,#450795,#450796,#450797,#450798,#450799,#450800,
#450801,#450802,#450803,#450804,#450805,#450806),.UNSPECIFIED.,.F.,.F.,
(4,3,3,3,3,3,4),(2.03347062056922,2.99427586331826,3.99236781775768,4.9904597721971,
5.98855172663652,6.98664368107594,7.59113618205511),.UNSPECIFIED.);
#26857=B_SPLINE_CURVE_WITH_KNOTS('',3,(#450812,#450813,#450814,#450815,
#450816,#450817,#450818),.UNSPECIFIED.,.F.,.F.,(4,1,1,1,4),(59.6902604182061,
59.7492646817576,60.747356636197,61.7454485906364,62.7435405450759),
 .UNSPECIFIED.);
#26858=B_SPLINE_CURVE_WITH_KNOTS('',3,(#450821,#450822,#450823,#450824,
#450825,#450826,#450827),.UNSPECIFIED.,.F.,.F.,(4,1,1,1,4),(59.6902604182061,
60.3122422972867,61.3103342517261,62.3084262061655,63.2692314489146),
 .UNSPECIFIED.);
#26859=B_SPLINE_CURVE_WITH_KNOTS('',3,(#450832,#450833,#450834,#450835,
#450836,#450837,#450838,#450839,#450840,#450841),.UNSPECIFIED.,.F.,.F.,
(4,1,1,1,1,1,1,4),(53.4070751110265,53.7607129551211,54.7588049095605,55.7568968639999,
56.7549888184393,57.7530807728788,58.7511727273182,59.6902604182061),
 .UNSPECIFIED.);
#26860=B_SPLINE_CURVE_WITH_KNOTS('',3,(#450842,#450843,#450844,#450845,
#450846,#450847,#450848,#450849,#450850,#450851),.UNSPECIFIED.,.F.,.F.,
(4,1,1,1,1,1,1,4),(53.4070751110265,54.3236905706502,55.3217825250896,56.319874479529,
57.3179664339684,58.3160583884079,59.3141503428473,59.6902604182061),
 .UNSPECIFIED.);
#26861=B_SPLINE_CURVE_WITH_KNOTS('',3,(#450856,#450857,#450858,#450859,
#450860,#450861,#450862,#450863,#450864,#450865),.UNSPECIFIED.,.F.,.F.,
(4,1,1,1,1,1,1,4),(47.1238898038469,47.7721612284846,48.770253182924,49.7683451373634,
50.7664370918028,51.7645290462422,52.7626210006817,53.4070751110265),
 .UNSPECIFIED.);
#26862=B_SPLINE_CURVE_WITH_KNOTS('',3,(#450866,#450867,#450868,#450869,
#450870,#450871,#450872,#450873,#450874,#450875,#450876),.UNSPECIFIED.,
 .F.,.F.,(4,1,1,1,1,1,1,1,4),(47.1238898038469,47.3370468895742,48.3351388440137,
49.3332307984531,50.3313227528925,51.3294147073319,52.3275066617713,53.3255986162108,
53.4070751110265),.UNSPECIFIED.);
#26863=B_SPLINE_CURVE_WITH_KNOTS('',3,(#450881,#450882,#450883,#450884,
#450885,#450886,#450887,#450888,#450889,#450890),.UNSPECIFIED.,.F.,.F.,
(4,1,1,1,1,1,1,4),(40.8407044966673,41.783609501848,42.7817014562875,43.7797934107269,
44.7778853651663,45.7759773196057,46.7740692740451,47.1238898038469),
 .UNSPECIFIED.);
#26864=B_SPLINE_CURVE_WITH_KNOTS('',3,(#450891,#450892,#450893,#450894,
#450895,#450896,#450897,#450898,#450899,#450900),.UNSPECIFIED.,.F.,.F.,
(4,1,1,1,1,1,1,4),(40.8407044966673,41.3484951629377,42.3465871173771,43.3446790718166,
44.342771026256,45.3408629806954,46.3389549351348,47.1238898038469),
 .UNSPECIFIED.);
#26865=B_SPLINE_CURVE_WITH_KNOTS('',3,(#450905,#450906,#450907,#450908,
#450909,#450910,#450911,#450912,#450913,#450914,#450915),.UNSPECIFIED.,
 .F.,.F.,(4,1,1,1,1,1,1,1,4),(34.5575191894877,34.7969658207721,35.7950577752115,
36.7931497296509,37.7912416840904,38.7893336385298,39.7874255929692,40.7855175474086,
40.8407044966673),.UNSPECIFIED.);
#26866=B_SPLINE_CURVE_WITH_KNOTS('',3,(#450916,#450917,#450918,#450919,
#450920,#450921,#450922,#450923,#450924,#450925),.UNSPECIFIED.,.F.,.F.,
(4,1,1,1,1,1,1,4),(34.5575191894877,35.3599434363012,36.3580353907406,37.35612734518,
38.3542192996195,39.3523112540589,40.3504032084983,40.8407044966673),
 .UNSPECIFIED.);
#26867=B_SPLINE_CURVE_WITH_KNOTS('',3,(#450930,#450931,#450932,#450933,
#450934,#450935,#450936,#450937,#450938,#450939),.UNSPECIFIED.,.F.,.F.,
(4,1,1,1,1,1,1,4),(28.2743338823081,28.8084140941356,29.806506048575,30.8045980030144,
31.8026899574538,32.8007819118933,33.7988738663327,34.5575191894877),
 .UNSPECIFIED.);
#26868=B_SPLINE_CURVE_WITH_KNOTS('',3,(#450940,#450941,#450942,#450943,
#450944,#450945,#450946,#450947,#450948,#450949,#450950),.UNSPECIFIED.,
 .F.,.F.,(4,1,1,1,1,1,1,1,4),(28.2743338823081,28.3732997552253,29.3713917096647,
30.3694836641041,31.3675756185435,32.3656675729829,33.3637595274224,34.3618514818618,
34.5575191894877),.UNSPECIFIED.);
#26869=B_SPLINE_CURVE_WITH_KNOTS('',3,(#450955,#450956,#450957,#450958,
#450959,#450960,#450961,#450962,#450963,#450964),.UNSPECIFIED.,.F.,.F.,
(4,1,1,1,1,1,1,4),(21.9911485751285,22.8198623674991,23.8179543219385,24.8160462763779,
25.8141382308173,26.8122301852567,27.8103221396962,28.2743338823081),
 .UNSPECIFIED.);
#26870=B_SPLINE_CURVE_WITH_KNOTS('',3,(#450965,#450966,#450967,#450968,
#450969,#450970,#450971,#450972,#450973,#450974),.UNSPECIFIED.,.F.,.F.,
(4,1,1,1,1,1,1,4),(21.9911485751285,22.3847480285887,23.3828399830282,24.3809319374676,
25.379023891907,26.3771158463464,27.3752078007858,28.2743338823081),
 .UNSPECIFIED.);
#26871=B_SPLINE_CURVE_WITH_KNOTS('',3,(#450980,#450981,#450982,#450983,
#450984),.UNSPECIFIED.,.F.,.F.,(4,1,4),(14.4000123930734,15.3981043475128,
15.7079632679489),.UNSPECIFIED.);
#26872=B_SPLINE_CURVE_WITH_KNOTS('',3,(#450987,#450988,#450989,#450990,
#450991),.UNSPECIFIED.,.F.,.F.,(4,1,4),(13.8743214892347,14.8351267319837,
15.7079632679489),.UNSPECIFIED.);
#26873=B_SPLINE_CURVE_WITH_KNOTS('',3,(#450998,#450999,#451000,#451001,
#451002,#451003,#451004),.UNSPECIFIED.,.F.,.F.,(4,3,4),(-48.8692190558412,
-47.9084138130922,-47.8494095495406),.UNSPECIFIED.);
#26874=B_SPLINE_CURVE_WITH_KNOTS('',3,(#451010,#451011,#451012,#451013,
#451014,#451015,#451016,#451017,#451018,#451019,#451020,#451021,#451022,
#451023,#451024,#451025,#451026,#451027,#451028),.UNSPECIFIED.,.F.,.F.,
(4,3,3,3,3,3,4),(45.2902480251326,45.9122299042133,46.9103218586527,47.9084138130921,
48.9065057675316,49.904597721971,50.9026896764104),.UNSPECIFIED.);
#26875=B_SPLINE_CURVE_WITH_KNOTS('',3,(#451030,#451031,#451032,#451033,
#451034,#451035,#451036,#451037,#451038,#451039,#451040,#451041,#451042,
#451043,#451044,#451045,#451046,#451047,#451048,#451049,#451050,#451051),
 .UNSPECIFIED.,.F.,.F.,(4,3,3,3,3,3,3,4),(-47.8494095495406,-46.9103218586527,
-45.9122299042133,-44.9141379497739,-43.9160459953345,-42.9179540408951,
-41.9198620864556,-41.5662242423611),.UNSPECIFIED.);
#26876=B_SPLINE_CURVE_WITH_KNOTS('',3,(#451056,#451057,#451058,#451059,
#451060,#451061,#451062,#451063,#451064,#451065,#451066,#451067,#451068,
#451069,#451070,#451071,#451072,#451073,#451074,#451075,#451076,#451077),
 .UNSPECIFIED.,.F.,.F.,(4,3,3,3,3,3,3,4),(39.007062717953,39.9236781775768,
40.9217701320162,41.9198620864556,42.917954040895,43.9160459953345,44.9141379497739,
45.2902480251326),.UNSPECIFIED.);
#26877=B_SPLINE_CURVE_WITH_KNOTS('',3,(#451078,#451079,#451080,#451081,
#451082,#451083,#451084,#451085,#451086,#451087,#451088,#451089,#451090,
#451091,#451092,#451093,#451094,#451095,#451096,#451097,#451098,#451099),
 .UNSPECIFIED.,.F.,.F.,(4,3,3,3,3,3,3,4),(-41.5662242423611,-40.9217701320162,
-39.9236781775768,-38.9255862231374,-37.927494268698,-36.9294023142585,
-35.9313103598191,-35.2830389351814),.UNSPECIFIED.);
#26878=B_SPLINE_CURVE_WITH_KNOTS('',3,(#451104,#451105,#451106,#451107,
#451108,#451109,#451110,#451111,#451112,#451113,#451114,#451115,#451116,
#451117,#451118,#451119,#451120,#451121,#451122,#451123,#451124,#451125,
#451126,#451127,#451128),.UNSPECIFIED.,.F.,.F.,(4,3,3,3,3,3,3,3,4),(32.7238774107735,
32.9370344965008,33.9351264509403,34.9332184053797,35.9313103598191,36.9294023142585,
37.9274942686979,38.9255862231374,39.007062717953),.UNSPECIFIED.);
#26879=B_SPLINE_CURVE_WITH_KNOTS('',3,(#451129,#451130,#451131,#451132,
#451133,#451134,#451135,#451136,#451137,#451138,#451139,#451140,#451141,
#451142,#451143,#451144,#451145,#451146,#451147,#451148,#451149,#451150),
 .UNSPECIFIED.,.F.,.F.,(4,3,3,3,3,3,3,4),(-35.2830389351814,-34.9332184053797,
-33.9351264509403,-32.9370344965009,-31.9389425420614,-30.940850587622,
-29.9427586331826,-28.9998536280018),.UNSPECIFIED.);
#26880=B_SPLINE_CURVE_WITH_KNOTS('',3,(#451155,#451156,#451157,#451158,
#451159,#451160,#451161,#451162,#451163,#451164,#451165,#451166,#451167,
#451168,#451169,#451170,#451171,#451172,#451173,#451174,#451175,#451176),
 .UNSPECIFIED.,.F.,.F.,(4,3,3,3,3,3,3,4),(26.4406921035939,26.9484827698643,
27.9465747243037,28.9446666787432,29.9427586331826,30.940850587622,31.9389425420614,
32.7238774107735),.UNSPECIFIED.);
#26881=B_SPLINE_CURVE_WITH_KNOTS('',3,(#451177,#451178,#451179,#451180,
#451181,#451182,#451183,#451184,#451185,#451186,#451187,#451188,#451189,
#451190,#451191,#451192,#451193,#451194,#451195,#451196,#451197,#451198,
#451199,#451200,#451201),.UNSPECIFIED.,.F.,.F.,(4,3,3,3,3,3,3,3,4),(-28.9998536280018,
-28.9446666787432,-27.9465747243038,-26.9484827698643,-25.9503908154249,
-24.9522988609855,-23.9542069065461,-22.9561149521067,-22.7166683208223),
 .UNSPECIFIED.);
#26882=B_SPLINE_CURVE_WITH_KNOTS('',3,(#451206,#451207,#451208,#451209,
#451210,#451211,#451212,#451213,#451214,#451215,#451216,#451217,#451218,
#451219,#451220,#451221,#451222,#451223,#451224,#451225,#451226,#451227),
 .UNSPECIFIED.,.F.,.F.,(4,3,3,3,3,3,3,4),(20.1575067964143,20.9599310432278,
21.9580229976672,22.9561149521067,23.9542069065461,24.9522988609855,25.9503908154249,
26.4406921035939),.UNSPECIFIED.);
#26883=B_SPLINE_CURVE_WITH_KNOTS('',3,(#451228,#451229,#451230,#451231,
#451232,#451233,#451234,#451235,#451236,#451237,#451238,#451239,#451240,
#451241,#451242,#451243,#451244,#451245,#451246,#451247,#451248,#451249),
 .UNSPECIFIED.,.F.,.F.,(4,3,3,3,3,3,3,4),(-22.7166683208223,-21.9580229976672,
-20.9599310432278,-19.9618390887884,-18.963747134349,-17.9656551799096,
-16.9675632254701,-16.4334830136427),.UNSPECIFIED.);
#26884=B_SPLINE_CURVE_WITH_KNOTS('',3,(#451254,#451255,#451256,#451257,
#451258,#451259,#451260,#451261,#451262,#451263,#451264,#451265,#451266,
#451267,#451268,#451269,#451270,#451271,#451272,#451273,#451274,#451275,
#451276,#451277,#451278),.UNSPECIFIED.,.F.,.F.,(4,3,3,3,3,3,3,3,4),(13.8743214892347,
13.9732873621519,14.9713793165913,15.9694712710307,16.9675632254701,17.9656551799096,
18.963747134349,19.9618390887884,20.1575067964143),.UNSPECIFIED.);
#26885=B_SPLINE_CURVE_WITH_KNOTS('',3,(#451279,#451280,#451281,#451282,
#451283,#451284,#451285,#451286,#451287,#451288,#451289,#451290,#451291,
#451292,#451293,#451294,#451295,#451296,#451297,#451298,#451299,#451300),
 .UNSPECIFIED.,.F.,.F.,(4,3,3,3,3,3,3,4),(-16.4334830136427,-15.9694712710307,
-14.9713793165913,-13.9732873621519,-12.9751954077125,-11.977103453273,
-10.9790114988336,-10.1502977064631),.UNSPECIFIED.);
#26886=B_SPLINE_CURVE_WITH_KNOTS('',3,(#451306,#451307,#451308,#451309,
#451310,#451311,#451312,#451313,#451314,#451315,#451316,#451317,#451318),
 .UNSPECIFIED.,.F.,.F.,(4,3,3,3,4),(-3.86711239928348,-2.99427586331826,
-1.99618390887884,-0.998091954439421,0.),.UNSPECIFIED.);
#26887=B_SPLINE_CURVE_WITH_KNOTS('',3,(#451321,#451322,#451323,#451324,
#451325,#451326,#451327,#451328,#451329,#451330,#451331,#451332,#451333,
#451334,#451335,#451336,#451337,#451338,#451339),.UNSPECIFIED.,.F.,.F.,
(4,3,3,3,3,3,4),(2.03347062056922,2.99427586331826,3.99236781775768,4.9904597721971,
5.98855172663652,6.98664368107594,7.59113618205511),.UNSPECIFIED.);
#26888=B_SPLINE_CURVE_WITH_KNOTS('',3,(#451345,#451346,#451347,#451348,
#451349,#451350,#451351),.UNSPECIFIED.,.F.,.F.,(4,1,1,1,4),(59.6902604182061,
59.7492646817576,60.747356636197,61.7454485906364,62.7435405450759),
 .UNSPECIFIED.);
#26889=B_SPLINE_CURVE_WITH_KNOTS('',3,(#451354,#451355,#451356,#451357,
#451358,#451359,#451360),.UNSPECIFIED.,.F.,.F.,(4,1,1,1,4),(59.6902604182061,
60.3122422972867,61.3103342517261,62.3084262061655,63.2692314489146),
 .UNSPECIFIED.);
#26890=B_SPLINE_CURVE_WITH_KNOTS('',3,(#451365,#451366,#451367,#451368,
#451369,#451370,#451371,#451372,#451373,#451374),.UNSPECIFIED.,.F.,.F.,
(4,1,1,1,1,1,1,4),(53.4070751110265,53.7607129551211,54.7588049095605,55.7568968639999,
56.7549888184393,57.7530807728788,58.7511727273182,59.6902604182061),
 .UNSPECIFIED.);
#26891=B_SPLINE_CURVE_WITH_KNOTS('',3,(#451375,#451376,#451377,#451378,
#451379,#451380,#451381,#451382,#451383,#451384),.UNSPECIFIED.,.F.,.F.,
(4,1,1,1,1,1,1,4),(53.4070751110265,54.3236905706502,55.3217825250896,56.319874479529,
57.3179664339684,58.3160583884079,59.3141503428473,59.6902604182061),
 .UNSPECIFIED.);
#26892=B_SPLINE_CURVE_WITH_KNOTS('',3,(#451389,#451390,#451391,#451392,
#451393,#451394,#451395,#451396,#451397,#451398),.UNSPECIFIED.,.F.,.F.,
(4,1,1,1,1,1,1,4),(47.1238898038469,47.7721612284846,48.770253182924,49.7683451373634,
50.7664370918028,51.7645290462422,52.7626210006817,53.4070751110265),
 .UNSPECIFIED.);
#26893=B_SPLINE_CURVE_WITH_KNOTS('',3,(#451399,#451400,#451401,#451402,
#451403,#451404,#451405,#451406,#451407,#451408,#451409),.UNSPECIFIED.,
 .F.,.F.,(4,1,1,1,1,1,1,1,4),(47.1238898038469,47.3370468895742,48.3351388440137,
49.3332307984531,50.3313227528925,51.3294147073319,52.3275066617713,53.3255986162108,
53.4070751110265),.UNSPECIFIED.);
#26894=B_SPLINE_CURVE_WITH_KNOTS('',3,(#451414,#451415,#451416,#451417,
#451418,#451419,#451420,#451421,#451422,#451423),.UNSPECIFIED.,.F.,.F.,
(4,1,1,1,1,1,1,4),(40.8407044966673,41.783609501848,42.7817014562875,43.7797934107269,
44.7778853651663,45.7759773196057,46.7740692740451,47.1238898038469),
 .UNSPECIFIED.);
#26895=B_SPLINE_CURVE_WITH_KNOTS('',3,(#451424,#451425,#451426,#451427,
#451428,#451429,#451430,#451431,#451432,#451433),.UNSPECIFIED.,.F.,.F.,
(4,1,1,1,1,1,1,4),(40.8407044966673,41.3484951629377,42.3465871173771,43.3446790718166,
44.342771026256,45.3408629806954,46.3389549351348,47.1238898038469),
 .UNSPECIFIED.);
#26896=B_SPLINE_CURVE_WITH_KNOTS('',3,(#451438,#451439,#451440,#451441,
#451442,#451443,#451444,#451445,#451446,#451447,#451448),.UNSPECIFIED.,
 .F.,.F.,(4,1,1,1,1,1,1,1,4),(34.5575191894877,34.7969658207721,35.7950577752115,
36.7931497296509,37.7912416840904,38.7893336385298,39.7874255929692,40.7855175474086,
40.8407044966673),.UNSPECIFIED.);
#26897=B_SPLINE_CURVE_WITH_KNOTS('',3,(#451449,#451450,#451451,#451452,
#451453,#451454,#451455,#451456,#451457,#451458),.UNSPECIFIED.,.F.,.F.,
(4,1,1,1,1,1,1,4),(34.5575191894877,35.3599434363012,36.3580353907406,37.35612734518,
38.3542192996195,39.3523112540589,40.3504032084983,40.8407044966673),
 .UNSPECIFIED.);
#26898=B_SPLINE_CURVE_WITH_KNOTS('',3,(#451463,#451464,#451465,#451466,
#451467,#451468,#451469,#451470,#451471,#451472),.UNSPECIFIED.,.F.,.F.,
(4,1,1,1,1,1,1,4),(28.2743338823081,28.8084140941356,29.806506048575,30.8045980030144,
31.8026899574538,32.8007819118933,33.7988738663327,34.5575191894877),
 .UNSPECIFIED.);
#26899=B_SPLINE_CURVE_WITH_KNOTS('',3,(#451473,#451474,#451475,#451476,
#451477,#451478,#451479,#451480,#451481,#451482,#451483),.UNSPECIFIED.,
 .F.,.F.,(4,1,1,1,1,1,1,1,4),(28.2743338823081,28.3732997552253,29.3713917096647,
30.3694836641041,31.3675756185435,32.3656675729829,33.3637595274224,34.3618514818618,
34.5575191894877),.UNSPECIFIED.);
#26900=B_SPLINE_CURVE_WITH_KNOTS('',3,(#451488,#451489,#451490,#451491,
#451492,#451493,#451494,#451495,#451496,#451497),.UNSPECIFIED.,.F.,.F.,
(4,1,1,1,1,1,1,4),(21.9911485751285,22.8198623674991,23.8179543219385,24.8160462763779,
25.8141382308173,26.8122301852567,27.8103221396962,28.2743338823081),
 .UNSPECIFIED.);
#26901=B_SPLINE_CURVE_WITH_KNOTS('',3,(#451498,#451499,#451500,#451501,
#451502,#451503,#451504,#451505,#451506,#451507),.UNSPECIFIED.,.F.,.F.,
(4,1,1,1,1,1,1,4),(21.9911485751285,22.3847480285887,23.3828399830282,24.3809319374676,
25.379023891907,26.3771158463464,27.3752078007858,28.2743338823081),
 .UNSPECIFIED.);
#26902=B_SPLINE_CURVE_WITH_KNOTS('',3,(#451513,#451514,#451515,#451516,
#451517),.UNSPECIFIED.,.F.,.F.,(4,1,4),(14.4000123930734,15.3981043475128,
15.7079632679489),.UNSPECIFIED.);
#26903=B_SPLINE_CURVE_WITH_KNOTS('',3,(#451520,#451521,#451522,#451523,
#451524),.UNSPECIFIED.,.F.,.F.,(4,1,4),(13.8743214892347,14.8351267319837,
15.7079632679489),.UNSPECIFIED.);
#26904=B_SPLINE_CURVE_WITH_KNOTS('',3,(#451540,#451541,#451542,#451543,
#451544,#451545,#451546,#451547,#451548,#451549,#451550,#451551,#451552,
#451553,#451554,#451555,#451556,#451557,#451558,#451559,#451560,#451561,
#451562,#451563,#451564,#451565,#451566,#451567,#451568,#451569,#451570,
#451571,#451572,#451573,#451574,#451575,#451576,#451577,#451578,#451579,
#451580,#451581,#451582,#451583,#451584,#451585,#451586,#451587,#451588,
#451589,#451590,#451591,#451592,#451593,#451594,#451595,#451596,#451597,
#451598,#451599,#451600,#451601,#451602,#451603,#451604,#451605,#451606,
#451607,#451608,#451609,#451610,#451611,#451612,#451613,#451614,#451615,
#451616,#451617,#451618),.UNSPECIFIED.,.F.,.F.,(4,3,3,3,3,3,3,3,3,3,3,3,
3,3,3,3,3,3,3,3,3,3,3,3,3,3,4),(0.,0.0157320924267747,0.0316472886091288,
0.043157780198946,0.0480880250790969,0.0511356327252552,0.0665923147581226,
0.0816964235607721,0.0922051230024958,0.0959158625638971,0.0986562987241478,
0.113270482254995,0.123731221327667,0.137671787499722,0.141347701639905,
0.14411982558934,0.15865675060424,0.173153963373766,0.180916686790059,0.184948756264495,
0.18803730480951,0.201934721427929,0.211309428016589,0.21535636816053,0.228670816766457,
0.235255750704108,0.23917877492942),.UNSPECIFIED.);
#26905=B_SPLINE_CURVE_WITH_KNOTS('',3,(#451619,#451620,#451621,#451622,
#451623,#451624,#451625,#451626,#451627,#451628,#451629,#451630,#451631,
#451632,#451633,#451634,#451635,#451636,#451637,#451638,#451639,#451640,
#451641,#451642,#451643,#451644,#451645,#451646,#451647,#451648,#451649,
#451650,#451651,#451652,#451653,#451654,#451655,#451656,#451657,#451658,
#451659,#451660,#451661,#451662,#451663,#451664,#451665,#451666,#451667,
#451668,#451669,#451670,#451671,#451672,#451673,#451674,#451675,#451676,
#451677,#451678,#451679,#451680,#451681,#451682,#451683,#451684,#451685,
#451686,#451687,#451688,#451689,#451690,#451691,#451692,#451693,#451694,
#451695,#451696,#451697),.UNSPECIFIED.,.F.,.F.,(4,3,3,3,3,3,3,3,3,3,3,3,
3,3,3,3,3,3,3,3,3,3,3,3,3,3,4),(0.,0.0130352311543815,0.0266669283949033,
0.0371674278206855,0.0406547610952736,0.0430558088931652,0.057131904576132,
0.0714875682820563,0.0812834071618324,0.0840733481352456,0.0867292191258407,
0.101529760808593,0.110670923801161,0.125085624608173,0.128310240996154,
0.131025696331468,0.145800277836723,0.160944486485529,0.169985276581641,
0.174963947365941,0.177680096517495,0.193348287176511,0.204022641009529,
0.208963013854378,0.224845444526331,0.233270807254426,0.238077416065722),
 .UNSPECIFIED.);
#26906=B_SPLINE_CURVE_WITH_KNOTS('',3,(#451698,#451699,#451700,#451701,
#451702,#451703,#451704,#451705,#451706,#451707,#451708,#451709,#451710,
#451711,#451712,#451713,#451714,#451715,#451716,#451717,#451718,#451719,
#451720,#451721,#451722,#451723,#451724,#451725,#451726,#451727,#451728,
#451729,#451730,#451731,#451732,#451733,#451734,#451735,#451736,#451737,
#451738,#451739,#451740,#451741,#451742,#451743,#451744,#451745,#451746,
#451747,#451748,#451749,#451750,#451751,#451752,#451753,#451754,#451755,
#451756,#451757,#451758,#451759,#451760,#451761,#451762,#451763,#451764,
#451765,#451766,#451767,#451768,#451769,#451770,#451771,#451772,#451773,
#451774,#451775,#451776),.UNSPECIFIED.,.F.,.F.,(4,3,3,3,3,3,3,3,3,3,3,3,
3,3,3,3,3,3,3,3,3,3,3,3,3,3,4),(0.,0.0157320924267752,0.0316472886090957,
0.0431577801989171,0.0480880250790769,0.0511356327253695,0.0665923147581514,
0.0816964235608268,0.0922051230025368,0.0959158625640407,0.0986562987234703,
0.113270482254332,0.123731221327667,0.137671787499722,0.141347701639849,
0.144119825587372,0.158656750602193,0.173153963371847,0.180916686788379,
0.184948756260439,0.188037304808125,0.201934721426646,0.211309428014682,
0.215356368159481,0.228670816765373,0.235255750704108,0.23917877492942),
 .UNSPECIFIED.);
#26907=B_SPLINE_CURVE_WITH_KNOTS('',3,(#451777,#451778,#451779,#451780,
#451781,#451782,#451783,#451784,#451785,#451786,#451787,#451788,#451789,
#451790,#451791,#451792,#451793,#451794,#451795,#451796,#451797,#451798,
#451799,#451800,#451801,#451802,#451803,#451804,#451805,#451806,#451807,
#451808,#451809,#451810,#451811,#451812,#451813,#451814,#451815,#451816,
#451817,#451818,#451819,#451820,#451821,#451822,#451823,#451824,#451825,
#451826,#451827,#451828,#451829,#451830,#451831,#451832,#451833,#451834,
#451835,#451836,#451837,#451838,#451839,#451840,#451841,#451842,#451843,
#451844,#451845,#451846,#451847,#451848,#451849,#451850,#451851,#451852,
#451853,#451854,#451855),.UNSPECIFIED.,.F.,.F.,(4,3,3,3,3,3,3,3,3,3,3,3,
3,3,3,3,3,3,3,3,3,3,3,3,3,3,4),(0.,0.0130352311543815,0.0266669283949033,
0.0371674278206855,0.0406547610952736,0.0430558088931652,0.057131904576132,
0.0714875682820563,0.0812834071618324,0.0840733481352456,0.0867292191258407,
0.101529760808593,0.110670923801161,0.125085624608173,0.128310240996154,
0.131025696331468,0.145800277836723,0.160944486485529,0.169985276581641,
0.174963947365941,0.177680096517495,0.193348287176511,0.204022641009529,
0.208963013854378,0.224845444526331,0.233270807254426,0.238077416065722),
 .UNSPECIFIED.);
#26908=B_SPLINE_CURVE_WITH_KNOTS('',3,(#451856,#451857,#451858,#451859,
#451860,#451861,#451862,#451863,#451864,#451865,#451866,#451867,#451868,
#451869,#451870,#451871,#451872,#451873,#451874,#451875,#451876,#451877,
#451878,#451879,#451880,#451881,#451882,#451883,#451884,#451885,#451886,
#451887,#451888,#451889,#451890,#451891,#451892,#451893,#451894,#451895,
#451896,#451897,#451898,#451899,#451900,#451901,#451902,#451903,#451904,
#451905,#451906,#451907,#451908,#451909,#451910,#451911,#451912,#451913,
#451914,#451915,#451916,#451917,#451918,#451919,#451920,#451921,#451922,
#451923,#451924,#451925,#451926,#451927,#451928,#451929,#451930,#451931,
#451932,#451933,#451934),.UNSPECIFIED.,.F.,.F.,(4,3,3,3,3,3,3,3,3,3,3,3,
3,3,3,3,3,3,3,3,3,3,3,3,3,3,4),(0.,0.0157320924267737,0.0316472886090531,
0.0431577801988798,0.0480880250789605,0.0511356327296043,0.0665923147621861,
0.081696423564749,0.0922051230054785,0.0959158625863417,0.098656298737445,
0.113270482268115,0.123731221327667,0.137671787499722,0.141347701639876,
0.144119825589662,0.1586567506045,0.173153963374121,0.18091668679037,0.184948756264717,
0.188037304802666,0.201934721421039,0.211309428006616,0.215356368156104,
0.228670816762204,0.235255750704108,0.23917877492942),.UNSPECIFIED.);
#26909=B_SPLINE_CURVE_WITH_KNOTS('',3,(#451935,#451936,#451937,#451938,
#451939,#451940,#451941,#451942,#451943,#451944,#451945,#451946,#451947,
#451948,#451949,#451950,#451951,#451952,#451953,#451954,#451955,#451956,
#451957,#451958,#451959,#451960,#451961,#451962,#451963,#451964,#451965,
#451966,#451967,#451968,#451969,#451970,#451971,#451972,#451973,#451974,
#451975,#451976,#451977,#451978,#451979,#451980,#451981,#451982,#451983,
#451984,#451985,#451986,#451987,#451988,#451989,#451990,#451991,#451992,
#451993,#451994,#451995,#451996,#451997,#451998,#451999,#452000,#452001,
#452002,#452003,#452004,#452005,#452006,#452007,#452008,#452009,#452010,
#452011,#452012,#452013),.UNSPECIFIED.,.F.,.F.,(4,3,3,3,3,3,3,3,3,3,3,3,
3,3,3,3,3,3,3,3,3,3,3,3,3,3,4),(0.,0.0130352311543805,0.026666928394927,
0.0371674278207062,0.0406547610703887,0.0430558088506834,0.0571319045324971,
0.0714875682385721,0.0812834071292192,0.0840733479829169,0.0867292190991322,
0.101529760781986,0.110670923801161,0.125085624608173,0.128310241000168,
0.131025696331686,0.145800277836979,0.160944486485698,0.169985276581789,
0.1749639473661,0.177680096519024,0.193348287178018,0.20402264101174,0.208963013855492,
0.224845444527478,0.233270807254426,0.238077416065722),.UNSPECIFIED.);
#26910=B_SPLINE_CURVE_WITH_KNOTS('',3,(#452014,#452015,#452016,#452017,
#452018,#452019,#452020,#452021,#452022,#452023,#452024,#452025,#452026,
#452027,#452028,#452029,#452030,#452031,#452032,#452033,#452034,#452035,
#452036,#452037,#452038,#452039,#452040,#452041,#452042,#452043,#452044,
#452045,#452046,#452047,#452048,#452049,#452050,#452051,#452052,#452053,
#452054,#452055,#452056,#452057,#452058,#452059,#452060,#452061,#452062,
#452063,#452064,#452065,#452066,#452067,#452068,#452069,#452070,#452071,
#452072,#452073,#452074,#452075,#452076,#452077,#452078,#452079,#452080,
#452081,#452082,#452083,#452084,#452085,#452086,#452087,#452088,#452089,
#452090,#452091,#452092),.UNSPECIFIED.,.F.,.F.,(4,3,3,3,3,3,3,3,3,3,3,3,
3,3,3,3,3,3,3,3,3,3,3,3,3,3,4),(0.,0.0157320924267737,0.0316472886090531,
0.0431577801988798,0.0480880250789605,0.0511356327296043,0.0665923147621861,
0.081696423564749,0.0922051230054785,0.0959158625863417,0.098656298737445,
0.113270482268115,0.123731221327667,0.137671787499722,0.141347701639876,
0.144119825589662,0.1586567506045,0.173153963374121,0.18091668679037,0.184948756264717,
0.188037304802666,0.201934721421039,0.211309428006616,0.215356368156104,
0.228670816762204,0.235255750704108,0.23917877492942),.UNSPECIFIED.);
#26911=B_SPLINE_CURVE_WITH_KNOTS('',3,(#452093,#452094,#452095,#452096,
#452097,#452098,#452099,#452100,#452101,#452102,#452103,#452104,#452105,
#452106,#452107,#452108,#452109,#452110,#452111,#452112,#452113,#452114,
#452115,#452116,#452117,#452118,#452119,#452120,#452121,#452122,#452123,
#452124,#452125,#452126,#452127,#452128,#452129,#452130,#452131,#452132,
#452133,#452134,#452135,#452136,#452137,#452138,#452139,#452140,#452141,
#452142,#452143,#452144,#452145,#452146,#452147,#452148,#452149,#452150,
#452151,#452152,#452153,#452154,#452155,#452156,#452157,#452158,#452159,
#452160,#452161,#452162,#452163,#452164,#452165,#452166,#452167,#452168,
#452169,#452170,#452171),.UNSPECIFIED.,.F.,.F.,(4,3,3,3,3,3,3,3,3,3,3,3,
3,3,3,3,3,3,3,3,3,3,3,3,3,3,4),(0.,0.0130352311543801,0.026666928394903,
0.0371674278206852,0.0406547610767215,0.0430558088631254,0.057131904545114,
0.0714875682511512,0.0812834071386536,0.0840733480328551,0.0867292191078698,
0.101529760790684,0.110670923801161,0.125085624608172,0.128310241001407,
0.131025696334341,0.145800277839661,0.160944486488484,0.169985276584227,
0.174963947370384,0.177680096527197,0.193348287186297,0.204022641023147,
0.208963013858931,0.224845444530877,0.233270807254426,0.238077416065722),
 .UNSPECIFIED.);
#26912=B_SPLINE_CURVE_WITH_KNOTS('',3,(#452173,#452174,#452175,#452176,
#452177,#452178,#452179,#452180,#452181,#452182,#452183),.UNSPECIFIED.,
 .F.,.F.,(4,1,1,1,1,1,1,1,4),(15.7079632679489,15.8332186864231,16.8313106408625,
17.829402595302,18.8274945497414,19.8255865041808,20.8236784586202,21.8217704130596,
21.9911485751285),.UNSPECIFIED.);
#26913=B_SPLINE_CURVE_WITH_KNOTS('',3,(#452184,#452185,#452186,#452187,
#452188,#452189,#452190,#452191,#452192,#452193),.UNSPECIFIED.,.F.,.F.,
(4,1,1,1,1,1,1,4),(15.7079632679489,16.3961963019522,17.3942882563917,18.3923802108311,
19.3904721652705,20.3885641197099,21.3866560741493,21.9911485751285),
 .UNSPECIFIED.);
#26914=B_SPLINE_CURVE_WITH_KNOTS('',3,(#452410,#452411,#452412,#452413,
#452414,#452415,#452416,#452417,#452418,#452419,#452420,#452421,#452422,
#452423,#452424,#452425,#452426,#452427,#452428,#452429,#452430,#452431,
#452432,#452433,#452434,#452435,#452436,#452437,#452438,#452439,#452440,
#452441,#452442,#452443,#452444,#452445,#452446,#452447,#452448,#452449,
#452450,#452451,#452452,#452453,#452454,#452455,#452456,#452457,#452458,
#452459,#452460,#452461,#452462,#452463,#452464,#452465,#452466,#452467,
#452468,#452469,#452470,#452471,#452472,#452473,#452474,#452475,#452476,
#452477,#452478,#452479,#452480,#452481,#452482,#452483,#452484,#452485,
#452486,#452487,#452488),.UNSPECIFIED.,.F.,.F.,(4,3,3,3,3,3,3,3,3,3,3,3,
3,3,3,3,3,3,3,3,3,3,3,3,3,3,4),(0.,0.0157320931414714,0.0316472893339854,
0.0431577808331959,0.0480880269721251,0.0511356325173917,0.0665923145021214,
0.081696422951762,0.0922051225457388,0.0959158592594865,0.0986562961493802,
0.113270479382768,0.123731221327669,0.137671787499727,0.141347701391183,
0.144119825431661,0.158656750491721,0.173153963159623,0.180916686602687,
0.184948755241336,0.188037304397269,0.201934720592235,0.211309426632634,
0.215356367558587,0.228670815451418,0.235255750704128,0.239178774929437),
 .UNSPECIFIED.);
#26915=B_SPLINE_CURVE_WITH_KNOTS('',3,(#452489,#452490,#452491,#452492,
#452493,#452494,#452495,#452496,#452497,#452498,#452499,#452500,#452501,
#452502,#452503,#452504,#452505,#452506,#452507,#452508,#452509,#452510,
#452511,#452512,#452513),.UNSPECIFIED.,.F.,.F.,(4,3,3,3,3,3,3,3,4),(-10.1502977064631,
-9.9809195443942,-8.98282758995478,-7.98473563551536,-6.98664368107594,
-5.98855172663652,-4.9904597721971,-3.99236781775768,-3.86711239928348),
 .UNSPECIFIED.);
#26916=B_SPLINE_CURVE_WITH_KNOTS('',3,(#452730,#452731,#452732,#452733,
#452734,#452735,#452736,#452737,#452738,#452739,#452740,#452741,#452742,
#452743,#452744,#452745,#452746,#452747,#452748,#452749,#452750,#452751,
#452752,#452753,#452754,#452755,#452756,#452757,#452758,#452759,#452760,
#452761,#452762,#452763,#452764,#452765,#452766,#452767,#452768,#452769,
#452770,#452771,#452772,#452773,#452774,#452775,#452776,#452777,#452778,
#452779,#452780,#452781,#452782,#452783,#452784,#452785,#452786,#452787,
#452788,#452789,#452790,#452791,#452792,#452793,#452794,#452795,#452796,
#452797,#452798,#452799,#452800,#452801,#452802,#452803,#452804,#452805,
#452806,#452807,#452808),.UNSPECIFIED.,.F.,.F.,(4,3,3,3,3,3,3,3,3,3,3,3,
3,3,3,3,3,3,3,3,3,3,3,3,3,3,4),(0.,0.0130352298242541,0.0266669261176872,
0.0371674258281218,0.0406547814925501,0.0430558447319413,0.0571319404399593,
0.0714876040892006,0.0812834340171916,0.0840734593866279,0.0867292385757745,
0.101529780369819,0.110670923801164,0.125085625301101,0.128310245101767,
0.131025701128335,0.145800283575492,0.160944492677408,0.169985281999537,
0.174963957321762,0.177680109845532,0.193348300597375,0.204022660000448,
0.208963012593868,0.224845443267828,0.233270807254441,0.238077416065717),
 .UNSPECIFIED.);
#26917=B_SPLINE_CURVE_WITH_KNOTS('',3,(#452809,#452810,#452811,#452812,
#452813,#452814,#452815,#452816,#452817,#452818,#452819,#452820,#452821,
#452822,#452823,#452824,#452825,#452826,#452827,#452828,#452829,#452830),
 .UNSPECIFIED.,.F.,.F.,(4,3,3,3,3,3,3,4),(7.59113618205511,7.98473563551536,
8.98282758995478,9.9809195443942,10.9790114988336,11.977103453273,12.9751954077125,
13.8743214892347),.UNSPECIFIED.);
#26918=B_SPLINE_CURVE_WITH_KNOTS('',3,(#452834,#452835,#452836,#452837,
#452838,#452839,#452840,#452841,#452842,#452843,#452844,#452845,#452846,
#452847,#452848,#452849,#452850,#452851,#452852,#452853,#452854,#452855,
#452856,#452857,#452858,#452859,#452860,#452861,#452862,#452863,#452864,
#452865,#452866,#452867,#452868,#452869,#452870,#452871,#452872,#452873,
#452874,#452875,#452876,#452877,#452878,#452879,#452880,#452881,#452882,
#452883,#452884,#452885,#452886,#452887,#452888,#452889,#452890,#452891,
#452892,#452893,#452894,#452895,#452896,#452897,#452898,#452899,#452900,
#452901,#452902,#452903,#452904,#452905,#452906,#452907,#452908,#452909,
#452910,#452911,#452912),.UNSPECIFIED.,.F.,.F.,(4,3,3,3,3,3,3,3,3,3,3,3,
3,3,3,3,3,3,3,3,3,3,3,3,3,3,4),(0.,0.0157320931414709,0.0316472893341372,
0.0431577808333288,0.0480880269725141,0.0511356325307602,0.0665923145154681,
0.081696422964954,0.0922051225556328,0.0959158593335102,0.0986562962157222,
0.113270479448293,0.123731221327669,0.137671787499727,0.141347701390983,
0.144119825446287,0.158656750506384,0.173153963174152,0.180916686615399,
0.184948755270777,0.18803730441128,0.201934720606637,0.211309426653049,
0.215356367562411,0.228670815455102,0.235255750704128,0.239178774929437),
 .UNSPECIFIED.);
#26919=B_SPLINE_CURVE_WITH_KNOTS('',3,(#452913,#452914,#452915,#452916,
#452917,#452918,#452919,#452920,#452921,#452922,#452923,#452924,#452925,
#452926,#452927,#452928,#452929,#452930,#452931,#452932,#452933,#452934,
#452935,#452936,#452937,#452938,#452939,#452940,#452941,#452942,#452943,
#452944,#452945,#452946,#452947,#452948,#452949,#452950,#452951,#452952,
#452953,#452954,#452955,#452956,#452957,#452958,#452959,#452960,#452961,
#452962,#452963,#452964,#452965,#452966,#452967,#452968,#452969,#452970,
#452971,#452972,#452973,#452974,#452975,#452976,#452977,#452978,#452979,
#452980,#452981,#452982,#452983,#452984,#452985,#452986,#452987,#452988,
#452989,#452990,#452991),.UNSPECIFIED.,.F.,.F.,(4,3,3,3,3,3,3,3,3,3,3,3,
3,3,3,3,3,3,3,3,3,3,3,3,3,3,4),(0.,0.0130352298242513,0.0266669261174319,
0.0371674258278985,0.0406547813928594,0.0430558445655346,0.057131940264528,
0.0714876039142613,0.0812834338859871,0.0840734588472805,0.0867292384812191,
0.101529780275389,0.110670923801164,0.125085625301103,0.12831024509547,
0.131025701136019,0.145800283582927,0.160944492684684,0.169985282005903,
0.174963957332129,0.17768010985427,0.193348300606252,0.20402266001364,0.208963012602614,
0.224845443276616,0.233270807254441,0.238077416065717),.UNSPECIFIED.);
#26920=B_SPLINE_CURVE_WITH_KNOTS('',3,(#452992,#452993,#452994,#452995,
#452996,#452997,#452998,#452999,#453000,#453001,#453002,#453003,#453004,
#453005,#453006,#453007,#453008,#453009,#453010,#453011,#453012,#453013,
#453014,#453015,#453016,#453017,#453018,#453019,#453020,#453021,#453022,
#453023,#453024,#453025,#453026,#453027,#453028,#453029,#453030,#453031,
#453032,#453033,#453034,#453035,#453036,#453037,#453038,#453039,#453040,
#453041,#453042,#453043,#453044,#453045,#453046,#453047,#453048,#453049,
#453050,#453051,#453052,#453053,#453054,#453055,#453056,#453057,#453058,
#453059,#453060,#453061,#453062,#453063,#453064,#453065,#453066,#453067,
#453068,#453069,#453070),.UNSPECIFIED.,.F.,.F.,(4,3,3,3,3,3,3,3,3,3,3,3,
3,3,3,3,3,3,3,3,3,3,3,3,3,3,4),(0.,0.015732093141471,0.0316472893339033,
0.0431577808331241,0.0480880269716089,0.0511356325101152,0.066592314495774,
0.0816964229456337,0.0922051225411426,0.0959158592248474,0.0986562961367495,
0.113270479370498,0.123731221327669,0.137671787499727,0.141347701390887,
0.144119825427528,0.158656750487409,0.173153963155311,0.180916686598913,
0.184948755232054,0.18803730438579,0.201934720581443,0.211309426616656,
0.215356367553738,0.228670815447029,0.235255750704128,0.239178774929437),
 .UNSPECIFIED.);
#26921=B_SPLINE_CURVE_WITH_KNOTS('',3,(#453071,#453072,#453073,#453074,
#453075,#453076,#453077,#453078,#453079,#453080,#453081,#453082,#453083,
#453084,#453085,#453086,#453087,#453088,#453089,#453090,#453091,#453092,
#453093,#453094,#453095,#453096,#453097,#453098,#453099,#453100,#453101,
#453102,#453103,#453104,#453105,#453106,#453107,#453108,#453109,#453110,
#453111,#453112,#453113,#453114,#453115,#453116,#453117,#453118,#453119,
#453120,#453121,#453122,#453123,#453124,#453125,#453126,#453127,#453128,
#453129,#453130,#453131,#453132,#453133,#453134,#453135,#453136,#453137,
#453138,#453139,#453140,#453141,#453142,#453143,#453144,#453145,#453146,
#453147,#453148,#453149),.UNSPECIFIED.,.F.,.F.,(4,3,3,3,3,3,3,3,3,3,3,3,
3,3,3,3,3,3,3,3,3,3,3,3,3,3,4),(0.,0.0130352298242513,0.0266669261174319,
0.0371674258278985,0.0406547813928594,0.0430558445655346,0.057131940264528,
0.0714876039142613,0.0812834338859871,0.0840734588472805,0.0867292384812191,
0.101529780275389,0.110670923801164,0.125085625301103,0.12831024509547,
0.131025701136019,0.145800283582927,0.160944492684684,0.169985282005903,
0.174963957332129,0.17768010985427,0.193348300606252,0.20402266001364,0.208963012602614,
0.224845443276616,0.233270807254441,0.238077416065717),.UNSPECIFIED.);
#26922=B_SPLINE_CURVE_WITH_KNOTS('',3,(#453150,#453151,#453152,#453153,
#453154,#453155,#453156,#453157,#453158,#453159,#453160,#453161,#453162,
#453163,#453164,#453165,#453166,#453167,#453168,#453169,#453170,#453171,
#453172,#453173,#453174,#453175,#453176,#453177,#453178,#453179,#453180,
#453181,#453182,#453183,#453184,#453185,#453186,#453187,#453188,#453189,
#453190,#453191,#453192,#453193,#453194,#453195,#453196,#453197,#453198,
#453199,#453200,#453201,#453202,#453203,#453204,#453205,#453206,#453207,
#453208,#453209,#453210,#453211,#453212,#453213,#453214,#453215,#453216,
#453217,#453218,#453219,#453220,#453221,#453222,#453223,#453224,#453225,
#453226,#453227,#453228),.UNSPECIFIED.,.F.,.F.,(4,3,3,3,3,3,3,3,3,3,3,3,
3,3,3,3,3,3,3,3,3,3,3,3,3,3,4),(0.,0.0157320931414714,0.0316472893339854,
0.0431577808331959,0.0480880269721251,0.0511356325173917,0.0665923145021214,
0.081696422951762,0.0922051225457388,0.0959158592594865,0.0986562961493802,
0.113270479382768,0.123731221327669,0.137671787499727,0.141347701391183,
0.144119825431661,0.158656750491721,0.173153963159623,0.180916686602687,
0.184948755241336,0.188037304397269,0.201934720592235,0.211309426632634,
0.215356367558587,0.228670815451418,0.235255750704128,0.239178774929437),
 .UNSPECIFIED.);
#26923=B_SPLINE_CURVE_WITH_KNOTS('',3,(#453229,#453230,#453231,#453232,
#453233,#453234,#453235,#453236,#453237,#453238,#453239,#453240,#453241,
#453242,#453243,#453244,#453245,#453246,#453247,#453248,#453249,#453250,
#453251,#453252,#453253,#453254,#453255,#453256,#453257,#453258,#453259,
#453260,#453261,#453262,#453263,#453264,#453265,#453266,#453267,#453268,
#453269,#453270,#453271,#453272,#453273,#453274,#453275,#453276,#453277,
#453278,#453279,#453280,#453281,#453282,#453283,#453284,#453285,#453286,
#453287,#453288,#453289,#453290,#453291,#453292,#453293,#453294,#453295,
#453296,#453297,#453298,#453299,#453300,#453301,#453302,#453303,#453304,
#453305,#453306,#453307),.UNSPECIFIED.,.F.,.F.,(4,3,3,3,3,3,3,3,3,3,3,3,
3,3,3,3,3,3,3,3,3,3,3,3,3,3,4),(0.,0.0130352298242544,0.0266669261174456,
0.0371674258279105,0.0406547815148651,0.0430558447696239,0.0571319404770745,
0.0714876041258789,0.0812834340447003,0.0840734595031264,0.0867292385960914,
0.101529780390005,0.110670923801164,0.125085625301101,0.128310245110238,
0.131025701127911,0.14580028357443,0.160944492676094,0.169985281998388,
0.17496395731976,0.177680109834163,0.193348300586186,0.204022659984646,
0.208963012605258,0.224845443279121,0.233270807254441,0.238077416065717),
 .UNSPECIFIED.);
#26924=B_SPLINE_CURVE_WITH_KNOTS('',3,(#453460,#453461,#453462,#453463,
#453464,#453465,#453466,#453467,#453468,#453469,#453470),.UNSPECIFIED.,
 .F.,.F.,(4,1,1,1,1,1,1,1,4),(15.7079632679489,15.8332186864231,16.8313106408625,
17.829402595302,18.8274945497414,19.8255865041808,20.8236784586202,21.8217704130596,
21.9911485751285),.UNSPECIFIED.);
#26925=B_SPLINE_CURVE_WITH_KNOTS('',3,(#453471,#453472,#453473,#453474,
#453475,#453476,#453477,#453478,#453479,#453480),.UNSPECIFIED.,.F.,.F.,
(4,1,1,1,1,1,1,4),(15.7079632679489,16.3961963019522,17.3942882563917,18.3923802108311,
19.3904721652705,20.3885641197099,21.3866560741493,21.9911485751285),
 .UNSPECIFIED.);
#26926=B_SPLINE_CURVE_WITH_KNOTS('',3,(#453697,#453698,#453699,#453700,
#453701,#453702,#453703,#453704,#453705,#453706,#453707,#453708,#453709,
#453710,#453711,#453712,#453713,#453714,#453715,#453716,#453717,#453718,
#453719,#453720,#453721),.UNSPECIFIED.,.F.,.F.,(4,3,3,3,3,3,3,3,4),(-10.1502977064631,
-9.9809195443942,-8.98282758995478,-7.98473563551536,-6.98664368107594,
-5.98855172663652,-4.9904597721971,-3.99236781775768,-3.86711239928348),
 .UNSPECIFIED.);
#26927=B_SPLINE_CURVE_WITH_KNOTS('',3,(#453938,#453939,#453940,#453941,
#453942,#453943,#453944,#453945,#453946,#453947,#453948,#453949,#453950,
#453951,#453952,#453953,#453954,#453955,#453956,#453957,#453958,#453959),
 .UNSPECIFIED.,.F.,.F.,(4,3,3,3,3,3,3,4),(7.59113618205511,7.98473563551536,
8.98282758995478,9.9809195443942,10.9790114988336,11.977103453273,12.9751954077125,
13.8743214892347),.UNSPECIFIED.);
#26928=B_SPLINE_CURVE_WITH_KNOTS('',3,(#453962,#453963,#453964,#453965,
#453966,#453967,#453968,#453969,#453970,#453971,#453972),.UNSPECIFIED.,
 .F.,.F.,(4,1,1,1,1,1,1,1,4),(15.7079632679489,15.8332186864231,16.8313106408625,
17.829402595302,18.8274945497414,19.8255865041808,20.8236784586202,21.8217704130596,
21.9911485751285),.UNSPECIFIED.);
#26929=B_SPLINE_CURVE_WITH_KNOTS('',3,(#453973,#453974,#453975,#453976,
#453977,#453978,#453979,#453980,#453981,#453982),.UNSPECIFIED.,.F.,.F.,
(4,1,1,1,1,1,1,4),(15.7079632679489,16.3961963019522,17.3942882563917,18.3923802108311,
19.3904721652705,20.3885641197099,21.3866560741493,21.9911485751285),
 .UNSPECIFIED.);
#26930=B_SPLINE_CURVE_WITH_KNOTS('',3,(#454199,#454200,#454201,#454202,
#454203,#454204,#454205,#454206,#454207,#454208,#454209,#454210,#454211,
#454212,#454213,#454214,#454215,#454216,#454217,#454218,#454219,#454220,
#454221,#454222,#454223),.UNSPECIFIED.,.F.,.F.,(4,3,3,3,3,3,3,3,4),(-10.1502977064631,
-9.9809195443942,-8.98282758995478,-7.98473563551536,-6.98664368107594,
-5.98855172663652,-4.9904597721971,-3.99236781775768,-3.86711239928348),
 .UNSPECIFIED.);
#26931=B_SPLINE_CURVE_WITH_KNOTS('',3,(#454440,#454441,#454442,#454443,
#454444,#454445,#454446,#454447,#454448,#454449,#454450,#454451,#454452,
#454453,#454454,#454455,#454456,#454457,#454458,#454459,#454460,#454461),
 .UNSPECIFIED.,.F.,.F.,(4,3,3,3,3,3,3,4),(7.59113618205511,7.98473563551536,
8.98282758995478,9.9809195443942,10.9790114988336,11.977103453273,12.9751954077125,
13.8743214892347),.UNSPECIFIED.);
#26932=B_SPLINE_CURVE_WITH_KNOTS('',3,(#454464,#454465,#454466,#454467,
#454468,#454469,#454470,#454471,#454472,#454473,#454474),.UNSPECIFIED.,
 .F.,.F.,(4,1,1,1,1,1,1,1,4),(15.7079632679489,15.8332186864231,16.8313106408625,
17.829402595302,18.8274945497414,19.8255865041808,20.8236784586202,21.8217704130596,
21.9911485751285),.UNSPECIFIED.);
#26933=B_SPLINE_CURVE_WITH_KNOTS('',3,(#454475,#454476,#454477,#454478,
#454479,#454480,#454481,#454482,#454483,#454484),.UNSPECIFIED.,.F.,.F.,
(4,1,1,1,1,1,1,4),(15.7079632679489,16.3961963019522,17.3942882563917,18.3923802108311,
19.3904721652705,20.3885641197099,21.3866560741493,21.9911485751285),
 .UNSPECIFIED.);
#26934=B_SPLINE_CURVE_WITH_KNOTS('',3,(#454701,#454702,#454703,#454704,
#454705,#454706,#454707,#454708,#454709,#454710,#454711,#454712,#454713,
#454714,#454715,#454716,#454717,#454718,#454719,#454720,#454721,#454722,
#454723,#454724,#454725),.UNSPECIFIED.,.F.,.F.,(4,3,3,3,3,3,3,3,4),(-10.1502977064631,
-9.9809195443942,-8.98282758995478,-7.98473563551536,-6.98664368107594,
-5.98855172663652,-4.9904597721971,-3.99236781775768,-3.86711239928348),
 .UNSPECIFIED.);
#26935=B_SPLINE_CURVE_WITH_KNOTS('',3,(#454942,#454943,#454944,#454945,
#454946,#454947,#454948,#454949,#454950,#454951,#454952,#454953,#454954,
#454955,#454956,#454957,#454958,#454959,#454960,#454961,#454962,#454963),
 .UNSPECIFIED.,.F.,.F.,(4,3,3,3,3,3,3,4),(7.59113618205511,7.98473563551536,
8.98282758995478,9.9809195443942,10.9790114988336,11.977103453273,12.9751954077125,
13.8743214892347),.UNSPECIFIED.);
#26936=B_SPLINE_CURVE_WITH_KNOTS('',3,(#454971,#454972,#454973,#454974,
#454975,#454976,#454977,#454978,#454979,#454980),.UNSPECIFIED.,.F.,.F.,
(4,3,3,4),(-4.09293042013066,-3.97768420534918,-2.98326315401189,-2.06773127522702),
 .UNSPECIFIED.);
#26937=B_SPLINE_CURVE_WITH_KNOTS('',3,(#454983,#454984,#454985,#454986,
#454987,#454988,#454989),.UNSPECIFIED.,.F.,.F.,(4,3,4),(0.,0.994421051337293,
1.11639350868612),.UNSPECIFIED.);
#26938=B_SPLINE_CURVE_WITH_KNOTS('',3,(#454994,#454995,#454996,#454997,
#454998,#454999,#455000,#455001,#455002,#455003,#455004,#455005,#455006,
#455007,#455008,#455009,#455010,#455011,#455012,#455013,#455014,#455015),
 .UNSPECIFIED.,.F.,.F.,(4,3,3,3,3,3,3,4),(-10.3761157273102,-9.94421051337296,
-8.94978946203567,-7.95536841069837,-6.96094735936108,-5.96652630802378,
-4.97210525668648,-4.09293042013066),.UNSPECIFIED.);
#26939=B_SPLINE_CURVE_WITH_KNOTS('',3,(#455016,#455017,#455018,#455019,
#455020,#455021,#455022,#455023,#455024,#455025,#455026,#455027,#455028,
#455029,#455030,#455031,#455032,#455033,#455034,#455035,#455036,#455037),
 .UNSPECIFIED.,.F.,.F.,(4,3,3,3,3,3,3,4),(1.11639350868612,1.98884210267459,
2.98326315401189,3.97768420534918,4.97210525668648,5.96652630802378,6.96094735936107,
7.39957881586571),.UNSPECIFIED.);
#26940=B_SPLINE_CURVE_WITH_KNOTS('',3,(#455042,#455043,#455044,#455045,
#455046,#455047,#455048,#455049,#455050,#455051,#455052,#455053,#455054,
#455055,#455056,#455057,#455058,#455059,#455060,#455061,#455062,#455063),
 .UNSPECIFIED.,.F.,.F.,(4,3,3,3,3,3,3,4),(-16.6593010344898,-15.9107368213967,
-14.9163157700594,-13.9218947187222,-12.9274736673849,-11.9330526160476,
-10.9386315647103,-10.3761157273102),.UNSPECIFIED.);
#26941=B_SPLINE_CURVE_WITH_KNOTS('',3,(#455064,#455065,#455066,#455067,
#455068,#455069,#455070,#455071,#455072,#455073,#455074,#455075,#455076,
#455077,#455078,#455079,#455080,#455081,#455082,#455083,#455084,#455085),
 .UNSPECIFIED.,.F.,.F.,(4,3,3,3,3,3,3,4),(7.39957881586571,7.95536841069837,
8.94978946203567,9.94421051337297,10.9386315647103,11.9330526160476,12.9274736673849,
13.6827641230453),.UNSPECIFIED.);
#26942=B_SPLINE_CURVE_WITH_KNOTS('',3,(#455090,#455091,#455092,#455093,
#455094,#455095,#455096,#455097,#455098,#455099,#455100,#455101,#455102,
#455103,#455104,#455105,#455106,#455107,#455108,#455109,#455110,#455111,
#455112,#455113,#455114),.UNSPECIFIED.,.F.,.F.,(4,3,3,3,3,3,3,3,4),(-22.9424863416694,
-22.8716841807578,-21.8772631294205,-20.8828420780832,-19.8884210267459,
-18.8939999754086,-17.8995789240713,-16.905157872734,-16.6593010344898),
 .UNSPECIFIED.);
#26943=B_SPLINE_CURVE_WITH_KNOTS('',3,(#455115,#455116,#455117,#455118,
#455119,#455120,#455121,#455122,#455123,#455124,#455125,#455126,#455127,
#455128,#455129,#455130,#455131,#455132,#455133,#455134,#455135,#455136,
#455137,#455138,#455139),.UNSPECIFIED.,.F.,.F.,(4,3,3,3,3,3,3,3,4),(13.6827641230453,
13.9218947187222,14.9163157700594,15.9107368213967,16.905157872734,17.8995789240713,
18.8939999754086,19.8884210267459,19.9659494302249),.UNSPECIFIED.);
#26944=B_SPLINE_CURVE_WITH_KNOTS('',3,(#455144,#455145,#455146,#455147,
#455148,#455149,#455150,#455151,#455152,#455153,#455154,#455155,#455156,
#455157,#455158,#455159,#455160,#455161,#455162,#455163,#455164,#455165),
 .UNSPECIFIED.,.F.,.F.,(4,3,3,3,3,3,3,4),(-29.225671648849,-28.8382104887816,
-27.8437894374443,-26.849368386107,-25.8549473347697,-24.8605262834324,
-23.8661052320951,-22.9424863416694),.UNSPECIFIED.);
#26945=B_SPLINE_CURVE_WITH_KNOTS('',3,(#455166,#455167,#455168,#455169,
#455170,#455171,#455172,#455173,#455174,#455175,#455176,#455177,#455178,
#455179,#455180,#455181,#455182,#455183,#455184,#455185,#455186,#455187),
 .UNSPECIFIED.,.F.,.F.,(4,3,3,3,3,3,3,4),(19.9659494302249,20.8828420780832,
21.8772631294205,22.8716841807578,23.8661052320951,24.8605262834324,25.8549473347697,
26.2491347374045),.UNSPECIFIED.);
#26946=B_SPLINE_CURVE_WITH_KNOTS('',3,(#455192,#455193,#455194,#455195,
#455196,#455197,#455198,#455199,#455200,#455201,#455202,#455203,#455204,
#455205,#455206,#455207,#455208,#455209,#455210,#455211,#455212,#455213),
 .UNSPECIFIED.,.F.,.F.,(4,3,3,3,3,3,3,4),(-35.5088569560286,-34.8047367968054,
-33.8103157454681,-32.8158946941308,-31.8214736427935,-30.8270525914562,
-29.8326315401189,-29.225671648849),.UNSPECIFIED.);
#26947=B_SPLINE_CURVE_WITH_KNOTS('',3,(#455214,#455215,#455216,#455217,
#455218,#455219,#455220,#455221,#455222,#455223,#455224,#455225,#455226,
#455227,#455228,#455229,#455230,#455231,#455232,#455233,#455234,#455235),
 .UNSPECIFIED.,.F.,.F.,(4,3,3,3,3,3,3,4),(26.2491347374045,26.849368386107,
27.8437894374443,28.8382104887816,29.8326315401189,30.8270525914562,31.8214736427935,
32.532320044584),.UNSPECIFIED.);
#26948=B_SPLINE_CURVE_WITH_KNOTS('',3,(#455240,#455241,#455242,#455243,
#455244,#455245,#455246,#455247,#455248,#455249,#455250,#455251,#455252,
#455253,#455254,#455255,#455256,#455257,#455258,#455259,#455260,#455261,
#455262,#455263,#455264),.UNSPECIFIED.,.F.,.F.,(4,3,3,3,3,3,3,3,4),(-41.7920422632082,
-41.7656841561665,-40.7712631048292,-39.7768420534919,-38.7824210021546,
-37.7879999508173,-36.79357889948,-35.7991578481427,-35.5088569560286),
 .UNSPECIFIED.);
#26949=B_SPLINE_CURVE_WITH_KNOTS('',3,(#455265,#455266,#455267,#455268,
#455269,#455270,#455271,#455272,#455273,#455274,#455275,#455276,#455277,
#455278,#455279,#455280,#455281,#455282,#455283,#455284,#455285,#455286,
#455287,#455288,#455289),.UNSPECIFIED.,.F.,.F.,(4,3,3,3,3,3,3,3,4),(32.532320044584,
32.8158946941308,33.8103157454681,34.8047367968054,35.7991578481427,36.79357889948,
37.7879999508173,38.7824210021546,38.8155053517636),.UNSPECIFIED.);
#26950=B_SPLINE_CURVE_WITH_KNOTS('',3,(#455294,#455295,#455296,#455297,
#455298,#455299,#455300,#455301,#455302,#455303,#455304,#455305,#455306,
#455307,#455308,#455309,#455310,#455311,#455312,#455313,#455314,#455315),
 .UNSPECIFIED.,.F.,.F.,(4,3,3,3,3,3,3,4),(-48.0752275703878,-47.7322104641902,
-46.7377894128529,-45.7433683615156,-44.7489473101783,-43.754526258841,
-42.7601052075037,-41.7920422632082),.UNSPECIFIED.);
#26951=B_SPLINE_CURVE_WITH_KNOTS('',3,(#455316,#455317,#455318,#455319,
#455320,#455321,#455322,#455323,#455324,#455325,#455326,#455327,#455328,
#455329,#455330,#455331,#455332,#455333,#455334,#455335,#455336,#455337),
 .UNSPECIFIED.,.F.,.F.,(4,3,3,3,3,3,3,4),(38.8155053517636,39.7768420534919,
40.7712631048292,41.7656841561664,42.7601052075037,43.754526258841,44.7489473101783,
45.0986906589432),.UNSPECIFIED.);
#26952=B_SPLINE_CURVE_WITH_KNOTS('',3,(#455342,#455343,#455344,#455345,
#455346,#455347,#455348,#455349,#455350,#455351,#455352,#455353,#455354,
#455355,#455356,#455357,#455358,#455359,#455360,#455361,#455362,#455363),
 .UNSPECIFIED.,.F.,.F.,(4,3,3,3,3,3,3,4),(-54.3584128775674,-53.698736772214,
-52.7043157208767,-51.7098946695394,-50.7154736182021,-49.7210525668648,
-48.7266315155275,-48.0752275703878),.UNSPECIFIED.);
#26953=B_SPLINE_CURVE_WITH_KNOTS('',3,(#455364,#455365,#455366,#455367,
#455368,#455369,#455370,#455371,#455372,#455373,#455374,#455375,#455376,
#455377,#455378,#455379,#455380,#455381,#455382,#455383,#455384,#455385),
 .UNSPECIFIED.,.F.,.F.,(4,3,3,3,3,3,3,4),(45.0986906589432,45.7433683615156,
46.7377894128529,47.7322104641902,48.7266315155275,49.7210525668648,50.7154736182021,
51.3818759661228),.UNSPECIFIED.);
#26954=B_SPLINE_CURVE_WITH_KNOTS('',3,(#455390,#455391,#455392,#455393,
#455394,#455395,#455396,#455397,#455398,#455399,#455400,#455401,#455402,
#455403,#455404,#455405,#455406,#455407,#455408,#455409,#455410,#455411),
 .UNSPECIFIED.,.F.,.F.,(4,3,3,3,3,3,3,4),(-60.641598184747,-59.6652630802378,
-58.6708420289005,-57.6764209775632,-56.6819999262259,-55.6875788748886,
-54.6931578235513,-54.3584128775674),.UNSPECIFIED.);
#26955=B_SPLINE_CURVE_WITH_KNOTS('',3,(#455412,#455413,#455414,#455415,
#455416,#455417,#455418,#455419,#455420,#455421,#455422,#455423,#455424,
#455425,#455426,#455427,#455428,#455429,#455430,#455431,#455432,#455433),
 .UNSPECIFIED.,.F.,.F.,(4,3,3,3,3,3,3,4),(51.3818759661228,51.7098946695394,
52.7043157208767,53.698736772214,54.6931578235513,55.6875788748886,56.6819999262259,
57.6650612733024),.UNSPECIFIED.);
#26956=B_SPLINE_CURVE_WITH_KNOTS('',3,(#455439,#455440,#455441,#455442,
#455443),.UNSPECIFIED.,.F.,.F.,(4,1,4),(72.2566310325653,72.2747169793933,
73.1902488581782),.UNSPECIFIED.);
#26957=B_SPLINE_CURVE_WITH_KNOTS('',3,(#455449,#455450,#455451,#455452,
#455453,#455454,#455455,#455456,#455457,#455458),.UNSPECIFIED.,.F.,.F.,
(4,1,1,1,1,1,1,4),(65.9734457253856,66.3081906713696,67.3026117227069,68.2970327740442,
69.2914538253815,70.2858748767188,71.280295928056,72.2566310325653),
 .UNSPECIFIED.);
#26958=B_SPLINE_CURVE_WITH_KNOTS('',3,(#455461,#455462,#455463,#455464,
#455465,#455466,#455467,#455468,#455469,#455470),.UNSPECIFIED.,.F.,.F.,
(4,1,1,1,1,1,1,4),(65.9734457253856,65.9848054296463,66.9792264809836,67.9736475323209,
68.9680685836582,69.9624896349955,70.9569106863328,71.9513317376701),
 .UNSPECIFIED.);
#26959=B_SPLINE_CURVE_WITH_KNOTS('',3,(#455475,#455476,#455477,#455478,
#455479,#455480,#455481,#455482,#455483,#455484),.UNSPECIFIED.,.F.,.F.,
(4,1,1,1,1,1,1,4),(59.6902604182061,60.3416643633458,61.3360854146831,62.3305064660204,
63.3249275173577,64.319348568695,65.3137696200323,65.9734457253856),
 .UNSPECIFIED.);
#26960=B_SPLINE_CURVE_WITH_KNOTS('',3,(#455485,#455486,#455487,#455488,
#455489,#455490,#455491,#455492,#455493,#455494),.UNSPECIFIED.,.F.,.F.,
(4,1,1,1,1,1,1,4),(59.6902604182061,60.0182791216226,61.0127001729599,62.0071212242972,
63.0015422756345,63.9959633269718,64.9903843783091,65.9734457253856),
 .UNSPECIFIED.);
#26961=B_SPLINE_CURVE_WITH_KNOTS('',3,(#455499,#455500,#455501,#455502,
#455503,#455504,#455505,#455506,#455507,#455508),.UNSPECIFIED.,.F.,.F.,
(4,1,1,1,1,1,1,4),(53.4070751110265,54.375138055322,55.3695591066593,56.3639801579966,
57.3584012093339,58.3528222606712,59.3472433120085,59.6902604182061),
 .UNSPECIFIED.);
#26962=B_SPLINE_CURVE_WITH_KNOTS('',3,(#455509,#455510,#455511,#455512,
#455513,#455514,#455515,#455516,#455517,#455518),.UNSPECIFIED.,.F.,.F.,
(4,1,1,1,1,1,1,4),(53.4070751110265,54.0517528135988,55.0461738649361,56.0405949162734,
57.0350159676107,58.029437018948,59.0238580702853,59.6902604182061),
 .UNSPECIFIED.);
#26963=B_SPLINE_CURVE_WITH_KNOTS('',3,(#455523,#455524,#455525,#455526,
#455527,#455528,#455529,#455530,#455531,#455532,#455533),.UNSPECIFIED.,
 .F.,.F.,(4,1,1,1,1,1,1,1,4),(47.1238898038469,47.4141906959609,48.4086117472982,
49.4030327986355,50.3974538499728,51.3918749013101,52.3862959526474,53.3807170039847,
53.4070751110265),.UNSPECIFIED.);
#26964=B_SPLINE_CURVE_WITH_KNOTS('',3,(#455534,#455535,#455536,#455537,
#455538,#455539,#455540,#455541,#455542,#455543),.UNSPECIFIED.,.F.,.F.,
(4,1,1,1,1,1,1,4),(47.1238898038469,48.085226505575,49.0796475569123,50.0740686082496,
51.0684896595869,52.0629107109242,53.0573317622615,53.4070751110265),
 .UNSPECIFIED.);
#26965=B_SPLINE_CURVE_WITH_KNOTS('',3,(#455548,#455549,#455550,#455551,
#455552,#455553,#455554,#455555,#455556,#455557),.UNSPECIFIED.,.F.,.F.,
(4,1,1,1,1,1,1,4),(40.8407044966673,41.4476643879372,42.4420854392745,43.4365064906117,
44.430927541949,45.4253485932863,46.4197696446236,47.1238898038469),
 .UNSPECIFIED.);
#26966=B_SPLINE_CURVE_WITH_KNOTS('',3,(#455558,#455559,#455560,#455561,
#455562,#455563,#455564,#455565,#455566,#455567,#455568),.UNSPECIFIED.,
 .F.,.F.,(4,1,1,1,1,1,1,1,4),(40.8407044966673,41.1242791462139,42.1187001975512,
43.1131212488885,44.1075423002258,45.1019633515631,46.0963844029004,47.0908054542377,
47.1238898038469),.UNSPECIFIED.);
#26967=B_SPLINE_CURVE_WITH_KNOTS('',3,(#455573,#455574,#455575,#455576,
#455577,#455578,#455579,#455580,#455581,#455582),.UNSPECIFIED.,.F.,.F.,
(4,1,1,1,1,1,1,4),(34.5575191894877,35.4811380799134,36.4755591312507,37.469980182588,
38.4644012339253,39.4588222852626,40.4532433365999,40.8407044966673),
 .UNSPECIFIED.);
#26968=B_SPLINE_CURVE_WITH_KNOTS('',3,(#455583,#455584,#455585,#455586,
#455587,#455588,#455589,#455590,#455591,#455592),.UNSPECIFIED.,.F.,.F.,
(4,1,1,1,1,1,1,4),(34.5575191894877,35.1577528381902,36.1521738895275,37.1465949408648,
38.1410159922021,39.1354370435394,40.1298580948767,40.8407044966673),
 .UNSPECIFIED.);
#26969=B_SPLINE_CURVE_WITH_KNOTS('',3,(#455597,#455598,#455599,#455600,
#455601,#455602,#455603,#455604,#455605,#455606,#455607),.UNSPECIFIED.,
 .F.,.F.,(4,1,1,1,1,1,1,1,4),(28.2743338823081,28.5201907205523,29.5146117718896,
30.5090328232269,31.5034538745642,32.4978749259015,33.4922959772388,34.4867170285761,
34.5575191894877),.UNSPECIFIED.);
#26970=B_SPLINE_CURVE_WITH_KNOTS('',3,(#455608,#455609,#455610,#455611,
#455612,#455613,#455614,#455615,#455616,#455617),.UNSPECIFIED.,.F.,.F.,
(4,1,1,1,1,1,1,4),(28.2743338823081,29.1912265301664,30.1856475815037,31.180068632841,
32.1744896841783,33.1689107355156,34.1633317868529,34.5575191894877),
 .UNSPECIFIED.);
#26971=B_SPLINE_CURVE_WITH_KNOTS('',3,(#455622,#455623,#455624,#455625,
#455626,#455627,#455628,#455629,#455630,#455631),.UNSPECIFIED.,.F.,.F.,
(4,1,1,1,1,1,1,4),(21.9911485751285,22.5536644125285,23.5480854638658,24.5425065152031,
25.5369275665404,26.5313486178777,27.525769669215,28.2743338823081),
 .UNSPECIFIED.);
#26972=B_SPLINE_CURVE_WITH_KNOTS('',3,(#455632,#455633,#455634,#455635,
#455636,#455637,#455638,#455639,#455640,#455641,#455642),.UNSPECIFIED.,
 .F.,.F.,(4,1,1,1,1,1,1,1,4),(21.9911485751285,22.2302791708053,23.2247002221426,
24.2191212734799,25.2135423248172,26.2079633761545,27.2023844274918,28.1968054788291,
28.2743338823081),.UNSPECIFIED.);
#26973=B_SPLINE_CURVE_WITH_KNOTS('',3,(#455647,#455648,#455649,#455650,
#455651,#455652,#455653,#455654,#455655,#455656),.UNSPECIFIED.,.F.,.F.,
(4,1,1,1,1,1,1,4),(15.7079632679489,16.5871381045047,17.581559155842,18.5759802071793,
19.5704012585166,20.5648223098539,21.5592433611912,21.9911485751285),
 .UNSPECIFIED.);
#26974=B_SPLINE_CURVE_WITH_KNOTS('',3,(#455657,#455658,#455659,#455660,
#455661,#455662,#455663,#455664,#455665,#455666),.UNSPECIFIED.,.F.,.F.,
(4,1,1,1,1,1,1,4),(15.7079632679489,16.2637528627815,17.2581739141188,18.2525949654561,
19.2470160167934,20.2414370681307,21.235858119468,21.9911485751285),
 .UNSPECIFIED.);
#26975=B_SPLINE_CURVE_WITH_KNOTS('',3,(#455672,#455673,#455674,#455675,
#455676,#455677,#455678,#455679,#455680,#455681),.UNSPECIFIED.,.F.,.F.,
(4,3,3,4),(-4.09293042013064,-3.9393605542126,-2.95452041565945,-2.06863817490912),
 .UNSPECIFIED.);
#26976=B_SPLINE_CURVE_WITH_KNOTS('',3,(#455684,#455685,#455686,#455687,
#455688,#455689,#455690),.UNSPECIFIED.,.F.,.F.,(4,3,4),(0.,0.984840138553148,
1.11730040836828),.UNSPECIFIED.);
#26977=B_SPLINE_CURVE_WITH_KNOTS('',3,(#455695,#455696,#455697,#455698,
#455699,#455700,#455701,#455702,#455703,#455704,#455705,#455706,#455707,
#455708,#455709,#455710,#455711,#455712,#455713,#455714,#455715,#455716),
 .UNSPECIFIED.,.F.,.F.,(4,3,3,3,3,3,3,4),(-10.3761157273102,-9.84840138553149,
-8.86356124697834,-7.87872110842519,-6.89388096987204,-5.9090408313189,
-4.92420069276575,-4.09293042013064),.UNSPECIFIED.);
#26978=B_SPLINE_CURVE_WITH_KNOTS('',3,(#455717,#455718,#455719,#455720,
#455721,#455722,#455723,#455724,#455725,#455726,#455727,#455728,#455729,
#455730,#455731,#455732,#455733,#455734,#455735,#455736,#455737,#455738),
 .UNSPECIFIED.,.F.,.F.,(4,3,3,3,3,3,3,4),(1.11730040836828,1.9696802771063,
2.95452041565944,3.93936055421259,4.92420069276574,5.90904083131889,6.89388096987204,
7.40048571554787),.UNSPECIFIED.);
#26979=B_SPLINE_CURVE_WITH_KNOTS('',3,(#455743,#455744,#455745,#455746,
#455747,#455748,#455749,#455750,#455751,#455752,#455753,#455754,#455755,
#455756,#455757,#455758,#455759,#455760,#455761,#455762,#455763,#455764),
 .UNSPECIFIED.,.F.,.F.,(4,3,3,3,3,3,3,4),(-16.6593010344898,-15.7574422168504,
-14.7726020782972,-13.7877619397441,-12.8029218011909,-11.8180816626378,
-10.8332415240846,-10.3761157273102),.UNSPECIFIED.);
#26980=B_SPLINE_CURVE_WITH_KNOTS('',3,(#455765,#455766,#455767,#455768,
#455769,#455770,#455771,#455772,#455773,#455774,#455775,#455776,#455777,
#455778,#455779,#455780,#455781,#455782,#455783,#455784,#455785,#455786),
 .UNSPECIFIED.,.F.,.F.,(4,3,3,3,3,3,3,4),(7.40048571554787,7.87872110842519,
8.86356124697834,9.84840138553149,10.8332415240846,11.8180816626378,12.8029218011909,
13.6836710227275),.UNSPECIFIED.);
#26981=B_SPLINE_CURVE_WITH_KNOTS('',3,(#455791,#455792,#455793,#455794,
#455795,#455796,#455797,#455798,#455799,#455800,#455801,#455802,#455803,
#455804,#455805,#455806,#455807,#455808,#455809,#455810,#455811,#455812,
#455813,#455814,#455815),.UNSPECIFIED.,.F.,.F.,(4,3,3,3,3,3,3,3,4),(-22.9424863416694,
-22.6513231867224,-21.6664830481693,-20.6816429096161,-19.696802771063,
-18.7119626325098,-17.7271224939567,-16.7422823554035,-16.6593010344898),
 .UNSPECIFIED.);
#26982=B_SPLINE_CURVE_WITH_KNOTS('',3,(#455816,#455817,#455818,#455819,
#455820,#455821,#455822,#455823,#455824,#455825,#455826,#455827,#455828,
#455829,#455830,#455831,#455832,#455833,#455834,#455835,#455836,#455837,
#455838,#455839,#455840),.UNSPECIFIED.,.F.,.F.,(4,3,3,3,3,3,3,3,4),(13.6836710227275,
13.7877619397441,14.7726020782972,15.7574422168504,16.7422823554035,17.7271224939567,
18.7119626325098,19.696802771063,19.966856329907),.UNSPECIFIED.);
#26983=B_SPLINE_CURVE_WITH_KNOTS('',3,(#455845,#455846,#455847,#455848,
#455849,#455850,#455851,#455852,#455853,#455854,#455855,#455856,#455857,
#455858,#455859,#455860,#455861,#455862,#455863,#455864,#455865,#455866),
 .UNSPECIFIED.,.F.,.F.,(4,3,3,3,3,3,3,4),(-29.225671648849,-28.5603640180413,
-27.5755238794882,-26.590683740935,-25.6058436023819,-24.6210034638287,
-23.6361633252756,-22.9424863416694),.UNSPECIFIED.);
#26984=B_SPLINE_CURVE_WITH_KNOTS('',3,(#455867,#455868,#455869,#455870,
#455871,#455872,#455873,#455874,#455875,#455876,#455877,#455878,#455879,
#455880,#455881,#455882,#455883,#455884,#455885,#455886,#455887,#455888),
 .UNSPECIFIED.,.F.,.F.,(4,3,3,3,3,3,3,4),(19.966856329907,20.6816429096161,
21.6664830481693,22.6513231867224,23.6361633252756,24.6210034638287,25.6058436023819,
26.2500416370866),.UNSPECIFIED.);
#26985=B_SPLINE_CURVE_WITH_KNOTS('',3,(#455894,#455895,#455896,#455897,
#455898,#455899),.UNSPECIFIED.,.F.,.F.,(4,1,1,4),(40.8407044966673,41.1602370044128,
42.1450771429659,43.0309593837163),.UNSPECIFIED.);
#26986=B_SPLINE_CURVE_WITH_KNOTS('',3,(#455902,#455903,#455904,#455905),
 .UNSPECIFIED.,.F.,.F.,(4,4),(40.8407044966673,41.7920422632082),
 .UNSPECIFIED.);
#26987=B_SPLINE_CURVE_WITH_KNOTS('',3,(#455910,#455911,#455912,#455913,
#455914,#455915,#455916,#455917,#455918,#455919),.UNSPECIFIED.,.F.,.F.,
(4,1,1,1,1,1,1,4),(34.5575191894877,35.2511961730939,36.236036311647,37.2208764502002,
38.2057165887533,39.1905567273065,40.1753968658596,40.8407044966673),
 .UNSPECIFIED.);
#26988=B_SPLINE_CURVE_WITH_KNOTS('',3,(#455920,#455921,#455922,#455923,
#455924,#455925,#455926,#455927,#455928,#455929,#455930),.UNSPECIFIED.,
 .F.,.F.,(4,1,1,1,1,1,1,1,4),(34.5575191894877,34.8981612933361,35.8830014318893,
36.8678415704424,37.8526817089956,38.8375218475487,39.8223619861019,40.807202124655,
40.8407044966673),.UNSPECIFIED.);
#26989=B_SPLINE_CURVE_WITH_KNOTS('',3,(#455935,#455936,#455937,#455938,
#455939,#455940,#455941,#455942,#455943,#455944,#455945),.UNSPECIFIED.,
 .F.,.F.,(4,1,1,1,1,1,1,1,4),(28.2743338823081,28.3573152032219,29.342155341775,
30.3269954803282,31.3118356188813,32.2966757574344,33.2815158959876,34.2663560345407,
34.5575191894877),.UNSPECIFIED.);
#26990=B_SPLINE_CURVE_WITH_KNOTS('',3,(#455946,#455947,#455948,#455949,
#455950,#455951,#455952,#455953,#455954,#455955),.UNSPECIFIED.,.F.,.F.,
(4,1,1,1,1,1,1,4),(28.2743338823081,28.9891204620172,29.9739606005704,30.9588007391235,
31.9436408776767,32.9284810162298,33.913321154783,34.5575191894877),
 .UNSPECIFIED.);
#26991=B_SPLINE_CURVE_WITH_KNOTS('',3,(#455960,#455961,#455962,#455963,
#455964,#455965,#455966,#455967,#455968,#455969),.UNSPECIFIED.,.F.,.F.,
(4,1,1,1,1,1,1,4),(21.9911485751285,22.448274371903,23.4331145104561,24.4179546490093,
25.4027947875624,26.3876349261156,27.3724750646687,28.2743338823081),
 .UNSPECIFIED.);
#26992=B_SPLINE_CURVE_WITH_KNOTS('',3,(#455970,#455971,#455972,#455973,
#455974,#455975,#455976,#455977,#455978,#455979,#455980),.UNSPECIFIED.,
 .F.,.F.,(4,1,1,1,1,1,1,1,4),(21.9911485751285,22.0952394921452,23.0800796306983,
24.0649197692515,25.0497599078046,26.0346000463578,27.0194401849109,28.0042803234641,
28.2743338823081),.UNSPECIFIED.);
#26993=B_SPLINE_CURVE_WITH_KNOTS('',3,(#455985,#455986,#455987,#455988,
#455989,#455990,#455991,#455992,#455993,#455994),.UNSPECIFIED.,.F.,.F.,
(4,1,1,1,1,1,1,4),(15.707963267949,16.5392335405841,17.5240736791372,18.5089138176904,
19.4937539562435,20.4785940947967,21.4634342333498,21.9911485751285),
 .UNSPECIFIED.);
#26994=B_SPLINE_CURVE_WITH_KNOTS('',3,(#455995,#455996,#455997,#455998,
#455999,#456000,#456001,#456002,#456003,#456004),.UNSPECIFIED.,.F.,.F.,
(4,1,1,1,1,1,1,4),(15.707963267949,16.1861986608263,17.1710387993794,18.1558789379326,
19.1407190764857,20.1255592150389,21.110399353592,21.9911485751285),
 .UNSPECIFIED.);
#26995=B_SPLINE_CURVE_WITH_KNOTS('',3,(#456154,#456155,#456156,#456157,
#456158,#456159,#456160,#456161,#456162,#456163,#456164,#456165,#456166,
#456167,#456168,#456169,#456170,#456171,#456172,#456173,#456174,#456175,
#456176,#456177,#456178,#456179,#456180,#456181,#456182,#456183,#456184,
#456185,#456186,#456187,#456188,#456189,#456190,#456191,#456192,#456193,
#456194,#456195,#456196,#456197,#456198,#456199,#456200,#456201,#456202,
#456203,#456204,#456205,#456206,#456207,#456208,#456209,#456210,#456211,
#456212,#456213,#456214,#456215,#456216,#456217,#456218,#456219,#456220,
#456221,#456222,#456223,#456224,#456225,#456226,#456227,#456228,#456229,
#456230,#456231,#456232,#456233,#456234,#456235,#456236,#456237,#456238,
#456239,#456240,#456241,#456242,#456243,#456244),.UNSPECIFIED.,.F.,.F.,
(4,3,3,3,3,3,3,3,3,3,3,3,3,3,3,3,3,3,3,3,3,3,3,3,3,3,3,3,3,3,4),(0.,0.0291704936873683,
0.0583901552072424,0.0892766589597223,0.102789504351432,0.112166362673238,
0.116534597984906,0.14527798460994,0.17392803078138,0.202083533954261,0.215008365363363,
0.220764604622565,0.22483118758101,0.252407730218333,0.279182155080764,
0.305482185227081,0.321094097925349,0.325435232071915,0.352007771215581,
0.37911010758988,0.405971172690074,0.418020595108885,0.425023905710974,
0.429595206514516,0.455898766278936,0.480742271809045,0.487658166045092,
0.494570770854422,0.519851794548597,0.544421019656577,0.55527278839937),
 .UNSPECIFIED.);
#26996=B_SPLINE_CURVE_WITH_KNOTS('',3,(#456245,#456246,#456247,#456248,
#456249,#456250,#456251,#456252,#456253,#456254,#456255,#456256,#456257,
#456258,#456259,#456260,#456261,#456262,#456263),.UNSPECIFIED.,.F.,.F.,
(4,3,3,3,3,3,4),(26.2500416370866,26.590683740935,27.5755238794882,28.5603640180413,
29.5452041565945,30.5300442951476,31.4159265358979),.UNSPECIFIED.);
#26997=B_SPLINE_CURVE_WITH_KNOTS('',3,(#456265,#456266,#456267,#456268,
#456269,#456270,#456271,#456272,#456273,#456274,#456275,#456276,#456277,
#456278,#456279,#456280,#456281,#456282,#456283,#456284,#456285,#456286,
#456287,#456288,#456289,#456290,#456291,#456292,#456293,#456294,#456295,
#456296,#456297,#456298,#456299,#456300,#456301,#456302,#456303,#456304,
#456305,#456306,#456307,#456308,#456309,#456310,#456311,#456312,#456313,
#456314,#456315,#456316,#456317,#456318,#456319,#456320,#456321,#456322,
#456323,#456324,#456325,#456326,#456327,#456328,#456329,#456330,#456331,
#456332,#456333,#456334,#456335,#456336,#456337,#456338,#456339,#456340,
#456341,#456342,#456343,#456344,#456345,#456346,#456347,#456348,#456349,
#456350,#456351,#456352,#456353,#456354,#456355),.UNSPECIFIED.,.F.,.F.,
(4,3,3,3,3,3,3,3,3,3,3,3,3,3,3,3,3,3,3,3,3,3,3,3,3,3,3,3,3,3,4),(0.,0.0238062091558073,
0.0483829200003844,0.0735693023851429,0.0861844508658027,0.0923222737131809,
0.09669810673984,0.122607870190124,0.149055649769671,0.175727680368522,
0.188356929884852,0.192627184956794,0.220007365861877,0.247709521968789,
0.2754116780757,0.285004370325409,0.293795122953647,0.298369842260591,0.325203400447931,
0.35364614768882,0.378533551524598,0.391516739337066,0.398116945812671,
0.403847639833503,0.432612326557626,0.462645589511981,0.47232137580103,
0.479347180528688,0.50891257055823,0.538120141855211,0.552745378375044),
 .UNSPECIFIED.);
#26998=B_SPLINE_CURVE_WITH_KNOTS('',3,(#456356,#456357,#456358,#456359,
#456360,#456361,#456362,#456363,#456364),.UNSPECIFIED.,.F.,.F.,(4,1,1,1,
1,1,4),(10.3761157273102,11.2619979680605,12.2468381066137,13.2316782451668,
14.21651838372,15.2013585222731,15.707963267949),.UNSPECIFIED.);
#26999=B_SPLINE_CURVE_WITH_KNOTS('',3,(#456368,#456369,#456370,#456371,
#456372,#456373,#456374,#456375),.UNSPECIFIED.,.F.,.F.,(4,1,1,1,1,4),(11.6150328478183,
12.5998729863715,13.5847131249246,14.5695532634778,15.5543934020309,15.707963267949),
 .UNSPECIFIED.);
#27000=B_SPLINE_CURVE_WITH_KNOTS('',3,(#456525,#456526,#456527,#456528,
#456529,#456530,#456531,#456532,#456533,#456534,#456535,#456536,#456537,
#456538,#456539,#456540,#456541,#456542,#456543,#456544,#456545,#456546,
#456547,#456548,#456549,#456550,#456551,#456552,#456553,#456554,#456555,
#456556,#456557,#456558,#456559,#456560,#456561,#456562,#456563,#456564,
#456565,#456566,#456567,#456568,#456569,#456570,#456571,#456572,#456573,
#456574,#456575,#456576,#456577,#456578,#456579,#456580,#456581,#456582,
#456583,#456584,#456585,#456586,#456587,#456588,#456589,#456590,#456591,
#456592,#456593,#456594,#456595,#456596,#456597,#456598,#456599,#456600,
#456601,#456602,#456603,#456604,#456605,#456606,#456607,#456608,#456609,
#456610,#456611,#456612,#456613,#456614,#456615),.UNSPECIFIED.,.F.,.F.,
(4,3,3,3,3,3,3,3,3,3,3,3,3,3,3,3,3,3,3,3,3,3,3,3,3,3,3,3,3,3,4),(0.,0.0238062091558071,
0.0483828706186186,0.0735692218797394,0.0861843753919871,0.0923221305421182,
0.0966981255468032,0.122607856296174,0.149055623017512,0.175727654618578,
0.18835688351681,0.192627137748861,0.220007313021443,0.247709495548573,
0.275411678075702,0.285004376041476,0.293795155716159,0.298369846935252,
0.325203393116049,0.353646141273424,0.378533545911127,0.391516729248669,
0.398116977240157,0.403847652647052,0.432612318543257,0.462645583501205,
0.472321362733173,0.479347182520809,0.508912572368484,0.538120187828272,
0.55274537837505),.UNSPECIFIED.);
#27001=B_SPLINE_CURVE_WITH_KNOTS('',3,(#456616,#456617,#456618,#456619,
#456620,#456621,#456622,#456623,#456624,#456625,#456626,#456627,#456628,
#456629,#456630,#456631,#456632,#456633,#456634,#456635,#456636,#456637,
#456638,#456639,#456640,#456641,#456642,#456643,#456644,#456645,#456646,
#456647,#456648,#456649,#456650,#456651,#456652,#456653,#456654,#456655,
#456656,#456657,#456658,#456659,#456660,#456661,#456662,#456663,#456664,
#456665,#456666,#456667,#456668,#456669,#456670,#456671,#456672,#456673,
#456674,#456675,#456676,#456677,#456678,#456679,#456680,#456681,#456682,
#456683,#456684,#456685,#456686,#456687,#456688,#456689,#456690,#456691,
#456692,#456693,#456694,#456695,#456696,#456697,#456698,#456699,#456700,
#456701,#456702,#456703,#456704,#456705,#456706),.UNSPECIFIED.,.F.,.F.,
(4,3,3,3,3,3,3,3,3,3,3,3,3,3,3,3,3,3,3,3,3,3,3,3,3,3,3,3,3,3,4),(0.,0.0291704936873701,
0.0583901514208582,0.0892766556466376,0.102789501245416,0.112166345743357,
0.116534589717914,0.145277976478382,0.173928009345204,0.20208347654446,
0.215008315129789,0.220764359590348,0.224831129685752,0.252407647279974,
0.279182017118223,0.305482185227093,0.321094097925361,0.325435232358679,
0.352007731597858,0.379110069176849,0.405971171510899,0.418020583618158,
0.42502391146057,0.42959521059718,0.455898797678682,0.480742295358858,0.487658257009521,
0.494570761890733,0.519851841940689,0.544421141195806,0.555272788399386),
 .UNSPECIFIED.);
#27002=B_SPLINE_CURVE_WITH_KNOTS('',3,(#456707,#456708,#456709,#456710,
#456711,#456712,#456713,#456714,#456715,#456716,#456717,#456718,#456719,
#456720,#456721,#456722),.UNSPECIFIED.,.F.,.F.,(4,3,3,3,3,4),(-33.4845647108071,
-32.4997245722539,-31.5148844337008,-30.5300442951476,-29.5452041565945,
-29.225671648849),.UNSPECIFIED.);
#27003=B_SPLINE_CURVE_WITH_KNOTS('',3,(#456732,#456733,#456734,#456735,
#456736,#456737,#456738,#456739,#456740,#456741,#456742,#456743,#456744,
#456745,#456746,#456747,#456748,#456749,#456750,#456751,#456752,#456753),
 .UNSPECIFIED.,.F.,.F.,(4,3,3,3,3,3,3,4),(-0.137266596901587,-0.120108272288889,
-0.114482300827285,-0.110524277642504,-0.080939047567984,-0.0517696842448276,
-0.0235157745135959,0.),.UNSPECIFIED.);
#27004=B_SPLINE_CURVE_WITH_KNOTS('',3,(#456755,#456756,#456757,#456758,
#456759,#456760,#456761,#456762,#456763,#456764,#456765,#456766,#456767,
#456768,#456769,#456770,#456771,#456772,#456773),.UNSPECIFIED.,.F.,.F.,
(4,3,3,3,3,3,4),(-0.658260979006767,-0.635315718400124,-0.606661307506358,
-0.584172758955614,-0.578302186585446,-0.54863415322041,-0.52069807482506),
 .UNSPECIFIED.);
#27005=B_SPLINE_CURVE_WITH_KNOTS('',3,(#457044,#457045,#457046,#457047,
#457048,#457049,#457050,#457051,#457052,#457053,#457054,#457055,#457056,
#457057,#457058,#457059,#457060,#457061,#457062,#457063,#457064,#457065,
#457066,#457067,#457068,#457069,#457070,#457071,#457072,#457073,#457074,
#457075,#457076,#457077,#457078,#457079,#457080,#457081,#457082,#457083,
#457084,#457085,#457086,#457087,#457088,#457089,#457090,#457091,#457092,
#457093,#457094,#457095,#457096,#457097,#457098,#457099,#457100,#457101,
#457102,#457103,#457104,#457105,#457106,#457107,#457108,#457109,#457110,
#457111,#457112,#457113),.UNSPECIFIED.,.F.,.F.,(4,3,3,3,3,3,3,3,3,3,3,3,
3,3,3,3,3,3,3,3,3,3,3,4),(0.,0.0272040286413901,0.0600270143818345,0.0934058988577766,
0.126267828410656,0.131862201401969,0.13651369641287,0.16911813316586,0.201670978277266,
0.233729929110374,0.249051354881678,0.259289013450942,0.263883210759706,
0.29536534390224,0.325978269163176,0.356301335280809,0.374706067837319,
0.381238410008019,0.386955324433938,0.417676149855772,0.448702433409449,
0.479505858091495,0.503539195732891,0.520698074825087),.UNSPECIFIED.);
#27006=B_SPLINE_CURVE_WITH_KNOTS('',3,(#457114,#457115,#457116,#457117,
#457118,#457119,#457120,#457121,#457122,#457123,#457124,#457125,#457126,
#457127,#457128,#457129),.UNSPECIFIED.,.F.,.F.,(4,3,3,3,3,4),(57.6650612733024,
57.6764209775632,58.6708420289005,59.6652630802378,60.6596841315751,61.57521601036),
 .UNSPECIFIED.);
#27007=B_SPLINE_CURVE_WITH_KNOTS('',3,(#457131,#457132,#457133,#457134,
#457135,#457136,#457137,#457138,#457139,#457140,#457141,#457142,#457143,
#457144,#457145,#457146,#457147,#457148,#457149,#457150,#457151,#457152,
#457153,#457154,#457155,#457156,#457157,#457158,#457159,#457160,#457161,
#457162,#457163,#457164,#457165,#457166,#457167,#457168,#457169,#457170,
#457171,#457172,#457173,#457174,#457175,#457176,#457177,#457178,#457179,
#457180,#457181,#457182,#457183,#457184,#457185,#457186,#457187,#457188,
#457189,#457190,#457191,#457192,#457193,#457194,#457195,#457196,#457197,
#457198,#457199,#457200,#457201,#457202,#457203,#457204,#457205,#457206,
#457207,#457208,#457209,#457210,#457211,#457212,#457213,#457214,#457215,
#457216,#457217,#457218),.UNSPECIFIED.,.F.,.F.,(4,3,3,3,3,3,3,3,3,3,3,3,
3,3,3,3,3,3,3,3,3,3,3,3,3,3,3,3,3,4),(0.,0.0228820365931952,0.051218373414923,
0.080268233877054,0.111010300783671,0.116758747556016,0.146658127377976,
0.177121111126461,0.207780701795497,0.222583710212308,0.229317438129826,
0.234676157420321,0.26606503457775,0.297281607920556,0.326204769129986,
0.346801497054257,0.352594205912184,0.356892740676827,0.387479019349114,
0.41883328811469,0.450858933696391,0.476470618974131,0.482836412282282,
0.515509333257769,0.548396254053967,0.563515013889454,0.570640443970302,
0.604038137402537,0.636956540638902,0.655752415918318),.UNSPECIFIED.);
#27008=B_SPLINE_CURVE_WITH_KNOTS('',3,(#457219,#457220,#457221,#457222,
#457223,#457224,#457225,#457226,#457227),.UNSPECIFIED.,.F.,.F.,(4,1,1,1,
1,1,4),(10.3761157273102,11.2916476060951,12.2860686574324,13.2804897087697,
14.2749107601069,15.2693318114442,15.7079632679489),.UNSPECIFIED.);
#27009=B_SPLINE_CURVE_WITH_KNOTS('',3,(#457231,#457232,#457233,#457234,
#457235,#457236,#457237,#457238),.UNSPECIFIED.,.F.,.F.,(4,1,1,1,1,4),(11.6150328478183,
12.6094538991556,13.6038749504929,14.5982960018302,15.5927170531675,15.7079632679489),
 .UNSPECIFIED.);
#27010=B_SPLINE_CURVE_WITH_KNOTS('',3,(#457507,#457508,#457509,#457510,
#457511,#457512,#457513,#457514,#457515,#457516,#457517,#457518,#457519,
#457520,#457521,#457522,#457523,#457524,#457525,#457526,#457527,#457528,
#457529,#457530,#457531,#457532,#457533,#457534,#457535,#457536,#457537,
#457538,#457539,#457540,#457541,#457542,#457543,#457544,#457545,#457546,
#457547,#457548,#457549,#457550,#457551,#457552,#457553,#457554,#457555,
#457556,#457557,#457558,#457559,#457560,#457561,#457562,#457563,#457564,
#457565,#457566,#457567,#457568,#457569,#457570,#457571,#457572,#457573,
#457574,#457575,#457576,#457577,#457578,#457579,#457580,#457581,#457582,
#457583,#457584,#457585,#457586,#457587,#457588,#457589,#457590,#457591,
#457592,#457593,#457594,#457595,#457596,#457597,#457598,#457599,#457600),
 .UNSPECIFIED.,.F.,.F.,(4,3,3,3,3,3,3,3,3,3,3,3,3,3,3,3,3,3,3,3,3,3,3,3,
3,3,3,3,3,3,3,4),(0.,0.0272040286413987,0.0600270092260691,0.0934058933249245,
0.126267823569411,0.131862171516485,0.13651368729204,0.169118124243381,
0.201670964051155,0.233729898345333,0.249051327962268,0.259288987827642,
0.263883168763017,0.295365290437433,0.325978188171709,0.356301335280814,
0.375173813013688,0.383411475909621,0.388182941704446,0.418653739168425,
0.449704751396772,0.480514094750049,0.494157308726131,0.502507051908377,
0.507342387999586,0.537640987329864,0.567795985249096,0.576607688145916,
0.582412660202483,0.611714236442306,0.640195300747252,0.658260979006793),
 .UNSPECIFIED.);
#27011=B_SPLINE_CURVE_WITH_KNOTS('',3,(#457602,#457603,#457604,#457605,
#457606,#457607,#457608,#457609,#457610,#457611,#457612,#457613,#457614),
 .UNSPECIFIED.,.F.,.F.,(4,3,3,3,4),(-63.642947285587,-62.6485262342497,
-61.6541051829124,-60.6596841315751,-60.641598184747),.UNSPECIFIED.);
#27012=B_SPLINE_CURVE_WITH_KNOTS('',3,(#457615,#457616,#457617,#457618,
#457619,#457620,#457621,#457622,#457623,#457624,#457625,#457626,#457627,
#457628,#457629,#457630,#457631,#457632,#457633,#457634,#457635,#457636,
#457637,#457638,#457639,#457640,#457641,#457642,#457643,#457644,#457645,
#457646,#457647,#457648,#457649,#457650,#457651,#457652,#457653,#457654,
#457655,#457656,#457657,#457658,#457659,#457660,#457661,#457662,#457663,
#457664,#457665,#457666,#457667,#457668,#457669,#457670,#457671,#457672,
#457673,#457674,#457675,#457676,#457677,#457678,#457679,#457680,#457681),
 .UNSPECIFIED.,.F.,.F.,(4,3,3,3,3,3,3,3,3,3,3,3,3,3,3,3,3,3,3,3,3,3,4),
(0.137266596905892,0.167584419985923,0.198231972141458,0.230225171388588,
0.234597263271361,0.265985606555594,0.297202865015363,0.326204769129979,
0.346801497054249,0.352594207537935,0.356892744389492,0.387479014259225,
0.418833269879323,0.450858809182976,0.476470510024891,0.482836382836457,
0.51550929223882,0.548396212827012,0.563514950346987,0.570640427639483,
0.604038123799383,0.636956554307592,0.6557524159183),.UNSPECIFIED.);
#27013=B_SPLINE_CURVE_WITH_KNOTS('',3,(#457738,#457739,#457740,#457741,
#457742,#457743,#457744,#457745,#457746,#457747),.UNSPECIFIED.,.F.,.F.,
(4,3,3,4),(-4.09293042013065,-3.97677500179867,-2.982581251349,-2.06863817490913),
 .UNSPECIFIED.);
#27014=B_SPLINE_CURVE_WITH_KNOTS('',3,(#457750,#457751,#457752,#457753,
#457754,#457755,#457756),.UNSPECIFIED.,.F.,.F.,(4,3,4),(0.,0.994193750449668,
1.11730040836827),.UNSPECIFIED.);
#27015=B_SPLINE_CURVE_WITH_KNOTS('',3,(#457761,#457762,#457763,#457764,
#457765,#457766,#457767,#457768,#457769,#457770,#457771,#457772,#457773,
#457774,#457775,#457776,#457777,#457778,#457779,#457780,#457781,#457782),
 .UNSPECIFIED.,.F.,.F.,(4,3,3,3,3,3,3,4),(-10.3761157273102,-9.94193750449666,
-8.94774375404699,-7.95355000359733,-6.95935625314767,-5.965162502698,-4.97096875224833,
-4.09293042013065),.UNSPECIFIED.);
#27016=B_SPLINE_CURVE_WITH_KNOTS('',3,(#457783,#457784,#457785,#457786,
#457787,#457788,#457789,#457790,#457791,#457792,#457793,#457794,#457795,
#457796,#457797,#457798,#457799,#457800,#457801,#457802,#457803,#457804),
 .UNSPECIFIED.,.F.,.F.,(4,3,3,3,3,3,3,4),(1.11730040836827,1.98838750089933,
2.982581251349,3.97677500179867,4.97096875224833,5.965162502698,6.95935625314766,
7.40048571554786),.UNSPECIFIED.);
#27017=B_SPLINE_CURVE_WITH_KNOTS('',3,(#457809,#457810,#457811,#457812,
#457813,#457814,#457815,#457816,#457817,#457818,#457819,#457820,#457821,
#457822,#457823,#457824,#457825,#457826,#457827,#457828,#457829,#457830),
 .UNSPECIFIED.,.F.,.F.,(4,3,3,3,3,3,3,4),(-16.6593010344898,-15.9071000071947,
-14.912906256745,-13.9187125062953,-12.9245187558457,-11.930325005396,-10.9361312549463,
-10.3761157273102),.UNSPECIFIED.);
#27018=B_SPLINE_CURVE_WITH_KNOTS('',3,(#457831,#457832,#457833,#457834,
#457835,#457836,#457837,#457838,#457839,#457840,#457841,#457842,#457843,
#457844,#457845,#457846,#457847,#457848,#457849,#457850,#457851,#457852),
 .UNSPECIFIED.,.F.,.F.,(4,3,3,3,3,3,3,4),(7.40048571554786,7.95355000359733,
8.947743754047,9.94193750449667,10.9361312549463,11.930325005396,12.9245187558457,
13.6836710227274),.UNSPECIFIED.);
#27019=B_SPLINE_CURVE_WITH_KNOTS('',3,(#457857,#457858,#457859,#457860,
#457861,#457862,#457863,#457864,#457865,#457866,#457867,#457868,#457869,
#457870,#457871,#457872,#457873,#457874,#457875,#457876,#457877,#457878,
#457879,#457880,#457881),.UNSPECIFIED.,.F.,.F.,(4,3,3,3,3,3,3,3,4),(-22.9424863416694,
-22.8664562603423,-21.8722625098927,-20.878068759443,-19.8838750089933,
-18.8896812585437,-17.895487508094,-16.9012937576443,-16.6593010344898),
 .UNSPECIFIED.);
#27020=B_SPLINE_CURVE_WITH_KNOTS('',3,(#457882,#457883,#457884,#457885,
#457886,#457887,#457888,#457889,#457890,#457891,#457892,#457893,#457894,
#457895,#457896,#457897,#457898,#457899,#457900,#457901,#457902,#457903,
#457904,#457905,#457906),.UNSPECIFIED.,.F.,.F.,(4,3,3,3,3,3,3,3,4),(13.6836710227274,
13.9187125062953,14.912906256745,15.9071000071947,16.9012937576443,17.895487508094,
18.8896812585436,19.8838750089933,19.966856329907),.UNSPECIFIED.);
#27021=B_SPLINE_CURVE_WITH_KNOTS('',3,(#457911,#457912,#457913,#457914,
#457915,#457916,#457917,#457918,#457919,#457920,#457921,#457922,#457923,
#457924,#457925,#457926,#457927,#457928,#457929,#457930,#457931,#457932),
 .UNSPECIFIED.,.F.,.F.,(4,3,3,3,3,3,3,4),(-29.225671648849,-28.8316187630403,
-27.8374250125907,-26.843231262141,-25.8490375116913,-24.8548437612417,
-23.860650010792,-22.9424863416694),.UNSPECIFIED.);
#27022=B_SPLINE_CURVE_WITH_KNOTS('',3,(#457933,#457934,#457935,#457936,
#457937,#457938,#457939,#457940,#457941,#457942,#457943,#457944,#457945,
#457946,#457947,#457948,#457949,#457950,#457951,#457952,#457953,#457954),
 .UNSPECIFIED.,.F.,.F.,(4,3,3,3,3,3,3,4),(19.966856329907,20.878068759443,
21.8722625098927,22.8664562603423,23.860650010792,24.8548437612417,25.8490375116913,
26.2500416370866),.UNSPECIFIED.);
#27023=B_SPLINE_CURVE_WITH_KNOTS('',3,(#457959,#457960,#457961,#457962,
#457963,#457964,#457965,#457966,#457967,#457968,#457969,#457970,#457971,
#457972,#457973,#457974,#457975,#457976,#457977,#457978,#457979,#457980),
 .UNSPECIFIED.,.F.,.F.,(4,3,3,3,3,3,3,4),(-35.5088569560286,-34.7967812657383,
-33.8025875152886,-32.808393764839,-31.8142000143893,-30.8200062639396,
-29.82581251349,-29.225671648849),.UNSPECIFIED.);
#27024=B_SPLINE_CURVE_WITH_KNOTS('',3,(#457981,#457982,#457983,#457984,
#457985,#457986,#457987,#457988,#457989,#457990,#457991,#457992,#457993,
#457994,#457995,#457996,#457997,#457998,#457999,#458000,#458001,#458002),
 .UNSPECIFIED.,.F.,.F.,(4,3,3,3,3,3,3,4),(26.2500416370866,26.843231262141,
27.8374250125906,28.8316187630403,29.82581251349,30.8200062639396,31.8142000143893,
32.5332269442662),.UNSPECIFIED.);
#27025=B_SPLINE_CURVE_WITH_KNOTS('',3,(#458008,#458009,#458010,#458011,
#458012,#458013),.UNSPECIFIED.,.F.,.F.,(4,1,1,4),(47.1238898038469,47.4060078640063,
48.400201614456,49.3141446908958),.UNSPECIFIED.);
#27026=B_SPLINE_CURVE_WITH_KNOTS('',3,(#458016,#458017,#458018,#458019),
 .UNSPECIFIED.,.F.,.F.,(4,4),(47.1238898038469,48.0752275703877),
 .UNSPECIFIED.);
#27027=B_SPLINE_CURVE_WITH_KNOTS('',3,(#458024,#458025,#458026,#458027,
#458028,#458029,#458030,#458031,#458032,#458033),.UNSPECIFIED.,.F.,.F.,
(4,1,1,1,1,1,1,4),(40.8407044966673,41.4408453613083,42.4350391117579,43.4292328622076,
44.4234266126573,45.4176203631069,46.4118141135566,47.1238898038469),
 .UNSPECIFIED.);
#27028=B_SPLINE_CURVE_WITH_KNOTS('',3,(#458034,#458035,#458036,#458037,
#458038,#458039,#458040,#458041,#458042,#458043,#458044),.UNSPECIFIED.,
 .F.,.F.,(4,1,1,1,1,1,1,1,4),(40.8407044966673,41.1158713172401,42.1100650676897,
43.1042588181394,44.0984525685891,45.0926463190387,46.0868400694884,47.081033819938,
47.1238898038469),.UNSPECIFIED.);
#27029=B_SPLINE_CURVE_WITH_KNOTS('',3,(#458049,#458050,#458051,#458052,
#458053,#458054,#458055,#458056,#458057,#458058),.UNSPECIFIED.,.F.,.F.,
(4,1,1,1,1,1,1,4),(34.5575191894877,35.4756828586103,36.46987660906,37.4640703595096,
38.4582641099593,39.452457860409,40.4466516108586,40.8407044966673),
 .UNSPECIFIED.);
#27030=B_SPLINE_CURVE_WITH_KNOTS('',3,(#458059,#458060,#458061,#458062,
#458063,#458064,#458065,#458066,#458067,#458068),.UNSPECIFIED.,.F.,.F.,
(4,1,1,1,1,1,1,4),(34.5575191894877,35.1507088145421,36.1449025649917,37.1390963154414,
38.1332900658911,39.1274838163407,40.1216775667904,40.8407044966673),
 .UNSPECIFIED.);
#27031=B_SPLINE_CURVE_WITH_KNOTS('',3,(#458073,#458074,#458075,#458076,
#458077,#458078,#458079,#458080,#458081,#458082,#458083),.UNSPECIFIED.,
 .F.,.F.,(4,1,1,1,1,1,1,1,4),(28.2743338823081,28.5163266054626,29.5105203559123,
30.504714106362,31.4989078568116,32.4931016072613,33.487295357711,34.4814891081606,
34.5575191894877),.UNSPECIFIED.);
#27032=B_SPLINE_CURVE_WITH_KNOTS('',3,(#458084,#458085,#458086,#458087,
#458088,#458089,#458090,#458091,#458092,#458093),.UNSPECIFIED.,.F.,.F.,
(4,1,1,1,1,1,1,4),(28.2743338823081,29.1855463118441,30.1797400622937,31.1739338127434,
32.1681275631931,33.1623213136427,34.1565150640924,34.5575191894877),
 .UNSPECIFIED.);
#27033=B_SPLINE_CURVE_WITH_KNOTS('',3,(#458098,#458099,#458100,#458101,
#458102,#458103,#458104,#458105,#458106,#458107),.UNSPECIFIED.,.F.,.F.,
(4,1,1,1,1,1,1,4),(21.9911485751285,22.5511641027646,23.5453578532143,24.539551603664,
25.5337453541136,26.5279391045633,27.522132855013,28.2743338823081),
 .UNSPECIFIED.);
#27034=B_SPLINE_CURVE_WITH_KNOTS('',3,(#458108,#458109,#458110,#458111,
#458112,#458113,#458114,#458115,#458116,#458117,#458118),.UNSPECIFIED.,
 .F.,.F.,(4,1,1,1,1,1,1,1,4),(21.9911485751285,22.2261900586964,23.2203838091461,
24.2145775595957,25.2087713100454,26.2029650604951,27.1971588109447,28.1913525613944,
28.2743338823081),.UNSPECIFIED.);
#27035=B_SPLINE_CURVE_WITH_KNOTS('',3,(#458123,#458124,#458125,#458126,
#458127,#458128,#458129,#458130,#458131,#458132),.UNSPECIFIED.,.F.,.F.,
(4,1,1,1,1,1,1,4),(15.707963267949,16.5860016000666,17.5801953505163,18.574389100966,
19.5685828514156,20.5627766018653,21.556970352315,21.9911485751285),
 .UNSPECIFIED.);
#27036=B_SPLINE_CURVE_WITH_KNOTS('',3,(#458133,#458134,#458135,#458136,
#458137,#458138,#458139,#458140,#458141,#458142),.UNSPECIFIED.,.F.,.F.,
(4,1,1,1,1,1,1,4),(15.7079632679489,16.2610275559984,17.2552213064481,18.2494150568977,
19.2436088073474,20.2378025577971,21.2319963082467,21.9911485751285),
 .UNSPECIFIED.);
#27037=B_SPLINE_CURVE_WITH_KNOTS('',3,(#458316,#458317,#458318,#458319,
#458320,#458321,#458322,#458323,#458324,#458325,#458326,#458327,#458328,
#458329,#458330,#458331,#458332,#458333,#458334,#458335,#458336,#458337,
#458338,#458339,#458340,#458341,#458342,#458343,#458344,#458345,#458346,
#458347,#458348,#458349,#458350,#458351,#458352,#458353,#458354,#458355,
#458356,#458357,#458358,#458359,#458360,#458361,#458362,#458363,#458364,
#458365,#458366,#458367,#458368,#458369,#458370,#458371,#458372,#458373,
#458374,#458375,#458376,#458377,#458378,#458379,#458380,#458381,#458382,
#458383,#458384,#458385,#458386,#458387,#458388,#458389,#458390,#458391,
#458392,#458393,#458394,#458395,#458396,#458397,#458398,#458399,#458400,
#458401,#458402,#458403,#458404,#458405,#458406),.UNSPECIFIED.,.F.,.F.,
(4,3,3,3,3,3,3,3,3,3,3,3,3,3,3,3,3,3,3,3,3,3,3,3,3,3,3,3,3,3,4),(0.,0.0236685322934883,
0.0528063043594954,0.0823663722021023,0.10994332106008,0.115411373478116,
0.144160926034357,0.172814778868534,0.200972611163827,0.213723780151589,
0.219404722989038,0.223657093795748,0.251236282026945,0.278024931664471,
0.302981963065925,0.318750139649266,0.324728551834005,0.329044372404637,
0.355724072542136,0.382823307195456,0.405976538950344,0.418034991670282,
0.425032985649591,0.429596993938966,0.4558996039235,0.480742900042471,0.487661128902617,
0.494570456238806,0.519844325943088,0.544403481761064,0.555272788399383),
 .UNSPECIFIED.);
#27038=B_SPLINE_CURVE_WITH_KNOTS('',3,(#458407,#458408,#458409,#458410,
#458411,#458412,#458413,#458414,#458415,#458416,#458417,#458418,#458419,
#458420,#458421,#458422,#458423,#458424,#458425),.UNSPECIFIED.,.F.,.F.,
(4,3,3,3,3,3,4),(32.5332269442662,32.808393764839,33.8025875152886,34.7967812657383,
35.790975016188,36.7851687666376,37.6991118430775),.UNSPECIFIED.);
#27039=B_SPLINE_CURVE_WITH_KNOTS('',3,(#458427,#458428,#458429,#458430,
#458431,#458432,#458433,#458434,#458435,#458436,#458437,#458438,#458439,
#458440,#458441,#458442,#458443,#458444,#458445,#458446,#458447,#458448,
#458449,#458450,#458451,#458452,#458453,#458454,#458455,#458456,#458457,
#458458,#458459,#458460,#458461,#458462,#458463,#458464,#458465,#458466,
#458467,#458468,#458469,#458470,#458471,#458472,#458473,#458474,#458475,
#458476,#458477,#458478,#458479,#458480,#458481,#458482,#458483,#458484,
#458485,#458486,#458487,#458488,#458489,#458490,#458491,#458492,#458493,
#458494,#458495,#458496,#458497,#458498,#458499),.UNSPECIFIED.,.F.,.F.,
(4,3,3,3,3,3,3,3,3,3,3,3,3,3,3,3,3,3,3,3,3,3,3,3,4),(0.114320004474185,
0.140646463311683,0.167305683383212,0.18050501793273,0.187500493757846,
0.191912134086234,0.195940743293992,0.223365066923526,0.250708382555933,
0.272900359779356,0.290390673441587,0.294837891004841,0.321589376711389,
0.349039104275635,0.37712868962266,0.38893376768078,0.397785923814993,0.403780458706632,
0.432556793723188,0.462603939886154,0.47221559599953,0.479349893094354,
0.508920882024724,0.53812271524797,0.552745378375053),.UNSPECIFIED.);
#27040=B_SPLINE_CURVE_WITH_KNOTS('',3,(#458501,#458502,#458503,#458504,
#458505,#458506,#458507,#458508,#458509,#458510,#458511,#458512,#458513,
#458514,#458515,#458516,#458517,#458518,#458519),.UNSPECIFIED.,.F.,.F.,
(4,3,3,3,3,3,4),(-0.555272788399385,-0.535926974079205,-0.51210059511606,
-0.492977818526996,-0.487964619258994,-0.462250939529163,-0.440621458226625),
 .UNSPECIFIED.);
#27041=B_SPLINE_CURVE_WITH_KNOTS('',3,(#458520,#458521,#458522,#458523,
#458524,#458525,#458526,#458527,#458528),.UNSPECIFIED.,.F.,.F.,(4,1,1,1,
1,1,4),(10.3761157273102,11.2900588037501,12.2842525541997,13.2784463046494,
14.2726400550991,15.2668338055487,15.7079632679489),.UNSPECIFIED.);
#27042=B_SPLINE_CURVE_WITH_KNOTS('',3,(#458533,#458534,#458535,#458536,
#458537,#458538,#458539,#458540,#458541,#458542,#458543,#458544,#458545,
#458546,#458547,#458548,#458549,#458550,#458551,#458552,#458553,#458554),
 .UNSPECIFIED.,.F.,.F.,(4,3,3,3,3,3,3,4),(-0.114320004469662,-0.100030003910954,
-0.0951255454647728,-0.0911591016833673,-0.0656020317264686,-0.040440074691218,
-0.0160653357605578,0.),.UNSPECIFIED.);
#27043=B_SPLINE_CURVE_WITH_KNOTS('',3,(#458557,#458558,#458559,#458560,
#458561,#458562,#458563,#458564),.UNSPECIFIED.,.F.,.F.,(4,1,1,1,1,4),(11.6150328478183,
12.609226598268,13.6034203487176,14.5976140991673,15.591807849617,15.707963267949),
 .UNSPECIFIED.);
#27044=B_SPLINE_CURVE_WITH_KNOTS('',3,(#458738,#458739,#458740,#458741,
#458742,#458743,#458744,#458745,#458746,#458747,#458748,#458749,#458750,
#458751,#458752,#458753,#458754,#458755,#458756,#458757,#458758,#458759,
#458760,#458761,#458762,#458763,#458764,#458765,#458766,#458767,#458768,
#458769,#458770,#458771,#458772,#458773,#458774,#458775,#458776,#458777,
#458778,#458779,#458780,#458781,#458782,#458783,#458784,#458785,#458786,
#458787,#458788,#458789,#458790,#458791,#458792,#458793,#458794,#458795,
#458796,#458797,#458798,#458799,#458800,#458801,#458802,#458803,#458804,
#458805,#458806,#458807,#458808,#458809,#458810,#458811,#458812,#458813,
#458814,#458815,#458816,#458817,#458818,#458819,#458820,#458821,#458822,
#458823,#458824,#458825),.UNSPECIFIED.,.F.,.F.,(4,3,3,3,3,3,3,3,3,3,3,3,
3,3,3,3,3,3,3,3,3,3,3,3,3,3,3,3,3,4),(0.,0.0192795947675992,0.0437654770936498,
0.0688779034214175,0.0817182074062708,0.0920073560018174,0.0968850155838629,
0.122826629537411,0.149299742410276,0.175980044535411,0.188287552210521,
0.192556368324891,0.219948063244321,0.247318645394406,0.272900359779344,
0.290390673441576,0.294837892322343,0.32158936959522,0.349039080657507,
0.377128651170303,0.388933697533704,0.397785724695364,0.403780440790509,
0.432556758586858,0.462603913533905,0.472215531591236,0.479349897615772,
0.508920886911059,0.538122756943474,0.552745378375047),.UNSPECIFIED.);
#27045=B_SPLINE_CURVE_WITH_KNOTS('',3,(#458826,#458827,#458828,#458829,
#458830,#458831,#458832,#458833,#458834,#458835,#458836,#458837,#458838,
#458839,#458840,#458841,#458842,#458843,#458844,#458845,#458846,#458847,
#458848,#458849,#458850,#458851,#458852,#458853,#458854,#458855,#458856,
#458857,#458858,#458859,#458860,#458861,#458862,#458863,#458864,#458865,
#458866,#458867,#458868,#458869,#458870,#458871,#458872,#458873,#458874,
#458875,#458876,#458877,#458878,#458879,#458880,#458881,#458882,#458883,
#458884,#458885,#458886,#458887,#458888,#458889,#458890,#458891,#458892),
 .UNSPECIFIED.,.F.,.F.,(4,3,3,3,3,3,3,3,3,3,3,3,3,3,3,3,3,3,3,3,3,3,4),
(0.,0.0236685322934977,0.052806299380084,0.0823663677191272,0.109943317137477,
0.115411369379879,0.144160922017529,0.172814764059765,0.200972567173901,
0.213723741660404,0.219404591129717,0.223657014160771,0.251236182714427,
0.2780247885744,0.30298196306593,0.318260936745704,0.323323365654122,0.327783619094247,
0.35466098512014,0.381765497654677,0.408577737768497,0.425213752504124,
0.440621458226614),.UNSPECIFIED.);
#27046=B_SPLINE_CURVE_WITH_KNOTS('',3,(#458893,#458894,#458895,#458896,
#458897,#458898,#458899,#458900,#458901,#458902,#458903,#458904,#458905,
#458906,#458907,#458908),.UNSPECIFIED.,.F.,.F.,(4,3,3,3,3,4),(-39.7677500179866,
-38.773556267537,-37.7793625170873,-36.7851687666377,-35.790975016188,-35.5088569560286),
 .UNSPECIFIED.);
#27047=LINE('',#130725,#30849);
#27048=LINE('',#130906,#30850);
#27049=LINE('',#131282,#30851);
#27050=LINE('',#131640,#30852);
#27051=LINE('',#131813,#30853);
#27052=LINE('',#131996,#30854);
#27053=LINE('',#132368,#30855);
#27054=LINE('',#132726,#30856);
#27055=LINE('',#132897,#30857);
#27056=LINE('',#133014,#30858);
#27057=LINE('',#133308,#30859);
#27058=LINE('',#133661,#30860);
#27059=LINE('',#133852,#30861);
#27060=LINE('',#133971,#30862);
#27061=LINE('',#134267,#30863);
#27062=LINE('',#134620,#30864);
#27063=LINE('',#136631,#30865);
#27064=LINE('',#136635,#30866);
#27065=LINE('',#137151,#30867);
#27066=LINE('',#137155,#30868);
#27067=LINE('',#137165,#30869);
#27068=LINE('',#137169,#30870);
#27069=LINE('',#137179,#30871);
#27070=LINE('',#137183,#30872);
#27071=LINE('',#137190,#30873);
#27072=LINE('',#137194,#30874);
#27073=LINE('',#137205,#30875);
#27074=LINE('',#137209,#30876);
#27075=LINE('',#137222,#30877);
#27076=LINE('',#137228,#30878);
#27077=LINE('',#137236,#30879);
#27078=LINE('',#137243,#30880);
#27079=LINE('',#137246,#30881);
#27080=LINE('',#137249,#30882);
#27081=LINE('',#137253,#30883);
#27082=LINE('',#137254,#30884);
#27083=LINE('',#137257,#30885);
#27084=LINE('',#137261,#30886);
#27085=LINE('',#137262,#30887);
#27086=LINE('',#137267,#30888);
#27087=LINE('',#137271,#30889);
#27088=LINE('',#137272,#30890);
#27089=LINE('',#137275,#30891);
#27090=LINE('',#137279,#30892);
#27091=LINE('',#137280,#30893);
#27092=LINE('',#137286,#30894);
#27093=LINE('',#137288,#30895);
#27094=LINE('',#137290,#30896);
#27095=LINE('',#137291,#30897);
#27096=LINE('',#137295,#30898);
#27097=LINE('',#137301,#30899);
#27098=LINE('',#137302,#30900);
#27099=LINE('',#137303,#30901);
#27100=LINE('',#137306,#30902);
#27101=LINE('',#137311,#30903);
#27102=LINE('',#137316,#30904);
#27103=LINE('',#137321,#30905);
#27104=LINE('',#137323,#30906);
#27105=LINE('',#137324,#30907);
#27106=LINE('',#137328,#30908);
#27107=LINE('',#137333,#30909);
#27108=LINE('',#137335,#30910);
#27109=LINE('',#137336,#30911);
#27110=LINE('',#137339,#30912);
#27111=LINE('',#137344,#30913);
#27112=LINE('',#137350,#30914);
#27113=LINE('',#137351,#30915);
#27114=LINE('',#137353,#30916);
#27115=LINE('',#137356,#30917);
#27116=LINE('',#137358,#30918);
#27117=LINE('',#137361,#30919);
#27118=LINE('',#137363,#30920);
#27119=LINE('',#137365,#30921);
#27120=LINE('',#137370,#30922);
#27121=LINE('',#137374,#30923);
#27122=LINE('',#137381,#30924);
#27123=LINE('',#137399,#30925);
#27124=LINE('',#137403,#30926);
#27125=LINE('',#137421,#30927);
#27126=LINE('',#137425,#30928);
#27127=LINE('',#137443,#30929);
#27128=LINE('',#137447,#30930);
#27129=LINE('',#137465,#30931);
#27130=LINE('',#137469,#30932);
#27131=LINE('',#137487,#30933);
#27132=LINE('',#137491,#30934);
#27133=LINE('',#137509,#30935);
#27134=LINE('',#137513,#30936);
#27135=LINE('',#137531,#30937);
#27136=LINE('',#137535,#30938);
#27137=LINE('',#137553,#30939);
#27138=LINE('',#137557,#30940);
#27139=LINE('',#137575,#30941);
#27140=LINE('',#137579,#30942);
#27141=LINE('',#137596,#30943);
#27142=LINE('',#137603,#30944);
#27143=LINE('',#137621,#30945);
#27144=LINE('',#137625,#30946);
#27145=LINE('',#137643,#30947);
#27146=LINE('',#137647,#30948);
#27147=LINE('',#137665,#30949);
#27148=LINE('',#137669,#30950);
#27149=LINE('',#137687,#30951);
#27150=LINE('',#137691,#30952);
#27151=LINE('',#137709,#30953);
#27152=LINE('',#137713,#30954);
#27153=LINE('',#137731,#30955);
#27154=LINE('',#137735,#30956);
#27155=LINE('',#137753,#30957);
#27156=LINE('',#137757,#30958);
#27157=LINE('',#137775,#30959);
#27158=LINE('',#137779,#30960);
#27159=LINE('',#137797,#30961);
#27160=LINE('',#137801,#30962);
#27161=LINE('',#137818,#30963);
#27162=LINE('',#137822,#30964);
#27163=LINE('',#137823,#30965);
#27164=LINE('',#137836,#30966);
#27165=LINE('',#137838,#30967);
#27166=LINE('',#137851,#30968);
#27167=LINE('',#137853,#30969);
#27168=LINE('',#137855,#30970);
#27169=LINE('',#137857,#30971);
#27170=LINE('',#137859,#30972);
#27171=LINE('',#137860,#30973);
#27172=LINE('',#137873,#30974);
#27173=LINE('',#137875,#30975);
#27174=LINE('',#137888,#30976);
#27175=LINE('',#137891,#30977);
#27176=LINE('',#137893,#30978);
#27177=LINE('',#137894,#30979);
#27178=LINE('',#137907,#30980);
#27179=LINE('',#137909,#30981);
#27180=LINE('',#137922,#30982);
#27181=LINE('',#137925,#30983);
#27182=LINE('',#137927,#30984);
#27183=LINE('',#137928,#30985);
#27184=LINE('',#137941,#30986);
#27185=LINE('',#137943,#30987);
#27186=LINE('',#137956,#30988);
#27187=LINE('',#137959,#30989);
#27188=LINE('',#137961,#30990);
#27189=LINE('',#137962,#30991);
#27190=LINE('',#137975,#30992);
#27191=LINE('',#137977,#30993);
#27192=LINE('',#137990,#30994);
#27193=LINE('',#137993,#30995);
#27194=LINE('',#137995,#30996);
#27195=LINE('',#137996,#30997);
#27196=LINE('',#138009,#30998);
#27197=LINE('',#138011,#30999);
#27198=LINE('',#138024,#31000);
#27199=LINE('',#138027,#31001);
#27200=LINE('',#138029,#31002);
#27201=LINE('',#138030,#31003);
#27202=LINE('',#138043,#31004);
#27203=LINE('',#138045,#31005);
#27204=LINE('',#138058,#31006);
#27205=LINE('',#138061,#31007);
#27206=LINE('',#138063,#31008);
#27207=LINE('',#138064,#31009);
#27208=LINE('',#138077,#31010);
#27209=LINE('',#138079,#31011);
#27210=LINE('',#138092,#31012);
#27211=LINE('',#138095,#31013);
#27212=LINE('',#138097,#31014);
#27213=LINE('',#138098,#31015);
#27214=LINE('',#138111,#31016);
#27215=LINE('',#138113,#31017);
#27216=LINE('',#138126,#31018);
#27217=LINE('',#138129,#31019);
#27218=LINE('',#138131,#31020);
#27219=LINE('',#138144,#31021);
#27220=LINE('',#138146,#31022);
#27221=LINE('',#138159,#31023);
#27222=LINE('',#138166,#31024);
#27223=LINE('',#138173,#31025);
#27224=LINE('',#138177,#31026);
#27225=LINE('',#138182,#31027);
#27226=LINE('',#138188,#31028);
#27227=LINE('',#138192,#31029);
#27228=LINE('',#138195,#31030);
#27229=LINE('',#138204,#31031);
#27230=LINE('',#138208,#31032);
#27231=LINE('',#138211,#31033);
#27232=LINE('',#138220,#31034);
#27233=LINE('',#138224,#31035);
#27234=LINE('',#138227,#31036);
#27235=LINE('',#138236,#31037);
#27236=LINE('',#138240,#31038);
#27237=LINE('',#138243,#31039);
#27238=LINE('',#138252,#31040);
#27239=LINE('',#138256,#31041);
#27240=LINE('',#138259,#31042);
#27241=LINE('',#138268,#31043);
#27242=LINE('',#138272,#31044);
#27243=LINE('',#138275,#31045);
#27244=LINE('',#138284,#31046);
#27245=LINE('',#138288,#31047);
#27246=LINE('',#138291,#31048);
#27247=LINE('',#138300,#31049);
#27248=LINE('',#138304,#31050);
#27249=LINE('',#138307,#31051);
#27250=LINE('',#138316,#31052);
#27251=LINE('',#138320,#31053);
#27252=LINE('',#138323,#31054);
#27253=LINE('',#138332,#31055);
#27254=LINE('',#138336,#31056);
#27255=LINE('',#138339,#31057);
#27256=LINE('',#138348,#31058);
#27257=LINE('',#138352,#31059);
#27258=LINE('',#138355,#31060);
#27259=LINE('',#138364,#31061);
#27260=LINE('',#138368,#31062);
#27261=LINE('',#138371,#31063);
#27262=LINE('',#138380,#31064);
#27263=LINE('',#138384,#31065);
#27264=LINE('',#138388,#31066);
#27265=LINE('',#138398,#31067);
#27266=LINE('',#138401,#31068);
#27267=LINE('',#138403,#31069);
#27268=LINE('',#138405,#31070);
#27269=LINE('',#138412,#31071);
#27270=LINE('',#138416,#31072);
#27271=LINE('',#138421,#31073);
#27272=LINE('',#138425,#31074);
#27273=LINE('',#138430,#31075);
#27274=LINE('',#138434,#31076);
#27275=LINE('',#138498,#31077);
#27276=LINE('',#138501,#31078);
#27277=LINE('',#138504,#31079);
#27278=LINE('',#138506,#31080);
#27279=LINE('',#138510,#31081);
#27280=LINE('',#138512,#31082);
#27281=LINE('',#138518,#31083);
#27282=LINE('',#138521,#31084);
#27283=LINE('',#138523,#31085);
#27284=LINE('',#138526,#31086);
#27285=LINE('',#138528,#31087);
#27286=LINE('',#138531,#31088);
#27287=LINE('',#138533,#31089);
#27288=LINE('',#138537,#31090);
#27289=LINE('',#138541,#31091);
#27290=LINE('',#138545,#31092);
#27291=LINE('',#138548,#31093);
#27292=LINE('',#138571,#31094);
#27293=LINE('',#138574,#31095);
#27294=LINE('',#138580,#31096);
#27295=LINE('',#138584,#31097);
#27296=LINE('',#138586,#31098);
#27297=LINE('',#138589,#31099);
#27298=LINE('',#138591,#31100);
#27299=LINE('',#138594,#31101);
#27300=LINE('',#138596,#31102);
#27301=LINE('',#138599,#31103);
#27302=LINE('',#138600,#31104);
#27303=LINE('',#138606,#31105);
#27304=LINE('',#138610,#31106);
#27305=LINE('',#138612,#31107);
#27306=LINE('',#138615,#31108);
#27307=LINE('',#138617,#31109);
#27308=LINE('',#138620,#31110);
#27309=LINE('',#138622,#31111);
#27310=LINE('',#138625,#31112);
#27311=LINE('',#138627,#31113);
#27312=LINE('',#138634,#31114);
#27313=LINE('',#138637,#31115);
#27314=LINE('',#138640,#31116);
#27315=LINE('',#138642,#31117);
#27316=LINE('',#138643,#31118);
#27317=LINE('',#138650,#31119);
#27318=LINE('',#138656,#31120);
#27319=LINE('',#138658,#31121);
#27320=LINE('',#138660,#31122);
#27321=LINE('',#138667,#31123);
#27322=LINE('',#138670,#31124);
#27323=LINE('',#138676,#31125);
#27324=LINE('',#138677,#31126);
#27325=LINE('',#138684,#31127);
#27326=LINE('',#138685,#31128);
#27327=LINE('',#138689,#31129);
#27328=LINE('',#138692,#31130);
#27329=LINE('',#138694,#31131);
#27330=LINE('',#138695,#31132);
#27331=LINE('',#138698,#31133);
#27332=LINE('',#138700,#31134);
#27333=LINE('',#138701,#31135);
#27334=LINE('',#138704,#31136);
#27335=LINE('',#138706,#31137);
#27336=LINE('',#138707,#31138);
#27337=LINE('',#138709,#31139);
#27338=LINE('',#138711,#31140);
#27339=LINE('',#138713,#31141);
#27340=LINE('',#138721,#31142);
#27341=LINE('',#138724,#31143);
#27342=LINE('',#138821,#31144);
#27343=LINE('',#138822,#31145);
#27344=LINE('',#138836,#31146);
#27345=LINE('',#138840,#31147);
#27346=LINE('',#138844,#31148);
#27347=LINE('',#138854,#31149);
#27348=LINE('',#138857,#31150);
#27349=LINE('',#138860,#31151);
#27350=LINE('',#138864,#31152);
#27351=LINE('',#138865,#31153);
#27352=LINE('',#138868,#31154);
#27353=LINE('',#138872,#31155);
#27354=LINE('',#138873,#31156);
#27355=LINE('',#138880,#31157);
#27356=LINE('',#138883,#31158);
#27357=LINE('',#138928,#31159);
#27358=LINE('',#138929,#31160);
#27359=LINE('',#138948,#31161);
#27360=LINE('',#138949,#31162);
#27361=LINE('',#138960,#31163);
#27362=LINE('',#138961,#31164);
#27363=LINE('',#139023,#31165);
#27364=LINE('',#139025,#31166);
#27365=LINE('',#139026,#31167);
#27366=LINE('',#139029,#31168);
#27367=LINE('',#139033,#31169);
#27368=LINE('',#139037,#31170);
#27369=LINE('',#139042,#31171);
#27370=LINE('',#139044,#31172);
#27371=LINE('',#139048,#31173);
#27372=LINE('',#139052,#31174);
#27373=LINE('',#139056,#31175);
#27374=LINE('',#139060,#31176);
#27375=LINE('',#139064,#31177);
#27376=LINE('',#139068,#31178);
#27377=LINE('',#139069,#31179);
#27378=LINE('',#139098,#31180);
#27379=LINE('',#139099,#31181);
#27380=LINE('',#139124,#31182);
#27381=LINE('',#139125,#31183);
#27382=LINE('',#139170,#31184);
#27383=LINE('',#139171,#31185);
#27384=LINE('',#139202,#31186);
#27385=LINE('',#139206,#31187);
#27386=LINE('',#139209,#31188);
#27387=LINE('',#139212,#31189);
#27388=LINE('',#139213,#31190);
#27389=LINE('',#139218,#31191);
#27390=LINE('',#139222,#31192);
#27391=LINE('',#139230,#31193);
#27392=LINE('',#139233,#31194);
#27393=LINE('',#139284,#31195);
#27394=LINE('',#139285,#31196);
#27395=LINE('',#139316,#31197);
#27396=LINE('',#139317,#31198);
#27397=LINE('',#139331,#31199);
#27398=LINE('',#139333,#31200);
#27399=LINE('',#139335,#31201);
#27400=LINE('',#139337,#31202);
#27401=LINE('',#139338,#31203);
#27402=LINE('',#139341,#31204);
#27403=LINE('',#139345,#31205);
#27404=LINE('',#139349,#31206);
#27405=LINE('',#139350,#31207);
#27406=LINE('',#139353,#31208);
#27407=LINE('',#139357,#31209);
#27408=LINE('',#139359,#31210);
#27409=LINE('',#139361,#31211);
#27410=LINE('',#139362,#31212);
#27411=LINE('',#139429,#31213);
#27412=LINE('',#139430,#31214);
#27413=LINE('',#139441,#31215);
#27414=LINE('',#139442,#31216);
#27415=LINE('',#139461,#31217);
#27416=LINE('',#139462,#31218);
#27417=LINE('',#139510,#31219);
#27418=LINE('',#139511,#31220);
#27419=LINE('',#139514,#31221);
#27420=LINE('',#139517,#31222);
#27421=LINE('',#139520,#31223);
#27422=LINE('',#139521,#31224);
#27423=LINE('',#139524,#31225);
#27424=LINE('',#139528,#31226);
#27425=LINE('',#139532,#31227);
#27426=LINE('',#139536,#31228);
#27427=LINE('',#139537,#31229);
#27428=LINE('',#139540,#31230);
#27429=LINE('',#139628,#31231);
#27430=LINE('',#139629,#31232);
#27431=LINE('',#139643,#31233);
#27432=LINE('',#139646,#31234);
#27433=LINE('',#139649,#31235);
#27434=LINE('',#139653,#31236);
#27435=LINE('',#139654,#31237);
#27436=LINE('',#139657,#31238);
#27437=LINE('',#139661,#31239);
#27438=LINE('',#139723,#31240);
#27439=LINE('',#139724,#31241);
#27440=LINE('',#139749,#31242);
#27441=LINE('',#139750,#31243);
#27442=LINE('',#139769,#31244);
#27443=LINE('',#139770,#31245);
#27444=LINE('',#139830,#31246);
#27445=LINE('',#139833,#31247);
#27446=LINE('',#139836,#31248);
#27447=LINE('',#139837,#31249);
#27448=LINE('',#139840,#31250);
#27449=LINE('',#139844,#31251);
#27450=LINE('',#139848,#31252);
#27451=LINE('',#139852,#31253);
#27452=LINE('',#139856,#31254);
#27453=LINE('',#139860,#31255);
#27454=LINE('',#139864,#31256);
#27455=LINE('',#139906,#31257);
#27456=LINE('',#139907,#31258);
#27457=LINE('',#139973,#31259);
#27458=LINE('',#139977,#31260);
#27459=LINE('',#139981,#31261);
#27460=LINE('',#139984,#31262);
#27461=LINE('',#139987,#31263);
#27462=LINE('',#139991,#31264);
#27463=LINE('',#139995,#31265);
#27464=LINE('',#139999,#31266);
#27465=LINE('',#140007,#31267);
#27466=LINE('',#140010,#31268);
#27467=LINE('',#140029,#31269);
#27468=LINE('',#140030,#31270);
#27469=LINE('',#140102,#31271);
#27470=LINE('',#140105,#31272);
#27471=LINE('',#140108,#31273);
#27472=LINE('',#140112,#31274);
#27473=LINE('',#140116,#31275);
#27474=LINE('',#140117,#31276);
#27475=LINE('',#140329,#31277);
#27476=LINE('',#140333,#31278);
#27477=LINE('',#140337,#31279);
#27478=LINE('',#140360,#31280);
#27479=LINE('',#140364,#31281);
#27480=LINE('',#140368,#31282);
#27481=LINE('',#140389,#31283);
#27482=LINE('',#140392,#31284);
#27483=LINE('',#140396,#31285);
#27484=LINE('',#140398,#31286);
#27485=LINE('',#140400,#31287);
#27486=LINE('',#140405,#31288);
#27487=LINE('',#140407,#31289);
#27488=LINE('',#140409,#31290);
#27489=LINE('',#140410,#31291);
#27490=LINE('',#140416,#31292);
#27491=LINE('',#140419,#31293);
#27492=LINE('',#140424,#31294);
#27493=LINE('',#140427,#31295);
#27494=LINE('',#140431,#31296);
#27495=LINE('',#140435,#31297);
#27496=LINE('',#140450,#31298);
#27497=LINE('',#140454,#31299);
#27498=LINE('',#140456,#31300);
#27499=LINE('',#140458,#31301);
#27500=LINE('',#140462,#31302);
#27501=LINE('',#140465,#31303);
#27502=LINE('',#140471,#31304);
#27503=LINE('',#140474,#31305);
#27504=LINE('',#140478,#31306);
#27505=LINE('',#140482,#31307);
#27506=LINE('',#140486,#31308);
#27507=LINE('',#140501,#31309);
#27508=LINE('',#140504,#31310);
#27509=LINE('',#140508,#31311);
#27510=LINE('',#140517,#31312);
#27511=LINE('',#140522,#31313);
#27512=LINE('',#140524,#31314);
#27513=LINE('',#140525,#31315);
#27514=LINE('',#140528,#31316);
#27515=LINE('',#140531,#31317);
#27516=LINE('',#140534,#31318);
#27517=LINE('',#140535,#31319);
#27518=LINE('',#140538,#31320);
#27519=LINE('',#140543,#31321);
#27520=LINE('',#140547,#31322);
#27521=LINE('',#140552,#31323);
#27522=LINE('',#140556,#31324);
#27523=LINE('',#140562,#31325);
#27524=LINE('',#140568,#31326);
#27525=LINE('',#140572,#31327);
#27526=LINE('',#140576,#31328);
#27527=LINE('',#140580,#31329);
#27528=LINE('',#140584,#31330);
#27529=LINE('',#140593,#31331);
#27530=LINE('',#140596,#31332);
#27531=LINE('',#140598,#31333);
#27532=LINE('',#140605,#31334);
#27533=LINE('',#140608,#31335);
#27534=LINE('',#140611,#31336);
#27535=LINE('',#140614,#31337);
#27536=LINE('',#140619,#31338);
#27537=LINE('',#140622,#31339);
#27538=LINE('',#140626,#31340);
#27539=LINE('',#140630,#31341);
#27540=LINE('',#140632,#31342);
#27541=LINE('',#140638,#31343);
#27542=LINE('',#140641,#31344);
#27543=LINE('',#140648,#31345);
#27544=LINE('',#140651,#31346);
#27545=LINE('',#140654,#31347);
#27546=LINE('',#140655,#31348);
#27547=LINE('',#140674,#31349);
#27548=LINE('',#140678,#31350);
#27549=LINE('',#140682,#31351);
#27550=LINE('',#140684,#31352);
#27551=LINE('',#140685,#31353);
#27552=LINE('',#140687,#31354);
#27553=LINE('',#140689,#31355);
#27554=LINE('',#140691,#31356);
#27555=LINE('',#140692,#31357);
#27556=LINE('',#140694,#31358);
#27557=LINE('',#140696,#31359);
#27558=LINE('',#140698,#31360);
#27559=LINE('',#140700,#31361);
#27560=LINE('',#140704,#31362);
#27561=LINE('',#140707,#31363);
#27562=LINE('',#140710,#31364);
#27563=LINE('',#140716,#31365);
#27564=LINE('',#140719,#31366);
#27565=LINE('',#140722,#31367);
#27566=LINE('',#140725,#31368);
#27567=LINE('',#140727,#31369);
#27568=LINE('',#140730,#31370);
#27569=LINE('',#140732,#31371);
#27570=LINE('',#140734,#31372);
#27571=LINE('',#140740,#31373);
#27572=LINE('',#140741,#31374);
#27573=LINE('',#140743,#31375);
#27574=LINE('',#140745,#31376);
#27575=LINE('',#140747,#31377);
#27576=LINE('',#140749,#31378);
#27577=LINE('',#140752,#31379);
#27578=LINE('',#140753,#31380);
#27579=LINE('',#140755,#31381);
#27580=LINE('',#140758,#31382);
#27581=LINE('',#140761,#31383);
#27582=LINE('',#140765,#31384);
#27583=LINE('',#140768,#31385);
#27584=LINE('',#140770,#31386);
#27585=LINE('',#140771,#31387);
#27586=LINE('',#140779,#31388);
#27587=LINE('',#140781,#31389);
#27588=LINE('',#140789,#31390);
#27589=LINE('',#140792,#31391);
#27590=LINE('',#140801,#31392);
#27591=LINE('',#140806,#31393);
#27592=LINE('',#140808,#31394);
#27593=LINE('',#140809,#31395);
#27594=LINE('',#140812,#31396);
#27595=LINE('',#140817,#31397);
#27596=LINE('',#140818,#31398);
#27597=LINE('',#140820,#31399);
#27598=LINE('',#140823,#31400);
#27599=LINE('',#140824,#31401);
#27600=LINE('',#140826,#31402);
#27601=LINE('',#140828,#31403);
#27602=LINE('',#140830,#31404);
#27603=LINE('',#140833,#31405);
#27604=LINE('',#140835,#31406);
#27605=LINE('',#140837,#31407);
#27606=LINE('',#140843,#31408);
#27607=LINE('',#140849,#31409);
#27608=LINE('',#140851,#31410);
#27609=LINE('',#140855,#31411);
#27610=LINE('',#140859,#31412);
#27611=LINE('',#140867,#31413);
#27612=LINE('',#140871,#31414);
#27613=LINE('',#140873,#31415);
#27614=LINE('',#140883,#31416);
#27615=LINE('',#140888,#31417);
#27616=LINE('',#140891,#31418);
#27617=LINE('',#140894,#31419);
#27618=LINE('',#140897,#31420);
#27619=LINE('',#140898,#31421);
#27620=LINE('',#140901,#31422);
#27621=LINE('',#140907,#31423);
#27622=LINE('',#140908,#31424);
#27623=LINE('',#140911,#31425);
#27624=LINE('',#140912,#31426);
#27625=LINE('',#140916,#31427);
#27626=LINE('',#140918,#31428);
#27627=LINE('',#140923,#31429);
#27628=LINE('',#140927,#31430);
#27629=LINE('',#140931,#31431);
#27630=LINE('',#140936,#31432);
#27631=LINE('',#140937,#31433);
#27632=LINE('',#140940,#31434);
#27633=LINE('',#140941,#31435);
#27634=LINE('',#140951,#31436);
#27635=LINE('',#140953,#31437);
#27636=LINE('',#140956,#31438);
#27637=LINE('',#140959,#31439);
#27638=LINE('',#140961,#31440);
#27639=LINE('',#140963,#31441);
#27640=LINE('',#140965,#31442);
#27641=LINE('',#140967,#31443);
#27642=LINE('',#140969,#31444);
#27643=LINE('',#140971,#31445);
#27644=LINE('',#140973,#31446);
#27645=LINE('',#140975,#31447);
#27646=LINE('',#140999,#31448);
#27647=LINE('',#141002,#31449);
#27648=LINE('',#141004,#31450);
#27649=LINE('',#141005,#31451);
#27650=LINE('',#141011,#31452);
#27651=LINE('',#141018,#31453);
#27652=LINE('',#141021,#31454);
#27653=LINE('',#141028,#31455);
#27654=LINE('',#141032,#31456);
#27655=LINE('',#141040,#31457);
#27656=LINE('',#141044,#31458);
#27657=LINE('',#141048,#31459);
#27658=LINE('',#141052,#31460);
#27659=LINE('',#141056,#31461);
#27660=LINE('',#141059,#31462);
#27661=LINE('',#141063,#31463);
#27662=LINE('',#141067,#31464);
#27663=LINE('',#141070,#31465);
#27664=LINE('',#141072,#31466);
#27665=LINE('',#141074,#31467);
#27666=LINE('',#141075,#31468);
#27667=LINE('',#141107,#31469);
#27668=LINE('',#141126,#31470);
#27669=LINE('',#141127,#31471);
#27670=LINE('',#141173,#31472);
#27671=LINE('',#141176,#31473);
#27672=LINE('',#141179,#31474);
#27673=LINE('',#141183,#31475);
#27674=LINE('',#141187,#31476);
#27675=LINE('',#141191,#31477);
#27676=LINE('',#141242,#31478);
#27677=LINE('',#141243,#31479);
#27678=LINE('',#141294,#31480);
#27679=LINE('',#141295,#31481);
#27680=LINE('',#141298,#31482);
#27681=LINE('',#141301,#31483);
#27682=LINE('',#141304,#31484);
#27683=LINE('',#141308,#31485);
#27684=LINE('',#141309,#31486);
#27685=LINE('',#141312,#31487);
#27686=LINE('',#141401,#31488);
#27687=LINE('',#141408,#31489);
#27688=LINE('',#141415,#31490);
#27689=LINE('',#141419,#31491);
#27690=LINE('',#141454,#31492);
#27691=LINE('',#141457,#31493);
#27692=LINE('',#141472,#31494);
#27693=LINE('',#141510,#31495);
#27694=LINE('',#141513,#31496);
#27695=LINE('',#141516,#31497);
#27696=LINE('',#141518,#31498);
#27697=LINE('',#141524,#31499);
#27698=LINE('',#141530,#31500);
#27699=LINE('',#141545,#31501);
#27700=LINE('',#141560,#31502);
#27701=LINE('',#141563,#31503);
#27702=LINE('',#141569,#31504);
#27703=LINE('',#141577,#31505);
#27704=LINE('',#141596,#31506);
#27705=LINE('',#141598,#31507);
#27706=LINE('',#141600,#31508);
#27707=LINE('',#141602,#31509);
#27708=LINE('',#141603,#31510);
#27709=LINE('',#141605,#31511);
#27710=LINE('',#141607,#31512);
#27711=LINE('',#141609,#31513);
#27712=LINE('',#141611,#31514);
#27713=LINE('',#141616,#31515);
#27714=LINE('',#141619,#31516);
#27715=LINE('',#141622,#31517);
#27716=LINE('',#141626,#31518);
#27717=LINE('',#141627,#31519);
#27718=LINE('',#141630,#31520);
#27719=LINE('',#141636,#31521);
#27720=LINE('',#141637,#31522);
#27721=LINE('',#141704,#31523);
#27722=LINE('',#141706,#31524);
#27723=LINE('',#141709,#31525);
#27724=LINE('',#141710,#31526);
#27725=LINE('',#141713,#31527);
#27726=LINE('',#141717,#31528);
#27727=LINE('',#141719,#31529);
#27728=LINE('',#141720,#31530);
#27729=LINE('',#141723,#31531);
#27730=LINE('',#141730,#31532);
#27731=LINE('',#141732,#31533);
#27732=LINE('',#141745,#31534);
#27733=LINE('',#141839,#31535);
#27734=LINE('',#141843,#31536);
#27735=LINE('',#141846,#31537);
#27736=LINE('',#141850,#31538);
#27737=LINE('',#141866,#31539);
#27738=LINE('',#141882,#31540);
#27739=LINE('',#141899,#31541);
#27740=LINE('',#141903,#31542);
#27741=LINE('',#141915,#31543);
#27742=LINE('',#141919,#31544);
#27743=LINE('',#141923,#31545);
#27744=LINE('',#141924,#31546);
#27745=LINE('',#141927,#31547);
#27746=LINE('',#141931,#31548);
#27747=LINE('',#141932,#31549);
#27748=LINE('',#141935,#31550);
#27749=LINE('',#141939,#31551);
#27750=LINE('',#141940,#31552);
#27751=LINE('',#141943,#31553);
#27752=LINE('',#141974,#31554);
#27753=LINE('',#141978,#31555);
#27754=LINE('',#142028,#31556);
#27755=LINE('',#142064,#31557);
#27756=LINE('',#142065,#31558);
#27757=LINE('',#142076,#31559);
#27758=LINE('',#142077,#31560);
#27759=LINE('',#142136,#31561);
#27760=LINE('',#142137,#31562);
#27761=LINE('',#142145,#31563);
#27762=LINE('',#142147,#31564);
#27763=LINE('',#142148,#31565);
#27764=LINE('',#142151,#31566);
#27765=LINE('',#142155,#31567);
#27766=LINE('',#142156,#31568);
#27767=LINE('',#142159,#31569);
#27768=LINE('',#142163,#31570);
#27769=LINE('',#142167,#31571);
#27770=LINE('',#142175,#31572);
#27771=LINE('',#142178,#31573);
#27772=LINE('',#142197,#31574);
#27773=LINE('',#142198,#31575);
#27774=LINE('',#142229,#31576);
#27775=LINE('',#142230,#31577);
#27776=LINE('',#142281,#31578);
#27777=LINE('',#142282,#31579);
#27778=LINE('',#142296,#31580);
#27779=LINE('',#142299,#31581);
#27780=LINE('',#142302,#31582);
#27781=LINE('',#142306,#31583);
#27782=LINE('',#142310,#31584);
#27783=LINE('',#142311,#31585);
#27784=LINE('',#142314,#31586);
#27785=LINE('',#142318,#31587);
#27786=LINE('',#142319,#31588);
#27787=LINE('',#142326,#31589);
#27788=LINE('',#142329,#31590);
#27789=LINE('',#142348,#31591);
#27790=LINE('',#142349,#31592);
#27791=LINE('',#142368,#31593);
#27792=LINE('',#142369,#31594);
#27793=LINE('',#142427,#31595);
#27794=LINE('',#142430,#31596);
#27795=LINE('',#142433,#31597);
#27796=LINE('',#142437,#31598);
#27797=LINE('',#142441,#31599);
#27798=LINE('',#142445,#31600);
#27799=LINE('',#142449,#31601);
#27800=LINE('',#142522,#31602);
#27801=LINE('',#142526,#31603);
#27802=LINE('',#142530,#31604);
#27803=LINE('',#142531,#31605);
#27804=LINE('',#142603,#31606);
#27805=LINE('',#142605,#31607);
#27806=LINE('',#142608,#31608);
#27807=LINE('',#142615,#31609);
#27808=LINE('',#142619,#31610);
#27809=LINE('',#142622,#31611);
#27810=LINE('',#142627,#31612);
#27811=LINE('',#142631,#31613);
#27812=LINE('',#142633,#31614);
#27813=LINE('',#142636,#31615);
#27814=LINE('',#142656,#31616);
#27815=LINE('',#142660,#31617);
#27816=LINE('',#142675,#31618);
#27817=LINE('',#142696,#31619);
#27818=LINE('',#142711,#31620);
#27819=LINE('',#142725,#31621);
#27820=LINE('',#142731,#31622);
#27821=LINE('',#142734,#31623);
#27822=LINE('',#142745,#31624);
#27823=LINE('',#142746,#31625);
#27824=LINE('',#142797,#31626);
#27825=LINE('',#142798,#31627);
#27826=LINE('',#142839,#31628);
#27827=LINE('',#142840,#31629);
#27828=LINE('',#142860,#31630);
#27829=LINE('',#142863,#31631);
#27830=LINE('',#142867,#31632);
#27831=LINE('',#142869,#31633);
#27832=LINE('',#142873,#31634);
#27833=LINE('',#142877,#31635);
#27834=LINE('',#142881,#31636);
#27835=LINE('',#142885,#31637);
#27836=LINE('',#142889,#31638);
#27837=LINE('',#142893,#31639);
#27838=LINE('',#142894,#31640);
#27839=LINE('',#142897,#31641);
#27840=LINE('',#142901,#31642);
#27841=LINE('',#142902,#31643);
#27842=LINE('',#142944,#31644);
#27843=LINE('',#142945,#31645);
#27844=LINE('',#142964,#31646);
#27845=LINE('',#142965,#31647);
#27846=LINE('',#143001,#31648);
#27847=LINE('',#143002,#31649);
#27848=LINE('',#143059,#31650);
#27849=LINE('',#143061,#31651);
#27850=LINE('',#143062,#31652);
#27851=LINE('',#143065,#31653);
#27852=LINE('',#143098,#31654);
#27853=LINE('',#143101,#31655);
#27854=LINE('',#143105,#31656);
#27855=LINE('',#143169,#31657);
#27856=LINE('',#143173,#31658);
#27857=LINE('',#143176,#31659);
#27858=LINE('',#143211,#31660);
#27859=LINE('',#143212,#31661);
#27860=LINE('',#143248,#31662);
#27861=LINE('',#143249,#31663);
#27862=LINE('',#143268,#31664);
#27863=LINE('',#143269,#31665);
#27864=LINE('',#143283,#31666);
#27865=LINE('',#143285,#31667);
#27866=LINE('',#143286,#31668);
#27867=LINE('',#143289,#31669);
#27868=LINE('',#143293,#31670);
#27869=LINE('',#143294,#31671);
#27870=LINE('',#143297,#31672);
#27871=LINE('',#143301,#31673);
#27872=LINE('',#143305,#31674);
#27873=LINE('',#143309,#31675);
#27874=LINE('',#143357,#31676);
#27875=LINE('',#143362,#31677);
#27876=LINE('',#143366,#31678);
#27877=LINE('',#143367,#31679);
#27878=LINE('',#143372,#31680);
#27879=LINE('',#143381,#31681);
#27880=LINE('',#143384,#31682);
#27881=LINE('',#143387,#31683);
#27882=LINE('',#143389,#31684);
#27883=LINE('',#143391,#31685);
#27884=LINE('',#143393,#31686);
#27885=LINE('',#143395,#31687);
#27886=LINE('',#143397,#31688);
#27887=LINE('',#143398,#31689);
#27888=LINE('',#143401,#31690);
#27889=LINE('',#143403,#31691);
#27890=LINE('',#143404,#31692);
#27891=LINE('',#143410,#31693);
#27892=LINE('',#143416,#31694);
#27893=LINE('',#143422,#31695);
#27894=LINE('',#143428,#31696);
#27895=LINE('',#143432,#31697);
#27896=LINE('',#143434,#31698);
#27897=LINE('',#143435,#31699);
#27898=LINE('',#143441,#31700);
#27899=LINE('',#143450,#31701);
#27900=LINE('',#143454,#31702);
#27901=LINE('',#143457,#31703);
#27902=LINE('',#143459,#31704);
#27903=LINE('',#143461,#31705);
#27904=LINE('',#143463,#31706);
#27905=LINE('',#143465,#31707);
#27906=LINE('',#143467,#31708);
#27907=LINE('',#143469,#31709);
#27908=LINE('',#143471,#31710);
#27909=LINE('',#143472,#31711);
#27910=LINE('',#143475,#31712);
#27911=LINE('',#143479,#31713);
#27912=LINE('',#143487,#31714);
#27913=LINE('',#143494,#31715);
#27914=LINE('',#143497,#31716);
#27915=LINE('',#143500,#31717);
#27916=LINE('',#143502,#31718);
#27917=LINE('',#143503,#31719);
#27918=LINE('',#143506,#31720);
#27919=LINE('',#143510,#31721);
#27920=LINE('',#143512,#31722);
#27921=LINE('',#143513,#31723);
#27922=LINE('',#143518,#31724);
#27923=LINE('',#143525,#31725);
#27924=LINE('',#143528,#31726);
#27925=LINE('',#143536,#31727);
#27926=LINE('',#143542,#31728);
#27927=LINE('',#143547,#31729);
#27928=LINE('',#143551,#31730);
#27929=LINE('',#143575,#31731);
#27930=LINE('',#143595,#31732);
#27931=LINE('',#143598,#31733);
#27932=LINE('',#143618,#31734);
#27933=LINE('',#143623,#31735);
#27934=LINE('',#143628,#31736);
#27935=LINE('',#143633,#31737);
#27936=LINE('',#143638,#31738);
#27937=LINE('',#143643,#31739);
#27938=LINE('',#143648,#31740);
#27939=LINE('',#143661,#31741);
#27940=LINE('',#143663,#31742);
#27941=LINE('',#143667,#31743);
#27942=LINE('',#143668,#31744);
#27943=LINE('',#143674,#31745);
#27944=LINE('',#143676,#31746);
#27945=LINE('',#143680,#31747);
#27946=LINE('',#143681,#31748);
#27947=LINE('',#143684,#31749);
#27948=LINE('',#143686,#31750);
#27949=LINE('',#143687,#31751);
#27950=LINE('',#143693,#31752);
#27951=LINE('',#143696,#31753);
#27952=LINE('',#143697,#31754);
#27953=LINE('',#143700,#31755);
#27954=LINE('',#143702,#31756);
#27955=LINE('',#143703,#31757);
#27956=LINE('',#143709,#31758);
#27957=LINE('',#143712,#31759);
#27958=LINE('',#143713,#31760);
#27959=LINE('',#143733,#31761);
#27960=LINE('',#143735,#31762);
#27961=LINE('',#143736,#31763);
#27962=LINE('',#143742,#31764);
#27963=LINE('',#143749,#31765);
#27964=LINE('',#143750,#31766);
#27965=LINE('',#143765,#31767);
#27966=LINE('',#143767,#31768);
#27967=LINE('',#143768,#31769);
#27968=LINE('',#143774,#31770);
#27969=LINE('',#143781,#31771);
#27970=LINE('',#143782,#31772);
#27971=LINE('',#143792,#31773);
#27972=LINE('',#143794,#31774);
#27973=LINE('',#143795,#31775);
#27974=LINE('',#143797,#31776);
#27975=LINE('',#143798,#31777);
#27976=LINE('',#143811,#31778);
#27977=LINE('',#143827,#31779);
#27978=LINE('',#143831,#31780);
#27979=LINE('',#143833,#31781);
#27980=LINE('',#143834,#31782);
#27981=LINE('',#143840,#31783);
#27982=LINE('',#143856,#31784);
#27983=LINE('',#143860,#31785);
#27984=LINE('',#143862,#31786);
#27985=LINE('',#143865,#31787);
#27986=LINE('',#143868,#31788);
#27987=LINE('',#143870,#31789);
#27988=LINE('',#143871,#31790);
#27989=LINE('',#143885,#31791);
#27990=LINE('',#143905,#31792);
#27991=LINE('',#143936,#31793);
#27992=LINE('',#143937,#31794);
#27993=LINE('',#143940,#31795);
#27994=LINE('',#143944,#31796);
#27995=LINE('',#143945,#31797);
#27996=LINE('',#143950,#31798);
#27997=LINE('',#143980,#31799);
#27998=LINE('',#143991,#31800);
#27999=LINE('',#144004,#31801);
#28000=LINE('',#144008,#31802);
#28001=LINE('',#144009,#31803);
#28002=LINE('',#144010,#31804);
#28003=LINE('',#144023,#31805);
#28004=LINE('',#144035,#31806);
#28005=LINE('',#144036,#31807);
#28006=LINE('',#144037,#31808);
#28007=LINE('',#144055,#31809);
#28008=LINE('',#144056,#31810);
#28009=LINE('',#144072,#31811);
#28010=LINE('',#144086,#31812);
#28011=LINE('',#144103,#31813);
#28012=LINE('',#144105,#31814);
#28013=LINE('',#144107,#31815);
#28014=LINE('',#144109,#31816);
#28015=LINE('',#144111,#31817);
#28016=LINE('',#144112,#31818);
#28017=LINE('',#144113,#31819);
#28018=LINE('',#144114,#31820);
#28019=LINE('',#144132,#31821);
#28020=LINE('',#144135,#31822);
#28021=LINE('',#144151,#31823);
#28022=LINE('',#144204,#31824);
#28023=LINE('',#144228,#31825);
#28024=LINE('',#144232,#31826);
#28025=LINE('',#144266,#31827);
#28026=LINE('',#144269,#31828);
#28027=LINE('',#144274,#31829);
#28028=LINE('',#144324,#31830);
#28029=LINE('',#144349,#31831);
#28030=LINE('',#144356,#31832);
#28031=LINE('',#144360,#31833);
#28032=LINE('',#144366,#31834);
#28033=LINE('',#144383,#31835);
#28034=LINE('',#144387,#31836);
#28035=LINE('',#144405,#31837);
#28036=LINE('',#144409,#31838);
#28037=LINE('',#144416,#31839);
#28038=LINE('',#144419,#31840);
#28039=LINE('',#144423,#31841);
#28040=LINE('',#144427,#31842);
#28041=LINE('',#144432,#31843);
#28042=LINE('',#144437,#31844);
#28043=LINE('',#144441,#31845);
#28044=LINE('',#144442,#31846);
#28045=LINE('',#144446,#31847);
#28046=LINE('',#144449,#31848);
#28047=LINE('',#144453,#31849);
#28048=LINE('',#144470,#31850);
#28049=LINE('',#144475,#31851);
#28050=LINE('',#144479,#31852);
#28051=LINE('',#144480,#31853);
#28052=LINE('',#144495,#31854);
#28053=LINE('',#144500,#31855);
#28054=LINE('',#144502,#31856);
#28055=LINE('',#144506,#31857);
#28056=LINE('',#144525,#31858);
#28057=LINE('',#144529,#31859);
#28058=LINE('',#144547,#31860);
#28059=LINE('',#144550,#31861);
#28060=LINE('',#144560,#31862);
#28061=LINE('',#144615,#31863);
#28062=LINE('',#144645,#31864);
#28063=LINE('',#144647,#31865);
#28064=LINE('',#144688,#31866);
#28065=LINE('',#144690,#31867);
#28066=LINE('',#144692,#31868);
#28067=LINE('',#144693,#31869);
#28068=LINE('',#144697,#31870);
#28069=LINE('',#144699,#31871);
#28070=LINE('',#144701,#31872);
#28071=LINE('',#144724,#31873);
#28072=LINE('',#144737,#31874);
#28073=LINE('',#144781,#31875);
#28074=LINE('',#144811,#31876);
#28075=LINE('',#144821,#31877);
#28076=LINE('',#144917,#31878);
#28077=LINE('',#144919,#31879);
#28078=LINE('',#144920,#31880);
#28079=LINE('',#144925,#31881);
#28080=LINE('',#144931,#31882);
#28081=LINE('',#144933,#31883);
#28082=LINE('',#144935,#31884);
#28083=LINE('',#144936,#31885);
#28084=LINE('',#144941,#31886);
#28085=LINE('',#144948,#31887);
#28086=LINE('',#144951,#31888);
#28087=LINE('',#144954,#31889);
#28088=LINE('',#144956,#31890);
#28089=LINE('',#144957,#31891);
#28090=LINE('',#144962,#31892);
#28091=LINE('',#144982,#31893);
#28092=LINE('',#144986,#31894);
#28093=LINE('',#144992,#31895);
#28094=LINE('',#144993,#31896);
#28095=LINE('',#144999,#31897);
#28096=LINE('',#145001,#31898);
#28097=LINE('',#145003,#31899);
#28098=LINE('',#145004,#31900);
#28099=LINE('',#145011,#31901);
#28100=LINE('',#145013,#31902);
#28101=LINE('',#145015,#31903);
#28102=LINE('',#145016,#31904);
#28103=LINE('',#145018,#31905);
#28104=LINE('',#145020,#31906);
#28105=LINE('',#145021,#31907);
#28106=LINE('',#145025,#31908);
#28107=LINE('',#145028,#31909);
#28108=LINE('',#145029,#31910);
#28109=LINE('',#145036,#31911);
#28110=LINE('',#145038,#31912);
#28111=LINE('',#145039,#31913);
#28112=LINE('',#145042,#31914);
#28113=LINE('',#145043,#31915);
#28114=LINE('',#145047,#31916);
#28115=LINE('',#145050,#31917);
#28116=LINE('',#145055,#31918);
#28117=LINE('',#145062,#31919);
#28118=LINE('',#145067,#31920);
#28119=LINE('',#145082,#31921);
#28120=LINE('',#145092,#31922);
#28121=LINE('',#145098,#31923);
#28122=LINE('',#145101,#31924);
#28123=LINE('',#145103,#31925);
#28124=LINE('',#145104,#31926);
#28125=LINE('',#145109,#31927);
#28126=LINE('',#145114,#31928);
#28127=LINE('',#145117,#31929);
#28128=LINE('',#145122,#31930);
#28129=LINE('',#145127,#31931);
#28130=LINE('',#145131,#31932);
#28131=LINE('',#145142,#31933);
#28132=LINE('',#145149,#31934);
#28133=LINE('',#145154,#31935);
#28134=LINE('',#145156,#31936);
#28135=LINE('',#145158,#31937);
#28136=LINE('',#145159,#31938);
#28137=LINE('',#145163,#31939);
#28138=LINE('',#145165,#31940);
#28139=LINE('',#145167,#31941);
#28140=LINE('',#145168,#31942);
#28141=LINE('',#145174,#31943);
#28142=LINE('',#145175,#31944);
#28143=LINE('',#145194,#31945);
#28144=LINE('',#145196,#31946);
#28145=LINE('',#145197,#31947);
#28146=LINE('',#145320,#31948);
#28147=LINE('',#145322,#31949);
#28148=LINE('',#145324,#31950);
#28149=LINE('',#145325,#31951);
#28150=LINE('',#145331,#31952);
#28151=LINE('',#145334,#31953);
#28152=LINE('',#145337,#31954);
#28153=LINE('',#145343,#31955);
#28154=LINE('',#145349,#31956);
#28155=LINE('',#145351,#31957);
#28156=LINE('',#145353,#31958);
#28157=LINE('',#145357,#31959);
#28158=LINE('',#145360,#31960);
#28159=LINE('',#145362,#31961);
#28160=LINE('',#145364,#31962);
#28161=LINE('',#145372,#31963);
#28162=LINE('',#145374,#31964);
#28163=LINE('',#145375,#31965);
#28164=LINE('',#145380,#31966);
#28165=LINE('',#145383,#31967);
#28166=LINE('',#145384,#31968);
#28167=LINE('',#145388,#31969);
#28168=LINE('',#145395,#31970);
#28169=LINE('',#145402,#31971);
#28170=LINE('',#145404,#31972);
#28171=LINE('',#145406,#31973);
#28172=LINE('',#145407,#31974);
#28173=LINE('',#145411,#31975);
#28174=LINE('',#145413,#31976);
#28175=LINE('',#145415,#31977);
#28176=LINE('',#145416,#31978);
#28177=LINE('',#145419,#31979);
#28178=LINE('',#145421,#31980);
#28179=LINE('',#145425,#31981);
#28180=LINE('',#145433,#31982);
#28181=LINE('',#145435,#31983);
#28182=LINE('',#145437,#31984);
#28183=LINE('',#145441,#31985);
#28184=LINE('',#145445,#31986);
#28185=LINE('',#145447,#31987);
#28186=LINE('',#145448,#31988);
#28187=LINE('',#145451,#31989);
#28188=LINE('',#145453,#31990);
#28189=LINE('',#145461,#31991);
#28190=LINE('',#145473,#31992);
#28191=LINE('',#145475,#31993);
#28192=LINE('',#145477,#31994);
#28193=LINE('',#145479,#31995);
#28194=LINE('',#145480,#31996);
#28195=LINE('',#145482,#31997);
#28196=LINE('',#145484,#31998);
#28197=LINE('',#145485,#31999);
#28198=LINE('',#145488,#32000);
#28199=LINE('',#145490,#32001);
#28200=LINE('',#145492,#32002);
#28201=LINE('',#145494,#32003);
#28202=LINE('',#145496,#32004);
#28203=LINE('',#145498,#32005);
#28204=LINE('',#145510,#32006);
#28205=LINE('',#145517,#32007);
#28206=LINE('',#145518,#32008);
#28207=LINE('',#145521,#32009);
#28208=LINE('',#145523,#32010);
#28209=LINE('',#145525,#32011);
#28210=LINE('',#145529,#32012);
#28211=LINE('',#145533,#32013);
#28212=LINE('',#145536,#32014);
#28213=LINE('',#145537,#32015);
#28214=LINE('',#145539,#32016);
#28215=LINE('',#145540,#32017);
#28216=LINE('',#145542,#32018);
#28217=LINE('',#145544,#32019);
#28218=LINE('',#145545,#32020);
#28219=LINE('',#145550,#32021);
#28220=LINE('',#145553,#32022);
#28221=LINE('',#145555,#32023);
#28222=LINE('',#145565,#32024);
#28223=LINE('',#145567,#32025);
#28224=LINE('',#145569,#32026);
#28225=LINE('',#145570,#32027);
#28226=LINE('',#145572,#32028);
#28227=LINE('',#145575,#32029);
#28228=LINE('',#145576,#32030);
#28229=LINE('',#145578,#32031);
#28230=LINE('',#145582,#32032);
#28231=LINE('',#145584,#32033);
#28232=LINE('',#145586,#32034);
#28233=LINE('',#145588,#32035);
#28234=LINE('',#145590,#32036);
#28235=LINE('',#145596,#32037);
#28236=LINE('',#145597,#32038);
#28237=LINE('',#145600,#32039);
#28238=LINE('',#145601,#32040);
#28239=LINE('',#145604,#32041);
#28240=LINE('',#145607,#32042);
#28241=LINE('',#145608,#32043);
#28242=LINE('',#145616,#32044);
#28243=LINE('',#145619,#32045);
#28244=LINE('',#145621,#32046);
#28245=LINE('',#145626,#32047);
#28246=LINE('',#145629,#32048);
#28247=LINE('',#145632,#32049);
#28248=LINE('',#145634,#32050);
#28249=LINE('',#145638,#32051);
#28250=LINE('',#145639,#32052);
#28251=LINE('',#145642,#32053);
#28252=LINE('',#145645,#32054);
#28253=LINE('',#145648,#32055);
#28254=LINE('',#145650,#32056);
#28255=LINE('',#145651,#32057);
#28256=LINE('',#145654,#32058);
#28257=LINE('',#145658,#32059);
#28258=LINE('',#145659,#32060);
#28259=LINE('',#145664,#32061);
#28260=LINE('',#145667,#32062);
#28261=LINE('',#145669,#32063);
#28262=LINE('',#145671,#32064);
#28263=LINE('',#145733,#32065);
#28264=LINE('',#145742,#32066);
#28265=LINE('',#145777,#32067);
#28266=LINE('',#145787,#32068);
#28267=LINE('',#145791,#32069);
#28268=LINE('',#145793,#32070);
#28269=LINE('',#145794,#32071);
#28270=LINE('',#145796,#32072);
#28271=LINE('',#145806,#32073);
#28272=LINE('',#145815,#32074);
#28273=LINE('',#145817,#32075);
#28274=LINE('',#145818,#32076);
#28275=LINE('',#145820,#32077);
#28276=LINE('',#145821,#32078);
#28277=LINE('',#145824,#32079);
#28278=LINE('',#145827,#32080);
#28279=LINE('',#145831,#32081);
#28280=LINE('',#145833,#32082);
#28281=LINE('',#145835,#32083);
#28282=LINE('',#145837,#32084);
#28283=LINE('',#145838,#32085);
#28284=LINE('',#145844,#32086);
#28285=LINE('',#145848,#32087);
#28286=LINE('',#145854,#32088);
#28287=LINE('',#145861,#32089);
#28288=LINE('',#145866,#32090);
#28289=LINE('',#145871,#32091);
#28290=LINE('',#147769,#32092);
#28291=LINE('',#147777,#32093);
#28292=LINE('',#147785,#32094);
#28293=LINE('',#147793,#32095);
#28294=LINE('',#147800,#32096);
#28295=LINE('',#147806,#32097);
#28296=LINE('',#147813,#32098);
#28297=LINE('',#147820,#32099);
#28298=LINE('',#147823,#32100);
#28299=LINE('',#147825,#32101);
#28300=LINE('',#148785,#32102);
#28301=LINE('',#149724,#32103);
#28302=LINE('',#152038,#32104);
#28303=LINE('',#152041,#32105);
#28304=LINE('',#152399,#32106);
#28305=LINE('',#152405,#32107);
#28306=LINE('',#152488,#32108);
#28307=LINE('',#152491,#32109);
#28308=LINE('',#152497,#32110);
#28309=LINE('',#152500,#32111);
#28310=LINE('',#152504,#32112);
#28311=LINE('',#152506,#32113);
#28312=LINE('',#152508,#32114);
#28313=LINE('',#152512,#32115);
#28314=LINE('',#152518,#32116);
#28315=LINE('',#152521,#32117);
#28316=LINE('',#152527,#32118);
#28317=LINE('',#152530,#32119);
#28318=LINE('',#152536,#32120);
#28319=LINE('',#152539,#32121);
#28320=LINE('',#152545,#32122);
#28321=LINE('',#152548,#32123);
#28322=LINE('',#152550,#32124);
#28323=LINE('',#152841,#32125);
#28324=LINE('',#152847,#32126);
#28325=LINE('',#152851,#32127);
#28326=LINE('',#152856,#32128);
#28327=LINE('',#152864,#32129);
#28328=LINE('',#152866,#32130);
#28329=LINE('',#152870,#32131);
#28330=LINE('',#152873,#32132);
#28331=LINE('',#152876,#32133);
#28332=LINE('',#152878,#32134);
#28333=LINE('',#152882,#32135);
#28334=LINE('',#152884,#32136);
#28335=LINE('',#152888,#32137);
#28336=LINE('',#152890,#32138);
#28337=LINE('',#152894,#32139);
#28338=LINE('',#152898,#32140);
#28339=LINE('',#152902,#32141);
#28340=LINE('',#152905,#32142);
#28341=LINE('',#152908,#32143);
#28342=LINE('',#152910,#32144);
#28343=LINE('',#152914,#32145);
#28344=LINE('',#152916,#32146);
#28345=LINE('',#152920,#32147);
#28346=LINE('',#152923,#32148);
#28347=LINE('',#152926,#32149);
#28348=LINE('',#152928,#32150);
#28349=LINE('',#152933,#32151);
#28350=LINE('',#152937,#32152);
#28351=LINE('',#152940,#32153);
#28352=LINE('',#152943,#32154);
#28353=LINE('',#152946,#32155);
#28354=LINE('',#152948,#32156);
#28355=LINE('',#152952,#32157);
#28356=LINE('',#152955,#32158);
#28357=LINE('',#152958,#32159);
#28358=LINE('',#152960,#32160);
#28359=LINE('',#152964,#32161);
#28360=LINE('',#152966,#32162);
#28361=LINE('',#152970,#32163);
#28362=LINE('',#152973,#32164);
#28363=LINE('',#152976,#32165);
#28364=LINE('',#152978,#32166);
#28365=LINE('',#152982,#32167);
#28366=LINE('',#152985,#32168);
#28367=LINE('',#152988,#32169);
#28368=LINE('',#152991,#32170);
#28369=LINE('',#152994,#32171);
#28370=LINE('',#152997,#32172);
#28371=LINE('',#153000,#32173);
#28372=LINE('',#153002,#32174);
#28373=LINE('',#153006,#32175);
#28374=LINE('',#153009,#32176);
#28375=LINE('',#153012,#32177);
#28376=LINE('',#153014,#32178);
#28377=LINE('',#153018,#32179);
#28378=LINE('',#153020,#32180);
#28379=LINE('',#153024,#32181);
#28380=LINE('',#153027,#32182);
#28381=LINE('',#153030,#32183);
#28382=LINE('',#153032,#32184);
#28383=LINE('',#153036,#32185);
#28384=LINE('',#153039,#32186);
#28385=LINE('',#153042,#32187);
#28386=LINE('',#153045,#32188);
#28387=LINE('',#153048,#32189);
#28388=LINE('',#153051,#32190);
#28389=LINE('',#153054,#32191);
#28390=LINE('',#153056,#32192);
#28391=LINE('',#153060,#32193);
#28392=LINE('',#153062,#32194);
#28393=LINE('',#153066,#32195);
#28394=LINE('',#153068,#32196);
#28395=LINE('',#153252,#32197);
#28396=LINE('',#153253,#32198);
#28397=LINE('',#153255,#32199);
#28398=LINE('',#153257,#32200);
#28399=LINE('',#153260,#32201);
#28400=LINE('',#153262,#32202);
#28401=LINE('',#153265,#32203);
#28402=LINE('',#153267,#32204);
#28403=LINE('',#153270,#32205);
#28404=LINE('',#153272,#32206);
#28405=LINE('',#153275,#32207);
#28406=LINE('',#153277,#32208);
#28407=LINE('',#153280,#32209);
#28408=LINE('',#153282,#32210);
#28409=LINE('',#153285,#32211);
#28410=LINE('',#153287,#32212);
#28411=LINE('',#153290,#32213);
#28412=LINE('',#153292,#32214);
#28413=LINE('',#153295,#32215);
#28414=LINE('',#153297,#32216);
#28415=LINE('',#153300,#32217);
#28416=LINE('',#153302,#32218);
#28417=LINE('',#153305,#32219);
#28418=LINE('',#153307,#32220);
#28419=LINE('',#153310,#32221);
#28420=LINE('',#153312,#32222);
#28421=LINE('',#153315,#32223);
#28422=LINE('',#153317,#32224);
#28423=LINE('',#153320,#32225);
#28424=LINE('',#153322,#32226);
#28425=LINE('',#153325,#32227);
#28426=LINE('',#153327,#32228);
#28427=LINE('',#153330,#32229);
#28428=LINE('',#153332,#32230);
#28429=LINE('',#153335,#32231);
#28430=LINE('',#153337,#32232);
#28431=LINE('',#153340,#32233);
#28432=LINE('',#153342,#32234);
#28433=LINE('',#153345,#32235);
#28434=LINE('',#153347,#32236);
#28435=LINE('',#153350,#32237);
#28436=LINE('',#153352,#32238);
#28437=LINE('',#153355,#32239);
#28438=LINE('',#153357,#32240);
#28439=LINE('',#153360,#32241);
#28440=LINE('',#153362,#32242);
#28441=LINE('',#153365,#32243);
#28442=LINE('',#153367,#32244);
#28443=LINE('',#153370,#32245);
#28444=LINE('',#153372,#32246);
#28445=LINE('',#153375,#32247);
#28446=LINE('',#153377,#32248);
#28447=LINE('',#153380,#32249);
#28448=LINE('',#153383,#32250);
#28449=LINE('',#153386,#32251);
#28450=LINE('',#153388,#32252);
#28451=LINE('',#153391,#32253);
#28452=LINE('',#153393,#32254);
#28453=LINE('',#153396,#32255);
#28454=LINE('',#153398,#32256);
#28455=LINE('',#153401,#32257);
#28456=LINE('',#153403,#32258);
#28457=LINE('',#153406,#32259);
#28458=LINE('',#153409,#32260);
#28459=LINE('',#153412,#32261);
#28460=LINE('',#153414,#32262);
#28461=LINE('',#153417,#32263);
#28462=LINE('',#153419,#32264);
#28463=LINE('',#153422,#32265);
#28464=LINE('',#153424,#32266);
#28465=LINE('',#153427,#32267);
#28466=LINE('',#153429,#32268);
#28467=LINE('',#153438,#32269);
#28468=LINE('',#153439,#32270);
#28469=LINE('',#153440,#32271);
#28470=LINE('',#153444,#32272);
#28471=LINE('',#153450,#32273);
#28472=LINE('',#153456,#32274);
#28473=LINE('',#153461,#32275);
#28474=LINE('',#153462,#32276);
#28475=LINE('',#153463,#32277);
#28476=LINE('',#153466,#32278);
#28477=LINE('',#153475,#32279);
#28478=LINE('',#153479,#32280);
#28479=LINE('',#153482,#32281);
#28480=LINE('',#153483,#32282);
#28481=LINE('',#153486,#32283);
#28482=LINE('',#153491,#32284);
#28483=LINE('',#153496,#32285);
#28484=LINE('',#153497,#32286);
#28485=LINE('',#153498,#32287);
#28486=LINE('',#153502,#32288);
#28487=LINE('',#153543,#32289);
#28488=LINE('',#153546,#32290);
#28489=LINE('',#154493,#32291);
#28490=LINE('',#156382,#32292);
#28491=LINE('',#157330,#32293);
#28492=LINE('',#157338,#32294);
#28493=LINE('',#157341,#32295);
#28494=LINE('',#158288,#32296);
#28495=LINE('',#160818,#32297);
#28496=LINE('',#160826,#32298);
#28497=LINE('',#160829,#32299);
#28498=LINE('',#163376,#32300);
#28499=LINE('',#164018,#32301);
#28500=LINE('',#164026,#32302);
#28501=LINE('',#164029,#32303);
#28502=LINE('',#164976,#32304);
#28503=LINE('',#167218,#32305);
#28504=LINE('',#167226,#32306);
#28505=LINE('',#167229,#32307);
#28506=LINE('',#170064,#32308);
#28507=LINE('',#171012,#32309);
#28508=LINE('',#171020,#32310);
#28509=LINE('',#171023,#32311);
#28510=LINE('',#171970,#32312);
#28511=LINE('',#174500,#32313);
#28512=LINE('',#174508,#32314);
#28513=LINE('',#174511,#32315);
#28514=LINE('',#177055,#32316);
#28515=LINE('',#177709,#32317);
#28516=LINE('',#177717,#32318);
#28517=LINE('',#177720,#32319);
#28518=LINE('',#178667,#32320);
#28519=LINE('',#181200,#32321);
#28520=LINE('',#181208,#32322);
#28521=LINE('',#181211,#32323);
#28522=LINE('',#183734,#32324);
#28523=LINE('',#184682,#32325);
#28524=LINE('',#184690,#32326);
#28525=LINE('',#184693,#32327);
#28526=LINE('',#185640,#32328);
#28527=LINE('',#187870,#32329);
#28528=LINE('',#187878,#32330);
#28529=LINE('',#187881,#32331);
#28530=LINE('',#190380,#32332);
#28531=LINE('',#191004,#32333);
#28532=LINE('',#191012,#32334);
#28533=LINE('',#191015,#32335);
#28534=LINE('',#191962,#32336);
#28535=LINE('',#194472,#32337);
#28536=LINE('',#194480,#32338);
#28537=LINE('',#194483,#32339);
#28538=LINE('',#197000,#32340);
#28539=LINE('',#197948,#32341);
#28540=LINE('',#197956,#32342);
#28541=LINE('',#197959,#32343);
#28542=LINE('',#198906,#32344);
#28543=LINE('',#201106,#32345);
#28544=LINE('',#201114,#32346);
#28545=LINE('',#201117,#32347);
#28546=LINE('',#203646,#32348);
#28547=LINE('',#204282,#32349);
#28548=LINE('',#204290,#32350);
#28549=LINE('',#204293,#32351);
#28550=LINE('',#205240,#32352);
#28551=LINE('',#207434,#32353);
#28552=LINE('',#207442,#32354);
#28553=LINE('',#207445,#32355);
#28554=LINE('',#209974,#32356);
#28555=LINE('',#210613,#32357);
#28556=LINE('',#210621,#32358);
#28557=LINE('',#210624,#32359);
#28558=LINE('',#211571,#32360);
#28559=LINE('',#213777,#32361);
#28560=LINE('',#213785,#32362);
#28561=LINE('',#213788,#32363);
#28562=LINE('',#216311,#32364);
#28563=LINE('',#216944,#32365);
#28564=LINE('',#216952,#32366);
#28565=LINE('',#216955,#32367);
#28566=LINE('',#217902,#32368);
#28567=LINE('',#220409,#32369);
#28568=LINE('',#220417,#32370);
#28569=LINE('',#220420,#32371);
#28570=LINE('',#222922,#32372);
#28571=LINE('',#223552,#32373);
#28572=LINE('',#223560,#32374);
#28573=LINE('',#223563,#32375);
#28574=LINE('',#224510,#32376);
#28575=LINE('',#226996,#32377);
#28576=LINE('',#227004,#32378);
#28577=LINE('',#227007,#32379);
#28578=LINE('',#229521,#32380);
#28579=LINE('',#230136,#32381);
#28580=LINE('',#230144,#32382);
#28581=LINE('',#230147,#32383);
#28582=LINE('',#231094,#32384);
#28583=LINE('',#233276,#32385);
#28584=LINE('',#233284,#32386);
#28585=LINE('',#233287,#32387);
#28586=LINE('',#235816,#32388);
#28587=LINE('',#236434,#32389);
#28588=LINE('',#236442,#32390);
#28589=LINE('',#236445,#32391);
#28590=LINE('',#237392,#32392);
#28591=LINE('',#239604,#32393);
#28592=LINE('',#239612,#32394);
#28593=LINE('',#239615,#32395);
#28594=LINE('',#242138,#32396);
#28595=LINE('',#242771,#32397);
#28596=LINE('',#242779,#32398);
#28597=LINE('',#242782,#32399);
#28598=LINE('',#243729,#32400);
#28599=LINE('',#246253,#32401);
#28600=LINE('',#246261,#32402);
#28601=LINE('',#246264,#32403);
#28602=LINE('',#248790,#32404);
#28603=LINE('',#249426,#32405);
#28604=LINE('',#249434,#32406);
#28605=LINE('',#249437,#32407);
#28606=LINE('',#250384,#32408);
#28607=LINE('',#252599,#32409);
#28608=LINE('',#252607,#32410);
#28609=LINE('',#252610,#32411);
#28610=LINE('',#255112,#32412);
#28611=LINE('',#255751,#32413);
#28612=LINE('',#255759,#32414);
#28613=LINE('',#255762,#32415);
#28614=LINE('',#256709,#32416);
#28615=LINE('',#258900,#32417);
#28616=LINE('',#258908,#32418);
#28617=LINE('',#258911,#32419);
#28618=LINE('',#261744,#32420);
#28619=LINE('',#262692,#32421);
#28620=LINE('',#262700,#32422);
#28621=LINE('',#262703,#32423);
#28622=LINE('',#263650,#32424);
#28623=LINE('',#266146,#32425);
#28624=LINE('',#266154,#32426);
#28625=LINE('',#266157,#32427);
#28626=LINE('',#268689,#32428);
#28627=LINE('',#269635,#32429);
#28628=LINE('',#269643,#32430);
#28629=LINE('',#269646,#32431);
#28630=LINE('',#270593,#32432);
#28631=LINE('',#272832,#32433);
#28632=LINE('',#272840,#32434);
#28633=LINE('',#272843,#32435);
#28634=LINE('',#275384,#32436);
#28635=LINE('',#276035,#32437);
#28636=LINE('',#276043,#32438);
#28637=LINE('',#276046,#32439);
#28638=LINE('',#276993,#32440);
#28639=LINE('',#279530,#32441);
#28640=LINE('',#279538,#32442);
#28641=LINE('',#279541,#32443);
#28642=LINE('',#282079,#32444);
#28643=LINE('',#282739,#32445);
#28644=LINE('',#282747,#32446);
#28645=LINE('',#282750,#32447);
#28646=LINE('',#283697,#32448);
#28647=LINE('',#286533,#32449);
#28648=LINE('',#286541,#32450);
#28649=LINE('',#286544,#32451);
#28650=LINE('',#289377,#32452);
#28651=LINE('',#290028,#32453);
#28652=LINE('',#290036,#32454);
#28653=LINE('',#290039,#32455);
#28654=LINE('',#290986,#32456);
#28655=LINE('',#293216,#32457);
#28656=LINE('',#293224,#32458);
#28657=LINE('',#293227,#32459);
#28658=LINE('',#295753,#32460);
#28659=LINE('',#297503,#32461);
#28660=LINE('',#297507,#32462);
#28661=LINE('',#297511,#32463);
#28662=LINE('',#297514,#32464);
#28663=LINE('',#300198,#32465);
#28664=LINE('',#300205,#32466);
#28665=LINE('',#300211,#32467);
#28666=LINE('',#300218,#32468);
#28667=LINE('',#300222,#32469);
#28668=LINE('',#300285,#32470);
#28669=LINE('',#300289,#32471);
#28670=LINE('',#300357,#32472);
#28671=LINE('',#300361,#32473);
#28672=LINE('',#300429,#32474);
#28673=LINE('',#300433,#32475);
#28674=LINE('',#300501,#32476);
#28675=LINE('',#300505,#32477);
#28676=LINE('',#300568,#32478);
#28677=LINE('',#300572,#32479);
#28678=LINE('',#300610,#32480);
#28679=LINE('',#300614,#32481);
#28680=LINE('',#300682,#32482);
#28681=LINE('',#300686,#32483);
#28682=LINE('',#300718,#32484);
#28683=LINE('',#300722,#32485);
#28684=LINE('',#300787,#32486);
#28685=LINE('',#300791,#32487);
#28686=LINE('',#300856,#32488);
#28687=LINE('',#300860,#32489);
#28688=LINE('',#300898,#32490);
#28689=LINE('',#300902,#32491);
#28690=LINE('',#300967,#32492);
#28691=LINE('',#300971,#32493);
#28692=LINE('',#301009,#32494);
#28693=LINE('',#301013,#32495);
#28694=LINE('',#301078,#32496);
#28695=LINE('',#301082,#32497);
#28696=LINE('',#301147,#32498);
#28697=LINE('',#301151,#32499);
#28698=LINE('',#301214,#32500);
#28699=LINE('',#301218,#32501);
#28700=LINE('',#301287,#32502);
#28701=LINE('',#301292,#32503);
#28702=LINE('',#301295,#32504);
#28703=LINE('',#302947,#32505);
#28704=LINE('',#302958,#32506);
#28705=LINE('',#302959,#32507);
#28706=LINE('',#302962,#32508);
#28707=LINE('',#302966,#32509);
#28708=LINE('',#302967,#32510);
#28709=LINE('',#304622,#32511);
#28710=LINE('',#304633,#32512);
#28711=LINE('',#306286,#32513);
#28712=LINE('',#306297,#32514);
#28713=LINE('',#306298,#32515);
#28714=LINE('',#306301,#32516);
#28715=LINE('',#306305,#32517);
#28716=LINE('',#306306,#32518);
#28717=LINE('',#307961,#32519);
#28718=LINE('',#307976,#32520);
#28719=LINE('',#309629,#32521);
#28720=LINE('',#309640,#32522);
#28721=LINE('',#309641,#32523);
#28722=LINE('',#309644,#32524);
#28723=LINE('',#309648,#32525);
#28724=LINE('',#309649,#32526);
#28725=LINE('',#311301,#32527);
#28726=LINE('',#311316,#32528);
#28727=LINE('',#312969,#32529);
#28728=LINE('',#312980,#32530);
#28729=LINE('',#312981,#32531);
#28730=LINE('',#312984,#32532);
#28731=LINE('',#312988,#32533);
#28732=LINE('',#312989,#32534);
#28733=LINE('',#314644,#32535);
#28734=LINE('',#314663,#32536);
#28735=LINE('',#316316,#32537);
#28736=LINE('',#316327,#32538);
#28737=LINE('',#316328,#32539);
#28738=LINE('',#316331,#32540);
#28739=LINE('',#316335,#32541);
#28740=LINE('',#316336,#32542);
#28741=LINE('',#317991,#32543);
#28742=LINE('',#318010,#32544);
#28743=LINE('',#319663,#32545);
#28744=LINE('',#319674,#32546);
#28745=LINE('',#319675,#32547);
#28746=LINE('',#319678,#32548);
#28747=LINE('',#319682,#32549);
#28748=LINE('',#319683,#32550);
#28749=LINE('',#321338,#32551);
#28750=LINE('',#321357,#32552);
#28751=LINE('',#323010,#32553);
#28752=LINE('',#323021,#32554);
#28753=LINE('',#323022,#32555);
#28754=LINE('',#323025,#32556);
#28755=LINE('',#323029,#32557);
#28756=LINE('',#323030,#32558);
#28757=LINE('',#324685,#32559);
#28758=LINE('',#324704,#32560);
#28759=LINE('',#326357,#32561);
#28760=LINE('',#326368,#32562);
#28761=LINE('',#326369,#32563);
#28762=LINE('',#326372,#32564);
#28763=LINE('',#326376,#32565);
#28764=LINE('',#326377,#32566);
#28765=LINE('',#328032,#32567);
#28766=LINE('',#328047,#32568);
#28767=LINE('',#329700,#32569);
#28768=LINE('',#329711,#32570);
#28769=LINE('',#329712,#32571);
#28770=LINE('',#329717,#32572);
#28771=LINE('',#329747,#32573);
#28772=LINE('',#329751,#32574);
#28773=LINE('',#329781,#32575);
#28774=LINE('',#329785,#32576);
#28775=LINE('',#329815,#32577);
#28776=LINE('',#329819,#32578);
#28777=LINE('',#329845,#32579);
#28778=LINE('',#329849,#32580);
#28779=LINE('',#329879,#32581);
#28780=LINE('',#329883,#32582);
#28781=LINE('',#329913,#32583);
#28782=LINE('',#329917,#32584);
#28783=LINE('',#329947,#32585);
#28784=LINE('',#329951,#32586);
#28785=LINE('',#329979,#32587);
#28786=LINE('',#329983,#32588);
#28787=LINE('',#329995,#32589);
#28788=LINE('',#329996,#32590);
#28789=LINE('',#331651,#32591);
#28790=LINE('',#331653,#32592);
#28791=LINE('',#333304,#32593);
#28792=LINE('',#333306,#32594);
#28793=LINE('',#334960,#32595);
#28794=LINE('',#334962,#32596);
#28795=LINE('',#334964,#32597);
#28796=LINE('',#334966,#32598);
#28797=LINE('',#334967,#32599);
#28798=LINE('',#334969,#32600);
#28799=LINE('',#336620,#32601);
#28800=LINE('',#336622,#32602);
#28801=LINE('',#338277,#32603);
#28802=LINE('',#338278,#32604);
#28803=LINE('',#338280,#32605);
#28804=LINE('',#338281,#32606);
#28805=LINE('',#339932,#32607);
#28806=LINE('',#339934,#32608);
#28807=LINE('',#341589,#32609);
#28808=LINE('',#341591,#32610);
#28809=LINE('',#343242,#32611);
#28810=LINE('',#343244,#32612);
#28811=LINE('',#344898,#32613);
#28812=LINE('',#344900,#32614);
#28813=LINE('',#344903,#32615);
#28814=LINE('',#344905,#32616);
#28815=LINE('',#344906,#32617);
#28816=LINE('',#344908,#32618);
#28817=LINE('',#346559,#32619);
#28818=LINE('',#346561,#32620);
#28819=LINE('',#348216,#32621);
#28820=LINE('',#348217,#32622);
#28821=LINE('',#348219,#32623);
#28822=LINE('',#348220,#32624);
#28823=LINE('',#349871,#32625);
#28824=LINE('',#349873,#32626);
#28825=LINE('',#351528,#32627);
#28826=LINE('',#351530,#32628);
#28827=LINE('',#353181,#32629);
#28828=LINE('',#353183,#32630);
#28829=LINE('',#354837,#32631);
#28830=LINE('',#354839,#32632);
#28831=LINE('',#354842,#32633);
#28832=LINE('',#354844,#32634);
#28833=LINE('',#354845,#32635);
#28834=LINE('',#354847,#32636);
#28835=LINE('',#356498,#32637);
#28836=LINE('',#356500,#32638);
#28837=LINE('',#358157,#32639);
#28838=LINE('',#358172,#32640);
#28839=LINE('',#358176,#32641);
#28840=LINE('',#358180,#32642);
#28841=LINE('',#358187,#32643);
#28842=LINE('',#358193,#32644);
#28843=LINE('',#358196,#32645);
#28844=LINE('',#358201,#32646);
#28845=LINE('',#358204,#32647);
#28846=LINE('',#358209,#32648);
#28847=LINE('',#358212,#32649);
#28848=LINE('',#358217,#32650);
#28849=LINE('',#358220,#32651);
#28850=LINE('',#358225,#32652);
#28851=LINE('',#358228,#32653);
#28852=LINE('',#358233,#32654);
#28853=LINE('',#358236,#32655);
#28854=LINE('',#358241,#32656);
#28855=LINE('',#358244,#32657);
#28856=LINE('',#358255,#32658);
#28857=LINE('',#358259,#32659);
#28858=LINE('',#358262,#32660);
#28859=LINE('',#358266,#32661);
#28860=LINE('',#358272,#32662);
#28861=LINE('',#358275,#32663);
#28862=LINE('',#358280,#32664);
#28863=LINE('',#358283,#32665);
#28864=LINE('',#358288,#32666);
#28865=LINE('',#358291,#32667);
#28866=LINE('',#358296,#32668);
#28867=LINE('',#358299,#32669);
#28868=LINE('',#358304,#32670);
#28869=LINE('',#358307,#32671);
#28870=LINE('',#358312,#32672);
#28871=LINE('',#358315,#32673);
#28872=LINE('',#358320,#32674);
#28873=LINE('',#358323,#32675);
#28874=LINE('',#358401,#32676);
#28875=LINE('',#358406,#32677);
#28876=LINE('',#358410,#32678);
#28877=LINE('',#358417,#32679);
#28878=LINE('',#358422,#32680);
#28879=LINE('',#358426,#32681);
#28880=LINE('',#358433,#32682);
#28881=LINE('',#358438,#32683);
#28882=LINE('',#358442,#32684);
#28883=LINE('',#358449,#32685);
#28884=LINE('',#358454,#32686);
#28885=LINE('',#358458,#32687);
#28886=LINE('',#358465,#32688);
#28887=LINE('',#358470,#32689);
#28888=LINE('',#358474,#32690);
#28889=LINE('',#358481,#32691);
#28890=LINE('',#358486,#32692);
#28891=LINE('',#358490,#32693);
#28892=LINE('',#358497,#32694);
#28893=LINE('',#358502,#32695);
#28894=LINE('',#358506,#32696);
#28895=LINE('',#358513,#32697);
#28896=LINE('',#358518,#32698);
#28897=LINE('',#358522,#32699);
#28898=LINE('',#358530,#32700);
#28899=LINE('',#358563,#32701);
#28900=LINE('',#358593,#32702);
#28901=LINE('',#358623,#32703);
#28902=LINE('',#358653,#32704);
#28903=LINE('',#358683,#32705);
#28904=LINE('',#358713,#32706);
#28905=LINE('',#358743,#32707);
#28906=LINE('',#358773,#32708);
#28907=LINE('',#358803,#32709);
#28908=LINE('',#358833,#32710);
#28909=LINE('',#358863,#32711);
#28910=LINE('',#358893,#32712);
#28911=LINE('',#358923,#32713);
#28912=LINE('',#358953,#32714);
#28913=LINE('',#358983,#32715);
#28914=LINE('',#359013,#32716);
#28915=LINE('',#359043,#32717);
#28916=LINE('',#359073,#32718);
#28917=LINE('',#359103,#32719);
#28918=LINE('',#359133,#32720);
#28919=LINE('',#359163,#32721);
#28920=LINE('',#359193,#32722);
#28921=LINE('',#359223,#32723);
#28922=LINE('',#359253,#32724);
#28923=LINE('',#359283,#32725);
#28924=LINE('',#359313,#32726);
#28925=LINE('',#359343,#32727);
#28926=LINE('',#359373,#32728);
#28927=LINE('',#359403,#32729);
#28928=LINE('',#359433,#32730);
#28929=LINE('',#359463,#32731);
#28930=LINE('',#359495,#32732);
#28931=LINE('',#359525,#32733);
#28932=LINE('',#359601,#32734);
#28933=LINE('',#359677,#32735);
#28934=LINE('',#359755,#32736);
#28935=LINE('',#359833,#32737);
#28936=LINE('',#359909,#32738);
#28937=LINE('',#359985,#32739);
#28938=LINE('',#360061,#32740);
#28939=LINE('',#360137,#32741);
#28940=LINE('',#360215,#32742);
#28941=LINE('',#360293,#32743);
#28942=LINE('',#360369,#32744);
#28943=LINE('',#360445,#32745);
#28944=LINE('',#360521,#32746);
#28945=LINE('',#360597,#32747);
#28946=LINE('',#360673,#32748);
#28947=LINE('',#360751,#32749);
#28948=LINE('',#360829,#32750);
#28949=LINE('',#360905,#32751);
#28950=LINE('',#360981,#32752);
#28951=LINE('',#361057,#32753);
#28952=LINE('',#361133,#32754);
#28953=LINE('',#361209,#32755);
#28954=LINE('',#361287,#32756);
#28955=LINE('',#361365,#32757);
#28956=LINE('',#361441,#32758);
#28957=LINE('',#361517,#32759);
#28958=LINE('',#361593,#32760);
#28959=LINE('',#361669,#32761);
#28960=LINE('',#361747,#32762);
#28961=LINE('',#361838,#32763);
#28962=LINE('',#361884,#32764);
#28963=LINE('',#362029,#32765);
#28964=LINE('',#362031,#32766);
#28965=LINE('',#362033,#32767);
#28966=LINE('',#362035,#32768);
#28967=LINE('',#362037,#32769);
#28968=LINE('',#362038,#32770);
#28969=LINE('',#362040,#32771);
#28970=LINE('',#362041,#32772);
#28971=LINE('',#362043,#32773);
#28972=LINE('',#362045,#32774);
#28973=LINE('',#362047,#32775);
#28974=LINE('',#362049,#32776);
#28975=LINE('',#366189,#32777);
#28976=LINE('',#366198,#32778);
#28977=LINE('',#366203,#32779);
#28978=LINE('',#366210,#32780);
#28979=LINE('',#366213,#32781);
#28980=LINE('',#366227,#32782);
#28981=LINE('',#366234,#32783);
#28982=LINE('',#366237,#32784);
#28983=LINE('',#366241,#32785);
#28984=LINE('',#366246,#32786);
#28985=LINE('',#366301,#32787);
#28986=LINE('',#366307,#32788);
#28987=LINE('',#366315,#32789);
#28988=LINE('',#366321,#32790);
#28989=LINE('',#366329,#32791);
#28990=LINE('',#366338,#32792);
#28991=LINE('',#366370,#32793);
#28992=LINE('',#366400,#32794);
#28993=LINE('',#366430,#32795);
#28994=LINE('',#366460,#32796);
#28995=LINE('',#366490,#32797);
#28996=LINE('',#366520,#32798);
#28997=LINE('',#366550,#32799);
#28998=LINE('',#366580,#32800);
#28999=LINE('',#366610,#32801);
#29000=LINE('',#366640,#32802);
#29001=LINE('',#366670,#32803);
#29002=LINE('',#366700,#32804);
#29003=LINE('',#366730,#32805);
#29004=LINE('',#366760,#32806);
#29005=LINE('',#366790,#32807);
#29006=LINE('',#366833,#32808);
#29007=LINE('',#366909,#32809);
#29008=LINE('',#366987,#32810);
#29009=LINE('',#367063,#32811);
#29010=LINE('',#367139,#32812);
#29011=LINE('',#367215,#32813);
#29012=LINE('',#367291,#32814);
#29013=LINE('',#367369,#32815);
#29014=LINE('',#367447,#32816);
#29015=LINE('',#367523,#32817);
#29016=LINE('',#367599,#32818);
#29017=LINE('',#367675,#32819);
#29018=LINE('',#367751,#32820);
#29019=LINE('',#367829,#32821);
#29020=LINE('',#367918,#32822);
#29021=LINE('',#367964,#32823);
#29022=LINE('',#368118,#32824);
#29023=LINE('',#368120,#32825);
#29024=LINE('',#368122,#32826);
#29025=LINE('',#368124,#32827);
#29026=LINE('',#368126,#32828);
#29027=LINE('',#368127,#32829);
#29028=LINE('',#368129,#32830);
#29029=LINE('',#368130,#32831);
#29030=LINE('',#368132,#32832);
#29031=LINE('',#368134,#32833);
#29032=LINE('',#368136,#32834);
#29033=LINE('',#368138,#32835);
#29034=LINE('',#368991,#32836);
#29035=LINE('',#369010,#32837);
#29036=LINE('',#369040,#32838);
#29037=LINE('',#369070,#32839);
#29038=LINE('',#369100,#32840);
#29039=LINE('',#369130,#32841);
#29040=LINE('',#369160,#32842);
#29041=LINE('',#369190,#32843);
#29042=LINE('',#369220,#32844);
#29043=LINE('',#369250,#32845);
#29044=LINE('',#369280,#32846);
#29045=LINE('',#369310,#32847);
#29046=LINE('',#369340,#32848);
#29047=LINE('',#369370,#32849);
#29048=LINE('',#369400,#32850);
#29049=LINE('',#369432,#32851);
#29050=LINE('',#369467,#32852);
#29051=LINE('',#369543,#32853);
#29052=LINE('',#369619,#32854);
#29053=LINE('',#369695,#32855);
#29054=LINE('',#369771,#32856);
#29055=LINE('',#369849,#32857);
#29056=LINE('',#369927,#32858);
#29057=LINE('',#370003,#32859);
#29058=LINE('',#370079,#32860);
#29059=LINE('',#370155,#32861);
#29060=LINE('',#370231,#32862);
#29061=LINE('',#370307,#32863);
#29062=LINE('',#370385,#32864);
#29063=LINE('',#370501,#32865);
#29064=LINE('',#370592,#32866);
#29065=LINE('',#370596,#32867);
#29066=LINE('',#370716,#32868);
#29067=LINE('',#370718,#32869);
#29068=LINE('',#370720,#32870);
#29069=LINE('',#370722,#32871);
#29070=LINE('',#370724,#32872);
#29071=LINE('',#370725,#32873);
#29072=LINE('',#370727,#32874);
#29073=LINE('',#370728,#32875);
#29074=LINE('',#370730,#32876);
#29075=LINE('',#370732,#32877);
#29076=LINE('',#370734,#32878);
#29077=LINE('',#370736,#32879);
#29078=LINE('',#371611,#32880);
#29079=LINE('',#371620,#32881);
#29080=LINE('',#371650,#32882);
#29081=LINE('',#371680,#32883);
#29082=LINE('',#371710,#32884);
#29083=LINE('',#371740,#32885);
#29084=LINE('',#371770,#32886);
#29085=LINE('',#371800,#32887);
#29086=LINE('',#371830,#32888);
#29087=LINE('',#371860,#32889);
#29088=LINE('',#371890,#32890);
#29089=LINE('',#371920,#32891);
#29090=LINE('',#371950,#32892);
#29091=LINE('',#371980,#32893);
#29092=LINE('',#372010,#32894);
#29093=LINE('',#372040,#32895);
#29094=LINE('',#372070,#32896);
#29095=LINE('',#372100,#32897);
#29096=LINE('',#372130,#32898);
#29097=LINE('',#372160,#32899);
#29098=LINE('',#372190,#32900);
#29099=LINE('',#372220,#32901);
#29100=LINE('',#372250,#32902);
#29101=LINE('',#372280,#32903);
#29102=LINE('',#372310,#32904);
#29103=LINE('',#372340,#32905);
#29104=LINE('',#372370,#32906);
#29105=LINE('',#372400,#32907);
#29106=LINE('',#372430,#32908);
#29107=LINE('',#372460,#32909);
#29108=LINE('',#372485,#32910);
#29109=LINE('',#372508,#32911);
#29110=LINE('',#372584,#32912);
#29111=LINE('',#372660,#32913);
#29112=LINE('',#372738,#32914);
#29113=LINE('',#372816,#32915);
#29114=LINE('',#372892,#32916);
#29115=LINE('',#372968,#32917);
#29116=LINE('',#373044,#32918);
#29117=LINE('',#373120,#32919);
#29118=LINE('',#373196,#32920);
#29119=LINE('',#373276,#32921);
#29120=LINE('',#373352,#32922);
#29121=LINE('',#373428,#32923);
#29122=LINE('',#373504,#32924);
#29123=LINE('',#373580,#32925);
#29124=LINE('',#373656,#32926);
#29125=LINE('',#373732,#32927);
#29126=LINE('',#373812,#32928);
#29127=LINE('',#373888,#32929);
#29128=LINE('',#373964,#32930);
#29129=LINE('',#374040,#32931);
#29130=LINE('',#374116,#32932);
#29131=LINE('',#374192,#32933);
#29132=LINE('',#374270,#32934);
#29133=LINE('',#374348,#32935);
#29134=LINE('',#374424,#32936);
#29135=LINE('',#374500,#32937);
#29136=LINE('',#374575,#32938);
#29137=LINE('',#374606,#32939);
#29138=LINE('',#374778,#32940);
#29139=LINE('',#374806,#32941);
#29140=LINE('',#375796,#32942);
#29141=LINE('',#376788,#32943);
#29142=LINE('',#376796,#32944);
#29143=LINE('',#376800,#32945);
#29144=LINE('',#376808,#32946);
#29145=LINE('',#376812,#32947);
#29146=LINE('',#376820,#32948);
#29147=LINE('',#376824,#32949);
#29148=LINE('',#376832,#32950);
#29149=LINE('',#376836,#32951);
#29150=LINE('',#376844,#32952);
#29151=LINE('',#376848,#32953);
#29152=LINE('',#376856,#32954);
#29153=LINE('',#376860,#32955);
#29154=LINE('',#376868,#32956);
#29155=LINE('',#376872,#32957);
#29156=LINE('',#376880,#32958);
#29157=LINE('',#376884,#32959);
#29158=LINE('',#376892,#32960);
#29159=LINE('',#376896,#32961);
#29160=LINE('',#376904,#32962);
#29161=LINE('',#376908,#32963);
#29162=LINE('',#376916,#32964);
#29163=LINE('',#376920,#32965);
#29164=LINE('',#376928,#32966);
#29165=LINE('',#376932,#32967);
#29166=LINE('',#376940,#32968);
#29167=LINE('',#376944,#32969);
#29168=LINE('',#376952,#32970);
#29169=LINE('',#376956,#32971);
#29170=LINE('',#376964,#32972);
#29171=LINE('',#376968,#32973);
#29172=LINE('',#376976,#32974);
#29173=LINE('',#376980,#32975);
#29174=LINE('',#376988,#32976);
#29175=LINE('',#376992,#32977);
#29176=LINE('',#377000,#32978);
#29177=LINE('',#377004,#32979);
#29178=LINE('',#377012,#32980);
#29179=LINE('',#377016,#32981);
#29180=LINE('',#377024,#32982);
#29181=LINE('',#377028,#32983);
#29182=LINE('',#377036,#32984);
#29183=LINE('',#377040,#32985);
#29184=LINE('',#377048,#32986);
#29185=LINE('',#377052,#32987);
#29186=LINE('',#377060,#32988);
#29187=LINE('',#377064,#32989);
#29188=LINE('',#377072,#32990);
#29189=LINE('',#377076,#32991);
#29190=LINE('',#377084,#32992);
#29191=LINE('',#377088,#32993);
#29192=LINE('',#377096,#32994);
#29193=LINE('',#377100,#32995);
#29194=LINE('',#377108,#32996);
#29195=LINE('',#377112,#32997);
#29196=LINE('',#377120,#32998);
#29197=LINE('',#377124,#32999);
#29198=LINE('',#377132,#33000);
#29199=LINE('',#377136,#33001);
#29200=LINE('',#377144,#33002);
#29201=LINE('',#377148,#33003);
#29202=LINE('',#377156,#33004);
#29203=LINE('',#377160,#33005);
#29204=LINE('',#377168,#33006);
#29205=LINE('',#377172,#33007);
#29206=LINE('',#377180,#33008);
#29207=LINE('',#377184,#33009);
#29208=LINE('',#377192,#33010);
#29209=LINE('',#377196,#33011);
#29210=LINE('',#377204,#33012);
#29211=LINE('',#377208,#33013);
#29212=LINE('',#377216,#33014);
#29213=LINE('',#377220,#33015);
#29214=LINE('',#377228,#33016);
#29215=LINE('',#377232,#33017);
#29216=LINE('',#377240,#33018);
#29217=LINE('',#377244,#33019);
#29218=LINE('',#377252,#33020);
#29219=LINE('',#377256,#33021);
#29220=LINE('',#377264,#33022);
#29221=LINE('',#377268,#33023);
#29222=LINE('',#377276,#33024);
#29223=LINE('',#377280,#33025);
#29224=LINE('',#377288,#33026);
#29225=LINE('',#377292,#33027);
#29226=LINE('',#377300,#33028);
#29227=LINE('',#377304,#33029);
#29228=LINE('',#377312,#33030);
#29229=LINE('',#377316,#33031);
#29230=LINE('',#377324,#33032);
#29231=LINE('',#377328,#33033);
#29232=LINE('',#377336,#33034);
#29233=LINE('',#377340,#33035);
#29234=LINE('',#377348,#33036);
#29235=LINE('',#377352,#33037);
#29236=LINE('',#377360,#33038);
#29237=LINE('',#377364,#33039);
#29238=LINE('',#377372,#33040);
#29239=LINE('',#377375,#33041);
#29240=LINE('',#377379,#33042);
#29241=LINE('',#377387,#33043);
#29242=LINE('',#377391,#33044);
#29243=LINE('',#377399,#33045);
#29244=LINE('',#377403,#33046);
#29245=LINE('',#377411,#33047);
#29246=LINE('',#377415,#33048);
#29247=LINE('',#377423,#33049);
#29248=LINE('',#377427,#33050);
#29249=LINE('',#377435,#33051);
#29250=LINE('',#377439,#33052);
#29251=LINE('',#377447,#33053);
#29252=LINE('',#377451,#33054);
#29253=LINE('',#377459,#33055);
#29254=LINE('',#377463,#33056);
#29255=LINE('',#377471,#33057);
#29256=LINE('',#377475,#33058);
#29257=LINE('',#377483,#33059);
#29258=LINE('',#377487,#33060);
#29259=LINE('',#377495,#33061);
#29260=LINE('',#377499,#33062);
#29261=LINE('',#377507,#33063);
#29262=LINE('',#377511,#33064);
#29263=LINE('',#377519,#33065);
#29264=LINE('',#377523,#33066);
#29265=LINE('',#377531,#33067);
#29266=LINE('',#377535,#33068);
#29267=LINE('',#377543,#33069);
#29268=LINE('',#377547,#33070);
#29269=LINE('',#377555,#33071);
#29270=LINE('',#377559,#33072);
#29271=LINE('',#377567,#33073);
#29272=LINE('',#377571,#33074);
#29273=LINE('',#377579,#33075);
#29274=LINE('',#377583,#33076);
#29275=LINE('',#377591,#33077);
#29276=LINE('',#377595,#33078);
#29277=LINE('',#377603,#33079);
#29278=LINE('',#377607,#33080);
#29279=LINE('',#377615,#33081);
#29280=LINE('',#377619,#33082);
#29281=LINE('',#377627,#33083);
#29282=LINE('',#377631,#33084);
#29283=LINE('',#377639,#33085);
#29284=LINE('',#377643,#33086);
#29285=LINE('',#377651,#33087);
#29286=LINE('',#377655,#33088);
#29287=LINE('',#377663,#33089);
#29288=LINE('',#377667,#33090);
#29289=LINE('',#377675,#33091);
#29290=LINE('',#377679,#33092);
#29291=LINE('',#377687,#33093);
#29292=LINE('',#377691,#33094);
#29293=LINE('',#377699,#33095);
#29294=LINE('',#377703,#33096);
#29295=LINE('',#377711,#33097);
#29296=LINE('',#377715,#33098);
#29297=LINE('',#377723,#33099);
#29298=LINE('',#377727,#33100);
#29299=LINE('',#377735,#33101);
#29300=LINE('',#377739,#33102);
#29301=LINE('',#377747,#33103);
#29302=LINE('',#377751,#33104);
#29303=LINE('',#377759,#33105);
#29304=LINE('',#377763,#33106);
#29305=LINE('',#377771,#33107);
#29306=LINE('',#377775,#33108);
#29307=LINE('',#377783,#33109);
#29308=LINE('',#377787,#33110);
#29309=LINE('',#377795,#33111);
#29310=LINE('',#377799,#33112);
#29311=LINE('',#377807,#33113);
#29312=LINE('',#377811,#33114);
#29313=LINE('',#377819,#33115);
#29314=LINE('',#377823,#33116);
#29315=LINE('',#377831,#33117);
#29316=LINE('',#377835,#33118);
#29317=LINE('',#377843,#33119);
#29318=LINE('',#377847,#33120);
#29319=LINE('',#377855,#33121);
#29320=LINE('',#377859,#33122);
#29321=LINE('',#377867,#33123);
#29322=LINE('',#377871,#33124);
#29323=LINE('',#377879,#33125);
#29324=LINE('',#377883,#33126);
#29325=LINE('',#377891,#33127);
#29326=LINE('',#377895,#33128);
#29327=LINE('',#377903,#33129);
#29328=LINE('',#377907,#33130);
#29329=LINE('',#377915,#33131);
#29330=LINE('',#377919,#33132);
#29331=LINE('',#377927,#33133);
#29332=LINE('',#377931,#33134);
#29333=LINE('',#377939,#33135);
#29334=LINE('',#377943,#33136);
#29335=LINE('',#377951,#33137);
#29336=LINE('',#377955,#33138);
#29337=LINE('',#377962,#33139);
#29338=LINE('',#378257,#33140);
#29339=LINE('',#378309,#33141);
#29340=LINE('',#378327,#33142);
#29341=LINE('',#378337,#33143);
#29342=LINE('',#378347,#33144);
#29343=LINE('',#378348,#33145);
#29344=LINE('',#378351,#33146);
#29345=LINE('',#378352,#33147);
#29346=LINE('',#378355,#33148);
#29347=LINE('',#378356,#33149);
#29348=LINE('',#378359,#33150);
#29349=LINE('',#378360,#33151);
#29350=LINE('',#378363,#33152);
#29351=LINE('',#378364,#33153);
#29352=LINE('',#378379,#33154);
#29353=LINE('',#378383,#33155);
#29354=LINE('',#378385,#33156);
#29355=LINE('',#378387,#33157);
#29356=LINE('',#378393,#33158);
#29357=LINE('',#378397,#33159);
#29358=LINE('',#378399,#33160);
#29359=LINE('',#378403,#33161);
#29360=LINE('',#380137,#33162);
#29361=LINE('',#380146,#33163);
#29362=LINE('',#380164,#33164);
#29363=LINE('',#380173,#33165);
#29364=LINE('',#380441,#33166);
#29365=LINE('',#380450,#33167);
#29366=LINE('',#380468,#33168);
#29367=LINE('',#380477,#33169);
#29368=LINE('',#380745,#33170);
#29369=LINE('',#380754,#33171);
#29370=LINE('',#380772,#33172);
#29371=LINE('',#380781,#33173);
#29372=LINE('',#381049,#33174);
#29373=LINE('',#381058,#33175);
#29374=LINE('',#381076,#33176);
#29375=LINE('',#381085,#33177);
#29376=LINE('',#381353,#33178);
#29377=LINE('',#381362,#33179);
#29378=LINE('',#381380,#33180);
#29379=LINE('',#381389,#33181);
#29380=LINE('',#381657,#33182);
#29381=LINE('',#381666,#33183);
#29382=LINE('',#381684,#33184);
#29383=LINE('',#381693,#33185);
#29384=LINE('',#381961,#33186);
#29385=LINE('',#381970,#33187);
#29386=LINE('',#381988,#33188);
#29387=LINE('',#381997,#33189);
#29388=LINE('',#382265,#33190);
#29389=LINE('',#382274,#33191);
#29390=LINE('',#382292,#33192);
#29391=LINE('',#382301,#33193);
#29392=LINE('',#382569,#33194);
#29393=LINE('',#382578,#33195);
#29394=LINE('',#382596,#33196);
#29395=LINE('',#382605,#33197);
#29396=LINE('',#382873,#33198);
#29397=LINE('',#382882,#33199);
#29398=LINE('',#382900,#33200);
#29399=LINE('',#382909,#33201);
#29400=LINE('',#383177,#33202);
#29401=LINE('',#383186,#33203);
#29402=LINE('',#383204,#33204);
#29403=LINE('',#383213,#33205);
#29404=LINE('',#383481,#33206);
#29405=LINE('',#383490,#33207);
#29406=LINE('',#383508,#33208);
#29407=LINE('',#383517,#33209);
#29408=LINE('',#383785,#33210);
#29409=LINE('',#383794,#33211);
#29410=LINE('',#383812,#33212);
#29411=LINE('',#383821,#33213);
#29412=LINE('',#384089,#33214);
#29413=LINE('',#384098,#33215);
#29414=LINE('',#384116,#33216);
#29415=LINE('',#384125,#33217);
#29416=LINE('',#384393,#33218);
#29417=LINE('',#384402,#33219);
#29418=LINE('',#384420,#33220);
#29419=LINE('',#384429,#33221);
#29420=LINE('',#384697,#33222);
#29421=LINE('',#384706,#33223);
#29422=LINE('',#384724,#33224);
#29423=LINE('',#384733,#33225);
#29424=LINE('',#385001,#33226);
#29425=LINE('',#385010,#33227);
#29426=LINE('',#385028,#33228);
#29427=LINE('',#385037,#33229);
#29428=LINE('',#385305,#33230);
#29429=LINE('',#385314,#33231);
#29430=LINE('',#385332,#33232);
#29431=LINE('',#385341,#33233);
#29432=LINE('',#385609,#33234);
#29433=LINE('',#385618,#33235);
#29434=LINE('',#385636,#33236);
#29435=LINE('',#385645,#33237);
#29436=LINE('',#385913,#33238);
#29437=LINE('',#385922,#33239);
#29438=LINE('',#385940,#33240);
#29439=LINE('',#385949,#33241);
#29440=LINE('',#386217,#33242);
#29441=LINE('',#386226,#33243);
#29442=LINE('',#386244,#33244);
#29443=LINE('',#386253,#33245);
#29444=LINE('',#386521,#33246);
#29445=LINE('',#386530,#33247);
#29446=LINE('',#386548,#33248);
#29447=LINE('',#386557,#33249);
#29448=LINE('',#386825,#33250);
#29449=LINE('',#386834,#33251);
#29450=LINE('',#386852,#33252);
#29451=LINE('',#386861,#33253);
#29452=LINE('',#387129,#33254);
#29453=LINE('',#387138,#33255);
#29454=LINE('',#387156,#33256);
#29455=LINE('',#387165,#33257);
#29456=LINE('',#387433,#33258);
#29457=LINE('',#387442,#33259);
#29458=LINE('',#387460,#33260);
#29459=LINE('',#387469,#33261);
#29460=LINE('',#387737,#33262);
#29461=LINE('',#387746,#33263);
#29462=LINE('',#387764,#33264);
#29463=LINE('',#387773,#33265);
#29464=LINE('',#388041,#33266);
#29465=LINE('',#388050,#33267);
#29466=LINE('',#388068,#33268);
#29467=LINE('',#388077,#33269);
#29468=LINE('',#388345,#33270);
#29469=LINE('',#388354,#33271);
#29470=LINE('',#388372,#33272);
#29471=LINE('',#388381,#33273);
#29472=LINE('',#388649,#33274);
#29473=LINE('',#388658,#33275);
#29474=LINE('',#388676,#33276);
#29475=LINE('',#388685,#33277);
#29476=LINE('',#388953,#33278);
#29477=LINE('',#388962,#33279);
#29478=LINE('',#388980,#33280);
#29479=LINE('',#388989,#33281);
#29480=LINE('',#389257,#33282);
#29481=LINE('',#389266,#33283);
#29482=LINE('',#389284,#33284);
#29483=LINE('',#389293,#33285);
#29484=LINE('',#389561,#33286);
#29485=LINE('',#389570,#33287);
#29486=LINE('',#389588,#33288);
#29487=LINE('',#389597,#33289);
#29488=LINE('',#389865,#33290);
#29489=LINE('',#389874,#33291);
#29490=LINE('',#389892,#33292);
#29491=LINE('',#389901,#33293);
#29492=LINE('',#390169,#33294);
#29493=LINE('',#390178,#33295);
#29494=LINE('',#390196,#33296);
#29495=LINE('',#390205,#33297);
#29496=LINE('',#390473,#33298);
#29497=LINE('',#390482,#33299);
#29498=LINE('',#390500,#33300);
#29499=LINE('',#390509,#33301);
#29500=LINE('',#390777,#33302);
#29501=LINE('',#390786,#33303);
#29502=LINE('',#390804,#33304);
#29503=LINE('',#390813,#33305);
#29504=LINE('',#391081,#33306);
#29505=LINE('',#391090,#33307);
#29506=LINE('',#391108,#33308);
#29507=LINE('',#391117,#33309);
#29508=LINE('',#391385,#33310);
#29509=LINE('',#391394,#33311);
#29510=LINE('',#391412,#33312);
#29511=LINE('',#391421,#33313);
#29512=LINE('',#391689,#33314);
#29513=LINE('',#391698,#33315);
#29514=LINE('',#391716,#33316);
#29515=LINE('',#391725,#33317);
#29516=LINE('',#391993,#33318);
#29517=LINE('',#392002,#33319);
#29518=LINE('',#392020,#33320);
#29519=LINE('',#392029,#33321);
#29520=LINE('',#392297,#33322);
#29521=LINE('',#392306,#33323);
#29522=LINE('',#392324,#33324);
#29523=LINE('',#392333,#33325);
#29524=LINE('',#392601,#33326);
#29525=LINE('',#392610,#33327);
#29526=LINE('',#392628,#33328);
#29527=LINE('',#392637,#33329);
#29528=LINE('',#392905,#33330);
#29529=LINE('',#392914,#33331);
#29530=LINE('',#392932,#33332);
#29531=LINE('',#392941,#33333);
#29532=LINE('',#393209,#33334);
#29533=LINE('',#393218,#33335);
#29534=LINE('',#393236,#33336);
#29535=LINE('',#393245,#33337);
#29536=LINE('',#393513,#33338);
#29537=LINE('',#393522,#33339);
#29538=LINE('',#393540,#33340);
#29539=LINE('',#393549,#33341);
#29540=LINE('',#393817,#33342);
#29541=LINE('',#393826,#33343);
#29542=LINE('',#393844,#33344);
#29543=LINE('',#393853,#33345);
#29544=LINE('',#394121,#33346);
#29545=LINE('',#394130,#33347);
#29546=LINE('',#394148,#33348);
#29547=LINE('',#394157,#33349);
#29548=LINE('',#394425,#33350);
#29549=LINE('',#394434,#33351);
#29550=LINE('',#394452,#33352);
#29551=LINE('',#394461,#33353);
#29552=LINE('',#394729,#33354);
#29553=LINE('',#394738,#33355);
#29554=LINE('',#394756,#33356);
#29555=LINE('',#394765,#33357);
#29556=LINE('',#395033,#33358);
#29557=LINE('',#395042,#33359);
#29558=LINE('',#395060,#33360);
#29559=LINE('',#395069,#33361);
#29560=LINE('',#395337,#33362);
#29561=LINE('',#395346,#33363);
#29562=LINE('',#395364,#33364);
#29563=LINE('',#395373,#33365);
#29564=LINE('',#395641,#33366);
#29565=LINE('',#395650,#33367);
#29566=LINE('',#395668,#33368);
#29567=LINE('',#395677,#33369);
#29568=LINE('',#395945,#33370);
#29569=LINE('',#395954,#33371);
#29570=LINE('',#395972,#33372);
#29571=LINE('',#395981,#33373);
#29572=LINE('',#396249,#33374);
#29573=LINE('',#396258,#33375);
#29574=LINE('',#396276,#33376);
#29575=LINE('',#396285,#33377);
#29576=LINE('',#396553,#33378);
#29577=LINE('',#396562,#33379);
#29578=LINE('',#396580,#33380);
#29579=LINE('',#396589,#33381);
#29580=LINE('',#396857,#33382);
#29581=LINE('',#396866,#33383);
#29582=LINE('',#396884,#33384);
#29583=LINE('',#396893,#33385);
#29584=LINE('',#397161,#33386);
#29585=LINE('',#397170,#33387);
#29586=LINE('',#397188,#33388);
#29587=LINE('',#397197,#33389);
#29588=LINE('',#397465,#33390);
#29589=LINE('',#397474,#33391);
#29590=LINE('',#397492,#33392);
#29591=LINE('',#397501,#33393);
#29592=LINE('',#397769,#33394);
#29593=LINE('',#397778,#33395);
#29594=LINE('',#397796,#33396);
#29595=LINE('',#397805,#33397);
#29596=LINE('',#398073,#33398);
#29597=LINE('',#398082,#33399);
#29598=LINE('',#398100,#33400);
#29599=LINE('',#398109,#33401);
#29600=LINE('',#398377,#33402);
#29601=LINE('',#398386,#33403);
#29602=LINE('',#398404,#33404);
#29603=LINE('',#398413,#33405);
#29604=LINE('',#398681,#33406);
#29605=LINE('',#398690,#33407);
#29606=LINE('',#398708,#33408);
#29607=LINE('',#398717,#33409);
#29608=LINE('',#398985,#33410);
#29609=LINE('',#398994,#33411);
#29610=LINE('',#399012,#33412);
#29611=LINE('',#399021,#33413);
#29612=LINE('',#399289,#33414);
#29613=LINE('',#399298,#33415);
#29614=LINE('',#399316,#33416);
#29615=LINE('',#399325,#33417);
#29616=LINE('',#399593,#33418);
#29617=LINE('',#399602,#33419);
#29618=LINE('',#399620,#33420);
#29619=LINE('',#399629,#33421);
#29620=LINE('',#399897,#33422);
#29621=LINE('',#399906,#33423);
#29622=LINE('',#399924,#33424);
#29623=LINE('',#399933,#33425);
#29624=LINE('',#400201,#33426);
#29625=LINE('',#400210,#33427);
#29626=LINE('',#400228,#33428);
#29627=LINE('',#400237,#33429);
#29628=LINE('',#400505,#33430);
#29629=LINE('',#400514,#33431);
#29630=LINE('',#400532,#33432);
#29631=LINE('',#400541,#33433);
#29632=LINE('',#400809,#33434);
#29633=LINE('',#400818,#33435);
#29634=LINE('',#400836,#33436);
#29635=LINE('',#400845,#33437);
#29636=LINE('',#401113,#33438);
#29637=LINE('',#401122,#33439);
#29638=LINE('',#401140,#33440);
#29639=LINE('',#401149,#33441);
#29640=LINE('',#401417,#33442);
#29641=LINE('',#401426,#33443);
#29642=LINE('',#401444,#33444);
#29643=LINE('',#401453,#33445);
#29644=LINE('',#401721,#33446);
#29645=LINE('',#401730,#33447);
#29646=LINE('',#401748,#33448);
#29647=LINE('',#401757,#33449);
#29648=LINE('',#402025,#33450);
#29649=LINE('',#402034,#33451);
#29650=LINE('',#402052,#33452);
#29651=LINE('',#402061,#33453);
#29652=LINE('',#402329,#33454);
#29653=LINE('',#402338,#33455);
#29654=LINE('',#402356,#33456);
#29655=LINE('',#402365,#33457);
#29656=LINE('',#402633,#33458);
#29657=LINE('',#402642,#33459);
#29658=LINE('',#402660,#33460);
#29659=LINE('',#402669,#33461);
#29660=LINE('',#402937,#33462);
#29661=LINE('',#402946,#33463);
#29662=LINE('',#402964,#33464);
#29663=LINE('',#402973,#33465);
#29664=LINE('',#403241,#33466);
#29665=LINE('',#403250,#33467);
#29666=LINE('',#403268,#33468);
#29667=LINE('',#403277,#33469);
#29668=LINE('',#403545,#33470);
#29669=LINE('',#403554,#33471);
#29670=LINE('',#403572,#33472);
#29671=LINE('',#403581,#33473);
#29672=LINE('',#403849,#33474);
#29673=LINE('',#403858,#33475);
#29674=LINE('',#403876,#33476);
#29675=LINE('',#403885,#33477);
#29676=LINE('',#404153,#33478);
#29677=LINE('',#404162,#33479);
#29678=LINE('',#404180,#33480);
#29679=LINE('',#404189,#33481);
#29680=LINE('',#404457,#33482);
#29681=LINE('',#404466,#33483);
#29682=LINE('',#404484,#33484);
#29683=LINE('',#404493,#33485);
#29684=LINE('',#404761,#33486);
#29685=LINE('',#404770,#33487);
#29686=LINE('',#404788,#33488);
#29687=LINE('',#404797,#33489);
#29688=LINE('',#405065,#33490);
#29689=LINE('',#405074,#33491);
#29690=LINE('',#405092,#33492);
#29691=LINE('',#405101,#33493);
#29692=LINE('',#405369,#33494);
#29693=LINE('',#405378,#33495);
#29694=LINE('',#405396,#33496);
#29695=LINE('',#405405,#33497);
#29696=LINE('',#405673,#33498);
#29697=LINE('',#405682,#33499);
#29698=LINE('',#405700,#33500);
#29699=LINE('',#405709,#33501);
#29700=LINE('',#405977,#33502);
#29701=LINE('',#405986,#33503);
#29702=LINE('',#406004,#33504);
#29703=LINE('',#406013,#33505);
#29704=LINE('',#406281,#33506);
#29705=LINE('',#406290,#33507);
#29706=LINE('',#406308,#33508);
#29707=LINE('',#406317,#33509);
#29708=LINE('',#406585,#33510);
#29709=LINE('',#406594,#33511);
#29710=LINE('',#406612,#33512);
#29711=LINE('',#406621,#33513);
#29712=LINE('',#406889,#33514);
#29713=LINE('',#406898,#33515);
#29714=LINE('',#406916,#33516);
#29715=LINE('',#406925,#33517);
#29716=LINE('',#407193,#33518);
#29717=LINE('',#407202,#33519);
#29718=LINE('',#407220,#33520);
#29719=LINE('',#407229,#33521);
#29720=LINE('',#407497,#33522);
#29721=LINE('',#407506,#33523);
#29722=LINE('',#407524,#33524);
#29723=LINE('',#407533,#33525);
#29724=LINE('',#407801,#33526);
#29725=LINE('',#407810,#33527);
#29726=LINE('',#407828,#33528);
#29727=LINE('',#407837,#33529);
#29728=LINE('',#408105,#33530);
#29729=LINE('',#408114,#33531);
#29730=LINE('',#408132,#33532);
#29731=LINE('',#408141,#33533);
#29732=LINE('',#408409,#33534);
#29733=LINE('',#408418,#33535);
#29734=LINE('',#408436,#33536);
#29735=LINE('',#408445,#33537);
#29736=LINE('',#408713,#33538);
#29737=LINE('',#408722,#33539);
#29738=LINE('',#408740,#33540);
#29739=LINE('',#408749,#33541);
#29740=LINE('',#409017,#33542);
#29741=LINE('',#409026,#33543);
#29742=LINE('',#409044,#33544);
#29743=LINE('',#409053,#33545);
#29744=LINE('',#409321,#33546);
#29745=LINE('',#409330,#33547);
#29746=LINE('',#409348,#33548);
#29747=LINE('',#409357,#33549);
#29748=LINE('',#409626,#33550);
#29749=LINE('',#409635,#33551);
#29750=LINE('',#409665,#33552);
#29751=LINE('',#409695,#33553);
#29752=LINE('',#409725,#33554);
#29753=LINE('',#409755,#33555);
#29754=LINE('',#409785,#33556);
#29755=LINE('',#409815,#33557);
#29756=LINE('',#409845,#33558);
#29757=LINE('',#409875,#33559);
#29758=LINE('',#409905,#33560);
#29759=LINE('',#409935,#33561);
#29760=LINE('',#409965,#33562);
#29761=LINE('',#409995,#33563);
#29762=LINE('',#410025,#33564);
#29763=LINE('',#410055,#33565);
#29764=LINE('',#410085,#33566);
#29765=LINE('',#410115,#33567);
#29766=LINE('',#410145,#33568);
#29767=LINE('',#410175,#33569);
#29768=LINE('',#410205,#33570);
#29769=LINE('',#410235,#33571);
#29770=LINE('',#410265,#33572);
#29771=LINE('',#410295,#33573);
#29772=LINE('',#410325,#33574);
#29773=LINE('',#410355,#33575);
#29774=LINE('',#410385,#33576);
#29775=LINE('',#410415,#33577);
#29776=LINE('',#410445,#33578);
#29777=LINE('',#410475,#33579);
#29778=LINE('',#410505,#33580);
#29779=LINE('',#410535,#33581);
#29780=LINE('',#410565,#33582);
#29781=LINE('',#410595,#33583);
#29782=LINE('',#410625,#33584);
#29783=LINE('',#410655,#33585);
#29784=LINE('',#410685,#33586);
#29785=LINE('',#410716,#33587);
#29786=LINE('',#410741,#33588);
#29787=LINE('',#410782,#33589);
#29788=LINE('',#410858,#33590);
#29789=LINE('',#410936,#33591);
#29790=LINE('',#411014,#33592);
#29791=LINE('',#411090,#33593);
#29792=LINE('',#411166,#33594);
#29793=LINE('',#411242,#33595);
#29794=LINE('',#411320,#33596);
#29795=LINE('',#411396,#33597);
#29796=LINE('',#411472,#33598);
#29797=LINE('',#411550,#33599);
#29798=LINE('',#411626,#33600);
#29799=LINE('',#411702,#33601);
#29800=LINE('',#411778,#33602);
#29801=LINE('',#411856,#33603);
#29802=LINE('',#411932,#33604);
#29803=LINE('',#412008,#33605);
#29804=LINE('',#412086,#33606);
#29805=LINE('',#412162,#33607);
#29806=LINE('',#412238,#33608);
#29807=LINE('',#412316,#33609);
#29808=LINE('',#412392,#33610);
#29809=LINE('',#412468,#33611);
#29810=LINE('',#412546,#33612);
#29811=LINE('',#412622,#33613);
#29812=LINE('',#412698,#33614);
#29813=LINE('',#412774,#33615);
#29814=LINE('',#412852,#33616);
#29815=LINE('',#412928,#33617);
#29816=LINE('',#413004,#33618);
#29817=LINE('',#413082,#33619);
#29818=LINE('',#413163,#33620);
#29819=LINE('',#413239,#33621);
#29820=LINE('',#413317,#33622);
#29821=LINE('',#413354,#33623);
#29822=LINE('',#414198,#33624);
#29823=LINE('',#414235,#33625);
#29824=LINE('',#414263,#33626);
#29825=LINE('',#414288,#33627);
#29826=LINE('',#414292,#33628);
#29827=LINE('',#414320,#33629);
#29828=LINE('',#414324,#33630);
#29829=LINE('',#414352,#33631);
#29830=LINE('',#414356,#33632);
#29831=LINE('',#414384,#33633);
#29832=LINE('',#414388,#33634);
#29833=LINE('',#414416,#33635);
#29834=LINE('',#414420,#33636);
#29835=LINE('',#414448,#33637);
#29836=LINE('',#414452,#33638);
#29837=LINE('',#414480,#33639);
#29838=LINE('',#414484,#33640);
#29839=LINE('',#414512,#33641);
#29840=LINE('',#414516,#33642);
#29841=LINE('',#414544,#33643);
#29842=LINE('',#414548,#33644);
#29843=LINE('',#414576,#33645);
#29844=LINE('',#414580,#33646);
#29845=LINE('',#414608,#33647);
#29846=LINE('',#414612,#33648);
#29847=LINE('',#414640,#33649);
#29848=LINE('',#414644,#33650);
#29849=LINE('',#414672,#33651);
#29850=LINE('',#414676,#33652);
#29851=LINE('',#414704,#33653);
#29852=LINE('',#414708,#33654);
#29853=LINE('',#414736,#33655);
#29854=LINE('',#414740,#33656);
#29855=LINE('',#414768,#33657);
#29856=LINE('',#414772,#33658);
#29857=LINE('',#414800,#33659);
#29858=LINE('',#414804,#33660);
#29859=LINE('',#414832,#33661);
#29860=LINE('',#414836,#33662);
#29861=LINE('',#414864,#33663);
#29862=LINE('',#414868,#33664);
#29863=LINE('',#414896,#33665);
#29864=LINE('',#414900,#33666);
#29865=LINE('',#414928,#33667);
#29866=LINE('',#414932,#33668);
#29867=LINE('',#414960,#33669);
#29868=LINE('',#414964,#33670);
#29869=LINE('',#414992,#33671);
#29870=LINE('',#414996,#33672);
#29871=LINE('',#415024,#33673);
#29872=LINE('',#415028,#33674);
#29873=LINE('',#415056,#33675);
#29874=LINE('',#415060,#33676);
#29875=LINE('',#415088,#33677);
#29876=LINE('',#415092,#33678);
#29877=LINE('',#415120,#33679);
#29878=LINE('',#415124,#33680);
#29879=LINE('',#415152,#33681);
#29880=LINE('',#415156,#33682);
#29881=LINE('',#415184,#33683);
#29882=LINE('',#415188,#33684);
#29883=LINE('',#415216,#33685);
#29884=LINE('',#415220,#33686);
#29885=LINE('',#415248,#33687);
#29886=LINE('',#415252,#33688);
#29887=LINE('',#415280,#33689);
#29888=LINE('',#415284,#33690);
#29889=LINE('',#415312,#33691);
#29890=LINE('',#415316,#33692);
#29891=LINE('',#415344,#33693);
#29892=LINE('',#415348,#33694);
#29893=LINE('',#415376,#33695);
#29894=LINE('',#415380,#33696);
#29895=LINE('',#415408,#33697);
#29896=LINE('',#415412,#33698);
#29897=LINE('',#415440,#33699);
#29898=LINE('',#415444,#33700);
#29899=LINE('',#415472,#33701);
#29900=LINE('',#415476,#33702);
#29901=LINE('',#415504,#33703);
#29902=LINE('',#415508,#33704);
#29903=LINE('',#415515,#33705);
#29904=LINE('',#415543,#33706);
#29905=LINE('',#415547,#33707);
#29906=LINE('',#415575,#33708);
#29907=LINE('',#415579,#33709);
#29908=LINE('',#415607,#33710);
#29909=LINE('',#415611,#33711);
#29910=LINE('',#415639,#33712);
#29911=LINE('',#415643,#33713);
#29912=LINE('',#415671,#33714);
#29913=LINE('',#415675,#33715);
#29914=LINE('',#415703,#33716);
#29915=LINE('',#415707,#33717);
#29916=LINE('',#415735,#33718);
#29917=LINE('',#415739,#33719);
#29918=LINE('',#415767,#33720);
#29919=LINE('',#415771,#33721);
#29920=LINE('',#415799,#33722);
#29921=LINE('',#415803,#33723);
#29922=LINE('',#415831,#33724);
#29923=LINE('',#415835,#33725);
#29924=LINE('',#415863,#33726);
#29925=LINE('',#415867,#33727);
#29926=LINE('',#415895,#33728);
#29927=LINE('',#415899,#33729);
#29928=LINE('',#415927,#33730);
#29929=LINE('',#415931,#33731);
#29930=LINE('',#415959,#33732);
#29931=LINE('',#415963,#33733);
#29932=LINE('',#415991,#33734);
#29933=LINE('',#415995,#33735);
#29934=LINE('',#416023,#33736);
#29935=LINE('',#416027,#33737);
#29936=LINE('',#416055,#33738);
#29937=LINE('',#416059,#33739);
#29938=LINE('',#416087,#33740);
#29939=LINE('',#416091,#33741);
#29940=LINE('',#416119,#33742);
#29941=LINE('',#416123,#33743);
#29942=LINE('',#416151,#33744);
#29943=LINE('',#416155,#33745);
#29944=LINE('',#416183,#33746);
#29945=LINE('',#416187,#33747);
#29946=LINE('',#416215,#33748);
#29947=LINE('',#416219,#33749);
#29948=LINE('',#416247,#33750);
#29949=LINE('',#416251,#33751);
#29950=LINE('',#416279,#33752);
#29951=LINE('',#416283,#33753);
#29952=LINE('',#416311,#33754);
#29953=LINE('',#416315,#33755);
#29954=LINE('',#416343,#33756);
#29955=LINE('',#416347,#33757);
#29956=LINE('',#416375,#33758);
#29957=LINE('',#416379,#33759);
#29958=LINE('',#416407,#33760);
#29959=LINE('',#416411,#33761);
#29960=LINE('',#416439,#33762);
#29961=LINE('',#416443,#33763);
#29962=LINE('',#416471,#33764);
#29963=LINE('',#416475,#33765);
#29964=LINE('',#416503,#33766);
#29965=LINE('',#416507,#33767);
#29966=LINE('',#416535,#33768);
#29967=LINE('',#416539,#33769);
#29968=LINE('',#416567,#33770);
#29969=LINE('',#416571,#33771);
#29970=LINE('',#416599,#33772);
#29971=LINE('',#416603,#33773);
#29972=LINE('',#416631,#33774);
#29973=LINE('',#416635,#33775);
#29974=LINE('',#416663,#33776);
#29975=LINE('',#416667,#33777);
#29976=LINE('',#416695,#33778);
#29977=LINE('',#416699,#33779);
#29978=LINE('',#416727,#33780);
#29979=LINE('',#416731,#33781);
#29980=LINE('',#416754,#33782);
#29981=LINE('',#416789,#33783);
#29982=LINE('',#416793,#33784);
#29983=LINE('',#416828,#33785);
#29984=LINE('',#416832,#33786);
#29985=LINE('',#416867,#33787);
#29986=LINE('',#416871,#33788);
#29987=LINE('',#416906,#33789);
#29988=LINE('',#416910,#33790);
#29989=LINE('',#416945,#33791);
#29990=LINE('',#416949,#33792);
#29991=LINE('',#416984,#33793);
#29992=LINE('',#416988,#33794);
#29993=LINE('',#417023,#33795);
#29994=LINE('',#417027,#33796);
#29995=LINE('',#417062,#33797);
#29996=LINE('',#417066,#33798);
#29997=LINE('',#417101,#33799);
#29998=LINE('',#417105,#33800);
#29999=LINE('',#417140,#33801);
#30000=LINE('',#417144,#33802);
#30001=LINE('',#417179,#33803);
#30002=LINE('',#417183,#33804);
#30003=LINE('',#417218,#33805);
#30004=LINE('',#417222,#33806);
#30005=LINE('',#417257,#33807);
#30006=LINE('',#417261,#33808);
#30007=LINE('',#417296,#33809);
#30008=LINE('',#417300,#33810);
#30009=LINE('',#417335,#33811);
#30010=LINE('',#417339,#33812);
#30011=LINE('',#417374,#33813);
#30012=LINE('',#417378,#33814);
#30013=LINE('',#417413,#33815);
#30014=LINE('',#417417,#33816);
#30015=LINE('',#417452,#33817);
#30016=LINE('',#417456,#33818);
#30017=LINE('',#417491,#33819);
#30018=LINE('',#417495,#33820);
#30019=LINE('',#417530,#33821);
#30020=LINE('',#417534,#33822);
#30021=LINE('',#417569,#33823);
#30022=LINE('',#417573,#33824);
#30023=LINE('',#417608,#33825);
#30024=LINE('',#417612,#33826);
#30025=LINE('',#417647,#33827);
#30026=LINE('',#417651,#33828);
#30027=LINE('',#417686,#33829);
#30028=LINE('',#417690,#33830);
#30029=LINE('',#417725,#33831);
#30030=LINE('',#417729,#33832);
#30031=LINE('',#417764,#33833);
#30032=LINE('',#417768,#33834);
#30033=LINE('',#417803,#33835);
#30034=LINE('',#417807,#33836);
#30035=LINE('',#417842,#33837);
#30036=LINE('',#417846,#33838);
#30037=LINE('',#417881,#33839);
#30038=LINE('',#417885,#33840);
#30039=LINE('',#417920,#33841);
#30040=LINE('',#417924,#33842);
#30041=LINE('',#417959,#33843);
#30042=LINE('',#417963,#33844);
#30043=LINE('',#417998,#33845);
#30044=LINE('',#418002,#33846);
#30045=LINE('',#418037,#33847);
#30046=LINE('',#418041,#33848);
#30047=LINE('',#418076,#33849);
#30048=LINE('',#418080,#33850);
#30049=LINE('',#418115,#33851);
#30050=LINE('',#418119,#33852);
#30051=LINE('',#418154,#33853);
#30052=LINE('',#418158,#33854);
#30053=LINE('',#418193,#33855);
#30054=LINE('',#418197,#33856);
#30055=LINE('',#418232,#33857);
#30056=LINE('',#418236,#33858);
#30057=LINE('',#418253,#33859);
#30058=LINE('',#418272,#33860);
#30059=LINE('',#418276,#33861);
#30060=LINE('',#418311,#33862);
#30061=LINE('',#418315,#33863);
#30062=LINE('',#418350,#33864);
#30063=LINE('',#418354,#33865);
#30064=LINE('',#418389,#33866);
#30065=LINE('',#418393,#33867);
#30066=LINE('',#418428,#33868);
#30067=LINE('',#418432,#33869);
#30068=LINE('',#418467,#33870);
#30069=LINE('',#418471,#33871);
#30070=LINE('',#418506,#33872);
#30071=LINE('',#418510,#33873);
#30072=LINE('',#418545,#33874);
#30073=LINE('',#418549,#33875);
#30074=LINE('',#418584,#33876);
#30075=LINE('',#418588,#33877);
#30076=LINE('',#418623,#33878);
#30077=LINE('',#418627,#33879);
#30078=LINE('',#418662,#33880);
#30079=LINE('',#418666,#33881);
#30080=LINE('',#418701,#33882);
#30081=LINE('',#418705,#33883);
#30082=LINE('',#418740,#33884);
#30083=LINE('',#418744,#33885);
#30084=LINE('',#418779,#33886);
#30085=LINE('',#418783,#33887);
#30086=LINE('',#418818,#33888);
#30087=LINE('',#418822,#33889);
#30088=LINE('',#418857,#33890);
#30089=LINE('',#418861,#33891);
#30090=LINE('',#418896,#33892);
#30091=LINE('',#418900,#33893);
#30092=LINE('',#418935,#33894);
#30093=LINE('',#418939,#33895);
#30094=LINE('',#418974,#33896);
#30095=LINE('',#418978,#33897);
#30096=LINE('',#419013,#33898);
#30097=LINE('',#419017,#33899);
#30098=LINE('',#419052,#33900);
#30099=LINE('',#419056,#33901);
#30100=LINE('',#419091,#33902);
#30101=LINE('',#419095,#33903);
#30102=LINE('',#419130,#33904);
#30103=LINE('',#419134,#33905);
#30104=LINE('',#419169,#33906);
#30105=LINE('',#419173,#33907);
#30106=LINE('',#419208,#33908);
#30107=LINE('',#419212,#33909);
#30108=LINE('',#419247,#33910);
#30109=LINE('',#419251,#33911);
#30110=LINE('',#419286,#33912);
#30111=LINE('',#419290,#33913);
#30112=LINE('',#419325,#33914);
#30113=LINE('',#419329,#33915);
#30114=LINE('',#419364,#33916);
#30115=LINE('',#419368,#33917);
#30116=LINE('',#419403,#33918);
#30117=LINE('',#419407,#33919);
#30118=LINE('',#419442,#33920);
#30119=LINE('',#419446,#33921);
#30120=LINE('',#419481,#33922);
#30121=LINE('',#419485,#33923);
#30122=LINE('',#419520,#33924);
#30123=LINE('',#419524,#33925);
#30124=LINE('',#419559,#33926);
#30125=LINE('',#419563,#33927);
#30126=LINE('',#419598,#33928);
#30127=LINE('',#419602,#33929);
#30128=LINE('',#419637,#33930);
#30129=LINE('',#419641,#33931);
#30130=LINE('',#419676,#33932);
#30131=LINE('',#419680,#33933);
#30132=LINE('',#419715,#33934);
#30133=LINE('',#419719,#33935);
#30134=LINE('',#419753,#33936);
#30135=LINE('',#419985,#33937);
#30136=LINE('',#420054,#33938);
#30137=LINE('',#420062,#33939);
#30138=LINE('',#420068,#33940);
#30139=LINE('',#420071,#33941);
#30140=LINE('',#420075,#33942);
#30141=LINE('',#420083,#33943);
#30142=LINE('',#420084,#33944);
#30143=LINE('',#420087,#33945);
#30144=LINE('',#420088,#33946);
#30145=LINE('',#420091,#33947);
#30146=LINE('',#420092,#33948);
#30147=LINE('',#420095,#33949);
#30148=LINE('',#420096,#33950);
#30149=LINE('',#420099,#33951);
#30150=LINE('',#420100,#33952);
#30151=LINE('',#420115,#33953);
#30152=LINE('',#420120,#33954);
#30153=LINE('',#420121,#33955);
#30154=LINE('',#420123,#33956);
#30155=LINE('',#420125,#33957);
#30156=LINE('',#420130,#33958);
#30157=LINE('',#420135,#33959);
#30158=LINE('',#420143,#33960);
#30159=LINE('',#422870,#33961);
#30160=LINE('',#422872,#33962);
#30161=LINE('',#422876,#33963);
#30162=LINE('',#422886,#33964);
#30163=LINE('',#422888,#33965);
#30164=LINE('',#422894,#33966);
#30165=LINE('',#423219,#33967);
#30166=LINE('',#423221,#33968);
#30167=LINE('',#423225,#33969);
#30168=LINE('',#423235,#33970);
#30169=LINE('',#423237,#33971);
#30170=LINE('',#423243,#33972);
#30171=LINE('',#423568,#33973);
#30172=LINE('',#423570,#33974);
#30173=LINE('',#423574,#33975);
#30174=LINE('',#423584,#33976);
#30175=LINE('',#423586,#33977);
#30176=LINE('',#423592,#33978);
#30177=LINE('',#423917,#33979);
#30178=LINE('',#423919,#33980);
#30179=LINE('',#423923,#33981);
#30180=LINE('',#423933,#33982);
#30181=LINE('',#423935,#33983);
#30182=LINE('',#423941,#33984);
#30183=LINE('',#424266,#33985);
#30184=LINE('',#424268,#33986);
#30185=LINE('',#424272,#33987);
#30186=LINE('',#424282,#33988);
#30187=LINE('',#424284,#33989);
#30188=LINE('',#424290,#33990);
#30189=LINE('',#424615,#33991);
#30190=LINE('',#424617,#33992);
#30191=LINE('',#424621,#33993);
#30192=LINE('',#424631,#33994);
#30193=LINE('',#424633,#33995);
#30194=LINE('',#424639,#33996);
#30195=LINE('',#424964,#33997);
#30196=LINE('',#424966,#33998);
#30197=LINE('',#424970,#33999);
#30198=LINE('',#424980,#34000);
#30199=LINE('',#424982,#34001);
#30200=LINE('',#424988,#34002);
#30201=LINE('',#425313,#34003);
#30202=LINE('',#425315,#34004);
#30203=LINE('',#425319,#34005);
#30204=LINE('',#425329,#34006);
#30205=LINE('',#425331,#34007);
#30206=LINE('',#425337,#34008);
#30207=LINE('',#425662,#34009);
#30208=LINE('',#425664,#34010);
#30209=LINE('',#425668,#34011);
#30210=LINE('',#425678,#34012);
#30211=LINE('',#425680,#34013);
#30212=LINE('',#425686,#34014);
#30213=LINE('',#426011,#34015);
#30214=LINE('',#426013,#34016);
#30215=LINE('',#426017,#34017);
#30216=LINE('',#426027,#34018);
#30217=LINE('',#426029,#34019);
#30218=LINE('',#426035,#34020);
#30219=LINE('',#426360,#34021);
#30220=LINE('',#426362,#34022);
#30221=LINE('',#426366,#34023);
#30222=LINE('',#426376,#34024);
#30223=LINE('',#426378,#34025);
#30224=LINE('',#426384,#34026);
#30225=LINE('',#426709,#34027);
#30226=LINE('',#426711,#34028);
#30227=LINE('',#426715,#34029);
#30228=LINE('',#426725,#34030);
#30229=LINE('',#426727,#34031);
#30230=LINE('',#426733,#34032);
#30231=LINE('',#427058,#34033);
#30232=LINE('',#427060,#34034);
#30233=LINE('',#427064,#34035);
#30234=LINE('',#427074,#34036);
#30235=LINE('',#427076,#34037);
#30236=LINE('',#427082,#34038);
#30237=LINE('',#427407,#34039);
#30238=LINE('',#427409,#34040);
#30239=LINE('',#427413,#34041);
#30240=LINE('',#427423,#34042);
#30241=LINE('',#427425,#34043);
#30242=LINE('',#427431,#34044);
#30243=LINE('',#427756,#34045);
#30244=LINE('',#427758,#34046);
#30245=LINE('',#427762,#34047);
#30246=LINE('',#427772,#34048);
#30247=LINE('',#427774,#34049);
#30248=LINE('',#427780,#34050);
#30249=LINE('',#428105,#34051);
#30250=LINE('',#428107,#34052);
#30251=LINE('',#428111,#34053);
#30252=LINE('',#428121,#34054);
#30253=LINE('',#428123,#34055);
#30254=LINE('',#428129,#34056);
#30255=LINE('',#428454,#34057);
#30256=LINE('',#428456,#34058);
#30257=LINE('',#428460,#34059);
#30258=LINE('',#428470,#34060);
#30259=LINE('',#428472,#34061);
#30260=LINE('',#428478,#34062);
#30261=LINE('',#428803,#34063);
#30262=LINE('',#428805,#34064);
#30263=LINE('',#428809,#34065);
#30264=LINE('',#428819,#34066);
#30265=LINE('',#428821,#34067);
#30266=LINE('',#428827,#34068);
#30267=LINE('',#429152,#34069);
#30268=LINE('',#429154,#34070);
#30269=LINE('',#429158,#34071);
#30270=LINE('',#429168,#34072);
#30271=LINE('',#429170,#34073);
#30272=LINE('',#429176,#34074);
#30273=LINE('',#429501,#34075);
#30274=LINE('',#429503,#34076);
#30275=LINE('',#429507,#34077);
#30276=LINE('',#429517,#34078);
#30277=LINE('',#429519,#34079);
#30278=LINE('',#429525,#34080);
#30279=LINE('',#429850,#34081);
#30280=LINE('',#429852,#34082);
#30281=LINE('',#429856,#34083);
#30282=LINE('',#429866,#34084);
#30283=LINE('',#429868,#34085);
#30284=LINE('',#429874,#34086);
#30285=LINE('',#430199,#34087);
#30286=LINE('',#430201,#34088);
#30287=LINE('',#430205,#34089);
#30288=LINE('',#430215,#34090);
#30289=LINE('',#430217,#34091);
#30290=LINE('',#430223,#34092);
#30291=LINE('',#430548,#34093);
#30292=LINE('',#430550,#34094);
#30293=LINE('',#430554,#34095);
#30294=LINE('',#430564,#34096);
#30295=LINE('',#430566,#34097);
#30296=LINE('',#430572,#34098);
#30297=LINE('',#430897,#34099);
#30298=LINE('',#430899,#34100);
#30299=LINE('',#430903,#34101);
#30300=LINE('',#430913,#34102);
#30301=LINE('',#430915,#34103);
#30302=LINE('',#430921,#34104);
#30303=LINE('',#431246,#34105);
#30304=LINE('',#431248,#34106);
#30305=LINE('',#431252,#34107);
#30306=LINE('',#431262,#34108);
#30307=LINE('',#431264,#34109);
#30308=LINE('',#431270,#34110);
#30309=LINE('',#431595,#34111);
#30310=LINE('',#431597,#34112);
#30311=LINE('',#431601,#34113);
#30312=LINE('',#431611,#34114);
#30313=LINE('',#431613,#34115);
#30314=LINE('',#431619,#34116);
#30315=LINE('',#431944,#34117);
#30316=LINE('',#431946,#34118);
#30317=LINE('',#431950,#34119);
#30318=LINE('',#431960,#34120);
#30319=LINE('',#431962,#34121);
#30320=LINE('',#431968,#34122);
#30321=LINE('',#432293,#34123);
#30322=LINE('',#432295,#34124);
#30323=LINE('',#432299,#34125);
#30324=LINE('',#432309,#34126);
#30325=LINE('',#432311,#34127);
#30326=LINE('',#432317,#34128);
#30327=LINE('',#432642,#34129);
#30328=LINE('',#432644,#34130);
#30329=LINE('',#432648,#34131);
#30330=LINE('',#432658,#34132);
#30331=LINE('',#432660,#34133);
#30332=LINE('',#432666,#34134);
#30333=LINE('',#432991,#34135);
#30334=LINE('',#432993,#34136);
#30335=LINE('',#432997,#34137);
#30336=LINE('',#433007,#34138);
#30337=LINE('',#433009,#34139);
#30338=LINE('',#433015,#34140);
#30339=LINE('',#433340,#34141);
#30340=LINE('',#433342,#34142);
#30341=LINE('',#433346,#34143);
#30342=LINE('',#433356,#34144);
#30343=LINE('',#433358,#34145);
#30344=LINE('',#433364,#34146);
#30345=LINE('',#433689,#34147);
#30346=LINE('',#433691,#34148);
#30347=LINE('',#433695,#34149);
#30348=LINE('',#433705,#34150);
#30349=LINE('',#433707,#34151);
#30350=LINE('',#433713,#34152);
#30351=LINE('',#434038,#34153);
#30352=LINE('',#434040,#34154);
#30353=LINE('',#434044,#34155);
#30354=LINE('',#434054,#34156);
#30355=LINE('',#434056,#34157);
#30356=LINE('',#434062,#34158);
#30357=LINE('',#434387,#34159);
#30358=LINE('',#434389,#34160);
#30359=LINE('',#434393,#34161);
#30360=LINE('',#434403,#34162);
#30361=LINE('',#434405,#34163);
#30362=LINE('',#434411,#34164);
#30363=LINE('',#434736,#34165);
#30364=LINE('',#434738,#34166);
#30365=LINE('',#434742,#34167);
#30366=LINE('',#434752,#34168);
#30367=LINE('',#434754,#34169);
#30368=LINE('',#434760,#34170);
#30369=LINE('',#435085,#34171);
#30370=LINE('',#435087,#34172);
#30371=LINE('',#435091,#34173);
#30372=LINE('',#435101,#34174);
#30373=LINE('',#435103,#34175);
#30374=LINE('',#435109,#34176);
#30375=LINE('',#435434,#34177);
#30376=LINE('',#435436,#34178);
#30377=LINE('',#435440,#34179);
#30378=LINE('',#435450,#34180);
#30379=LINE('',#435452,#34181);
#30380=LINE('',#435458,#34182);
#30381=LINE('',#435783,#34183);
#30382=LINE('',#435785,#34184);
#30383=LINE('',#435789,#34185);
#30384=LINE('',#435799,#34186);
#30385=LINE('',#435801,#34187);
#30386=LINE('',#435807,#34188);
#30387=LINE('',#436132,#34189);
#30388=LINE('',#436134,#34190);
#30389=LINE('',#436138,#34191);
#30390=LINE('',#436148,#34192);
#30391=LINE('',#436150,#34193);
#30392=LINE('',#436156,#34194);
#30393=LINE('',#436481,#34195);
#30394=LINE('',#436483,#34196);
#30395=LINE('',#436487,#34197);
#30396=LINE('',#436497,#34198);
#30397=LINE('',#436499,#34199);
#30398=LINE('',#436505,#34200);
#30399=LINE('',#436830,#34201);
#30400=LINE('',#436832,#34202);
#30401=LINE('',#436836,#34203);
#30402=LINE('',#436846,#34204);
#30403=LINE('',#436848,#34205);
#30404=LINE('',#436854,#34206);
#30405=LINE('',#437179,#34207);
#30406=LINE('',#437181,#34208);
#30407=LINE('',#437185,#34209);
#30408=LINE('',#437195,#34210);
#30409=LINE('',#437197,#34211);
#30410=LINE('',#437203,#34212);
#30411=LINE('',#437528,#34213);
#30412=LINE('',#437530,#34214);
#30413=LINE('',#437534,#34215);
#30414=LINE('',#437544,#34216);
#30415=LINE('',#437546,#34217);
#30416=LINE('',#437552,#34218);
#30417=LINE('',#437877,#34219);
#30418=LINE('',#437879,#34220);
#30419=LINE('',#437883,#34221);
#30420=LINE('',#437893,#34222);
#30421=LINE('',#437895,#34223);
#30422=LINE('',#437901,#34224);
#30423=LINE('',#438226,#34225);
#30424=LINE('',#438228,#34226);
#30425=LINE('',#438232,#34227);
#30426=LINE('',#438242,#34228);
#30427=LINE('',#438244,#34229);
#30428=LINE('',#438250,#34230);
#30429=LINE('',#438575,#34231);
#30430=LINE('',#438577,#34232);
#30431=LINE('',#438581,#34233);
#30432=LINE('',#438591,#34234);
#30433=LINE('',#438593,#34235);
#30434=LINE('',#438599,#34236);
#30435=LINE('',#438924,#34237);
#30436=LINE('',#438926,#34238);
#30437=LINE('',#438930,#34239);
#30438=LINE('',#438940,#34240);
#30439=LINE('',#438942,#34241);
#30440=LINE('',#438948,#34242);
#30441=LINE('',#439273,#34243);
#30442=LINE('',#439275,#34244);
#30443=LINE('',#439279,#34245);
#30444=LINE('',#439289,#34246);
#30445=LINE('',#439291,#34247);
#30446=LINE('',#439297,#34248);
#30447=LINE('',#439622,#34249);
#30448=LINE('',#439624,#34250);
#30449=LINE('',#439628,#34251);
#30450=LINE('',#439638,#34252);
#30451=LINE('',#439640,#34253);
#30452=LINE('',#439646,#34254);
#30453=LINE('',#439971,#34255);
#30454=LINE('',#439973,#34256);
#30455=LINE('',#439977,#34257);
#30456=LINE('',#439987,#34258);
#30457=LINE('',#439989,#34259);
#30458=LINE('',#439995,#34260);
#30459=LINE('',#440320,#34261);
#30460=LINE('',#440322,#34262);
#30461=LINE('',#440326,#34263);
#30462=LINE('',#440336,#34264);
#30463=LINE('',#440338,#34265);
#30464=LINE('',#440344,#34266);
#30465=LINE('',#440669,#34267);
#30466=LINE('',#440671,#34268);
#30467=LINE('',#440675,#34269);
#30468=LINE('',#440685,#34270);
#30469=LINE('',#440687,#34271);
#30470=LINE('',#440693,#34272);
#30471=LINE('',#441018,#34273);
#30472=LINE('',#441020,#34274);
#30473=LINE('',#441024,#34275);
#30474=LINE('',#441034,#34276);
#30475=LINE('',#441036,#34277);
#30476=LINE('',#441042,#34278);
#30477=LINE('',#441367,#34279);
#30478=LINE('',#441369,#34280);
#30479=LINE('',#441373,#34281);
#30480=LINE('',#441383,#34282);
#30481=LINE('',#441385,#34283);
#30482=LINE('',#441391,#34284);
#30483=LINE('',#441716,#34285);
#30484=LINE('',#441718,#34286);
#30485=LINE('',#441722,#34287);
#30486=LINE('',#441732,#34288);
#30487=LINE('',#441734,#34289);
#30488=LINE('',#441740,#34290);
#30489=LINE('',#442065,#34291);
#30490=LINE('',#442067,#34292);
#30491=LINE('',#442071,#34293);
#30492=LINE('',#442081,#34294);
#30493=LINE('',#442083,#34295);
#30494=LINE('',#442089,#34296);
#30495=LINE('',#442414,#34297);
#30496=LINE('',#442416,#34298);
#30497=LINE('',#442420,#34299);
#30498=LINE('',#442430,#34300);
#30499=LINE('',#442432,#34301);
#30500=LINE('',#442438,#34302);
#30501=LINE('',#442763,#34303);
#30502=LINE('',#442765,#34304);
#30503=LINE('',#442769,#34305);
#30504=LINE('',#442779,#34306);
#30505=LINE('',#442781,#34307);
#30506=LINE('',#442787,#34308);
#30507=LINE('',#443112,#34309);
#30508=LINE('',#443114,#34310);
#30509=LINE('',#443118,#34311);
#30510=LINE('',#443128,#34312);
#30511=LINE('',#443130,#34313);
#30512=LINE('',#443136,#34314);
#30513=LINE('',#443461,#34315);
#30514=LINE('',#443463,#34316);
#30515=LINE('',#443467,#34317);
#30516=LINE('',#443477,#34318);
#30517=LINE('',#443479,#34319);
#30518=LINE('',#443485,#34320);
#30519=LINE('',#443810,#34321);
#30520=LINE('',#443812,#34322);
#30521=LINE('',#443816,#34323);
#30522=LINE('',#443826,#34324);
#30523=LINE('',#443828,#34325);
#30524=LINE('',#443834,#34326);
#30525=LINE('',#444159,#34327);
#30526=LINE('',#444161,#34328);
#30527=LINE('',#444165,#34329);
#30528=LINE('',#444175,#34330);
#30529=LINE('',#444177,#34331);
#30530=LINE('',#444183,#34332);
#30531=LINE('',#444508,#34333);
#30532=LINE('',#444510,#34334);
#30533=LINE('',#444514,#34335);
#30534=LINE('',#444524,#34336);
#30535=LINE('',#444526,#34337);
#30536=LINE('',#444532,#34338);
#30537=LINE('',#444857,#34339);
#30538=LINE('',#444859,#34340);
#30539=LINE('',#444863,#34341);
#30540=LINE('',#444873,#34342);
#30541=LINE('',#444875,#34343);
#30542=LINE('',#444881,#34344);
#30543=LINE('',#445206,#34345);
#30544=LINE('',#445208,#34346);
#30545=LINE('',#445212,#34347);
#30546=LINE('',#445222,#34348);
#30547=LINE('',#445224,#34349);
#30548=LINE('',#445230,#34350);
#30549=LINE('',#445555,#34351);
#30550=LINE('',#445557,#34352);
#30551=LINE('',#445561,#34353);
#30552=LINE('',#445571,#34354);
#30553=LINE('',#445573,#34355);
#30554=LINE('',#445579,#34356);
#30555=LINE('',#445904,#34357);
#30556=LINE('',#445906,#34358);
#30557=LINE('',#445910,#34359);
#30558=LINE('',#445920,#34360);
#30559=LINE('',#445922,#34361);
#30560=LINE('',#445928,#34362);
#30561=LINE('',#446253,#34363);
#30562=LINE('',#446255,#34364);
#30563=LINE('',#446259,#34365);
#30564=LINE('',#446269,#34366);
#30565=LINE('',#446271,#34367);
#30566=LINE('',#446277,#34368);
#30567=LINE('',#446602,#34369);
#30568=LINE('',#446604,#34370);
#30569=LINE('',#446608,#34371);
#30570=LINE('',#446618,#34372);
#30571=LINE('',#446620,#34373);
#30572=LINE('',#446626,#34374);
#30573=LINE('',#446951,#34375);
#30574=LINE('',#446953,#34376);
#30575=LINE('',#446957,#34377);
#30576=LINE('',#446967,#34378);
#30577=LINE('',#446969,#34379);
#30578=LINE('',#446975,#34380);
#30579=LINE('',#447300,#34381);
#30580=LINE('',#447302,#34382);
#30581=LINE('',#447306,#34383);
#30582=LINE('',#447316,#34384);
#30583=LINE('',#447318,#34385);
#30584=LINE('',#447324,#34386);
#30585=LINE('',#447649,#34387);
#30586=LINE('',#447651,#34388);
#30587=LINE('',#447655,#34389);
#30588=LINE('',#447665,#34390);
#30589=LINE('',#447667,#34391);
#30590=LINE('',#447673,#34392);
#30591=LINE('',#447998,#34393);
#30592=LINE('',#448000,#34394);
#30593=LINE('',#448004,#34395);
#30594=LINE('',#448014,#34396);
#30595=LINE('',#448016,#34397);
#30596=LINE('',#448022,#34398);
#30597=LINE('',#448347,#34399);
#30598=LINE('',#448349,#34400);
#30599=LINE('',#448353,#34401);
#30600=LINE('',#448363,#34402);
#30601=LINE('',#448365,#34403);
#30602=LINE('',#448371,#34404);
#30603=LINE('',#448696,#34405);
#30604=LINE('',#448698,#34406);
#30605=LINE('',#448702,#34407);
#30606=LINE('',#448712,#34408);
#30607=LINE('',#448714,#34409);
#30608=LINE('',#448720,#34410);
#30609=LINE('',#449045,#34411);
#30610=LINE('',#449047,#34412);
#30611=LINE('',#449051,#34413);
#30612=LINE('',#449061,#34414);
#30613=LINE('',#449063,#34415);
#30614=LINE('',#449069,#34416);
#30615=LINE('',#449396,#34417);
#30616=LINE('',#449409,#34418);
#30617=LINE('',#449456,#34419);
#30618=LINE('',#449504,#34420);
#30619=LINE('',#449555,#34421);
#30620=LINE('',#449606,#34422);
#30621=LINE('',#449654,#34423);
#30622=LINE('',#449705,#34424);
#30623=LINE('',#449744,#34425);
#30624=LINE('',#449765,#34426);
#30625=LINE('',#449789,#34427);
#30626=LINE('',#449814,#34428);
#30627=LINE('',#449838,#34429);
#30628=LINE('',#449863,#34430);
#30629=LINE('',#449888,#34431);
#30630=LINE('',#449912,#34432);
#30631=LINE('',#449929,#34433);
#30632=LINE('',#449942,#34434);
#30633=LINE('',#449989,#34435);
#30634=LINE('',#450037,#34436);
#30635=LINE('',#450088,#34437);
#30636=LINE('',#450139,#34438);
#30637=LINE('',#450187,#34439);
#30638=LINE('',#450238,#34440);
#30639=LINE('',#450277,#34441);
#30640=LINE('',#450298,#34442);
#30641=LINE('',#450322,#34443);
#30642=LINE('',#450347,#34444);
#30643=LINE('',#450371,#34445);
#30644=LINE('',#450396,#34446);
#30645=LINE('',#450421,#34447);
#30646=LINE('',#450445,#34448);
#30647=LINE('',#450462,#34449);
#30648=LINE('',#450475,#34450);
#30649=LINE('',#450522,#34451);
#30650=LINE('',#450570,#34452);
#30651=LINE('',#450621,#34453);
#30652=LINE('',#450672,#34454);
#30653=LINE('',#450720,#34455);
#30654=LINE('',#450771,#34456);
#30655=LINE('',#450810,#34457);
#30656=LINE('',#450831,#34458);
#30657=LINE('',#450855,#34459);
#30658=LINE('',#450880,#34460);
#30659=LINE('',#450904,#34461);
#30660=LINE('',#450929,#34462);
#30661=LINE('',#450954,#34463);
#30662=LINE('',#450978,#34464);
#30663=LINE('',#450995,#34465);
#30664=LINE('',#451008,#34466);
#30665=LINE('',#451055,#34467);
#30666=LINE('',#451103,#34468);
#30667=LINE('',#451154,#34469);
#30668=LINE('',#451205,#34470);
#30669=LINE('',#451253,#34471);
#30670=LINE('',#451304,#34472);
#30671=LINE('',#451343,#34473);
#30672=LINE('',#451364,#34474);
#30673=LINE('',#451388,#34475);
#30674=LINE('',#451413,#34476);
#30675=LINE('',#451437,#34477);
#30676=LINE('',#451462,#34478);
#30677=LINE('',#451487,#34479);
#30678=LINE('',#451511,#34480);
#30679=LINE('',#451529,#34481);
#30680=LINE('',#451536,#34482);
#30681=LINE('',#453315,#34483);
#30682=LINE('',#453319,#34484);
#30683=LINE('',#453323,#34485);
#30684=LINE('',#453328,#34486);
#30685=LINE('',#453331,#34487);
#30686=LINE('',#453336,#34488);
#30687=LINE('',#453341,#34489);
#30688=LINE('',#453347,#34490);
#30689=LINE('',#453353,#34491);
#30690=LINE('',#453359,#34492);
#30691=LINE('',#453365,#34493);
#30692=LINE('',#453371,#34494);
#30693=LINE('',#453377,#34495);
#30694=LINE('',#453383,#34496);
#30695=LINE('',#453389,#34497);
#30696=LINE('',#453395,#34498);
#30697=LINE('',#453401,#34499);
#30698=LINE('',#453407,#34500);
#30699=LINE('',#453413,#34501);
#30700=LINE('',#453419,#34502);
#30701=LINE('',#453425,#34503);
#30702=LINE('',#453431,#34504);
#30703=LINE('',#453437,#34505);
#30704=LINE('',#454969,#34506);
#30705=LINE('',#454993,#34507);
#30706=LINE('',#455041,#34508);
#30707=LINE('',#455089,#34509);
#30708=LINE('',#455143,#34510);
#30709=LINE('',#455191,#34511);
#30710=LINE('',#455239,#34512);
#30711=LINE('',#455293,#34513);
#30712=LINE('',#455341,#34514);
#30713=LINE('',#455389,#34515);
#30714=LINE('',#455437,#34516);
#30715=LINE('',#455448,#34517);
#30716=LINE('',#455474,#34518);
#30717=LINE('',#455498,#34519);
#30718=LINE('',#455522,#34520);
#30719=LINE('',#455547,#34521);
#30720=LINE('',#455572,#34522);
#30721=LINE('',#455596,#34523);
#30722=LINE('',#455621,#34524);
#30723=LINE('',#455646,#34525);
#30724=LINE('',#455670,#34526);
#30725=LINE('',#455694,#34527);
#30726=LINE('',#455742,#34528);
#30727=LINE('',#455790,#34529);
#30728=LINE('',#455844,#34530);
#30729=LINE('',#455892,#34531);
#30730=LINE('',#455909,#34532);
#30731=LINE('',#455934,#34533);
#30732=LINE('',#455959,#34534);
#30733=LINE('',#455984,#34535);
#30734=LINE('',#457688,#34536);
#30735=LINE('',#457693,#34537);
#30736=LINE('',#457697,#34538);
#30737=LINE('',#457703,#34539);
#30738=LINE('',#457708,#34540);
#30739=LINE('',#457712,#34541);
#30740=LINE('',#457726,#34542);
#30741=LINE('',#457730,#34543);
#30742=LINE('',#457736,#34544);
#30743=LINE('',#457760,#34545);
#30744=LINE('',#457808,#34546);
#30745=LINE('',#457856,#34547);
#30746=LINE('',#457910,#34548);
#30747=LINE('',#457958,#34549);
#30748=LINE('',#458006,#34550);
#30749=LINE('',#458023,#34551);
#30750=LINE('',#458048,#34552);
#30751=LINE('',#458072,#34553);
#30752=LINE('',#458097,#34554);
#30753=LINE('',#458122,#34555);
#30754=LINE('',#458922,#34556);
#30755=LINE('',#458929,#34557);
#30756=LINE('',#458933,#34558);
#30757=LINE('',#458938,#34559);
#30758=LINE('',#458942,#34560);
#30759=LINE('',#458949,#34561);
#30760=LINE('',#458951,#34562);
#30761=LINE('',#458955,#34563);
#30762=LINE('',#458959,#34564);
#30763=LINE('',#458961,#34565);
#30764=LINE('',#458963,#34566);
#30765=LINE('',#458965,#34567);
#30766=LINE('',#458967,#34568);
#30767=LINE('',#458968,#34569);
#30768=LINE('',#458972,#34570);
#30769=LINE('',#458974,#34571);
#30770=LINE('',#458976,#34572);
#30771=LINE('',#458978,#34573);
#30772=LINE('',#458980,#34574);
#30773=LINE('',#458981,#34575);
#30774=LINE('',#458983,#34576);
#30775=LINE('',#458984,#34577);
#30776=LINE('',#458986,#34578);
#30777=LINE('',#458988,#34579);
#30778=LINE('',#458990,#34580);
#30779=LINE('',#458992,#34581);
#30780=LINE('',#459000,#34582);
#30781=LINE('',#459006,#34583);
#30782=LINE('',#459012,#34584);
#30783=LINE('',#459018,#34585);
#30784=LINE('',#459024,#34586);
#30785=LINE('',#459031,#34587);
#30786=LINE('',#459034,#34588);
#30787=LINE('',#459038,#34589);
#30788=LINE('',#459040,#34590);
#30789=LINE('',#459042,#34591);
#30790=LINE('',#459043,#34592);
#30791=LINE('',#459047,#34593);
#30792=LINE('',#459049,#34594);
#30793=LINE('',#459051,#34595);
#30794=LINE('',#459052,#34596);
#30795=LINE('',#459055,#34597);
#30796=LINE('',#459057,#34598);
#30797=LINE('',#459059,#34599);
#30798=LINE('',#459061,#34600);
#30799=LINE('',#459063,#34601);
#30800=LINE('',#459065,#34602);
#30801=LINE('',#459066,#34603);
#30802=LINE('',#459070,#34604);
#30803=LINE('',#459072,#34605);
#30804=LINE('',#459074,#34606);
#30805=LINE('',#459075,#34607);
#30806=LINE('',#459079,#34608);
#30807=LINE('',#459081,#34609);
#30808=LINE('',#459082,#34610);
#30809=LINE('',#459084,#34611);
#30810=LINE('',#459086,#34612);
#30811=LINE('',#459088,#34613);
#30812=LINE('',#459089,#34614);
#30813=LINE('',#459093,#34615);
#30814=LINE('',#459095,#34616);
#30815=LINE('',#459097,#34617);
#30816=LINE('',#459098,#34618);
#30817=LINE('',#459102,#34619);
#30818=LINE('',#459104,#34620);
#30819=LINE('',#459106,#34621);
#30820=LINE('',#459107,#34622);
#30821=LINE('',#459109,#34623);
#30822=LINE('',#459110,#34624);
#30823=LINE('',#459112,#34625);
#30824=LINE('',#459113,#34626);
#30825=LINE('',#459117,#34627);
#30826=LINE('',#459119,#34628);
#30827=LINE('',#459121,#34629);
#30828=LINE('',#459122,#34630);
#30829=LINE('',#459124,#34631);
#30830=LINE('',#459125,#34632);
#30831=LINE('',#459127,#34633);
#30832=LINE('',#459129,#34634);
#30833=LINE('',#459131,#34635);
#30834=LINE('',#459133,#34636);
#30835=LINE('',#459134,#34637);
#30836=LINE('',#459136,#34638);
#30837=LINE('',#459138,#34639);
#30838=LINE('',#459140,#34640);
#30839=LINE('',#459142,#34641);
#30840=LINE('',#459144,#34642);
#30841=LINE('',#459146,#34643);
#30842=LINE('',#459148,#34644);
#30843=LINE('',#459150,#34645);
#30844=LINE('',#459152,#34646);
#30845=LINE('',#459154,#34647);
#30846=LINE('',#459156,#34648);
#30847=LINE('',#459158,#34649);
#30848=LINE('',#459160,#34650);
#30849=VECTOR('',#105583,1.2645);
#30850=VECTOR('',#105588,1.2645);
#30851=VECTOR('',#105591,1.2645);
#30852=VECTOR('',#105594,1.2645);
#30853=VECTOR('',#105599,1.2645);
#30854=VECTOR('',#105604,1.2645);
#30855=VECTOR('',#105607,1.2645);
#30856=VECTOR('',#105610,1.2645);
#30857=VECTOR('',#105615,1.543);
#30858=VECTOR('',#105620,1.543);
#30859=VECTOR('',#105623,1.543);
#30860=VECTOR('',#105626,1.543);
#30861=VECTOR('',#105631,1.543);
#30862=VECTOR('',#105636,1.543);
#30863=VECTOR('',#105639,1.543);
#30864=VECTOR('',#105642,1.543);
#30865=VECTOR('',#105657,10.);
#30866=VECTOR('',#105660,10.);
#30867=VECTOR('',#105669,10.);
#30868=VECTOR('',#105672,10.);
#30869=VECTOR('',#105683,7.95);
#30870=VECTOR('',#105688,8.);
#30871=VECTOR('',#105699,18.2);
#30872=VECTOR('',#105706,18.25);
#30873=VECTOR('',#105707,10.);
#30874=VECTOR('',#105710,10.);
#30875=VECTOR('',#105711,10.);
#30876=VECTOR('',#105714,10.);
#30877=VECTOR('',#105723,18.2);
#30878=VECTOR('',#105732,18.25);
#30879=VECTOR('',#105741,2.55);
#30880=VECTOR('',#105750,2.5);
#30881=VECTOR('',#105755,18.2);
#30882=VECTOR('',#105758,10.);
#30883=VECTOR('',#105763,10.);
#30884=VECTOR('',#105764,10.);
#30885=VECTOR('',#105767,10.);
#30886=VECTOR('',#105772,10.);
#30887=VECTOR('',#105773,10.);
#30888=VECTOR('',#105780,10.);
#30889=VECTOR('',#105785,10.);
#30890=VECTOR('',#105786,10.);
#30891=VECTOR('',#105789,10.);
#30892=VECTOR('',#105794,10.);
#30893=VECTOR('',#105795,10.);
#30894=VECTOR('',#105802,10.);
#30895=VECTOR('',#105803,10.);
#30896=VECTOR('',#105804,10.);
#30897=VECTOR('',#105805,10.);
#30898=VECTOR('',#105808,10.);
#30899=VECTOR('',#105815,10.);
#30900=VECTOR('',#105816,10.);
#30901=VECTOR('',#105817,10.);
#30902=VECTOR('',#105820,10.);
#30903=VECTOR('',#105827,10.);
#30904=VECTOR('',#105832,10.);
#30905=VECTOR('',#105839,10.);
#30906=VECTOR('',#105840,10.);
#30907=VECTOR('',#105841,10.);
#30908=VECTOR('',#105844,10.);
#30909=VECTOR('',#105851,10.);
#30910=VECTOR('',#105852,10.);
#30911=VECTOR('',#105853,10.);
#30912=VECTOR('',#105856,10.);
#30913=VECTOR('',#105863,10.);
#30914=VECTOR('',#105874,10.);
#30915=VECTOR('',#105875,10.);
#30916=VECTOR('',#105878,10.);
#30917=VECTOR('',#105883,10.);
#30918=VECTOR('',#105886,10.);
#30919=VECTOR('',#105891,10.);
#30920=VECTOR('',#105894,10.);
#30921=VECTOR('',#105897,10.);
#30922=VECTOR('',#105902,1.15);
#30923=VECTOR('',#105907,1.);
#30924=VECTOR('',#105914,10.);
#30925=VECTOR('',#105917,10.);
#30926=VECTOR('',#105920,10.);
#30927=VECTOR('',#105923,10.);
#30928=VECTOR('',#105926,10.);
#30929=VECTOR('',#105929,10.);
#30930=VECTOR('',#105932,10.);
#30931=VECTOR('',#105935,10.);
#30932=VECTOR('',#105938,10.);
#30933=VECTOR('',#105941,10.);
#30934=VECTOR('',#105944,10.);
#30935=VECTOR('',#105947,10.);
#30936=VECTOR('',#105950,10.);
#30937=VECTOR('',#105953,10.);
#30938=VECTOR('',#105956,10.);
#30939=VECTOR('',#105959,10.);
#30940=VECTOR('',#105962,10.);
#30941=VECTOR('',#105965,10.);
#30942=VECTOR('',#105968,10.);
#30943=VECTOR('',#105971,10.);
#30944=VECTOR('',#105978,10.);
#30945=VECTOR('',#105981,10.);
#30946=VECTOR('',#105984,10.);
#30947=VECTOR('',#105987,10.);
#30948=VECTOR('',#105990,10.);
#30949=VECTOR('',#105993,10.);
#30950=VECTOR('',#105996,10.);
#30951=VECTOR('',#105999,10.);
#30952=VECTOR('',#106002,10.);
#30953=VECTOR('',#106005,10.);
#30954=VECTOR('',#106008,10.);
#30955=VECTOR('',#106011,10.);
#30956=VECTOR('',#106014,10.);
#30957=VECTOR('',#106017,10.);
#30958=VECTOR('',#106020,10.);
#30959=VECTOR('',#106023,10.);
#30960=VECTOR('',#106026,10.);
#30961=VECTOR('',#106029,10.);
#30962=VECTOR('',#106032,10.);
#30963=VECTOR('',#106035,10.);
#30964=VECTOR('',#106040,10.);
#30965=VECTOR('',#106041,10.);
#30966=VECTOR('',#106042,10.);
#30967=VECTOR('',#106045,10.);
#30968=VECTOR('',#106046,10.);
#30969=VECTOR('',#106049,10.);
#30970=VECTOR('',#106052,10.);
#30971=VECTOR('',#106055,10.);
#30972=VECTOR('',#106058,10.);
#30973=VECTOR('',#106059,10.);
#30974=VECTOR('',#106060,10.);
#30975=VECTOR('',#106063,10.);
#30976=VECTOR('',#106064,10.);
#30977=VECTOR('',#106069,10.);
#30978=VECTOR('',#106072,10.);
#30979=VECTOR('',#106073,10.);
#30980=VECTOR('',#106074,10.);
#30981=VECTOR('',#106077,10.);
#30982=VECTOR('',#106078,10.);
#30983=VECTOR('',#106083,10.);
#30984=VECTOR('',#106086,10.);
#30985=VECTOR('',#106087,10.);
#30986=VECTOR('',#106088,10.);
#30987=VECTOR('',#106091,10.);
#30988=VECTOR('',#106092,10.);
#30989=VECTOR('',#106097,10.);
#30990=VECTOR('',#106100,10.);
#30991=VECTOR('',#106101,10.);
#30992=VECTOR('',#106102,10.);
#30993=VECTOR('',#106105,10.);
#30994=VECTOR('',#106106,10.);
#30995=VECTOR('',#106111,10.);
#30996=VECTOR('',#106114,10.);
#30997=VECTOR('',#106115,10.);
#30998=VECTOR('',#106116,10.);
#30999=VECTOR('',#106119,10.);
#31000=VECTOR('',#106120,10.);
#31001=VECTOR('',#106125,10.);
#31002=VECTOR('',#106128,10.);
#31003=VECTOR('',#106129,10.);
#31004=VECTOR('',#106130,10.);
#31005=VECTOR('',#106133,10.);
#31006=VECTOR('',#106134,10.);
#31007=VECTOR('',#106139,10.);
#31008=VECTOR('',#106142,10.);
#31009=VECTOR('',#106143,10.);
#31010=VECTOR('',#106144,10.);
#31011=VECTOR('',#106147,10.);
#31012=VECTOR('',#106148,10.);
#31013=VECTOR('',#106153,10.);
#31014=VECTOR('',#106156,10.);
#31015=VECTOR('',#106157,10.);
#31016=VECTOR('',#106158,10.);
#31017=VECTOR('',#106161,10.);
#31018=VECTOR('',#106162,10.);
#31019=VECTOR('',#106167,10.);
#31020=VECTOR('',#106170,10.);
#31021=VECTOR('',#106171,10.);
#31022=VECTOR('',#106174,10.);
#31023=VECTOR('',#106175,10.);
#31024=VECTOR('',#106182,17.45);
#31025=VECTOR('',#106191,17.45);
#31026=VECTOR('',#106196,17.5);
#31027=VECTOR('',#106203,17.5);
#31028=VECTOR('',#106208,17.45);
#31029=VECTOR('',#106215,17.45);
#31030=VECTOR('',#106218,17.5);
#31031=VECTOR('',#106227,17.45);
#31032=VECTOR('',#106234,17.45);
#31033=VECTOR('',#106237,17.5);
#31034=VECTOR('',#106246,17.45);
#31035=VECTOR('',#106253,17.45);
#31036=VECTOR('',#106256,17.5);
#31037=VECTOR('',#106265,17.45);
#31038=VECTOR('',#106272,17.45);
#31039=VECTOR('',#106275,17.5);
#31040=VECTOR('',#106284,17.45);
#31041=VECTOR('',#106291,17.45);
#31042=VECTOR('',#106294,17.5);
#31043=VECTOR('',#106303,17.45);
#31044=VECTOR('',#106310,17.45);
#31045=VECTOR('',#106313,17.5);
#31046=VECTOR('',#106322,17.45);
#31047=VECTOR('',#106329,17.45);
#31048=VECTOR('',#106332,17.5);
#31049=VECTOR('',#106341,17.45);
#31050=VECTOR('',#106348,17.45);
#31051=VECTOR('',#106351,17.5);
#31052=VECTOR('',#106360,17.45);
#31053=VECTOR('',#106367,17.45);
#31054=VECTOR('',#106370,17.5);
#31055=VECTOR('',#106379,17.45);
#31056=VECTOR('',#106386,17.45);
#31057=VECTOR('',#106389,17.5);
#31058=VECTOR('',#106398,17.45);
#31059=VECTOR('',#106405,17.45);
#31060=VECTOR('',#106408,17.5);
#31061=VECTOR('',#106417,17.45);
#31062=VECTOR('',#106424,17.45);
#31063=VECTOR('',#106427,17.5);
#31064=VECTOR('',#106436,17.45);
#31065=VECTOR('',#106443,17.45);
#31066=VECTOR('',#106448,17.5);
#31067=VECTOR('',#106459,17.45);
#31068=VECTOR('',#106464,17.45);
#31069=VECTOR('',#106467,17.5);
#31070=VECTOR('',#106470,1.5);
#31071=VECTOR('',#106479,1000.);
#31072=VECTOR('',#106482,1000.);
#31073=VECTOR('',#106487,1000.);
#31074=VECTOR('',#106490,1000.);
#31075=VECTOR('',#106495,1000.);
#31076=VECTOR('',#106498,1000.);
#31077=VECTOR('',#106527,1000.);
#31078=VECTOR('',#106530,1000.);
#31079=VECTOR('',#106533,1000.);
#31080=VECTOR('',#106534,1000.);
#31081=VECTOR('',#106539,1000.);
#31082=VECTOR('',#106540,1000.);
#31083=VECTOR('',#106547,2.);
#31084=VECTOR('',#106550,1000.);
#31085=VECTOR('',#106551,1000.);
#31086=VECTOR('',#106554,1000.);
#31087=VECTOR('',#106555,1000.);
#31088=VECTOR('',#106558,1000.);
#31089=VECTOR('',#106559,1000.);
#31090=VECTOR('',#106562,1000.);
#31091=VECTOR('',#106565,1000.);
#31092=VECTOR('',#106570,1000.);
#31093=VECTOR('',#106573,1000.);
#31094=VECTOR('',#106584,1000.);
#31095=VECTOR('',#106587,1000.);
#31096=VECTOR('',#106592,3.);
#31097=VECTOR('',#106597,1000.);
#31098=VECTOR('',#106598,1000.);
#31099=VECTOR('',#106601,1000.);
#31100=VECTOR('',#106602,1000.);
#31101=VECTOR('',#106605,1000.);
#31102=VECTOR('',#106606,1000.);
#31103=VECTOR('',#106609,1000.);
#31104=VECTOR('',#106610,1000.);
#31105=VECTOR('',#106617,5.);
#31106=VECTOR('',#106624,1000.);
#31107=VECTOR('',#106627,1000.);
#31108=VECTOR('',#106632,1000.);
#31109=VECTOR('',#106635,1000.);
#31110=VECTOR('',#106640,1000.);
#31111=VECTOR('',#106643,1000.);
#31112=VECTOR('',#106648,1000.);
#31113=VECTOR('',#106651,1000.);
#31114=VECTOR('',#106658,10.);
#31115=VECTOR('',#106661,10.);
#31116=VECTOR('',#106664,10.);
#31117=VECTOR('',#106665,10.);
#31118=VECTOR('',#106666,10.);
#31119=VECTOR('',#106673,10.);
#31120=VECTOR('',#106678,10.);
#31121=VECTOR('',#106679,10.);
#31122=VECTOR('',#106680,10.);
#31123=VECTOR('',#106689,10.);
#31124=VECTOR('',#106692,10.);
#31125=VECTOR('',#106699,10.);
#31126=VECTOR('',#106700,10.);
#31127=VECTOR('',#106709,10.);
#31128=VECTOR('',#106710,10.);
#31129=VECTOR('',#106715,10.);
#31130=VECTOR('',#106718,10.);
#31131=VECTOR('',#106719,10.);
#31132=VECTOR('',#106720,10.);
#31133=VECTOR('',#106723,10.);
#31134=VECTOR('',#106724,10.);
#31135=VECTOR('',#106725,10.);
#31136=VECTOR('',#106728,10.);
#31137=VECTOR('',#106729,10.);
#31138=VECTOR('',#106730,10.);
#31139=VECTOR('',#106733,10.);
#31140=VECTOR('',#106736,10.);
#31141=VECTOR('',#106739,10.);
#31142=VECTOR('',#106748,10.);
#31143=VECTOR('',#106751,10.);
#31144=VECTOR('',#106804,10.);
#31145=VECTOR('',#106805,10.);
#31146=VECTOR('',#106812,10.);
#31147=VECTOR('',#106815,10.);
#31148=VECTOR('',#106818,10.);
#31149=VECTOR('',#106819,12.);
#31150=VECTOR('',#106822,10.);
#31151=VECTOR('',#106825,10.);
#31152=VECTOR('',#106830,10.);
#31153=VECTOR('',#106831,10.);
#31154=VECTOR('',#106834,10.);
#31155=VECTOR('',#106839,10.);
#31156=VECTOR('',#106840,10.);
#31157=VECTOR('',#106847,10.);
#31158=VECTOR('',#106850,10.);
#31159=VECTOR('',#106875,10.);
#31160=VECTOR('',#106876,10.);
#31161=VECTOR('',#106887,10.);
#31162=VECTOR('',#106888,10.);
#31163=VECTOR('',#106901,10.);
#31164=VECTOR('',#106902,10.);
#31165=VECTOR('',#106939,10.);
#31166=VECTOR('',#106940,10.);
#31167=VECTOR('',#106941,10.);
#31168=VECTOR('',#106944,10.);
#31169=VECTOR('',#106949,10.);
#31170=VECTOR('',#106954,10.);
#31171=VECTOR('',#106961,3.15);
#31172=VECTOR('',#106962,10.);
#31173=VECTOR('',#106965,10.);
#31174=VECTOR('',#106968,10.);
#31175=VECTOR('',#106971,10.);
#31176=VECTOR('',#106974,10.);
#31177=VECTOR('',#106979,10.);
#31178=VECTOR('',#106984,10.);
#31179=VECTOR('',#106985,10.);
#31180=VECTOR('',#107008,10.);
#31181=VECTOR('',#107009,10.);
#31182=VECTOR('',#107020,10.);
#31183=VECTOR('',#107021,10.);
#31184=VECTOR('',#107046,10.);
#31185=VECTOR('',#107047,10.);
#31186=VECTOR('',#107066,10.);
#31187=VECTOR('',#107069,10.);
#31188=VECTOR('',#107072,3.2);
#31189=VECTOR('',#107075,10.);
#31190=VECTOR('',#107076,10.);
#31191=VECTOR('',#107083,10.);
#31192=VECTOR('',#107088,10.);
#31193=VECTOR('',#107097,10.);
#31194=VECTOR('',#107100,10.);
#31195=VECTOR('',#107141,10.);
#31196=VECTOR('',#107142,10.);
#31197=VECTOR('',#107161,10.);
#31198=VECTOR('',#107162,10.);
#31199=VECTOR('',#107169,5.80000000000001);
#31200=VECTOR('',#107170,10.);
#31201=VECTOR('',#107171,10.);
#31202=VECTOR('',#107172,10.);
#31203=VECTOR('',#107173,3.2);
#31204=VECTOR('',#107176,5.80000000000001);
#31205=VECTOR('',#107181,10.);
#31206=VECTOR('',#107186,10.);
#31207=VECTOR('',#107187,10.);
#31208=VECTOR('',#107190,10.);
#31209=VECTOR('',#107195,10.);
#31210=VECTOR('',#107196,10.);
#31211=VECTOR('',#107197,10.);
#31212=VECTOR('',#107198,10.);
#31213=VECTOR('',#107243,10.);
#31214=VECTOR('',#107244,10.);
#31215=VECTOR('',#107257,10.);
#31216=VECTOR('',#107258,10.);
#31217=VECTOR('',#107269,10.);
#31218=VECTOR('',#107270,10.);
#31219=VECTOR('',#107293,10.);
#31220=VECTOR('',#107294,10.);
#31221=VECTOR('',#107297,10.);
#31222=VECTOR('',#107300,10.);
#31223=VECTOR('',#107303,10.);
#31224=VECTOR('',#107304,10.);
#31225=VECTOR('',#107307,10.);
#31226=VECTOR('',#107312,0.800000000000001);
#31227=VECTOR('',#107317,0.800000000000001);
#31228=VECTOR('',#107322,10.);
#31229=VECTOR('',#107323,10.);
#31230=VECTOR('',#107326,10.);
#31231=VECTOR('',#107387,10.);
#31232=VECTOR('',#107388,10.);
#31233=VECTOR('',#107395,17.3949617393671);
#31234=VECTOR('',#107398,10.);
#31235=VECTOR('',#107401,10.);
#31236=VECTOR('',#107406,10.);
#31237=VECTOR('',#107407,10.);
#31238=VECTOR('',#107410,10.);
#31239=VECTOR('',#107415,9.3949617393671);
#31240=VECTOR('',#107470,10.);
#31241=VECTOR('',#107471,10.);
#31242=VECTOR('',#107482,10.);
#31243=VECTOR('',#107483,10.);
#31244=VECTOR('',#107494,10.);
#31245=VECTOR('',#107495,10.);
#31246=VECTOR('',#107530,10.);
#31247=VECTOR('',#107533,10.);
#31248=VECTOR('',#107536,10.);
#31249=VECTOR('',#107537,10.);
#31250=VECTOR('',#107540,10.);
#31251=VECTOR('',#107545,10.);
#31252=VECTOR('',#107550,10.);
#31253=VECTOR('',#107555,9.45);
#31254=VECTOR('',#107560,10.);
#31255=VECTOR('',#107565,10.);
#31256=VECTOR('',#107568,10.);
#31257=VECTOR('',#107601,10.);
#31258=VECTOR('',#107602,10.);
#31259=VECTOR('',#107637,10.);
#31260=VECTOR('',#107640,10.);
#31261=VECTOR('',#107643,10.);
#31262=VECTOR('',#107646,10.);
#31263=VECTOR('',#107649,10.);
#31264=VECTOR('',#107654,10.);
#31265=VECTOR('',#107659,10.);
#31266=VECTOR('',#107664,0.8);
#31267=VECTOR('',#107673,10.);
#31268=VECTOR('',#107676,10.);
#31269=VECTOR('',#107687,10.);
#31270=VECTOR('',#107688,10.);
#31271=VECTOR('',#107723,10.);
#31272=VECTOR('',#107726,3.6);
#31273=VECTOR('',#107729,10.);
#31274=VECTOR('',#107734,10.);
#31275=VECTOR('',#107739,10.);
#31276=VECTOR('',#107740,10.);
#31277=VECTOR('',#107749,10.);
#31278=VECTOR('',#107754,10.);
#31279=VECTOR('',#107757,10.);
#31280=VECTOR('',#107764,10.);
#31281=VECTOR('',#107767,10.);
#31282=VECTOR('',#107770,8.45);
#31283=VECTOR('',#107783,10.);
#31284=VECTOR('',#107786,10.);
#31285=VECTOR('',#107789,10.);
#31286=VECTOR('',#107790,10.);
#31287=VECTOR('',#107791,10.);
#31288=VECTOR('',#107798,10.);
#31289=VECTOR('',#107799,10.);
#31290=VECTOR('',#107800,10.);
#31291=VECTOR('',#107801,10.);
#31292=VECTOR('',#107806,10.);
#31293=VECTOR('',#107809,10.);
#31294=VECTOR('',#107814,10.);
#31295=VECTOR('',#107817,10.);
#31296=VECTOR('',#107820,10.);
#31297=VECTOR('',#107823,10.);
#31298=VECTOR('',#107838,10.);
#31299=VECTOR('',#107841,10.);
#31300=VECTOR('',#107842,10.);
#31301=VECTOR('',#107843,10.);
#31302=VECTOR('',#107846,10.);
#31303=VECTOR('',#107849,10.);
#31304=VECTOR('',#107856,10.);
#31305=VECTOR('',#107859,10.);
#31306=VECTOR('',#107862,10.);
#31307=VECTOR('',#107865,10.);
#31308=VECTOR('',#107868,10.);
#31309=VECTOR('',#107885,10.);
#31310=VECTOR('',#107888,10.);
#31311=VECTOR('',#107891,10.);
#31312=VECTOR('',#107900,10.);
#31313=VECTOR('',#107905,10.);
#31314=VECTOR('',#107906,10.);
#31315=VECTOR('',#107907,10.);
#31316=VECTOR('',#107910,10.);
#31317=VECTOR('',#107913,10.);
#31318=VECTOR('',#107916,10.);
#31319=VECTOR('',#107917,10.);
#31320=VECTOR('',#107920,10.);
#31321=VECTOR('',#107925,10.);
#31322=VECTOR('',#107928,10.);
#31323=VECTOR('',#107933,10.);
#31324=VECTOR('',#107936,10.);
#31325=VECTOR('',#107941,10.);
#31326=VECTOR('',#107946,10.);
#31327=VECTOR('',#107949,10.);
#31328=VECTOR('',#107952,10.);
#31329=VECTOR('',#107955,10.);
#31330=VECTOR('',#107958,10.);
#31331=VECTOR('',#107969,10.);
#31332=VECTOR('',#107972,10.);
#31333=VECTOR('',#107973,10.);
#31334=VECTOR('',#107978,10.);
#31335=VECTOR('',#107981,10.);
#31336=VECTOR('',#107984,10.);
#31337=VECTOR('',#107987,10.);
#31338=VECTOR('',#107988,10.);
#31339=VECTOR('',#107991,10.);
#31340=VECTOR('',#107994,10.);
#31341=VECTOR('',#107997,10.);
#31342=VECTOR('',#107998,10.);
#31343=VECTOR('',#108003,10.);
#31344=VECTOR('',#108006,10.);
#31345=VECTOR('',#108015,10.);
#31346=VECTOR('',#108018,10.);
#31347=VECTOR('',#108021,10.);
#31348=VECTOR('',#108022,10.);
#31349=VECTOR('',#108045,10.);
#31350=VECTOR('',#108050,10.);
#31351=VECTOR('',#108055,10.);
#31352=VECTOR('',#108058,10.);
#31353=VECTOR('',#108059,10.);
#31354=VECTOR('',#108062,10.);
#31355=VECTOR('',#108065,10.);
#31356=VECTOR('',#108068,7.69496173936711);
#31357=VECTOR('',#108069,10.);
#31358=VECTOR('',#108072,7.6949617393671);
#31359=VECTOR('',#108075,10.);
#31360=VECTOR('',#108078,10.);
#31361=VECTOR('',#108081,10.);
#31362=VECTOR('',#108086,10.);
#31363=VECTOR('',#108089,10.);
#31364=VECTOR('',#108092,9.45);
#31365=VECTOR('',#108101,23.7449617393671);
#31366=VECTOR('',#108104,10.);
#31367=VECTOR('',#108107,0.4);
#31368=VECTOR('',#108112,0.8);
#31369=VECTOR('',#108113,10.);
#31370=VECTOR('',#108118,0.8);
#31371=VECTOR('',#108121,10.);
#31372=VECTOR('',#108124,10.);
#31373=VECTOR('',#108135,3.2);
#31374=VECTOR('',#108136,10.);
#31375=VECTOR('',#108139,10.);
#31376=VECTOR('',#108142,10.);
#31377=VECTOR('',#108145,10.);
#31378=VECTOR('',#108148,10.);
#31379=VECTOR('',#108153,10.);
#31380=VECTOR('',#108154,4.65);
#31381=VECTOR('',#108157,10.0999999997296);
#31382=VECTOR('',#108162,10.);
#31383=VECTOR('',#108167,10.);
#31384=VECTOR('',#108174,10.);
#31385=VECTOR('',#108177,10.);
#31386=VECTOR('',#108178,10.);
#31387=VECTOR('',#108179,10.);
#31388=VECTOR('',#108190,10.);
#31389=VECTOR('',#108193,10.);
#31390=VECTOR('',#108204,10.);
#31391=VECTOR('',#108207,10.);
#31392=VECTOR('',#108222,10.);
#31393=VECTOR('',#108229,10.);
#31394=VECTOR('',#108230,10.);
#31395=VECTOR('',#108231,10.);
#31396=VECTOR('',#108234,10.);
#31397=VECTOR('',#108243,10.);
#31398=VECTOR('',#108244,10.);
#31399=VECTOR('',#108247,4.1);
#31400=VECTOR('',#108252,10.);
#31401=VECTOR('',#108253,10.);
#31402=VECTOR('',#108256,10.);
#31403=VECTOR('',#108259,10.);
#31404=VECTOR('',#108262,10.);
#31405=VECTOR('',#108267,0.8);
#31406=VECTOR('',#108270,13.4);
#31407=VECTOR('',#108273,10.);
#31408=VECTOR('',#108284,10.);
#31409=VECTOR('',#108293,10.);
#31410=VECTOR('',#108294,10.);
#31411=VECTOR('',#108297,10.);
#31412=VECTOR('',#108300,10.);
#31413=VECTOR('',#108313,10.);
#31414=VECTOR('',#108320,10.);
#31415=VECTOR('',#108323,10.);
#31416=VECTOR('',#108338,1.6);
#31417=VECTOR('',#108345,1.6);
#31418=VECTOR('',#108348,10.);
#31419=VECTOR('',#108351,10.);
#31420=VECTOR('',#108354,10.);
#31421=VECTOR('',#108355,10.);
#31422=VECTOR('',#108358,10.);
#31423=VECTOR('',#108365,10.);
#31424=VECTOR('',#108366,10.);
#31425=VECTOR('',#108369,10.);
#31426=VECTOR('',#108370,10.);
#31427=VECTOR('',#108375,10.);
#31428=VECTOR('',#108378,10.);
#31429=VECTOR('',#108385,3.05);
#31430=VECTOR('',#108390,2.);
#31431=VECTOR('',#108395,10.);
#31432=VECTOR('',#108400,10.);
#31433=VECTOR('',#108401,10.);
#31434=VECTOR('',#108404,10.);
#31435=VECTOR('',#108405,10.);
#31436=VECTOR('',#108420,10.);
#31437=VECTOR('',#108421,10.);
#31438=VECTOR('',#108424,10.);
#31439=VECTOR('',#108429,1.6);
#31440=VECTOR('',#108432,1.55);
#31441=VECTOR('',#108435,2.15);
#31442=VECTOR('',#108438,10.);
#31443=VECTOR('',#108441,10.);
#31444=VECTOR('',#108444,10.);
#31445=VECTOR('',#108447,10.);
#31446=VECTOR('',#108450,10.);
#31447=VECTOR('',#108453,10.);
#31448=VECTOR('',#108458,10.);
#31449=VECTOR('',#108461,10.);
#31450=VECTOR('',#108462,10.);
#31451=VECTOR('',#108463,10.);
#31452=VECTOR('',#108472,10.);
#31453=VECTOR('',#108479,10.);
#31454=VECTOR('',#108482,10.);
#31455=VECTOR('',#108489,10.);
#31456=VECTOR('',#108492,10.);
#31457=VECTOR('',#108499,10.);
#31458=VECTOR('',#108502,10.);
#31459=VECTOR('',#108505,10.);
#31460=VECTOR('',#108508,10.);
#31461=VECTOR('',#108511,10.);
#31462=VECTOR('',#108514,10.);
#31463=VECTOR('',#108519,10.);
#31464=VECTOR('',#108524,10.);
#31465=VECTOR('',#108527,10.);
#31466=VECTOR('',#108528,10.);
#31467=VECTOR('',#108529,10.);
#31468=VECTOR('',#108530,10.);
#31469=VECTOR('',#108551,10.);
#31470=VECTOR('',#108562,10.);
#31471=VECTOR('',#108563,10.);
#31472=VECTOR('',#108584,10.);
#31473=VECTOR('',#108587,10.);
#31474=VECTOR('',#108590,10.);
#31475=VECTOR('',#108595,10.);
#31476=VECTOR('',#108600,10.);
#31477=VECTOR('',#108603,10.);
#31478=VECTOR('',#108628,10.);
#31479=VECTOR('',#108629,10.);
#31480=VECTOR('',#108658,10.);
#31481=VECTOR('',#108659,10.);
#31482=VECTOR('',#108662,10.);
#31483=VECTOR('',#108665,10.);
#31484=VECTOR('',#108668,10.);
#31485=VECTOR('',#108673,10.);
#31486=VECTOR('',#108674,10.);
#31487=VECTOR('',#108677,10.);
#31488=VECTOR('',#108706,0.599999999999999);
#31489=VECTOR('',#108707,10.);
#31490=VECTOR('',#108708,0.599999999999999);
#31491=VECTOR('',#108711,10.);
#31492=VECTOR('',#108712,10.);
#31493=VECTOR('',#108715,0.599999999999999);
#31494=VECTOR('',#108718,10.);
#31495=VECTOR('',#108725,10.);
#31496=VECTOR('',#108728,10.);
#31497=VECTOR('',#108731,10.);
#31498=VECTOR('',#108732,10.);
#31499=VECTOR('',#108739,10.);
#31500=VECTOR('',#108740,10.);
#31501=VECTOR('',#108741,10.);
#31502=VECTOR('',#108750,10.);
#31503=VECTOR('',#108753,10.);
#31504=VECTOR('',#108758,10.);
#31505=VECTOR('',#108763,10.);
#31506=VECTOR('',#108768,0.75);
#31507=VECTOR('',#108769,10.);
#31508=VECTOR('',#108770,10.);
#31509=VECTOR('',#108771,10.);
#31510=VECTOR('',#108772,10.);
#31511=VECTOR('',#108773,10.);
#31512=VECTOR('',#108774,10.);
#31513=VECTOR('',#108775,10.);
#31514=VECTOR('',#108776,10.);
#31515=VECTOR('',#108777,10.);
#31516=VECTOR('',#108780,10.);
#31517=VECTOR('',#108783,10.);
#31518=VECTOR('',#108788,10.);
#31519=VECTOR('',#108789,10.);
#31520=VECTOR('',#108792,10.);
#31521=VECTOR('',#108795,10.);
#31522=VECTOR('',#108796,10.);
#31523=VECTOR('',#108827,10.);
#31524=VECTOR('',#108828,10.);
#31525=VECTOR('',#108833,10.);
#31526=VECTOR('',#108834,10.);
#31527=VECTOR('',#108837,10.);
#31528=VECTOR('',#108840,10.);
#31529=VECTOR('',#108841,10.);
#31530=VECTOR('',#108842,10.);
#31531=VECTOR('',#108845,10.);
#31532=VECTOR('',#108846,10.);
#31533=VECTOR('',#108847,10.);
#31534=VECTOR('',#108850,10.);
#31535=VECTOR('',#108885,10.);
#31536=VECTOR('',#108888,10.);
#31537=VECTOR('',#108891,10.);
#31538=VECTOR('',#108896,10.);
#31539=VECTOR('',#108905,10.);
#31540=VECTOR('',#108914,10.);
#31541=VECTOR('',#108925,0.600000000000001);
#31542=VECTOR('',#108928,0.600000000000001);
#31543=VECTOR('',#108931,3.2);
#31544=VECTOR('',#108936,10.);
#31545=VECTOR('',#108941,10.);
#31546=VECTOR('',#108942,10.);
#31547=VECTOR('',#108945,10.);
#31548=VECTOR('',#108950,10.);
#31549=VECTOR('',#108951,10.);
#31550=VECTOR('',#108954,10.);
#31551=VECTOR('',#108959,10.);
#31552=VECTOR('',#108960,10.);
#31553=VECTOR('',#108963,10.);
#31554=VECTOR('',#108970,9.3);
#31555=VECTOR('',#108973,10.);
#31556=VECTOR('',#108976,10.);
#31557=VECTOR('',#109001,10.);
#31558=VECTOR('',#109002,10.);
#31559=VECTOR('',#109015,10.);
#31560=VECTOR('',#109016,10.);
#31561=VECTOR('',#109051,10.);
#31562=VECTOR('',#109052,10.);
#31563=VECTOR('',#109065,10.);
#31564=VECTOR('',#109066,10.);
#31565=VECTOR('',#109067,0.800000000000001);
#31566=VECTOR('',#109070,10.);
#31567=VECTOR('',#109075,10.);
#31568=VECTOR('',#109076,10.);
#31569=VECTOR('',#109079,10.);
#31570=VECTOR('',#109084,10.);
#31571=VECTOR('',#109089,5.7);
#31572=VECTOR('',#109098,10.);
#31573=VECTOR('',#109101,10.);
#31574=VECTOR('',#109112,10.);
#31575=VECTOR('',#109113,10.);
#31576=VECTOR('',#109132,10.);
#31577=VECTOR('',#109133,10.);
#31578=VECTOR('',#109166,10.);
#31579=VECTOR('',#109167,10.);
#31580=VECTOR('',#109174,10.);
#31581=VECTOR('',#109177,10.);
#31582=VECTOR('',#109180,19.0949617393671);
#31583=VECTOR('',#109185,10.);
#31584=VECTOR('',#109190,10.);
#31585=VECTOR('',#109191,10.);
#31586=VECTOR('',#109194,10.);
#31587=VECTOR('',#109199,10.);
#31588=VECTOR('',#109200,10.);
#31589=VECTOR('',#109207,10.);
#31590=VECTOR('',#109210,10.);
#31591=VECTOR('',#109221,10.);
#31592=VECTOR('',#109222,10.);
#31593=VECTOR('',#109233,10.);
#31594=VECTOR('',#109234,10.);
#31595=VECTOR('',#109279,6.2);
#31596=VECTOR('',#109282,4.1);
#31597=VECTOR('',#109285,10.);
#31598=VECTOR('',#109290,10.);
#31599=VECTOR('',#109293,10.);
#31600=VECTOR('',#109298,10.);
#31601=VECTOR('',#109301,10.);
#31602=VECTOR('',#109304,10.);
#31603=VECTOR('',#109309,10.);
#31604=VECTOR('',#109314,10.);
#31605=VECTOR('',#109315,10.);
#31606=VECTOR('',#109348,10.);
#31607=VECTOR('',#109349,10.);
#31608=VECTOR('',#109354,10.);
#31609=VECTOR('',#109355,10.);
#31610=VECTOR('',#109360,10.);
#31611=VECTOR('',#109363,10.);
#31612=VECTOR('',#109368,10.);
#31613=VECTOR('',#109371,10.);
#31614=VECTOR('',#109372,10.);
#31615=VECTOR('',#109375,10.);
#31616=VECTOR('',#109378,10.);
#31617=VECTOR('',#109383,12.05);
#31618=VECTOR('',#109386,10.);
#31619=VECTOR('',#109387,10.);
#31620=VECTOR('',#109390,12.05);
#31621=VECTOR('',#109391,10.);
#31622=VECTOR('',#109396,10.);
#31623=VECTOR('',#109399,10.);
#31624=VECTOR('',#109412,10.);
#31625=VECTOR('',#109413,10.);
#31626=VECTOR('',#109438,10.);
#31627=VECTOR('',#109439,10.);
#31628=VECTOR('',#109466,10.);
#31629=VECTOR('',#109467,10.);
#31630=VECTOR('',#109474,10.);
#31631=VECTOR('',#109477,10.);
#31632=VECTOR('',#109482,3.5);
#31633=VECTOR('',#109483,10.);
#31634=VECTOR('',#109486,10.);
#31635=VECTOR('',#109489,10.);
#31636=VECTOR('',#109492,10.);
#31637=VECTOR('',#109495,10.);
#31638=VECTOR('',#109500,10.);
#31639=VECTOR('',#109505,0.8);
#31640=VECTOR('',#109506,10.);
#31641=VECTOR('',#109509,0.8);
#31642=VECTOR('',#109514,0.8);
#31643=VECTOR('',#109515,10.);
#31644=VECTOR('',#109536,10.);
#31645=VECTOR('',#109537,10.);
#31646=VECTOR('',#109548,10.);
#31647=VECTOR('',#109549,10.);
#31648=VECTOR('',#109572,10.);
#31649=VECTOR('',#109573,10.);
#31650=VECTOR('',#109594,10.);
#31651=VECTOR('',#109595,10.);
#31652=VECTOR('',#109596,10.);
#31653=VECTOR('',#109599,10.);
#31654=VECTOR('',#109606,10.);
#31655=VECTOR('',#109609,10.);
#31656=VECTOR('',#109612,10.);
#31657=VECTOR('',#109619,10.);
#31658=VECTOR('',#109622,10.);
#31659=VECTOR('',#109625,10.);
#31660=VECTOR('',#109648,10.);
#31661=VECTOR('',#109649,10.);
#31662=VECTOR('',#109672,10.);
#31663=VECTOR('',#109673,10.);
#31664=VECTOR('',#109684,10.);
#31665=VECTOR('',#109685,10.);
#31666=VECTOR('',#109692,10.);
#31667=VECTOR('',#109693,10.);
#31668=VECTOR('',#109694,10.);
#31669=VECTOR('',#109697,10.);
#31670=VECTOR('',#109702,10.);
#31671=VECTOR('',#109703,10.);
#31672=VECTOR('',#109706,10.);
#31673=VECTOR('',#109711,10.);
#31674=VECTOR('',#109714,10.);
#31675=VECTOR('',#109717,10.);
#31676=VECTOR('',#109722,10.);
#31677=VECTOR('',#109729,10.);
#31678=VECTOR('',#109734,10.);
#31679=VECTOR('',#109735,10.);
#31680=VECTOR('',#109742,10.);
#31681=VECTOR('',#109753,0.4);
#31682=VECTOR('',#109756,0.4);
#31683=VECTOR('',#109759,10.);
#31684=VECTOR('',#109760,10.);
#31685=VECTOR('',#109761,10.);
#31686=VECTOR('',#109762,10.);
#31687=VECTOR('',#109763,10.);
#31688=VECTOR('',#109764,10.);
#31689=VECTOR('',#109765,10.);
#31690=VECTOR('',#109768,10.);
#31691=VECTOR('',#109769,10.);
#31692=VECTOR('',#109770,10.);
#31693=VECTOR('',#109779,10.);
#31694=VECTOR('',#109786,10.);
#31695=VECTOR('',#109793,10.);
#31696=VECTOR('',#109800,10.);
#31697=VECTOR('',#109805,10.);
#31698=VECTOR('',#109806,10.);
#31699=VECTOR('',#109807,10.);
#31700=VECTOR('',#109814,10.);
#31701=VECTOR('',#109825,1.6);
#31702=VECTOR('',#109830,2.6);
#31703=VECTOR('',#109833,10.);
#31704=VECTOR('',#109834,10.);
#31705=VECTOR('',#109835,10.);
#31706=VECTOR('',#109836,10.);
#31707=VECTOR('',#109837,10.);
#31708=VECTOR('',#109838,10.);
#31709=VECTOR('',#109839,10.);
#31710=VECTOR('',#109840,10.);
#31711=VECTOR('',#109841,10.);
#31712=VECTOR('',#109844,10.);
#31713=VECTOR('',#109849,4.2);
#31714=VECTOR('',#109860,10.);
#31715=VECTOR('',#109867,10.);
#31716=VECTOR('',#109870,10.);
#31717=VECTOR('',#109873,10.);
#31718=VECTOR('',#109874,10.);
#31719=VECTOR('',#109875,10.);
#31720=VECTOR('',#109878,10.);
#31721=VECTOR('',#109883,10.);
#31722=VECTOR('',#109884,10.);
#31723=VECTOR('',#109885,10.);
#31724=VECTOR('',#109890,10.);
#31725=VECTOR('',#109897,10.);
#31726=VECTOR('',#109900,10.);
#31727=VECTOR('',#109911,1.6);
#31728=VECTOR('',#109918,10.);
#31729=VECTOR('',#109923,10.);
#31730=VECTOR('',#109926,10.);
#31731=VECTOR('',#109931,10.);
#31732=VECTOR('',#109932,10.);
#31733=VECTOR('',#109935,10.);
#31734=VECTOR('',#109936,10.);
#31735=VECTOR('',#109941,1.3);
#31736=VECTOR('',#109946,10.);
#31737=VECTOR('',#109953,1.70000000000355);
#31738=VECTOR('',#109958,1.3);
#31739=VECTOR('',#109963,10.);
#31740=VECTOR('',#109970,1.70000000000355);
#31741=VECTOR('',#109977,10.);
#31742=VECTOR('',#109978,10.);
#31743=VECTOR('',#109981,10.);
#31744=VECTOR('',#109982,10.);
#31745=VECTOR('',#109987,10.);
#31746=VECTOR('',#109988,10.);
#31747=VECTOR('',#109991,10.);
#31748=VECTOR('',#109992,10.);
#31749=VECTOR('',#109995,10.);
#31750=VECTOR('',#109996,10.);
#31751=VECTOR('',#109997,10.);
#31752=VECTOR('',#110004,10.);
#31753=VECTOR('',#110007,10.);
#31754=VECTOR('',#110008,10.);
#31755=VECTOR('',#110011,10.);
#31756=VECTOR('',#110012,10.);
#31757=VECTOR('',#110013,10.);
#31758=VECTOR('',#110020,10.);
#31759=VECTOR('',#110023,10.);
#31760=VECTOR('',#110024,10.);
#31761=VECTOR('',#110047,10.);
#31762=VECTOR('',#110048,10.);
#31763=VECTOR('',#110049,10.);
#31764=VECTOR('',#110056,10.);
#31765=VECTOR('',#110059,10.);
#31766=VECTOR('',#110060,10.);
#31767=VECTOR('',#110065,10.);
#31768=VECTOR('',#110066,10.);
#31769=VECTOR('',#110067,10.);
#31770=VECTOR('',#110074,10.);
#31771=VECTOR('',#110077,10.);
#31772=VECTOR('',#110078,10.);
#31773=VECTOR('',#110083,10.);
#31774=VECTOR('',#110084,10.);
#31775=VECTOR('',#110085,10.);
#31776=VECTOR('',#110088,10.);
#31777=VECTOR('',#110089,10.);
#31778=VECTOR('',#110092,10.);
#31779=VECTOR('',#110093,10.);
#31780=VECTOR('',#110098,10.);
#31781=VECTOR('',#110099,10.);
#31782=VECTOR('',#110100,10.);
#31783=VECTOR('',#110105,11.95);
#31784=VECTOR('',#110106,10.);
#31785=VECTOR('',#110109,10.);
#31786=VECTOR('',#110110,10.);
#31787=VECTOR('',#110113,10.);
#31788=VECTOR('',#110116,10.);
#31789=VECTOR('',#110117,10.);
#31790=VECTOR('',#110118,10.);
#31791=VECTOR('',#110121,10.);
#31792=VECTOR('',#110134,2.);
#31793=VECTOR('',#110141,10.);
#31794=VECTOR('',#110142,10.);
#31795=VECTOR('',#110145,10.);
#31796=VECTOR('',#110150,10.);
#31797=VECTOR('',#110151,10.);
#31798=VECTOR('',#110156,10.);
#31799=VECTOR('',#110161,10.);
#31800=VECTOR('',#110178,5.79999999999998);
#31801=VECTOR('',#110183,10.);
#31802=VECTOR('',#110186,10.);
#31803=VECTOR('',#110187,10.);
#31804=VECTOR('',#110188,10.);
#31805=VECTOR('',#110191,10.);
#31806=VECTOR('',#110194,10.);
#31807=VECTOR('',#110195,10.);
#31808=VECTOR('',#110196,10.);
#31809=VECTOR('',#110207,10.);
#31810=VECTOR('',#110208,10.);
#31811=VECTOR('',#110215,10.);
#31812=VECTOR('',#110220,10.);
#31813=VECTOR('',#110231,10.);
#31814=VECTOR('',#110234,10.);
#31815=VECTOR('',#110237,10.);
#31816=VECTOR('',#110240,10.);
#31817=VECTOR('',#110243,10.);
#31818=VECTOR('',#110244,10.);
#31819=VECTOR('',#110245,10.);
#31820=VECTOR('',#110246,10.);
#31821=VECTOR('',#110249,10.);
#31822=VECTOR('',#110252,10.);
#31823=VECTOR('',#110255,0.599999999999999);
#31824=VECTOR('',#110266,10.);
#31825=VECTOR('',#110279,10.);
#31826=VECTOR('',#110282,10.);
#31827=VECTOR('',#110285,10.);
#31828=VECTOR('',#110288,10.);
#31829=VECTOR('',#110293,0.800000000000001);
#31830=VECTOR('',#110298,10.);
#31831=VECTOR('',#110307,3.95);
#31832=VECTOR('',#110316,4.15);
#31833=VECTOR('',#110321,2.25);
#31834=VECTOR('',#110328,2.6);
#31835=VECTOR('',#110337,1.6);
#31836=VECTOR('',#110342,10.);
#31837=VECTOR('',#110347,2.14999999999987);
#31838=VECTOR('',#110352,2.);
#31839=VECTOR('',#110359,10.);
#31840=VECTOR('',#110362,10.);
#31841=VECTOR('',#110365,10.);
#31842=VECTOR('',#110368,10.);
#31843=VECTOR('',#110373,10.);
#31844=VECTOR('',#110380,10.);
#31845=VECTOR('',#110385,10.);
#31846=VECTOR('',#110386,10.);
#31847=VECTOR('',#110391,10.);
#31848=VECTOR('',#110394,10.);
#31849=VECTOR('',#110397,10.);
#31850=VECTOR('',#110398,10.);
#31851=VECTOR('',#110403,3.1);
#31852=VECTOR('',#110408,10.);
#31853=VECTOR('',#110409,10.);
#31854=VECTOR('',#110412,10.);
#31855=VECTOR('',#110419,10.);
#31856=VECTOR('',#110422,10.);
#31857=VECTOR('',#110427,10.);
#31858=VECTOR('',#110446,1.55);
#31859=VECTOR('',#110451,1.5);
#31860=VECTOR('',#110474,1.65);
#31861=VECTOR('',#110479,3.625);
#31862=VECTOR('',#110490,1.1);
#31863=VECTOR('',#110507,2.1);
#31864=VECTOR('',#110534,0.75);
#31865=VECTOR('',#110537,10.);
#31866=VECTOR('',#110544,10.);
#31867=VECTOR('',#110545,10.);
#31868=VECTOR('',#110546,10.);
#31869=VECTOR('',#110547,10.);
#31870=VECTOR('',#110550,10.);
#31871=VECTOR('',#110551,10.);
#31872=VECTOR('',#110552,10.);
#31873=VECTOR('',#110569,10.);
#31874=VECTOR('',#110570,10.);
#31875=VECTOR('',#110605,10.);
#31876=VECTOR('',#110612,0.6);
#31877=VECTOR('',#110615,10.);
#31878=VECTOR('',#110630,10.);
#31879=VECTOR('',#110631,10.);
#31880=VECTOR('',#110632,10.);
#31881=VECTOR('',#110639,4.1);
#31882=VECTOR('',#110648,10.);
#31883=VECTOR('',#110649,10.);
#31884=VECTOR('',#110650,10.);
#31885=VECTOR('',#110651,10.);
#31886=VECTOR('',#110656,10.);
#31887=VECTOR('',#110663,10.);
#31888=VECTOR('',#110666,10.);
#31889=VECTOR('',#110669,10.);
#31890=VECTOR('',#110670,10.);
#31891=VECTOR('',#110671,10.);
#31892=VECTOR('',#110676,10.);
#31893=VECTOR('',#110689,10.);
#31894=VECTOR('',#110694,10.);
#31895=VECTOR('',#110703,10.);
#31896=VECTOR('',#110704,10.);
#31897=VECTOR('',#110711,10.);
#31898=VECTOR('',#110712,10.);
#31899=VECTOR('',#110713,10.);
#31900=VECTOR('',#110714,10.);
#31901=VECTOR('',#110723,10.);
#31902=VECTOR('',#110724,10.);
#31903=VECTOR('',#110725,10.);
#31904=VECTOR('',#110726,10.);
#31905=VECTOR('',#110727,10.);
#31906=VECTOR('',#110728,10.);
#31907=VECTOR('',#110729,10.);
#31908=VECTOR('',#110734,10.);
#31909=VECTOR('',#110737,10.);
#31910=VECTOR('',#110738,10.);
#31911=VECTOR('',#110747,10.);
#31912=VECTOR('',#110750,10.);
#31913=VECTOR('',#110751,10.);
#31914=VECTOR('',#110754,10.);
#31915=VECTOR('',#110755,10.);
#31916=VECTOR('',#110760,10.);
#31917=VECTOR('',#110763,10.);
#31918=VECTOR('',#110768,10.);
#31919=VECTOR('',#110777,10.);
#31920=VECTOR('',#110784,10.);
#31921=VECTOR('',#110793,10.);
#31922=VECTOR('',#110808,3.05);
#31923=VECTOR('',#110817,3.15);
#31924=VECTOR('',#110820,10.);
#31925=VECTOR('',#110821,10.);
#31926=VECTOR('',#110822,10.);
#31927=VECTOR('',#110827,10.);
#31928=VECTOR('',#110832,10.);
#31929=VECTOR('',#110835,10.);
#31930=VECTOR('',#110840,10.);
#31931=VECTOR('',#110845,10.);
#31932=VECTOR('',#110848,10.);
#31933=VECTOR('',#110867,1.);
#31934=VECTOR('',#110874,10.);
#31935=VECTOR('',#110879,10.);
#31936=VECTOR('',#110880,10.);
#31937=VECTOR('',#110881,10.);
#31938=VECTOR('',#110882,10.);
#31939=VECTOR('',#110885,10.);
#31940=VECTOR('',#110886,10.);
#31941=VECTOR('',#110887,10.);
#31942=VECTOR('',#110888,10.);
#31943=VECTOR('',#110899,10.);
#31944=VECTOR('',#110900,10.);
#31945=VECTOR('',#110927,10.);
#31946=VECTOR('',#110928,10.);
#31947=VECTOR('',#110929,10.);
#31948=VECTOR('',#110956,10.);
#31949=VECTOR('',#110959,10.);
#31950=VECTOR('',#110962,10.);
#31951=VECTOR('',#110963,10.);
#31952=VECTOR('',#110972,10.);
#31953=VECTOR('',#110975,10.);
#31954=VECTOR('',#110978,10.);
#31955=VECTOR('',#110989,10.);
#31956=VECTOR('',#111000,10.);
#31957=VECTOR('',#111003,10.);
#31958=VECTOR('',#111006,10.);
#31959=VECTOR('',#111013,4.1);
#31960=VECTOR('',#111018,10.);
#31961=VECTOR('',#111021,10.);
#31962=VECTOR('',#111024,10.);
#31963=VECTOR('',#111037,10.);
#31964=VECTOR('',#111038,10.);
#31965=VECTOR('',#111039,10.);
#31966=VECTOR('',#111044,10.);
#31967=VECTOR('',#111049,10.);
#31968=VECTOR('',#111050,10.);
#31969=VECTOR('',#111057,1.);
#31970=VECTOR('',#111070,10.);
#31971=VECTOR('',#111079,10.);
#31972=VECTOR('',#111080,10.);
#31973=VECTOR('',#111081,10.);
#31974=VECTOR('',#111082,10.);
#31975=VECTOR('',#111085,10.);
#31976=VECTOR('',#111086,10.);
#31977=VECTOR('',#111087,10.);
#31978=VECTOR('',#111088,10.);
#31979=VECTOR('',#111091,10.);
#31980=VECTOR('',#111092,10.);
#31981=VECTOR('',#111095,10.);
#31982=VECTOR('',#111102,10.);
#31983=VECTOR('',#111103,10.);
#31984=VECTOR('',#111104,10.);
#31985=VECTOR('',#111107,10.);
#31986=VECTOR('',#111110,10.);
#31987=VECTOR('',#111111,10.);
#31988=VECTOR('',#111112,10.);
#31989=VECTOR('',#111115,10.);
#31990=VECTOR('',#111116,10.);
#31991=VECTOR('',#111123,10.);
#31992=VECTOR('',#111134,10.);
#31993=VECTOR('',#111135,10.);
#31994=VECTOR('',#111136,10.);
#31995=VECTOR('',#111137,10.);
#31996=VECTOR('',#111138,10.);
#31997=VECTOR('',#111141,10.);
#31998=VECTOR('',#111142,10.);
#31999=VECTOR('',#111143,10.);
#32000=VECTOR('',#111146,10.);
#32001=VECTOR('',#111147,10.);
#32002=VECTOR('',#111148,10.);
#32003=VECTOR('',#111149,10.);
#32004=VECTOR('',#111150,10.);
#32005=VECTOR('',#111151,10.);
#32006=VECTOR('',#111162,10.);
#32007=VECTOR('',#111171,10.);
#32008=VECTOR('',#111172,10.);
#32009=VECTOR('',#111175,8.);
#32010=VECTOR('',#111176,10.);
#32011=VECTOR('',#111177,10.);
#32012=VECTOR('',#111180,10.);
#32013=VECTOR('',#111183,10.);
#32014=VECTOR('',#111186,10.);
#32015=VECTOR('',#111187,8.);
#32016=VECTOR('',#111190,10.);
#32017=VECTOR('',#111191,10.);
#32018=VECTOR('',#111192,10.);
#32019=VECTOR('',#111193,10.);
#32020=VECTOR('',#111194,10.);
#32021=VECTOR('',#111197,10.);
#32022=VECTOR('',#111200,10.);
#32023=VECTOR('',#111203,10.);
#32024=VECTOR('',#111208,10.);
#32025=VECTOR('',#111211,10.);
#32026=VECTOR('',#111214,5.);
#32027=VECTOR('',#111215,10.);
#32028=VECTOR('',#111218,10.);
#32029=VECTOR('',#111221,10.);
#32030=VECTOR('',#111222,10.);
#32031=VECTOR('',#111225,10.);
#32032=VECTOR('',#111230,10.);
#32033=VECTOR('',#111231,10.);
#32034=VECTOR('',#111232,10.);
#32035=VECTOR('',#111233,10.);
#32036=VECTOR('',#111234,10.);
#32037=VECTOR('',#111241,10.);
#32038=VECTOR('',#111242,10.);
#32039=VECTOR('',#111245,10.);
#32040=VECTOR('',#111246,10.);
#32041=VECTOR('',#111249,10.);
#32042=VECTOR('',#111252,10.);
#32043=VECTOR('',#111253,10.);
#32044=VECTOR('',#111260,10.);
#32045=VECTOR('',#111265,10.);
#32046=VECTOR('',#111268,10.);
#32047=VECTOR('',#111275,10.);
#32048=VECTOR('',#111278,10.);
#32049=VECTOR('',#111281,10.);
#32050=VECTOR('',#111282,10.);
#32051=VECTOR('',#111287,10.);
#32052=VECTOR('',#111288,10.);
#32053=VECTOR('',#111291,10.);
#32054=VECTOR('',#111296,10.);
#32055=VECTOR('',#111299,10.);
#32056=VECTOR('',#111300,10.);
#32057=VECTOR('',#111301,10.);
#32058=VECTOR('',#111304,10.);
#32059=VECTOR('',#111309,10.);
#32060=VECTOR('',#111310,10.);
#32061=VECTOR('',#111317,10.);
#32062=VECTOR('',#111320,10.);
#32063=VECTOR('',#111323,10.);
#32064=VECTOR('',#111326,10.);
#32065=VECTOR('',#111339,10.);
#32066=VECTOR('',#111350,10.);
#32067=VECTOR('',#111365,10.);
#32068=VECTOR('',#111378,10.);
#32069=VECTOR('',#111383,10.);
#32070=VECTOR('',#111386,10.);
#32071=VECTOR('',#111387,10.);
#32072=VECTOR('',#111390,10.);
#32073=VECTOR('',#111403,10.);
#32074=VECTOR('',#111414,10.);
#32075=VECTOR('',#111417,10.);
#32076=VECTOR('',#111418,5.);
#32077=VECTOR('',#111421,10.);
#32078=VECTOR('',#111422,10.);
#32079=VECTOR('',#111427,10.);
#32080=VECTOR('',#111432,1.5);
#32081=VECTOR('',#111439,10.);
#32082=VECTOR('',#111442,1.6);
#32083=VECTOR('',#111445,1.5);
#32084=VECTOR('',#111448,4.);
#32085=VECTOR('',#111449,4.);
#32086=VECTOR('',#111456,1.4);
#32087=VECTOR('',#111461,1.5);
#32088=VECTOR('',#111470,1.4);
#32089=VECTOR('',#111479,1.45);
#32090=VECTOR('',#111486,1.5);
#32091=VECTOR('',#111493,1.45);
#32092=VECTOR('',#111922,2.9);
#32093=VECTOR('',#111931,1.5);
#32094=VECTOR('',#111940,1.5);
#32095=VECTOR('',#111949,8.8);
#32096=VECTOR('',#111958,1.7);
#32097=VECTOR('',#111965,1.7);
#32098=VECTOR('',#111972,3.3);
#32099=VECTOR('',#111981,2.5);
#32100=VECTOR('',#111986,1.5);
#32101=VECTOR('',#111989,1.5);
#32102=VECTOR('',#111992,9.);
#32103=VECTOR('',#111997,9.);
#32104=VECTOR('',#112000,3.5);
#32105=VECTOR('',#112005,2.5);
#32106=VECTOR('',#112716,1.);
#32107=VECTOR('',#112723,1.);
#32108=VECTOR('',#112824,2.3);
#32109=VECTOR('',#112827,2.3);
#32110=VECTOR('',#112832,2.3);
#32111=VECTOR('',#112835,2.299999999);
#32112=VECTOR('',#112840,3.5);
#32113=VECTOR('',#112843,1.5);
#32114=VECTOR('',#112846,1.5);
#32115=VECTOR('',#112851,3.);
#32116=VECTOR('',#112856,5.);
#32117=VECTOR('',#112859,5.);
#32118=VECTOR('',#112864,5.);
#32119=VECTOR('',#112867,5.);
#32120=VECTOR('',#112872,5.);
#32121=VECTOR('',#112875,5.);
#32122=VECTOR('',#112880,5.);
#32123=VECTOR('',#112883,5.);
#32124=VECTOR('',#112886,1.5);
#32125=VECTOR('',#113181,1.40306029339696);
#32126=VECTOR('',#113186,1.40306029339696);
#32127=VECTOR('',#113189,1.40306029339696);
#32128=VECTOR('',#113194,1.40306029339696);
#32129=VECTOR('',#113203,5.);
#32130=VECTOR('',#113204,5.);
#32131=VECTOR('',#113209,5.);
#32132=VECTOR('',#113212,5.);
#32133=VECTOR('',#113215,5.);
#32134=VECTOR('',#113216,5.);
#32135=VECTOR('',#113221,5.);
#32136=VECTOR('',#113222,5.);
#32137=VECTOR('',#113227,5.);
#32138=VECTOR('',#113228,5.);
#32139=VECTOR('',#113233,5.);
#32140=VECTOR('',#113238,5.);
#32141=VECTOR('',#113243,5.);
#32142=VECTOR('',#113246,5.);
#32143=VECTOR('',#113249,5.);
#32144=VECTOR('',#113250,5.);
#32145=VECTOR('',#113255,5.);
#32146=VECTOR('',#113256,5.);
#32147=VECTOR('',#113261,5.);
#32148=VECTOR('',#113264,5.);
#32149=VECTOR('',#113267,5.);
#32150=VECTOR('',#113268,5.);
#32151=VECTOR('',#113275,5.);
#32152=VECTOR('',#113280,5.);
#32153=VECTOR('',#113283,5.);
#32154=VECTOR('',#113286,5.);
#32155=VECTOR('',#113289,5.);
#32156=VECTOR('',#113290,5.);
#32157=VECTOR('',#113295,5.);
#32158=VECTOR('',#113298,5.);
#32159=VECTOR('',#113301,5.);
#32160=VECTOR('',#113302,5.);
#32161=VECTOR('',#113307,5.);
#32162=VECTOR('',#113308,5.);
#32163=VECTOR('',#113313,5.);
#32164=VECTOR('',#113316,5.);
#32165=VECTOR('',#113319,5.);
#32166=VECTOR('',#113320,5.);
#32167=VECTOR('',#113325,5.);
#32168=VECTOR('',#113328,5.);
#32169=VECTOR('',#113331,5.);
#32170=VECTOR('',#113334,5.);
#32171=VECTOR('',#113337,5.);
#32172=VECTOR('',#113340,5.);
#32173=VECTOR('',#113343,5.);
#32174=VECTOR('',#113344,5.);
#32175=VECTOR('',#113349,5.);
#32176=VECTOR('',#113352,5.);
#32177=VECTOR('',#113355,5.);
#32178=VECTOR('',#113356,5.);
#32179=VECTOR('',#113361,5.);
#32180=VECTOR('',#113362,5.);
#32181=VECTOR('',#113367,5.);
#32182=VECTOR('',#113370,5.);
#32183=VECTOR('',#113373,5.);
#32184=VECTOR('',#113374,5.);
#32185=VECTOR('',#113379,5.);
#32186=VECTOR('',#113382,5.);
#32187=VECTOR('',#113385,5.);
#32188=VECTOR('',#113388,5.);
#32189=VECTOR('',#113391,5.);
#32190=VECTOR('',#113394,5.);
#32191=VECTOR('',#113397,5.);
#32192=VECTOR('',#113398,5.);
#32193=VECTOR('',#113403,5.);
#32194=VECTOR('',#113404,5.);
#32195=VECTOR('',#113409,5.);
#32196=VECTOR('',#113410,5.);
#32197=VECTOR('',#113633,5.);
#32198=VECTOR('',#113634,5.);
#32199=VECTOR('',#113637,5.);
#32200=VECTOR('',#113640,5.);
#32201=VECTOR('',#113645,5.);
#32202=VECTOR('',#113648,5.);
#32203=VECTOR('',#113653,5.);
#32204=VECTOR('',#113656,5.);
#32205=VECTOR('',#113661,5.);
#32206=VECTOR('',#113664,5.);
#32207=VECTOR('',#113669,5.);
#32208=VECTOR('',#113672,5.);
#32209=VECTOR('',#113677,5.);
#32210=VECTOR('',#113680,5.);
#32211=VECTOR('',#113685,5.);
#32212=VECTOR('',#113688,5.);
#32213=VECTOR('',#113693,5.);
#32214=VECTOR('',#113696,5.);
#32215=VECTOR('',#113701,5.);
#32216=VECTOR('',#113704,5.);
#32217=VECTOR('',#113709,5.);
#32218=VECTOR('',#113712,5.);
#32219=VECTOR('',#113717,5.);
#32220=VECTOR('',#113720,5.);
#32221=VECTOR('',#113725,5.);
#32222=VECTOR('',#113728,5.);
#32223=VECTOR('',#113733,5.);
#32224=VECTOR('',#113736,5.);
#32225=VECTOR('',#113741,5.);
#32226=VECTOR('',#113744,5.);
#32227=VECTOR('',#113749,5.);
#32228=VECTOR('',#113752,5.);
#32229=VECTOR('',#113757,5.);
#32230=VECTOR('',#113760,5.);
#32231=VECTOR('',#113765,5.);
#32232=VECTOR('',#113768,5.);
#32233=VECTOR('',#113773,5.);
#32234=VECTOR('',#113776,5.);
#32235=VECTOR('',#113781,5.);
#32236=VECTOR('',#113784,5.);
#32237=VECTOR('',#113789,5.);
#32238=VECTOR('',#113792,5.);
#32239=VECTOR('',#113797,5.);
#32240=VECTOR('',#113800,5.);
#32241=VECTOR('',#113805,5.);
#32242=VECTOR('',#113808,5.);
#32243=VECTOR('',#113813,5.);
#32244=VECTOR('',#113816,5.);
#32245=VECTOR('',#113821,5.);
#32246=VECTOR('',#113824,5.);
#32247=VECTOR('',#113829,5.);
#32248=VECTOR('',#113832,5.);
#32249=VECTOR('',#113837,5.);
#32250=VECTOR('',#113842,5.);
#32251=VECTOR('',#113847,5.);
#32252=VECTOR('',#113850,5.);
#32253=VECTOR('',#113855,5.);
#32254=VECTOR('',#113858,5.);
#32255=VECTOR('',#113863,5.);
#32256=VECTOR('',#113866,5.);
#32257=VECTOR('',#113871,5.);
#32258=VECTOR('',#113874,5.);
#32259=VECTOR('',#113879,5.);
#32260=VECTOR('',#113884,5.);
#32261=VECTOR('',#113889,5.);
#32262=VECTOR('',#113892,5.);
#32263=VECTOR('',#113897,5.);
#32264=VECTOR('',#113900,5.);
#32265=VECTOR('',#113905,5.);
#32266=VECTOR('',#113908,5.);
#32267=VECTOR('',#113913,5.);
#32268=VECTOR('',#113916,5.);
#32269=VECTOR('',#113929,2.3);
#32270=VECTOR('',#113930,1.40306029239696);
#32271=VECTOR('',#113931,1.40306029239696);
#32272=VECTOR('',#113934,2.3);
#32273=VECTOR('',#113941,2.3);
#32274=VECTOR('',#113948,2.3);
#32275=VECTOR('',#113955,2.3);
#32276=VECTOR('',#113956,1.40306029239696);
#32277=VECTOR('',#113957,1.40306029239696);
#32278=VECTOR('',#113960,2.3);
#32279=VECTOR('',#113973,2.3);
#32280=VECTOR('',#113976,2.3);
#32281=VECTOR('',#113981,1.40306029339696);
#32282=VECTOR('',#113982,1.40306029239696);
#32283=VECTOR('',#113985,2.3);
#32284=VECTOR('',#113992,2.3);
#32285=VECTOR('',#113997,2.3);
#32286=VECTOR('',#113998,1.40306029339696);
#32287=VECTOR('',#113999,1.40306029239696);
#32288=VECTOR('',#114002,2.3);
#32289=VECTOR('',#114077,3.);
#32290=VECTOR('',#114080,3.);
#32291=VECTOR('',#114081,3.);
#32292=VECTOR('',#114082,3.);
#32293=VECTOR('',#114085,3.);
#32294=VECTOR('',#114094,3.);
#32295=VECTOR('',#114097,3.);
#32296=VECTOR('',#114098,3.);
#32297=VECTOR('',#114101,3.);
#32298=VECTOR('',#114110,3.);
#32299=VECTOR('',#114113,3.);
#32300=VECTOR('',#114114,3.);
#32301=VECTOR('',#114117,3.);
#32302=VECTOR('',#114126,3.);
#32303=VECTOR('',#114129,3.);
#32304=VECTOR('',#114130,3.);
#32305=VECTOR('',#114133,3.);
#32306=VECTOR('',#114142,3.);
#32307=VECTOR('',#114145,3.);
#32308=VECTOR('',#114146,3.);
#32309=VECTOR('',#114149,3.);
#32310=VECTOR('',#114158,3.);
#32311=VECTOR('',#114161,3.);
#32312=VECTOR('',#114162,3.);
#32313=VECTOR('',#114165,3.);
#32314=VECTOR('',#114174,3.);
#32315=VECTOR('',#114177,3.);
#32316=VECTOR('',#114178,3.);
#32317=VECTOR('',#114181,3.);
#32318=VECTOR('',#114190,3.);
#32319=VECTOR('',#114193,3.);
#32320=VECTOR('',#114194,3.);
#32321=VECTOR('',#114197,3.);
#32322=VECTOR('',#114206,3.);
#32323=VECTOR('',#114209,3.);
#32324=VECTOR('',#114210,3.);
#32325=VECTOR('',#114213,3.);
#32326=VECTOR('',#114222,3.);
#32327=VECTOR('',#114225,3.);
#32328=VECTOR('',#114226,3.);
#32329=VECTOR('',#114229,3.);
#32330=VECTOR('',#114238,3.);
#32331=VECTOR('',#114241,3.);
#32332=VECTOR('',#114242,3.);
#32333=VECTOR('',#114245,3.);
#32334=VECTOR('',#114254,3.);
#32335=VECTOR('',#114257,3.);
#32336=VECTOR('',#114258,3.);
#32337=VECTOR('',#114261,3.);
#32338=VECTOR('',#114270,3.);
#32339=VECTOR('',#114273,3.);
#32340=VECTOR('',#114274,3.);
#32341=VECTOR('',#114277,3.);
#32342=VECTOR('',#114286,3.);
#32343=VECTOR('',#114289,3.);
#32344=VECTOR('',#114290,3.);
#32345=VECTOR('',#114293,3.);
#32346=VECTOR('',#114302,3.);
#32347=VECTOR('',#114305,3.);
#32348=VECTOR('',#114306,3.);
#32349=VECTOR('',#114309,3.);
#32350=VECTOR('',#114318,3.);
#32351=VECTOR('',#114321,3.);
#32352=VECTOR('',#114322,3.);
#32353=VECTOR('',#114325,3.);
#32354=VECTOR('',#114334,3.);
#32355=VECTOR('',#114337,3.);
#32356=VECTOR('',#114338,3.);
#32357=VECTOR('',#114341,3.);
#32358=VECTOR('',#114350,3.);
#32359=VECTOR('',#114353,3.);
#32360=VECTOR('',#114354,3.);
#32361=VECTOR('',#114357,3.);
#32362=VECTOR('',#114366,3.);
#32363=VECTOR('',#114369,3.);
#32364=VECTOR('',#114370,3.);
#32365=VECTOR('',#114373,3.);
#32366=VECTOR('',#114382,3.);
#32367=VECTOR('',#114385,3.);
#32368=VECTOR('',#114386,3.);
#32369=VECTOR('',#114389,3.);
#32370=VECTOR('',#114398,3.);
#32371=VECTOR('',#114401,3.);
#32372=VECTOR('',#114402,3.);
#32373=VECTOR('',#114405,3.);
#32374=VECTOR('',#114414,3.);
#32375=VECTOR('',#114417,3.);
#32376=VECTOR('',#114418,3.);
#32377=VECTOR('',#114421,3.);
#32378=VECTOR('',#114430,3.);
#32379=VECTOR('',#114433,3.);
#32380=VECTOR('',#114434,3.);
#32381=VECTOR('',#114437,3.);
#32382=VECTOR('',#114446,3.);
#32383=VECTOR('',#114449,3.);
#32384=VECTOR('',#114450,3.);
#32385=VECTOR('',#114453,3.);
#32386=VECTOR('',#114462,3.);
#32387=VECTOR('',#114465,3.);
#32388=VECTOR('',#114466,3.);
#32389=VECTOR('',#114469,3.);
#32390=VECTOR('',#114478,3.);
#32391=VECTOR('',#114481,3.);
#32392=VECTOR('',#114482,3.);
#32393=VECTOR('',#114485,3.);
#32394=VECTOR('',#114494,3.);
#32395=VECTOR('',#114497,3.);
#32396=VECTOR('',#114498,3.);
#32397=VECTOR('',#114501,3.);
#32398=VECTOR('',#114510,3.);
#32399=VECTOR('',#114513,3.);
#32400=VECTOR('',#114514,3.);
#32401=VECTOR('',#114517,3.);
#32402=VECTOR('',#114526,3.);
#32403=VECTOR('',#114529,3.);
#32404=VECTOR('',#114530,3.);
#32405=VECTOR('',#114533,3.);
#32406=VECTOR('',#114542,3.);
#32407=VECTOR('',#114545,3.);
#32408=VECTOR('',#114546,3.);
#32409=VECTOR('',#114549,3.);
#32410=VECTOR('',#114558,3.);
#32411=VECTOR('',#114561,3.);
#32412=VECTOR('',#114562,3.);
#32413=VECTOR('',#114565,3.);
#32414=VECTOR('',#114574,3.);
#32415=VECTOR('',#114577,3.);
#32416=VECTOR('',#114578,3.);
#32417=VECTOR('',#114581,3.);
#32418=VECTOR('',#114590,3.);
#32419=VECTOR('',#114593,3.);
#32420=VECTOR('',#114594,3.);
#32421=VECTOR('',#114597,3.);
#32422=VECTOR('',#114606,3.);
#32423=VECTOR('',#114609,3.);
#32424=VECTOR('',#114610,3.);
#32425=VECTOR('',#114613,3.);
#32426=VECTOR('',#114622,3.);
#32427=VECTOR('',#114625,3.);
#32428=VECTOR('',#114626,3.);
#32429=VECTOR('',#114629,3.);
#32430=VECTOR('',#114638,3.);
#32431=VECTOR('',#114641,3.);
#32432=VECTOR('',#114642,3.);
#32433=VECTOR('',#114645,3.);
#32434=VECTOR('',#114654,3.);
#32435=VECTOR('',#114657,3.);
#32436=VECTOR('',#114658,3.);
#32437=VECTOR('',#114661,3.);
#32438=VECTOR('',#114670,3.);
#32439=VECTOR('',#114673,3.);
#32440=VECTOR('',#114674,3.);
#32441=VECTOR('',#114677,3.);
#32442=VECTOR('',#114686,3.);
#32443=VECTOR('',#114689,3.);
#32444=VECTOR('',#114690,3.);
#32445=VECTOR('',#114693,3.);
#32446=VECTOR('',#114702,3.);
#32447=VECTOR('',#114705,3.);
#32448=VECTOR('',#114706,3.);
#32449=VECTOR('',#114709,3.);
#32450=VECTOR('',#114718,3.);
#32451=VECTOR('',#114721,3.);
#32452=VECTOR('',#114722,3.);
#32453=VECTOR('',#114725,3.);
#32454=VECTOR('',#114734,3.);
#32455=VECTOR('',#114737,3.);
#32456=VECTOR('',#114738,3.);
#32457=VECTOR('',#114741,3.);
#32458=VECTOR('',#114750,3.);
#32459=VECTOR('',#114753,3.);
#32460=VECTOR('',#114754,3.);
#32461=VECTOR('',#114767,3.);
#32462=VECTOR('',#114772,3.);
#32463=VECTOR('',#114777,3.);
#32464=VECTOR('',#114780,3.);
#32465=VECTOR('',#114783,3.5);
#32466=VECTOR('',#114792,1.5);
#32467=VECTOR('',#114799,1.5);
#32468=VECTOR('',#114808,0.368727902070758);
#32469=VECTOR('',#114811,0.368744954930928);
#32470=VECTOR('',#114814,0.368727849984952);
#32471=VECTOR('',#114817,0.368744955088197);
#32472=VECTOR('',#114820,0.368727849938405);
#32473=VECTOR('',#114823,0.368744956005126);
#32474=VECTOR('',#114826,0.368727850051691);
#32475=VECTOR('',#114829,0.368744956006768);
#32476=VECTOR('',#114832,0.368727850019134);
#32477=VECTOR('',#114835,0.368744954912587);
#32478=VECTOR('',#114838,0.368727849038679);
#32479=VECTOR('',#114841,0.368744954818811);
#32480=VECTOR('',#114844,0.368727849942864);
#32481=VECTOR('',#114847,0.368744954945107);
#32482=VECTOR('',#114850,0.368727848847665);
#32483=VECTOR('',#114853,0.368744955050679);
#32484=VECTOR('',#114856,0.36872784901569);
#32485=VECTOR('',#114859,0.368744955038109);
#32486=VECTOR('',#114862,0.368727900991839);
#32487=VECTOR('',#114865,0.368744954973241);
#32488=VECTOR('',#114868,0.368727902134879);
#32489=VECTOR('',#114871,0.368744955084494);
#32490=VECTOR('',#114874,0.368727901012447);
#32491=VECTOR('',#114877,0.368744954201684);
#32492=VECTOR('',#114880,0.368727902088567);
#32493=VECTOR('',#114883,0.368744955058901);
#32494=VECTOR('',#114886,0.368727901040032);
#32495=VECTOR('',#114889,0.368744955063777);
#32496=VECTOR('',#114892,0.368727900880366);
#32497=VECTOR('',#114895,0.368744954861438);
#32498=VECTOR('',#114898,0.368727901937789);
#32499=VECTOR('',#114901,0.368744955126573);
#32500=VECTOR('',#114904,0.368727902027393);
#32501=VECTOR('',#114907,0.368744956235032);
#32502=VECTOR('',#114916,3.5);
#32503=VECTOR('',#114923,10.);
#32504=VECTOR('',#114926,10.);
#32505=VECTOR('',#114927,10.);
#32506=VECTOR('',#114930,10.);
#32507=VECTOR('',#114931,10.);
#32508=VECTOR('',#114934,10.);
#32509=VECTOR('',#114939,10.);
#32510=VECTOR('',#114940,10.);
#32511=VECTOR('',#114941,10.);
#32512=VECTOR('',#114944,10.);
#32513=VECTOR('',#114947,10.);
#32514=VECTOR('',#114950,10.);
#32515=VECTOR('',#114951,10.);
#32516=VECTOR('',#114954,10.);
#32517=VECTOR('',#114959,10.);
#32518=VECTOR('',#114960,10.);
#32519=VECTOR('',#114961,10.);
#32520=VECTOR('',#114964,10.);
#32521=VECTOR('',#114967,10.);
#32522=VECTOR('',#114970,10.);
#32523=VECTOR('',#114971,10.);
#32524=VECTOR('',#114974,10.);
#32525=VECTOR('',#114979,10.);
#32526=VECTOR('',#114980,10.);
#32527=VECTOR('',#114981,10.);
#32528=VECTOR('',#114984,10.);
#32529=VECTOR('',#114987,10.);
#32530=VECTOR('',#114990,10.);
#32531=VECTOR('',#114991,10.);
#32532=VECTOR('',#114994,10.);
#32533=VECTOR('',#114999,10.);
#32534=VECTOR('',#115000,10.);
#32535=VECTOR('',#115001,10.);
#32536=VECTOR('',#115004,10.);
#32537=VECTOR('',#115007,10.);
#32538=VECTOR('',#115010,10.);
#32539=VECTOR('',#115011,10.);
#32540=VECTOR('',#115014,10.);
#32541=VECTOR('',#115019,10.);
#32542=VECTOR('',#115020,10.);
#32543=VECTOR('',#115021,10.);
#32544=VECTOR('',#115024,10.);
#32545=VECTOR('',#115027,10.);
#32546=VECTOR('',#115030,10.);
#32547=VECTOR('',#115031,10.);
#32548=VECTOR('',#115034,10.);
#32549=VECTOR('',#115039,10.);
#32550=VECTOR('',#115040,10.);
#32551=VECTOR('',#115041,10.);
#32552=VECTOR('',#115044,10.);
#32553=VECTOR('',#115047,10.);
#32554=VECTOR('',#115050,10.);
#32555=VECTOR('',#115051,10.);
#32556=VECTOR('',#115054,10.);
#32557=VECTOR('',#115059,10.);
#32558=VECTOR('',#115060,10.);
#32559=VECTOR('',#115061,10.);
#32560=VECTOR('',#115064,10.);
#32561=VECTOR('',#115067,10.);
#32562=VECTOR('',#115070,10.);
#32563=VECTOR('',#115071,10.);
#32564=VECTOR('',#115074,10.);
#32565=VECTOR('',#115079,10.);
#32566=VECTOR('',#115080,10.);
#32567=VECTOR('',#115081,10.);
#32568=VECTOR('',#115084,10.);
#32569=VECTOR('',#115087,10.);
#32570=VECTOR('',#115090,10.);
#32571=VECTOR('',#115091,10.);
#32572=VECTOR('',#115096,10.);
#32573=VECTOR('',#115099,10.);
#32574=VECTOR('',#115102,10.);
#32575=VECTOR('',#115105,10.);
#32576=VECTOR('',#115108,10.);
#32577=VECTOR('',#115111,10.);
#32578=VECTOR('',#115114,10.);
#32579=VECTOR('',#115117,10.);
#32580=VECTOR('',#115120,10.);
#32581=VECTOR('',#115123,10.);
#32582=VECTOR('',#115126,10.);
#32583=VECTOR('',#115129,10.);
#32584=VECTOR('',#115132,10.);
#32585=VECTOR('',#115135,10.);
#32586=VECTOR('',#115138,10.);
#32587=VECTOR('',#115141,10.);
#32588=VECTOR('',#115144,10.);
#32589=VECTOR('',#115147,10.);
#32590=VECTOR('',#115148,10.);
#32591=VECTOR('',#115151,10.);
#32592=VECTOR('',#115154,10.);
#32593=VECTOR('',#115155,10.);
#32594=VECTOR('',#115158,10.);
#32595=VECTOR('',#115159,10.);
#32596=VECTOR('',#115162,10.);
#32597=VECTOR('',#115165,10.);
#32598=VECTOR('',#115168,10.);
#32599=VECTOR('',#115169,10.);
#32600=VECTOR('',#115172,10.);
#32601=VECTOR('',#115173,10.);
#32602=VECTOR('',#115176,10.);
#32603=VECTOR('',#115179,10.);
#32604=VECTOR('',#115180,10.);
#32605=VECTOR('',#115183,10.);
#32606=VECTOR('',#115184,10.);
#32607=VECTOR('',#115185,10.);
#32608=VECTOR('',#115188,10.);
#32609=VECTOR('',#115191,10.);
#32610=VECTOR('',#115194,10.);
#32611=VECTOR('',#115195,10.);
#32612=VECTOR('',#115198,10.);
#32613=VECTOR('',#115199,10.);
#32614=VECTOR('',#115202,10.);
#32615=VECTOR('',#115207,10.);
#32616=VECTOR('',#115210,10.);
#32617=VECTOR('',#115211,10.);
#32618=VECTOR('',#115214,10.);
#32619=VECTOR('',#115215,10.);
#32620=VECTOR('',#115218,10.);
#32621=VECTOR('',#115221,10.);
#32622=VECTOR('',#115222,10.);
#32623=VECTOR('',#115225,10.);
#32624=VECTOR('',#115226,10.);
#32625=VECTOR('',#115227,10.);
#32626=VECTOR('',#115230,10.);
#32627=VECTOR('',#115233,10.);
#32628=VECTOR('',#115236,10.);
#32629=VECTOR('',#115237,10.);
#32630=VECTOR('',#115240,10.);
#32631=VECTOR('',#115241,10.);
#32632=VECTOR('',#115244,10.);
#32633=VECTOR('',#115249,10.);
#32634=VECTOR('',#115252,10.);
#32635=VECTOR('',#115253,10.);
#32636=VECTOR('',#115256,10.);
#32637=VECTOR('',#115257,10.);
#32638=VECTOR('',#115260,10.);
#32639=VECTOR('',#115265,3.5);
#32640=VECTOR('',#115286,1.6);
#32641=VECTOR('',#115289,10.);
#32642=VECTOR('',#115292,1.6);
#32643=VECTOR('',#115299,10.);
#32644=VECTOR('',#115304,10.);
#32645=VECTOR('',#115307,10.);
#32646=VECTOR('',#115310,10.);
#32647=VECTOR('',#115313,10.);
#32648=VECTOR('',#115316,10.);
#32649=VECTOR('',#115319,10.);
#32650=VECTOR('',#115322,10.);
#32651=VECTOR('',#115325,10.);
#32652=VECTOR('',#115328,10.);
#32653=VECTOR('',#115331,10.);
#32654=VECTOR('',#115334,10.);
#32655=VECTOR('',#115337,10.);
#32656=VECTOR('',#115340,10.);
#32657=VECTOR('',#115343,10.);
#32658=VECTOR('',#115356,2.4);
#32659=VECTOR('',#115359,10.);
#32660=VECTOR('',#115362,2.4);
#32661=VECTOR('',#115365,10.);
#32662=VECTOR('',#115370,10.);
#32663=VECTOR('',#115373,10.);
#32664=VECTOR('',#115376,10.);
#32665=VECTOR('',#115379,10.);
#32666=VECTOR('',#115382,10.);
#32667=VECTOR('',#115385,10.);
#32668=VECTOR('',#115388,10.);
#32669=VECTOR('',#115391,10.);
#32670=VECTOR('',#115394,10.);
#32671=VECTOR('',#115397,10.);
#32672=VECTOR('',#115400,10.);
#32673=VECTOR('',#115403,10.);
#32674=VECTOR('',#115406,10.);
#32675=VECTOR('',#115409,10.);
#32676=VECTOR('',#115556,0.4875);
#32677=VECTOR('',#115563,0.5);
#32678=VECTOR('',#115568,0.4875);
#32679=VECTOR('',#115577,0.4875);
#32680=VECTOR('',#115584,0.5);
#32681=VECTOR('',#115589,0.4875);
#32682=VECTOR('',#115598,0.4875);
#32683=VECTOR('',#115605,0.5);
#32684=VECTOR('',#115610,0.4875);
#32685=VECTOR('',#115619,0.4875);
#32686=VECTOR('',#115626,0.5);
#32687=VECTOR('',#115631,0.4875);
#32688=VECTOR('',#115640,0.4875);
#32689=VECTOR('',#115647,0.5);
#32690=VECTOR('',#115652,0.4875);
#32691=VECTOR('',#115661,0.4875);
#32692=VECTOR('',#115668,0.5);
#32693=VECTOR('',#115673,0.4875);
#32694=VECTOR('',#115682,0.4875);
#32695=VECTOR('',#115689,0.5);
#32696=VECTOR('',#115694,0.4875);
#32697=VECTOR('',#115703,0.4875);
#32698=VECTOR('',#115710,0.5);
#32699=VECTOR('',#115715,0.4875);
#32700=VECTOR('',#115726,1.17524047358084);
#32701=VECTOR('',#115731,1.17524047358084);
#32702=VECTOR('',#115734,1.17524047358084);
#32703=VECTOR('',#115737,1.17524047358084);
#32704=VECTOR('',#115740,1.17524047358084);
#32705=VECTOR('',#115743,1.17524047358084);
#32706=VECTOR('',#115746,1.17524047358084);
#32707=VECTOR('',#115749,1.17524047358084);
#32708=VECTOR('',#115752,1.17524047358084);
#32709=VECTOR('',#115755,1.17524047358084);
#32710=VECTOR('',#115758,1.17524047358084);
#32711=VECTOR('',#115761,1.17524047358084);
#32712=VECTOR('',#115764,1.17524047358084);
#32713=VECTOR('',#115767,1.17524047358084);
#32714=VECTOR('',#115770,1.17524047358084);
#32715=VECTOR('',#115773,1.17524047358084);
#32716=VECTOR('',#115776,1.17524047358084);
#32717=VECTOR('',#115779,1.17524047358084);
#32718=VECTOR('',#115782,1.17524047358084);
#32719=VECTOR('',#115785,1.17524047358084);
#32720=VECTOR('',#115788,1.17524047358084);
#32721=VECTOR('',#115791,1.17524047358084);
#32722=VECTOR('',#115794,1.17524047358084);
#32723=VECTOR('',#115797,1.17524047358084);
#32724=VECTOR('',#115800,1.17524047358084);
#32725=VECTOR('',#115803,1.17524047358084);
#32726=VECTOR('',#115806,1.17524047358084);
#32727=VECTOR('',#115809,1.17524047358084);
#32728=VECTOR('',#115812,1.17524047358084);
#32729=VECTOR('',#115815,1.17524047358084);
#32730=VECTOR('',#115818,1.17524047358084);
#32731=VECTOR('',#115821,1.17524047358084);
#32732=VECTOR('',#115826,1.5);
#32733=VECTOR('',#115831,1.5);
#32734=VECTOR('',#115834,1.5);
#32735=VECTOR('',#115837,1.5);
#32736=VECTOR('',#115840,1.5);
#32737=VECTOR('',#115843,1.5);
#32738=VECTOR('',#115846,1.5);
#32739=VECTOR('',#115849,1.5);
#32740=VECTOR('',#115852,1.5);
#32741=VECTOR('',#115855,1.5);
#32742=VECTOR('',#115858,1.5);
#32743=VECTOR('',#115861,1.5);
#32744=VECTOR('',#115864,1.5);
#32745=VECTOR('',#115867,1.5);
#32746=VECTOR('',#115870,1.5);
#32747=VECTOR('',#115873,1.5);
#32748=VECTOR('',#115876,1.5);
#32749=VECTOR('',#115879,1.5);
#32750=VECTOR('',#115882,1.5);
#32751=VECTOR('',#115885,1.5);
#32752=VECTOR('',#115888,1.5);
#32753=VECTOR('',#115891,1.5);
#32754=VECTOR('',#115894,1.5);
#32755=VECTOR('',#115897,1.5);
#32756=VECTOR('',#115900,1.5);
#32757=VECTOR('',#115903,1.5);
#32758=VECTOR('',#115906,1.5);
#32759=VECTOR('',#115909,1.5);
#32760=VECTOR('',#115912,1.5);
#32761=VECTOR('',#115915,1.5);
#32762=VECTOR('',#115918,1.5);
#32763=VECTOR('',#115933,3.5);
#32764=VECTOR('',#115942,1.125);
#32765=VECTOR('',#115977,1000.);
#32766=VECTOR('',#115978,1000.);
#32767=VECTOR('',#115979,1000.);
#32768=VECTOR('',#115980,1000.);
#32769=VECTOR('',#115981,1000.);
#32770=VECTOR('',#115982,1000.);
#32771=VECTOR('',#115985,1000.);
#32772=VECTOR('',#115986,1000.);
#32773=VECTOR('',#115989,1000.);
#32774=VECTOR('',#115992,1000.);
#32775=VECTOR('',#115995,1000.);
#32776=VECTOR('',#115998,1000.);
#32777=VECTOR('',#116043,2.40384615384615);
#32778=VECTOR('',#116056,2.40384615384615);
#32779=VECTOR('',#116061,2.875);
#32780=VECTOR('',#116070,3.);
#32781=VECTOR('',#116073,3.);
#32782=VECTOR('',#116092,1.625);
#32783=VECTOR('',#116101,1.5);
#32784=VECTOR('',#116104,1.5);
#32785=VECTOR('',#116109,2.09615384615385);
#32786=VECTOR('',#116116,2.09615384615385);
#32787=VECTOR('',#116173,2.40384615384615);
#32788=VECTOR('',#116180,2.09615384615385);
#32789=VECTOR('',#116191,2.40384615384615);
#32790=VECTOR('',#116198,2.09615384615385);
#32791=VECTOR('',#116209,1.17524047358091);
#32792=VECTOR('',#116214,1.17524047358091);
#32793=VECTOR('',#116219,1.17524047358091);
#32794=VECTOR('',#116222,1.17524047358091);
#32795=VECTOR('',#116225,1.17524047358091);
#32796=VECTOR('',#116228,1.17524047358091);
#32797=VECTOR('',#116231,1.17524047358091);
#32798=VECTOR('',#116234,1.17524047358091);
#32799=VECTOR('',#116237,1.17524047358091);
#32800=VECTOR('',#116240,1.17524047358091);
#32801=VECTOR('',#116243,1.17524047358091);
#32802=VECTOR('',#116246,1.17524047358091);
#32803=VECTOR('',#116249,1.17524047358091);
#32804=VECTOR('',#116252,1.17524047358091);
#32805=VECTOR('',#116255,1.17524047358091);
#32806=VECTOR('',#116258,1.17524047358091);
#32807=VECTOR('',#116261,1.5);
#32808=VECTOR('',#116266,1.5);
#32809=VECTOR('',#116269,1.5);
#32810=VECTOR('',#116272,1.5);
#32811=VECTOR('',#116275,1.5);
#32812=VECTOR('',#116278,1.5);
#32813=VECTOR('',#116281,1.5);
#32814=VECTOR('',#116284,1.5);
#32815=VECTOR('',#116287,1.5);
#32816=VECTOR('',#116290,1.5);
#32817=VECTOR('',#116293,1.5);
#32818=VECTOR('',#116296,1.5);
#32819=VECTOR('',#116299,1.5);
#32820=VECTOR('',#116302,1.5);
#32821=VECTOR('',#116305,1.5);
#32822=VECTOR('',#116320,3.5);
#32823=VECTOR('',#116327,1.125);
#32824=VECTOR('',#116364,1000.);
#32825=VECTOR('',#116365,1000.);
#32826=VECTOR('',#116366,1000.);
#32827=VECTOR('',#116367,1000.);
#32828=VECTOR('',#116368,1000.);
#32829=VECTOR('',#116369,1000.);
#32830=VECTOR('',#116372,1000.);
#32831=VECTOR('',#116373,1000.);
#32832=VECTOR('',#116376,1000.);
#32833=VECTOR('',#116379,1000.);
#32834=VECTOR('',#116382,1000.);
#32835=VECTOR('',#116385,1000.);
#32836=VECTOR('',#116394,0.957716426222737);
#32837=VECTOR('',#116399,0.957716426222737);
#32838=VECTOR('',#116402,0.957716426222737);
#32839=VECTOR('',#116405,0.957716426222737);
#32840=VECTOR('',#116408,0.957716426222737);
#32841=VECTOR('',#116411,0.957716426222737);
#32842=VECTOR('',#116414,0.957716426222737);
#32843=VECTOR('',#116417,0.957716426222737);
#32844=VECTOR('',#116420,0.957716426222737);
#32845=VECTOR('',#116423,0.957716426222737);
#32846=VECTOR('',#116426,0.957716426222737);
#32847=VECTOR('',#116429,0.957716426222737);
#32848=VECTOR('',#116432,0.957716426222737);
#32849=VECTOR('',#116435,0.957716426222737);
#32850=VECTOR('',#116438,0.957716426222737);
#32851=VECTOR('',#116443,1.25000000000001);
#32852=VECTOR('',#116448,1.25000000000001);
#32853=VECTOR('',#116451,1.25000000000001);
#32854=VECTOR('',#116454,1.25000000000001);
#32855=VECTOR('',#116457,1.25000000000001);
#32856=VECTOR('',#116460,1.25000000000001);
#32857=VECTOR('',#116463,1.25000000000001);
#32858=VECTOR('',#116466,1.25000000000001);
#32859=VECTOR('',#116469,1.25000000000001);
#32860=VECTOR('',#116472,1.25000000000001);
#32861=VECTOR('',#116475,1.25000000000001);
#32862=VECTOR('',#116478,1.25000000000001);
#32863=VECTOR('',#116481,1.25000000000001);
#32864=VECTOR('',#116484,1.25000000000001);
#32865=VECTOR('',#116489,1.25000000000001);
#32866=VECTOR('',#116504,2.5);
#32867=VECTOR('',#116509,2.5);
#32868=VECTOR('',#116540,1000.);
#32869=VECTOR('',#116541,1000.);
#32870=VECTOR('',#116542,1000.);
#32871=VECTOR('',#116543,1000.);
#32872=VECTOR('',#116544,1000.);
#32873=VECTOR('',#116545,1000.);
#32874=VECTOR('',#116548,1000.);
#32875=VECTOR('',#116549,1000.);
#32876=VECTOR('',#116552,1000.);
#32877=VECTOR('',#116555,1000.);
#32878=VECTOR('',#116558,1000.);
#32879=VECTOR('',#116561,1000.);
#32880=VECTOR('',#116572,1.17524047358083);
#32881=VECTOR('',#116577,1.17524047358083);
#32882=VECTOR('',#116580,1.17524047358083);
#32883=VECTOR('',#116583,1.17524047358083);
#32884=VECTOR('',#116586,1.17524047358083);
#32885=VECTOR('',#116589,1.17524047358083);
#32886=VECTOR('',#116592,1.17524047358083);
#32887=VECTOR('',#116595,1.17524047358083);
#32888=VECTOR('',#116598,1.17524047358083);
#32889=VECTOR('',#116601,1.17524047358083);
#32890=VECTOR('',#116604,1.17524047358083);
#32891=VECTOR('',#116607,1.17524047358083);
#32892=VECTOR('',#116610,1.17524047358083);
#32893=VECTOR('',#116613,1.17524047358083);
#32894=VECTOR('',#116616,1.17524047358083);
#32895=VECTOR('',#116619,1.17524047358083);
#32896=VECTOR('',#116622,1.17524047358083);
#32897=VECTOR('',#116625,1.17524047358083);
#32898=VECTOR('',#116628,1.17524047358083);
#32899=VECTOR('',#116631,1.17524047358083);
#32900=VECTOR('',#116634,1.17524047358083);
#32901=VECTOR('',#116637,1.17524047358083);
#32902=VECTOR('',#116640,1.17524047358083);
#32903=VECTOR('',#116643,1.17524047358083);
#32904=VECTOR('',#116646,1.17524047358083);
#32905=VECTOR('',#116649,1.17524047358083);
#32906=VECTOR('',#116652,1.17524047358083);
#32907=VECTOR('',#116655,1.17524047358083);
#32908=VECTOR('',#116658,1.17524047358083);
#32909=VECTOR('',#116661,1.5);
#32910=VECTOR('',#116664,1.5);
#32911=VECTOR('',#116671,1.5);
#32912=VECTOR('',#116674,1.5);
#32913=VECTOR('',#116677,1.5);
#32914=VECTOR('',#116680,1.5);
#32915=VECTOR('',#116683,1.5);
#32916=VECTOR('',#116686,1.5);
#32917=VECTOR('',#116689,1.5);
#32918=VECTOR('',#116692,1.5);
#32919=VECTOR('',#116695,1.5);
#32920=VECTOR('',#116698,1.5);
#32921=VECTOR('',#116701,1.5);
#32922=VECTOR('',#116704,1.5);
#32923=VECTOR('',#116707,1.5);
#32924=VECTOR('',#116710,1.5);
#32925=VECTOR('',#116713,1.5);
#32926=VECTOR('',#116716,1.5);
#32927=VECTOR('',#116719,1.5);
#32928=VECTOR('',#116722,1.5);
#32929=VECTOR('',#116725,1.5);
#32930=VECTOR('',#116728,1.5);
#32931=VECTOR('',#116731,1.5);
#32932=VECTOR('',#116734,1.5);
#32933=VECTOR('',#116737,1.5);
#32934=VECTOR('',#116740,1.5);
#32935=VECTOR('',#116743,1.5);
#32936=VECTOR('',#116746,1.5);
#32937=VECTOR('',#116749,1.5);
#32938=VECTOR('',#116752,999.999999999989);
#32939=VECTOR('',#116757,1.17524047358083);
#32940=VECTOR('',#116778,1.25);
#32941=VECTOR('',#116807,2.54610912703474);
#32942=VECTOR('',#117014,2.73389087296526);
#32943=VECTOR('',#117225,1000.);
#32944=VECTOR('',#117232,1000.);
#32945=VECTOR('',#117235,1000.);
#32946=VECTOR('',#117242,1000.);
#32947=VECTOR('',#117245,1000.);
#32948=VECTOR('',#117252,1000.);
#32949=VECTOR('',#117255,1000.);
#32950=VECTOR('',#117262,1000.);
#32951=VECTOR('',#117265,1000.);
#32952=VECTOR('',#117272,1000.);
#32953=VECTOR('',#117275,1000.);
#32954=VECTOR('',#117282,1000.);
#32955=VECTOR('',#117285,1000.);
#32956=VECTOR('',#117292,1000.);
#32957=VECTOR('',#117295,1000.);
#32958=VECTOR('',#117302,1000.);
#32959=VECTOR('',#117305,1000.);
#32960=VECTOR('',#117312,1000.);
#32961=VECTOR('',#117315,1000.);
#32962=VECTOR('',#117322,1000.);
#32963=VECTOR('',#117325,1000.);
#32964=VECTOR('',#117332,1000.);
#32965=VECTOR('',#117335,1000.);
#32966=VECTOR('',#117342,1000.);
#32967=VECTOR('',#117345,1000.);
#32968=VECTOR('',#117352,1000.);
#32969=VECTOR('',#117355,1000.);
#32970=VECTOR('',#117362,1000.);
#32971=VECTOR('',#117365,1000.);
#32972=VECTOR('',#117372,1000.);
#32973=VECTOR('',#117375,1000.);
#32974=VECTOR('',#117382,1000.);
#32975=VECTOR('',#117385,1000.);
#32976=VECTOR('',#117392,1000.);
#32977=VECTOR('',#117395,1000.);
#32978=VECTOR('',#117402,1000.);
#32979=VECTOR('',#117405,1000.);
#32980=VECTOR('',#117412,1000.);
#32981=VECTOR('',#117415,1000.);
#32982=VECTOR('',#117422,1000.);
#32983=VECTOR('',#117425,1000.);
#32984=VECTOR('',#117432,1000.);
#32985=VECTOR('',#117435,1000.);
#32986=VECTOR('',#117442,1000.);
#32987=VECTOR('',#117445,1000.);
#32988=VECTOR('',#117452,1000.);
#32989=VECTOR('',#117455,1000.);
#32990=VECTOR('',#117462,1000.);
#32991=VECTOR('',#117465,1000.);
#32992=VECTOR('',#117472,1000.);
#32993=VECTOR('',#117475,1000.);
#32994=VECTOR('',#117482,1000.);
#32995=VECTOR('',#117485,1000.);
#32996=VECTOR('',#117492,1000.);
#32997=VECTOR('',#117495,1000.);
#32998=VECTOR('',#117502,1000.);
#32999=VECTOR('',#117505,1000.);
#33000=VECTOR('',#117512,1000.);
#33001=VECTOR('',#117515,1000.);
#33002=VECTOR('',#117522,1000.);
#33003=VECTOR('',#117525,1000.);
#33004=VECTOR('',#117532,1000.);
#33005=VECTOR('',#117535,1000.);
#33006=VECTOR('',#117542,1000.);
#33007=VECTOR('',#117545,1000.);
#33008=VECTOR('',#117552,1000.);
#33009=VECTOR('',#117555,1000.);
#33010=VECTOR('',#117562,1000.);
#33011=VECTOR('',#117565,1000.);
#33012=VECTOR('',#117572,1000.);
#33013=VECTOR('',#117575,1000.);
#33014=VECTOR('',#117582,1000.);
#33015=VECTOR('',#117585,1000.);
#33016=VECTOR('',#117592,1000.);
#33017=VECTOR('',#117595,1000.);
#33018=VECTOR('',#117602,1000.);
#33019=VECTOR('',#117605,1000.);
#33020=VECTOR('',#117612,1000.);
#33021=VECTOR('',#117615,1000.);
#33022=VECTOR('',#117622,1000.);
#33023=VECTOR('',#117625,1000.);
#33024=VECTOR('',#117632,1000.);
#33025=VECTOR('',#117635,1000.);
#33026=VECTOR('',#117642,1000.);
#33027=VECTOR('',#117645,1000.);
#33028=VECTOR('',#117652,1000.);
#33029=VECTOR('',#117655,1000.);
#33030=VECTOR('',#117662,1000.);
#33031=VECTOR('',#117665,1000.);
#33032=VECTOR('',#117672,1000.);
#33033=VECTOR('',#117675,1000.);
#33034=VECTOR('',#117682,1000.);
#33035=VECTOR('',#117685,1000.);
#33036=VECTOR('',#117692,1000.);
#33037=VECTOR('',#117695,1000.);
#33038=VECTOR('',#117702,1000.);
#33039=VECTOR('',#117705,1000.);
#33040=VECTOR('',#117712,1000.);
#33041=VECTOR('',#117715,2.75);
#33042=VECTOR('',#117718,1000.);
#33043=VECTOR('',#117725,1000.);
#33044=VECTOR('',#117728,1000.);
#33045=VECTOR('',#117735,1000.);
#33046=VECTOR('',#117738,1000.);
#33047=VECTOR('',#117745,1000.);
#33048=VECTOR('',#117748,1000.);
#33049=VECTOR('',#117755,1000.);
#33050=VECTOR('',#117758,1000.);
#33051=VECTOR('',#117765,1000.);
#33052=VECTOR('',#117768,1000.);
#33053=VECTOR('',#117775,1000.);
#33054=VECTOR('',#117778,1000.);
#33055=VECTOR('',#117785,1000.);
#33056=VECTOR('',#117788,1000.);
#33057=VECTOR('',#117795,1000.);
#33058=VECTOR('',#117798,1000.);
#33059=VECTOR('',#117805,1000.);
#33060=VECTOR('',#117808,1000.);
#33061=VECTOR('',#117815,1000.);
#33062=VECTOR('',#117818,1000.);
#33063=VECTOR('',#117825,1000.);
#33064=VECTOR('',#117828,1000.);
#33065=VECTOR('',#117835,1000.);
#33066=VECTOR('',#117838,1000.);
#33067=VECTOR('',#117845,1000.);
#33068=VECTOR('',#117848,1000.);
#33069=VECTOR('',#117855,1000.);
#33070=VECTOR('',#117858,1000.);
#33071=VECTOR('',#117865,1000.);
#33072=VECTOR('',#117868,1000.);
#33073=VECTOR('',#117875,1000.);
#33074=VECTOR('',#117878,1000.);
#33075=VECTOR('',#117885,1000.);
#33076=VECTOR('',#117888,1000.);
#33077=VECTOR('',#117895,1000.);
#33078=VECTOR('',#117898,1000.);
#33079=VECTOR('',#117905,1000.);
#33080=VECTOR('',#117908,1000.);
#33081=VECTOR('',#117915,1000.);
#33082=VECTOR('',#117918,1000.);
#33083=VECTOR('',#117925,1000.);
#33084=VECTOR('',#117928,1000.);
#33085=VECTOR('',#117935,1000.);
#33086=VECTOR('',#117938,1000.);
#33087=VECTOR('',#117945,1000.);
#33088=VECTOR('',#117948,1000.);
#33089=VECTOR('',#117955,1000.);
#33090=VECTOR('',#117958,1000.);
#33091=VECTOR('',#117965,1000.);
#33092=VECTOR('',#117968,1000.);
#33093=VECTOR('',#117975,1000.);
#33094=VECTOR('',#117978,1000.);
#33095=VECTOR('',#117985,1000.);
#33096=VECTOR('',#117988,1000.);
#33097=VECTOR('',#117995,1000.);
#33098=VECTOR('',#117998,1000.);
#33099=VECTOR('',#118005,1000.);
#33100=VECTOR('',#118008,1000.);
#33101=VECTOR('',#118015,1000.);
#33102=VECTOR('',#118018,1000.);
#33103=VECTOR('',#118025,1000.);
#33104=VECTOR('',#118028,1000.);
#33105=VECTOR('',#118035,1000.);
#33106=VECTOR('',#118038,1000.);
#33107=VECTOR('',#118045,1000.);
#33108=VECTOR('',#118048,1000.);
#33109=VECTOR('',#118055,1000.);
#33110=VECTOR('',#118058,1000.);
#33111=VECTOR('',#118065,1000.);
#33112=VECTOR('',#118068,1000.);
#33113=VECTOR('',#118075,1000.);
#33114=VECTOR('',#118078,1000.);
#33115=VECTOR('',#118085,1000.);
#33116=VECTOR('',#118088,1000.);
#33117=VECTOR('',#118095,1000.);
#33118=VECTOR('',#118098,1000.);
#33119=VECTOR('',#118105,1000.);
#33120=VECTOR('',#118108,1000.);
#33121=VECTOR('',#118115,1000.);
#33122=VECTOR('',#118118,1000.);
#33123=VECTOR('',#118125,1000.);
#33124=VECTOR('',#118128,1000.);
#33125=VECTOR('',#118135,1000.);
#33126=VECTOR('',#118138,1000.);
#33127=VECTOR('',#118145,1000.);
#33128=VECTOR('',#118148,1000.);
#33129=VECTOR('',#118155,1000.);
#33130=VECTOR('',#118158,1000.);
#33131=VECTOR('',#118165,1000.);
#33132=VECTOR('',#118168,1000.);
#33133=VECTOR('',#118175,1000.);
#33134=VECTOR('',#118178,1000.);
#33135=VECTOR('',#118185,1000.);
#33136=VECTOR('',#118188,1000.);
#33137=VECTOR('',#118195,1000.);
#33138=VECTOR('',#118198,1000.);
#33139=VECTOR('',#118205,1000.);
#33140=VECTOR('',#118790,1000.);
#33141=VECTOR('',#118791,1000.);
#33142=VECTOR('',#118798,1000.);
#33143=VECTOR('',#118803,1000.);
#33144=VECTOR('',#118806,1000.);
#33145=VECTOR('',#118807,1000.);
#33146=VECTOR('',#118810,1000.);
#33147=VECTOR('',#118811,1000.);
#33148=VECTOR('',#118814,1000.);
#33149=VECTOR('',#118815,1000.);
#33150=VECTOR('',#118818,1000.);
#33151=VECTOR('',#118819,1000.);
#33152=VECTOR('',#118822,1000.);
#33153=VECTOR('',#118823,1000.);
#33154=VECTOR('',#118844,1000.);
#33155=VECTOR('',#118845,1000.);
#33156=VECTOR('',#118848,1000.);
#33157=VECTOR('',#118851,1000.);
#33158=VECTOR('',#118854,1000.);
#33159=VECTOR('',#118855,1000.);
#33160=VECTOR('',#118858,1000.);
#33161=VECTOR('',#118859,1000.);
#33162=VECTOR('',#118916,1000.);
#33163=VECTOR('',#118919,1000.);
#33164=VECTOR('',#118924,1000.);
#33165=VECTOR('',#118925,1000.);
#33166=VECTOR('',#118966,1000.);
#33167=VECTOR('',#118969,1000.);
#33168=VECTOR('',#118974,1000.);
#33169=VECTOR('',#118975,1000.);
#33170=VECTOR('',#119016,1000.);
#33171=VECTOR('',#119019,1000.);
#33172=VECTOR('',#119024,1000.);
#33173=VECTOR('',#119025,1000.);
#33174=VECTOR('',#119066,1000.);
#33175=VECTOR('',#119069,1000.);
#33176=VECTOR('',#119074,1000.);
#33177=VECTOR('',#119075,1000.);
#33178=VECTOR('',#119116,1000.);
#33179=VECTOR('',#119119,1000.);
#33180=VECTOR('',#119124,1000.);
#33181=VECTOR('',#119125,1000.);
#33182=VECTOR('',#119166,1000.);
#33183=VECTOR('',#119169,1000.);
#33184=VECTOR('',#119174,1000.);
#33185=VECTOR('',#119175,1000.);
#33186=VECTOR('',#119216,1000.);
#33187=VECTOR('',#119219,1000.);
#33188=VECTOR('',#119224,1000.);
#33189=VECTOR('',#119225,1000.);
#33190=VECTOR('',#119266,1000.);
#33191=VECTOR('',#119269,1000.);
#33192=VECTOR('',#119274,1000.);
#33193=VECTOR('',#119275,1000.);
#33194=VECTOR('',#119316,1000.);
#33195=VECTOR('',#119319,1000.);
#33196=VECTOR('',#119324,1000.);
#33197=VECTOR('',#119325,1000.);
#33198=VECTOR('',#119366,1000.);
#33199=VECTOR('',#119369,1000.);
#33200=VECTOR('',#119374,1000.);
#33201=VECTOR('',#119375,1000.);
#33202=VECTOR('',#119416,1000.);
#33203=VECTOR('',#119419,1000.);
#33204=VECTOR('',#119424,1000.);
#33205=VECTOR('',#119425,1000.);
#33206=VECTOR('',#119466,1000.);
#33207=VECTOR('',#119469,1000.);
#33208=VECTOR('',#119474,1000.);
#33209=VECTOR('',#119475,1000.);
#33210=VECTOR('',#119516,1000.);
#33211=VECTOR('',#119519,1000.);
#33212=VECTOR('',#119524,1000.);
#33213=VECTOR('',#119525,1000.);
#33214=VECTOR('',#119566,1000.);
#33215=VECTOR('',#119569,1000.);
#33216=VECTOR('',#119574,1000.);
#33217=VECTOR('',#119575,1000.);
#33218=VECTOR('',#119616,1000.);
#33219=VECTOR('',#119619,1000.);
#33220=VECTOR('',#119624,1000.);
#33221=VECTOR('',#119625,1000.);
#33222=VECTOR('',#119666,1000.);
#33223=VECTOR('',#119669,1000.);
#33224=VECTOR('',#119674,1000.);
#33225=VECTOR('',#119675,1000.);
#33226=VECTOR('',#119716,1000.);
#33227=VECTOR('',#119719,1000.);
#33228=VECTOR('',#119724,1000.);
#33229=VECTOR('',#119725,1000.);
#33230=VECTOR('',#119766,1000.);
#33231=VECTOR('',#119769,1000.);
#33232=VECTOR('',#119774,1000.);
#33233=VECTOR('',#119775,1000.);
#33234=VECTOR('',#119816,1000.);
#33235=VECTOR('',#119819,1000.);
#33236=VECTOR('',#119824,1000.);
#33237=VECTOR('',#119825,1000.);
#33238=VECTOR('',#119866,1000.);
#33239=VECTOR('',#119869,1000.);
#33240=VECTOR('',#119874,1000.);
#33241=VECTOR('',#119875,1000.);
#33242=VECTOR('',#119916,1000.);
#33243=VECTOR('',#119919,1000.);
#33244=VECTOR('',#119924,1000.);
#33245=VECTOR('',#119925,1000.);
#33246=VECTOR('',#119966,1000.);
#33247=VECTOR('',#119969,1000.);
#33248=VECTOR('',#119974,1000.);
#33249=VECTOR('',#119975,1000.);
#33250=VECTOR('',#120016,1000.);
#33251=VECTOR('',#120019,1000.);
#33252=VECTOR('',#120024,1000.);
#33253=VECTOR('',#120025,1000.);
#33254=VECTOR('',#120066,1000.);
#33255=VECTOR('',#120069,1000.);
#33256=VECTOR('',#120074,1000.);
#33257=VECTOR('',#120075,1000.);
#33258=VECTOR('',#120116,1000.);
#33259=VECTOR('',#120119,1000.);
#33260=VECTOR('',#120124,1000.);
#33261=VECTOR('',#120125,1000.);
#33262=VECTOR('',#120166,1000.);
#33263=VECTOR('',#120169,1000.);
#33264=VECTOR('',#120174,1000.);
#33265=VECTOR('',#120175,1000.);
#33266=VECTOR('',#120216,1000.);
#33267=VECTOR('',#120219,1000.);
#33268=VECTOR('',#120224,1000.);
#33269=VECTOR('',#120225,1000.);
#33270=VECTOR('',#120266,1000.);
#33271=VECTOR('',#120269,1000.);
#33272=VECTOR('',#120274,1000.);
#33273=VECTOR('',#120275,1000.);
#33274=VECTOR('',#120316,1000.);
#33275=VECTOR('',#120319,1000.);
#33276=VECTOR('',#120324,1000.);
#33277=VECTOR('',#120325,1000.);
#33278=VECTOR('',#120366,1000.);
#33279=VECTOR('',#120369,1000.);
#33280=VECTOR('',#120374,1000.);
#33281=VECTOR('',#120375,1000.);
#33282=VECTOR('',#120416,1000.);
#33283=VECTOR('',#120419,1000.);
#33284=VECTOR('',#120424,1000.);
#33285=VECTOR('',#120425,1000.);
#33286=VECTOR('',#120466,1000.);
#33287=VECTOR('',#120469,1000.);
#33288=VECTOR('',#120474,1000.);
#33289=VECTOR('',#120475,1000.);
#33290=VECTOR('',#120516,1000.);
#33291=VECTOR('',#120519,1000.);
#33292=VECTOR('',#120524,1000.);
#33293=VECTOR('',#120525,1000.);
#33294=VECTOR('',#120566,1000.);
#33295=VECTOR('',#120569,1000.);
#33296=VECTOR('',#120574,1000.);
#33297=VECTOR('',#120575,1000.);
#33298=VECTOR('',#120616,1000.);
#33299=VECTOR('',#120619,1000.);
#33300=VECTOR('',#120624,1000.);
#33301=VECTOR('',#120625,1000.);
#33302=VECTOR('',#120666,1000.);
#33303=VECTOR('',#120669,1000.);
#33304=VECTOR('',#120674,1000.);
#33305=VECTOR('',#120675,1000.);
#33306=VECTOR('',#120716,1000.);
#33307=VECTOR('',#120719,1000.);
#33308=VECTOR('',#120724,1000.);
#33309=VECTOR('',#120725,1000.);
#33310=VECTOR('',#120766,1000.);
#33311=VECTOR('',#120769,1000.);
#33312=VECTOR('',#120774,1000.);
#33313=VECTOR('',#120775,1000.);
#33314=VECTOR('',#120816,1000.);
#33315=VECTOR('',#120819,1000.);
#33316=VECTOR('',#120824,1000.);
#33317=VECTOR('',#120825,1000.);
#33318=VECTOR('',#120866,1000.);
#33319=VECTOR('',#120869,1000.);
#33320=VECTOR('',#120874,1000.);
#33321=VECTOR('',#120875,1000.);
#33322=VECTOR('',#120916,1000.);
#33323=VECTOR('',#120919,1000.);
#33324=VECTOR('',#120924,1000.);
#33325=VECTOR('',#120925,1000.);
#33326=VECTOR('',#120966,1000.);
#33327=VECTOR('',#120969,1000.);
#33328=VECTOR('',#120974,1000.);
#33329=VECTOR('',#120975,1000.);
#33330=VECTOR('',#121016,1000.);
#33331=VECTOR('',#121019,1000.);
#33332=VECTOR('',#121024,1000.);
#33333=VECTOR('',#121025,1000.);
#33334=VECTOR('',#121066,1000.);
#33335=VECTOR('',#121069,1000.);
#33336=VECTOR('',#121074,1000.);
#33337=VECTOR('',#121075,1000.);
#33338=VECTOR('',#121116,1000.);
#33339=VECTOR('',#121119,1000.);
#33340=VECTOR('',#121124,1000.);
#33341=VECTOR('',#121125,1000.);
#33342=VECTOR('',#121166,1000.);
#33343=VECTOR('',#121169,1000.);
#33344=VECTOR('',#121174,1000.);
#33345=VECTOR('',#121175,1000.);
#33346=VECTOR('',#121216,1000.);
#33347=VECTOR('',#121219,1000.);
#33348=VECTOR('',#121224,1000.);
#33349=VECTOR('',#121225,1000.);
#33350=VECTOR('',#121266,1000.);
#33351=VECTOR('',#121269,1000.);
#33352=VECTOR('',#121274,1000.);
#33353=VECTOR('',#121275,1000.);
#33354=VECTOR('',#121316,1000.);
#33355=VECTOR('',#121319,1000.);
#33356=VECTOR('',#121324,1000.);
#33357=VECTOR('',#121325,1000.);
#33358=VECTOR('',#121366,1000.);
#33359=VECTOR('',#121369,1000.);
#33360=VECTOR('',#121374,1000.);
#33361=VECTOR('',#121375,1000.);
#33362=VECTOR('',#121416,1000.);
#33363=VECTOR('',#121419,1000.);
#33364=VECTOR('',#121424,1000.);
#33365=VECTOR('',#121425,1000.);
#33366=VECTOR('',#121466,1000.);
#33367=VECTOR('',#121469,1000.);
#33368=VECTOR('',#121474,1000.);
#33369=VECTOR('',#121475,1000.);
#33370=VECTOR('',#121516,1000.);
#33371=VECTOR('',#121519,1000.);
#33372=VECTOR('',#121524,1000.);
#33373=VECTOR('',#121525,1000.);
#33374=VECTOR('',#121566,1000.);
#33375=VECTOR('',#121569,1000.);
#33376=VECTOR('',#121574,1000.);
#33377=VECTOR('',#121575,1000.);
#33378=VECTOR('',#121616,1000.);
#33379=VECTOR('',#121619,1000.);
#33380=VECTOR('',#121624,1000.);
#33381=VECTOR('',#121625,1000.);
#33382=VECTOR('',#121666,1000.);
#33383=VECTOR('',#121669,1000.);
#33384=VECTOR('',#121674,1000.);
#33385=VECTOR('',#121675,1000.);
#33386=VECTOR('',#121716,1000.);
#33387=VECTOR('',#121719,1000.);
#33388=VECTOR('',#121724,1000.);
#33389=VECTOR('',#121725,1000.);
#33390=VECTOR('',#121766,1000.);
#33391=VECTOR('',#121769,1000.);
#33392=VECTOR('',#121774,1000.);
#33393=VECTOR('',#121775,1000.);
#33394=VECTOR('',#121816,1000.);
#33395=VECTOR('',#121819,1000.);
#33396=VECTOR('',#121824,1000.);
#33397=VECTOR('',#121825,1000.);
#33398=VECTOR('',#121866,1000.);
#33399=VECTOR('',#121869,1000.);
#33400=VECTOR('',#121874,1000.);
#33401=VECTOR('',#121875,1000.);
#33402=VECTOR('',#121916,1000.);
#33403=VECTOR('',#121919,1000.);
#33404=VECTOR('',#121924,1000.);
#33405=VECTOR('',#121925,1000.);
#33406=VECTOR('',#121966,1000.);
#33407=VECTOR('',#121969,1000.);
#33408=VECTOR('',#121974,1000.);
#33409=VECTOR('',#121975,1000.);
#33410=VECTOR('',#122016,1000.);
#33411=VECTOR('',#122019,1000.);
#33412=VECTOR('',#122024,1000.);
#33413=VECTOR('',#122025,1000.);
#33414=VECTOR('',#122066,1000.);
#33415=VECTOR('',#122069,1000.);
#33416=VECTOR('',#122074,1000.);
#33417=VECTOR('',#122075,1000.);
#33418=VECTOR('',#122116,1000.);
#33419=VECTOR('',#122119,1000.);
#33420=VECTOR('',#122124,1000.);
#33421=VECTOR('',#122125,1000.);
#33422=VECTOR('',#122166,1000.);
#33423=VECTOR('',#122169,1000.);
#33424=VECTOR('',#122174,1000.);
#33425=VECTOR('',#122175,1000.);
#33426=VECTOR('',#122216,1000.);
#33427=VECTOR('',#122219,1000.);
#33428=VECTOR('',#122224,1000.);
#33429=VECTOR('',#122225,1000.);
#33430=VECTOR('',#122266,1000.);
#33431=VECTOR('',#122269,1000.);
#33432=VECTOR('',#122274,1000.);
#33433=VECTOR('',#122275,1000.);
#33434=VECTOR('',#122316,1000.);
#33435=VECTOR('',#122319,1000.);
#33436=VECTOR('',#122324,1000.);
#33437=VECTOR('',#122325,1000.);
#33438=VECTOR('',#122366,1000.);
#33439=VECTOR('',#122369,1000.);
#33440=VECTOR('',#122374,1000.);
#33441=VECTOR('',#122375,1000.);
#33442=VECTOR('',#122416,1000.);
#33443=VECTOR('',#122419,1000.);
#33444=VECTOR('',#122424,1000.);
#33445=VECTOR('',#122425,1000.);
#33446=VECTOR('',#122466,1000.);
#33447=VECTOR('',#122469,1000.);
#33448=VECTOR('',#122474,1000.);
#33449=VECTOR('',#122475,1000.);
#33450=VECTOR('',#122516,1000.);
#33451=VECTOR('',#122519,1000.);
#33452=VECTOR('',#122524,1000.);
#33453=VECTOR('',#122525,1000.);
#33454=VECTOR('',#122566,1000.);
#33455=VECTOR('',#122569,1000.);
#33456=VECTOR('',#122574,1000.);
#33457=VECTOR('',#122575,1000.);
#33458=VECTOR('',#122616,1000.);
#33459=VECTOR('',#122619,1000.);
#33460=VECTOR('',#122624,1000.);
#33461=VECTOR('',#122625,1000.);
#33462=VECTOR('',#122666,1000.);
#33463=VECTOR('',#122669,1000.);
#33464=VECTOR('',#122674,1000.);
#33465=VECTOR('',#122675,1000.);
#33466=VECTOR('',#122716,1000.);
#33467=VECTOR('',#122719,1000.);
#33468=VECTOR('',#122724,1000.);
#33469=VECTOR('',#122725,1000.);
#33470=VECTOR('',#122766,1000.);
#33471=VECTOR('',#122769,1000.);
#33472=VECTOR('',#122774,1000.);
#33473=VECTOR('',#122775,1000.);
#33474=VECTOR('',#122816,1000.);
#33475=VECTOR('',#122819,1000.);
#33476=VECTOR('',#122824,1000.);
#33477=VECTOR('',#122825,1000.);
#33478=VECTOR('',#122866,1000.);
#33479=VECTOR('',#122869,1000.);
#33480=VECTOR('',#122874,1000.);
#33481=VECTOR('',#122875,1000.);
#33482=VECTOR('',#122916,1000.);
#33483=VECTOR('',#122919,1000.);
#33484=VECTOR('',#122924,1000.);
#33485=VECTOR('',#122925,1000.);
#33486=VECTOR('',#122966,1000.);
#33487=VECTOR('',#122969,1000.);
#33488=VECTOR('',#122974,1000.);
#33489=VECTOR('',#122975,1000.);
#33490=VECTOR('',#123016,1000.);
#33491=VECTOR('',#123019,1000.);
#33492=VECTOR('',#123024,1000.);
#33493=VECTOR('',#123025,1000.);
#33494=VECTOR('',#123066,1000.);
#33495=VECTOR('',#123069,1000.);
#33496=VECTOR('',#123074,1000.);
#33497=VECTOR('',#123075,1000.);
#33498=VECTOR('',#123116,1000.);
#33499=VECTOR('',#123119,1000.);
#33500=VECTOR('',#123124,1000.);
#33501=VECTOR('',#123125,1000.);
#33502=VECTOR('',#123166,1000.);
#33503=VECTOR('',#123169,1000.);
#33504=VECTOR('',#123174,1000.);
#33505=VECTOR('',#123175,1000.);
#33506=VECTOR('',#123216,1000.);
#33507=VECTOR('',#123219,1000.);
#33508=VECTOR('',#123224,1000.);
#33509=VECTOR('',#123225,1000.);
#33510=VECTOR('',#123266,1000.);
#33511=VECTOR('',#123269,1000.);
#33512=VECTOR('',#123274,1000.);
#33513=VECTOR('',#123275,1000.);
#33514=VECTOR('',#123316,1000.);
#33515=VECTOR('',#123319,1000.);
#33516=VECTOR('',#123324,1000.);
#33517=VECTOR('',#123325,1000.);
#33518=VECTOR('',#123366,1000.);
#33519=VECTOR('',#123369,1000.);
#33520=VECTOR('',#123374,1000.);
#33521=VECTOR('',#123375,1000.);
#33522=VECTOR('',#123416,1000.);
#33523=VECTOR('',#123419,1000.);
#33524=VECTOR('',#123424,1000.);
#33525=VECTOR('',#123425,1000.);
#33526=VECTOR('',#123466,1000.);
#33527=VECTOR('',#123469,1000.);
#33528=VECTOR('',#123474,1000.);
#33529=VECTOR('',#123475,1000.);
#33530=VECTOR('',#123516,1000.);
#33531=VECTOR('',#123519,1000.);
#33532=VECTOR('',#123524,1000.);
#33533=VECTOR('',#123525,1000.);
#33534=VECTOR('',#123566,1000.);
#33535=VECTOR('',#123569,1000.);
#33536=VECTOR('',#123574,1000.);
#33537=VECTOR('',#123575,1000.);
#33538=VECTOR('',#123616,1000.);
#33539=VECTOR('',#123619,1000.);
#33540=VECTOR('',#123624,1000.);
#33541=VECTOR('',#123625,1000.);
#33542=VECTOR('',#123666,1000.);
#33543=VECTOR('',#123669,1000.);
#33544=VECTOR('',#123674,1000.);
#33545=VECTOR('',#123675,1000.);
#33546=VECTOR('',#123716,1000.);
#33547=VECTOR('',#123719,1000.);
#33548=VECTOR('',#123724,1000.);
#33549=VECTOR('',#123725,1000.);
#33550=VECTOR('',#123768,1.17524047358089);
#33551=VECTOR('',#123773,1.17524047358089);
#33552=VECTOR('',#123776,1.17524047358089);
#33553=VECTOR('',#123779,1.17524047358089);
#33554=VECTOR('',#123782,1.17524047358089);
#33555=VECTOR('',#123785,1.17524047358089);
#33556=VECTOR('',#123788,1.17524047358089);
#33557=VECTOR('',#123791,1.17524047358089);
#33558=VECTOR('',#123794,1.17524047358089);
#33559=VECTOR('',#123797,1.17524047358089);
#33560=VECTOR('',#123800,1.17524047358089);
#33561=VECTOR('',#123803,1.17524047358089);
#33562=VECTOR('',#123806,1.17524047358089);
#33563=VECTOR('',#123809,1.17524047358089);
#33564=VECTOR('',#123812,1.17524047358089);
#33565=VECTOR('',#123815,1.17524047358089);
#33566=VECTOR('',#123818,1.17524047358089);
#33567=VECTOR('',#123821,1.17524047358089);
#33568=VECTOR('',#123824,1.17524047358089);
#33569=VECTOR('',#123827,1.17524047358089);
#33570=VECTOR('',#123830,1.17524047358089);
#33571=VECTOR('',#123833,1.17524047358089);
#33572=VECTOR('',#123836,1.17524047358089);
#33573=VECTOR('',#123839,1.17524047358089);
#33574=VECTOR('',#123842,1.17524047358089);
#33575=VECTOR('',#123845,1.17524047358089);
#33576=VECTOR('',#123848,1.17524047358089);
#33577=VECTOR('',#123851,1.17524047358089);
#33578=VECTOR('',#123854,1.17524047358089);
#33579=VECTOR('',#123857,1.17524047358089);
#33580=VECTOR('',#123860,1.17524047358089);
#33581=VECTOR('',#123863,1.17524047358089);
#33582=VECTOR('',#123866,1.17524047358089);
#33583=VECTOR('',#123869,1.17524047358089);
#33584=VECTOR('',#123872,1.17524047358089);
#33585=VECTOR('',#123875,1.17524047358089);
#33586=VECTOR('',#123878,999.999999999989);
#33587=VECTOR('',#123883,1.17524047358087);
#33588=VECTOR('',#123888,1.50000000000006);
#33589=VECTOR('',#123893,1.50000000000006);
#33590=VECTOR('',#123896,1.50000000000006);
#33591=VECTOR('',#123899,1.50000000000006);
#33592=VECTOR('',#123902,1.50000000000006);
#33593=VECTOR('',#123905,1.50000000000006);
#33594=VECTOR('',#123908,1.50000000000006);
#33595=VECTOR('',#123911,1.50000000000006);
#33596=VECTOR('',#123914,1.50000000000006);
#33597=VECTOR('',#123917,1.50000000000006);
#33598=VECTOR('',#123920,1.50000000000006);
#33599=VECTOR('',#123923,1.50000000000006);
#33600=VECTOR('',#123926,1.50000000000006);
#33601=VECTOR('',#123929,1.50000000000006);
#33602=VECTOR('',#123932,1.50000000000006);
#33603=VECTOR('',#123935,1.50000000000006);
#33604=VECTOR('',#123938,1.50000000000006);
#33605=VECTOR('',#123941,1.50000000000006);
#33606=VECTOR('',#123944,1.50000000000006);
#33607=VECTOR('',#123947,1.50000000000006);
#33608=VECTOR('',#123950,1.50000000000006);
#33609=VECTOR('',#123953,1.50000000000006);
#33610=VECTOR('',#123956,1.50000000000006);
#33611=VECTOR('',#123959,1.50000000000006);
#33612=VECTOR('',#123962,1.50000000000006);
#33613=VECTOR('',#123965,1.50000000000006);
#33614=VECTOR('',#123968,1.50000000000006);
#33615=VECTOR('',#123971,1.50000000000006);
#33616=VECTOR('',#123974,1.50000000000006);
#33617=VECTOR('',#123977,1.50000000000006);
#33618=VECTOR('',#123980,1.50000000000006);
#33619=VECTOR('',#123983,1.50000000000006);
#33620=VECTOR('',#123986,1.50000000000006);
#33621=VECTOR('',#123989,1.50000000000006);
#33622=VECTOR('',#123994,1.50000000000006);
#33623=VECTOR('',#123997,1.50000000000006);
#33624=VECTOR('',#124780,1.50000000000006);
#33625=VECTOR('',#124785,1.25);
#33626=VECTOR('',#124814,2.55577460325564);
#33627=VECTOR('',#124823,10.);
#33628=VECTOR('',#124826,10.);
#33629=VECTOR('',#124827,10.);
#33630=VECTOR('',#124830,10.);
#33631=VECTOR('',#124831,10.);
#33632=VECTOR('',#124834,10.);
#33633=VECTOR('',#124835,10.);
#33634=VECTOR('',#124838,10.);
#33635=VECTOR('',#124839,10.);
#33636=VECTOR('',#124842,10.);
#33637=VECTOR('',#124843,10.);
#33638=VECTOR('',#124846,10.);
#33639=VECTOR('',#124847,10.);
#33640=VECTOR('',#124850,10.);
#33641=VECTOR('',#124851,10.);
#33642=VECTOR('',#124854,10.);
#33643=VECTOR('',#124855,10.);
#33644=VECTOR('',#124858,10.);
#33645=VECTOR('',#124859,10.);
#33646=VECTOR('',#124862,10.);
#33647=VECTOR('',#124863,10.);
#33648=VECTOR('',#124866,10.);
#33649=VECTOR('',#124867,10.);
#33650=VECTOR('',#124870,10.);
#33651=VECTOR('',#124871,10.);
#33652=VECTOR('',#124874,10.);
#33653=VECTOR('',#124875,10.);
#33654=VECTOR('',#124878,10.);
#33655=VECTOR('',#124879,10.);
#33656=VECTOR('',#124882,10.);
#33657=VECTOR('',#124883,10.);
#33658=VECTOR('',#124886,10.);
#33659=VECTOR('',#124887,10.);
#33660=VECTOR('',#124890,10.);
#33661=VECTOR('',#124891,10.);
#33662=VECTOR('',#124894,10.);
#33663=VECTOR('',#124895,10.);
#33664=VECTOR('',#124898,10.);
#33665=VECTOR('',#124899,10.);
#33666=VECTOR('',#124902,10.);
#33667=VECTOR('',#124903,10.);
#33668=VECTOR('',#124906,10.);
#33669=VECTOR('',#124907,10.);
#33670=VECTOR('',#124910,10.);
#33671=VECTOR('',#124911,10.);
#33672=VECTOR('',#124914,10.);
#33673=VECTOR('',#124915,10.);
#33674=VECTOR('',#124918,10.);
#33675=VECTOR('',#124919,10.);
#33676=VECTOR('',#124922,10.);
#33677=VECTOR('',#124923,10.);
#33678=VECTOR('',#124926,10.);
#33679=VECTOR('',#124927,10.);
#33680=VECTOR('',#124930,10.);
#33681=VECTOR('',#124931,10.);
#33682=VECTOR('',#124934,10.);
#33683=VECTOR('',#124935,10.);
#33684=VECTOR('',#124938,10.);
#33685=VECTOR('',#124939,10.);
#33686=VECTOR('',#124942,10.);
#33687=VECTOR('',#124943,10.);
#33688=VECTOR('',#124946,10.);
#33689=VECTOR('',#124947,10.);
#33690=VECTOR('',#124950,10.);
#33691=VECTOR('',#124951,10.);
#33692=VECTOR('',#124954,10.);
#33693=VECTOR('',#124955,10.);
#33694=VECTOR('',#124958,10.);
#33695=VECTOR('',#124959,10.);
#33696=VECTOR('',#124962,10.);
#33697=VECTOR('',#124963,10.);
#33698=VECTOR('',#124966,10.);
#33699=VECTOR('',#124967,10.);
#33700=VECTOR('',#124970,10.);
#33701=VECTOR('',#124971,10.);
#33702=VECTOR('',#124974,10.);
#33703=VECTOR('',#124975,10.);
#33704=VECTOR('',#124978,2.72422539674441);
#33705=VECTOR('',#124985,10.);
#33706=VECTOR('',#124986,10.);
#33707=VECTOR('',#124989,10.);
#33708=VECTOR('',#124990,10.);
#33709=VECTOR('',#124993,10.);
#33710=VECTOR('',#124994,10.);
#33711=VECTOR('',#124997,10.);
#33712=VECTOR('',#124998,10.);
#33713=VECTOR('',#125001,10.);
#33714=VECTOR('',#125002,10.);
#33715=VECTOR('',#125005,10.);
#33716=VECTOR('',#125006,10.);
#33717=VECTOR('',#125009,10.);
#33718=VECTOR('',#125010,10.);
#33719=VECTOR('',#125013,10.);
#33720=VECTOR('',#125014,10.);
#33721=VECTOR('',#125017,10.);
#33722=VECTOR('',#125018,10.);
#33723=VECTOR('',#125021,10.);
#33724=VECTOR('',#125022,10.);
#33725=VECTOR('',#125025,10.);
#33726=VECTOR('',#125026,10.);
#33727=VECTOR('',#125029,10.);
#33728=VECTOR('',#125030,10.);
#33729=VECTOR('',#125033,10.);
#33730=VECTOR('',#125034,10.);
#33731=VECTOR('',#125037,10.);
#33732=VECTOR('',#125038,10.);
#33733=VECTOR('',#125041,10.);
#33734=VECTOR('',#125042,10.);
#33735=VECTOR('',#125045,10.);
#33736=VECTOR('',#125046,10.);
#33737=VECTOR('',#125049,10.);
#33738=VECTOR('',#125050,10.);
#33739=VECTOR('',#125053,10.);
#33740=VECTOR('',#125054,10.);
#33741=VECTOR('',#125057,10.);
#33742=VECTOR('',#125058,10.);
#33743=VECTOR('',#125061,10.);
#33744=VECTOR('',#125062,10.);
#33745=VECTOR('',#125065,10.);
#33746=VECTOR('',#125066,10.);
#33747=VECTOR('',#125069,10.);
#33748=VECTOR('',#125070,10.);
#33749=VECTOR('',#125073,10.);
#33750=VECTOR('',#125074,10.);
#33751=VECTOR('',#125077,10.);
#33752=VECTOR('',#125078,10.);
#33753=VECTOR('',#125081,10.);
#33754=VECTOR('',#125082,10.);
#33755=VECTOR('',#125085,10.);
#33756=VECTOR('',#125086,10.);
#33757=VECTOR('',#125089,10.);
#33758=VECTOR('',#125090,10.);
#33759=VECTOR('',#125093,10.);
#33760=VECTOR('',#125094,10.);
#33761=VECTOR('',#125097,10.);
#33762=VECTOR('',#125098,10.);
#33763=VECTOR('',#125101,10.);
#33764=VECTOR('',#125102,10.);
#33765=VECTOR('',#125105,10.);
#33766=VECTOR('',#125106,10.);
#33767=VECTOR('',#125109,10.);
#33768=VECTOR('',#125110,10.);
#33769=VECTOR('',#125113,10.);
#33770=VECTOR('',#125114,10.);
#33771=VECTOR('',#125117,10.);
#33772=VECTOR('',#125118,10.);
#33773=VECTOR('',#125121,10.);
#33774=VECTOR('',#125122,10.);
#33775=VECTOR('',#125125,10.);
#33776=VECTOR('',#125126,10.);
#33777=VECTOR('',#125129,10.);
#33778=VECTOR('',#125130,10.);
#33779=VECTOR('',#125133,10.);
#33780=VECTOR('',#125134,10.);
#33781=VECTOR('',#125137,10.);
#33782=VECTOR('',#125148,1000.);
#33783=VECTOR('',#125149,1000.);
#33784=VECTOR('',#125152,1000.);
#33785=VECTOR('',#125153,1000.);
#33786=VECTOR('',#125156,1000.);
#33787=VECTOR('',#125157,1000.);
#33788=VECTOR('',#125160,1000.);
#33789=VECTOR('',#125161,1000.);
#33790=VECTOR('',#125164,1000.);
#33791=VECTOR('',#125165,1000.);
#33792=VECTOR('',#125168,1000.);
#33793=VECTOR('',#125169,1000.);
#33794=VECTOR('',#125172,1000.);
#33795=VECTOR('',#125173,1000.);
#33796=VECTOR('',#125176,1000.);
#33797=VECTOR('',#125177,1000.);
#33798=VECTOR('',#125180,1000.);
#33799=VECTOR('',#125181,1000.);
#33800=VECTOR('',#125184,1000.);
#33801=VECTOR('',#125185,1000.);
#33802=VECTOR('',#125188,1000.);
#33803=VECTOR('',#125189,1000.);
#33804=VECTOR('',#125192,1000.);
#33805=VECTOR('',#125193,1000.);
#33806=VECTOR('',#125196,1000.);
#33807=VECTOR('',#125197,1000.);
#33808=VECTOR('',#125200,1000.);
#33809=VECTOR('',#125201,1000.);
#33810=VECTOR('',#125204,1000.);
#33811=VECTOR('',#125205,1000.);
#33812=VECTOR('',#125208,1000.);
#33813=VECTOR('',#125209,1000.);
#33814=VECTOR('',#125212,1000.);
#33815=VECTOR('',#125213,1000.);
#33816=VECTOR('',#125216,1000.);
#33817=VECTOR('',#125217,1000.);
#33818=VECTOR('',#125220,1000.);
#33819=VECTOR('',#125221,1000.);
#33820=VECTOR('',#125224,1000.);
#33821=VECTOR('',#125225,1000.);
#33822=VECTOR('',#125228,1000.);
#33823=VECTOR('',#125229,1000.);
#33824=VECTOR('',#125232,1000.);
#33825=VECTOR('',#125233,1000.);
#33826=VECTOR('',#125236,1000.);
#33827=VECTOR('',#125237,1000.);
#33828=VECTOR('',#125240,1000.);
#33829=VECTOR('',#125241,1000.);
#33830=VECTOR('',#125244,1000.);
#33831=VECTOR('',#125245,1000.);
#33832=VECTOR('',#125248,1000.);
#33833=VECTOR('',#125249,1000.);
#33834=VECTOR('',#125252,1000.);
#33835=VECTOR('',#125253,1000.);
#33836=VECTOR('',#125256,1000.);
#33837=VECTOR('',#125257,1000.);
#33838=VECTOR('',#125260,1000.);
#33839=VECTOR('',#125261,1000.);
#33840=VECTOR('',#125264,1000.);
#33841=VECTOR('',#125265,1000.);
#33842=VECTOR('',#125268,1000.);
#33843=VECTOR('',#125269,1000.);
#33844=VECTOR('',#125272,1000.);
#33845=VECTOR('',#125273,1000.);
#33846=VECTOR('',#125276,1000.);
#33847=VECTOR('',#125277,1000.);
#33848=VECTOR('',#125280,1000.);
#33849=VECTOR('',#125281,1000.);
#33850=VECTOR('',#125284,1000.);
#33851=VECTOR('',#125285,1000.);
#33852=VECTOR('',#125288,1000.);
#33853=VECTOR('',#125289,1000.);
#33854=VECTOR('',#125292,1000.);
#33855=VECTOR('',#125293,1000.);
#33856=VECTOR('',#125296,1000.);
#33857=VECTOR('',#125297,1000.);
#33858=VECTOR('',#125300,1000.);
#33859=VECTOR('',#125301,2.75);
#33860=VECTOR('',#125302,1000.);
#33861=VECTOR('',#125305,1000.);
#33862=VECTOR('',#125306,1000.);
#33863=VECTOR('',#125309,1000.);
#33864=VECTOR('',#125310,1000.);
#33865=VECTOR('',#125313,1000.);
#33866=VECTOR('',#125314,1000.);
#33867=VECTOR('',#125317,1000.);
#33868=VECTOR('',#125318,1000.);
#33869=VECTOR('',#125321,1000.);
#33870=VECTOR('',#125322,1000.);
#33871=VECTOR('',#125325,1000.);
#33872=VECTOR('',#125326,1000.);
#33873=VECTOR('',#125329,1000.);
#33874=VECTOR('',#125330,1000.);
#33875=VECTOR('',#125333,1000.);
#33876=VECTOR('',#125334,1000.);
#33877=VECTOR('',#125337,1000.);
#33878=VECTOR('',#125338,1000.);
#33879=VECTOR('',#125341,1000.);
#33880=VECTOR('',#125342,1000.);
#33881=VECTOR('',#125345,1000.);
#33882=VECTOR('',#125346,1000.);
#33883=VECTOR('',#125349,1000.);
#33884=VECTOR('',#125350,1000.);
#33885=VECTOR('',#125353,1000.);
#33886=VECTOR('',#125354,1000.);
#33887=VECTOR('',#125357,1000.);
#33888=VECTOR('',#125358,1000.);
#33889=VECTOR('',#125361,1000.);
#33890=VECTOR('',#125362,1000.);
#33891=VECTOR('',#125365,1000.);
#33892=VECTOR('',#125366,1000.);
#33893=VECTOR('',#125369,1000.);
#33894=VECTOR('',#125370,1000.);
#33895=VECTOR('',#125373,1000.);
#33896=VECTOR('',#125374,1000.);
#33897=VECTOR('',#125377,1000.);
#33898=VECTOR('',#125378,1000.);
#33899=VECTOR('',#125381,1000.);
#33900=VECTOR('',#125382,1000.);
#33901=VECTOR('',#125385,1000.);
#33902=VECTOR('',#125386,1000.);
#33903=VECTOR('',#125389,1000.);
#33904=VECTOR('',#125390,1000.);
#33905=VECTOR('',#125393,1000.);
#33906=VECTOR('',#125394,1000.);
#33907=VECTOR('',#125397,1000.);
#33908=VECTOR('',#125398,1000.);
#33909=VECTOR('',#125401,1000.);
#33910=VECTOR('',#125402,1000.);
#33911=VECTOR('',#125405,1000.);
#33912=VECTOR('',#125406,1000.);
#33913=VECTOR('',#125409,1000.);
#33914=VECTOR('',#125410,1000.);
#33915=VECTOR('',#125413,1000.);
#33916=VECTOR('',#125414,1000.);
#33917=VECTOR('',#125417,1000.);
#33918=VECTOR('',#125418,1000.);
#33919=VECTOR('',#125421,1000.);
#33920=VECTOR('',#125422,1000.);
#33921=VECTOR('',#125425,1000.);
#33922=VECTOR('',#125426,1000.);
#33923=VECTOR('',#125429,1000.);
#33924=VECTOR('',#125430,1000.);
#33925=VECTOR('',#125433,1000.);
#33926=VECTOR('',#125434,1000.);
#33927=VECTOR('',#125437,1000.);
#33928=VECTOR('',#125438,1000.);
#33929=VECTOR('',#125441,1000.);
#33930=VECTOR('',#125442,1000.);
#33931=VECTOR('',#125445,1000.);
#33932=VECTOR('',#125446,1000.);
#33933=VECTOR('',#125449,1000.);
#33934=VECTOR('',#125450,1000.);
#33935=VECTOR('',#125453,1000.);
#33936=VECTOR('',#125454,1000.);
#33937=VECTOR('',#125913,1000.);
#33938=VECTOR('',#125914,1000.);
#33939=VECTOR('',#125923,10.);
#33940=VECTOR('',#125924,1000.);
#33941=VECTOR('',#125927,10.);
#33942=VECTOR('',#125930,1000.);
#33943=VECTOR('',#125935,1000.);
#33944=VECTOR('',#125936,1000.);
#33945=VECTOR('',#125939,1000.);
#33946=VECTOR('',#125940,1000.);
#33947=VECTOR('',#125943,1000.);
#33948=VECTOR('',#125944,1000.);
#33949=VECTOR('',#125947,1000.);
#33950=VECTOR('',#125948,1000.);
#33951=VECTOR('',#125951,1000.);
#33952=VECTOR('',#125952,1000.);
#33953=VECTOR('',#125973,1000.);
#33954=VECTOR('',#125974,1000.);
#33955=VECTOR('',#125975,1000.);
#33956=VECTOR('',#125978,1000.);
#33957=VECTOR('',#125981,1000.);
#33958=VECTOR('',#125984,1000.);
#33959=VECTOR('',#125987,1000.);
#33960=VECTOR('',#125990,1000.);
#33961=VECTOR('',#126037,1000.);
#33962=VECTOR('',#126038,10.);
#33963=VECTOR('',#126041,1000.);
#33964=VECTOR('',#126046,10.);
#33965=VECTOR('',#126047,1000.);
#33966=VECTOR('',#126048,1000.);
#33967=VECTOR('',#126085,1000.);
#33968=VECTOR('',#126086,10.);
#33969=VECTOR('',#126089,1000.);
#33970=VECTOR('',#126094,10.);
#33971=VECTOR('',#126095,1000.);
#33972=VECTOR('',#126096,1000.);
#33973=VECTOR('',#126133,1000.);
#33974=VECTOR('',#126134,10.);
#33975=VECTOR('',#126137,1000.);
#33976=VECTOR('',#126142,10.);
#33977=VECTOR('',#126143,1000.);
#33978=VECTOR('',#126144,1000.);
#33979=VECTOR('',#126181,1000.);
#33980=VECTOR('',#126182,10.);
#33981=VECTOR('',#126185,1000.);
#33982=VECTOR('',#126190,10.);
#33983=VECTOR('',#126191,1000.);
#33984=VECTOR('',#126192,1000.);
#33985=VECTOR('',#126229,1000.);
#33986=VECTOR('',#126230,10.);
#33987=VECTOR('',#126233,1000.);
#33988=VECTOR('',#126238,10.);
#33989=VECTOR('',#126239,1000.);
#33990=VECTOR('',#126240,1000.);
#33991=VECTOR('',#126277,1000.);
#33992=VECTOR('',#126278,10.);
#33993=VECTOR('',#126281,1000.);
#33994=VECTOR('',#126286,10.);
#33995=VECTOR('',#126287,1000.);
#33996=VECTOR('',#126288,1000.);
#33997=VECTOR('',#126325,1000.);
#33998=VECTOR('',#126326,10.);
#33999=VECTOR('',#126329,1000.);
#34000=VECTOR('',#126334,10.);
#34001=VECTOR('',#126335,1000.);
#34002=VECTOR('',#126336,1000.);
#34003=VECTOR('',#126373,1000.);
#34004=VECTOR('',#126374,10.);
#34005=VECTOR('',#126377,1000.);
#34006=VECTOR('',#126382,10.);
#34007=VECTOR('',#126383,1000.);
#34008=VECTOR('',#126384,1000.);
#34009=VECTOR('',#126421,1000.);
#34010=VECTOR('',#126422,10.);
#34011=VECTOR('',#126425,1000.);
#34012=VECTOR('',#126430,10.);
#34013=VECTOR('',#126431,1000.);
#34014=VECTOR('',#126432,1000.);
#34015=VECTOR('',#126469,1000.);
#34016=VECTOR('',#126470,10.);
#34017=VECTOR('',#126473,1000.);
#34018=VECTOR('',#126478,10.);
#34019=VECTOR('',#126479,1000.);
#34020=VECTOR('',#126480,1000.);
#34021=VECTOR('',#126517,1000.);
#34022=VECTOR('',#126518,10.);
#34023=VECTOR('',#126521,1000.);
#34024=VECTOR('',#126526,10.);
#34025=VECTOR('',#126527,1000.);
#34026=VECTOR('',#126528,1000.);
#34027=VECTOR('',#126565,1000.);
#34028=VECTOR('',#126566,10.);
#34029=VECTOR('',#126569,1000.);
#34030=VECTOR('',#126574,10.);
#34031=VECTOR('',#126575,1000.);
#34032=VECTOR('',#126576,1000.);
#34033=VECTOR('',#126613,1000.);
#34034=VECTOR('',#126614,10.);
#34035=VECTOR('',#126617,1000.);
#34036=VECTOR('',#126622,10.);
#34037=VECTOR('',#126623,1000.);
#34038=VECTOR('',#126624,1000.);
#34039=VECTOR('',#126661,1000.);
#34040=VECTOR('',#126662,10.);
#34041=VECTOR('',#126665,1000.);
#34042=VECTOR('',#126670,10.);
#34043=VECTOR('',#126671,1000.);
#34044=VECTOR('',#126672,1000.);
#34045=VECTOR('',#126709,1000.);
#34046=VECTOR('',#126710,10.);
#34047=VECTOR('',#126713,1000.);
#34048=VECTOR('',#126718,10.);
#34049=VECTOR('',#126719,1000.);
#34050=VECTOR('',#126720,1000.);
#34051=VECTOR('',#126757,1000.);
#34052=VECTOR('',#126758,10.);
#34053=VECTOR('',#126761,1000.);
#34054=VECTOR('',#126766,10.);
#34055=VECTOR('',#126767,1000.);
#34056=VECTOR('',#126768,1000.);
#34057=VECTOR('',#126805,1000.);
#34058=VECTOR('',#126806,10.);
#34059=VECTOR('',#126809,1000.);
#34060=VECTOR('',#126814,10.);
#34061=VECTOR('',#126815,1000.);
#34062=VECTOR('',#126816,1000.);
#34063=VECTOR('',#126853,1000.);
#34064=VECTOR('',#126854,10.);
#34065=VECTOR('',#126857,1000.);
#34066=VECTOR('',#126862,10.);
#34067=VECTOR('',#126863,1000.);
#34068=VECTOR('',#126864,1000.);
#34069=VECTOR('',#126901,1000.);
#34070=VECTOR('',#126902,10.);
#34071=VECTOR('',#126905,1000.);
#34072=VECTOR('',#126910,10.);
#34073=VECTOR('',#126911,1000.);
#34074=VECTOR('',#126912,1000.);
#34075=VECTOR('',#126949,1000.);
#34076=VECTOR('',#126950,10.);
#34077=VECTOR('',#126953,1000.);
#34078=VECTOR('',#126958,10.);
#34079=VECTOR('',#126959,1000.);
#34080=VECTOR('',#126960,1000.);
#34081=VECTOR('',#126997,1000.);
#34082=VECTOR('',#126998,10.);
#34083=VECTOR('',#127001,1000.);
#34084=VECTOR('',#127006,10.);
#34085=VECTOR('',#127007,1000.);
#34086=VECTOR('',#127008,1000.);
#34087=VECTOR('',#127045,1000.);
#34088=VECTOR('',#127046,10.);
#34089=VECTOR('',#127049,1000.);
#34090=VECTOR('',#127054,10.);
#34091=VECTOR('',#127055,1000.);
#34092=VECTOR('',#127056,1000.);
#34093=VECTOR('',#127093,1000.);
#34094=VECTOR('',#127094,10.);
#34095=VECTOR('',#127097,1000.);
#34096=VECTOR('',#127102,10.);
#34097=VECTOR('',#127103,1000.);
#34098=VECTOR('',#127104,1000.);
#34099=VECTOR('',#127141,1000.);
#34100=VECTOR('',#127142,10.);
#34101=VECTOR('',#127145,1000.);
#34102=VECTOR('',#127150,10.);
#34103=VECTOR('',#127151,1000.);
#34104=VECTOR('',#127152,1000.);
#34105=VECTOR('',#127189,1000.);
#34106=VECTOR('',#127190,10.);
#34107=VECTOR('',#127193,1000.);
#34108=VECTOR('',#127198,10.);
#34109=VECTOR('',#127199,1000.);
#34110=VECTOR('',#127200,1000.);
#34111=VECTOR('',#127237,1000.);
#34112=VECTOR('',#127238,10.);
#34113=VECTOR('',#127241,1000.);
#34114=VECTOR('',#127246,10.);
#34115=VECTOR('',#127247,1000.);
#34116=VECTOR('',#127248,1000.);
#34117=VECTOR('',#127285,1000.);
#34118=VECTOR('',#127286,10.);
#34119=VECTOR('',#127289,1000.);
#34120=VECTOR('',#127294,10.);
#34121=VECTOR('',#127295,1000.);
#34122=VECTOR('',#127296,1000.);
#34123=VECTOR('',#127333,1000.);
#34124=VECTOR('',#127334,10.);
#34125=VECTOR('',#127337,1000.);
#34126=VECTOR('',#127342,10.);
#34127=VECTOR('',#127343,1000.);
#34128=VECTOR('',#127344,1000.);
#34129=VECTOR('',#127381,1000.);
#34130=VECTOR('',#127382,10.);
#34131=VECTOR('',#127385,1000.);
#34132=VECTOR('',#127390,10.);
#34133=VECTOR('',#127391,1000.);
#34134=VECTOR('',#127392,1000.);
#34135=VECTOR('',#127429,1000.);
#34136=VECTOR('',#127430,10.);
#34137=VECTOR('',#127433,1000.);
#34138=VECTOR('',#127438,10.);
#34139=VECTOR('',#127439,1000.);
#34140=VECTOR('',#127440,1000.);
#34141=VECTOR('',#127477,1000.);
#34142=VECTOR('',#127478,10.);
#34143=VECTOR('',#127481,1000.);
#34144=VECTOR('',#127486,10.);
#34145=VECTOR('',#127487,1000.);
#34146=VECTOR('',#127488,1000.);
#34147=VECTOR('',#127525,1000.);
#34148=VECTOR('',#127526,10.);
#34149=VECTOR('',#127529,1000.);
#34150=VECTOR('',#127534,10.);
#34151=VECTOR('',#127535,1000.);
#34152=VECTOR('',#127536,1000.);
#34153=VECTOR('',#127573,1000.);
#34154=VECTOR('',#127574,10.);
#34155=VECTOR('',#127577,1000.);
#34156=VECTOR('',#127582,10.);
#34157=VECTOR('',#127583,1000.);
#34158=VECTOR('',#127584,1000.);
#34159=VECTOR('',#127621,1000.);
#34160=VECTOR('',#127622,10.);
#34161=VECTOR('',#127625,1000.);
#34162=VECTOR('',#127630,10.);
#34163=VECTOR('',#127631,1000.);
#34164=VECTOR('',#127632,1000.);
#34165=VECTOR('',#127669,1000.);
#34166=VECTOR('',#127670,10.);
#34167=VECTOR('',#127673,1000.);
#34168=VECTOR('',#127678,10.);
#34169=VECTOR('',#127679,1000.);
#34170=VECTOR('',#127680,1000.);
#34171=VECTOR('',#127717,1000.);
#34172=VECTOR('',#127718,10.);
#34173=VECTOR('',#127721,1000.);
#34174=VECTOR('',#127726,10.);
#34175=VECTOR('',#127727,1000.);
#34176=VECTOR('',#127728,1000.);
#34177=VECTOR('',#127765,1000.);
#34178=VECTOR('',#127766,10.);
#34179=VECTOR('',#127769,1000.);
#34180=VECTOR('',#127774,10.);
#34181=VECTOR('',#127775,1000.);
#34182=VECTOR('',#127776,1000.);
#34183=VECTOR('',#127813,1000.);
#34184=VECTOR('',#127814,10.);
#34185=VECTOR('',#127817,1000.);
#34186=VECTOR('',#127822,10.);
#34187=VECTOR('',#127823,1000.);
#34188=VECTOR('',#127824,1000.);
#34189=VECTOR('',#127861,1000.);
#34190=VECTOR('',#127862,10.);
#34191=VECTOR('',#127865,1000.);
#34192=VECTOR('',#127870,10.);
#34193=VECTOR('',#127871,1000.);
#34194=VECTOR('',#127872,1000.);
#34195=VECTOR('',#127909,1000.);
#34196=VECTOR('',#127910,10.);
#34197=VECTOR('',#127913,1000.);
#34198=VECTOR('',#127918,10.);
#34199=VECTOR('',#127919,1000.);
#34200=VECTOR('',#127920,1000.);
#34201=VECTOR('',#127957,1000.);
#34202=VECTOR('',#127958,10.);
#34203=VECTOR('',#127961,1000.);
#34204=VECTOR('',#127966,10.);
#34205=VECTOR('',#127967,1000.);
#34206=VECTOR('',#127968,1000.);
#34207=VECTOR('',#128005,1000.);
#34208=VECTOR('',#128006,10.);
#34209=VECTOR('',#128009,1000.);
#34210=VECTOR('',#128014,10.);
#34211=VECTOR('',#128015,1000.);
#34212=VECTOR('',#128016,1000.);
#34213=VECTOR('',#128053,1000.);
#34214=VECTOR('',#128054,10.);
#34215=VECTOR('',#128057,1000.);
#34216=VECTOR('',#128062,10.);
#34217=VECTOR('',#128063,1000.);
#34218=VECTOR('',#128064,1000.);
#34219=VECTOR('',#128101,1000.);
#34220=VECTOR('',#128102,10.);
#34221=VECTOR('',#128105,1000.);
#34222=VECTOR('',#128110,10.);
#34223=VECTOR('',#128111,1000.);
#34224=VECTOR('',#128112,1000.);
#34225=VECTOR('',#128149,1000.);
#34226=VECTOR('',#128150,10.);
#34227=VECTOR('',#128153,1000.);
#34228=VECTOR('',#128158,10.);
#34229=VECTOR('',#128159,1000.);
#34230=VECTOR('',#128160,1000.);
#34231=VECTOR('',#128197,1000.);
#34232=VECTOR('',#128198,10.);
#34233=VECTOR('',#128201,1000.);
#34234=VECTOR('',#128206,10.);
#34235=VECTOR('',#128207,1000.);
#34236=VECTOR('',#128208,1000.);
#34237=VECTOR('',#128245,1000.);
#34238=VECTOR('',#128246,10.);
#34239=VECTOR('',#128249,1000.);
#34240=VECTOR('',#128254,10.);
#34241=VECTOR('',#128255,1000.);
#34242=VECTOR('',#128256,1000.);
#34243=VECTOR('',#128293,1000.);
#34244=VECTOR('',#128294,10.);
#34245=VECTOR('',#128297,1000.);
#34246=VECTOR('',#128302,10.);
#34247=VECTOR('',#128303,1000.);
#34248=VECTOR('',#128304,1000.);
#34249=VECTOR('',#128341,1000.);
#34250=VECTOR('',#128342,10.);
#34251=VECTOR('',#128345,1000.);
#34252=VECTOR('',#128350,10.);
#34253=VECTOR('',#128351,1000.);
#34254=VECTOR('',#128352,1000.);
#34255=VECTOR('',#128389,1000.);
#34256=VECTOR('',#128390,10.);
#34257=VECTOR('',#128393,1000.);
#34258=VECTOR('',#128398,10.);
#34259=VECTOR('',#128399,1000.);
#34260=VECTOR('',#128400,1000.);
#34261=VECTOR('',#128437,1000.);
#34262=VECTOR('',#128438,10.);
#34263=VECTOR('',#128441,1000.);
#34264=VECTOR('',#128446,10.);
#34265=VECTOR('',#128447,1000.);
#34266=VECTOR('',#128448,1000.);
#34267=VECTOR('',#128485,1000.);
#34268=VECTOR('',#128486,10.);
#34269=VECTOR('',#128489,1000.);
#34270=VECTOR('',#128494,10.);
#34271=VECTOR('',#128495,1000.);
#34272=VECTOR('',#128496,1000.);
#34273=VECTOR('',#128533,1000.);
#34274=VECTOR('',#128534,10.);
#34275=VECTOR('',#128537,1000.);
#34276=VECTOR('',#128542,10.);
#34277=VECTOR('',#128543,1000.);
#34278=VECTOR('',#128544,1000.);
#34279=VECTOR('',#128581,1000.);
#34280=VECTOR('',#128582,10.);
#34281=VECTOR('',#128585,1000.);
#34282=VECTOR('',#128590,10.);
#34283=VECTOR('',#128591,1000.);
#34284=VECTOR('',#128592,1000.);
#34285=VECTOR('',#128629,1000.);
#34286=VECTOR('',#128630,10.);
#34287=VECTOR('',#128633,1000.);
#34288=VECTOR('',#128638,10.);
#34289=VECTOR('',#128639,1000.);
#34290=VECTOR('',#128640,1000.);
#34291=VECTOR('',#128677,1000.);
#34292=VECTOR('',#128678,10.);
#34293=VECTOR('',#128681,1000.);
#34294=VECTOR('',#128686,10.);
#34295=VECTOR('',#128687,1000.);
#34296=VECTOR('',#128688,1000.);
#34297=VECTOR('',#128725,1000.);
#34298=VECTOR('',#128726,10.);
#34299=VECTOR('',#128729,1000.);
#34300=VECTOR('',#128734,10.);
#34301=VECTOR('',#128735,1000.);
#34302=VECTOR('',#128736,1000.);
#34303=VECTOR('',#128773,1000.);
#34304=VECTOR('',#128774,10.);
#34305=VECTOR('',#128777,1000.);
#34306=VECTOR('',#128782,10.);
#34307=VECTOR('',#128783,1000.);
#34308=VECTOR('',#128784,1000.);
#34309=VECTOR('',#128821,1000.);
#34310=VECTOR('',#128822,10.);
#34311=VECTOR('',#128825,1000.);
#34312=VECTOR('',#128830,10.);
#34313=VECTOR('',#128831,1000.);
#34314=VECTOR('',#128832,1000.);
#34315=VECTOR('',#128869,1000.);
#34316=VECTOR('',#128870,10.);
#34317=VECTOR('',#128873,1000.);
#34318=VECTOR('',#128878,10.);
#34319=VECTOR('',#128879,1000.);
#34320=VECTOR('',#128880,1000.);
#34321=VECTOR('',#128917,1000.);
#34322=VECTOR('',#128918,10.);
#34323=VECTOR('',#128921,1000.);
#34324=VECTOR('',#128926,10.);
#34325=VECTOR('',#128927,1000.);
#34326=VECTOR('',#128928,1000.);
#34327=VECTOR('',#128965,1000.);
#34328=VECTOR('',#128966,10.);
#34329=VECTOR('',#128969,1000.);
#34330=VECTOR('',#128974,10.);
#34331=VECTOR('',#128975,1000.);
#34332=VECTOR('',#128976,1000.);
#34333=VECTOR('',#129013,1000.);
#34334=VECTOR('',#129014,10.);
#34335=VECTOR('',#129017,1000.);
#34336=VECTOR('',#129022,10.);
#34337=VECTOR('',#129023,1000.);
#34338=VECTOR('',#129024,1000.);
#34339=VECTOR('',#129061,1000.);
#34340=VECTOR('',#129062,10.);
#34341=VECTOR('',#129065,1000.);
#34342=VECTOR('',#129070,10.);
#34343=VECTOR('',#129071,1000.);
#34344=VECTOR('',#129072,1000.);
#34345=VECTOR('',#129109,1000.);
#34346=VECTOR('',#129110,10.);
#34347=VECTOR('',#129113,1000.);
#34348=VECTOR('',#129118,10.);
#34349=VECTOR('',#129119,1000.);
#34350=VECTOR('',#129120,1000.);
#34351=VECTOR('',#129157,1000.);
#34352=VECTOR('',#129158,10.);
#34353=VECTOR('',#129161,1000.);
#34354=VECTOR('',#129166,10.);
#34355=VECTOR('',#129167,1000.);
#34356=VECTOR('',#129168,1000.);
#34357=VECTOR('',#129205,1000.);
#34358=VECTOR('',#129206,10.);
#34359=VECTOR('',#129209,1000.);
#34360=VECTOR('',#129214,10.);
#34361=VECTOR('',#129215,1000.);
#34362=VECTOR('',#129216,1000.);
#34363=VECTOR('',#129253,1000.);
#34364=VECTOR('',#129254,10.);
#34365=VECTOR('',#129257,1000.);
#34366=VECTOR('',#129262,10.);
#34367=VECTOR('',#129263,1000.);
#34368=VECTOR('',#129264,1000.);
#34369=VECTOR('',#129301,1000.);
#34370=VECTOR('',#129302,10.);
#34371=VECTOR('',#129305,1000.);
#34372=VECTOR('',#129310,10.);
#34373=VECTOR('',#129311,1000.);
#34374=VECTOR('',#129312,1000.);
#34375=VECTOR('',#129349,1000.);
#34376=VECTOR('',#129350,10.);
#34377=VECTOR('',#129353,1000.);
#34378=VECTOR('',#129358,10.);
#34379=VECTOR('',#129359,1000.);
#34380=VECTOR('',#129360,1000.);
#34381=VECTOR('',#129397,1000.);
#34382=VECTOR('',#129398,10.);
#34383=VECTOR('',#129401,1000.);
#34384=VECTOR('',#129406,10.);
#34385=VECTOR('',#129407,1000.);
#34386=VECTOR('',#129408,1000.);
#34387=VECTOR('',#129445,1000.);
#34388=VECTOR('',#129446,10.);
#34389=VECTOR('',#129449,1000.);
#34390=VECTOR('',#129454,10.);
#34391=VECTOR('',#129455,1000.);
#34392=VECTOR('',#129456,1000.);
#34393=VECTOR('',#129493,1000.);
#34394=VECTOR('',#129494,10.);
#34395=VECTOR('',#129497,1000.);
#34396=VECTOR('',#129502,10.);
#34397=VECTOR('',#129503,1000.);
#34398=VECTOR('',#129504,1000.);
#34399=VECTOR('',#129541,1000.);
#34400=VECTOR('',#129542,10.);
#34401=VECTOR('',#129545,1000.);
#34402=VECTOR('',#129550,10.);
#34403=VECTOR('',#129551,1000.);
#34404=VECTOR('',#129552,1000.);
#34405=VECTOR('',#129589,1000.);
#34406=VECTOR('',#129590,10.);
#34407=VECTOR('',#129593,1000.);
#34408=VECTOR('',#129598,10.);
#34409=VECTOR('',#129599,1000.);
#34410=VECTOR('',#129600,1000.);
#34411=VECTOR('',#129637,1000.);
#34412=VECTOR('',#129638,10.);
#34413=VECTOR('',#129641,1000.);
#34414=VECTOR('',#129646,10.);
#34415=VECTOR('',#129647,1000.);
#34416=VECTOR('',#129648,1000.);
#34417=VECTOR('',#129689,1.25);
#34418=VECTOR('',#129694,1.25);
#34419=VECTOR('',#129699,1.25);
#34420=VECTOR('',#129702,1.25);
#34421=VECTOR('',#129705,1.25);
#34422=VECTOR('',#129708,1.25);
#34423=VECTOR('',#129711,1.25);
#34424=VECTOR('',#129714,1.25);
#34425=VECTOR('',#129719,1.29);
#34426=VECTOR('',#129724,1.29);
#34427=VECTOR('',#129727,1.29);
#34428=VECTOR('',#129730,1.29);
#34429=VECTOR('',#129733,1.29);
#34430=VECTOR('',#129736,1.29);
#34431=VECTOR('',#129739,1.29);
#34432=VECTOR('',#129742,1.29);
#34433=VECTOR('',#129747,1.25);
#34434=VECTOR('',#129752,1.25);
#34435=VECTOR('',#129757,1.25);
#34436=VECTOR('',#129760,1.25);
#34437=VECTOR('',#129763,1.25);
#34438=VECTOR('',#129766,1.25);
#34439=VECTOR('',#129769,1.25);
#34440=VECTOR('',#129772,1.25);
#34441=VECTOR('',#129777,1.29);
#34442=VECTOR('',#129782,1.29);
#34443=VECTOR('',#129785,1.29);
#34444=VECTOR('',#129788,1.29);
#34445=VECTOR('',#129791,1.29);
#34446=VECTOR('',#129794,1.29);
#34447=VECTOR('',#129797,1.29);
#34448=VECTOR('',#129800,1.29);
#34449=VECTOR('',#129805,1.25);
#34450=VECTOR('',#129810,1.25);
#34451=VECTOR('',#129815,1.25);
#34452=VECTOR('',#129818,1.25);
#34453=VECTOR('',#129821,1.25);
#34454=VECTOR('',#129824,1.25);
#34455=VECTOR('',#129827,1.25);
#34456=VECTOR('',#129830,1.25);
#34457=VECTOR('',#129835,1.29);
#34458=VECTOR('',#129840,1.29);
#34459=VECTOR('',#129843,1.29);
#34460=VECTOR('',#129846,1.29);
#34461=VECTOR('',#129849,1.29);
#34462=VECTOR('',#129852,1.29);
#34463=VECTOR('',#129855,1.29);
#34464=VECTOR('',#129858,1.29);
#34465=VECTOR('',#129863,1.25);
#34466=VECTOR('',#129868,1.25);
#34467=VECTOR('',#129873,1.25);
#34468=VECTOR('',#129876,1.25);
#34469=VECTOR('',#129879,1.25);
#34470=VECTOR('',#129882,1.25);
#34471=VECTOR('',#129885,1.25);
#34472=VECTOR('',#129888,1.25);
#34473=VECTOR('',#129893,1.29);
#34474=VECTOR('',#129898,1.29);
#34475=VECTOR('',#129901,1.29);
#34476=VECTOR('',#129904,1.29);
#34477=VECTOR('',#129907,1.29);
#34478=VECTOR('',#129910,1.29);
#34479=VECTOR('',#129913,1.29);
#34480=VECTOR('',#129916,1.29);
#34481=VECTOR('',#129923,2.25);
#34482=VECTOR('',#129932,2.1);
#34483=VECTOR('',#129951,11.15);
#34484=VECTOR('',#129956,1.99999999999997);
#34485=VECTOR('',#129961,3.5);
#34486=VECTOR('',#129968,11.15);
#34487=VECTOR('',#129971,11.15);
#34488=VECTOR('',#129978,4.95184441433916);
#34489=VECTOR('',#129983,11.15);
#34490=VECTOR('',#129990,5.08286386254677);
#34491=VECTOR('',#129997,11.15);
#34492=VECTOR('',#130004,5.21388331075437);
#34493=VECTOR('',#130011,11.15);
#34494=VECTOR('',#130018,5.34490275896198);
#34495=VECTOR('',#130025,11.15);
#34496=VECTOR('',#130032,5.47592220716958);
#34497=VECTOR('',#130039,11.15);
#34498=VECTOR('',#130046,5.60694165537719);
#34499=VECTOR('',#130053,11.15);
#34500=VECTOR('',#130060,5.73796110358479);
#34501=VECTOR('',#130067,11.15);
#34502=VECTOR('',#130074,5.8689805517924);
#34503=VECTOR('',#130081,11.15);
#34504=VECTOR('',#130088,6.);
#34505=VECTOR('',#130095,11.15);
#34506=VECTOR('',#130154,3.5);
#34507=VECTOR('',#130159,3.5);
#34508=VECTOR('',#130162,3.5);
#34509=VECTOR('',#130165,3.5);
#34510=VECTOR('',#130168,3.5);
#34511=VECTOR('',#130171,3.5);
#34512=VECTOR('',#130174,3.5);
#34513=VECTOR('',#130177,3.5);
#34514=VECTOR('',#130180,3.5);
#34515=VECTOR('',#130183,3.5);
#34516=VECTOR('',#130186,2.872);
#34517=VECTOR('',#130191,2.872);
#34518=VECTOR('',#130196,2.872);
#34519=VECTOR('',#130199,2.872);
#34520=VECTOR('',#130202,2.872);
#34521=VECTOR('',#130205,2.872);
#34522=VECTOR('',#130208,2.872);
#34523=VECTOR('',#130211,2.872);
#34524=VECTOR('',#130214,2.872);
#34525=VECTOR('',#130217,2.872);
#34526=VECTOR('',#130220,3.);
#34527=VECTOR('',#130225,3.);
#34528=VECTOR('',#130228,3.);
#34529=VECTOR('',#130231,3.);
#34530=VECTOR('',#130234,3.);
#34531=VECTOR('',#130237,2.37175);
#34532=VECTOR('',#130242,2.37175);
#34533=VECTOR('',#130245,2.37175);
#34534=VECTOR('',#130248,2.37175);
#34535=VECTOR('',#130251,2.37175);
#34536=VECTOR('',#130280,2.5);
#34537=VECTOR('',#130287,1.4);
#34538=VECTOR('',#130294,3.);
#34539=VECTOR('',#130301,2.1);
#34540=VECTOR('',#130308,2.1);
#34541=VECTOR('',#130313,1.);
#34542=VECTOR('',#130334,1.);
#34543=VECTOR('',#130339,2.);
#34544=VECTOR('',#130346,3.);
#34545=VECTOR('',#130351,3.);
#34546=VECTOR('',#130354,3.);
#34547=VECTOR('',#130357,3.);
#34548=VECTOR('',#130360,3.);
#34549=VECTOR('',#130363,3.);
#34550=VECTOR('',#130366,2.37175);
#34551=VECTOR('',#130371,2.37175);
#34552=VECTOR('',#130374,2.37175);
#34553=VECTOR('',#130377,2.37175);
#34554=VECTOR('',#130380,2.37175);
#34555=VECTOR('',#130383,2.37175);
#34556=VECTOR('',#130410,0.75);
#34557=VECTOR('',#130419,0.75);
#34558=VECTOR('',#130424,0.2);
#34559=VECTOR('',#130429,0.5);
#34560=VECTOR('',#130434,2.5);
#34561=VECTOR('',#130443,1.5);
#34562=VECTOR('',#130446,1.);
#34563=VECTOR('',#130451,0.2);
#34564=VECTOR('',#130454,1000.);
#34565=VECTOR('',#130455,999.999999999999);
#34566=VECTOR('',#130456,1000.);
#34567=VECTOR('',#130457,1000.);
#34568=VECTOR('',#130458,999.999999999999);
#34569=VECTOR('',#130459,1000.);
#34570=VECTOR('',#130462,1000.);
#34571=VECTOR('',#130463,1000.);
#34572=VECTOR('',#130464,999.999999999999);
#34573=VECTOR('',#130465,1000.);
#34574=VECTOR('',#130466,1000.);
#34575=VECTOR('',#130467,999.999999999999);
#34576=VECTOR('',#130470,1000.);
#34577=VECTOR('',#130471,1000.);
#34578=VECTOR('',#130474,1000.);
#34579=VECTOR('',#130477,1000.);
#34580=VECTOR('',#130480,1000.);
#34581=VECTOR('',#130483,1000.);
#34582=VECTOR('',#130494,3.);
#34583=VECTOR('',#130501,1.5);
#34584=VECTOR('',#130508,1.5);
#34585=VECTOR('',#130515,0.750000000000001);
#34586=VECTOR('',#130522,1.5);
#34587=VECTOR('',#130529,1000.);
#34588=VECTOR('',#130532,1000.);
#34589=VECTOR('',#130535,1000.);
#34590=VECTOR('',#130536,1000.);
#34591=VECTOR('',#130537,1000.);
#34592=VECTOR('',#130538,1000.);
#34593=VECTOR('',#130541,1000.);
#34594=VECTOR('',#130542,1000.);
#34595=VECTOR('',#130543,1000.);
#34596=VECTOR('',#130544,1000.);
#34597=VECTOR('',#130547,1000.);
#34598=VECTOR('',#130548,1000.);
#34599=VECTOR('',#130549,1000.);
#34600=VECTOR('',#130550,1000.);
#34601=VECTOR('',#130551,1000.);
#34602=VECTOR('',#130552,1000.);
#34603=VECTOR('',#130553,1000.);
#34604=VECTOR('',#130556,1000.);
#34605=VECTOR('',#130557,1000.);
#34606=VECTOR('',#130558,1000.);
#34607=VECTOR('',#130559,1000.);
#34608=VECTOR('',#130562,1000.);
#34609=VECTOR('',#130563,1000.);
#34610=VECTOR('',#130564,1000.);
#34611=VECTOR('',#130565,1000.);
#34612=VECTOR('',#130566,1000.);
#34613=VECTOR('',#130567,1000.);
#34614=VECTOR('',#130568,1000.);
#34615=VECTOR('',#130571,1000.);
#34616=VECTOR('',#130572,1000.);
#34617=VECTOR('',#130573,1000.);
#34618=VECTOR('',#130574,1000.);
#34619=VECTOR('',#130577,1000.);
#34620=VECTOR('',#130578,1000.);
#34621=VECTOR('',#130579,1000.);
#34622=VECTOR('',#130580,1000.);
#34623=VECTOR('',#130583,1000.);
#34624=VECTOR('',#130584,1000.);
#34625=VECTOR('',#130587,1000.);
#34626=VECTOR('',#130588,1000.);
#34627=VECTOR('',#130595,1000.);
#34628=VECTOR('',#130598,1000.);
#34629=VECTOR('',#130601,1000.);
#34630=VECTOR('',#130602,1000.);
#34631=VECTOR('',#130605,1000.);
#34632=VECTOR('',#130606,1000.);
#34633=VECTOR('',#130609,1000.);
#34634=VECTOR('',#130612,1000.);
#34635=VECTOR('',#130615,1000.);
#34636=VECTOR('',#130618,1000.);
#34637=VECTOR('',#130619,1000.);
#34638=VECTOR('',#130622,1000.);
#34639=VECTOR('',#130625,1000.);
#34640=VECTOR('',#130628,1000.);
#34641=VECTOR('',#130631,1000.);
#34642=VECTOR('',#130634,1000.);
#34643=VECTOR('',#130637,1000.);
#34644=VECTOR('',#130640,1000.);
#34645=VECTOR('',#130643,1000.);
#34646=VECTOR('',#130646,1000.);
#34647=VECTOR('',#130649,1000.);
#34648=VECTOR('',#130652,1000.);
#34649=VECTOR('',#130655,1000.);
#34650=VECTOR('',#130658,1000.);
#34651=VERTEX_POINT('',#130723);
#34652=VERTEX_POINT('',#130724);
#34653=VERTEX_POINT('',#130726);
#34654=VERTEX_POINT('',#130794);
#34655=VERTEX_POINT('',#130817);
#34656=VERTEX_POINT('',#130904);
#34657=VERTEX_POINT('',#130905);
#34658=VERTEX_POINT('',#130907);
#34659=VERTEX_POINT('',#131280);
#34660=VERTEX_POINT('',#131281);
#34661=VERTEX_POINT('',#131283);
#34662=VERTEX_POINT('',#131638);
#34663=VERTEX_POINT('',#131639);
#34664=VERTEX_POINT('',#131641);
#34665=VERTEX_POINT('',#131684);
#34666=VERTEX_POINT('',#131811);
#34667=VERTEX_POINT('',#131812);
#34668=VERTEX_POINT('',#131814);
#34669=VERTEX_POINT('',#131882);
#34670=VERTEX_POINT('',#131905);
#34671=VERTEX_POINT('',#131994);
#34672=VERTEX_POINT('',#131995);
#34673=VERTEX_POINT('',#131997);
#34674=VERTEX_POINT('',#132366);
#34675=VERTEX_POINT('',#132367);
#34676=VERTEX_POINT('',#132369);
#34677=VERTEX_POINT('',#132724);
#34678=VERTEX_POINT('',#132725);
#34679=VERTEX_POINT('',#132727);
#34680=VERTEX_POINT('',#132768);
#34681=VERTEX_POINT('',#132895);
#34682=VERTEX_POINT('',#132896);
#34683=VERTEX_POINT('',#132898);
#34684=VERTEX_POINT('',#132951);
#34685=VERTEX_POINT('',#133012);
#34686=VERTEX_POINT('',#133013);
#34687=VERTEX_POINT('',#133015);
#34688=VERTEX_POINT('',#133158);
#34689=VERTEX_POINT('',#133306);
#34690=VERTEX_POINT('',#133307);
#34691=VERTEX_POINT('',#133309);
#34692=VERTEX_POINT('',#133509);
#34693=VERTEX_POINT('',#133659);
#34694=VERTEX_POINT('',#133660);
#34695=VERTEX_POINT('',#133662);
#34696=VERTEX_POINT('',#133717);
#34697=VERTEX_POINT('',#133755);
#34698=VERTEX_POINT('',#133850);
#34699=VERTEX_POINT('',#133851);
#34700=VERTEX_POINT('',#133853);
#34701=VERTEX_POINT('',#133906);
#34702=VERTEX_POINT('',#133969);
#34703=VERTEX_POINT('',#133970);
#34704=VERTEX_POINT('',#133972);
#34705=VERTEX_POINT('',#134117);
#34706=VERTEX_POINT('',#134265);
#34707=VERTEX_POINT('',#134266);
#34708=VERTEX_POINT('',#134268);
#34709=VERTEX_POINT('',#134468);
#34710=VERTEX_POINT('',#134618);
#34711=VERTEX_POINT('',#134619);
#34712=VERTEX_POINT('',#134621);
#34713=VERTEX_POINT('',#134676);
#34714=VERTEX_POINT('',#134714);
#34715=VERTEX_POINT('',#135387);
#34716=VERTEX_POINT('',#135752);
#34717=VERTEX_POINT('',#136542);
#34718=VERTEX_POINT('',#136627);
#34719=VERTEX_POINT('',#136628);
#34720=VERTEX_POINT('',#136630);
#34721=VERTEX_POINT('',#136632);
#34722=VERTEX_POINT('',#136634);
#34723=VERTEX_POINT('',#136636);
#34724=VERTEX_POINT('',#137065);
#34725=VERTEX_POINT('',#137147);
#34726=VERTEX_POINT('',#137148);
#34727=VERTEX_POINT('',#137150);
#34728=VERTEX_POINT('',#137152);
#34729=VERTEX_POINT('',#137154);
#34730=VERTEX_POINT('',#137156);
#34731=VERTEX_POINT('',#137158);
#34732=VERTEX_POINT('',#137162);
#34733=VERTEX_POINT('',#137164);
#34734=VERTEX_POINT('',#137168);
#34735=VERTEX_POINT('',#137172);
#34736=VERTEX_POINT('',#137175);
#34737=VERTEX_POINT('',#137176);
#34738=VERTEX_POINT('',#137178);
#34739=VERTEX_POINT('',#137184);
#34740=VERTEX_POINT('',#137189);
#34741=VERTEX_POINT('',#137191);
#34742=VERTEX_POINT('',#137193);
#34743=VERTEX_POINT('',#137199);
#34744=VERTEX_POINT('',#137204);
#34745=VERTEX_POINT('',#137206);
#34746=VERTEX_POINT('',#137208);
#34747=VERTEX_POINT('',#137215);
#34748=VERTEX_POINT('',#137218);
#34749=VERTEX_POINT('',#137219);
#34750=VERTEX_POINT('',#137221);
#34751=VERTEX_POINT('',#137226);
#34752=VERTEX_POINT('',#137230);
#34753=VERTEX_POINT('',#137233);
#34754=VERTEX_POINT('',#137235);
#34755=VERTEX_POINT('',#137239);
#34756=VERTEX_POINT('',#137242);
#34757=VERTEX_POINT('',#137248);
#34758=VERTEX_POINT('',#137252);
#34759=VERTEX_POINT('',#137256);
#34760=VERTEX_POINT('',#137260);
#34761=VERTEX_POINT('',#137266);
#34762=VERTEX_POINT('',#137270);
#34763=VERTEX_POINT('',#137274);
#34764=VERTEX_POINT('',#137278);
#34765=VERTEX_POINT('',#137284);
#34766=VERTEX_POINT('',#137285);
#34767=VERTEX_POINT('',#137287);
#34768=VERTEX_POINT('',#137289);
#34769=VERTEX_POINT('',#137293);
#34770=VERTEX_POINT('',#137294);
#34771=VERTEX_POINT('',#137299);
#34772=VERTEX_POINT('',#137300);
#34773=VERTEX_POINT('',#137305);
#34774=VERTEX_POINT('',#137310);
#34775=VERTEX_POINT('',#137314);
#34776=VERTEX_POINT('',#137315);
#34777=VERTEX_POINT('',#137320);
#34778=VERTEX_POINT('',#137322);
#34779=VERTEX_POINT('',#137326);
#34780=VERTEX_POINT('',#137327);
#34781=VERTEX_POINT('',#137332);
#34782=VERTEX_POINT('',#137334);
#34783=VERTEX_POINT('',#137338);
#34784=VERTEX_POINT('',#137343);
#34785=VERTEX_POINT('',#137367);
#34786=VERTEX_POINT('',#137369);
#34787=VERTEX_POINT('',#137373);
#34788=VERTEX_POINT('',#137377);
#34789=VERTEX_POINT('',#137378);
#34790=VERTEX_POINT('',#137380);
#34791=VERTEX_POINT('',#137382);
#34792=VERTEX_POINT('',#137389);
#34793=VERTEX_POINT('',#137391);
#34794=VERTEX_POINT('',#137398);
#34795=VERTEX_POINT('',#137400);
#34796=VERTEX_POINT('',#137402);
#34797=VERTEX_POINT('',#137404);
#34798=VERTEX_POINT('',#137411);
#34799=VERTEX_POINT('',#137413);
#34800=VERTEX_POINT('',#137420);
#34801=VERTEX_POINT('',#137422);
#34802=VERTEX_POINT('',#137424);
#34803=VERTEX_POINT('',#137426);
#34804=VERTEX_POINT('',#137433);
#34805=VERTEX_POINT('',#137435);
#34806=VERTEX_POINT('',#137442);
#34807=VERTEX_POINT('',#137444);
#34808=VERTEX_POINT('',#137446);
#34809=VERTEX_POINT('',#137448);
#34810=VERTEX_POINT('',#137455);
#34811=VERTEX_POINT('',#137457);
#34812=VERTEX_POINT('',#137464);
#34813=VERTEX_POINT('',#137466);
#34814=VERTEX_POINT('',#137468);
#34815=VERTEX_POINT('',#137470);
#34816=VERTEX_POINT('',#137477);
#34817=VERTEX_POINT('',#137479);
#34818=VERTEX_POINT('',#137486);
#34819=VERTEX_POINT('',#137488);
#34820=VERTEX_POINT('',#137490);
#34821=VERTEX_POINT('',#137492);
#34822=VERTEX_POINT('',#137499);
#34823=VERTEX_POINT('',#137501);
#34824=VERTEX_POINT('',#137508);
#34825=VERTEX_POINT('',#137510);
#34826=VERTEX_POINT('',#137512);
#34827=VERTEX_POINT('',#137514);
#34828=VERTEX_POINT('',#137521);
#34829=VERTEX_POINT('',#137523);
#34830=VERTEX_POINT('',#137530);
#34831=VERTEX_POINT('',#137532);
#34832=VERTEX_POINT('',#137534);
#34833=VERTEX_POINT('',#137536);
#34834=VERTEX_POINT('',#137543);
#34835=VERTEX_POINT('',#137545);
#34836=VERTEX_POINT('',#137552);
#34837=VERTEX_POINT('',#137554);
#34838=VERTEX_POINT('',#137556);
#34839=VERTEX_POINT('',#137558);
#34840=VERTEX_POINT('',#137565);
#34841=VERTEX_POINT('',#137567);
#34842=VERTEX_POINT('',#137574);
#34843=VERTEX_POINT('',#137576);
#34844=VERTEX_POINT('',#137578);
#34845=VERTEX_POINT('',#137580);
#34846=VERTEX_POINT('',#137587);
#34847=VERTEX_POINT('',#137589);
#34848=VERTEX_POINT('',#137599);
#34849=VERTEX_POINT('',#137600);
#34850=VERTEX_POINT('',#137602);
#34851=VERTEX_POINT('',#137604);
#34852=VERTEX_POINT('',#137611);
#34853=VERTEX_POINT('',#137613);
#34854=VERTEX_POINT('',#137620);
#34855=VERTEX_POINT('',#137622);
#34856=VERTEX_POINT('',#137624);
#34857=VERTEX_POINT('',#137626);
#34858=VERTEX_POINT('',#137633);
#34859=VERTEX_POINT('',#137635);
#34860=VERTEX_POINT('',#137642);
#34861=VERTEX_POINT('',#137644);
#34862=VERTEX_POINT('',#137646);
#34863=VERTEX_POINT('',#137648);
#34864=VERTEX_POINT('',#137655);
#34865=VERTEX_POINT('',#137657);
#34866=VERTEX_POINT('',#137664);
#34867=VERTEX_POINT('',#137666);
#34868=VERTEX_POINT('',#137668);
#34869=VERTEX_POINT('',#137670);
#34870=VERTEX_POINT('',#137677);
#34871=VERTEX_POINT('',#137679);
#34872=VERTEX_POINT('',#137686);
#34873=VERTEX_POINT('',#137688);
#34874=VERTEX_POINT('',#137690);
#34875=VERTEX_POINT('',#137692);
#34876=VERTEX_POINT('',#137699);
#34877=VERTEX_POINT('',#137701);
#34878=VERTEX_POINT('',#137708);
#34879=VERTEX_POINT('',#137710);
#34880=VERTEX_POINT('',#137712);
#34881=VERTEX_POINT('',#137714);
#34882=VERTEX_POINT('',#137721);
#34883=VERTEX_POINT('',#137723);
#34884=VERTEX_POINT('',#137730);
#34885=VERTEX_POINT('',#137732);
#34886=VERTEX_POINT('',#137734);
#34887=VERTEX_POINT('',#137736);
#34888=VERTEX_POINT('',#137743);
#34889=VERTEX_POINT('',#137745);
#34890=VERTEX_POINT('',#137752);
#34891=VERTEX_POINT('',#137754);
#34892=VERTEX_POINT('',#137756);
#34893=VERTEX_POINT('',#137758);
#34894=VERTEX_POINT('',#137765);
#34895=VERTEX_POINT('',#137767);
#34896=VERTEX_POINT('',#137774);
#34897=VERTEX_POINT('',#137776);
#34898=VERTEX_POINT('',#137778);
#34899=VERTEX_POINT('',#137780);
#34900=VERTEX_POINT('',#137787);
#34901=VERTEX_POINT('',#137789);
#34902=VERTEX_POINT('',#137796);
#34903=VERTEX_POINT('',#137798);
#34904=VERTEX_POINT('',#137800);
#34905=VERTEX_POINT('',#137802);
#34906=VERTEX_POINT('',#137809);
#34907=VERTEX_POINT('',#137811);
#34908=VERTEX_POINT('',#137819);
#34909=VERTEX_POINT('',#138162);
#34910=VERTEX_POINT('',#138163);
#34911=VERTEX_POINT('',#138165);
#34912=VERTEX_POINT('',#138170);
#34913=VERTEX_POINT('',#138171);
#34914=VERTEX_POINT('',#138176);
#34915=VERTEX_POINT('',#138178);
#34916=VERTEX_POINT('',#138184);
#34917=VERTEX_POINT('',#138185);
#34918=VERTEX_POINT('',#138187);
#34919=VERTEX_POINT('',#138194);
#34920=VERTEX_POINT('',#138196);
#34921=VERTEX_POINT('',#138200);
#34922=VERTEX_POINT('',#138201);
#34923=VERTEX_POINT('',#138203);
#34924=VERTEX_POINT('',#138210);
#34925=VERTEX_POINT('',#138212);
#34926=VERTEX_POINT('',#138216);
#34927=VERTEX_POINT('',#138217);
#34928=VERTEX_POINT('',#138219);
#34929=VERTEX_POINT('',#138226);
#34930=VERTEX_POINT('',#138228);
#34931=VERTEX_POINT('',#138232);
#34932=VERTEX_POINT('',#138233);
#34933=VERTEX_POINT('',#138235);
#34934=VERTEX_POINT('',#138242);
#34935=VERTEX_POINT('',#138244);
#34936=VERTEX_POINT('',#138248);
#34937=VERTEX_POINT('',#138249);
#34938=VERTEX_POINT('',#138251);
#34939=VERTEX_POINT('',#138258);
#34940=VERTEX_POINT('',#138260);
#34941=VERTEX_POINT('',#138264);
#34942=VERTEX_POINT('',#138265);
#34943=VERTEX_POINT('',#138267);
#34944=VERTEX_POINT('',#138274);
#34945=VERTEX_POINT('',#138276);
#34946=VERTEX_POINT('',#138280);
#34947=VERTEX_POINT('',#138281);
#34948=VERTEX_POINT('',#138283);
#34949=VERTEX_POINT('',#138290);
#34950=VERTEX_POINT('',#138292);
#34951=VERTEX_POINT('',#138296);
#34952=VERTEX_POINT('',#138297);
#34953=VERTEX_POINT('',#138299);
#34954=VERTEX_POINT('',#138306);
#34955=VERTEX_POINT('',#138308);
#34956=VERTEX_POINT('',#138312);
#34957=VERTEX_POINT('',#138313);
#34958=VERTEX_POINT('',#138315);
#34959=VERTEX_POINT('',#138322);
#34960=VERTEX_POINT('',#138324);
#34961=VERTEX_POINT('',#138328);
#34962=VERTEX_POINT('',#138329);
#34963=VERTEX_POINT('',#138331);
#34964=VERTEX_POINT('',#138338);
#34965=VERTEX_POINT('',#138340);
#34966=VERTEX_POINT('',#138344);
#34967=VERTEX_POINT('',#138345);
#34968=VERTEX_POINT('',#138347);
#34969=VERTEX_POINT('',#138354);
#34970=VERTEX_POINT('',#138356);
#34971=VERTEX_POINT('',#138360);
#34972=VERTEX_POINT('',#138361);
#34973=VERTEX_POINT('',#138363);
#34974=VERTEX_POINT('',#138370);
#34975=VERTEX_POINT('',#138372);
#34976=VERTEX_POINT('',#138376);
#34977=VERTEX_POINT('',#138377);
#34978=VERTEX_POINT('',#138379);
#34979=VERTEX_POINT('',#138387);
#34980=VERTEX_POINT('',#138389);
#34981=VERTEX_POINT('',#138393);
#34982=VERTEX_POINT('',#138394);
#34983=VERTEX_POINT('',#138397);
#34984=VERTEX_POINT('',#138410);
#34985=VERTEX_POINT('',#138411);
#34986=VERTEX_POINT('',#138413);
#34987=VERTEX_POINT('',#138415);
#34988=VERTEX_POINT('',#138419);
#34989=VERTEX_POINT('',#138420);
#34990=VERTEX_POINT('',#138422);
#34991=VERTEX_POINT('',#138424);
#34992=VERTEX_POINT('',#138428);
#34993=VERTEX_POINT('',#138429);
#34994=VERTEX_POINT('',#138431);
#34995=VERTEX_POINT('',#138433);
#34996=VERTEX_POINT('',#138437);
#34997=VERTEX_POINT('',#138441);
#34998=VERTEX_POINT('',#138447);
#34999=VERTEX_POINT('',#138451);
#35000=VERTEX_POINT('',#138457);
#35001=VERTEX_POINT('',#138461);
#35002=VERTEX_POINT('',#138467);
#35003=VERTEX_POINT('',#138471);
#35004=VERTEX_POINT('',#138477);
#35005=VERTEX_POINT('',#138481);
#35006=VERTEX_POINT('',#138487);
#35007=VERTEX_POINT('',#138491);
#35008=VERTEX_POINT('',#138497);
#35009=VERTEX_POINT('',#138499);
#35010=VERTEX_POINT('',#138503);
#35011=VERTEX_POINT('',#138505);
#35012=VERTEX_POINT('',#138509);
#35013=VERTEX_POINT('',#138511);
#35014=VERTEX_POINT('',#138515);
#35015=VERTEX_POINT('',#138517);
#35016=VERTEX_POINT('',#138519);
#35017=VERTEX_POINT('',#138522);
#35018=VERTEX_POINT('',#138524);
#35019=VERTEX_POINT('',#138527);
#35020=VERTEX_POINT('',#138529);
#35021=VERTEX_POINT('',#138532);
#35022=VERTEX_POINT('',#138534);
#35023=VERTEX_POINT('',#138536);
#35024=VERTEX_POINT('',#138538);
#35025=VERTEX_POINT('',#138540);
#35026=VERTEX_POINT('',#138544);
#35027=VERTEX_POINT('',#138546);
#35028=VERTEX_POINT('',#138550);
#35029=VERTEX_POINT('',#138554);
#35030=VERTEX_POINT('',#138560);
#35031=VERTEX_POINT('',#138564);
#35032=VERTEX_POINT('',#138570);
#35033=VERTEX_POINT('',#138572);
#35034=VERTEX_POINT('',#138576);
#35035=VERTEX_POINT('',#138577);
#35036=VERTEX_POINT('',#138579);
#35037=VERTEX_POINT('',#138582);
#35038=VERTEX_POINT('',#138585);
#35039=VERTEX_POINT('',#138587);
#35040=VERTEX_POINT('',#138590);
#35041=VERTEX_POINT('',#138592);
#35042=VERTEX_POINT('',#138595);
#35043=VERTEX_POINT('',#138597);
#35044=VERTEX_POINT('',#138602);
#35045=VERTEX_POINT('',#138605);
#35046=VERTEX_POINT('',#138630);
#35047=VERTEX_POINT('',#138631);
#35048=VERTEX_POINT('',#138633);
#35049=VERTEX_POINT('',#138635);
#35050=VERTEX_POINT('',#138639);
#35051=VERTEX_POINT('',#138641);
#35052=VERTEX_POINT('',#138645);
#35053=VERTEX_POINT('',#138647);
#35054=VERTEX_POINT('',#138649);
#35055=VERTEX_POINT('',#138651);
#35056=VERTEX_POINT('',#138653);
#35057=VERTEX_POINT('',#138655);
#35058=VERTEX_POINT('',#138657);
#35059=VERTEX_POINT('',#138659);
#35060=VERTEX_POINT('',#138661);
#35061=VERTEX_POINT('',#138665);
#35062=VERTEX_POINT('',#138669);
#35063=VERTEX_POINT('',#138673);
#35064=VERTEX_POINT('',#138674);
#35065=VERTEX_POINT('',#138681);
#35066=VERTEX_POINT('',#138682);
#35067=VERTEX_POINT('',#138687);
#35068=VERTEX_POINT('',#138691);
#35069=VERTEX_POINT('',#138693);
#35070=VERTEX_POINT('',#138697);
#35071=VERTEX_POINT('',#138699);
#35072=VERTEX_POINT('',#138703);
#35073=VERTEX_POINT('',#138705);
#35074=VERTEX_POINT('',#138717);
#35075=VERTEX_POINT('',#138718);
#35076=VERTEX_POINT('',#138720);
#35077=VERTEX_POINT('',#138722);
#35078=VERTEX_POINT('',#138740);
#35079=VERTEX_POINT('',#138741);
#35080=VERTEX_POINT('',#138746);
#35081=VERTEX_POINT('',#138747);
#35082=VERTEX_POINT('',#138766);
#35083=VERTEX_POINT('',#138767);
#35084=VERTEX_POINT('',#138772);
#35085=VERTEX_POINT('',#138773);
#35086=VERTEX_POINT('',#138792);
#35087=VERTEX_POINT('',#138793);
#35088=VERTEX_POINT('',#138798);
#35089=VERTEX_POINT('',#138799);
#35090=VERTEX_POINT('',#138812);
#35091=VERTEX_POINT('',#138813);
#35092=VERTEX_POINT('',#138818);
#35093=VERTEX_POINT('',#138819);
#35094=VERTEX_POINT('',#138835);
#35095=VERTEX_POINT('',#138837);
#35096=VERTEX_POINT('',#138839);
#35097=VERTEX_POINT('',#138841);
#35098=VERTEX_POINT('',#138843);
#35099=VERTEX_POINT('',#138845);
#35100=VERTEX_POINT('',#138853);
#35101=VERTEX_POINT('',#138855);
#35102=VERTEX_POINT('',#138859);
#35103=VERTEX_POINT('',#138863);
#35104=VERTEX_POINT('',#138867);
#35105=VERTEX_POINT('',#138871);
#35106=VERTEX_POINT('',#138876);
#35107=VERTEX_POINT('',#138877);
#35108=VERTEX_POINT('',#138879);
#35109=VERTEX_POINT('',#138881);
#35110=VERTEX_POINT('',#138893);
#35111=VERTEX_POINT('',#138894);
#35112=VERTEX_POINT('',#138899);
#35113=VERTEX_POINT('',#138900);
#35114=VERTEX_POINT('',#138919);
#35115=VERTEX_POINT('',#138920);
#35116=VERTEX_POINT('',#138925);
#35117=VERTEX_POINT('',#138926);
#35118=VERTEX_POINT('',#138939);
#35119=VERTEX_POINT('',#138940);
#35120=VERTEX_POINT('',#138945);
#35121=VERTEX_POINT('',#138946);
#35122=VERTEX_POINT('',#138951);
#35123=VERTEX_POINT('',#138952);
#35124=VERTEX_POINT('',#138957);
#35125=VERTEX_POINT('',#138958);
#35126=VERTEX_POINT('',#138977);
#35127=VERTEX_POINT('',#138978);
#35128=VERTEX_POINT('',#138983);
#35129=VERTEX_POINT('',#138984);
#35130=VERTEX_POINT('',#138997);
#35131=VERTEX_POINT('',#138998);
#35132=VERTEX_POINT('',#139003);
#35133=VERTEX_POINT('',#139004);
#35134=VERTEX_POINT('',#139006);
#35135=VERTEX_POINT('',#139022);
#35136=VERTEX_POINT('',#139024);
#35137=VERTEX_POINT('',#139028);
#35138=VERTEX_POINT('',#139032);
#35139=VERTEX_POINT('',#139036);
#35140=VERTEX_POINT('',#139040);
#35141=VERTEX_POINT('',#139043);
#35142=VERTEX_POINT('',#139045);
#35143=VERTEX_POINT('',#139047);
#35144=VERTEX_POINT('',#139049);
#35145=VERTEX_POINT('',#139051);
#35146=VERTEX_POINT('',#139053);
#35147=VERTEX_POINT('',#139055);
#35148=VERTEX_POINT('',#139057);
#35149=VERTEX_POINT('',#139059);
#35150=VERTEX_POINT('',#139063);
#35151=VERTEX_POINT('',#139067);
#35152=VERTEX_POINT('',#139072);
#35153=VERTEX_POINT('',#139073);
#35154=VERTEX_POINT('',#139075);
#35155=VERTEX_POINT('',#139077);
#35156=VERTEX_POINT('',#139089);
#35157=VERTEX_POINT('',#139090);
#35158=VERTEX_POINT('',#139095);
#35159=VERTEX_POINT('',#139096);
#35160=VERTEX_POINT('',#139115);
#35161=VERTEX_POINT('',#139116);
#35162=VERTEX_POINT('',#139121);
#35163=VERTEX_POINT('',#139122);
#35164=VERTEX_POINT('',#139141);
#35165=VERTEX_POINT('',#139142);
#35166=VERTEX_POINT('',#139147);
#35167=VERTEX_POINT('',#139148);
#35168=VERTEX_POINT('',#139161);
#35169=VERTEX_POINT('',#139162);
#35170=VERTEX_POINT('',#139167);
#35171=VERTEX_POINT('',#139168);
#35172=VERTEX_POINT('',#139181);
#35173=VERTEX_POINT('',#139186);
#35174=VERTEX_POINT('',#139201);
#35175=VERTEX_POINT('',#139203);
#35176=VERTEX_POINT('',#139205);
#35177=VERTEX_POINT('',#139207);
#35178=VERTEX_POINT('',#139211);
#35179=VERTEX_POINT('',#139217);
#35180=VERTEX_POINT('',#139221);
#35181=VERTEX_POINT('',#139226);
#35182=VERTEX_POINT('',#139227);
#35183=VERTEX_POINT('',#139229);
#35184=VERTEX_POINT('',#139231);
#35185=VERTEX_POINT('',#139243);
#35186=VERTEX_POINT('',#139244);
#35187=VERTEX_POINT('',#139249);
#35188=VERTEX_POINT('',#139250);
#35189=VERTEX_POINT('',#139263);
#35190=VERTEX_POINT('',#139264);
#35191=VERTEX_POINT('',#139269);
#35192=VERTEX_POINT('',#139270);
#35193=VERTEX_POINT('',#139275);
#35194=VERTEX_POINT('',#139276);
#35195=VERTEX_POINT('',#139281);
#35196=VERTEX_POINT('',#139282);
#35197=VERTEX_POINT('',#139287);
#35198=VERTEX_POINT('',#139288);
#35199=VERTEX_POINT('',#139307);
#35200=VERTEX_POINT('',#139308);
#35201=VERTEX_POINT('',#139313);
#35202=VERTEX_POINT('',#139314);
#35203=VERTEX_POINT('',#139330);
#35204=VERTEX_POINT('',#139332);
#35205=VERTEX_POINT('',#139334);
#35206=VERTEX_POINT('',#139336);
#35207=VERTEX_POINT('',#139340);
#35208=VERTEX_POINT('',#139344);
#35209=VERTEX_POINT('',#139348);
#35210=VERTEX_POINT('',#139352);
#35211=VERTEX_POINT('',#139356);
#35212=VERTEX_POINT('',#139358);
#35213=VERTEX_POINT('',#139360);
#35214=VERTEX_POINT('',#139365);
#35215=VERTEX_POINT('',#139366);
#35216=VERTEX_POINT('',#139368);
#35217=VERTEX_POINT('',#139370);
#35218=VERTEX_POINT('',#139388);
#35219=VERTEX_POINT('',#139389);
#35220=VERTEX_POINT('',#139394);
#35221=VERTEX_POINT('',#139395);
#35222=VERTEX_POINT('',#139400);
#35223=VERTEX_POINT('',#139401);
#35224=VERTEX_POINT('',#139420);
#35225=VERTEX_POINT('',#139421);
#35226=VERTEX_POINT('',#139426);
#35227=VERTEX_POINT('',#139427);
#35228=VERTEX_POINT('',#139432);
#35229=VERTEX_POINT('',#139433);
#35230=VERTEX_POINT('',#139438);
#35231=VERTEX_POINT('',#139439);
#35232=VERTEX_POINT('',#139452);
#35233=VERTEX_POINT('',#139453);
#35234=VERTEX_POINT('',#139458);
#35235=VERTEX_POINT('',#139459);
#35236=VERTEX_POINT('',#139478);
#35237=VERTEX_POINT('',#139479);
#35238=VERTEX_POINT('',#139484);
#35239=VERTEX_POINT('',#139485);
#35240=VERTEX_POINT('',#139504);
#35241=VERTEX_POINT('',#139505);
#35242=VERTEX_POINT('',#139513);
#35243=VERTEX_POINT('',#139515);
#35244=VERTEX_POINT('',#139519);
#35245=VERTEX_POINT('',#139523);
#35246=VERTEX_POINT('',#139527);
#35247=VERTEX_POINT('',#139531);
#35248=VERTEX_POINT('',#139535);
#35249=VERTEX_POINT('',#139539);
#35250=VERTEX_POINT('',#139544);
#35251=VERTEX_POINT('',#139545);
#35252=VERTEX_POINT('',#139547);
#35253=VERTEX_POINT('',#139549);
#35254=VERTEX_POINT('',#139553);
#35255=VERTEX_POINT('',#139554);
#35256=VERTEX_POINT('',#139573);
#35257=VERTEX_POINT('',#139574);
#35258=VERTEX_POINT('',#139579);
#35259=VERTEX_POINT('',#139580);
#35260=VERTEX_POINT('',#139593);
#35261=VERTEX_POINT('',#139594);
#35262=VERTEX_POINT('',#139599);
#35263=VERTEX_POINT('',#139600);
#35264=VERTEX_POINT('',#139619);
#35265=VERTEX_POINT('',#139620);
#35266=VERTEX_POINT('',#139625);
#35267=VERTEX_POINT('',#139626);
#35268=VERTEX_POINT('',#139642);
#35269=VERTEX_POINT('',#139644);
#35270=VERTEX_POINT('',#139648);
#35271=VERTEX_POINT('',#139652);
#35272=VERTEX_POINT('',#139656);
#35273=VERTEX_POINT('',#139660);
#35274=VERTEX_POINT('',#139665);
#35275=VERTEX_POINT('',#139666);
#35276=VERTEX_POINT('',#139668);
#35277=VERTEX_POINT('',#139670);
#35278=VERTEX_POINT('',#139682);
#35279=VERTEX_POINT('',#139683);
#35280=VERTEX_POINT('',#139688);
#35281=VERTEX_POINT('',#139689);
#35282=VERTEX_POINT('',#139694);
#35283=VERTEX_POINT('',#139695);
#35284=VERTEX_POINT('',#139700);
#35285=VERTEX_POINT('',#139701);
#35286=VERTEX_POINT('',#139714);
#35287=VERTEX_POINT('',#139715);
#35288=VERTEX_POINT('',#139720);
#35289=VERTEX_POINT('',#139721);
#35290=VERTEX_POINT('',#139740);
#35291=VERTEX_POINT('',#139741);
#35292=VERTEX_POINT('',#139746);
#35293=VERTEX_POINT('',#139747);
#35294=VERTEX_POINT('',#139760);
#35295=VERTEX_POINT('',#139761);
#35296=VERTEX_POINT('',#139766);
#35297=VERTEX_POINT('',#139767);
#35298=VERTEX_POINT('',#139780);
#35299=VERTEX_POINT('',#139781);
#35300=VERTEX_POINT('',#139786);
#35301=VERTEX_POINT('',#139787);
#35302=VERTEX_POINT('',#139800);
#35303=VERTEX_POINT('',#139801);
#35304=VERTEX_POINT('',#139806);
#35305=VERTEX_POINT('',#139807);
#35306=VERTEX_POINT('',#139829);
#35307=VERTEX_POINT('',#139831);
#35308=VERTEX_POINT('',#139835);
#35309=VERTEX_POINT('',#139839);
#35310=VERTEX_POINT('',#139843);
#35311=VERTEX_POINT('',#139847);
#35312=VERTEX_POINT('',#139851);
#35313=VERTEX_POINT('',#139855);
#35314=VERTEX_POINT('',#139859);
#35315=VERTEX_POINT('',#139861);
#35316=VERTEX_POINT('',#139863);
#35317=VERTEX_POINT('',#139868);
#35318=VERTEX_POINT('',#139869);
#35319=VERTEX_POINT('',#139871);
#35320=VERTEX_POINT('',#139873);
#35321=VERTEX_POINT('',#139891);
#35322=VERTEX_POINT('',#139892);
#35323=VERTEX_POINT('',#139897);
#35324=VERTEX_POINT('',#139898);
#35325=VERTEX_POINT('',#139903);
#35326=VERTEX_POINT('',#139904);
#35327=VERTEX_POINT('',#139917);
#35328=VERTEX_POINT('',#139918);
#35329=VERTEX_POINT('',#139923);
#35330=VERTEX_POINT('',#139924);
#35331=VERTEX_POINT('',#139943);
#35332=VERTEX_POINT('',#139944);
#35333=VERTEX_POINT('',#139949);
#35334=VERTEX_POINT('',#139950);
#35335=VERTEX_POINT('',#139972);
#35336=VERTEX_POINT('',#139974);
#35337=VERTEX_POINT('',#139976);
#35338=VERTEX_POINT('',#139978);
#35339=VERTEX_POINT('',#139980);
#35340=VERTEX_POINT('',#139982);
#35341=VERTEX_POINT('',#139986);
#35342=VERTEX_POINT('',#139990);
#35343=VERTEX_POINT('',#139994);
#35344=VERTEX_POINT('',#139998);
#35345=VERTEX_POINT('',#140003);
#35346=VERTEX_POINT('',#140004);
#35347=VERTEX_POINT('',#140006);
#35348=VERTEX_POINT('',#140008);
#35349=VERTEX_POINT('',#140020);
#35350=VERTEX_POINT('',#140021);
#35351=VERTEX_POINT('',#140026);
#35352=VERTEX_POINT('',#140027);
#35353=VERTEX_POINT('',#140046);
#35354=VERTEX_POINT('',#140047);
#35355=VERTEX_POINT('',#140052);
#35356=VERTEX_POINT('',#140053);
#35357=VERTEX_POINT('',#140072);
#35358=VERTEX_POINT('',#140073);
#35359=VERTEX_POINT('',#140078);
#35360=VERTEX_POINT('',#140079);
#35361=VERTEX_POINT('',#140101);
#35362=VERTEX_POINT('',#140103);
#35363=VERTEX_POINT('',#140107);
#35364=VERTEX_POINT('',#140111);
#35365=VERTEX_POINT('',#140115);
#35366=VERTEX_POINT('',#140164);
#35367=VERTEX_POINT('',#140165);
#35368=VERTEX_POINT('',#140197);
#35369=VERTEX_POINT('',#140207);
#35370=VERTEX_POINT('',#140242);
#35371=VERTEX_POINT('',#140291);
#35372=VERTEX_POINT('',#140328);
#35373=VERTEX_POINT('',#140332);
#35374=VERTEX_POINT('',#140334);
#35375=VERTEX_POINT('',#140336);
#35376=VERTEX_POINT('',#140338);
#35377=VERTEX_POINT('',#140340);
#35378=VERTEX_POINT('',#140347);
#35379=VERTEX_POINT('',#140349);
#35380=VERTEX_POINT('',#140357);
#35381=VERTEX_POINT('',#140359);
#35382=VERTEX_POINT('',#140361);
#35383=VERTEX_POINT('',#140363);
#35384=VERTEX_POINT('',#140365);
#35385=VERTEX_POINT('',#140367);
#35386=VERTEX_POINT('',#140385);
#35387=VERTEX_POINT('',#140387);
#35388=VERTEX_POINT('',#140391);
#35389=VERTEX_POINT('',#140393);
#35390=VERTEX_POINT('',#140395);
#35391=VERTEX_POINT('',#140397);
#35392=VERTEX_POINT('',#140399);
#35393=VERTEX_POINT('',#140404);
#35394=VERTEX_POINT('',#140406);
#35395=VERTEX_POINT('',#140408);
#35396=VERTEX_POINT('',#140412);
#35397=VERTEX_POINT('',#140413);
#35398=VERTEX_POINT('',#140415);
#35399=VERTEX_POINT('',#140417);
#35400=VERTEX_POINT('',#140421);
#35401=VERTEX_POINT('',#140423);
#35402=VERTEX_POINT('',#140425);
#35403=VERTEX_POINT('',#140428);
#35404=VERTEX_POINT('',#140430);
#35405=VERTEX_POINT('',#140432);
#35406=VERTEX_POINT('',#140434);
#35407=VERTEX_POINT('',#140436);
#35408=VERTEX_POINT('',#140439);
#35409=VERTEX_POINT('',#140441);
#35410=VERTEX_POINT('',#140443);
#35411=VERTEX_POINT('',#140445);
#35412=VERTEX_POINT('',#140447);
#35413=VERTEX_POINT('',#140449);
#35414=VERTEX_POINT('',#140451);
#35415=VERTEX_POINT('',#140453);
#35416=VERTEX_POINT('',#140455);
#35417=VERTEX_POINT('',#140457);
#35418=VERTEX_POINT('',#140459);
#35419=VERTEX_POINT('',#140461);
#35420=VERTEX_POINT('',#140463);
#35421=VERTEX_POINT('',#140466);
#35422=VERTEX_POINT('',#140469);
#35423=VERTEX_POINT('',#140473);
#35424=VERTEX_POINT('',#140475);
#35425=VERTEX_POINT('',#140477);
#35426=VERTEX_POINT('',#140479);
#35427=VERTEX_POINT('',#140481);
#35428=VERTEX_POINT('',#140483);
#35429=VERTEX_POINT('',#140485);
#35430=VERTEX_POINT('',#140487);
#35431=VERTEX_POINT('',#140491);
#35432=VERTEX_POINT('',#140493);
#35433=VERTEX_POINT('',#140495);
#35434=VERTEX_POINT('',#140497);
#35435=VERTEX_POINT('',#140500);
#35436=VERTEX_POINT('',#140502);
#35437=VERTEX_POINT('',#140505);
#35438=VERTEX_POINT('',#140506);
#35439=VERTEX_POINT('',#140509);
#35440=VERTEX_POINT('',#140511);
#35441=VERTEX_POINT('',#140513);
#35442=VERTEX_POINT('',#140515);
#35443=VERTEX_POINT('',#140518);
#35444=VERTEX_POINT('',#140521);
#35445=VERTEX_POINT('',#140523);
#35446=VERTEX_POINT('',#140527);
#35447=VERTEX_POINT('',#140529);
#35448=VERTEX_POINT('',#140533);
#35449=VERTEX_POINT('',#140537);
#35450=VERTEX_POINT('',#140540);
#35451=VERTEX_POINT('',#140542);
#35452=VERTEX_POINT('',#140544);
#35453=VERTEX_POINT('',#140546);
#35454=VERTEX_POINT('',#140549);
#35455=VERTEX_POINT('',#140551);
#35456=VERTEX_POINT('',#140553);
#35457=VERTEX_POINT('',#140555);
#35458=VERTEX_POINT('',#140557);
#35459=VERTEX_POINT('',#140559);
#35460=VERTEX_POINT('',#140561);
#35461=VERTEX_POINT('',#140563);
#35462=VERTEX_POINT('',#140565);
#35463=VERTEX_POINT('',#140567);
#35464=VERTEX_POINT('',#140569);
#35465=VERTEX_POINT('',#140571);
#35466=VERTEX_POINT('',#140573);
#35467=VERTEX_POINT('',#140575);
#35468=VERTEX_POINT('',#140578);
#35469=VERTEX_POINT('',#140579);
#35470=VERTEX_POINT('',#140581);
#35471=VERTEX_POINT('',#140583);
#35472=VERTEX_POINT('',#140586);
#35473=VERTEX_POINT('',#140588);
#35474=VERTEX_POINT('',#140590);
#35475=VERTEX_POINT('',#140595);
#35476=VERTEX_POINT('',#140597);
#35477=VERTEX_POINT('',#140603);
#35478=VERTEX_POINT('',#140607);
#35479=VERTEX_POINT('',#140609);
#35480=VERTEX_POINT('',#140613);
#35481=VERTEX_POINT('',#140615);
#35482=VERTEX_POINT('',#140621);
#35483=VERTEX_POINT('',#140623);
#35484=VERTEX_POINT('',#140625);
#35485=VERTEX_POINT('',#140627);
#35486=VERTEX_POINT('',#140629);
#35487=VERTEX_POINT('',#140631);
#35488=VERTEX_POINT('',#140633);
#35489=VERTEX_POINT('',#140635);
#35490=VERTEX_POINT('',#140637);
#35491=VERTEX_POINT('',#140639);
#35492=VERTEX_POINT('',#140642);
#35493=VERTEX_POINT('',#140647);
#35494=VERTEX_POINT('',#140649);
#35495=VERTEX_POINT('',#140653);
#35496=VERTEX_POINT('',#140659);
#35497=VERTEX_POINT('',#140661);
#35498=VERTEX_POINT('',#140663);
#35499=VERTEX_POINT('',#140665);
#35500=VERTEX_POINT('',#140669);
#35501=VERTEX_POINT('',#140671);
#35502=VERTEX_POINT('',#140673);
#35503=VERTEX_POINT('',#140676);
#35504=VERTEX_POINT('',#140679);
#35505=VERTEX_POINT('',#140703);
#35506=VERTEX_POINT('',#140705);
#35507=VERTEX_POINT('',#140709);
#35508=VERTEX_POINT('',#140715);
#35509=VERTEX_POINT('',#140717);
#35510=VERTEX_POINT('',#140721);
#35511=VERTEX_POINT('',#140726);
#35512=VERTEX_POINT('',#140767);
#35513=VERTEX_POINT('',#140769);
#35514=VERTEX_POINT('',#140774);
#35515=VERTEX_POINT('',#140777);
#35516=VERTEX_POINT('',#140785);
#35517=VERTEX_POINT('',#140788);
#35518=VERTEX_POINT('',#140790);
#35519=VERTEX_POINT('',#140799);
#35520=VERTEX_POINT('',#140805);
#35521=VERTEX_POINT('',#140807);
#35522=VERTEX_POINT('',#140811);
#35523=VERTEX_POINT('',#140848);
#35524=VERTEX_POINT('',#140850);
#35525=VERTEX_POINT('',#140852);
#35526=VERTEX_POINT('',#140854);
#35527=VERTEX_POINT('',#140856);
#35528=VERTEX_POINT('',#140858);
#35529=VERTEX_POINT('',#140862);
#35530=VERTEX_POINT('',#140878);
#35531=VERTEX_POINT('',#140881);
#35532=VERTEX_POINT('',#140885);
#35533=VERTEX_POINT('',#140890);
#35534=VERTEX_POINT('',#140892);
#35535=VERTEX_POINT('',#140896);
#35536=VERTEX_POINT('',#140900);
#35537=VERTEX_POINT('',#140904);
#35538=VERTEX_POINT('',#140905);
#35539=VERTEX_POINT('',#140910);
#35540=VERTEX_POINT('',#140914);
#35541=VERTEX_POINT('',#140920);
#35542=VERTEX_POINT('',#140925);
#35543=VERTEX_POINT('',#140929);
#35544=VERTEX_POINT('',#140933);
#35545=VERTEX_POINT('',#140934);
#35546=VERTEX_POINT('',#140939);
#35547=VERTEX_POINT('',#140948);
#35548=VERTEX_POINT('',#140949);
#35549=VERTEX_POINT('',#140952);
#35550=VERTEX_POINT('',#140954);
#35551=VERTEX_POINT('',#140978);
#35552=VERTEX_POINT('',#140979);
#35553=VERTEX_POINT('',#140990);
#35554=VERTEX_POINT('',#141001);
#35555=VERTEX_POINT('',#141003);
#35556=VERTEX_POINT('',#141007);
#35557=VERTEX_POINT('',#141014);
#35558=VERTEX_POINT('',#141015);
#35559=VERTEX_POINT('',#141017);
#35560=VERTEX_POINT('',#141019);
#35561=VERTEX_POINT('',#141023);
#35562=VERTEX_POINT('',#141025);
#35563=VERTEX_POINT('',#141027);
#35564=VERTEX_POINT('',#141029);
#35565=VERTEX_POINT('',#141031);
#35566=VERTEX_POINT('',#141033);
#35567=VERTEX_POINT('',#141035);
#35568=VERTEX_POINT('',#141037);
#35569=VERTEX_POINT('',#141039);
#35570=VERTEX_POINT('',#141041);
#35571=VERTEX_POINT('',#141043);
#35572=VERTEX_POINT('',#141045);
#35573=VERTEX_POINT('',#141047);
#35574=VERTEX_POINT('',#141049);
#35575=VERTEX_POINT('',#141051);
#35576=VERTEX_POINT('',#141053);
#35577=VERTEX_POINT('',#141055);
#35578=VERTEX_POINT('',#141057);
#35579=VERTEX_POINT('',#141061);
#35580=VERTEX_POINT('',#141065);
#35581=VERTEX_POINT('',#141069);
#35582=VERTEX_POINT('',#141071);
#35583=VERTEX_POINT('',#141073);
#35584=VERTEX_POINT('',#141077);
#35585=VERTEX_POINT('',#141078);
#35586=VERTEX_POINT('',#141080);
#35587=VERTEX_POINT('',#141082);
#35588=VERTEX_POINT('',#141100);
#35589=VERTEX_POINT('',#141105);
#35590=VERTEX_POINT('',#141117);
#35591=VERTEX_POINT('',#141118);
#35592=VERTEX_POINT('',#141123);
#35593=VERTEX_POINT('',#141124);
#35594=VERTEX_POINT('',#141143);
#35595=VERTEX_POINT('',#141144);
#35596=VERTEX_POINT('',#141149);
#35597=VERTEX_POINT('',#141150);
#35598=VERTEX_POINT('',#141172);
#35599=VERTEX_POINT('',#141174);
#35600=VERTEX_POINT('',#141178);
#35601=VERTEX_POINT('',#141182);
#35602=VERTEX_POINT('',#141186);
#35603=VERTEX_POINT('',#141188);
#35604=VERTEX_POINT('',#141190);
#35605=VERTEX_POINT('',#141195);
#35606=VERTEX_POINT('',#141196);
#35607=VERTEX_POINT('',#141198);
#35608=VERTEX_POINT('',#141200);
#35609=VERTEX_POINT('',#141217);
#35610=VERTEX_POINT('',#141218);
#35611=VERTEX_POINT('',#141220);
#35612=VERTEX_POINT('',#141222);
#35613=VERTEX_POINT('',#141239);
#35614=VERTEX_POINT('',#141240);
#35615=VERTEX_POINT('',#141248);
#35616=VERTEX_POINT('',#141249);
#35617=VERTEX_POINT('',#141251);
#35618=VERTEX_POINT('',#141253);
#35619=VERTEX_POINT('',#141273);
#35620=VERTEX_POINT('',#141275);
#35621=VERTEX_POINT('',#141297);
#35622=VERTEX_POINT('',#141299);
#35623=VERTEX_POINT('',#141303);
#35624=VERTEX_POINT('',#141307);
#35625=VERTEX_POINT('',#141311);
#35626=VERTEX_POINT('',#141316);
#35627=VERTEX_POINT('',#141317);
#35628=VERTEX_POINT('',#141330);
#35629=VERTEX_POINT('',#141332);
#35630=VERTEX_POINT('',#141334);
#35631=VERTEX_POINT('',#141359);
#35632=VERTEX_POINT('',#141360);
#35633=VERTEX_POINT('',#141365);
#35634=VERTEX_POINT('',#141366);
#35635=VERTEX_POINT('',#141373);
#35636=VERTEX_POINT('',#141375);
#35637=VERTEX_POINT('',#141391);
#35638=VERTEX_POINT('',#141400);
#35639=VERTEX_POINT('',#141402);
#35640=VERTEX_POINT('',#141407);
#35641=VERTEX_POINT('',#141409);
#35642=VERTEX_POINT('',#141414);
#35643=VERTEX_POINT('',#141416);
#35644=VERTEX_POINT('',#141418);
#35645=VERTEX_POINT('',#141420);
#35646=VERTEX_POINT('',#141427);
#35647=VERTEX_POINT('',#141434);
#35648=VERTEX_POINT('',#141449);
#35649=VERTEX_POINT('',#141456);
#35650=VERTEX_POINT('',#141471);
#35651=VERTEX_POINT('',#141473);
#35652=VERTEX_POINT('',#141475);
#35653=VERTEX_POINT('',#141491);
#35654=VERTEX_POINT('',#141509);
#35655=VERTEX_POINT('',#141511);
#35656=VERTEX_POINT('',#141515);
#35657=VERTEX_POINT('',#141517);
#35658=VERTEX_POINT('',#141521);
#35659=VERTEX_POINT('',#141523);
#35660=VERTEX_POINT('',#141525);
#35661=VERTEX_POINT('',#141529);
#35662=VERTEX_POINT('',#141531);
#35663=VERTEX_POINT('',#141535);
#35664=VERTEX_POINT('',#141544);
#35665=VERTEX_POINT('',#141556);
#35666=VERTEX_POINT('',#141562);
#35667=VERTEX_POINT('',#141564);
#35668=VERTEX_POINT('',#141566);
#35669=VERTEX_POINT('',#141568);
#35670=VERTEX_POINT('',#141573);
#35671=VERTEX_POINT('',#141576);
#35672=VERTEX_POINT('',#141593);
#35673=VERTEX_POINT('',#141595);
#35674=VERTEX_POINT('',#141597);
#35675=VERTEX_POINT('',#141599);
#35676=VERTEX_POINT('',#141601);
#35677=VERTEX_POINT('',#141604);
#35678=VERTEX_POINT('',#141606);
#35679=VERTEX_POINT('',#141608);
#35680=VERTEX_POINT('',#141610);
#35681=VERTEX_POINT('',#141612);
#35682=VERTEX_POINT('',#141618);
#35683=VERTEX_POINT('',#141620);
#35684=VERTEX_POINT('',#141624);
#35685=VERTEX_POINT('',#141629);
#35686=VERTEX_POINT('',#141635);
#35687=VERTEX_POINT('',#141639);
#35688=VERTEX_POINT('',#141640);
#35689=VERTEX_POINT('',#141642);
#35690=VERTEX_POINT('',#141644);
#35691=VERTEX_POINT('',#141677);
#35692=VERTEX_POINT('',#141678);
#35693=VERTEX_POINT('',#141683);
#35694=VERTEX_POINT('',#141684);
#35695=VERTEX_POINT('',#141697);
#35696=VERTEX_POINT('',#141698);
#35697=VERTEX_POINT('',#141703);
#35698=VERTEX_POINT('',#141705);
#35699=VERTEX_POINT('',#141712);
#35700=VERTEX_POINT('',#141714);
#35701=VERTEX_POINT('',#141716);
#35702=VERTEX_POINT('',#141718);
#35703=VERTEX_POINT('',#141722);
#35704=VERTEX_POINT('',#141724);
#35705=VERTEX_POINT('',#141729);
#35706=VERTEX_POINT('',#141731);
#35707=VERTEX_POINT('',#141744);
#35708=VERTEX_POINT('',#141749);
#35709=VERTEX_POINT('',#141750);
#35710=VERTEX_POINT('',#141755);
#35711=VERTEX_POINT('',#141757);
#35712=VERTEX_POINT('',#141762);
#35713=VERTEX_POINT('',#141777);
#35714=VERTEX_POINT('',#141779);
#35715=VERTEX_POINT('',#141788);
#35716=VERTEX_POINT('',#141820);
#35717=VERTEX_POINT('',#141824);
#35718=VERTEX_POINT('',#141828);
#35719=VERTEX_POINT('',#141830);
#35720=VERTEX_POINT('',#141834);
#35721=VERTEX_POINT('',#141836);
#35722=VERTEX_POINT('',#141838);
#35723=VERTEX_POINT('',#141840);
#35724=VERTEX_POINT('',#141842);
#35725=VERTEX_POINT('',#141844);
#35726=VERTEX_POINT('',#141848);
#35727=VERTEX_POINT('',#141860);
#35728=VERTEX_POINT('',#141864);
#35729=VERTEX_POINT('',#141876);
#35730=VERTEX_POINT('',#141880);
#35731=VERTEX_POINT('',#141892);
#35732=VERTEX_POINT('',#141898);
#35733=VERTEX_POINT('',#141900);
#35734=VERTEX_POINT('',#141902);
#35735=VERTEX_POINT('',#141914);
#35736=VERTEX_POINT('',#141918);
#35737=VERTEX_POINT('',#141922);
#35738=VERTEX_POINT('',#141926);
#35739=VERTEX_POINT('',#141930);
#35740=VERTEX_POINT('',#141934);
#35741=VERTEX_POINT('',#141938);
#35742=VERTEX_POINT('',#141942);
#35743=VERTEX_POINT('',#141971);
#35744=VERTEX_POINT('',#141973);
#35745=VERTEX_POINT('',#141975);
#35746=VERTEX_POINT('',#141977);
#35747=VERTEX_POINT('',#141979);
#35748=VERTEX_POINT('',#141981);
#35749=VERTEX_POINT('',#141988);
#35750=VERTEX_POINT('',#142013);
#35751=VERTEX_POINT('',#142027);
#35752=VERTEX_POINT('',#142032);
#35753=VERTEX_POINT('',#142033);
#35754=VERTEX_POINT('',#142035);
#35755=VERTEX_POINT('',#142037);
#35756=VERTEX_POINT('',#142055);
#35757=VERTEX_POINT('',#142056);
#35758=VERTEX_POINT('',#142061);
#35759=VERTEX_POINT('',#142062);
#35760=VERTEX_POINT('',#142067);
#35761=VERTEX_POINT('',#142068);
#35762=VERTEX_POINT('',#142073);
#35763=VERTEX_POINT('',#142074);
#35764=VERTEX_POINT('',#142093);
#35765=VERTEX_POINT('',#142094);
#35766=VERTEX_POINT('',#142099);
#35767=VERTEX_POINT('',#142100);
#35768=VERTEX_POINT('',#142102);
#35769=VERTEX_POINT('',#142104);
#35770=VERTEX_POINT('',#142122);
#35771=VERTEX_POINT('',#142123);
#35772=VERTEX_POINT('',#142128);
#35773=VERTEX_POINT('',#142129);
#35774=VERTEX_POINT('',#142134);
#35775=VERTEX_POINT('',#142144);
#35776=VERTEX_POINT('',#142146);
#35777=VERTEX_POINT('',#142150);
#35778=VERTEX_POINT('',#142154);
#35779=VERTEX_POINT('',#142158);
#35780=VERTEX_POINT('',#142162);
#35781=VERTEX_POINT('',#142166);
#35782=VERTEX_POINT('',#142171);
#35783=VERTEX_POINT('',#142172);
#35784=VERTEX_POINT('',#142174);
#35785=VERTEX_POINT('',#142176);
#35786=VERTEX_POINT('',#142188);
#35787=VERTEX_POINT('',#142189);
#35788=VERTEX_POINT('',#142194);
#35789=VERTEX_POINT('',#142195);
#35790=VERTEX_POINT('',#142200);
#35791=VERTEX_POINT('',#142201);
#35792=VERTEX_POINT('',#142220);
#35793=VERTEX_POINT('',#142221);
#35794=VERTEX_POINT('',#142226);
#35795=VERTEX_POINT('',#142227);
#35796=VERTEX_POINT('',#142232);
#35797=VERTEX_POINT('',#142233);
#35798=VERTEX_POINT('',#142252);
#35799=VERTEX_POINT('',#142253);
#35800=VERTEX_POINT('',#142258);
#35801=VERTEX_POINT('',#142259);
#35802=VERTEX_POINT('',#142272);
#35803=VERTEX_POINT('',#142273);
#35804=VERTEX_POINT('',#142278);
#35805=VERTEX_POINT('',#142279);
#35806=VERTEX_POINT('',#142295);
#35807=VERTEX_POINT('',#142297);
#35808=VERTEX_POINT('',#142301);
#35809=VERTEX_POINT('',#142305);
#35810=VERTEX_POINT('',#142309);
#35811=VERTEX_POINT('',#142313);
#35812=VERTEX_POINT('',#142317);
#35813=VERTEX_POINT('',#142322);
#35814=VERTEX_POINT('',#142323);
#35815=VERTEX_POINT('',#142325);
#35816=VERTEX_POINT('',#142327);
#35817=VERTEX_POINT('',#142339);
#35818=VERTEX_POINT('',#142340);
#35819=VERTEX_POINT('',#142345);
#35820=VERTEX_POINT('',#142346);
#35821=VERTEX_POINT('',#142359);
#35822=VERTEX_POINT('',#142360);
#35823=VERTEX_POINT('',#142365);
#35824=VERTEX_POINT('',#142366);
#35825=VERTEX_POINT('',#142371);
#35826=VERTEX_POINT('',#142372);
#35827=VERTEX_POINT('',#142377);
#35828=VERTEX_POINT('',#142378);
#35829=VERTEX_POINT('',#142397);
#35830=VERTEX_POINT('',#142398);
#35831=VERTEX_POINT('',#142403);
#35832=VERTEX_POINT('',#142404);
#35833=VERTEX_POINT('',#142409);
#35834=VERTEX_POINT('',#142410);
#35835=VERTEX_POINT('',#142426);
#35836=VERTEX_POINT('',#142428);
#35837=VERTEX_POINT('',#142432);
#35838=VERTEX_POINT('',#142436);
#35839=VERTEX_POINT('',#142438);
#35840=VERTEX_POINT('',#142440);
#35841=VERTEX_POINT('',#142444);
#35842=VERTEX_POINT('',#142446);
#35843=VERTEX_POINT('',#142448);
#35844=VERTEX_POINT('',#142450);
#35845=VERTEX_POINT('',#142464);
#35846=VERTEX_POINT('',#142493);
#35847=VERTEX_POINT('',#142519);
#35848=VERTEX_POINT('',#142521);
#35849=VERTEX_POINT('',#142525);
#35850=VERTEX_POINT('',#142529);
#35851=VERTEX_POINT('',#142534);
#35852=VERTEX_POINT('',#142535);
#35853=VERTEX_POINT('',#142537);
#35854=VERTEX_POINT('',#142539);
#35855=VERTEX_POINT('',#142570);
#35856=VERTEX_POINT('',#142571);
#35857=VERTEX_POINT('',#142576);
#35858=VERTEX_POINT('',#142577);
#35859=VERTEX_POINT('',#142596);
#35860=VERTEX_POINT('',#142597);
#35861=VERTEX_POINT('',#142602);
#35862=VERTEX_POINT('',#142604);
#35863=VERTEX_POINT('',#142609);
#35864=VERTEX_POINT('',#142614);
#35865=VERTEX_POINT('',#142618);
#35866=VERTEX_POINT('',#142620);
#35867=VERTEX_POINT('',#142624);
#35868=VERTEX_POINT('',#142626);
#35869=VERTEX_POINT('',#142628);
#35870=VERTEX_POINT('',#142630);
#35871=VERTEX_POINT('',#142632);
#35872=VERTEX_POINT('',#142634);
#35873=VERTEX_POINT('',#142638);
#35874=VERTEX_POINT('',#142659);
#35875=VERTEX_POINT('',#142661);
#35876=VERTEX_POINT('',#142663);
#35877=VERTEX_POINT('',#142674);
#35878=VERTEX_POINT('',#142676);
#35879=VERTEX_POINT('',#142695);
#35880=VERTEX_POINT('',#142697);
#35881=VERTEX_POINT('',#142708);
#35882=VERTEX_POINT('',#142710);
#35883=VERTEX_POINT('',#142712);
#35884=VERTEX_POINT('',#142727);
#35885=VERTEX_POINT('',#142728);
#35886=VERTEX_POINT('',#142730);
#35887=VERTEX_POINT('',#142732);
#35888=VERTEX_POINT('',#142736);
#35889=VERTEX_POINT('',#142737);
#35890=VERTEX_POINT('',#142742);
#35891=VERTEX_POINT('',#142743);
#35892=VERTEX_POINT('',#142762);
#35893=VERTEX_POINT('',#142763);
#35894=VERTEX_POINT('',#142768);
#35895=VERTEX_POINT('',#142769);
#35896=VERTEX_POINT('',#142788);
#35897=VERTEX_POINT('',#142789);
#35898=VERTEX_POINT('',#142794);
#35899=VERTEX_POINT('',#142795);
#35900=VERTEX_POINT('',#142808);
#35901=VERTEX_POINT('',#142809);
#35902=VERTEX_POINT('',#142814);
#35903=VERTEX_POINT('',#142815);
#35904=VERTEX_POINT('',#142817);
#35905=VERTEX_POINT('',#142830);
#35906=VERTEX_POINT('',#142831);
#35907=VERTEX_POINT('',#142836);
#35908=VERTEX_POINT('',#142837);
#35909=VERTEX_POINT('',#142859);
#35910=VERTEX_POINT('',#142861);
#35911=VERTEX_POINT('',#142865);
#35912=VERTEX_POINT('',#142868);
#35913=VERTEX_POINT('',#142870);
#35914=VERTEX_POINT('',#142872);
#35915=VERTEX_POINT('',#142874);
#35916=VERTEX_POINT('',#142876);
#35917=VERTEX_POINT('',#142878);
#35918=VERTEX_POINT('',#142880);
#35919=VERTEX_POINT('',#142882);
#35920=VERTEX_POINT('',#142884);
#35921=VERTEX_POINT('',#142888);
#35922=VERTEX_POINT('',#142892);
#35923=VERTEX_POINT('',#142896);
#35924=VERTEX_POINT('',#142900);
#35925=VERTEX_POINT('',#142905);
#35926=VERTEX_POINT('',#142906);
#35927=VERTEX_POINT('',#142908);
#35928=VERTEX_POINT('',#142910);
#35929=VERTEX_POINT('',#142935);
#35930=VERTEX_POINT('',#142936);
#35931=VERTEX_POINT('',#142941);
#35932=VERTEX_POINT('',#142942);
#35933=VERTEX_POINT('',#142955);
#35934=VERTEX_POINT('',#142956);
#35935=VERTEX_POINT('',#142961);
#35936=VERTEX_POINT('',#142962);
#35937=VERTEX_POINT('',#142975);
#35938=VERTEX_POINT('',#142980);
#35939=VERTEX_POINT('',#142992);
#35940=VERTEX_POINT('',#142993);
#35941=VERTEX_POINT('',#142998);
#35942=VERTEX_POINT('',#142999);
#35943=VERTEX_POINT('',#143018);
#35944=VERTEX_POINT('',#143019);
#35945=VERTEX_POINT('',#143024);
#35946=VERTEX_POINT('',#143026);
#35947=VERTEX_POINT('',#143043);
#35948=VERTEX_POINT('',#143044);
#35949=VERTEX_POINT('',#143058);
#35950=VERTEX_POINT('',#143060);
#35951=VERTEX_POINT('',#143064);
#35952=VERTEX_POINT('',#143097);
#35953=VERTEX_POINT('',#143100);
#35954=VERTEX_POINT('',#143102);
#35955=VERTEX_POINT('',#143104);
#35956=VERTEX_POINT('',#143106);
#35957=VERTEX_POINT('',#143108);
#35958=VERTEX_POINT('',#143128);
#35959=VERTEX_POINT('',#143143);
#35960=VERTEX_POINT('',#143156);
#35961=VERTEX_POINT('',#143164);
#35962=VERTEX_POINT('',#143166);
#35963=VERTEX_POINT('',#143168);
#35964=VERTEX_POINT('',#143170);
#35965=VERTEX_POINT('',#143172);
#35966=VERTEX_POINT('',#143174);
#35967=VERTEX_POINT('',#143179);
#35968=VERTEX_POINT('',#143180);
#35969=VERTEX_POINT('',#143182);
#35970=VERTEX_POINT('',#143184);
#35971=VERTEX_POINT('',#143202);
#35972=VERTEX_POINT('',#143203);
#35973=VERTEX_POINT('',#143208);
#35974=VERTEX_POINT('',#143209);
#35975=VERTEX_POINT('',#143222);
#35976=VERTEX_POINT('',#143227);
#35977=VERTEX_POINT('',#143239);
#35978=VERTEX_POINT('',#143240);
#35979=VERTEX_POINT('',#143245);
#35980=VERTEX_POINT('',#143246);
#35981=VERTEX_POINT('',#143259);
#35982=VERTEX_POINT('',#143260);
#35983=VERTEX_POINT('',#143265);
#35984=VERTEX_POINT('',#143266);
#35985=VERTEX_POINT('',#143282);
#35986=VERTEX_POINT('',#143284);
#35987=VERTEX_POINT('',#143288);
#35988=VERTEX_POINT('',#143292);
#35989=VERTEX_POINT('',#143296);
#35990=VERTEX_POINT('',#143300);
#35991=VERTEX_POINT('',#143302);
#35992=VERTEX_POINT('',#143304);
#35993=VERTEX_POINT('',#143306);
#35994=VERTEX_POINT('',#143308);
#35995=VERTEX_POINT('',#143310);
#35996=VERTEX_POINT('',#143312);
#35997=VERTEX_POINT('',#143319);
#35998=VERTEX_POINT('',#143332);
#35999=VERTEX_POINT('',#143347);
#36000=VERTEX_POINT('',#143354);
#36001=VERTEX_POINT('',#143356);
#36002=VERTEX_POINT('',#143361);
#36003=VERTEX_POINT('',#143365);
#36004=VERTEX_POINT('',#143371);
#36005=VERTEX_POINT('',#143377);
#36006=VERTEX_POINT('',#143378);
#36007=VERTEX_POINT('',#143380);
#36008=VERTEX_POINT('',#143382);
#36009=VERTEX_POINT('',#143386);
#36010=VERTEX_POINT('',#143388);
#36011=VERTEX_POINT('',#143390);
#36012=VERTEX_POINT('',#143392);
#36013=VERTEX_POINT('',#143394);
#36014=VERTEX_POINT('',#143396);
#36015=VERTEX_POINT('',#143400);
#36016=VERTEX_POINT('',#143402);
#36017=VERTEX_POINT('',#143409);
#36018=VERTEX_POINT('',#143413);
#36019=VERTEX_POINT('',#143415);
#36020=VERTEX_POINT('',#143419);
#36021=VERTEX_POINT('',#143421);
#36022=VERTEX_POINT('',#143425);
#36023=VERTEX_POINT('',#143427);
#36024=VERTEX_POINT('',#143431);
#36025=VERTEX_POINT('',#143433);
#36026=VERTEX_POINT('',#143437);
#36027=VERTEX_POINT('',#143439);
#36028=VERTEX_POINT('',#143443);
#36029=VERTEX_POINT('',#143445);
#36030=VERTEX_POINT('',#143448);
#36031=VERTEX_POINT('',#143452);
#36032=VERTEX_POINT('',#143456);
#36033=VERTEX_POINT('',#143458);
#36034=VERTEX_POINT('',#143460);
#36035=VERTEX_POINT('',#143462);
#36036=VERTEX_POINT('',#143464);
#36037=VERTEX_POINT('',#143466);
#36038=VERTEX_POINT('',#143468);
#36039=VERTEX_POINT('',#143470);
#36040=VERTEX_POINT('',#143474);
#36041=VERTEX_POINT('',#143478);
#36042=VERTEX_POINT('',#143484);
#36043=VERTEX_POINT('',#143486);
#36044=VERTEX_POINT('',#143490);
#36045=VERTEX_POINT('',#143491);
#36046=VERTEX_POINT('',#143493);
#36047=VERTEX_POINT('',#143495);
#36048=VERTEX_POINT('',#143499);
#36049=VERTEX_POINT('',#143501);
#36050=VERTEX_POINT('',#143505);
#36051=VERTEX_POINT('',#143509);
#36052=VERTEX_POINT('',#143511);
#36053=VERTEX_POINT('',#143515);
#36054=VERTEX_POINT('',#143517);
#36055=VERTEX_POINT('',#143521);
#36056=VERTEX_POINT('',#143522);
#36057=VERTEX_POINT('',#143524);
#36058=VERTEX_POINT('',#143526);
#36059=VERTEX_POINT('',#143533);
#36060=VERTEX_POINT('',#143535);
#36061=VERTEX_POINT('',#143539);
#36062=VERTEX_POINT('',#143541);
#36063=VERTEX_POINT('',#143545);
#36064=VERTEX_POINT('',#143546);
#36065=VERTEX_POINT('',#143548);
#36066=VERTEX_POINT('',#143550);
#36067=VERTEX_POINT('',#143554);
#36068=VERTEX_POINT('',#143555);
#36069=VERTEX_POINT('',#143574);
#36070=VERTEX_POINT('',#143576);
#36071=VERTEX_POINT('',#143597);
#36072=VERTEX_POINT('',#143599);
#36073=VERTEX_POINT('',#143620);
#36074=VERTEX_POINT('',#143622);
#36075=VERTEX_POINT('',#143626);
#36076=VERTEX_POINT('',#143627);
#36077=VERTEX_POINT('',#143630);
#36078=VERTEX_POINT('',#143635);
#36079=VERTEX_POINT('',#143637);
#36080=VERTEX_POINT('',#143641);
#36081=VERTEX_POINT('',#143642);
#36082=VERTEX_POINT('',#143645);
#36083=VERTEX_POINT('',#143657);
#36084=VERTEX_POINT('',#143658);
#36085=VERTEX_POINT('',#143660);
#36086=VERTEX_POINT('',#143662);
#36087=VERTEX_POINT('',#143664);
#36088=VERTEX_POINT('',#143666);
#36089=VERTEX_POINT('',#143670);
#36090=VERTEX_POINT('',#143671);
#36091=VERTEX_POINT('',#143673);
#36092=VERTEX_POINT('',#143675);
#36093=VERTEX_POINT('',#143677);
#36094=VERTEX_POINT('',#143679);
#36095=VERTEX_POINT('',#143683);
#36096=VERTEX_POINT('',#143685);
#36097=VERTEX_POINT('',#143689);
#36098=VERTEX_POINT('',#143691);
#36099=VERTEX_POINT('',#143695);
#36100=VERTEX_POINT('',#143699);
#36101=VERTEX_POINT('',#143701);
#36102=VERTEX_POINT('',#143705);
#36103=VERTEX_POINT('',#143707);
#36104=VERTEX_POINT('',#143711);
#36105=VERTEX_POINT('',#143716);
#36106=VERTEX_POINT('',#143722);
#36107=VERTEX_POINT('',#143727);
#36108=VERTEX_POINT('',#143728);
#36109=VERTEX_POINT('',#143732);
#36110=VERTEX_POINT('',#143734);
#36111=VERTEX_POINT('',#143738);
#36112=VERTEX_POINT('',#143740);
#36113=VERTEX_POINT('',#143744);
#36114=VERTEX_POINT('',#143748);
#36115=VERTEX_POINT('',#143759);
#36116=VERTEX_POINT('',#143760);
#36117=VERTEX_POINT('',#143764);
#36118=VERTEX_POINT('',#143766);
#36119=VERTEX_POINT('',#143770);
#36120=VERTEX_POINT('',#143772);
#36121=VERTEX_POINT('',#143776);
#36122=VERTEX_POINT('',#143780);
#36123=VERTEX_POINT('',#143791);
#36124=VERTEX_POINT('',#143793);
#36125=VERTEX_POINT('',#143800);
#36126=VERTEX_POINT('',#143812);
#36127=VERTEX_POINT('',#143830);
#36128=VERTEX_POINT('',#143832);
#36129=VERTEX_POINT('',#143836);
#36130=VERTEX_POINT('',#143837);
#36131=VERTEX_POINT('',#143839);
#36132=VERTEX_POINT('',#143841);
#36133=VERTEX_POINT('',#143858);
#36134=VERTEX_POINT('',#143859);
#36135=VERTEX_POINT('',#143861);
#36136=VERTEX_POINT('',#143863);
#36137=VERTEX_POINT('',#143867);
#36138=VERTEX_POINT('',#143869);
#36139=VERTEX_POINT('',#143873);
#36140=VERTEX_POINT('',#143874);
#36141=VERTEX_POINT('',#143898);
#36142=VERTEX_POINT('',#143900);
#36143=VERTEX_POINT('',#143903);
#36144=VERTEX_POINT('',#143907);
#36145=VERTEX_POINT('',#143908);
#36146=VERTEX_POINT('',#143929);
#36147=VERTEX_POINT('',#143935);
#36148=VERTEX_POINT('',#143939);
#36149=VERTEX_POINT('',#143943);
#36150=VERTEX_POINT('',#143948);
#36151=VERTEX_POINT('',#143949);
#36152=VERTEX_POINT('',#143957);
#36153=VERTEX_POINT('',#143977);
#36154=VERTEX_POINT('',#143979);
#36155=VERTEX_POINT('',#143983);
#36156=VERTEX_POINT('',#143989);
#36157=VERTEX_POINT('',#143993);
#36158=VERTEX_POINT('',#143994);
#36159=VERTEX_POINT('',#144006);
#36160=VERTEX_POINT('',#144007);
#36161=VERTEX_POINT('',#144012);
#36162=VERTEX_POINT('',#144033);
#36163=VERTEX_POINT('',#144034);
#36164=VERTEX_POINT('',#144039);
#36165=VERTEX_POINT('',#144054);
#36166=VERTEX_POINT('',#144059);
#36167=VERTEX_POINT('',#144071);
#36168=VERTEX_POINT('',#144073);
#36169=VERTEX_POINT('',#144088);
#36170=VERTEX_POINT('',#144116);
#36171=VERTEX_POINT('',#144117);
#36172=VERTEX_POINT('',#144131);
#36173=VERTEX_POINT('',#144133);
#36174=VERTEX_POINT('',#144137);
#36175=VERTEX_POINT('',#144150);
#36176=VERTEX_POINT('',#144154);
#36177=VERTEX_POINT('',#144155);
#36178=VERTEX_POINT('',#144162);
#36179=VERTEX_POINT('',#144167);
#36180=VERTEX_POINT('',#144184);
#36181=VERTEX_POINT('',#144202);
#36182=VERTEX_POINT('',#144203);
#36183=VERTEX_POINT('',#144205);
#36184=VERTEX_POINT('',#144230);
#36185=VERTEX_POINT('',#144231);
#36186=VERTEX_POINT('',#144233);
#36187=VERTEX_POINT('',#144247);
#36188=VERTEX_POINT('',#144248);
#36189=VERTEX_POINT('',#144265);
#36190=VERTEX_POINT('',#144267);
#36191=VERTEX_POINT('',#144271);
#36192=VERTEX_POINT('',#144273);
#36193=VERTEX_POINT('',#144275);
#36194=VERTEX_POINT('',#144282);
#36195=VERTEX_POINT('',#144289);
#36196=VERTEX_POINT('',#144307);
#36197=VERTEX_POINT('',#144322);
#36198=VERTEX_POINT('',#144326);
#36199=VERTEX_POINT('',#144331);
#36200=VERTEX_POINT('',#144346);
#36201=VERTEX_POINT('',#144348);
#36202=VERTEX_POINT('',#144352);
#36203=VERTEX_POINT('',#144355);
#36204=VERTEX_POINT('',#144359);
#36205=VERTEX_POINT('',#144363);
#36206=VERTEX_POINT('',#144365);
#36207=VERTEX_POINT('',#144380);
#36208=VERTEX_POINT('',#144382);
#36209=VERTEX_POINT('',#144386);
#36210=VERTEX_POINT('',#144402);
#36211=VERTEX_POINT('',#144404);
#36212=VERTEX_POINT('',#144408);
#36213=VERTEX_POINT('',#144412);
#36214=VERTEX_POINT('',#144413);
#36215=VERTEX_POINT('',#144415);
#36216=VERTEX_POINT('',#144417);
#36217=VERTEX_POINT('',#144421);
#36218=VERTEX_POINT('',#144422);
#36219=VERTEX_POINT('',#144424);
#36220=VERTEX_POINT('',#144426);
#36221=VERTEX_POINT('',#144430);
#36222=VERTEX_POINT('',#144431);
#36223=VERTEX_POINT('',#144436);
#36224=VERTEX_POINT('',#144440);
#36225=VERTEX_POINT('',#144444);
#36226=VERTEX_POINT('',#144448);
#36227=VERTEX_POINT('',#144450);
#36228=VERTEX_POINT('',#144452);
#36229=VERTEX_POINT('',#144454);
#36230=VERTEX_POINT('',#144461);
#36231=VERTEX_POINT('',#144472);
#36232=VERTEX_POINT('',#144474);
#36233=VERTEX_POINT('',#144478);
#36234=VERTEX_POINT('',#144482);
#36235=VERTEX_POINT('',#144494);
#36236=VERTEX_POINT('',#144498);
#36237=VERTEX_POINT('',#144505);
#36238=VERTEX_POINT('',#144507);
#36239=VERTEX_POINT('',#144516);
#36240=VERTEX_POINT('',#144519);
#36241=VERTEX_POINT('',#144521);
#36242=VERTEX_POINT('',#144524);
#36243=VERTEX_POINT('',#144528);
#36244=VERTEX_POINT('',#144534);
#36245=VERTEX_POINT('',#144535);
#36246=VERTEX_POINT('',#144545);
#36247=VERTEX_POINT('',#144552);
#36248=VERTEX_POINT('',#144554);
#36249=VERTEX_POINT('',#144557);
#36250=VERTEX_POINT('',#144558);
#36251=VERTEX_POINT('',#144563);
#36252=VERTEX_POINT('',#144572);
#36253=VERTEX_POINT('',#144586);
#36254=VERTEX_POINT('',#144595);
#36255=VERTEX_POINT('',#144617);
#36256=VERTEX_POINT('',#144643);
#36257=VERTEX_POINT('',#144644);
#36258=VERTEX_POINT('',#144649);
#36259=VERTEX_POINT('',#144686);
#36260=VERTEX_POINT('',#144687);
#36261=VERTEX_POINT('',#144689);
#36262=VERTEX_POINT('',#144691);
#36263=VERTEX_POINT('',#144695);
#36264=VERTEX_POINT('',#144696);
#36265=VERTEX_POINT('',#144698);
#36266=VERTEX_POINT('',#144700);
#36267=VERTEX_POINT('',#144711);
#36268=VERTEX_POINT('',#144715);
#36269=VERTEX_POINT('',#144716);
#36270=VERTEX_POINT('',#144718);
#36271=VERTEX_POINT('',#144780);
#36272=VERTEX_POINT('',#144810);
#36273=VERTEX_POINT('',#144813);
#36274=VERTEX_POINT('',#144902);
#36275=VERTEX_POINT('',#144910);
#36276=VERTEX_POINT('',#144916);
#36277=VERTEX_POINT('',#144918);
#36278=VERTEX_POINT('',#144924);
#36279=VERTEX_POINT('',#144930);
#36280=VERTEX_POINT('',#144932);
#36281=VERTEX_POINT('',#144934);
#36282=VERTEX_POINT('',#144938);
#36283=VERTEX_POINT('',#144940);
#36284=VERTEX_POINT('',#144944);
#36285=VERTEX_POINT('',#144945);
#36286=VERTEX_POINT('',#144947);
#36287=VERTEX_POINT('',#144949);
#36288=VERTEX_POINT('',#144953);
#36289=VERTEX_POINT('',#144955);
#36290=VERTEX_POINT('',#144959);
#36291=VERTEX_POINT('',#144961);
#36292=VERTEX_POINT('',#144965);
#36293=VERTEX_POINT('',#144966);
#36294=VERTEX_POINT('',#144971);
#36295=VERTEX_POINT('',#144981);
#36296=VERTEX_POINT('',#144985);
#36297=VERTEX_POINT('',#144991);
#36298=VERTEX_POINT('',#144997);
#36299=VERTEX_POINT('',#144998);
#36300=VERTEX_POINT('',#145000);
#36301=VERTEX_POINT('',#145002);
#36302=VERTEX_POINT('',#145009);
#36303=VERTEX_POINT('',#145010);
#36304=VERTEX_POINT('',#145012);
#36305=VERTEX_POINT('',#145014);
#36306=VERTEX_POINT('',#145017);
#36307=VERTEX_POINT('',#145019);
#36308=VERTEX_POINT('',#145023);
#36309=VERTEX_POINT('',#145027);
#36310=VERTEX_POINT('',#145033);
#36311=VERTEX_POINT('',#145034);
#36312=VERTEX_POINT('',#145041);
#36313=VERTEX_POINT('',#145045);
#36314=VERTEX_POINT('',#145049);
#36315=VERTEX_POINT('',#145053);
#36316=VERTEX_POINT('',#145054);
#36317=VERTEX_POINT('',#145059);
#36318=VERTEX_POINT('',#145061);
#36319=VERTEX_POINT('',#145066);
#36320=VERTEX_POINT('',#145070);
#36321=VERTEX_POINT('',#145071);
#36322=VERTEX_POINT('',#145079);
#36323=VERTEX_POINT('',#145081);
#36324=VERTEX_POINT('',#145088);
#36325=VERTEX_POINT('',#145089);
#36326=VERTEX_POINT('',#145094);
#36327=VERTEX_POINT('',#145100);
#36328=VERTEX_POINT('',#145102);
#36329=VERTEX_POINT('',#145106);
#36330=VERTEX_POINT('',#145108);
#36331=VERTEX_POINT('',#145111);
#36332=VERTEX_POINT('',#145113);
#36333=VERTEX_POINT('',#145115);
#36334=VERTEX_POINT('',#145119);
#36335=VERTEX_POINT('',#145121);
#36336=VERTEX_POINT('',#145124);
#36337=VERTEX_POINT('',#145126);
#36338=VERTEX_POINT('',#145128);
#36339=VERTEX_POINT('',#145130);
#36340=VERTEX_POINT('',#145133);
#36341=VERTEX_POINT('',#145144);
#36342=VERTEX_POINT('',#145146);
#36343=VERTEX_POINT('',#145148);
#36344=VERTEX_POINT('',#145152);
#36345=VERTEX_POINT('',#145153);
#36346=VERTEX_POINT('',#145155);
#36347=VERTEX_POINT('',#145157);
#36348=VERTEX_POINT('',#145161);
#36349=VERTEX_POINT('',#145162);
#36350=VERTEX_POINT('',#145164);
#36351=VERTEX_POINT('',#145166);
#36352=VERTEX_POINT('',#145193);
#36353=VERTEX_POINT('',#145195);
#36354=VERTEX_POINT('',#145201);
#36355=VERTEX_POINT('',#145266);
#36356=VERTEX_POINT('',#145318);
#36357=VERTEX_POINT('',#145330);
#36358=VERTEX_POINT('',#145332);
#36359=VERTEX_POINT('',#145336);
#36360=VERTEX_POINT('',#145371);
#36361=VERTEX_POINT('',#145373);
#36362=VERTEX_POINT('',#145377);
#36363=VERTEX_POINT('',#145379);
#36364=VERTEX_POINT('',#145400);
#36365=VERTEX_POINT('',#145401);
#36366=VERTEX_POINT('',#145403);
#36367=VERTEX_POINT('',#145405);
#36368=VERTEX_POINT('',#145409);
#36369=VERTEX_POINT('',#145410);
#36370=VERTEX_POINT('',#145412);
#36371=VERTEX_POINT('',#145414);
#36372=VERTEX_POINT('',#145418);
#36373=VERTEX_POINT('',#145420);
#36374=VERTEX_POINT('',#145422);
#36375=VERTEX_POINT('',#145424);
#36376=VERTEX_POINT('',#145426);
#36377=VERTEX_POINT('',#145428);
#36378=VERTEX_POINT('',#145430);
#36379=VERTEX_POINT('',#145432);
#36380=VERTEX_POINT('',#145434);
#36381=VERTEX_POINT('',#145436);
#36382=VERTEX_POINT('',#145438);
#36383=VERTEX_POINT('',#145440);
#36384=VERTEX_POINT('',#145442);
#36385=VERTEX_POINT('',#145444);
#36386=VERTEX_POINT('',#145446);
#36387=VERTEX_POINT('',#145450);
#36388=VERTEX_POINT('',#145452);
#36389=VERTEX_POINT('',#145454);
#36390=VERTEX_POINT('',#145456);
#36391=VERTEX_POINT('',#145458);
#36392=VERTEX_POINT('',#145460);
#36393=VERTEX_POINT('',#145462);
#36394=VERTEX_POINT('',#145464);
#36395=VERTEX_POINT('',#145466);
#36396=VERTEX_POINT('',#145468);
#36397=VERTEX_POINT('',#145470);
#36398=VERTEX_POINT('',#145472);
#36399=VERTEX_POINT('',#145474);
#36400=VERTEX_POINT('',#145476);
#36401=VERTEX_POINT('',#145478);
#36402=VERTEX_POINT('',#145483);
#36403=VERTEX_POINT('',#145487);
#36404=VERTEX_POINT('',#145489);
#36405=VERTEX_POINT('',#145491);
#36406=VERTEX_POINT('',#145493);
#36407=VERTEX_POINT('',#145495);
#36408=VERTEX_POINT('',#145497);
#36409=VERTEX_POINT('',#145499);
#36410=VERTEX_POINT('',#145501);
#36411=VERTEX_POINT('',#145503);
#36412=VERTEX_POINT('',#145505);
#36413=VERTEX_POINT('',#145507);
#36414=VERTEX_POINT('',#145509);
#36415=VERTEX_POINT('',#145511);
#36416=VERTEX_POINT('',#145513);
#36417=VERTEX_POINT('',#145520);
#36418=VERTEX_POINT('',#145522);
#36419=VERTEX_POINT('',#145524);
#36420=VERTEX_POINT('',#145526);
#36421=VERTEX_POINT('',#145528);
#36422=VERTEX_POINT('',#145530);
#36423=VERTEX_POINT('',#145532);
#36424=VERTEX_POINT('',#145534);
#36425=VERTEX_POINT('',#145541);
#36426=VERTEX_POINT('',#145543);
#36427=VERTEX_POINT('',#145546);
#36428=VERTEX_POINT('',#145547);
#36429=VERTEX_POINT('',#145549);
#36430=VERTEX_POINT('',#145551);
#36431=VERTEX_POINT('',#145558);
#36432=VERTEX_POINT('',#145574);
#36433=VERTEX_POINT('',#145581);
#36434=VERTEX_POINT('',#145583);
#36435=VERTEX_POINT('',#145585);
#36436=VERTEX_POINT('',#145587);
#36437=VERTEX_POINT('',#145589);
#36438=VERTEX_POINT('',#145593);
#36439=VERTEX_POINT('',#145594);
#36440=VERTEX_POINT('',#145599);
#36441=VERTEX_POINT('',#145603);
#36442=VERTEX_POINT('',#145606);
#36443=VERTEX_POINT('',#145609);
#36444=VERTEX_POINT('',#145611);
#36445=VERTEX_POINT('',#145613);
#36446=VERTEX_POINT('',#145615);
#36447=VERTEX_POINT('',#145625);
#36448=VERTEX_POINT('',#145627);
#36449=VERTEX_POINT('',#145631);
#36450=VERTEX_POINT('',#145633);
#36451=VERTEX_POINT('',#145637);
#36452=VERTEX_POINT('',#145641);
#36453=VERTEX_POINT('',#145647);
#36454=VERTEX_POINT('',#145649);
#36455=VERTEX_POINT('',#145653);
#36456=VERTEX_POINT('',#145657);
#36457=VERTEX_POINT('',#145663);
#36458=VERTEX_POINT('',#145665);
#36459=VERTEX_POINT('',#145674);
#36460=VERTEX_POINT('',#145681);
#36461=VERTEX_POINT('',#145688);
#36462=VERTEX_POINT('',#145699);
#36463=VERTEX_POINT('',#145706);
#36464=VERTEX_POINT('',#145713);
#36465=VERTEX_POINT('',#145722);
#36466=VERTEX_POINT('',#145731);
#36467=VERTEX_POINT('',#145732);
#36468=VERTEX_POINT('',#145736);
#36469=VERTEX_POINT('',#145739);
#36470=VERTEX_POINT('',#145741);
#36471=VERTEX_POINT('',#145744);
#36472=VERTEX_POINT('',#145747);
#36473=VERTEX_POINT('',#145752);
#36474=VERTEX_POINT('',#145761);
#36475=VERTEX_POINT('',#145768);
#36476=VERTEX_POINT('',#145775);
#36477=VERTEX_POINT('',#145776);
#36478=VERTEX_POINT('',#145780);
#36479=VERTEX_POINT('',#145783);
#36480=VERTEX_POINT('',#145785);
#36481=VERTEX_POINT('',#145788);
#36482=VERTEX_POINT('',#145799);
#36483=VERTEX_POINT('',#145801);
#36484=VERTEX_POINT('',#145804);
#36485=VERTEX_POINT('',#145808);
#36486=VERTEX_POINT('',#145810);
#36487=VERTEX_POINT('',#145813);
#36488=VERTEX_POINT('',#145841);
#36489=VERTEX_POINT('',#145843);
#36490=VERTEX_POINT('',#145847);
#36491=VERTEX_POINT('',#145852);
#36492=VERTEX_POINT('',#145858);
#36493=VERTEX_POINT('',#145860);
#36494=VERTEX_POINT('',#145864);
#36495=VERTEX_POINT('',#145869);
#36496=VERTEX_POINT('',#145875);
#36497=VERTEX_POINT('',#145876);
#36498=VERTEX_POINT('',#145887);
#36499=VERTEX_POINT('',#145889);
#36500=VERTEX_POINT('',#145902);
#36501=VERTEX_POINT('',#145903);
#36502=VERTEX_POINT('',#145914);
#36503=VERTEX_POINT('',#145916);
#36504=VERTEX_POINT('',#145929);
#36505=VERTEX_POINT('',#145930);
#36506=VERTEX_POINT('',#145941);
#36507=VERTEX_POINT('',#145943);
#36508=VERTEX_POINT('',#145956);
#36509=VERTEX_POINT('',#145957);
#36510=VERTEX_POINT('',#145968);
#36511=VERTEX_POINT('',#145970);
#36512=VERTEX_POINT('',#145983);
#36513=VERTEX_POINT('',#145984);
#36514=VERTEX_POINT('',#145995);
#36515=VERTEX_POINT('',#145997);
#36516=VERTEX_POINT('',#146010);
#36517=VERTEX_POINT('',#146011);
#36518=VERTEX_POINT('',#146022);
#36519=VERTEX_POINT('',#146024);
#36520=VERTEX_POINT('',#146037);
#36521=VERTEX_POINT('',#146038);
#36522=VERTEX_POINT('',#146049);
#36523=VERTEX_POINT('',#146051);
#36524=VERTEX_POINT('',#146064);
#36525=VERTEX_POINT('',#146065);
#36526=VERTEX_POINT('',#146076);
#36527=VERTEX_POINT('',#146078);
#36528=VERTEX_POINT('',#146091);
#36529=VERTEX_POINT('',#146092);
#36530=VERTEX_POINT('',#146103);
#36531=VERTEX_POINT('',#146105);
#36532=VERTEX_POINT('',#146118);
#36533=VERTEX_POINT('',#146119);
#36534=VERTEX_POINT('',#146130);
#36535=VERTEX_POINT('',#146132);
#36536=VERTEX_POINT('',#146145);
#36537=VERTEX_POINT('',#146146);
#36538=VERTEX_POINT('',#146157);
#36539=VERTEX_POINT('',#146159);
#36540=VERTEX_POINT('',#146172);
#36541=VERTEX_POINT('',#146173);
#36542=VERTEX_POINT('',#146184);
#36543=VERTEX_POINT('',#146186);
#36544=VERTEX_POINT('',#146199);
#36545=VERTEX_POINT('',#146200);
#36546=VERTEX_POINT('',#146211);
#36547=VERTEX_POINT('',#146213);
#36548=VERTEX_POINT('',#146226);
#36549=VERTEX_POINT('',#146227);
#36550=VERTEX_POINT('',#146238);
#36551=VERTEX_POINT('',#146240);
#36552=VERTEX_POINT('',#146253);
#36553=VERTEX_POINT('',#146254);
#36554=VERTEX_POINT('',#146265);
#36555=VERTEX_POINT('',#146267);
#36556=VERTEX_POINT('',#146280);
#36557=VERTEX_POINT('',#146281);
#36558=VERTEX_POINT('',#146292);
#36559=VERTEX_POINT('',#146294);
#36560=VERTEX_POINT('',#146307);
#36561=VERTEX_POINT('',#146308);
#36562=VERTEX_POINT('',#146319);
#36563=VERTEX_POINT('',#146321);
#36564=VERTEX_POINT('',#146334);
#36565=VERTEX_POINT('',#146335);
#36566=VERTEX_POINT('',#146346);
#36567=VERTEX_POINT('',#146348);
#36568=VERTEX_POINT('',#146361);
#36569=VERTEX_POINT('',#146362);
#36570=VERTEX_POINT('',#146373);
#36571=VERTEX_POINT('',#146375);
#36572=VERTEX_POINT('',#146388);
#36573=VERTEX_POINT('',#146389);
#36574=VERTEX_POINT('',#146400);
#36575=VERTEX_POINT('',#146402);
#36576=VERTEX_POINT('',#146415);
#36577=VERTEX_POINT('',#146416);
#36578=VERTEX_POINT('',#146427);
#36579=VERTEX_POINT('',#146429);
#36580=VERTEX_POINT('',#146442);
#36581=VERTEX_POINT('',#146443);
#36582=VERTEX_POINT('',#146454);
#36583=VERTEX_POINT('',#146456);
#36584=VERTEX_POINT('',#146469);
#36585=VERTEX_POINT('',#146470);
#36586=VERTEX_POINT('',#146481);
#36587=VERTEX_POINT('',#146483);
#36588=VERTEX_POINT('',#146496);
#36589=VERTEX_POINT('',#146497);
#36590=VERTEX_POINT('',#146508);
#36591=VERTEX_POINT('',#146510);
#36592=VERTEX_POINT('',#146523);
#36593=VERTEX_POINT('',#146524);
#36594=VERTEX_POINT('',#146535);
#36595=VERTEX_POINT('',#146537);
#36596=VERTEX_POINT('',#146550);
#36597=VERTEX_POINT('',#146551);
#36598=VERTEX_POINT('',#146562);
#36599=VERTEX_POINT('',#146564);
#36600=VERTEX_POINT('',#146577);
#36601=VERTEX_POINT('',#146578);
#36602=VERTEX_POINT('',#146589);
#36603=VERTEX_POINT('',#146591);
#36604=VERTEX_POINT('',#146604);
#36605=VERTEX_POINT('',#146605);
#36606=VERTEX_POINT('',#146616);
#36607=VERTEX_POINT('',#146618);
#36608=VERTEX_POINT('',#146631);
#36609=VERTEX_POINT('',#146632);
#36610=VERTEX_POINT('',#146643);
#36611=VERTEX_POINT('',#146645);
#36612=VERTEX_POINT('',#146658);
#36613=VERTEX_POINT('',#146659);
#36614=VERTEX_POINT('',#146670);
#36615=VERTEX_POINT('',#146672);
#36616=VERTEX_POINT('',#146685);
#36617=VERTEX_POINT('',#146686);
#36618=VERTEX_POINT('',#146697);
#36619=VERTEX_POINT('',#146699);
#36620=VERTEX_POINT('',#146712);
#36621=VERTEX_POINT('',#146713);
#36622=VERTEX_POINT('',#146724);
#36623=VERTEX_POINT('',#146726);
#36624=VERTEX_POINT('',#146739);
#36625=VERTEX_POINT('',#146740);
#36626=VERTEX_POINT('',#146751);
#36627=VERTEX_POINT('',#146753);
#36628=VERTEX_POINT('',#146766);
#36629=VERTEX_POINT('',#146767);
#36630=VERTEX_POINT('',#146778);
#36631=VERTEX_POINT('',#146780);
#36632=VERTEX_POINT('',#146793);
#36633=VERTEX_POINT('',#146794);
#36634=VERTEX_POINT('',#146805);
#36635=VERTEX_POINT('',#146807);
#36636=VERTEX_POINT('',#146820);
#36637=VERTEX_POINT('',#146821);
#36638=VERTEX_POINT('',#146832);
#36639=VERTEX_POINT('',#146834);
#36640=VERTEX_POINT('',#146847);
#36641=VERTEX_POINT('',#146848);
#36642=VERTEX_POINT('',#146859);
#36643=VERTEX_POINT('',#146861);
#36644=VERTEX_POINT('',#146874);
#36645=VERTEX_POINT('',#146875);
#36646=VERTEX_POINT('',#146886);
#36647=VERTEX_POINT('',#146888);
#36648=VERTEX_POINT('',#146901);
#36649=VERTEX_POINT('',#146902);
#36650=VERTEX_POINT('',#146913);
#36651=VERTEX_POINT('',#146915);
#36652=VERTEX_POINT('',#146928);
#36653=VERTEX_POINT('',#146929);
#36654=VERTEX_POINT('',#146940);
#36655=VERTEX_POINT('',#146942);
#36656=VERTEX_POINT('',#146955);
#36657=VERTEX_POINT('',#146956);
#36658=VERTEX_POINT('',#146967);
#36659=VERTEX_POINT('',#146969);
#36660=VERTEX_POINT('',#146982);
#36661=VERTEX_POINT('',#146983);
#36662=VERTEX_POINT('',#146994);
#36663=VERTEX_POINT('',#146996);
#36664=VERTEX_POINT('',#147009);
#36665=VERTEX_POINT('',#147010);
#36666=VERTEX_POINT('',#147021);
#36667=VERTEX_POINT('',#147023);
#36668=VERTEX_POINT('',#147036);
#36669=VERTEX_POINT('',#147037);
#36670=VERTEX_POINT('',#147048);
#36671=VERTEX_POINT('',#147050);
#36672=VERTEX_POINT('',#147063);
#36673=VERTEX_POINT('',#147064);
#36674=VERTEX_POINT('',#147075);
#36675=VERTEX_POINT('',#147077);
#36676=VERTEX_POINT('',#147090);
#36677=VERTEX_POINT('',#147091);
#36678=VERTEX_POINT('',#147102);
#36679=VERTEX_POINT('',#147104);
#36680=VERTEX_POINT('',#147117);
#36681=VERTEX_POINT('',#147118);
#36682=VERTEX_POINT('',#147129);
#36683=VERTEX_POINT('',#147131);
#36684=VERTEX_POINT('',#147144);
#36685=VERTEX_POINT('',#147145);
#36686=VERTEX_POINT('',#147156);
#36687=VERTEX_POINT('',#147158);
#36688=VERTEX_POINT('',#147171);
#36689=VERTEX_POINT('',#147172);
#36690=VERTEX_POINT('',#147183);
#36691=VERTEX_POINT('',#147185);
#36692=VERTEX_POINT('',#147198);
#36693=VERTEX_POINT('',#147199);
#36694=VERTEX_POINT('',#147210);
#36695=VERTEX_POINT('',#147212);
#36696=VERTEX_POINT('',#147225);
#36697=VERTEX_POINT('',#147226);
#36698=VERTEX_POINT('',#147237);
#36699=VERTEX_POINT('',#147239);
#36700=VERTEX_POINT('',#147252);
#36701=VERTEX_POINT('',#147253);
#36702=VERTEX_POINT('',#147264);
#36703=VERTEX_POINT('',#147266);
#36704=VERTEX_POINT('',#147279);
#36705=VERTEX_POINT('',#147280);
#36706=VERTEX_POINT('',#147291);
#36707=VERTEX_POINT('',#147293);
#36708=VERTEX_POINT('',#147306);
#36709=VERTEX_POINT('',#147307);
#36710=VERTEX_POINT('',#147318);
#36711=VERTEX_POINT('',#147320);
#36712=VERTEX_POINT('',#147333);
#36713=VERTEX_POINT('',#147334);
#36714=VERTEX_POINT('',#147345);
#36715=VERTEX_POINT('',#147347);
#36716=VERTEX_POINT('',#147360);
#36717=VERTEX_POINT('',#147361);
#36718=VERTEX_POINT('',#147372);
#36719=VERTEX_POINT('',#147374);
#36720=VERTEX_POINT('',#147387);
#36721=VERTEX_POINT('',#147388);
#36722=VERTEX_POINT('',#147399);
#36723=VERTEX_POINT('',#147401);
#36724=VERTEX_POINT('',#147414);
#36725=VERTEX_POINT('',#147415);
#36726=VERTEX_POINT('',#147426);
#36727=VERTEX_POINT('',#147428);
#36728=VERTEX_POINT('',#147441);
#36729=VERTEX_POINT('',#147442);
#36730=VERTEX_POINT('',#147453);
#36731=VERTEX_POINT('',#147455);
#36732=VERTEX_POINT('',#147468);
#36733=VERTEX_POINT('',#147469);
#36734=VERTEX_POINT('',#147480);
#36735=VERTEX_POINT('',#147482);
#36736=VERTEX_POINT('',#147495);
#36737=VERTEX_POINT('',#147496);
#36738=VERTEX_POINT('',#147507);
#36739=VERTEX_POINT('',#147509);
#36740=VERTEX_POINT('',#147522);
#36741=VERTEX_POINT('',#147523);
#36742=VERTEX_POINT('',#147534);
#36743=VERTEX_POINT('',#147536);
#36744=VERTEX_POINT('',#147549);
#36745=VERTEX_POINT('',#147550);
#36746=VERTEX_POINT('',#147561);
#36747=VERTEX_POINT('',#147563);
#36748=VERTEX_POINT('',#147576);
#36749=VERTEX_POINT('',#147577);
#36750=VERTEX_POINT('',#147588);
#36751=VERTEX_POINT('',#147590);
#36752=VERTEX_POINT('',#147603);
#36753=VERTEX_POINT('',#147604);
#36754=VERTEX_POINT('',#147615);
#36755=VERTEX_POINT('',#147617);
#36756=VERTEX_POINT('',#147630);
#36757=VERTEX_POINT('',#147631);
#36758=VERTEX_POINT('',#147642);
#36759=VERTEX_POINT('',#147644);
#36760=VERTEX_POINT('',#147657);
#36761=VERTEX_POINT('',#147658);
#36762=VERTEX_POINT('',#147669);
#36763=VERTEX_POINT('',#147671);
#36764=VERTEX_POINT('',#147684);
#36765=VERTEX_POINT('',#147685);
#36766=VERTEX_POINT('',#147696);
#36767=VERTEX_POINT('',#147698);
#36768=VERTEX_POINT('',#147711);
#36769=VERTEX_POINT('',#147712);
#36770=VERTEX_POINT('',#147723);
#36771=VERTEX_POINT('',#147725);
#36772=VERTEX_POINT('',#147738);
#36773=VERTEX_POINT('',#147739);
#36774=VERTEX_POINT('',#147750);
#36775=VERTEX_POINT('',#147752);
#36776=VERTEX_POINT('',#147765);
#36777=VERTEX_POINT('',#147766);
#36778=VERTEX_POINT('',#147768);
#36779=VERTEX_POINT('',#147773);
#36780=VERTEX_POINT('',#147774);
#36781=VERTEX_POINT('',#147776);
#36782=VERTEX_POINT('',#147781);
#36783=VERTEX_POINT('',#147782);
#36784=VERTEX_POINT('',#147784);
#36785=VERTEX_POINT('',#147789);
#36786=VERTEX_POINT('',#147790);
#36787=VERTEX_POINT('',#147792);
#36788=VERTEX_POINT('',#147797);
#36789=VERTEX_POINT('',#147799);
#36790=VERTEX_POINT('',#147803);
#36791=VERTEX_POINT('',#147805);
#36792=VERTEX_POINT('',#147809);
#36793=VERTEX_POINT('',#147810);
#36794=VERTEX_POINT('',#147812);
#36795=VERTEX_POINT('',#147817);
#36796=VERTEX_POINT('',#147819);
#36797=VERTEX_POINT('',#147827);
#36798=VERTEX_POINT('',#147828);
#36799=VERTEX_POINT('',#147850);
#36800=VERTEX_POINT('',#147855);
#36801=VERTEX_POINT('',#147877);
#36802=VERTEX_POINT('',#147882);
#36803=VERTEX_POINT('',#147904);
#36804=VERTEX_POINT('',#147909);
#36805=VERTEX_POINT('',#147931);
#36806=VERTEX_POINT('',#147936);
#36807=VERTEX_POINT('',#147958);
#36808=VERTEX_POINT('',#147963);
#36809=VERTEX_POINT('',#147985);
#36810=VERTEX_POINT('',#147990);
#36811=VERTEX_POINT('',#148012);
#36812=VERTEX_POINT('',#148017);
#36813=VERTEX_POINT('',#148039);
#36814=VERTEX_POINT('',#148044);
#36815=VERTEX_POINT('',#148066);
#36816=VERTEX_POINT('',#148071);
#36817=VERTEX_POINT('',#148093);
#36818=VERTEX_POINT('',#148098);
#36819=VERTEX_POINT('',#148120);
#36820=VERTEX_POINT('',#148125);
#36821=VERTEX_POINT('',#148147);
#36822=VERTEX_POINT('',#148152);
#36823=VERTEX_POINT('',#148174);
#36824=VERTEX_POINT('',#148179);
#36825=VERTEX_POINT('',#148201);
#36826=VERTEX_POINT('',#148206);
#36827=VERTEX_POINT('',#148228);
#36828=VERTEX_POINT('',#148233);
#36829=VERTEX_POINT('',#148255);
#36830=VERTEX_POINT('',#148260);
#36831=VERTEX_POINT('',#148282);
#36832=VERTEX_POINT('',#148287);
#36833=VERTEX_POINT('',#148309);
#36834=VERTEX_POINT('',#148314);
#36835=VERTEX_POINT('',#148336);
#36836=VERTEX_POINT('',#148341);
#36837=VERTEX_POINT('',#148363);
#36838=VERTEX_POINT('',#148368);
#36839=VERTEX_POINT('',#148390);
#36840=VERTEX_POINT('',#148395);
#36841=VERTEX_POINT('',#148417);
#36842=VERTEX_POINT('',#148422);
#36843=VERTEX_POINT('',#148444);
#36844=VERTEX_POINT('',#148449);
#36845=VERTEX_POINT('',#148471);
#36846=VERTEX_POINT('',#148476);
#36847=VERTEX_POINT('',#148498);
#36848=VERTEX_POINT('',#148503);
#36849=VERTEX_POINT('',#148525);
#36850=VERTEX_POINT('',#148530);
#36851=VERTEX_POINT('',#148552);
#36852=VERTEX_POINT('',#148557);
#36853=VERTEX_POINT('',#148579);
#36854=VERTEX_POINT('',#148584);
#36855=VERTEX_POINT('',#148606);
#36856=VERTEX_POINT('',#148611);
#36857=VERTEX_POINT('',#148633);
#36858=VERTEX_POINT('',#148638);
#36859=VERTEX_POINT('',#148660);
#36860=VERTEX_POINT('',#148665);
#36861=VERTEX_POINT('',#148687);
#36862=VERTEX_POINT('',#148692);
#36863=VERTEX_POINT('',#148714);
#36864=VERTEX_POINT('',#148719);
#36865=VERTEX_POINT('',#148741);
#36866=VERTEX_POINT('',#148746);
#36867=VERTEX_POINT('',#148768);
#36868=VERTEX_POINT('',#148773);
#36869=VERTEX_POINT('',#148784);
#36870=VERTEX_POINT('',#148787);
#36871=VERTEX_POINT('',#148800);
#36872=VERTEX_POINT('',#148805);
#36873=VERTEX_POINT('',#148827);
#36874=VERTEX_POINT('',#148832);
#36875=VERTEX_POINT('',#148854);
#36876=VERTEX_POINT('',#148859);
#36877=VERTEX_POINT('',#148881);
#36878=VERTEX_POINT('',#148886);
#36879=VERTEX_POINT('',#148908);
#36880=VERTEX_POINT('',#148913);
#36881=VERTEX_POINT('',#148935);
#36882=VERTEX_POINT('',#148940);
#36883=VERTEX_POINT('',#148962);
#36884=VERTEX_POINT('',#148967);
#36885=VERTEX_POINT('',#148989);
#36886=VERTEX_POINT('',#148994);
#36887=VERTEX_POINT('',#149016);
#36888=VERTEX_POINT('',#149021);
#36889=VERTEX_POINT('',#149043);
#36890=VERTEX_POINT('',#149048);
#36891=VERTEX_POINT('',#149070);
#36892=VERTEX_POINT('',#149075);
#36893=VERTEX_POINT('',#149097);
#36894=VERTEX_POINT('',#149102);
#36895=VERTEX_POINT('',#149124);
#36896=VERTEX_POINT('',#149129);
#36897=VERTEX_POINT('',#149151);
#36898=VERTEX_POINT('',#149156);
#36899=VERTEX_POINT('',#149178);
#36900=VERTEX_POINT('',#149183);
#36901=VERTEX_POINT('',#149205);
#36902=VERTEX_POINT('',#149210);
#36903=VERTEX_POINT('',#149232);
#36904=VERTEX_POINT('',#149237);
#36905=VERTEX_POINT('',#149259);
#36906=VERTEX_POINT('',#149264);
#36907=VERTEX_POINT('',#149286);
#36908=VERTEX_POINT('',#149291);
#36909=VERTEX_POINT('',#149313);
#36910=VERTEX_POINT('',#149318);
#36911=VERTEX_POINT('',#149340);
#36912=VERTEX_POINT('',#149345);
#36913=VERTEX_POINT('',#149367);
#36914=VERTEX_POINT('',#149372);
#36915=VERTEX_POINT('',#149394);
#36916=VERTEX_POINT('',#149399);
#36917=VERTEX_POINT('',#149421);
#36918=VERTEX_POINT('',#149426);
#36919=VERTEX_POINT('',#149448);
#36920=VERTEX_POINT('',#149453);
#36921=VERTEX_POINT('',#149475);
#36922=VERTEX_POINT('',#149480);
#36923=VERTEX_POINT('',#149502);
#36924=VERTEX_POINT('',#149507);
#36925=VERTEX_POINT('',#149529);
#36926=VERTEX_POINT('',#149534);
#36927=VERTEX_POINT('',#149556);
#36928=VERTEX_POINT('',#149561);
#36929=VERTEX_POINT('',#149583);
#36930=VERTEX_POINT('',#149588);
#36931=VERTEX_POINT('',#149610);
#36932=VERTEX_POINT('',#149615);
#36933=VERTEX_POINT('',#149637);
#36934=VERTEX_POINT('',#149642);
#36935=VERTEX_POINT('',#149664);
#36936=VERTEX_POINT('',#149669);
#36937=VERTEX_POINT('',#149691);
#36938=VERTEX_POINT('',#149696);
#36939=VERTEX_POINT('',#149723);
#36940=VERTEX_POINT('',#149725);
#36941=VERTEX_POINT('',#149742);
#36942=VERTEX_POINT('',#149749);
#36943=VERTEX_POINT('',#149775);
#36944=VERTEX_POINT('',#149782);
#36945=VERTEX_POINT('',#149808);
#36946=VERTEX_POINT('',#149815);
#36947=VERTEX_POINT('',#149841);
#36948=VERTEX_POINT('',#149848);
#36949=VERTEX_POINT('',#149874);
#36950=VERTEX_POINT('',#149881);
#36951=VERTEX_POINT('',#149907);
#36952=VERTEX_POINT('',#149914);
#36953=VERTEX_POINT('',#149940);
#36954=VERTEX_POINT('',#149947);
#36955=VERTEX_POINT('',#149973);
#36956=VERTEX_POINT('',#149980);
#36957=VERTEX_POINT('',#150006);
#36958=VERTEX_POINT('',#150013);
#36959=VERTEX_POINT('',#150039);
#36960=VERTEX_POINT('',#150046);
#36961=VERTEX_POINT('',#150072);
#36962=VERTEX_POINT('',#150079);
#36963=VERTEX_POINT('',#150105);
#36964=VERTEX_POINT('',#150112);
#36965=VERTEX_POINT('',#150138);
#36966=VERTEX_POINT('',#150145);
#36967=VERTEX_POINT('',#150171);
#36968=VERTEX_POINT('',#150178);
#36969=VERTEX_POINT('',#150204);
#36970=VERTEX_POINT('',#150211);
#36971=VERTEX_POINT('',#150237);
#36972=VERTEX_POINT('',#150244);
#36973=VERTEX_POINT('',#150270);
#36974=VERTEX_POINT('',#150277);
#36975=VERTEX_POINT('',#150303);
#36976=VERTEX_POINT('',#150310);
#36977=VERTEX_POINT('',#150336);
#36978=VERTEX_POINT('',#150343);
#36979=VERTEX_POINT('',#150369);
#36980=VERTEX_POINT('',#150376);
#36981=VERTEX_POINT('',#150402);
#36982=VERTEX_POINT('',#150409);
#36983=VERTEX_POINT('',#150435);
#36984=VERTEX_POINT('',#150442);
#36985=VERTEX_POINT('',#150468);
#36986=VERTEX_POINT('',#150475);
#36987=VERTEX_POINT('',#150501);
#36988=VERTEX_POINT('',#150508);
#36989=VERTEX_POINT('',#150534);
#36990=VERTEX_POINT('',#150541);
#36991=VERTEX_POINT('',#150567);
#36992=VERTEX_POINT('',#150574);
#36993=VERTEX_POINT('',#150600);
#36994=VERTEX_POINT('',#150607);
#36995=VERTEX_POINT('',#150633);
#36996=VERTEX_POINT('',#150640);
#36997=VERTEX_POINT('',#150666);
#36998=VERTEX_POINT('',#150673);
#36999=VERTEX_POINT('',#150699);
#37000=VERTEX_POINT('',#150706);
#37001=VERTEX_POINT('',#150732);
#37002=VERTEX_POINT('',#150739);
#37003=VERTEX_POINT('',#150765);
#37004=VERTEX_POINT('',#150772);
#37005=VERTEX_POINT('',#150798);
#37006=VERTEX_POINT('',#150805);
#37007=VERTEX_POINT('',#150831);
#37008=VERTEX_POINT('',#150838);
#37009=VERTEX_POINT('',#150864);
#37010=VERTEX_POINT('',#150871);
#37011=VERTEX_POINT('',#150897);
#37012=VERTEX_POINT('',#150904);
#37013=VERTEX_POINT('',#150930);
#37014=VERTEX_POINT('',#150937);
#37015=VERTEX_POINT('',#150963);
#37016=VERTEX_POINT('',#150970);
#37017=VERTEX_POINT('',#150996);
#37018=VERTEX_POINT('',#151003);
#37019=VERTEX_POINT('',#151029);
#37020=VERTEX_POINT('',#151036);
#37021=VERTEX_POINT('',#151062);
#37022=VERTEX_POINT('',#151069);
#37023=VERTEX_POINT('',#151095);
#37024=VERTEX_POINT('',#151102);
#37025=VERTEX_POINT('',#151128);
#37026=VERTEX_POINT('',#151135);
#37027=VERTEX_POINT('',#151161);
#37028=VERTEX_POINT('',#151168);
#37029=VERTEX_POINT('',#151194);
#37030=VERTEX_POINT('',#151201);
#37031=VERTEX_POINT('',#151227);
#37032=VERTEX_POINT('',#151234);
#37033=VERTEX_POINT('',#151260);
#37034=VERTEX_POINT('',#151267);
#37035=VERTEX_POINT('',#151293);
#37036=VERTEX_POINT('',#151300);
#37037=VERTEX_POINT('',#151326);
#37038=VERTEX_POINT('',#151333);
#37039=VERTEX_POINT('',#151359);
#37040=VERTEX_POINT('',#151366);
#37041=VERTEX_POINT('',#151392);
#37042=VERTEX_POINT('',#151399);
#37043=VERTEX_POINT('',#151425);
#37044=VERTEX_POINT('',#151432);
#37045=VERTEX_POINT('',#151458);
#37046=VERTEX_POINT('',#151465);
#37047=VERTEX_POINT('',#151491);
#37048=VERTEX_POINT('',#151498);
#37049=VERTEX_POINT('',#151524);
#37050=VERTEX_POINT('',#151531);
#37051=VERTEX_POINT('',#151557);
#37052=VERTEX_POINT('',#151564);
#37053=VERTEX_POINT('',#151590);
#37054=VERTEX_POINT('',#151597);
#37055=VERTEX_POINT('',#151623);
#37056=VERTEX_POINT('',#151630);
#37057=VERTEX_POINT('',#151656);
#37058=VERTEX_POINT('',#151663);
#37059=VERTEX_POINT('',#151689);
#37060=VERTEX_POINT('',#151696);
#37061=VERTEX_POINT('',#151722);
#37062=VERTEX_POINT('',#151729);
#37063=VERTEX_POINT('',#151755);
#37064=VERTEX_POINT('',#151762);
#37065=VERTEX_POINT('',#151788);
#37066=VERTEX_POINT('',#151795);
#37067=VERTEX_POINT('',#151821);
#37068=VERTEX_POINT('',#151828);
#37069=VERTEX_POINT('',#151854);
#37070=VERTEX_POINT('',#151861);
#37071=VERTEX_POINT('',#151887);
#37072=VERTEX_POINT('',#151894);
#37073=VERTEX_POINT('',#151920);
#37074=VERTEX_POINT('',#151927);
#37075=VERTEX_POINT('',#151953);
#37076=VERTEX_POINT('',#151960);
#37077=VERTEX_POINT('',#151986);
#37078=VERTEX_POINT('',#151993);
#37079=VERTEX_POINT('',#152019);
#37080=VERTEX_POINT('',#152037);
#37081=VERTEX_POINT('',#152396);
#37082=VERTEX_POINT('',#152398);
#37083=VERTEX_POINT('',#152402);
#37084=VERTEX_POINT('',#152404);
#37085=VERTEX_POINT('',#152408);
#37086=VERTEX_POINT('',#152410);
#37087=VERTEX_POINT('',#152414);
#37088=VERTEX_POINT('',#152416);
#37089=VERTEX_POINT('',#152420);
#37090=VERTEX_POINT('',#152421);
#37091=VERTEX_POINT('',#152423);
#37092=VERTEX_POINT('',#152428);
#37093=VERTEX_POINT('',#152430);
#37094=VERTEX_POINT('',#152434);
#37095=VERTEX_POINT('',#152436);
#37096=VERTEX_POINT('',#152438);
#37097=VERTEX_POINT('',#152442);
#37098=VERTEX_POINT('',#152443);
#37099=VERTEX_POINT('',#152445);
#37100=VERTEX_POINT('',#152447);
#37101=VERTEX_POINT('',#152451);
#37102=VERTEX_POINT('',#152452);
#37103=VERTEX_POINT('',#152454);
#37104=VERTEX_POINT('',#152456);
#37105=VERTEX_POINT('',#152460);
#37106=VERTEX_POINT('',#152462);
#37107=VERTEX_POINT('',#152464);
#37108=VERTEX_POINT('',#152468);
#37109=VERTEX_POINT('',#152470);
#37110=VERTEX_POINT('',#152472);
#37111=VERTEX_POINT('',#152476);
#37112=VERTEX_POINT('',#152478);
#37113=VERTEX_POINT('',#152480);
#37114=VERTEX_POINT('',#152484);
#37115=VERTEX_POINT('',#152485);
#37116=VERTEX_POINT('',#152487);
#37117=VERTEX_POINT('',#152489);
#37118=VERTEX_POINT('',#152493);
#37119=VERTEX_POINT('',#152494);
#37120=VERTEX_POINT('',#152496);
#37121=VERTEX_POINT('',#152498);
#37122=VERTEX_POINT('',#152502);
#37123=VERTEX_POINT('',#152510);
#37124=VERTEX_POINT('',#152514);
#37125=VERTEX_POINT('',#152515);
#37126=VERTEX_POINT('',#152517);
#37127=VERTEX_POINT('',#152519);
#37128=VERTEX_POINT('',#152523);
#37129=VERTEX_POINT('',#152524);
#37130=VERTEX_POINT('',#152526);
#37131=VERTEX_POINT('',#152528);
#37132=VERTEX_POINT('',#152532);
#37133=VERTEX_POINT('',#152533);
#37134=VERTEX_POINT('',#152535);
#37135=VERTEX_POINT('',#152537);
#37136=VERTEX_POINT('',#152541);
#37137=VERTEX_POINT('',#152542);
#37138=VERTEX_POINT('',#152544);
#37139=VERTEX_POINT('',#152546);
#37140=VERTEX_POINT('',#152552);
#37141=VERTEX_POINT('',#152553);
#37142=VERTEX_POINT('',#152555);
#37143=VERTEX_POINT('',#152557);
#37144=VERTEX_POINT('',#152559);
#37145=VERTEX_POINT('',#152561);
#37146=VERTEX_POINT('',#152563);
#37147=VERTEX_POINT('',#152565);
#37148=VERTEX_POINT('',#152567);
#37149=VERTEX_POINT('',#152569);
#37150=VERTEX_POINT('',#152571);
#37151=VERTEX_POINT('',#152573);
#37152=VERTEX_POINT('',#152575);
#37153=VERTEX_POINT('',#152577);
#37154=VERTEX_POINT('',#152579);
#37155=VERTEX_POINT('',#152581);
#37156=VERTEX_POINT('',#152583);
#37157=VERTEX_POINT('',#152585);
#37158=VERTEX_POINT('',#152587);
#37159=VERTEX_POINT('',#152589);
#37160=VERTEX_POINT('',#152591);
#37161=VERTEX_POINT('',#152593);
#37162=VERTEX_POINT('',#152595);
#37163=VERTEX_POINT('',#152597);
#37164=VERTEX_POINT('',#152599);
#37165=VERTEX_POINT('',#152601);
#37166=VERTEX_POINT('',#152603);
#37167=VERTEX_POINT('',#152605);
#37168=VERTEX_POINT('',#152607);
#37169=VERTEX_POINT('',#152609);
#37170=VERTEX_POINT('',#152612);
#37171=VERTEX_POINT('',#152614);
#37172=VERTEX_POINT('',#152617);
#37173=VERTEX_POINT('',#152619);
#37174=VERTEX_POINT('',#152621);
#37175=VERTEX_POINT('',#152623);
#37176=VERTEX_POINT('',#152625);
#37177=VERTEX_POINT('',#152627);
#37178=VERTEX_POINT('',#152629);
#37179=VERTEX_POINT('',#152631);
#37180=VERTEX_POINT('',#152633);
#37181=VERTEX_POINT('',#152635);
#37182=VERTEX_POINT('',#152637);
#37183=VERTEX_POINT('',#152639);
#37184=VERTEX_POINT('',#152641);
#37185=VERTEX_POINT('',#152643);
#37186=VERTEX_POINT('',#152645);
#37187=VERTEX_POINT('',#152647);
#37188=VERTEX_POINT('',#152649);
#37189=VERTEX_POINT('',#152651);
#37190=VERTEX_POINT('',#152653);
#37191=VERTEX_POINT('',#152655);
#37192=VERTEX_POINT('',#152657);
#37193=VERTEX_POINT('',#152659);
#37194=VERTEX_POINT('',#152661);
#37195=VERTEX_POINT('',#152663);
#37196=VERTEX_POINT('',#152665);
#37197=VERTEX_POINT('',#152667);
#37198=VERTEX_POINT('',#152669);
#37199=VERTEX_POINT('',#152671);
#37200=VERTEX_POINT('',#152673);
#37201=VERTEX_POINT('',#152675);
#37202=VERTEX_POINT('',#152677);
#37203=VERTEX_POINT('',#152679);
#37204=VERTEX_POINT('',#152681);
#37205=VERTEX_POINT('',#152683);
#37206=VERTEX_POINT('',#152685);
#37207=VERTEX_POINT('',#152687);
#37208=VERTEX_POINT('',#152689);
#37209=VERTEX_POINT('',#152691);
#37210=VERTEX_POINT('',#152693);
#37211=VERTEX_POINT('',#152695);
#37212=VERTEX_POINT('',#152697);
#37213=VERTEX_POINT('',#152699);
#37214=VERTEX_POINT('',#152701);
#37215=VERTEX_POINT('',#152703);
#37216=VERTEX_POINT('',#152705);
#37217=VERTEX_POINT('',#152707);
#37218=VERTEX_POINT('',#152709);
#37219=VERTEX_POINT('',#152711);
#37220=VERTEX_POINT('',#152713);
#37221=VERTEX_POINT('',#152715);
#37222=VERTEX_POINT('',#152717);
#37223=VERTEX_POINT('',#152719);
#37224=VERTEX_POINT('',#152721);
#37225=VERTEX_POINT('',#152723);
#37226=VERTEX_POINT('',#152725);
#37227=VERTEX_POINT('',#152727);
#37228=VERTEX_POINT('',#152729);
#37229=VERTEX_POINT('',#152731);
#37230=VERTEX_POINT('',#152733);
#37231=VERTEX_POINT('',#152735);
#37232=VERTEX_POINT('',#152737);
#37233=VERTEX_POINT('',#152739);
#37234=VERTEX_POINT('',#152741);
#37235=VERTEX_POINT('',#152743);
#37236=VERTEX_POINT('',#152745);
#37237=VERTEX_POINT('',#152747);
#37238=VERTEX_POINT('',#152749);
#37239=VERTEX_POINT('',#152751);
#37240=VERTEX_POINT('',#152753);
#37241=VERTEX_POINT('',#152755);
#37242=VERTEX_POINT('',#152757);
#37243=VERTEX_POINT('',#152759);
#37244=VERTEX_POINT('',#152761);
#37245=VERTEX_POINT('',#152763);
#37246=VERTEX_POINT('',#152765);
#37247=VERTEX_POINT('',#152767);
#37248=VERTEX_POINT('',#152769);
#37249=VERTEX_POINT('',#152771);
#37250=VERTEX_POINT('',#152773);
#37251=VERTEX_POINT('',#152775);
#37252=VERTEX_POINT('',#152777);
#37253=VERTEX_POINT('',#152779);
#37254=VERTEX_POINT('',#152781);
#37255=VERTEX_POINT('',#152783);
#37256=VERTEX_POINT('',#152786);
#37257=VERTEX_POINT('',#152788);
#37258=VERTEX_POINT('',#152791);
#37259=VERTEX_POINT('',#152793);
#37260=VERTEX_POINT('',#152795);
#37261=VERTEX_POINT('',#152797);
#37262=VERTEX_POINT('',#152799);
#37263=VERTEX_POINT('',#152801);
#37264=VERTEX_POINT('',#152803);
#37265=VERTEX_POINT('',#152805);
#37266=VERTEX_POINT('',#152807);
#37267=VERTEX_POINT('',#152809);
#37268=VERTEX_POINT('',#152811);
#37269=VERTEX_POINT('',#152813);
#37270=VERTEX_POINT('',#152815);
#37271=VERTEX_POINT('',#152817);
#37272=VERTEX_POINT('',#152819);
#37273=VERTEX_POINT('',#152821);
#37274=VERTEX_POINT('',#152823);
#37275=VERTEX_POINT('',#152825);
#37276=VERTEX_POINT('',#152827);
#37277=VERTEX_POINT('',#152829);
#37278=VERTEX_POINT('',#152831);
#37279=VERTEX_POINT('',#152833);
#37280=VERTEX_POINT('',#152836);
#37281=VERTEX_POINT('',#152837);
#37282=VERTEX_POINT('',#152839);
#37283=VERTEX_POINT('',#152842);
#37284=VERTEX_POINT('',#152844);
#37285=VERTEX_POINT('',#152846);
#37286=VERTEX_POINT('',#152849);
#37287=VERTEX_POINT('',#152850);
#37288=VERTEX_POINT('',#152852);
#37289=VERTEX_POINT('',#152855);
#37290=VERTEX_POINT('',#152857);
#37291=VERTEX_POINT('',#152859);
#37292=VERTEX_POINT('',#152863);
#37293=VERTEX_POINT('',#152865);
#37294=VERTEX_POINT('',#152869);
#37295=VERTEX_POINT('',#152871);
#37296=VERTEX_POINT('',#152875);
#37297=VERTEX_POINT('',#152877);
#37298=VERTEX_POINT('',#152881);
#37299=VERTEX_POINT('',#152883);
#37300=VERTEX_POINT('',#152887);
#37301=VERTEX_POINT('',#152889);
#37302=VERTEX_POINT('',#152893);
#37303=VERTEX_POINT('',#152897);
#37304=VERTEX_POINT('',#152901);
#37305=VERTEX_POINT('',#152903);
#37306=VERTEX_POINT('',#152907);
#37307=VERTEX_POINT('',#152909);
#37308=VERTEX_POINT('',#152913);
#37309=VERTEX_POINT('',#152915);
#37310=VERTEX_POINT('',#152919);
#37311=VERTEX_POINT('',#152921);
#37312=VERTEX_POINT('',#152925);
#37313=VERTEX_POINT('',#152927);
#37314=VERTEX_POINT('',#152931);
#37315=VERTEX_POINT('',#152935);
#37316=VERTEX_POINT('',#152939);
#37317=VERTEX_POINT('',#152941);
#37318=VERTEX_POINT('',#152945);
#37319=VERTEX_POINT('',#152947);
#37320=VERTEX_POINT('',#152951);
#37321=VERTEX_POINT('',#152953);
#37322=VERTEX_POINT('',#152957);
#37323=VERTEX_POINT('',#152959);
#37324=VERTEX_POINT('',#152963);
#37325=VERTEX_POINT('',#152965);
#37326=VERTEX_POINT('',#152969);
#37327=VERTEX_POINT('',#152971);
#37328=VERTEX_POINT('',#152975);
#37329=VERTEX_POINT('',#152977);
#37330=VERTEX_POINT('',#152981);
#37331=VERTEX_POINT('',#152983);
#37332=VERTEX_POINT('',#152987);
#37333=VERTEX_POINT('',#152989);
#37334=VERTEX_POINT('',#152993);
#37335=VERTEX_POINT('',#152995);
#37336=VERTEX_POINT('',#152999);
#37337=VERTEX_POINT('',#153001);
#37338=VERTEX_POINT('',#153005);
#37339=VERTEX_POINT('',#153007);
#37340=VERTEX_POINT('',#153011);
#37341=VERTEX_POINT('',#153013);
#37342=VERTEX_POINT('',#153017);
#37343=VERTEX_POINT('',#153019);
#37344=VERTEX_POINT('',#153023);
#37345=VERTEX_POINT('',#153025);
#37346=VERTEX_POINT('',#153029);
#37347=VERTEX_POINT('',#153031);
#37348=VERTEX_POINT('',#153035);
#37349=VERTEX_POINT('',#153037);
#37350=VERTEX_POINT('',#153041);
#37351=VERTEX_POINT('',#153043);
#37352=VERTEX_POINT('',#153047);
#37353=VERTEX_POINT('',#153049);
#37354=VERTEX_POINT('',#153053);
#37355=VERTEX_POINT('',#153055);
#37356=VERTEX_POINT('',#153059);
#37357=VERTEX_POINT('',#153061);
#37358=VERTEX_POINT('',#153065);
#37359=VERTEX_POINT('',#153067);
#37360=VERTEX_POINT('',#153071);
#37361=VERTEX_POINT('',#153073);
#37362=VERTEX_POINT('',#153075);
#37363=VERTEX_POINT('',#153078);
#37364=VERTEX_POINT('',#153080);
#37365=VERTEX_POINT('',#153083);
#37366=VERTEX_POINT('',#153085);
#37367=VERTEX_POINT('',#153088);
#37368=VERTEX_POINT('',#153090);
#37369=VERTEX_POINT('',#153093);
#37370=VERTEX_POINT('',#153095);
#37371=VERTEX_POINT('',#153098);
#37372=VERTEX_POINT('',#153101);
#37373=VERTEX_POINT('',#153104);
#37374=VERTEX_POINT('',#153106);
#37375=VERTEX_POINT('',#153108);
#37376=VERTEX_POINT('',#153110);
#37377=VERTEX_POINT('',#153112);
#37378=VERTEX_POINT('',#153114);
#37379=VERTEX_POINT('',#153117);
#37380=VERTEX_POINT('',#153119);
#37381=VERTEX_POINT('',#153122);
#37382=VERTEX_POINT('',#153124);
#37383=VERTEX_POINT('',#153127);
#37384=VERTEX_POINT('',#153129);
#37385=VERTEX_POINT('',#153132);
#37386=VERTEX_POINT('',#153134);
#37387=VERTEX_POINT('',#153137);
#37388=VERTEX_POINT('',#153139);
#37389=VERTEX_POINT('',#153142);
#37390=VERTEX_POINT('',#153144);
#37391=VERTEX_POINT('',#153147);
#37392=VERTEX_POINT('',#153149);
#37393=VERTEX_POINT('',#153152);
#37394=VERTEX_POINT('',#153154);
#37395=VERTEX_POINT('',#153157);
#37396=VERTEX_POINT('',#153159);
#37397=VERTEX_POINT('',#153162);
#37398=VERTEX_POINT('',#153164);
#37399=VERTEX_POINT('',#153167);
#37400=VERTEX_POINT('',#153169);
#37401=VERTEX_POINT('',#153172);
#37402=VERTEX_POINT('',#153174);
#37403=VERTEX_POINT('',#153177);
#37404=VERTEX_POINT('',#153179);
#37405=VERTEX_POINT('',#153182);
#37406=VERTEX_POINT('',#153184);
#37407=VERTEX_POINT('',#153187);
#37408=VERTEX_POINT('',#153189);
#37409=VERTEX_POINT('',#153192);
#37410=VERTEX_POINT('',#153194);
#37411=VERTEX_POINT('',#153197);
#37412=VERTEX_POINT('',#153199);
#37413=VERTEX_POINT('',#153202);
#37414=VERTEX_POINT('',#153204);
#37415=VERTEX_POINT('',#153207);
#37416=VERTEX_POINT('',#153209);
#37417=VERTEX_POINT('',#153212);
#37418=VERTEX_POINT('',#153215);
#37419=VERTEX_POINT('',#153218);
#37420=VERTEX_POINT('',#153220);
#37421=VERTEX_POINT('',#153223);
#37422=VERTEX_POINT('',#153225);
#37423=VERTEX_POINT('',#153228);
#37424=VERTEX_POINT('',#153230);
#37425=VERTEX_POINT('',#153233);
#37426=VERTEX_POINT('',#153235);
#37427=VERTEX_POINT('',#153238);
#37428=VERTEX_POINT('',#153240);
#37429=VERTEX_POINT('',#153243);
#37430=VERTEX_POINT('',#153245);
#37431=VERTEX_POINT('',#153248);
#37432=VERTEX_POINT('',#153436);
#37433=VERTEX_POINT('',#153437);
#37434=VERTEX_POINT('',#153442);
#37435=VERTEX_POINT('',#153443);
#37436=VERTEX_POINT('',#153448);
#37437=VERTEX_POINT('',#153449);
#37438=VERTEX_POINT('',#153454);
#37439=VERTEX_POINT('',#153455);
#37440=VERTEX_POINT('',#153460);
#37441=VERTEX_POINT('',#153465);
#37442=VERTEX_POINT('',#153473);
#37443=VERTEX_POINT('',#153474);
#37444=VERTEX_POINT('',#153476);
#37445=VERTEX_POINT('',#153478);
#37446=VERTEX_POINT('',#153485);
#37447=VERTEX_POINT('',#153490);
#37448=VERTEX_POINT('',#153494);
#37449=VERTEX_POINT('',#153495);
#37450=VERTEX_POINT('',#153500);
#37451=VERTEX_POINT('',#153501);
#37452=VERTEX_POINT('',#153539);
#37453=VERTEX_POINT('',#153540);
#37454=VERTEX_POINT('',#153542);
#37455=VERTEX_POINT('',#153544);
#37456=VERTEX_POINT('',#154491);
#37457=VERTEX_POINT('',#154492);
#37458=VERTEX_POINT('',#156380);
#37459=VERTEX_POINT('',#156381);
#37460=VERTEX_POINT('',#157328);
#37461=VERTEX_POINT('',#157329);
#37462=VERTEX_POINT('',#157334);
#37463=VERTEX_POINT('',#157335);
#37464=VERTEX_POINT('',#157337);
#37465=VERTEX_POINT('',#157339);
#37466=VERTEX_POINT('',#158286);
#37467=VERTEX_POINT('',#158287);
#37468=VERTEX_POINT('',#160816);
#37469=VERTEX_POINT('',#160817);
#37470=VERTEX_POINT('',#160822);
#37471=VERTEX_POINT('',#160823);
#37472=VERTEX_POINT('',#160825);
#37473=VERTEX_POINT('',#160827);
#37474=VERTEX_POINT('',#163374);
#37475=VERTEX_POINT('',#163375);
#37476=VERTEX_POINT('',#164016);
#37477=VERTEX_POINT('',#164017);
#37478=VERTEX_POINT('',#164022);
#37479=VERTEX_POINT('',#164023);
#37480=VERTEX_POINT('',#164025);
#37481=VERTEX_POINT('',#164027);
#37482=VERTEX_POINT('',#164974);
#37483=VERTEX_POINT('',#164975);
#37484=VERTEX_POINT('',#167216);
#37485=VERTEX_POINT('',#167217);
#37486=VERTEX_POINT('',#167222);
#37487=VERTEX_POINT('',#167223);
#37488=VERTEX_POINT('',#167225);
#37489=VERTEX_POINT('',#167227);
#37490=VERTEX_POINT('',#170062);
#37491=VERTEX_POINT('',#170063);
#37492=VERTEX_POINT('',#171010);
#37493=VERTEX_POINT('',#171011);
#37494=VERTEX_POINT('',#171016);
#37495=VERTEX_POINT('',#171017);
#37496=VERTEX_POINT('',#171019);
#37497=VERTEX_POINT('',#171021);
#37498=VERTEX_POINT('',#171968);
#37499=VERTEX_POINT('',#171969);
#37500=VERTEX_POINT('',#174498);
#37501=VERTEX_POINT('',#174499);
#37502=VERTEX_POINT('',#174504);
#37503=VERTEX_POINT('',#174505);
#37504=VERTEX_POINT('',#174507);
#37505=VERTEX_POINT('',#174509);
#37506=VERTEX_POINT('',#177053);
#37507=VERTEX_POINT('',#177054);
#37508=VERTEX_POINT('',#177707);
#37509=VERTEX_POINT('',#177708);
#37510=VERTEX_POINT('',#177713);
#37511=VERTEX_POINT('',#177714);
#37512=VERTEX_POINT('',#177716);
#37513=VERTEX_POINT('',#177718);
#37514=VERTEX_POINT('',#178665);
#37515=VERTEX_POINT('',#178666);
#37516=VERTEX_POINT('',#181198);
#37517=VERTEX_POINT('',#181199);
#37518=VERTEX_POINT('',#181204);
#37519=VERTEX_POINT('',#181205);
#37520=VERTEX_POINT('',#181207);
#37521=VERTEX_POINT('',#181209);
#37522=VERTEX_POINT('',#183732);
#37523=VERTEX_POINT('',#183733);
#37524=VERTEX_POINT('',#184680);
#37525=VERTEX_POINT('',#184681);
#37526=VERTEX_POINT('',#184686);
#37527=VERTEX_POINT('',#184687);
#37528=VERTEX_POINT('',#184689);
#37529=VERTEX_POINT('',#184691);
#37530=VERTEX_POINT('',#185638);
#37531=VERTEX_POINT('',#185639);
#37532=VERTEX_POINT('',#187868);
#37533=VERTEX_POINT('',#187869);
#37534=VERTEX_POINT('',#187874);
#37535=VERTEX_POINT('',#187875);
#37536=VERTEX_POINT('',#187877);
#37537=VERTEX_POINT('',#187879);
#37538=VERTEX_POINT('',#190378);
#37539=VERTEX_POINT('',#190379);
#37540=VERTEX_POINT('',#191002);
#37541=VERTEX_POINT('',#191003);
#37542=VERTEX_POINT('',#191008);
#37543=VERTEX_POINT('',#191009);
#37544=VERTEX_POINT('',#191011);
#37545=VERTEX_POINT('',#191013);
#37546=VERTEX_POINT('',#191960);
#37547=VERTEX_POINT('',#191961);
#37548=VERTEX_POINT('',#194470);
#37549=VERTEX_POINT('',#194471);
#37550=VERTEX_POINT('',#194476);
#37551=VERTEX_POINT('',#194477);
#37552=VERTEX_POINT('',#194479);
#37553=VERTEX_POINT('',#194481);
#37554=VERTEX_POINT('',#196998);
#37555=VERTEX_POINT('',#196999);
#37556=VERTEX_POINT('',#197946);
#37557=VERTEX_POINT('',#197947);
#37558=VERTEX_POINT('',#197952);
#37559=VERTEX_POINT('',#197953);
#37560=VERTEX_POINT('',#197955);
#37561=VERTEX_POINT('',#197957);
#37562=VERTEX_POINT('',#198904);
#37563=VERTEX_POINT('',#198905);
#37564=VERTEX_POINT('',#201104);
#37565=VERTEX_POINT('',#201105);
#37566=VERTEX_POINT('',#201110);
#37567=VERTEX_POINT('',#201111);
#37568=VERTEX_POINT('',#201113);
#37569=VERTEX_POINT('',#201115);
#37570=VERTEX_POINT('',#203644);
#37571=VERTEX_POINT('',#203645);
#37572=VERTEX_POINT('',#204280);
#37573=VERTEX_POINT('',#204281);
#37574=VERTEX_POINT('',#204286);
#37575=VERTEX_POINT('',#204287);
#37576=VERTEX_POINT('',#204289);
#37577=VERTEX_POINT('',#204291);
#37578=VERTEX_POINT('',#205238);
#37579=VERTEX_POINT('',#205239);
#37580=VERTEX_POINT('',#207432);
#37581=VERTEX_POINT('',#207433);
#37582=VERTEX_POINT('',#207438);
#37583=VERTEX_POINT('',#207439);
#37584=VERTEX_POINT('',#207441);
#37585=VERTEX_POINT('',#207443);
#37586=VERTEX_POINT('',#209972);
#37587=VERTEX_POINT('',#209973);
#37588=VERTEX_POINT('',#210611);
#37589=VERTEX_POINT('',#210612);
#37590=VERTEX_POINT('',#210617);
#37591=VERTEX_POINT('',#210618);
#37592=VERTEX_POINT('',#210620);
#37593=VERTEX_POINT('',#210622);
#37594=VERTEX_POINT('',#211569);
#37595=VERTEX_POINT('',#211570);
#37596=VERTEX_POINT('',#213775);
#37597=VERTEX_POINT('',#213776);
#37598=VERTEX_POINT('',#213781);
#37599=VERTEX_POINT('',#213782);
#37600=VERTEX_POINT('',#213784);
#37601=VERTEX_POINT('',#213786);
#37602=VERTEX_POINT('',#216309);
#37603=VERTEX_POINT('',#216310);
#37604=VERTEX_POINT('',#216942);
#37605=VERTEX_POINT('',#216943);
#37606=VERTEX_POINT('',#216948);
#37607=VERTEX_POINT('',#216949);
#37608=VERTEX_POINT('',#216951);
#37609=VERTEX_POINT('',#216953);
#37610=VERTEX_POINT('',#217900);
#37611=VERTEX_POINT('',#217901);
#37612=VERTEX_POINT('',#220407);
#37613=VERTEX_POINT('',#220408);
#37614=VERTEX_POINT('',#220413);
#37615=VERTEX_POINT('',#220414);
#37616=VERTEX_POINT('',#220416);
#37617=VERTEX_POINT('',#220418);
#37618=VERTEX_POINT('',#222920);
#37619=VERTEX_POINT('',#222921);
#37620=VERTEX_POINT('',#223550);
#37621=VERTEX_POINT('',#223551);
#37622=VERTEX_POINT('',#223556);
#37623=VERTEX_POINT('',#223557);
#37624=VERTEX_POINT('',#223559);
#37625=VERTEX_POINT('',#223561);
#37626=VERTEX_POINT('',#224508);
#37627=VERTEX_POINT('',#224509);
#37628=VERTEX_POINT('',#226994);
#37629=VERTEX_POINT('',#226995);
#37630=VERTEX_POINT('',#227000);
#37631=VERTEX_POINT('',#227001);
#37632=VERTEX_POINT('',#227003);
#37633=VERTEX_POINT('',#227005);
#37634=VERTEX_POINT('',#229519);
#37635=VERTEX_POINT('',#229520);
#37636=VERTEX_POINT('',#230134);
#37637=VERTEX_POINT('',#230135);
#37638=VERTEX_POINT('',#230140);
#37639=VERTEX_POINT('',#230141);
#37640=VERTEX_POINT('',#230143);
#37641=VERTEX_POINT('',#230145);
#37642=VERTEX_POINT('',#231092);
#37643=VERTEX_POINT('',#231093);
#37644=VERTEX_POINT('',#233274);
#37645=VERTEX_POINT('',#233275);
#37646=VERTEX_POINT('',#233280);
#37647=VERTEX_POINT('',#233281);
#37648=VERTEX_POINT('',#233283);
#37649=VERTEX_POINT('',#233285);
#37650=VERTEX_POINT('',#235814);
#37651=VERTEX_POINT('',#235815);
#37652=VERTEX_POINT('',#236432);
#37653=VERTEX_POINT('',#236433);
#37654=VERTEX_POINT('',#236438);
#37655=VERTEX_POINT('',#236439);
#37656=VERTEX_POINT('',#236441);
#37657=VERTEX_POINT('',#236443);
#37658=VERTEX_POINT('',#237390);
#37659=VERTEX_POINT('',#237391);
#37660=VERTEX_POINT('',#239602);
#37661=VERTEX_POINT('',#239603);
#37662=VERTEX_POINT('',#239608);
#37663=VERTEX_POINT('',#239609);
#37664=VERTEX_POINT('',#239611);
#37665=VERTEX_POINT('',#239613);
#37666=VERTEX_POINT('',#242136);
#37667=VERTEX_POINT('',#242137);
#37668=VERTEX_POINT('',#242769);
#37669=VERTEX_POINT('',#242770);
#37670=VERTEX_POINT('',#242775);
#37671=VERTEX_POINT('',#242776);
#37672=VERTEX_POINT('',#242778);
#37673=VERTEX_POINT('',#242780);
#37674=VERTEX_POINT('',#243727);
#37675=VERTEX_POINT('',#243728);
#37676=VERTEX_POINT('',#246251);
#37677=VERTEX_POINT('',#246252);
#37678=VERTEX_POINT('',#246257);
#37679=VERTEX_POINT('',#246258);
#37680=VERTEX_POINT('',#246260);
#37681=VERTEX_POINT('',#246262);
#37682=VERTEX_POINT('',#248788);
#37683=VERTEX_POINT('',#248789);
#37684=VERTEX_POINT('',#249424);
#37685=VERTEX_POINT('',#249425);
#37686=VERTEX_POINT('',#249430);
#37687=VERTEX_POINT('',#249431);
#37688=VERTEX_POINT('',#249433);
#37689=VERTEX_POINT('',#249435);
#37690=VERTEX_POINT('',#250382);
#37691=VERTEX_POINT('',#250383);
#37692=VERTEX_POINT('',#252597);
#37693=VERTEX_POINT('',#252598);
#37694=VERTEX_POINT('',#252603);
#37695=VERTEX_POINT('',#252604);
#37696=VERTEX_POINT('',#252606);
#37697=VERTEX_POINT('',#252608);
#37698=VERTEX_POINT('',#255110);
#37699=VERTEX_POINT('',#255111);
#37700=VERTEX_POINT('',#255749);
#37701=VERTEX_POINT('',#255750);
#37702=VERTEX_POINT('',#255755);
#37703=VERTEX_POINT('',#255756);
#37704=VERTEX_POINT('',#255758);
#37705=VERTEX_POINT('',#255760);
#37706=VERTEX_POINT('',#256707);
#37707=VERTEX_POINT('',#256708);
#37708=VERTEX_POINT('',#258898);
#37709=VERTEX_POINT('',#258899);
#37710=VERTEX_POINT('',#258904);
#37711=VERTEX_POINT('',#258905);
#37712=VERTEX_POINT('',#258907);
#37713=VERTEX_POINT('',#258909);
#37714=VERTEX_POINT('',#261742);
#37715=VERTEX_POINT('',#261743);
#37716=VERTEX_POINT('',#262690);
#37717=VERTEX_POINT('',#262691);
#37718=VERTEX_POINT('',#262696);
#37719=VERTEX_POINT('',#262697);
#37720=VERTEX_POINT('',#262699);
#37721=VERTEX_POINT('',#262701);
#37722=VERTEX_POINT('',#263648);
#37723=VERTEX_POINT('',#263649);
#37724=VERTEX_POINT('',#266144);
#37725=VERTEX_POINT('',#266145);
#37726=VERTEX_POINT('',#266150);
#37727=VERTEX_POINT('',#266151);
#37728=VERTEX_POINT('',#266153);
#37729=VERTEX_POINT('',#266155);
#37730=VERTEX_POINT('',#268687);
#37731=VERTEX_POINT('',#268688);
#37732=VERTEX_POINT('',#269633);
#37733=VERTEX_POINT('',#269634);
#37734=VERTEX_POINT('',#269639);
#37735=VERTEX_POINT('',#269640);
#37736=VERTEX_POINT('',#269642);
#37737=VERTEX_POINT('',#269644);
#37738=VERTEX_POINT('',#270591);
#37739=VERTEX_POINT('',#270592);
#37740=VERTEX_POINT('',#272830);
#37741=VERTEX_POINT('',#272831);
#37742=VERTEX_POINT('',#272836);
#37743=VERTEX_POINT('',#272837);
#37744=VERTEX_POINT('',#272839);
#37745=VERTEX_POINT('',#272841);
#37746=VERTEX_POINT('',#275382);
#37747=VERTEX_POINT('',#275383);
#37748=VERTEX_POINT('',#276033);
#37749=VERTEX_POINT('',#276034);
#37750=VERTEX_POINT('',#276039);
#37751=VERTEX_POINT('',#276040);
#37752=VERTEX_POINT('',#276042);
#37753=VERTEX_POINT('',#276044);
#37754=VERTEX_POINT('',#276991);
#37755=VERTEX_POINT('',#276992);
#37756=VERTEX_POINT('',#279528);
#37757=VERTEX_POINT('',#279529);
#37758=VERTEX_POINT('',#279534);
#37759=VERTEX_POINT('',#279535);
#37760=VERTEX_POINT('',#279537);
#37761=VERTEX_POINT('',#279539);
#37762=VERTEX_POINT('',#282077);
#37763=VERTEX_POINT('',#282078);
#37764=VERTEX_POINT('',#282737);
#37765=VERTEX_POINT('',#282738);
#37766=VERTEX_POINT('',#282743);
#37767=VERTEX_POINT('',#282744);
#37768=VERTEX_POINT('',#282746);
#37769=VERTEX_POINT('',#282748);
#37770=VERTEX_POINT('',#283695);
#37771=VERTEX_POINT('',#283696);
#37772=VERTEX_POINT('',#286531);
#37773=VERTEX_POINT('',#286532);
#37774=VERTEX_POINT('',#286537);
#37775=VERTEX_POINT('',#286538);
#37776=VERTEX_POINT('',#286540);
#37777=VERTEX_POINT('',#286542);
#37778=VERTEX_POINT('',#289375);
#37779=VERTEX_POINT('',#289376);
#37780=VERTEX_POINT('',#290026);
#37781=VERTEX_POINT('',#290027);
#37782=VERTEX_POINT('',#290032);
#37783=VERTEX_POINT('',#290033);
#37784=VERTEX_POINT('',#290035);
#37785=VERTEX_POINT('',#290037);
#37786=VERTEX_POINT('',#290984);
#37787=VERTEX_POINT('',#290985);
#37788=VERTEX_POINT('',#293214);
#37789=VERTEX_POINT('',#293215);
#37790=VERTEX_POINT('',#293220);
#37791=VERTEX_POINT('',#293221);
#37792=VERTEX_POINT('',#293223);
#37793=VERTEX_POINT('',#293225);
#37794=VERTEX_POINT('',#295751);
#37795=VERTEX_POINT('',#295752);
#37796=VERTEX_POINT('',#296699);
#37797=VERTEX_POINT('',#296701);
#37798=VERTEX_POINT('',#296703);
#37799=VERTEX_POINT('',#297175);
#37800=VERTEX_POINT('',#297499);
#37801=VERTEX_POINT('',#297502);
#37802=VERTEX_POINT('',#297506);
#37803=VERTEX_POINT('',#297510);
#37804=VERTEX_POINT('',#297512);
#37805=VERTEX_POINT('',#300197);
#37806=VERTEX_POINT('',#300202);
#37807=VERTEX_POINT('',#300204);
#37808=VERTEX_POINT('',#300208);
#37809=VERTEX_POINT('',#300210);
#37810=VERTEX_POINT('',#300216);
#37811=VERTEX_POINT('',#300217);
#37812=VERTEX_POINT('',#300219);
#37813=VERTEX_POINT('',#300221);
#37814=VERTEX_POINT('',#300223);
#37815=VERTEX_POINT('',#300238);
#37816=VERTEX_POINT('',#300240);
#37817=VERTEX_POINT('',#300284);
#37818=VERTEX_POINT('',#300286);
#37819=VERTEX_POINT('',#300288);
#37820=VERTEX_POINT('',#300290);
#37821=VERTEX_POINT('',#300307);
#37822=VERTEX_POINT('',#300309);
#37823=VERTEX_POINT('',#300356);
#37824=VERTEX_POINT('',#300358);
#37825=VERTEX_POINT('',#300360);
#37826=VERTEX_POINT('',#300362);
#37827=VERTEX_POINT('',#300379);
#37828=VERTEX_POINT('',#300381);
#37829=VERTEX_POINT('',#300428);
#37830=VERTEX_POINT('',#300430);
#37831=VERTEX_POINT('',#300432);
#37832=VERTEX_POINT('',#300434);
#37833=VERTEX_POINT('',#300451);
#37834=VERTEX_POINT('',#300453);
#37835=VERTEX_POINT('',#300500);
#37836=VERTEX_POINT('',#300502);
#37837=VERTEX_POINT('',#300504);
#37838=VERTEX_POINT('',#300506);
#37839=VERTEX_POINT('',#300521);
#37840=VERTEX_POINT('',#300523);
#37841=VERTEX_POINT('',#300567);
#37842=VERTEX_POINT('',#300569);
#37843=VERTEX_POINT('',#300571);
#37844=VERTEX_POINT('',#300573);
#37845=VERTEX_POINT('',#300590);
#37846=VERTEX_POINT('',#300592);
#37847=VERTEX_POINT('',#300609);
#37848=VERTEX_POINT('',#300611);
#37849=VERTEX_POINT('',#300613);
#37850=VERTEX_POINT('',#300615);
#37851=VERTEX_POINT('',#300632);
#37852=VERTEX_POINT('',#300634);
#37853=VERTEX_POINT('',#300681);
#37854=VERTEX_POINT('',#300683);
#37855=VERTEX_POINT('',#300685);
#37856=VERTEX_POINT('',#300687);
#37857=VERTEX_POINT('',#300704);
#37858=VERTEX_POINT('',#300706);
#37859=VERTEX_POINT('',#300717);
#37860=VERTEX_POINT('',#300719);
#37861=VERTEX_POINT('',#300721);
#37862=VERTEX_POINT('',#300723);
#37863=VERTEX_POINT('',#300740);
#37864=VERTEX_POINT('',#300742);
#37865=VERTEX_POINT('',#300786);
#37866=VERTEX_POINT('',#300788);
#37867=VERTEX_POINT('',#300790);
#37868=VERTEX_POINT('',#300792);
#37869=VERTEX_POINT('',#300809);
#37870=VERTEX_POINT('',#300811);
#37871=VERTEX_POINT('',#300855);
#37872=VERTEX_POINT('',#300857);
#37873=VERTEX_POINT('',#300859);
#37874=VERTEX_POINT('',#300861);
#37875=VERTEX_POINT('',#300878);
#37876=VERTEX_POINT('',#300880);
#37877=VERTEX_POINT('',#300897);
#37878=VERTEX_POINT('',#300899);
#37879=VERTEX_POINT('',#300901);
#37880=VERTEX_POINT('',#300903);
#37881=VERTEX_POINT('',#300920);
#37882=VERTEX_POINT('',#300922);
#37883=VERTEX_POINT('',#300966);
#37884=VERTEX_POINT('',#300968);
#37885=VERTEX_POINT('',#300970);
#37886=VERTEX_POINT('',#300972);
#37887=VERTEX_POINT('',#300989);
#37888=VERTEX_POINT('',#300991);
#37889=VERTEX_POINT('',#301008);
#37890=VERTEX_POINT('',#301010);
#37891=VERTEX_POINT('',#301012);
#37892=VERTEX_POINT('',#301014);
#37893=VERTEX_POINT('',#301031);
#37894=VERTEX_POINT('',#301033);
#37895=VERTEX_POINT('',#301077);
#37896=VERTEX_POINT('',#301079);
#37897=VERTEX_POINT('',#301081);
#37898=VERTEX_POINT('',#301083);
#37899=VERTEX_POINT('',#301100);
#37900=VERTEX_POINT('',#301102);
#37901=VERTEX_POINT('',#301146);
#37902=VERTEX_POINT('',#301148);
#37903=VERTEX_POINT('',#301150);
#37904=VERTEX_POINT('',#301152);
#37905=VERTEX_POINT('',#301167);
#37906=VERTEX_POINT('',#301169);
#37907=VERTEX_POINT('',#301213);
#37908=VERTEX_POINT('',#301215);
#37909=VERTEX_POINT('',#301217);
#37910=VERTEX_POINT('',#301219);
#37911=VERTEX_POINT('',#301236);
#37912=VERTEX_POINT('',#301281);
#37913=VERTEX_POINT('',#301284);
#37914=VERTEX_POINT('',#301286);
#37915=VERTEX_POINT('',#301291);
#37916=VERTEX_POINT('',#301293);
#37917=VERTEX_POINT('',#302946);
#37918=VERTEX_POINT('',#302957);
#37919=VERTEX_POINT('',#302961);
#37920=VERTEX_POINT('',#302965);
#37921=VERTEX_POINT('',#304621);
#37922=VERTEX_POINT('',#304632);
#37923=VERTEX_POINT('',#306285);
#37924=VERTEX_POINT('',#306296);
#37925=VERTEX_POINT('',#306300);
#37926=VERTEX_POINT('',#306304);
#37927=VERTEX_POINT('',#307960);
#37928=VERTEX_POINT('',#307975);
#37929=VERTEX_POINT('',#309628);
#37930=VERTEX_POINT('',#309639);
#37931=VERTEX_POINT('',#309643);
#37932=VERTEX_POINT('',#309647);
#37933=VERTEX_POINT('',#311300);
#37934=VERTEX_POINT('',#311315);
#37935=VERTEX_POINT('',#312968);
#37936=VERTEX_POINT('',#312979);
#37937=VERTEX_POINT('',#312983);
#37938=VERTEX_POINT('',#312987);
#37939=VERTEX_POINT('',#314643);
#37940=VERTEX_POINT('',#314662);
#37941=VERTEX_POINT('',#316315);
#37942=VERTEX_POINT('',#316326);
#37943=VERTEX_POINT('',#316330);
#37944=VERTEX_POINT('',#316334);
#37945=VERTEX_POINT('',#317990);
#37946=VERTEX_POINT('',#318009);
#37947=VERTEX_POINT('',#319662);
#37948=VERTEX_POINT('',#319673);
#37949=VERTEX_POINT('',#319677);
#37950=VERTEX_POINT('',#319681);
#37951=VERTEX_POINT('',#321337);
#37952=VERTEX_POINT('',#321356);
#37953=VERTEX_POINT('',#323009);
#37954=VERTEX_POINT('',#323020);
#37955=VERTEX_POINT('',#323024);
#37956=VERTEX_POINT('',#323028);
#37957=VERTEX_POINT('',#324684);
#37958=VERTEX_POINT('',#324703);
#37959=VERTEX_POINT('',#326356);
#37960=VERTEX_POINT('',#326367);
#37961=VERTEX_POINT('',#326371);
#37962=VERTEX_POINT('',#326375);
#37963=VERTEX_POINT('',#328031);
#37964=VERTEX_POINT('',#328046);
#37965=VERTEX_POINT('',#329699);
#37966=VERTEX_POINT('',#329710);
#37967=VERTEX_POINT('',#329714);
#37968=VERTEX_POINT('',#329716);
#37969=VERTEX_POINT('',#329718);
#37970=VERTEX_POINT('',#329735);
#37971=VERTEX_POINT('',#329737);
#37972=VERTEX_POINT('',#329746);
#37973=VERTEX_POINT('',#329748);
#37974=VERTEX_POINT('',#329750);
#37975=VERTEX_POINT('',#329752);
#37976=VERTEX_POINT('',#329769);
#37977=VERTEX_POINT('',#329771);
#37978=VERTEX_POINT('',#329780);
#37979=VERTEX_POINT('',#329782);
#37980=VERTEX_POINT('',#329784);
#37981=VERTEX_POINT('',#329786);
#37982=VERTEX_POINT('',#329803);
#37983=VERTEX_POINT('',#329805);
#37984=VERTEX_POINT('',#329814);
#37985=VERTEX_POINT('',#329816);
#37986=VERTEX_POINT('',#329818);
#37987=VERTEX_POINT('',#329820);
#37988=VERTEX_POINT('',#329833);
#37989=VERTEX_POINT('',#329835);
#37990=VERTEX_POINT('',#329844);
#37991=VERTEX_POINT('',#329846);
#37992=VERTEX_POINT('',#329848);
#37993=VERTEX_POINT('',#329850);
#37994=VERTEX_POINT('',#329867);
#37995=VERTEX_POINT('',#329869);
#37996=VERTEX_POINT('',#329878);
#37997=VERTEX_POINT('',#329880);
#37998=VERTEX_POINT('',#329882);
#37999=VERTEX_POINT('',#329884);
#38000=VERTEX_POINT('',#329901);
#38001=VERTEX_POINT('',#329903);
#38002=VERTEX_POINT('',#329912);
#38003=VERTEX_POINT('',#329914);
#38004=VERTEX_POINT('',#329916);
#38005=VERTEX_POINT('',#329918);
#38006=VERTEX_POINT('',#329935);
#38007=VERTEX_POINT('',#329937);
#38008=VERTEX_POINT('',#329946);
#38009=VERTEX_POINT('',#329948);
#38010=VERTEX_POINT('',#329950);
#38011=VERTEX_POINT('',#329952);
#38012=VERTEX_POINT('',#329967);
#38013=VERTEX_POINT('',#329969);
#38014=VERTEX_POINT('',#329978);
#38015=VERTEX_POINT('',#329980);
#38016=VERTEX_POINT('',#329982);
#38017=VERTEX_POINT('',#358156);
#38018=VERTEX_POINT('',#358162);
#38019=VERTEX_POINT('',#358164);
#38020=VERTEX_POINT('',#358168);
#38021=VERTEX_POINT('',#358171);
#38022=VERTEX_POINT('',#358173);
#38023=VERTEX_POINT('',#358175);
#38024=VERTEX_POINT('',#358177);
#38025=VERTEX_POINT('',#358179);
#38026=VERTEX_POINT('',#358181);
#38027=VERTEX_POINT('',#358184);
#38028=VERTEX_POINT('',#358186);
#38029=VERTEX_POINT('',#358189);
#38030=VERTEX_POINT('',#358190);
#38031=VERTEX_POINT('',#358192);
#38032=VERTEX_POINT('',#358194);
#38033=VERTEX_POINT('',#358197);
#38034=VERTEX_POINT('',#358198);
#38035=VERTEX_POINT('',#358200);
#38036=VERTEX_POINT('',#358202);
#38037=VERTEX_POINT('',#358205);
#38038=VERTEX_POINT('',#358206);
#38039=VERTEX_POINT('',#358208);
#38040=VERTEX_POINT('',#358210);
#38041=VERTEX_POINT('',#358213);
#38042=VERTEX_POINT('',#358214);
#38043=VERTEX_POINT('',#358216);
#38044=VERTEX_POINT('',#358218);
#38045=VERTEX_POINT('',#358221);
#38046=VERTEX_POINT('',#358222);
#38047=VERTEX_POINT('',#358224);
#38048=VERTEX_POINT('',#358226);
#38049=VERTEX_POINT('',#358229);
#38050=VERTEX_POINT('',#358230);
#38051=VERTEX_POINT('',#358232);
#38052=VERTEX_POINT('',#358234);
#38053=VERTEX_POINT('',#358237);
#38054=VERTEX_POINT('',#358238);
#38055=VERTEX_POINT('',#358240);
#38056=VERTEX_POINT('',#358242);
#38057=VERTEX_POINT('',#358246);
#38058=VERTEX_POINT('',#358248);
#38059=VERTEX_POINT('',#358252);
#38060=VERTEX_POINT('',#358254);
#38061=VERTEX_POINT('',#358256);
#38062=VERTEX_POINT('',#358258);
#38063=VERTEX_POINT('',#358260);
#38064=VERTEX_POINT('',#358263);
#38065=VERTEX_POINT('',#358265);
#38066=VERTEX_POINT('',#358268);
#38067=VERTEX_POINT('',#358269);
#38068=VERTEX_POINT('',#358271);
#38069=VERTEX_POINT('',#358273);
#38070=VERTEX_POINT('',#358276);
#38071=VERTEX_POINT('',#358277);
#38072=VERTEX_POINT('',#358279);
#38073=VERTEX_POINT('',#358281);
#38074=VERTEX_POINT('',#358284);
#38075=VERTEX_POINT('',#358285);
#38076=VERTEX_POINT('',#358287);
#38077=VERTEX_POINT('',#358289);
#38078=VERTEX_POINT('',#358292);
#38079=VERTEX_POINT('',#358293);
#38080=VERTEX_POINT('',#358295);
#38081=VERTEX_POINT('',#358297);
#38082=VERTEX_POINT('',#358300);
#38083=VERTEX_POINT('',#358301);
#38084=VERTEX_POINT('',#358303);
#38085=VERTEX_POINT('',#358305);
#38086=VERTEX_POINT('',#358308);
#38087=VERTEX_POINT('',#358309);
#38088=VERTEX_POINT('',#358311);
#38089=VERTEX_POINT('',#358313);
#38090=VERTEX_POINT('',#358316);
#38091=VERTEX_POINT('',#358317);
#38092=VERTEX_POINT('',#358319);
#38093=VERTEX_POINT('',#358321);
#38094=VERTEX_POINT('',#358325);
#38095=VERTEX_POINT('',#358329);
#38096=VERTEX_POINT('',#358398);
#38097=VERTEX_POINT('',#358400);
#38098=VERTEX_POINT('',#358404);
#38099=VERTEX_POINT('',#358409);
#38100=VERTEX_POINT('',#358414);
#38101=VERTEX_POINT('',#358416);
#38102=VERTEX_POINT('',#358420);
#38103=VERTEX_POINT('',#358425);
#38104=VERTEX_POINT('',#358430);
#38105=VERTEX_POINT('',#358432);
#38106=VERTEX_POINT('',#358436);
#38107=VERTEX_POINT('',#358441);
#38108=VERTEX_POINT('',#358446);
#38109=VERTEX_POINT('',#358448);
#38110=VERTEX_POINT('',#358452);
#38111=VERTEX_POINT('',#358457);
#38112=VERTEX_POINT('',#358462);
#38113=VERTEX_POINT('',#358464);
#38114=VERTEX_POINT('',#358468);
#38115=VERTEX_POINT('',#358473);
#38116=VERTEX_POINT('',#358478);
#38117=VERTEX_POINT('',#358480);
#38118=VERTEX_POINT('',#358484);
#38119=VERTEX_POINT('',#358489);
#38120=VERTEX_POINT('',#358494);
#38121=VERTEX_POINT('',#358496);
#38122=VERTEX_POINT('',#358500);
#38123=VERTEX_POINT('',#358505);
#38124=VERTEX_POINT('',#358510);
#38125=VERTEX_POINT('',#358512);
#38126=VERTEX_POINT('',#358516);
#38127=VERTEX_POINT('',#358521);
#38128=VERTEX_POINT('',#358528);
#38129=VERTEX_POINT('',#358529);
#38130=VERTEX_POINT('',#358531);
#38131=VERTEX_POINT('',#358545);
#38132=VERTEX_POINT('',#358561);
#38133=VERTEX_POINT('',#358562);
#38134=VERTEX_POINT('',#358591);
#38135=VERTEX_POINT('',#358592);
#38136=VERTEX_POINT('',#358621);
#38137=VERTEX_POINT('',#358622);
#38138=VERTEX_POINT('',#358651);
#38139=VERTEX_POINT('',#358652);
#38140=VERTEX_POINT('',#358681);
#38141=VERTEX_POINT('',#358682);
#38142=VERTEX_POINT('',#358711);
#38143=VERTEX_POINT('',#358712);
#38144=VERTEX_POINT('',#358741);
#38145=VERTEX_POINT('',#358742);
#38146=VERTEX_POINT('',#358771);
#38147=VERTEX_POINT('',#358772);
#38148=VERTEX_POINT('',#358801);
#38149=VERTEX_POINT('',#358802);
#38150=VERTEX_POINT('',#358831);
#38151=VERTEX_POINT('',#358832);
#38152=VERTEX_POINT('',#358861);
#38153=VERTEX_POINT('',#358862);
#38154=VERTEX_POINT('',#358891);
#38155=VERTEX_POINT('',#358892);
#38156=VERTEX_POINT('',#358921);
#38157=VERTEX_POINT('',#358922);
#38158=VERTEX_POINT('',#358951);
#38159=VERTEX_POINT('',#358952);
#38160=VERTEX_POINT('',#358981);
#38161=VERTEX_POINT('',#358982);
#38162=VERTEX_POINT('',#359011);
#38163=VERTEX_POINT('',#359012);
#38164=VERTEX_POINT('',#359041);
#38165=VERTEX_POINT('',#359042);
#38166=VERTEX_POINT('',#359071);
#38167=VERTEX_POINT('',#359072);
#38168=VERTEX_POINT('',#359101);
#38169=VERTEX_POINT('',#359102);
#38170=VERTEX_POINT('',#359131);
#38171=VERTEX_POINT('',#359132);
#38172=VERTEX_POINT('',#359161);
#38173=VERTEX_POINT('',#359162);
#38174=VERTEX_POINT('',#359191);
#38175=VERTEX_POINT('',#359192);
#38176=VERTEX_POINT('',#359221);
#38177=VERTEX_POINT('',#359222);
#38178=VERTEX_POINT('',#359251);
#38179=VERTEX_POINT('',#359252);
#38180=VERTEX_POINT('',#359281);
#38181=VERTEX_POINT('',#359282);
#38182=VERTEX_POINT('',#359311);
#38183=VERTEX_POINT('',#359312);
#38184=VERTEX_POINT('',#359341);
#38185=VERTEX_POINT('',#359342);
#38186=VERTEX_POINT('',#359371);
#38187=VERTEX_POINT('',#359372);
#38188=VERTEX_POINT('',#359401);
#38189=VERTEX_POINT('',#359402);
#38190=VERTEX_POINT('',#359431);
#38191=VERTEX_POINT('',#359432);
#38192=VERTEX_POINT('',#359461);
#38193=VERTEX_POINT('',#359462);
#38194=VERTEX_POINT('',#359464);
#38195=VERTEX_POINT('',#359493);
#38196=VERTEX_POINT('',#359494);
#38197=VERTEX_POINT('',#359496);
#38198=VERTEX_POINT('',#359504);
#38199=VERTEX_POINT('',#359523);
#38200=VERTEX_POINT('',#359524);
#38201=VERTEX_POINT('',#359599);
#38202=VERTEX_POINT('',#359600);
#38203=VERTEX_POINT('',#359675);
#38204=VERTEX_POINT('',#359676);
#38205=VERTEX_POINT('',#359753);
#38206=VERTEX_POINT('',#359754);
#38207=VERTEX_POINT('',#359831);
#38208=VERTEX_POINT('',#359832);
#38209=VERTEX_POINT('',#359907);
#38210=VERTEX_POINT('',#359908);
#38211=VERTEX_POINT('',#359983);
#38212=VERTEX_POINT('',#359984);
#38213=VERTEX_POINT('',#360059);
#38214=VERTEX_POINT('',#360060);
#38215=VERTEX_POINT('',#360135);
#38216=VERTEX_POINT('',#360136);
#38217=VERTEX_POINT('',#360213);
#38218=VERTEX_POINT('',#360214);
#38219=VERTEX_POINT('',#360291);
#38220=VERTEX_POINT('',#360292);
#38221=VERTEX_POINT('',#360367);
#38222=VERTEX_POINT('',#360368);
#38223=VERTEX_POINT('',#360443);
#38224=VERTEX_POINT('',#360444);
#38225=VERTEX_POINT('',#360519);
#38226=VERTEX_POINT('',#360520);
#38227=VERTEX_POINT('',#360595);
#38228=VERTEX_POINT('',#360596);
#38229=VERTEX_POINT('',#360671);
#38230=VERTEX_POINT('',#360672);
#38231=VERTEX_POINT('',#360749);
#38232=VERTEX_POINT('',#360750);
#38233=VERTEX_POINT('',#360827);
#38234=VERTEX_POINT('',#360828);
#38235=VERTEX_POINT('',#360903);
#38236=VERTEX_POINT('',#360904);
#38237=VERTEX_POINT('',#360979);
#38238=VERTEX_POINT('',#360980);
#38239=VERTEX_POINT('',#361055);
#38240=VERTEX_POINT('',#361056);
#38241=VERTEX_POINT('',#361131);
#38242=VERTEX_POINT('',#361132);
#38243=VERTEX_POINT('',#361207);
#38244=VERTEX_POINT('',#361208);
#38245=VERTEX_POINT('',#361285);
#38246=VERTEX_POINT('',#361286);
#38247=VERTEX_POINT('',#361363);
#38248=VERTEX_POINT('',#361364);
#38249=VERTEX_POINT('',#361439);
#38250=VERTEX_POINT('',#361440);
#38251=VERTEX_POINT('',#361515);
#38252=VERTEX_POINT('',#361516);
#38253=VERTEX_POINT('',#361591);
#38254=VERTEX_POINT('',#361592);
#38255=VERTEX_POINT('',#361667);
#38256=VERTEX_POINT('',#361668);
#38257=VERTEX_POINT('',#361745);
#38258=VERTEX_POINT('',#361746);
#38259=VERTEX_POINT('',#361823);
#38260=VERTEX_POINT('',#361824);
#38261=VERTEX_POINT('',#361830);
#38262=VERTEX_POINT('',#361832);
#38263=VERTEX_POINT('',#361835);
#38264=VERTEX_POINT('',#361837);
#38265=VERTEX_POINT('',#361841);
#38266=VERTEX_POINT('',#361843);
#38267=VERTEX_POINT('',#361856);
#38268=VERTEX_POINT('',#361858);
#38269=VERTEX_POINT('',#361883);
#38270=VERTEX_POINT('',#361903);
#38271=VERTEX_POINT('',#361997);
#38272=VERTEX_POINT('',#361998);
#38273=VERTEX_POINT('',#362000);
#38274=VERTEX_POINT('',#362003);
#38275=VERTEX_POINT('',#362027);
#38276=VERTEX_POINT('',#362028);
#38277=VERTEX_POINT('',#362030);
#38278=VERTEX_POINT('',#362032);
#38279=VERTEX_POINT('',#362034);
#38280=VERTEX_POINT('',#362036);
#38281=VERTEX_POINT('',#363847);
#38282=VERTEX_POINT('',#363848);
#38283=VERTEX_POINT('',#363850);
#38284=VERTEX_POINT('',#363880);
#38285=VERTEX_POINT('',#363882);
#38286=VERTEX_POINT('',#364606);
#38287=VERTEX_POINT('',#364607);
#38288=VERTEX_POINT('',#364609);
#38289=VERTEX_POINT('',#365012);
#38290=VERTEX_POINT('',#365013);
#38291=VERTEX_POINT('',#365277);
#38292=VERTEX_POINT('',#365974);
#38293=VERTEX_POINT('',#366186);
#38294=VERTEX_POINT('',#366188);
#38295=VERTEX_POINT('',#366192);
#38296=VERTEX_POINT('',#366196);
#38297=VERTEX_POINT('',#366200);
#38298=VERTEX_POINT('',#366202);
#38299=VERTEX_POINT('',#366206);
#38300=VERTEX_POINT('',#366207);
#38301=VERTEX_POINT('',#366212);
#38302=VERTEX_POINT('',#366218);
#38303=VERTEX_POINT('',#366220);
#38304=VERTEX_POINT('',#366224);
#38305=VERTEX_POINT('',#366226);
#38306=VERTEX_POINT('',#366230);
#38307=VERTEX_POINT('',#366231);
#38308=VERTEX_POINT('',#366236);
#38309=VERTEX_POINT('',#366240);
#38310=VERTEX_POINT('',#366244);
#38311=VERTEX_POINT('',#366250);
#38312=VERTEX_POINT('',#366251);
#38313=VERTEX_POINT('',#366254);
#38314=VERTEX_POINT('',#366255);
#38315=VERTEX_POINT('',#366258);
#38316=VERTEX_POINT('',#366259);
#38317=VERTEX_POINT('',#366262);
#38318=VERTEX_POINT('',#366263);
#38319=VERTEX_POINT('',#366266);
#38320=VERTEX_POINT('',#366267);
#38321=VERTEX_POINT('',#366270);
#38322=VERTEX_POINT('',#366271);
#38323=VERTEX_POINT('',#366274);
#38324=VERTEX_POINT('',#366275);
#38325=VERTEX_POINT('',#366278);
#38326=VERTEX_POINT('',#366279);
#38327=VERTEX_POINT('',#366282);
#38328=VERTEX_POINT('',#366283);
#38329=VERTEX_POINT('',#366286);
#38330=VERTEX_POINT('',#366287);
#38331=VERTEX_POINT('',#366290);
#38332=VERTEX_POINT('',#366291);
#38333=VERTEX_POINT('',#366294);
#38334=VERTEX_POINT('',#366295);
#38335=VERTEX_POINT('',#366298);
#38336=VERTEX_POINT('',#366300);
#38337=VERTEX_POINT('',#366304);
#38338=VERTEX_POINT('',#366306);
#38339=VERTEX_POINT('',#366312);
#38340=VERTEX_POINT('',#366314);
#38341=VERTEX_POINT('',#366318);
#38342=VERTEX_POINT('',#366320);
#38343=VERTEX_POINT('',#366327);
#38344=VERTEX_POINT('',#366328);
#38345=VERTEX_POINT('',#366330);
#38346=VERTEX_POINT('',#366336);
#38347=VERTEX_POINT('',#366337);
#38348=VERTEX_POINT('',#366352);
#38349=VERTEX_POINT('',#366368);
#38350=VERTEX_POINT('',#366369);
#38351=VERTEX_POINT('',#366398);
#38352=VERTEX_POINT('',#366399);
#38353=VERTEX_POINT('',#366428);
#38354=VERTEX_POINT('',#366429);
#38355=VERTEX_POINT('',#366458);
#38356=VERTEX_POINT('',#366459);
#38357=VERTEX_POINT('',#366488);
#38358=VERTEX_POINT('',#366489);
#38359=VERTEX_POINT('',#366518);
#38360=VERTEX_POINT('',#366519);
#38361=VERTEX_POINT('',#366548);
#38362=VERTEX_POINT('',#366549);
#38363=VERTEX_POINT('',#366578);
#38364=VERTEX_POINT('',#366579);
#38365=VERTEX_POINT('',#366608);
#38366=VERTEX_POINT('',#366609);
#38367=VERTEX_POINT('',#366638);
#38368=VERTEX_POINT('',#366639);
#38369=VERTEX_POINT('',#366668);
#38370=VERTEX_POINT('',#366669);
#38371=VERTEX_POINT('',#366698);
#38372=VERTEX_POINT('',#366699);
#38373=VERTEX_POINT('',#366728);
#38374=VERTEX_POINT('',#366729);
#38375=VERTEX_POINT('',#366758);
#38376=VERTEX_POINT('',#366759);
#38377=VERTEX_POINT('',#366788);
#38378=VERTEX_POINT('',#366789);
#38379=VERTEX_POINT('',#366791);
#38380=VERTEX_POINT('',#366812);
#38381=VERTEX_POINT('',#366831);
#38382=VERTEX_POINT('',#366832);
#38383=VERTEX_POINT('',#366907);
#38384=VERTEX_POINT('',#366908);
#38385=VERTEX_POINT('',#366985);
#38386=VERTEX_POINT('',#366986);
#38387=VERTEX_POINT('',#367061);
#38388=VERTEX_POINT('',#367062);
#38389=VERTEX_POINT('',#367137);
#38390=VERTEX_POINT('',#367138);
#38391=VERTEX_POINT('',#367213);
#38392=VERTEX_POINT('',#367214);
#38393=VERTEX_POINT('',#367289);
#38394=VERTEX_POINT('',#367290);
#38395=VERTEX_POINT('',#367367);
#38396=VERTEX_POINT('',#367368);
#38397=VERTEX_POINT('',#367445);
#38398=VERTEX_POINT('',#367446);
#38399=VERTEX_POINT('',#367521);
#38400=VERTEX_POINT('',#367522);
#38401=VERTEX_POINT('',#367597);
#38402=VERTEX_POINT('',#367598);
#38403=VERTEX_POINT('',#367673);
#38404=VERTEX_POINT('',#367674);
#38405=VERTEX_POINT('',#367749);
#38406=VERTEX_POINT('',#367750);
#38407=VERTEX_POINT('',#367827);
#38408=VERTEX_POINT('',#367828);
#38409=VERTEX_POINT('',#367903);
#38410=VERTEX_POINT('',#367904);
#38411=VERTEX_POINT('',#367910);
#38412=VERTEX_POINT('',#367912);
#38413=VERTEX_POINT('',#367915);
#38414=VERTEX_POINT('',#367917);
#38415=VERTEX_POINT('',#367921);
#38416=VERTEX_POINT('',#367934);
#38417=VERTEX_POINT('',#367936);
#38418=VERTEX_POINT('',#367963);
#38419=VERTEX_POINT('',#368047);
#38420=VERTEX_POINT('',#368066);
#38421=VERTEX_POINT('',#368086);
#38422=VERTEX_POINT('',#368087);
#38423=VERTEX_POINT('',#368089);
#38424=VERTEX_POINT('',#368092);
#38425=VERTEX_POINT('',#368116);
#38426=VERTEX_POINT('',#368117);
#38427=VERTEX_POINT('',#368119);
#38428=VERTEX_POINT('',#368121);
#38429=VERTEX_POINT('',#368123);
#38430=VERTEX_POINT('',#368125);
#38431=VERTEX_POINT('',#368989);
#38432=VERTEX_POINT('',#368990);
#38433=VERTEX_POINT('',#368992);
#38434=VERTEX_POINT('',#369000);
#38435=VERTEX_POINT('',#369008);
#38436=VERTEX_POINT('',#369009);
#38437=VERTEX_POINT('',#369038);
#38438=VERTEX_POINT('',#369039);
#38439=VERTEX_POINT('',#369068);
#38440=VERTEX_POINT('',#369069);
#38441=VERTEX_POINT('',#369098);
#38442=VERTEX_POINT('',#369099);
#38443=VERTEX_POINT('',#369128);
#38444=VERTEX_POINT('',#369129);
#38445=VERTEX_POINT('',#369158);
#38446=VERTEX_POINT('',#369159);
#38447=VERTEX_POINT('',#369188);
#38448=VERTEX_POINT('',#369189);
#38449=VERTEX_POINT('',#369218);
#38450=VERTEX_POINT('',#369219);
#38451=VERTEX_POINT('',#369248);
#38452=VERTEX_POINT('',#369249);
#38453=VERTEX_POINT('',#369278);
#38454=VERTEX_POINT('',#369279);
#38455=VERTEX_POINT('',#369308);
#38456=VERTEX_POINT('',#369309);
#38457=VERTEX_POINT('',#369338);
#38458=VERTEX_POINT('',#369339);
#38459=VERTEX_POINT('',#369368);
#38460=VERTEX_POINT('',#369369);
#38461=VERTEX_POINT('',#369398);
#38462=VERTEX_POINT('',#369399);
#38463=VERTEX_POINT('',#369401);
#38464=VERTEX_POINT('',#369430);
#38465=VERTEX_POINT('',#369431);
#38466=VERTEX_POINT('',#369433);
#38467=VERTEX_POINT('',#369450);
#38468=VERTEX_POINT('',#369465);
#38469=VERTEX_POINT('',#369466);
#38470=VERTEX_POINT('',#369541);
#38471=VERTEX_POINT('',#369542);
#38472=VERTEX_POINT('',#369617);
#38473=VERTEX_POINT('',#369618);
#38474=VERTEX_POINT('',#369693);
#38475=VERTEX_POINT('',#369694);
#38476=VERTEX_POINT('',#369769);
#38477=VERTEX_POINT('',#369770);
#38478=VERTEX_POINT('',#369847);
#38479=VERTEX_POINT('',#369848);
#38480=VERTEX_POINT('',#369925);
#38481=VERTEX_POINT('',#369926);
#38482=VERTEX_POINT('',#370001);
#38483=VERTEX_POINT('',#370002);
#38484=VERTEX_POINT('',#370077);
#38485=VERTEX_POINT('',#370078);
#38486=VERTEX_POINT('',#370153);
#38487=VERTEX_POINT('',#370154);
#38488=VERTEX_POINT('',#370229);
#38489=VERTEX_POINT('',#370230);
#38490=VERTEX_POINT('',#370305);
#38491=VERTEX_POINT('',#370306);
#38492=VERTEX_POINT('',#370383);
#38493=VERTEX_POINT('',#370384);
#38494=VERTEX_POINT('',#370461);
#38495=VERTEX_POINT('',#370475);
#38496=VERTEX_POINT('',#370500);
#38497=VERTEX_POINT('',#370522);
#38498=VERTEX_POINT('',#370553);
#38499=VERTEX_POINT('',#370582);
#38500=VERTEX_POINT('',#370583);
#38501=VERTEX_POINT('',#370589);
#38502=VERTEX_POINT('',#370591);
#38503=VERTEX_POINT('',#370595);
#38504=VERTEX_POINT('',#370597);
#38505=VERTEX_POINT('',#370623);
#38506=VERTEX_POINT('',#370663);
#38507=VERTEX_POINT('',#370665);
#38508=VERTEX_POINT('',#370667);
#38509=VERTEX_POINT('',#370669);
#38510=VERTEX_POINT('',#370714);
#38511=VERTEX_POINT('',#370715);
#38512=VERTEX_POINT('',#370717);
#38513=VERTEX_POINT('',#370719);
#38514=VERTEX_POINT('',#370721);
#38515=VERTEX_POINT('',#370723);
#38516=VERTEX_POINT('',#371609);
#38517=VERTEX_POINT('',#371610);
#38518=VERTEX_POINT('',#371612);
#38519=VERTEX_POINT('',#371618);
#38520=VERTEX_POINT('',#371619);
#38521=VERTEX_POINT('',#371648);
#38522=VERTEX_POINT('',#371649);
#38523=VERTEX_POINT('',#371678);
#38524=VERTEX_POINT('',#371679);
#38525=VERTEX_POINT('',#371708);
#38526=VERTEX_POINT('',#371709);
#38527=VERTEX_POINT('',#371738);
#38528=VERTEX_POINT('',#371739);
#38529=VERTEX_POINT('',#371768);
#38530=VERTEX_POINT('',#371769);
#38531=VERTEX_POINT('',#371798);
#38532=VERTEX_POINT('',#371799);
#38533=VERTEX_POINT('',#371828);
#38534=VERTEX_POINT('',#371829);
#38535=VERTEX_POINT('',#371858);
#38536=VERTEX_POINT('',#371859);
#38537=VERTEX_POINT('',#371888);
#38538=VERTEX_POINT('',#371889);
#38539=VERTEX_POINT('',#371918);
#38540=VERTEX_POINT('',#371919);
#38541=VERTEX_POINT('',#371948);
#38542=VERTEX_POINT('',#371949);
#38543=VERTEX_POINT('',#371978);
#38544=VERTEX_POINT('',#371979);
#38545=VERTEX_POINT('',#372008);
#38546=VERTEX_POINT('',#372009);
#38547=VERTEX_POINT('',#372038);
#38548=VERTEX_POINT('',#372039);
#38549=VERTEX_POINT('',#372068);
#38550=VERTEX_POINT('',#372069);
#38551=VERTEX_POINT('',#372098);
#38552=VERTEX_POINT('',#372099);
#38553=VERTEX_POINT('',#372128);
#38554=VERTEX_POINT('',#372129);
#38555=VERTEX_POINT('',#372158);
#38556=VERTEX_POINT('',#372159);
#38557=VERTEX_POINT('',#372188);
#38558=VERTEX_POINT('',#372189);
#38559=VERTEX_POINT('',#372218);
#38560=VERTEX_POINT('',#372219);
#38561=VERTEX_POINT('',#372248);
#38562=VERTEX_POINT('',#372249);
#38563=VERTEX_POINT('',#372278);
#38564=VERTEX_POINT('',#372279);
#38565=VERTEX_POINT('',#372308);
#38566=VERTEX_POINT('',#372309);
#38567=VERTEX_POINT('',#372338);
#38568=VERTEX_POINT('',#372339);
#38569=VERTEX_POINT('',#372368);
#38570=VERTEX_POINT('',#372369);
#38571=VERTEX_POINT('',#372398);
#38572=VERTEX_POINT('',#372399);
#38573=VERTEX_POINT('',#372428);
#38574=VERTEX_POINT('',#372429);
#38575=VERTEX_POINT('',#372458);
#38576=VERTEX_POINT('',#372459);
#38577=VERTEX_POINT('',#372461);
#38578=VERTEX_POINT('',#372482);
#38579=VERTEX_POINT('',#372484);
#38580=VERTEX_POINT('',#372487);
#38581=VERTEX_POINT('',#372506);
#38582=VERTEX_POINT('',#372507);
#38583=VERTEX_POINT('',#372582);
#38584=VERTEX_POINT('',#372583);
#38585=VERTEX_POINT('',#372658);
#38586=VERTEX_POINT('',#372659);
#38587=VERTEX_POINT('',#372736);
#38588=VERTEX_POINT('',#372737);
#38589=VERTEX_POINT('',#372814);
#38590=VERTEX_POINT('',#372815);
#38591=VERTEX_POINT('',#372890);
#38592=VERTEX_POINT('',#372891);
#38593=VERTEX_POINT('',#372966);
#38594=VERTEX_POINT('',#372967);
#38595=VERTEX_POINT('',#373042);
#38596=VERTEX_POINT('',#373043);
#38597=VERTEX_POINT('',#373118);
#38598=VERTEX_POINT('',#373119);
#38599=VERTEX_POINT('',#373194);
#38600=VERTEX_POINT('',#373195);
#38601=VERTEX_POINT('',#373274);
#38602=VERTEX_POINT('',#373275);
#38603=VERTEX_POINT('',#373350);
#38604=VERTEX_POINT('',#373351);
#38605=VERTEX_POINT('',#373426);
#38606=VERTEX_POINT('',#373427);
#38607=VERTEX_POINT('',#373502);
#38608=VERTEX_POINT('',#373503);
#38609=VERTEX_POINT('',#373578);
#38610=VERTEX_POINT('',#373579);
#38611=VERTEX_POINT('',#373654);
#38612=VERTEX_POINT('',#373655);
#38613=VERTEX_POINT('',#373730);
#38614=VERTEX_POINT('',#373731);
#38615=VERTEX_POINT('',#373810);
#38616=VERTEX_POINT('',#373811);
#38617=VERTEX_POINT('',#373886);
#38618=VERTEX_POINT('',#373887);
#38619=VERTEX_POINT('',#373962);
#38620=VERTEX_POINT('',#373963);
#38621=VERTEX_POINT('',#374038);
#38622=VERTEX_POINT('',#374039);
#38623=VERTEX_POINT('',#374114);
#38624=VERTEX_POINT('',#374115);
#38625=VERTEX_POINT('',#374190);
#38626=VERTEX_POINT('',#374191);
#38627=VERTEX_POINT('',#374268);
#38628=VERTEX_POINT('',#374269);
#38629=VERTEX_POINT('',#374346);
#38630=VERTEX_POINT('',#374347);
#38631=VERTEX_POINT('',#374422);
#38632=VERTEX_POINT('',#374423);
#38633=VERTEX_POINT('',#374498);
#38634=VERTEX_POINT('',#374499);
#38635=VERTEX_POINT('',#374574);
#38636=VERTEX_POINT('',#374576);
#38637=VERTEX_POINT('',#374591);
#38638=VERTEX_POINT('',#374604);
#38639=VERTEX_POINT('',#374605);
#38640=VERTEX_POINT('',#374638);
#38641=VERTEX_POINT('',#374653);
#38642=VERTEX_POINT('',#374772);
#38643=VERTEX_POINT('',#374776);
#38644=VERTEX_POINT('',#374777);
#38645=VERTEX_POINT('',#374779);
#38646=VERTEX_POINT('',#374781);
#38647=VERTEX_POINT('',#374783);
#38648=VERTEX_POINT('',#374785);
#38649=VERTEX_POINT('',#374787);
#38650=VERTEX_POINT('',#374791);
#38651=VERTEX_POINT('',#374792);
#38652=VERTEX_POINT('',#374798);
#38653=VERTEX_POINT('',#374800);
#38654=VERTEX_POINT('',#374804);
#38655=VERTEX_POINT('',#374808);
#38656=VERTEX_POINT('',#374812);
#38657=VERTEX_POINT('',#374813);
#38658=VERTEX_POINT('',#374815);
#38659=VERTEX_POINT('',#374823);
#38660=VERTEX_POINT('',#374825);
#38661=VERTEX_POINT('',#374833);
#38662=VERTEX_POINT('',#374835);
#38663=VERTEX_POINT('',#374843);
#38664=VERTEX_POINT('',#374845);
#38665=VERTEX_POINT('',#374853);
#38666=VERTEX_POINT('',#374855);
#38667=VERTEX_POINT('',#374863);
#38668=VERTEX_POINT('',#374865);
#38669=VERTEX_POINT('',#374873);
#38670=VERTEX_POINT('',#374875);
#38671=VERTEX_POINT('',#374883);
#38672=VERTEX_POINT('',#374885);
#38673=VERTEX_POINT('',#374893);
#38674=VERTEX_POINT('',#374895);
#38675=VERTEX_POINT('',#374903);
#38676=VERTEX_POINT('',#374905);
#38677=VERTEX_POINT('',#374913);
#38678=VERTEX_POINT('',#374915);
#38679=VERTEX_POINT('',#374923);
#38680=VERTEX_POINT('',#374925);
#38681=VERTEX_POINT('',#374933);
#38682=VERTEX_POINT('',#374935);
#38683=VERTEX_POINT('',#374943);
#38684=VERTEX_POINT('',#374945);
#38685=VERTEX_POINT('',#374953);
#38686=VERTEX_POINT('',#374955);
#38687=VERTEX_POINT('',#374963);
#38688=VERTEX_POINT('',#374965);
#38689=VERTEX_POINT('',#374973);
#38690=VERTEX_POINT('',#374975);
#38691=VERTEX_POINT('',#374983);
#38692=VERTEX_POINT('',#374985);
#38693=VERTEX_POINT('',#374993);
#38694=VERTEX_POINT('',#374995);
#38695=VERTEX_POINT('',#375003);
#38696=VERTEX_POINT('',#375005);
#38697=VERTEX_POINT('',#375013);
#38698=VERTEX_POINT('',#375015);
#38699=VERTEX_POINT('',#375023);
#38700=VERTEX_POINT('',#375025);
#38701=VERTEX_POINT('',#375033);
#38702=VERTEX_POINT('',#375035);
#38703=VERTEX_POINT('',#375043);
#38704=VERTEX_POINT('',#375045);
#38705=VERTEX_POINT('',#375053);
#38706=VERTEX_POINT('',#375055);
#38707=VERTEX_POINT('',#375063);
#38708=VERTEX_POINT('',#375065);
#38709=VERTEX_POINT('',#375073);
#38710=VERTEX_POINT('',#375075);
#38711=VERTEX_POINT('',#375083);
#38712=VERTEX_POINT('',#375085);
#38713=VERTEX_POINT('',#375093);
#38714=VERTEX_POINT('',#375095);
#38715=VERTEX_POINT('',#375103);
#38716=VERTEX_POINT('',#375105);
#38717=VERTEX_POINT('',#375113);
#38718=VERTEX_POINT('',#375115);
#38719=VERTEX_POINT('',#375123);
#38720=VERTEX_POINT('',#375125);
#38721=VERTEX_POINT('',#375133);
#38722=VERTEX_POINT('',#375135);
#38723=VERTEX_POINT('',#375143);
#38724=VERTEX_POINT('',#375145);
#38725=VERTEX_POINT('',#375153);
#38726=VERTEX_POINT('',#375155);
#38727=VERTEX_POINT('',#375163);
#38728=VERTEX_POINT('',#375165);
#38729=VERTEX_POINT('',#375173);
#38730=VERTEX_POINT('',#375175);
#38731=VERTEX_POINT('',#375183);
#38732=VERTEX_POINT('',#375185);
#38733=VERTEX_POINT('',#375193);
#38734=VERTEX_POINT('',#375195);
#38735=VERTEX_POINT('',#375203);
#38736=VERTEX_POINT('',#375205);
#38737=VERTEX_POINT('',#375213);
#38738=VERTEX_POINT('',#375215);
#38739=VERTEX_POINT('',#375223);
#38740=VERTEX_POINT('',#375225);
#38741=VERTEX_POINT('',#375233);
#38742=VERTEX_POINT('',#375235);
#38743=VERTEX_POINT('',#375243);
#38744=VERTEX_POINT('',#375245);
#38745=VERTEX_POINT('',#375253);
#38746=VERTEX_POINT('',#375255);
#38747=VERTEX_POINT('',#375263);
#38748=VERTEX_POINT('',#375265);
#38749=VERTEX_POINT('',#375273);
#38750=VERTEX_POINT('',#375275);
#38751=VERTEX_POINT('',#375283);
#38752=VERTEX_POINT('',#375285);
#38753=VERTEX_POINT('',#375293);
#38754=VERTEX_POINT('',#375295);
#38755=VERTEX_POINT('',#375303);
#38756=VERTEX_POINT('',#375305);
#38757=VERTEX_POINT('',#375313);
#38758=VERTEX_POINT('',#375315);
#38759=VERTEX_POINT('',#375323);
#38760=VERTEX_POINT('',#375325);
#38761=VERTEX_POINT('',#375333);
#38762=VERTEX_POINT('',#375335);
#38763=VERTEX_POINT('',#375343);
#38764=VERTEX_POINT('',#375345);
#38765=VERTEX_POINT('',#375353);
#38766=VERTEX_POINT('',#375355);
#38767=VERTEX_POINT('',#375363);
#38768=VERTEX_POINT('',#375365);
#38769=VERTEX_POINT('',#375373);
#38770=VERTEX_POINT('',#375375);
#38771=VERTEX_POINT('',#375383);
#38772=VERTEX_POINT('',#375385);
#38773=VERTEX_POINT('',#375393);
#38774=VERTEX_POINT('',#375395);
#38775=VERTEX_POINT('',#375403);
#38776=VERTEX_POINT('',#375405);
#38777=VERTEX_POINT('',#375413);
#38778=VERTEX_POINT('',#375415);
#38779=VERTEX_POINT('',#375423);
#38780=VERTEX_POINT('',#375425);
#38781=VERTEX_POINT('',#375433);
#38782=VERTEX_POINT('',#375435);
#38783=VERTEX_POINT('',#375443);
#38784=VERTEX_POINT('',#375445);
#38785=VERTEX_POINT('',#375453);
#38786=VERTEX_POINT('',#375455);
#38787=VERTEX_POINT('',#375463);
#38788=VERTEX_POINT('',#375465);
#38789=VERTEX_POINT('',#375473);
#38790=VERTEX_POINT('',#375475);
#38791=VERTEX_POINT('',#375483);
#38792=VERTEX_POINT('',#375485);
#38793=VERTEX_POINT('',#375493);
#38794=VERTEX_POINT('',#375495);
#38795=VERTEX_POINT('',#375503);
#38796=VERTEX_POINT('',#375505);
#38797=VERTEX_POINT('',#375513);
#38798=VERTEX_POINT('',#375515);
#38799=VERTEX_POINT('',#375523);
#38800=VERTEX_POINT('',#375525);
#38801=VERTEX_POINT('',#375533);
#38802=VERTEX_POINT('',#375535);
#38803=VERTEX_POINT('',#375543);
#38804=VERTEX_POINT('',#375545);
#38805=VERTEX_POINT('',#375553);
#38806=VERTEX_POINT('',#375555);
#38807=VERTEX_POINT('',#375563);
#38808=VERTEX_POINT('',#375565);
#38809=VERTEX_POINT('',#375573);
#38810=VERTEX_POINT('',#375575);
#38811=VERTEX_POINT('',#375583);
#38812=VERTEX_POINT('',#375585);
#38813=VERTEX_POINT('',#375593);
#38814=VERTEX_POINT('',#375595);
#38815=VERTEX_POINT('',#375603);
#38816=VERTEX_POINT('',#375605);
#38817=VERTEX_POINT('',#375613);
#38818=VERTEX_POINT('',#375615);
#38819=VERTEX_POINT('',#375623);
#38820=VERTEX_POINT('',#375625);
#38821=VERTEX_POINT('',#375633);
#38822=VERTEX_POINT('',#375635);
#38823=VERTEX_POINT('',#375643);
#38824=VERTEX_POINT('',#375645);
#38825=VERTEX_POINT('',#375653);
#38826=VERTEX_POINT('',#375655);
#38827=VERTEX_POINT('',#375663);
#38828=VERTEX_POINT('',#375665);
#38829=VERTEX_POINT('',#375673);
#38830=VERTEX_POINT('',#375675);
#38831=VERTEX_POINT('',#375683);
#38832=VERTEX_POINT('',#375685);
#38833=VERTEX_POINT('',#375693);
#38834=VERTEX_POINT('',#375695);
#38835=VERTEX_POINT('',#375703);
#38836=VERTEX_POINT('',#375705);
#38837=VERTEX_POINT('',#375713);
#38838=VERTEX_POINT('',#375715);
#38839=VERTEX_POINT('',#375723);
#38840=VERTEX_POINT('',#375725);
#38841=VERTEX_POINT('',#375733);
#38842=VERTEX_POINT('',#375735);
#38843=VERTEX_POINT('',#375743);
#38844=VERTEX_POINT('',#375745);
#38845=VERTEX_POINT('',#375753);
#38846=VERTEX_POINT('',#375755);
#38847=VERTEX_POINT('',#375763);
#38848=VERTEX_POINT('',#375765);
#38849=VERTEX_POINT('',#375773);
#38850=VERTEX_POINT('',#375775);
#38851=VERTEX_POINT('',#375783);
#38852=VERTEX_POINT('',#375785);
#38853=VERTEX_POINT('',#375793);
#38854=VERTEX_POINT('',#375795);
#38855=VERTEX_POINT('',#375797);
#38856=VERTEX_POINT('',#375800);
#38857=VERTEX_POINT('',#375802);
#38858=VERTEX_POINT('',#375810);
#38859=VERTEX_POINT('',#375812);
#38860=VERTEX_POINT('',#375820);
#38861=VERTEX_POINT('',#375822);
#38862=VERTEX_POINT('',#375830);
#38863=VERTEX_POINT('',#375832);
#38864=VERTEX_POINT('',#375840);
#38865=VERTEX_POINT('',#375842);
#38866=VERTEX_POINT('',#375850);
#38867=VERTEX_POINT('',#375852);
#38868=VERTEX_POINT('',#375860);
#38869=VERTEX_POINT('',#375862);
#38870=VERTEX_POINT('',#375870);
#38871=VERTEX_POINT('',#375872);
#38872=VERTEX_POINT('',#375880);
#38873=VERTEX_POINT('',#375882);
#38874=VERTEX_POINT('',#375890);
#38875=VERTEX_POINT('',#375892);
#38876=VERTEX_POINT('',#375900);
#38877=VERTEX_POINT('',#375902);
#38878=VERTEX_POINT('',#375910);
#38879=VERTEX_POINT('',#375912);
#38880=VERTEX_POINT('',#375920);
#38881=VERTEX_POINT('',#375922);
#38882=VERTEX_POINT('',#375930);
#38883=VERTEX_POINT('',#375932);
#38884=VERTEX_POINT('',#375940);
#38885=VERTEX_POINT('',#375942);
#38886=VERTEX_POINT('',#375950);
#38887=VERTEX_POINT('',#375952);
#38888=VERTEX_POINT('',#375960);
#38889=VERTEX_POINT('',#375962);
#38890=VERTEX_POINT('',#375970);
#38891=VERTEX_POINT('',#375972);
#38892=VERTEX_POINT('',#375980);
#38893=VERTEX_POINT('',#375982);
#38894=VERTEX_POINT('',#375990);
#38895=VERTEX_POINT('',#375992);
#38896=VERTEX_POINT('',#376000);
#38897=VERTEX_POINT('',#376002);
#38898=VERTEX_POINT('',#376010);
#38899=VERTEX_POINT('',#376012);
#38900=VERTEX_POINT('',#376020);
#38901=VERTEX_POINT('',#376022);
#38902=VERTEX_POINT('',#376030);
#38903=VERTEX_POINT('',#376032);
#38904=VERTEX_POINT('',#376040);
#38905=VERTEX_POINT('',#376042);
#38906=VERTEX_POINT('',#376050);
#38907=VERTEX_POINT('',#376052);
#38908=VERTEX_POINT('',#376060);
#38909=VERTEX_POINT('',#376062);
#38910=VERTEX_POINT('',#376070);
#38911=VERTEX_POINT('',#376072);
#38912=VERTEX_POINT('',#376080);
#38913=VERTEX_POINT('',#376082);
#38914=VERTEX_POINT('',#376090);
#38915=VERTEX_POINT('',#376092);
#38916=VERTEX_POINT('',#376100);
#38917=VERTEX_POINT('',#376102);
#38918=VERTEX_POINT('',#376110);
#38919=VERTEX_POINT('',#376112);
#38920=VERTEX_POINT('',#376120);
#38921=VERTEX_POINT('',#376122);
#38922=VERTEX_POINT('',#376130);
#38923=VERTEX_POINT('',#376132);
#38924=VERTEX_POINT('',#376140);
#38925=VERTEX_POINT('',#376142);
#38926=VERTEX_POINT('',#376150);
#38927=VERTEX_POINT('',#376152);
#38928=VERTEX_POINT('',#376160);
#38929=VERTEX_POINT('',#376162);
#38930=VERTEX_POINT('',#376170);
#38931=VERTEX_POINT('',#376172);
#38932=VERTEX_POINT('',#376180);
#38933=VERTEX_POINT('',#376182);
#38934=VERTEX_POINT('',#376190);
#38935=VERTEX_POINT('',#376192);
#38936=VERTEX_POINT('',#376200);
#38937=VERTEX_POINT('',#376202);
#38938=VERTEX_POINT('',#376210);
#38939=VERTEX_POINT('',#376212);
#38940=VERTEX_POINT('',#376220);
#38941=VERTEX_POINT('',#376222);
#38942=VERTEX_POINT('',#376230);
#38943=VERTEX_POINT('',#376232);
#38944=VERTEX_POINT('',#376240);
#38945=VERTEX_POINT('',#376242);
#38946=VERTEX_POINT('',#376250);
#38947=VERTEX_POINT('',#376252);
#38948=VERTEX_POINT('',#376260);
#38949=VERTEX_POINT('',#376262);
#38950=VERTEX_POINT('',#376270);
#38951=VERTEX_POINT('',#376272);
#38952=VERTEX_POINT('',#376280);
#38953=VERTEX_POINT('',#376282);
#38954=VERTEX_POINT('',#376290);
#38955=VERTEX_POINT('',#376292);
#38956=VERTEX_POINT('',#376300);
#38957=VERTEX_POINT('',#376302);
#38958=VERTEX_POINT('',#376310);
#38959=VERTEX_POINT('',#376312);
#38960=VERTEX_POINT('',#376320);
#38961=VERTEX_POINT('',#376322);
#38962=VERTEX_POINT('',#376330);
#38963=VERTEX_POINT('',#376332);
#38964=VERTEX_POINT('',#376340);
#38965=VERTEX_POINT('',#376342);
#38966=VERTEX_POINT('',#376350);
#38967=VERTEX_POINT('',#376352);
#38968=VERTEX_POINT('',#376360);
#38969=VERTEX_POINT('',#376362);
#38970=VERTEX_POINT('',#376370);
#38971=VERTEX_POINT('',#376372);
#38972=VERTEX_POINT('',#376380);
#38973=VERTEX_POINT('',#376382);
#38974=VERTEX_POINT('',#376390);
#38975=VERTEX_POINT('',#376392);
#38976=VERTEX_POINT('',#376400);
#38977=VERTEX_POINT('',#376402);
#38978=VERTEX_POINT('',#376410);
#38979=VERTEX_POINT('',#376412);
#38980=VERTEX_POINT('',#376420);
#38981=VERTEX_POINT('',#376422);
#38982=VERTEX_POINT('',#376430);
#38983=VERTEX_POINT('',#376432);
#38984=VERTEX_POINT('',#376440);
#38985=VERTEX_POINT('',#376442);
#38986=VERTEX_POINT('',#376450);
#38987=VERTEX_POINT('',#376452);
#38988=VERTEX_POINT('',#376460);
#38989=VERTEX_POINT('',#376462);
#38990=VERTEX_POINT('',#376470);
#38991=VERTEX_POINT('',#376472);
#38992=VERTEX_POINT('',#376480);
#38993=VERTEX_POINT('',#376482);
#38994=VERTEX_POINT('',#376490);
#38995=VERTEX_POINT('',#376492);
#38996=VERTEX_POINT('',#376500);
#38997=VERTEX_POINT('',#376502);
#38998=VERTEX_POINT('',#376510);
#38999=VERTEX_POINT('',#376512);
#39000=VERTEX_POINT('',#376520);
#39001=VERTEX_POINT('',#376522);
#39002=VERTEX_POINT('',#376530);
#39003=VERTEX_POINT('',#376532);
#39004=VERTEX_POINT('',#376540);
#39005=VERTEX_POINT('',#376542);
#39006=VERTEX_POINT('',#376550);
#39007=VERTEX_POINT('',#376552);
#39008=VERTEX_POINT('',#376560);
#39009=VERTEX_POINT('',#376562);
#39010=VERTEX_POINT('',#376570);
#39011=VERTEX_POINT('',#376572);
#39012=VERTEX_POINT('',#376580);
#39013=VERTEX_POINT('',#376582);
#39014=VERTEX_POINT('',#376590);
#39015=VERTEX_POINT('',#376592);
#39016=VERTEX_POINT('',#376600);
#39017=VERTEX_POINT('',#376602);
#39018=VERTEX_POINT('',#376610);
#39019=VERTEX_POINT('',#376612);
#39020=VERTEX_POINT('',#376620);
#39021=VERTEX_POINT('',#376622);
#39022=VERTEX_POINT('',#376630);
#39023=VERTEX_POINT('',#376632);
#39024=VERTEX_POINT('',#376640);
#39025=VERTEX_POINT('',#376642);
#39026=VERTEX_POINT('',#376650);
#39027=VERTEX_POINT('',#376652);
#39028=VERTEX_POINT('',#376660);
#39029=VERTEX_POINT('',#376662);
#39030=VERTEX_POINT('',#376670);
#39031=VERTEX_POINT('',#376672);
#39032=VERTEX_POINT('',#376680);
#39033=VERTEX_POINT('',#376682);
#39034=VERTEX_POINT('',#376690);
#39035=VERTEX_POINT('',#376692);
#39036=VERTEX_POINT('',#376700);
#39037=VERTEX_POINT('',#376702);
#39038=VERTEX_POINT('',#376710);
#39039=VERTEX_POINT('',#376712);
#39040=VERTEX_POINT('',#376720);
#39041=VERTEX_POINT('',#376722);
#39042=VERTEX_POINT('',#376730);
#39043=VERTEX_POINT('',#376732);
#39044=VERTEX_POINT('',#376740);
#39045=VERTEX_POINT('',#376742);
#39046=VERTEX_POINT('',#376750);
#39047=VERTEX_POINT('',#376752);
#39048=VERTEX_POINT('',#376760);
#39049=VERTEX_POINT('',#376762);
#39050=VERTEX_POINT('',#376770);
#39051=VERTEX_POINT('',#376780);
#39052=VERTEX_POINT('',#376784);
#39053=VERTEX_POINT('',#376785);
#39054=VERTEX_POINT('',#376787);
#39055=VERTEX_POINT('',#376789);
#39056=VERTEX_POINT('',#376791);
#39057=VERTEX_POINT('',#376793);
#39058=VERTEX_POINT('',#376795);
#39059=VERTEX_POINT('',#376797);
#39060=VERTEX_POINT('',#376799);
#39061=VERTEX_POINT('',#376801);
#39062=VERTEX_POINT('',#376803);
#39063=VERTEX_POINT('',#376805);
#39064=VERTEX_POINT('',#376807);
#39065=VERTEX_POINT('',#376809);
#39066=VERTEX_POINT('',#376811);
#39067=VERTEX_POINT('',#376813);
#39068=VERTEX_POINT('',#376815);
#39069=VERTEX_POINT('',#376817);
#39070=VERTEX_POINT('',#376819);
#39071=VERTEX_POINT('',#376821);
#39072=VERTEX_POINT('',#376823);
#39073=VERTEX_POINT('',#376825);
#39074=VERTEX_POINT('',#376827);
#39075=VERTEX_POINT('',#376829);
#39076=VERTEX_POINT('',#376831);
#39077=VERTEX_POINT('',#376833);
#39078=VERTEX_POINT('',#376835);
#39079=VERTEX_POINT('',#376837);
#39080=VERTEX_POINT('',#376839);
#39081=VERTEX_POINT('',#376841);
#39082=VERTEX_POINT('',#376843);
#39083=VERTEX_POINT('',#376845);
#39084=VERTEX_POINT('',#376847);
#39085=VERTEX_POINT('',#376849);
#39086=VERTEX_POINT('',#376851);
#39087=VERTEX_POINT('',#376853);
#39088=VERTEX_POINT('',#376855);
#39089=VERTEX_POINT('',#376857);
#39090=VERTEX_POINT('',#376859);
#39091=VERTEX_POINT('',#376861);
#39092=VERTEX_POINT('',#376863);
#39093=VERTEX_POINT('',#376865);
#39094=VERTEX_POINT('',#376867);
#39095=VERTEX_POINT('',#376869);
#39096=VERTEX_POINT('',#376871);
#39097=VERTEX_POINT('',#376873);
#39098=VERTEX_POINT('',#376875);
#39099=VERTEX_POINT('',#376877);
#39100=VERTEX_POINT('',#376879);
#39101=VERTEX_POINT('',#376881);
#39102=VERTEX_POINT('',#376883);
#39103=VERTEX_POINT('',#376885);
#39104=VERTEX_POINT('',#376887);
#39105=VERTEX_POINT('',#376889);
#39106=VERTEX_POINT('',#376891);
#39107=VERTEX_POINT('',#376893);
#39108=VERTEX_POINT('',#376895);
#39109=VERTEX_POINT('',#376897);
#39110=VERTEX_POINT('',#376899);
#39111=VERTEX_POINT('',#376901);
#39112=VERTEX_POINT('',#376903);
#39113=VERTEX_POINT('',#376905);
#39114=VERTEX_POINT('',#376907);
#39115=VERTEX_POINT('',#376909);
#39116=VERTEX_POINT('',#376911);
#39117=VERTEX_POINT('',#376913);
#39118=VERTEX_POINT('',#376915);
#39119=VERTEX_POINT('',#376917);
#39120=VERTEX_POINT('',#376919);
#39121=VERTEX_POINT('',#376921);
#39122=VERTEX_POINT('',#376923);
#39123=VERTEX_POINT('',#376925);
#39124=VERTEX_POINT('',#376927);
#39125=VERTEX_POINT('',#376929);
#39126=VERTEX_POINT('',#376931);
#39127=VERTEX_POINT('',#376933);
#39128=VERTEX_POINT('',#376935);
#39129=VERTEX_POINT('',#376937);
#39130=VERTEX_POINT('',#376939);
#39131=VERTEX_POINT('',#376941);
#39132=VERTEX_POINT('',#376943);
#39133=VERTEX_POINT('',#376945);
#39134=VERTEX_POINT('',#376947);
#39135=VERTEX_POINT('',#376949);
#39136=VERTEX_POINT('',#376951);
#39137=VERTEX_POINT('',#376953);
#39138=VERTEX_POINT('',#376955);
#39139=VERTEX_POINT('',#376957);
#39140=VERTEX_POINT('',#376959);
#39141=VERTEX_POINT('',#376961);
#39142=VERTEX_POINT('',#376963);
#39143=VERTEX_POINT('',#376965);
#39144=VERTEX_POINT('',#376967);
#39145=VERTEX_POINT('',#376969);
#39146=VERTEX_POINT('',#376971);
#39147=VERTEX_POINT('',#376973);
#39148=VERTEX_POINT('',#376975);
#39149=VERTEX_POINT('',#376977);
#39150=VERTEX_POINT('',#376979);
#39151=VERTEX_POINT('',#376981);
#39152=VERTEX_POINT('',#376983);
#39153=VERTEX_POINT('',#376985);
#39154=VERTEX_POINT('',#376987);
#39155=VERTEX_POINT('',#376989);
#39156=VERTEX_POINT('',#376991);
#39157=VERTEX_POINT('',#376993);
#39158=VERTEX_POINT('',#376995);
#39159=VERTEX_POINT('',#376997);
#39160=VERTEX_POINT('',#376999);
#39161=VERTEX_POINT('',#377001);
#39162=VERTEX_POINT('',#377003);
#39163=VERTEX_POINT('',#377005);
#39164=VERTEX_POINT('',#377007);
#39165=VERTEX_POINT('',#377009);
#39166=VERTEX_POINT('',#377011);
#39167=VERTEX_POINT('',#377013);
#39168=VERTEX_POINT('',#377015);
#39169=VERTEX_POINT('',#377017);
#39170=VERTEX_POINT('',#377019);
#39171=VERTEX_POINT('',#377021);
#39172=VERTEX_POINT('',#377023);
#39173=VERTEX_POINT('',#377025);
#39174=VERTEX_POINT('',#377027);
#39175=VERTEX_POINT('',#377029);
#39176=VERTEX_POINT('',#377031);
#39177=VERTEX_POINT('',#377033);
#39178=VERTEX_POINT('',#377035);
#39179=VERTEX_POINT('',#377037);
#39180=VERTEX_POINT('',#377039);
#39181=VERTEX_POINT('',#377041);
#39182=VERTEX_POINT('',#377043);
#39183=VERTEX_POINT('',#377045);
#39184=VERTEX_POINT('',#377047);
#39185=VERTEX_POINT('',#377049);
#39186=VERTEX_POINT('',#377051);
#39187=VERTEX_POINT('',#377053);
#39188=VERTEX_POINT('',#377055);
#39189=VERTEX_POINT('',#377057);
#39190=VERTEX_POINT('',#377059);
#39191=VERTEX_POINT('',#377061);
#39192=VERTEX_POINT('',#377063);
#39193=VERTEX_POINT('',#377065);
#39194=VERTEX_POINT('',#377067);
#39195=VERTEX_POINT('',#377069);
#39196=VERTEX_POINT('',#377071);
#39197=VERTEX_POINT('',#377073);
#39198=VERTEX_POINT('',#377075);
#39199=VERTEX_POINT('',#377077);
#39200=VERTEX_POINT('',#377079);
#39201=VERTEX_POINT('',#377081);
#39202=VERTEX_POINT('',#377083);
#39203=VERTEX_POINT('',#377085);
#39204=VERTEX_POINT('',#377087);
#39205=VERTEX_POINT('',#377089);
#39206=VERTEX_POINT('',#377091);
#39207=VERTEX_POINT('',#377093);
#39208=VERTEX_POINT('',#377095);
#39209=VERTEX_POINT('',#377097);
#39210=VERTEX_POINT('',#377099);
#39211=VERTEX_POINT('',#377101);
#39212=VERTEX_POINT('',#377103);
#39213=VERTEX_POINT('',#377105);
#39214=VERTEX_POINT('',#377107);
#39215=VERTEX_POINT('',#377109);
#39216=VERTEX_POINT('',#377111);
#39217=VERTEX_POINT('',#377113);
#39218=VERTEX_POINT('',#377115);
#39219=VERTEX_POINT('',#377117);
#39220=VERTEX_POINT('',#377119);
#39221=VERTEX_POINT('',#377121);
#39222=VERTEX_POINT('',#377123);
#39223=VERTEX_POINT('',#377125);
#39224=VERTEX_POINT('',#377127);
#39225=VERTEX_POINT('',#377129);
#39226=VERTEX_POINT('',#377131);
#39227=VERTEX_POINT('',#377133);
#39228=VERTEX_POINT('',#377135);
#39229=VERTEX_POINT('',#377137);
#39230=VERTEX_POINT('',#377139);
#39231=VERTEX_POINT('',#377141);
#39232=VERTEX_POINT('',#377143);
#39233=VERTEX_POINT('',#377145);
#39234=VERTEX_POINT('',#377147);
#39235=VERTEX_POINT('',#377149);
#39236=VERTEX_POINT('',#377151);
#39237=VERTEX_POINT('',#377153);
#39238=VERTEX_POINT('',#377155);
#39239=VERTEX_POINT('',#377157);
#39240=VERTEX_POINT('',#377159);
#39241=VERTEX_POINT('',#377161);
#39242=VERTEX_POINT('',#377163);
#39243=VERTEX_POINT('',#377165);
#39244=VERTEX_POINT('',#377167);
#39245=VERTEX_POINT('',#377169);
#39246=VERTEX_POINT('',#377171);
#39247=VERTEX_POINT('',#377173);
#39248=VERTEX_POINT('',#377175);
#39249=VERTEX_POINT('',#377177);
#39250=VERTEX_POINT('',#377179);
#39251=VERTEX_POINT('',#377181);
#39252=VERTEX_POINT('',#377183);
#39253=VERTEX_POINT('',#377185);
#39254=VERTEX_POINT('',#377187);
#39255=VERTEX_POINT('',#377189);
#39256=VERTEX_POINT('',#377191);
#39257=VERTEX_POINT('',#377193);
#39258=VERTEX_POINT('',#377195);
#39259=VERTEX_POINT('',#377197);
#39260=VERTEX_POINT('',#377199);
#39261=VERTEX_POINT('',#377201);
#39262=VERTEX_POINT('',#377203);
#39263=VERTEX_POINT('',#377205);
#39264=VERTEX_POINT('',#377207);
#39265=VERTEX_POINT('',#377209);
#39266=VERTEX_POINT('',#377211);
#39267=VERTEX_POINT('',#377213);
#39268=VERTEX_POINT('',#377215);
#39269=VERTEX_POINT('',#377217);
#39270=VERTEX_POINT('',#377219);
#39271=VERTEX_POINT('',#377221);
#39272=VERTEX_POINT('',#377223);
#39273=VERTEX_POINT('',#377225);
#39274=VERTEX_POINT('',#377227);
#39275=VERTEX_POINT('',#377229);
#39276=VERTEX_POINT('',#377231);
#39277=VERTEX_POINT('',#377233);
#39278=VERTEX_POINT('',#377235);
#39279=VERTEX_POINT('',#377237);
#39280=VERTEX_POINT('',#377239);
#39281=VERTEX_POINT('',#377241);
#39282=VERTEX_POINT('',#377243);
#39283=VERTEX_POINT('',#377245);
#39284=VERTEX_POINT('',#377247);
#39285=VERTEX_POINT('',#377249);
#39286=VERTEX_POINT('',#377251);
#39287=VERTEX_POINT('',#377253);
#39288=VERTEX_POINT('',#377255);
#39289=VERTEX_POINT('',#377257);
#39290=VERTEX_POINT('',#377259);
#39291=VERTEX_POINT('',#377261);
#39292=VERTEX_POINT('',#377263);
#39293=VERTEX_POINT('',#377265);
#39294=VERTEX_POINT('',#377267);
#39295=VERTEX_POINT('',#377269);
#39296=VERTEX_POINT('',#377271);
#39297=VERTEX_POINT('',#377273);
#39298=VERTEX_POINT('',#377275);
#39299=VERTEX_POINT('',#377277);
#39300=VERTEX_POINT('',#377279);
#39301=VERTEX_POINT('',#377281);
#39302=VERTEX_POINT('',#377283);
#39303=VERTEX_POINT('',#377285);
#39304=VERTEX_POINT('',#377287);
#39305=VERTEX_POINT('',#377289);
#39306=VERTEX_POINT('',#377291);
#39307=VERTEX_POINT('',#377293);
#39308=VERTEX_POINT('',#377295);
#39309=VERTEX_POINT('',#377297);
#39310=VERTEX_POINT('',#377299);
#39311=VERTEX_POINT('',#377301);
#39312=VERTEX_POINT('',#377303);
#39313=VERTEX_POINT('',#377305);
#39314=VERTEX_POINT('',#377307);
#39315=VERTEX_POINT('',#377309);
#39316=VERTEX_POINT('',#377311);
#39317=VERTEX_POINT('',#377313);
#39318=VERTEX_POINT('',#377315);
#39319=VERTEX_POINT('',#377317);
#39320=VERTEX_POINT('',#377319);
#39321=VERTEX_POINT('',#377321);
#39322=VERTEX_POINT('',#377323);
#39323=VERTEX_POINT('',#377325);
#39324=VERTEX_POINT('',#377327);
#39325=VERTEX_POINT('',#377329);
#39326=VERTEX_POINT('',#377331);
#39327=VERTEX_POINT('',#377333);
#39328=VERTEX_POINT('',#377335);
#39329=VERTEX_POINT('',#377337);
#39330=VERTEX_POINT('',#377339);
#39331=VERTEX_POINT('',#377341);
#39332=VERTEX_POINT('',#377343);
#39333=VERTEX_POINT('',#377345);
#39334=VERTEX_POINT('',#377347);
#39335=VERTEX_POINT('',#377349);
#39336=VERTEX_POINT('',#377351);
#39337=VERTEX_POINT('',#377353);
#39338=VERTEX_POINT('',#377355);
#39339=VERTEX_POINT('',#377357);
#39340=VERTEX_POINT('',#377359);
#39341=VERTEX_POINT('',#377361);
#39342=VERTEX_POINT('',#377363);
#39343=VERTEX_POINT('',#377365);
#39344=VERTEX_POINT('',#377367);
#39345=VERTEX_POINT('',#377369);
#39346=VERTEX_POINT('',#377371);
#39347=VERTEX_POINT('',#377373);
#39348=VERTEX_POINT('',#377376);
#39349=VERTEX_POINT('',#377378);
#39350=VERTEX_POINT('',#377380);
#39351=VERTEX_POINT('',#377382);
#39352=VERTEX_POINT('',#377384);
#39353=VERTEX_POINT('',#377386);
#39354=VERTEX_POINT('',#377388);
#39355=VERTEX_POINT('',#377390);
#39356=VERTEX_POINT('',#377392);
#39357=VERTEX_POINT('',#377394);
#39358=VERTEX_POINT('',#377396);
#39359=VERTEX_POINT('',#377398);
#39360=VERTEX_POINT('',#377400);
#39361=VERTEX_POINT('',#377402);
#39362=VERTEX_POINT('',#377404);
#39363=VERTEX_POINT('',#377406);
#39364=VERTEX_POINT('',#377408);
#39365=VERTEX_POINT('',#377410);
#39366=VERTEX_POINT('',#377412);
#39367=VERTEX_POINT('',#377414);
#39368=VERTEX_POINT('',#377416);
#39369=VERTEX_POINT('',#377418);
#39370=VERTEX_POINT('',#377420);
#39371=VERTEX_POINT('',#377422);
#39372=VERTEX_POINT('',#377424);
#39373=VERTEX_POINT('',#377426);
#39374=VERTEX_POINT('',#377428);
#39375=VERTEX_POINT('',#377430);
#39376=VERTEX_POINT('',#377432);
#39377=VERTEX_POINT('',#377434);
#39378=VERTEX_POINT('',#377436);
#39379=VERTEX_POINT('',#377438);
#39380=VERTEX_POINT('',#377440);
#39381=VERTEX_POINT('',#377442);
#39382=VERTEX_POINT('',#377444);
#39383=VERTEX_POINT('',#377446);
#39384=VERTEX_POINT('',#377448);
#39385=VERTEX_POINT('',#377450);
#39386=VERTEX_POINT('',#377452);
#39387=VERTEX_POINT('',#377454);
#39388=VERTEX_POINT('',#377456);
#39389=VERTEX_POINT('',#377458);
#39390=VERTEX_POINT('',#377460);
#39391=VERTEX_POINT('',#377462);
#39392=VERTEX_POINT('',#377464);
#39393=VERTEX_POINT('',#377466);
#39394=VERTEX_POINT('',#377468);
#39395=VERTEX_POINT('',#377470);
#39396=VERTEX_POINT('',#377472);
#39397=VERTEX_POINT('',#377474);
#39398=VERTEX_POINT('',#377476);
#39399=VERTEX_POINT('',#377478);
#39400=VERTEX_POINT('',#377480);
#39401=VERTEX_POINT('',#377482);
#39402=VERTEX_POINT('',#377484);
#39403=VERTEX_POINT('',#377486);
#39404=VERTEX_POINT('',#377488);
#39405=VERTEX_POINT('',#377490);
#39406=VERTEX_POINT('',#377492);
#39407=VERTEX_POINT('',#377494);
#39408=VERTEX_POINT('',#377496);
#39409=VERTEX_POINT('',#377498);
#39410=VERTEX_POINT('',#377500);
#39411=VERTEX_POINT('',#377502);
#39412=VERTEX_POINT('',#377504);
#39413=VERTEX_POINT('',#377506);
#39414=VERTEX_POINT('',#377508);
#39415=VERTEX_POINT('',#377510);
#39416=VERTEX_POINT('',#377512);
#39417=VERTEX_POINT('',#377514);
#39418=VERTEX_POINT('',#377516);
#39419=VERTEX_POINT('',#377518);
#39420=VERTEX_POINT('',#377520);
#39421=VERTEX_POINT('',#377522);
#39422=VERTEX_POINT('',#377524);
#39423=VERTEX_POINT('',#377526);
#39424=VERTEX_POINT('',#377528);
#39425=VERTEX_POINT('',#377530);
#39426=VERTEX_POINT('',#377532);
#39427=VERTEX_POINT('',#377534);
#39428=VERTEX_POINT('',#377536);
#39429=VERTEX_POINT('',#377538);
#39430=VERTEX_POINT('',#377540);
#39431=VERTEX_POINT('',#377542);
#39432=VERTEX_POINT('',#377544);
#39433=VERTEX_POINT('',#377546);
#39434=VERTEX_POINT('',#377548);
#39435=VERTEX_POINT('',#377550);
#39436=VERTEX_POINT('',#377552);
#39437=VERTEX_POINT('',#377554);
#39438=VERTEX_POINT('',#377556);
#39439=VERTEX_POINT('',#377558);
#39440=VERTEX_POINT('',#377560);
#39441=VERTEX_POINT('',#377562);
#39442=VERTEX_POINT('',#377564);
#39443=VERTEX_POINT('',#377566);
#39444=VERTEX_POINT('',#377568);
#39445=VERTEX_POINT('',#377570);
#39446=VERTEX_POINT('',#377572);
#39447=VERTEX_POINT('',#377574);
#39448=VERTEX_POINT('',#377576);
#39449=VERTEX_POINT('',#377578);
#39450=VERTEX_POINT('',#377580);
#39451=VERTEX_POINT('',#377582);
#39452=VERTEX_POINT('',#377584);
#39453=VERTEX_POINT('',#377586);
#39454=VERTEX_POINT('',#377588);
#39455=VERTEX_POINT('',#377590);
#39456=VERTEX_POINT('',#377592);
#39457=VERTEX_POINT('',#377594);
#39458=VERTEX_POINT('',#377596);
#39459=VERTEX_POINT('',#377598);
#39460=VERTEX_POINT('',#377600);
#39461=VERTEX_POINT('',#377602);
#39462=VERTEX_POINT('',#377604);
#39463=VERTEX_POINT('',#377606);
#39464=VERTEX_POINT('',#377608);
#39465=VERTEX_POINT('',#377610);
#39466=VERTEX_POINT('',#377612);
#39467=VERTEX_POINT('',#377614);
#39468=VERTEX_POINT('',#377616);
#39469=VERTEX_POINT('',#377618);
#39470=VERTEX_POINT('',#377620);
#39471=VERTEX_POINT('',#377622);
#39472=VERTEX_POINT('',#377624);
#39473=VERTEX_POINT('',#377626);
#39474=VERTEX_POINT('',#377628);
#39475=VERTEX_POINT('',#377630);
#39476=VERTEX_POINT('',#377632);
#39477=VERTEX_POINT('',#377634);
#39478=VERTEX_POINT('',#377636);
#39479=VERTEX_POINT('',#377638);
#39480=VERTEX_POINT('',#377640);
#39481=VERTEX_POINT('',#377642);
#39482=VERTEX_POINT('',#377644);
#39483=VERTEX_POINT('',#377646);
#39484=VERTEX_POINT('',#377648);
#39485=VERTEX_POINT('',#377650);
#39486=VERTEX_POINT('',#377652);
#39487=VERTEX_POINT('',#377654);
#39488=VERTEX_POINT('',#377656);
#39489=VERTEX_POINT('',#377658);
#39490=VERTEX_POINT('',#377660);
#39491=VERTEX_POINT('',#377662);
#39492=VERTEX_POINT('',#377664);
#39493=VERTEX_POINT('',#377666);
#39494=VERTEX_POINT('',#377668);
#39495=VERTEX_POINT('',#377670);
#39496=VERTEX_POINT('',#377672);
#39497=VERTEX_POINT('',#377674);
#39498=VERTEX_POINT('',#377676);
#39499=VERTEX_POINT('',#377678);
#39500=VERTEX_POINT('',#377680);
#39501=VERTEX_POINT('',#377682);
#39502=VERTEX_POINT('',#377684);
#39503=VERTEX_POINT('',#377686);
#39504=VERTEX_POINT('',#377688);
#39505=VERTEX_POINT('',#377690);
#39506=VERTEX_POINT('',#377692);
#39507=VERTEX_POINT('',#377694);
#39508=VERTEX_POINT('',#377696);
#39509=VERTEX_POINT('',#377698);
#39510=VERTEX_POINT('',#377700);
#39511=VERTEX_POINT('',#377702);
#39512=VERTEX_POINT('',#377704);
#39513=VERTEX_POINT('',#377706);
#39514=VERTEX_POINT('',#377708);
#39515=VERTEX_POINT('',#377710);
#39516=VERTEX_POINT('',#377712);
#39517=VERTEX_POINT('',#377714);
#39518=VERTEX_POINT('',#377716);
#39519=VERTEX_POINT('',#377718);
#39520=VERTEX_POINT('',#377720);
#39521=VERTEX_POINT('',#377722);
#39522=VERTEX_POINT('',#377724);
#39523=VERTEX_POINT('',#377726);
#39524=VERTEX_POINT('',#377728);
#39525=VERTEX_POINT('',#377730);
#39526=VERTEX_POINT('',#377732);
#39527=VERTEX_POINT('',#377734);
#39528=VERTEX_POINT('',#377736);
#39529=VERTEX_POINT('',#377738);
#39530=VERTEX_POINT('',#377740);
#39531=VERTEX_POINT('',#377742);
#39532=VERTEX_POINT('',#377744);
#39533=VERTEX_POINT('',#377746);
#39534=VERTEX_POINT('',#377748);
#39535=VERTEX_POINT('',#377750);
#39536=VERTEX_POINT('',#377752);
#39537=VERTEX_POINT('',#377754);
#39538=VERTEX_POINT('',#377756);
#39539=VERTEX_POINT('',#377758);
#39540=VERTEX_POINT('',#377760);
#39541=VERTEX_POINT('',#377762);
#39542=VERTEX_POINT('',#377764);
#39543=VERTEX_POINT('',#377766);
#39544=VERTEX_POINT('',#377768);
#39545=VERTEX_POINT('',#377770);
#39546=VERTEX_POINT('',#377772);
#39547=VERTEX_POINT('',#377774);
#39548=VERTEX_POINT('',#377776);
#39549=VERTEX_POINT('',#377778);
#39550=VERTEX_POINT('',#377780);
#39551=VERTEX_POINT('',#377782);
#39552=VERTEX_POINT('',#377784);
#39553=VERTEX_POINT('',#377786);
#39554=VERTEX_POINT('',#377788);
#39555=VERTEX_POINT('',#377790);
#39556=VERTEX_POINT('',#377792);
#39557=VERTEX_POINT('',#377794);
#39558=VERTEX_POINT('',#377796);
#39559=VERTEX_POINT('',#377798);
#39560=VERTEX_POINT('',#377800);
#39561=VERTEX_POINT('',#377802);
#39562=VERTEX_POINT('',#377804);
#39563=VERTEX_POINT('',#377806);
#39564=VERTEX_POINT('',#377808);
#39565=VERTEX_POINT('',#377810);
#39566=VERTEX_POINT('',#377812);
#39567=VERTEX_POINT('',#377814);
#39568=VERTEX_POINT('',#377816);
#39569=VERTEX_POINT('',#377818);
#39570=VERTEX_POINT('',#377820);
#39571=VERTEX_POINT('',#377822);
#39572=VERTEX_POINT('',#377824);
#39573=VERTEX_POINT('',#377826);
#39574=VERTEX_POINT('',#377828);
#39575=VERTEX_POINT('',#377830);
#39576=VERTEX_POINT('',#377832);
#39577=VERTEX_POINT('',#377834);
#39578=VERTEX_POINT('',#377836);
#39579=VERTEX_POINT('',#377838);
#39580=VERTEX_POINT('',#377840);
#39581=VERTEX_POINT('',#377842);
#39582=VERTEX_POINT('',#377844);
#39583=VERTEX_POINT('',#377846);
#39584=VERTEX_POINT('',#377848);
#39585=VERTEX_POINT('',#377850);
#39586=VERTEX_POINT('',#377852);
#39587=VERTEX_POINT('',#377854);
#39588=VERTEX_POINT('',#377856);
#39589=VERTEX_POINT('',#377858);
#39590=VERTEX_POINT('',#377860);
#39591=VERTEX_POINT('',#377862);
#39592=VERTEX_POINT('',#377864);
#39593=VERTEX_POINT('',#377866);
#39594=VERTEX_POINT('',#377868);
#39595=VERTEX_POINT('',#377870);
#39596=VERTEX_POINT('',#377872);
#39597=VERTEX_POINT('',#377874);
#39598=VERTEX_POINT('',#377876);
#39599=VERTEX_POINT('',#377878);
#39600=VERTEX_POINT('',#377880);
#39601=VERTEX_POINT('',#377882);
#39602=VERTEX_POINT('',#377884);
#39603=VERTEX_POINT('',#377886);
#39604=VERTEX_POINT('',#377888);
#39605=VERTEX_POINT('',#377890);
#39606=VERTEX_POINT('',#377892);
#39607=VERTEX_POINT('',#377894);
#39608=VERTEX_POINT('',#377896);
#39609=VERTEX_POINT('',#377898);
#39610=VERTEX_POINT('',#377900);
#39611=VERTEX_POINT('',#377902);
#39612=VERTEX_POINT('',#377904);
#39613=VERTEX_POINT('',#377906);
#39614=VERTEX_POINT('',#377908);
#39615=VERTEX_POINT('',#377910);
#39616=VERTEX_POINT('',#377912);
#39617=VERTEX_POINT('',#377914);
#39618=VERTEX_POINT('',#377916);
#39619=VERTEX_POINT('',#377918);
#39620=VERTEX_POINT('',#377920);
#39621=VERTEX_POINT('',#377922);
#39622=VERTEX_POINT('',#377924);
#39623=VERTEX_POINT('',#377926);
#39624=VERTEX_POINT('',#377928);
#39625=VERTEX_POINT('',#377930);
#39626=VERTEX_POINT('',#377932);
#39627=VERTEX_POINT('',#377934);
#39628=VERTEX_POINT('',#377936);
#39629=VERTEX_POINT('',#377938);
#39630=VERTEX_POINT('',#377940);
#39631=VERTEX_POINT('',#377942);
#39632=VERTEX_POINT('',#377944);
#39633=VERTEX_POINT('',#377946);
#39634=VERTEX_POINT('',#377948);
#39635=VERTEX_POINT('',#377950);
#39636=VERTEX_POINT('',#377952);
#39637=VERTEX_POINT('',#377954);
#39638=VERTEX_POINT('',#377956);
#39639=VERTEX_POINT('',#377958);
#39640=VERTEX_POINT('',#377960);
#39641=VERTEX_POINT('',#378255);
#39642=VERTEX_POINT('',#378256);
#39643=VERTEX_POINT('',#378258);
#39644=VERTEX_POINT('',#378308);
#39645=VERTEX_POINT('',#378312);
#39646=VERTEX_POINT('',#378313);
#39647=VERTEX_POINT('',#378319);
#39648=VERTEX_POINT('',#378329);
#39649=VERTEX_POINT('',#378334);
#39650=VERTEX_POINT('',#378336);
#39651=VERTEX_POINT('',#378346);
#39652=VERTEX_POINT('',#378350);
#39653=VERTEX_POINT('',#378354);
#39654=VERTEX_POINT('',#378358);
#39655=VERTEX_POINT('',#378362);
#39656=VERTEX_POINT('',#378366);
#39657=VERTEX_POINT('',#378367);
#39658=VERTEX_POINT('',#378370);
#39659=VERTEX_POINT('',#378372);
#39660=VERTEX_POINT('',#378392);
#39661=VERTEX_POINT('',#379922);
#39662=VERTEX_POINT('',#379923);
#39663=VERTEX_POINT('',#379928);
#39664=VERTEX_POINT('',#380135);
#39665=VERTEX_POINT('',#380136);
#39666=VERTEX_POINT('',#380138);
#39667=VERTEX_POINT('',#380143);
#39668=VERTEX_POINT('',#380145);
#39669=VERTEX_POINT('',#380155);
#39670=VERTEX_POINT('',#380156);
#39671=VERTEX_POINT('',#380158);
#39672=VERTEX_POINT('',#380163);
#39673=VERTEX_POINT('',#380165);
#39674=VERTEX_POINT('',#380237);
#39675=VERTEX_POINT('',#380269);
#39676=VERTEX_POINT('',#380300);
#39677=VERTEX_POINT('',#380439);
#39678=VERTEX_POINT('',#380440);
#39679=VERTEX_POINT('',#380442);
#39680=VERTEX_POINT('',#380447);
#39681=VERTEX_POINT('',#380449);
#39682=VERTEX_POINT('',#380459);
#39683=VERTEX_POINT('',#380460);
#39684=VERTEX_POINT('',#380462);
#39685=VERTEX_POINT('',#380467);
#39686=VERTEX_POINT('',#380469);
#39687=VERTEX_POINT('',#380541);
#39688=VERTEX_POINT('',#380573);
#39689=VERTEX_POINT('',#380604);
#39690=VERTEX_POINT('',#380743);
#39691=VERTEX_POINT('',#380744);
#39692=VERTEX_POINT('',#380746);
#39693=VERTEX_POINT('',#380751);
#39694=VERTEX_POINT('',#380753);
#39695=VERTEX_POINT('',#380763);
#39696=VERTEX_POINT('',#380764);
#39697=VERTEX_POINT('',#380766);
#39698=VERTEX_POINT('',#380771);
#39699=VERTEX_POINT('',#380773);
#39700=VERTEX_POINT('',#380845);
#39701=VERTEX_POINT('',#380877);
#39702=VERTEX_POINT('',#380908);
#39703=VERTEX_POINT('',#381047);
#39704=VERTEX_POINT('',#381048);
#39705=VERTEX_POINT('',#381050);
#39706=VERTEX_POINT('',#381055);
#39707=VERTEX_POINT('',#381057);
#39708=VERTEX_POINT('',#381067);
#39709=VERTEX_POINT('',#381068);
#39710=VERTEX_POINT('',#381070);
#39711=VERTEX_POINT('',#381075);
#39712=VERTEX_POINT('',#381077);
#39713=VERTEX_POINT('',#381149);
#39714=VERTEX_POINT('',#381181);
#39715=VERTEX_POINT('',#381212);
#39716=VERTEX_POINT('',#381351);
#39717=VERTEX_POINT('',#381352);
#39718=VERTEX_POINT('',#381354);
#39719=VERTEX_POINT('',#381359);
#39720=VERTEX_POINT('',#381361);
#39721=VERTEX_POINT('',#381371);
#39722=VERTEX_POINT('',#381372);
#39723=VERTEX_POINT('',#381374);
#39724=VERTEX_POINT('',#381379);
#39725=VERTEX_POINT('',#381381);
#39726=VERTEX_POINT('',#381453);
#39727=VERTEX_POINT('',#381485);
#39728=VERTEX_POINT('',#381516);
#39729=VERTEX_POINT('',#381655);
#39730=VERTEX_POINT('',#381656);
#39731=VERTEX_POINT('',#381658);
#39732=VERTEX_POINT('',#381663);
#39733=VERTEX_POINT('',#381665);
#39734=VERTEX_POINT('',#381675);
#39735=VERTEX_POINT('',#381676);
#39736=VERTEX_POINT('',#381678);
#39737=VERTEX_POINT('',#381683);
#39738=VERTEX_POINT('',#381685);
#39739=VERTEX_POINT('',#381757);
#39740=VERTEX_POINT('',#381789);
#39741=VERTEX_POINT('',#381820);
#39742=VERTEX_POINT('',#381959);
#39743=VERTEX_POINT('',#381960);
#39744=VERTEX_POINT('',#381962);
#39745=VERTEX_POINT('',#381967);
#39746=VERTEX_POINT('',#381969);
#39747=VERTEX_POINT('',#381979);
#39748=VERTEX_POINT('',#381980);
#39749=VERTEX_POINT('',#381982);
#39750=VERTEX_POINT('',#381987);
#39751=VERTEX_POINT('',#381989);
#39752=VERTEX_POINT('',#382061);
#39753=VERTEX_POINT('',#382093);
#39754=VERTEX_POINT('',#382124);
#39755=VERTEX_POINT('',#382263);
#39756=VERTEX_POINT('',#382264);
#39757=VERTEX_POINT('',#382266);
#39758=VERTEX_POINT('',#382271);
#39759=VERTEX_POINT('',#382273);
#39760=VERTEX_POINT('',#382283);
#39761=VERTEX_POINT('',#382284);
#39762=VERTEX_POINT('',#382286);
#39763=VERTEX_POINT('',#382291);
#39764=VERTEX_POINT('',#382293);
#39765=VERTEX_POINT('',#382365);
#39766=VERTEX_POINT('',#382397);
#39767=VERTEX_POINT('',#382428);
#39768=VERTEX_POINT('',#382567);
#39769=VERTEX_POINT('',#382568);
#39770=VERTEX_POINT('',#382570);
#39771=VERTEX_POINT('',#382575);
#39772=VERTEX_POINT('',#382577);
#39773=VERTEX_POINT('',#382587);
#39774=VERTEX_POINT('',#382588);
#39775=VERTEX_POINT('',#382590);
#39776=VERTEX_POINT('',#382595);
#39777=VERTEX_POINT('',#382597);
#39778=VERTEX_POINT('',#382669);
#39779=VERTEX_POINT('',#382701);
#39780=VERTEX_POINT('',#382732);
#39781=VERTEX_POINT('',#382871);
#39782=VERTEX_POINT('',#382872);
#39783=VERTEX_POINT('',#382874);
#39784=VERTEX_POINT('',#382879);
#39785=VERTEX_POINT('',#382881);
#39786=VERTEX_POINT('',#382891);
#39787=VERTEX_POINT('',#382892);
#39788=VERTEX_POINT('',#382894);
#39789=VERTEX_POINT('',#382899);
#39790=VERTEX_POINT('',#382901);
#39791=VERTEX_POINT('',#382973);
#39792=VERTEX_POINT('',#383005);
#39793=VERTEX_POINT('',#383036);
#39794=VERTEX_POINT('',#383175);
#39795=VERTEX_POINT('',#383176);
#39796=VERTEX_POINT('',#383178);
#39797=VERTEX_POINT('',#383183);
#39798=VERTEX_POINT('',#383185);
#39799=VERTEX_POINT('',#383195);
#39800=VERTEX_POINT('',#383196);
#39801=VERTEX_POINT('',#383198);
#39802=VERTEX_POINT('',#383203);
#39803=VERTEX_POINT('',#383205);
#39804=VERTEX_POINT('',#383277);
#39805=VERTEX_POINT('',#383309);
#39806=VERTEX_POINT('',#383340);
#39807=VERTEX_POINT('',#383479);
#39808=VERTEX_POINT('',#383480);
#39809=VERTEX_POINT('',#383482);
#39810=VERTEX_POINT('',#383487);
#39811=VERTEX_POINT('',#383489);
#39812=VERTEX_POINT('',#383499);
#39813=VERTEX_POINT('',#383500);
#39814=VERTEX_POINT('',#383502);
#39815=VERTEX_POINT('',#383507);
#39816=VERTEX_POINT('',#383509);
#39817=VERTEX_POINT('',#383581);
#39818=VERTEX_POINT('',#383613);
#39819=VERTEX_POINT('',#383644);
#39820=VERTEX_POINT('',#383783);
#39821=VERTEX_POINT('',#383784);
#39822=VERTEX_POINT('',#383786);
#39823=VERTEX_POINT('',#383791);
#39824=VERTEX_POINT('',#383793);
#39825=VERTEX_POINT('',#383803);
#39826=VERTEX_POINT('',#383804);
#39827=VERTEX_POINT('',#383806);
#39828=VERTEX_POINT('',#383811);
#39829=VERTEX_POINT('',#383813);
#39830=VERTEX_POINT('',#383885);
#39831=VERTEX_POINT('',#383917);
#39832=VERTEX_POINT('',#383948);
#39833=VERTEX_POINT('',#384087);
#39834=VERTEX_POINT('',#384088);
#39835=VERTEX_POINT('',#384090);
#39836=VERTEX_POINT('',#384095);
#39837=VERTEX_POINT('',#384097);
#39838=VERTEX_POINT('',#384107);
#39839=VERTEX_POINT('',#384108);
#39840=VERTEX_POINT('',#384110);
#39841=VERTEX_POINT('',#384115);
#39842=VERTEX_POINT('',#384117);
#39843=VERTEX_POINT('',#384189);
#39844=VERTEX_POINT('',#384221);
#39845=VERTEX_POINT('',#384252);
#39846=VERTEX_POINT('',#384391);
#39847=VERTEX_POINT('',#384392);
#39848=VERTEX_POINT('',#384394);
#39849=VERTEX_POINT('',#384399);
#39850=VERTEX_POINT('',#384401);
#39851=VERTEX_POINT('',#384411);
#39852=VERTEX_POINT('',#384412);
#39853=VERTEX_POINT('',#384414);
#39854=VERTEX_POINT('',#384419);
#39855=VERTEX_POINT('',#384421);
#39856=VERTEX_POINT('',#384493);
#39857=VERTEX_POINT('',#384525);
#39858=VERTEX_POINT('',#384556);
#39859=VERTEX_POINT('',#384695);
#39860=VERTEX_POINT('',#384696);
#39861=VERTEX_POINT('',#384698);
#39862=VERTEX_POINT('',#384703);
#39863=VERTEX_POINT('',#384705);
#39864=VERTEX_POINT('',#384715);
#39865=VERTEX_POINT('',#384716);
#39866=VERTEX_POINT('',#384718);
#39867=VERTEX_POINT('',#384723);
#39868=VERTEX_POINT('',#384725);
#39869=VERTEX_POINT('',#384797);
#39870=VERTEX_POINT('',#384829);
#39871=VERTEX_POINT('',#384860);
#39872=VERTEX_POINT('',#384999);
#39873=VERTEX_POINT('',#385000);
#39874=VERTEX_POINT('',#385002);
#39875=VERTEX_POINT('',#385007);
#39876=VERTEX_POINT('',#385009);
#39877=VERTEX_POINT('',#385019);
#39878=VERTEX_POINT('',#385020);
#39879=VERTEX_POINT('',#385022);
#39880=VERTEX_POINT('',#385027);
#39881=VERTEX_POINT('',#385029);
#39882=VERTEX_POINT('',#385101);
#39883=VERTEX_POINT('',#385133);
#39884=VERTEX_POINT('',#385164);
#39885=VERTEX_POINT('',#385303);
#39886=VERTEX_POINT('',#385304);
#39887=VERTEX_POINT('',#385306);
#39888=VERTEX_POINT('',#385311);
#39889=VERTEX_POINT('',#385313);
#39890=VERTEX_POINT('',#385323);
#39891=VERTEX_POINT('',#385324);
#39892=VERTEX_POINT('',#385326);
#39893=VERTEX_POINT('',#385331);
#39894=VERTEX_POINT('',#385333);
#39895=VERTEX_POINT('',#385405);
#39896=VERTEX_POINT('',#385437);
#39897=VERTEX_POINT('',#385468);
#39898=VERTEX_POINT('',#385607);
#39899=VERTEX_POINT('',#385608);
#39900=VERTEX_POINT('',#385610);
#39901=VERTEX_POINT('',#385615);
#39902=VERTEX_POINT('',#385617);
#39903=VERTEX_POINT('',#385627);
#39904=VERTEX_POINT('',#385628);
#39905=VERTEX_POINT('',#385630);
#39906=VERTEX_POINT('',#385635);
#39907=VERTEX_POINT('',#385637);
#39908=VERTEX_POINT('',#385709);
#39909=VERTEX_POINT('',#385741);
#39910=VERTEX_POINT('',#385772);
#39911=VERTEX_POINT('',#385911);
#39912=VERTEX_POINT('',#385912);
#39913=VERTEX_POINT('',#385914);
#39914=VERTEX_POINT('',#385919);
#39915=VERTEX_POINT('',#385921);
#39916=VERTEX_POINT('',#385931);
#39917=VERTEX_POINT('',#385932);
#39918=VERTEX_POINT('',#385934);
#39919=VERTEX_POINT('',#385939);
#39920=VERTEX_POINT('',#385941);
#39921=VERTEX_POINT('',#386013);
#39922=VERTEX_POINT('',#386045);
#39923=VERTEX_POINT('',#386076);
#39924=VERTEX_POINT('',#386215);
#39925=VERTEX_POINT('',#386216);
#39926=VERTEX_POINT('',#386218);
#39927=VERTEX_POINT('',#386223);
#39928=VERTEX_POINT('',#386225);
#39929=VERTEX_POINT('',#386235);
#39930=VERTEX_POINT('',#386236);
#39931=VERTEX_POINT('',#386238);
#39932=VERTEX_POINT('',#386243);
#39933=VERTEX_POINT('',#386245);
#39934=VERTEX_POINT('',#386317);
#39935=VERTEX_POINT('',#386349);
#39936=VERTEX_POINT('',#386380);
#39937=VERTEX_POINT('',#386519);
#39938=VERTEX_POINT('',#386520);
#39939=VERTEX_POINT('',#386522);
#39940=VERTEX_POINT('',#386527);
#39941=VERTEX_POINT('',#386529);
#39942=VERTEX_POINT('',#386539);
#39943=VERTEX_POINT('',#386540);
#39944=VERTEX_POINT('',#386542);
#39945=VERTEX_POINT('',#386547);
#39946=VERTEX_POINT('',#386549);
#39947=VERTEX_POINT('',#386621);
#39948=VERTEX_POINT('',#386653);
#39949=VERTEX_POINT('',#386684);
#39950=VERTEX_POINT('',#386823);
#39951=VERTEX_POINT('',#386824);
#39952=VERTEX_POINT('',#386826);
#39953=VERTEX_POINT('',#386831);
#39954=VERTEX_POINT('',#386833);
#39955=VERTEX_POINT('',#386843);
#39956=VERTEX_POINT('',#386844);
#39957=VERTEX_POINT('',#386846);
#39958=VERTEX_POINT('',#386851);
#39959=VERTEX_POINT('',#386853);
#39960=VERTEX_POINT('',#386925);
#39961=VERTEX_POINT('',#386957);
#39962=VERTEX_POINT('',#386988);
#39963=VERTEX_POINT('',#387127);
#39964=VERTEX_POINT('',#387128);
#39965=VERTEX_POINT('',#387130);
#39966=VERTEX_POINT('',#387135);
#39967=VERTEX_POINT('',#387137);
#39968=VERTEX_POINT('',#387147);
#39969=VERTEX_POINT('',#387148);
#39970=VERTEX_POINT('',#387150);
#39971=VERTEX_POINT('',#387155);
#39972=VERTEX_POINT('',#387157);
#39973=VERTEX_POINT('',#387229);
#39974=VERTEX_POINT('',#387261);
#39975=VERTEX_POINT('',#387292);
#39976=VERTEX_POINT('',#387431);
#39977=VERTEX_POINT('',#387432);
#39978=VERTEX_POINT('',#387434);
#39979=VERTEX_POINT('',#387439);
#39980=VERTEX_POINT('',#387441);
#39981=VERTEX_POINT('',#387451);
#39982=VERTEX_POINT('',#387452);
#39983=VERTEX_POINT('',#387454);
#39984=VERTEX_POINT('',#387459);
#39985=VERTEX_POINT('',#387461);
#39986=VERTEX_POINT('',#387533);
#39987=VERTEX_POINT('',#387565);
#39988=VERTEX_POINT('',#387596);
#39989=VERTEX_POINT('',#387735);
#39990=VERTEX_POINT('',#387736);
#39991=VERTEX_POINT('',#387738);
#39992=VERTEX_POINT('',#387743);
#39993=VERTEX_POINT('',#387745);
#39994=VERTEX_POINT('',#387755);
#39995=VERTEX_POINT('',#387756);
#39996=VERTEX_POINT('',#387758);
#39997=VERTEX_POINT('',#387763);
#39998=VERTEX_POINT('',#387765);
#39999=VERTEX_POINT('',#387837);
#40000=VERTEX_POINT('',#387869);
#40001=VERTEX_POINT('',#387900);
#40002=VERTEX_POINT('',#388039);
#40003=VERTEX_POINT('',#388040);
#40004=VERTEX_POINT('',#388042);
#40005=VERTEX_POINT('',#388047);
#40006=VERTEX_POINT('',#388049);
#40007=VERTEX_POINT('',#388059);
#40008=VERTEX_POINT('',#388060);
#40009=VERTEX_POINT('',#388062);
#40010=VERTEX_POINT('',#388067);
#40011=VERTEX_POINT('',#388069);
#40012=VERTEX_POINT('',#388141);
#40013=VERTEX_POINT('',#388173);
#40014=VERTEX_POINT('',#388204);
#40015=VERTEX_POINT('',#388343);
#40016=VERTEX_POINT('',#388344);
#40017=VERTEX_POINT('',#388346);
#40018=VERTEX_POINT('',#388351);
#40019=VERTEX_POINT('',#388353);
#40020=VERTEX_POINT('',#388363);
#40021=VERTEX_POINT('',#388364);
#40022=VERTEX_POINT('',#388366);
#40023=VERTEX_POINT('',#388371);
#40024=VERTEX_POINT('',#388373);
#40025=VERTEX_POINT('',#388445);
#40026=VERTEX_POINT('',#388477);
#40027=VERTEX_POINT('',#388508);
#40028=VERTEX_POINT('',#388647);
#40029=VERTEX_POINT('',#388648);
#40030=VERTEX_POINT('',#388650);
#40031=VERTEX_POINT('',#388655);
#40032=VERTEX_POINT('',#388657);
#40033=VERTEX_POINT('',#388667);
#40034=VERTEX_POINT('',#388668);
#40035=VERTEX_POINT('',#388670);
#40036=VERTEX_POINT('',#388675);
#40037=VERTEX_POINT('',#388677);
#40038=VERTEX_POINT('',#388749);
#40039=VERTEX_POINT('',#388781);
#40040=VERTEX_POINT('',#388812);
#40041=VERTEX_POINT('',#388951);
#40042=VERTEX_POINT('',#388952);
#40043=VERTEX_POINT('',#388954);
#40044=VERTEX_POINT('',#388959);
#40045=VERTEX_POINT('',#388961);
#40046=VERTEX_POINT('',#388971);
#40047=VERTEX_POINT('',#388972);
#40048=VERTEX_POINT('',#388974);
#40049=VERTEX_POINT('',#388979);
#40050=VERTEX_POINT('',#388981);
#40051=VERTEX_POINT('',#389053);
#40052=VERTEX_POINT('',#389085);
#40053=VERTEX_POINT('',#389116);
#40054=VERTEX_POINT('',#389255);
#40055=VERTEX_POINT('',#389256);
#40056=VERTEX_POINT('',#389258);
#40057=VERTEX_POINT('',#389263);
#40058=VERTEX_POINT('',#389265);
#40059=VERTEX_POINT('',#389275);
#40060=VERTEX_POINT('',#389276);
#40061=VERTEX_POINT('',#389278);
#40062=VERTEX_POINT('',#389283);
#40063=VERTEX_POINT('',#389285);
#40064=VERTEX_POINT('',#389357);
#40065=VERTEX_POINT('',#389389);
#40066=VERTEX_POINT('',#389420);
#40067=VERTEX_POINT('',#389559);
#40068=VERTEX_POINT('',#389560);
#40069=VERTEX_POINT('',#389562);
#40070=VERTEX_POINT('',#389567);
#40071=VERTEX_POINT('',#389569);
#40072=VERTEX_POINT('',#389579);
#40073=VERTEX_POINT('',#389580);
#40074=VERTEX_POINT('',#389582);
#40075=VERTEX_POINT('',#389587);
#40076=VERTEX_POINT('',#389589);
#40077=VERTEX_POINT('',#389661);
#40078=VERTEX_POINT('',#389693);
#40079=VERTEX_POINT('',#389724);
#40080=VERTEX_POINT('',#389863);
#40081=VERTEX_POINT('',#389864);
#40082=VERTEX_POINT('',#389866);
#40083=VERTEX_POINT('',#389871);
#40084=VERTEX_POINT('',#389873);
#40085=VERTEX_POINT('',#389883);
#40086=VERTEX_POINT('',#389884);
#40087=VERTEX_POINT('',#389886);
#40088=VERTEX_POINT('',#389891);
#40089=VERTEX_POINT('',#389893);
#40090=VERTEX_POINT('',#389965);
#40091=VERTEX_POINT('',#389997);
#40092=VERTEX_POINT('',#390028);
#40093=VERTEX_POINT('',#390167);
#40094=VERTEX_POINT('',#390168);
#40095=VERTEX_POINT('',#390170);
#40096=VERTEX_POINT('',#390175);
#40097=VERTEX_POINT('',#390177);
#40098=VERTEX_POINT('',#390187);
#40099=VERTEX_POINT('',#390188);
#40100=VERTEX_POINT('',#390190);
#40101=VERTEX_POINT('',#390195);
#40102=VERTEX_POINT('',#390197);
#40103=VERTEX_POINT('',#390269);
#40104=VERTEX_POINT('',#390301);
#40105=VERTEX_POINT('',#390332);
#40106=VERTEX_POINT('',#390471);
#40107=VERTEX_POINT('',#390472);
#40108=VERTEX_POINT('',#390474);
#40109=VERTEX_POINT('',#390479);
#40110=VERTEX_POINT('',#390481);
#40111=VERTEX_POINT('',#390491);
#40112=VERTEX_POINT('',#390492);
#40113=VERTEX_POINT('',#390494);
#40114=VERTEX_POINT('',#390499);
#40115=VERTEX_POINT('',#390501);
#40116=VERTEX_POINT('',#390573);
#40117=VERTEX_POINT('',#390605);
#40118=VERTEX_POINT('',#390636);
#40119=VERTEX_POINT('',#390775);
#40120=VERTEX_POINT('',#390776);
#40121=VERTEX_POINT('',#390778);
#40122=VERTEX_POINT('',#390783);
#40123=VERTEX_POINT('',#390785);
#40124=VERTEX_POINT('',#390795);
#40125=VERTEX_POINT('',#390796);
#40126=VERTEX_POINT('',#390798);
#40127=VERTEX_POINT('',#390803);
#40128=VERTEX_POINT('',#390805);
#40129=VERTEX_POINT('',#390877);
#40130=VERTEX_POINT('',#390909);
#40131=VERTEX_POINT('',#390940);
#40132=VERTEX_POINT('',#391079);
#40133=VERTEX_POINT('',#391080);
#40134=VERTEX_POINT('',#391082);
#40135=VERTEX_POINT('',#391087);
#40136=VERTEX_POINT('',#391089);
#40137=VERTEX_POINT('',#391099);
#40138=VERTEX_POINT('',#391100);
#40139=VERTEX_POINT('',#391102);
#40140=VERTEX_POINT('',#391107);
#40141=VERTEX_POINT('',#391109);
#40142=VERTEX_POINT('',#391181);
#40143=VERTEX_POINT('',#391213);
#40144=VERTEX_POINT('',#391244);
#40145=VERTEX_POINT('',#391383);
#40146=VERTEX_POINT('',#391384);
#40147=VERTEX_POINT('',#391386);
#40148=VERTEX_POINT('',#391391);
#40149=VERTEX_POINT('',#391393);
#40150=VERTEX_POINT('',#391403);
#40151=VERTEX_POINT('',#391404);
#40152=VERTEX_POINT('',#391406);
#40153=VERTEX_POINT('',#391411);
#40154=VERTEX_POINT('',#391413);
#40155=VERTEX_POINT('',#391485);
#40156=VERTEX_POINT('',#391517);
#40157=VERTEX_POINT('',#391548);
#40158=VERTEX_POINT('',#391687);
#40159=VERTEX_POINT('',#391688);
#40160=VERTEX_POINT('',#391690);
#40161=VERTEX_POINT('',#391695);
#40162=VERTEX_POINT('',#391697);
#40163=VERTEX_POINT('',#391707);
#40164=VERTEX_POINT('',#391708);
#40165=VERTEX_POINT('',#391710);
#40166=VERTEX_POINT('',#391715);
#40167=VERTEX_POINT('',#391717);
#40168=VERTEX_POINT('',#391789);
#40169=VERTEX_POINT('',#391821);
#40170=VERTEX_POINT('',#391852);
#40171=VERTEX_POINT('',#391991);
#40172=VERTEX_POINT('',#391992);
#40173=VERTEX_POINT('',#391994);
#40174=VERTEX_POINT('',#391999);
#40175=VERTEX_POINT('',#392001);
#40176=VERTEX_POINT('',#392011);
#40177=VERTEX_POINT('',#392012);
#40178=VERTEX_POINT('',#392014);
#40179=VERTEX_POINT('',#392019);
#40180=VERTEX_POINT('',#392021);
#40181=VERTEX_POINT('',#392093);
#40182=VERTEX_POINT('',#392125);
#40183=VERTEX_POINT('',#392156);
#40184=VERTEX_POINT('',#392295);
#40185=VERTEX_POINT('',#392296);
#40186=VERTEX_POINT('',#392298);
#40187=VERTEX_POINT('',#392303);
#40188=VERTEX_POINT('',#392305);
#40189=VERTEX_POINT('',#392315);
#40190=VERTEX_POINT('',#392316);
#40191=VERTEX_POINT('',#392318);
#40192=VERTEX_POINT('',#392323);
#40193=VERTEX_POINT('',#392325);
#40194=VERTEX_POINT('',#392397);
#40195=VERTEX_POINT('',#392429);
#40196=VERTEX_POINT('',#392460);
#40197=VERTEX_POINT('',#392599);
#40198=VERTEX_POINT('',#392600);
#40199=VERTEX_POINT('',#392602);
#40200=VERTEX_POINT('',#392607);
#40201=VERTEX_POINT('',#392609);
#40202=VERTEX_POINT('',#392619);
#40203=VERTEX_POINT('',#392620);
#40204=VERTEX_POINT('',#392622);
#40205=VERTEX_POINT('',#392627);
#40206=VERTEX_POINT('',#392629);
#40207=VERTEX_POINT('',#392701);
#40208=VERTEX_POINT('',#392733);
#40209=VERTEX_POINT('',#392764);
#40210=VERTEX_POINT('',#392903);
#40211=VERTEX_POINT('',#392904);
#40212=VERTEX_POINT('',#392906);
#40213=VERTEX_POINT('',#392911);
#40214=VERTEX_POINT('',#392913);
#40215=VERTEX_POINT('',#392923);
#40216=VERTEX_POINT('',#392924);
#40217=VERTEX_POINT('',#392926);
#40218=VERTEX_POINT('',#392931);
#40219=VERTEX_POINT('',#392933);
#40220=VERTEX_POINT('',#393005);
#40221=VERTEX_POINT('',#393037);
#40222=VERTEX_POINT('',#393068);
#40223=VERTEX_POINT('',#393207);
#40224=VERTEX_POINT('',#393208);
#40225=VERTEX_POINT('',#393210);
#40226=VERTEX_POINT('',#393215);
#40227=VERTEX_POINT('',#393217);
#40228=VERTEX_POINT('',#393227);
#40229=VERTEX_POINT('',#393228);
#40230=VERTEX_POINT('',#393230);
#40231=VERTEX_POINT('',#393235);
#40232=VERTEX_POINT('',#393237);
#40233=VERTEX_POINT('',#393309);
#40234=VERTEX_POINT('',#393341);
#40235=VERTEX_POINT('',#393372);
#40236=VERTEX_POINT('',#393511);
#40237=VERTEX_POINT('',#393512);
#40238=VERTEX_POINT('',#393514);
#40239=VERTEX_POINT('',#393519);
#40240=VERTEX_POINT('',#393521);
#40241=VERTEX_POINT('',#393531);
#40242=VERTEX_POINT('',#393532);
#40243=VERTEX_POINT('',#393534);
#40244=VERTEX_POINT('',#393539);
#40245=VERTEX_POINT('',#393541);
#40246=VERTEX_POINT('',#393613);
#40247=VERTEX_POINT('',#393645);
#40248=VERTEX_POINT('',#393676);
#40249=VERTEX_POINT('',#393815);
#40250=VERTEX_POINT('',#393816);
#40251=VERTEX_POINT('',#393818);
#40252=VERTEX_POINT('',#393823);
#40253=VERTEX_POINT('',#393825);
#40254=VERTEX_POINT('',#393835);
#40255=VERTEX_POINT('',#393836);
#40256=VERTEX_POINT('',#393838);
#40257=VERTEX_POINT('',#393843);
#40258=VERTEX_POINT('',#393845);
#40259=VERTEX_POINT('',#393917);
#40260=VERTEX_POINT('',#393949);
#40261=VERTEX_POINT('',#393980);
#40262=VERTEX_POINT('',#394119);
#40263=VERTEX_POINT('',#394120);
#40264=VERTEX_POINT('',#394122);
#40265=VERTEX_POINT('',#394127);
#40266=VERTEX_POINT('',#394129);
#40267=VERTEX_POINT('',#394139);
#40268=VERTEX_POINT('',#394140);
#40269=VERTEX_POINT('',#394142);
#40270=VERTEX_POINT('',#394147);
#40271=VERTEX_POINT('',#394149);
#40272=VERTEX_POINT('',#394221);
#40273=VERTEX_POINT('',#394253);
#40274=VERTEX_POINT('',#394284);
#40275=VERTEX_POINT('',#394423);
#40276=VERTEX_POINT('',#394424);
#40277=VERTEX_POINT('',#394426);
#40278=VERTEX_POINT('',#394431);
#40279=VERTEX_POINT('',#394433);
#40280=VERTEX_POINT('',#394443);
#40281=VERTEX_POINT('',#394444);
#40282=VERTEX_POINT('',#394446);
#40283=VERTEX_POINT('',#394451);
#40284=VERTEX_POINT('',#394453);
#40285=VERTEX_POINT('',#394525);
#40286=VERTEX_POINT('',#394557);
#40287=VERTEX_POINT('',#394588);
#40288=VERTEX_POINT('',#394727);
#40289=VERTEX_POINT('',#394728);
#40290=VERTEX_POINT('',#394730);
#40291=VERTEX_POINT('',#394735);
#40292=VERTEX_POINT('',#394737);
#40293=VERTEX_POINT('',#394747);
#40294=VERTEX_POINT('',#394748);
#40295=VERTEX_POINT('',#394750);
#40296=VERTEX_POINT('',#394755);
#40297=VERTEX_POINT('',#394757);
#40298=VERTEX_POINT('',#394829);
#40299=VERTEX_POINT('',#394861);
#40300=VERTEX_POINT('',#394892);
#40301=VERTEX_POINT('',#395031);
#40302=VERTEX_POINT('',#395032);
#40303=VERTEX_POINT('',#395034);
#40304=VERTEX_POINT('',#395039);
#40305=VERTEX_POINT('',#395041);
#40306=VERTEX_POINT('',#395051);
#40307=VERTEX_POINT('',#395052);
#40308=VERTEX_POINT('',#395054);
#40309=VERTEX_POINT('',#395059);
#40310=VERTEX_POINT('',#395061);
#40311=VERTEX_POINT('',#395133);
#40312=VERTEX_POINT('',#395165);
#40313=VERTEX_POINT('',#395196);
#40314=VERTEX_POINT('',#395335);
#40315=VERTEX_POINT('',#395336);
#40316=VERTEX_POINT('',#395338);
#40317=VERTEX_POINT('',#395343);
#40318=VERTEX_POINT('',#395345);
#40319=VERTEX_POINT('',#395355);
#40320=VERTEX_POINT('',#395356);
#40321=VERTEX_POINT('',#395358);
#40322=VERTEX_POINT('',#395363);
#40323=VERTEX_POINT('',#395365);
#40324=VERTEX_POINT('',#395437);
#40325=VERTEX_POINT('',#395469);
#40326=VERTEX_POINT('',#395500);
#40327=VERTEX_POINT('',#395639);
#40328=VERTEX_POINT('',#395640);
#40329=VERTEX_POINT('',#395642);
#40330=VERTEX_POINT('',#395647);
#40331=VERTEX_POINT('',#395649);
#40332=VERTEX_POINT('',#395659);
#40333=VERTEX_POINT('',#395660);
#40334=VERTEX_POINT('',#395662);
#40335=VERTEX_POINT('',#395667);
#40336=VERTEX_POINT('',#395669);
#40337=VERTEX_POINT('',#395741);
#40338=VERTEX_POINT('',#395773);
#40339=VERTEX_POINT('',#395804);
#40340=VERTEX_POINT('',#395943);
#40341=VERTEX_POINT('',#395944);
#40342=VERTEX_POINT('',#395946);
#40343=VERTEX_POINT('',#395951);
#40344=VERTEX_POINT('',#395953);
#40345=VERTEX_POINT('',#395963);
#40346=VERTEX_POINT('',#395964);
#40347=VERTEX_POINT('',#395966);
#40348=VERTEX_POINT('',#395971);
#40349=VERTEX_POINT('',#395973);
#40350=VERTEX_POINT('',#396045);
#40351=VERTEX_POINT('',#396077);
#40352=VERTEX_POINT('',#396108);
#40353=VERTEX_POINT('',#396247);
#40354=VERTEX_POINT('',#396248);
#40355=VERTEX_POINT('',#396250);
#40356=VERTEX_POINT('',#396255);
#40357=VERTEX_POINT('',#396257);
#40358=VERTEX_POINT('',#396267);
#40359=VERTEX_POINT('',#396268);
#40360=VERTEX_POINT('',#396270);
#40361=VERTEX_POINT('',#396275);
#40362=VERTEX_POINT('',#396277);
#40363=VERTEX_POINT('',#396349);
#40364=VERTEX_POINT('',#396381);
#40365=VERTEX_POINT('',#396412);
#40366=VERTEX_POINT('',#396551);
#40367=VERTEX_POINT('',#396552);
#40368=VERTEX_POINT('',#396554);
#40369=VERTEX_POINT('',#396559);
#40370=VERTEX_POINT('',#396561);
#40371=VERTEX_POINT('',#396571);
#40372=VERTEX_POINT('',#396572);
#40373=VERTEX_POINT('',#396574);
#40374=VERTEX_POINT('',#396579);
#40375=VERTEX_POINT('',#396581);
#40376=VERTEX_POINT('',#396653);
#40377=VERTEX_POINT('',#396685);
#40378=VERTEX_POINT('',#396716);
#40379=VERTEX_POINT('',#396855);
#40380=VERTEX_POINT('',#396856);
#40381=VERTEX_POINT('',#396858);
#40382=VERTEX_POINT('',#396863);
#40383=VERTEX_POINT('',#396865);
#40384=VERTEX_POINT('',#396875);
#40385=VERTEX_POINT('',#396876);
#40386=VERTEX_POINT('',#396878);
#40387=VERTEX_POINT('',#396883);
#40388=VERTEX_POINT('',#396885);
#40389=VERTEX_POINT('',#396957);
#40390=VERTEX_POINT('',#396989);
#40391=VERTEX_POINT('',#397020);
#40392=VERTEX_POINT('',#397159);
#40393=VERTEX_POINT('',#397160);
#40394=VERTEX_POINT('',#397162);
#40395=VERTEX_POINT('',#397167);
#40396=VERTEX_POINT('',#397169);
#40397=VERTEX_POINT('',#397179);
#40398=VERTEX_POINT('',#397180);
#40399=VERTEX_POINT('',#397182);
#40400=VERTEX_POINT('',#397187);
#40401=VERTEX_POINT('',#397189);
#40402=VERTEX_POINT('',#397261);
#40403=VERTEX_POINT('',#397293);
#40404=VERTEX_POINT('',#397324);
#40405=VERTEX_POINT('',#397463);
#40406=VERTEX_POINT('',#397464);
#40407=VERTEX_POINT('',#397466);
#40408=VERTEX_POINT('',#397471);
#40409=VERTEX_POINT('',#397473);
#40410=VERTEX_POINT('',#397483);
#40411=VERTEX_POINT('',#397484);
#40412=VERTEX_POINT('',#397486);
#40413=VERTEX_POINT('',#397491);
#40414=VERTEX_POINT('',#397493);
#40415=VERTEX_POINT('',#397565);
#40416=VERTEX_POINT('',#397597);
#40417=VERTEX_POINT('',#397628);
#40418=VERTEX_POINT('',#397767);
#40419=VERTEX_POINT('',#397768);
#40420=VERTEX_POINT('',#397770);
#40421=VERTEX_POINT('',#397775);
#40422=VERTEX_POINT('',#397777);
#40423=VERTEX_POINT('',#397787);
#40424=VERTEX_POINT('',#397788);
#40425=VERTEX_POINT('',#397790);
#40426=VERTEX_POINT('',#397795);
#40427=VERTEX_POINT('',#397797);
#40428=VERTEX_POINT('',#397869);
#40429=VERTEX_POINT('',#397901);
#40430=VERTEX_POINT('',#397932);
#40431=VERTEX_POINT('',#398071);
#40432=VERTEX_POINT('',#398072);
#40433=VERTEX_POINT('',#398074);
#40434=VERTEX_POINT('',#398079);
#40435=VERTEX_POINT('',#398081);
#40436=VERTEX_POINT('',#398091);
#40437=VERTEX_POINT('',#398092);
#40438=VERTEX_POINT('',#398094);
#40439=VERTEX_POINT('',#398099);
#40440=VERTEX_POINT('',#398101);
#40441=VERTEX_POINT('',#398173);
#40442=VERTEX_POINT('',#398205);
#40443=VERTEX_POINT('',#398236);
#40444=VERTEX_POINT('',#398375);
#40445=VERTEX_POINT('',#398376);
#40446=VERTEX_POINT('',#398378);
#40447=VERTEX_POINT('',#398383);
#40448=VERTEX_POINT('',#398385);
#40449=VERTEX_POINT('',#398395);
#40450=VERTEX_POINT('',#398396);
#40451=VERTEX_POINT('',#398398);
#40452=VERTEX_POINT('',#398403);
#40453=VERTEX_POINT('',#398405);
#40454=VERTEX_POINT('',#398477);
#40455=VERTEX_POINT('',#398509);
#40456=VERTEX_POINT('',#398540);
#40457=VERTEX_POINT('',#398679);
#40458=VERTEX_POINT('',#398680);
#40459=VERTEX_POINT('',#398682);
#40460=VERTEX_POINT('',#398687);
#40461=VERTEX_POINT('',#398689);
#40462=VERTEX_POINT('',#398699);
#40463=VERTEX_POINT('',#398700);
#40464=VERTEX_POINT('',#398702);
#40465=VERTEX_POINT('',#398707);
#40466=VERTEX_POINT('',#398709);
#40467=VERTEX_POINT('',#398781);
#40468=VERTEX_POINT('',#398813);
#40469=VERTEX_POINT('',#398844);
#40470=VERTEX_POINT('',#398983);
#40471=VERTEX_POINT('',#398984);
#40472=VERTEX_POINT('',#398986);
#40473=VERTEX_POINT('',#398991);
#40474=VERTEX_POINT('',#398993);
#40475=VERTEX_POINT('',#399003);
#40476=VERTEX_POINT('',#399004);
#40477=VERTEX_POINT('',#399006);
#40478=VERTEX_POINT('',#399011);
#40479=VERTEX_POINT('',#399013);
#40480=VERTEX_POINT('',#399085);
#40481=VERTEX_POINT('',#399117);
#40482=VERTEX_POINT('',#399148);
#40483=VERTEX_POINT('',#399287);
#40484=VERTEX_POINT('',#399288);
#40485=VERTEX_POINT('',#399290);
#40486=VERTEX_POINT('',#399295);
#40487=VERTEX_POINT('',#399297);
#40488=VERTEX_POINT('',#399307);
#40489=VERTEX_POINT('',#399308);
#40490=VERTEX_POINT('',#399310);
#40491=VERTEX_POINT('',#399315);
#40492=VERTEX_POINT('',#399317);
#40493=VERTEX_POINT('',#399389);
#40494=VERTEX_POINT('',#399421);
#40495=VERTEX_POINT('',#399452);
#40496=VERTEX_POINT('',#399591);
#40497=VERTEX_POINT('',#399592);
#40498=VERTEX_POINT('',#399594);
#40499=VERTEX_POINT('',#399599);
#40500=VERTEX_POINT('',#399601);
#40501=VERTEX_POINT('',#399611);
#40502=VERTEX_POINT('',#399612);
#40503=VERTEX_POINT('',#399614);
#40504=VERTEX_POINT('',#399619);
#40505=VERTEX_POINT('',#399621);
#40506=VERTEX_POINT('',#399693);
#40507=VERTEX_POINT('',#399725);
#40508=VERTEX_POINT('',#399756);
#40509=VERTEX_POINT('',#399895);
#40510=VERTEX_POINT('',#399896);
#40511=VERTEX_POINT('',#399898);
#40512=VERTEX_POINT('',#399903);
#40513=VERTEX_POINT('',#399905);
#40514=VERTEX_POINT('',#399915);
#40515=VERTEX_POINT('',#399916);
#40516=VERTEX_POINT('',#399918);
#40517=VERTEX_POINT('',#399923);
#40518=VERTEX_POINT('',#399925);
#40519=VERTEX_POINT('',#399997);
#40520=VERTEX_POINT('',#400029);
#40521=VERTEX_POINT('',#400060);
#40522=VERTEX_POINT('',#400199);
#40523=VERTEX_POINT('',#400200);
#40524=VERTEX_POINT('',#400202);
#40525=VERTEX_POINT('',#400207);
#40526=VERTEX_POINT('',#400209);
#40527=VERTEX_POINT('',#400219);
#40528=VERTEX_POINT('',#400220);
#40529=VERTEX_POINT('',#400222);
#40530=VERTEX_POINT('',#400227);
#40531=VERTEX_POINT('',#400229);
#40532=VERTEX_POINT('',#400301);
#40533=VERTEX_POINT('',#400333);
#40534=VERTEX_POINT('',#400364);
#40535=VERTEX_POINT('',#400503);
#40536=VERTEX_POINT('',#400504);
#40537=VERTEX_POINT('',#400506);
#40538=VERTEX_POINT('',#400511);
#40539=VERTEX_POINT('',#400513);
#40540=VERTEX_POINT('',#400523);
#40541=VERTEX_POINT('',#400524);
#40542=VERTEX_POINT('',#400526);
#40543=VERTEX_POINT('',#400531);
#40544=VERTEX_POINT('',#400533);
#40545=VERTEX_POINT('',#400605);
#40546=VERTEX_POINT('',#400637);
#40547=VERTEX_POINT('',#400668);
#40548=VERTEX_POINT('',#400807);
#40549=VERTEX_POINT('',#400808);
#40550=VERTEX_POINT('',#400810);
#40551=VERTEX_POINT('',#400815);
#40552=VERTEX_POINT('',#400817);
#40553=VERTEX_POINT('',#400827);
#40554=VERTEX_POINT('',#400828);
#40555=VERTEX_POINT('',#400830);
#40556=VERTEX_POINT('',#400835);
#40557=VERTEX_POINT('',#400837);
#40558=VERTEX_POINT('',#400909);
#40559=VERTEX_POINT('',#400941);
#40560=VERTEX_POINT('',#400972);
#40561=VERTEX_POINT('',#401111);
#40562=VERTEX_POINT('',#401112);
#40563=VERTEX_POINT('',#401114);
#40564=VERTEX_POINT('',#401119);
#40565=VERTEX_POINT('',#401121);
#40566=VERTEX_POINT('',#401131);
#40567=VERTEX_POINT('',#401132);
#40568=VERTEX_POINT('',#401134);
#40569=VERTEX_POINT('',#401139);
#40570=VERTEX_POINT('',#401141);
#40571=VERTEX_POINT('',#401213);
#40572=VERTEX_POINT('',#401245);
#40573=VERTEX_POINT('',#401276);
#40574=VERTEX_POINT('',#401415);
#40575=VERTEX_POINT('',#401416);
#40576=VERTEX_POINT('',#401418);
#40577=VERTEX_POINT('',#401423);
#40578=VERTEX_POINT('',#401425);
#40579=VERTEX_POINT('',#401435);
#40580=VERTEX_POINT('',#401436);
#40581=VERTEX_POINT('',#401438);
#40582=VERTEX_POINT('',#401443);
#40583=VERTEX_POINT('',#401445);
#40584=VERTEX_POINT('',#401517);
#40585=VERTEX_POINT('',#401549);
#40586=VERTEX_POINT('',#401580);
#40587=VERTEX_POINT('',#401719);
#40588=VERTEX_POINT('',#401720);
#40589=VERTEX_POINT('',#401722);
#40590=VERTEX_POINT('',#401727);
#40591=VERTEX_POINT('',#401729);
#40592=VERTEX_POINT('',#401739);
#40593=VERTEX_POINT('',#401740);
#40594=VERTEX_POINT('',#401742);
#40595=VERTEX_POINT('',#401747);
#40596=VERTEX_POINT('',#401749);
#40597=VERTEX_POINT('',#401821);
#40598=VERTEX_POINT('',#401853);
#40599=VERTEX_POINT('',#401884);
#40600=VERTEX_POINT('',#402023);
#40601=VERTEX_POINT('',#402024);
#40602=VERTEX_POINT('',#402026);
#40603=VERTEX_POINT('',#402031);
#40604=VERTEX_POINT('',#402033);
#40605=VERTEX_POINT('',#402043);
#40606=VERTEX_POINT('',#402044);
#40607=VERTEX_POINT('',#402046);
#40608=VERTEX_POINT('',#402051);
#40609=VERTEX_POINT('',#402053);
#40610=VERTEX_POINT('',#402125);
#40611=VERTEX_POINT('',#402157);
#40612=VERTEX_POINT('',#402188);
#40613=VERTEX_POINT('',#402327);
#40614=VERTEX_POINT('',#402328);
#40615=VERTEX_POINT('',#402330);
#40616=VERTEX_POINT('',#402335);
#40617=VERTEX_POINT('',#402337);
#40618=VERTEX_POINT('',#402347);
#40619=VERTEX_POINT('',#402348);
#40620=VERTEX_POINT('',#402350);
#40621=VERTEX_POINT('',#402355);
#40622=VERTEX_POINT('',#402357);
#40623=VERTEX_POINT('',#402429);
#40624=VERTEX_POINT('',#402461);
#40625=VERTEX_POINT('',#402492);
#40626=VERTEX_POINT('',#402631);
#40627=VERTEX_POINT('',#402632);
#40628=VERTEX_POINT('',#402634);
#40629=VERTEX_POINT('',#402639);
#40630=VERTEX_POINT('',#402641);
#40631=VERTEX_POINT('',#402651);
#40632=VERTEX_POINT('',#402652);
#40633=VERTEX_POINT('',#402654);
#40634=VERTEX_POINT('',#402659);
#40635=VERTEX_POINT('',#402661);
#40636=VERTEX_POINT('',#402733);
#40637=VERTEX_POINT('',#402765);
#40638=VERTEX_POINT('',#402796);
#40639=VERTEX_POINT('',#402935);
#40640=VERTEX_POINT('',#402936);
#40641=VERTEX_POINT('',#402938);
#40642=VERTEX_POINT('',#402943);
#40643=VERTEX_POINT('',#402945);
#40644=VERTEX_POINT('',#402955);
#40645=VERTEX_POINT('',#402956);
#40646=VERTEX_POINT('',#402958);
#40647=VERTEX_POINT('',#402963);
#40648=VERTEX_POINT('',#402965);
#40649=VERTEX_POINT('',#403037);
#40650=VERTEX_POINT('',#403069);
#40651=VERTEX_POINT('',#403100);
#40652=VERTEX_POINT('',#403239);
#40653=VERTEX_POINT('',#403240);
#40654=VERTEX_POINT('',#403242);
#40655=VERTEX_POINT('',#403247);
#40656=VERTEX_POINT('',#403249);
#40657=VERTEX_POINT('',#403259);
#40658=VERTEX_POINT('',#403260);
#40659=VERTEX_POINT('',#403262);
#40660=VERTEX_POINT('',#403267);
#40661=VERTEX_POINT('',#403269);
#40662=VERTEX_POINT('',#403341);
#40663=VERTEX_POINT('',#403373);
#40664=VERTEX_POINT('',#403404);
#40665=VERTEX_POINT('',#403543);
#40666=VERTEX_POINT('',#403544);
#40667=VERTEX_POINT('',#403546);
#40668=VERTEX_POINT('',#403551);
#40669=VERTEX_POINT('',#403553);
#40670=VERTEX_POINT('',#403563);
#40671=VERTEX_POINT('',#403564);
#40672=VERTEX_POINT('',#403566);
#40673=VERTEX_POINT('',#403571);
#40674=VERTEX_POINT('',#403573);
#40675=VERTEX_POINT('',#403645);
#40676=VERTEX_POINT('',#403677);
#40677=VERTEX_POINT('',#403708);
#40678=VERTEX_POINT('',#403847);
#40679=VERTEX_POINT('',#403848);
#40680=VERTEX_POINT('',#403850);
#40681=VERTEX_POINT('',#403855);
#40682=VERTEX_POINT('',#403857);
#40683=VERTEX_POINT('',#403867);
#40684=VERTEX_POINT('',#403868);
#40685=VERTEX_POINT('',#403870);
#40686=VERTEX_POINT('',#403875);
#40687=VERTEX_POINT('',#403877);
#40688=VERTEX_POINT('',#403949);
#40689=VERTEX_POINT('',#403981);
#40690=VERTEX_POINT('',#404012);
#40691=VERTEX_POINT('',#404151);
#40692=VERTEX_POINT('',#404152);
#40693=VERTEX_POINT('',#404154);
#40694=VERTEX_POINT('',#404159);
#40695=VERTEX_POINT('',#404161);
#40696=VERTEX_POINT('',#404171);
#40697=VERTEX_POINT('',#404172);
#40698=VERTEX_POINT('',#404174);
#40699=VERTEX_POINT('',#404179);
#40700=VERTEX_POINT('',#404181);
#40701=VERTEX_POINT('',#404253);
#40702=VERTEX_POINT('',#404285);
#40703=VERTEX_POINT('',#404316);
#40704=VERTEX_POINT('',#404455);
#40705=VERTEX_POINT('',#404456);
#40706=VERTEX_POINT('',#404458);
#40707=VERTEX_POINT('',#404463);
#40708=VERTEX_POINT('',#404465);
#40709=VERTEX_POINT('',#404475);
#40710=VERTEX_POINT('',#404476);
#40711=VERTEX_POINT('',#404478);
#40712=VERTEX_POINT('',#404483);
#40713=VERTEX_POINT('',#404485);
#40714=VERTEX_POINT('',#404557);
#40715=VERTEX_POINT('',#404589);
#40716=VERTEX_POINT('',#404620);
#40717=VERTEX_POINT('',#404759);
#40718=VERTEX_POINT('',#404760);
#40719=VERTEX_POINT('',#404762);
#40720=VERTEX_POINT('',#404767);
#40721=VERTEX_POINT('',#404769);
#40722=VERTEX_POINT('',#404779);
#40723=VERTEX_POINT('',#404780);
#40724=VERTEX_POINT('',#404782);
#40725=VERTEX_POINT('',#404787);
#40726=VERTEX_POINT('',#404789);
#40727=VERTEX_POINT('',#404861);
#40728=VERTEX_POINT('',#404893);
#40729=VERTEX_POINT('',#404924);
#40730=VERTEX_POINT('',#405063);
#40731=VERTEX_POINT('',#405064);
#40732=VERTEX_POINT('',#405066);
#40733=VERTEX_POINT('',#405071);
#40734=VERTEX_POINT('',#405073);
#40735=VERTEX_POINT('',#405083);
#40736=VERTEX_POINT('',#405084);
#40737=VERTEX_POINT('',#405086);
#40738=VERTEX_POINT('',#405091);
#40739=VERTEX_POINT('',#405093);
#40740=VERTEX_POINT('',#405165);
#40741=VERTEX_POINT('',#405197);
#40742=VERTEX_POINT('',#405228);
#40743=VERTEX_POINT('',#405367);
#40744=VERTEX_POINT('',#405368);
#40745=VERTEX_POINT('',#405370);
#40746=VERTEX_POINT('',#405375);
#40747=VERTEX_POINT('',#405377);
#40748=VERTEX_POINT('',#405387);
#40749=VERTEX_POINT('',#405388);
#40750=VERTEX_POINT('',#405390);
#40751=VERTEX_POINT('',#405395);
#40752=VERTEX_POINT('',#405397);
#40753=VERTEX_POINT('',#405469);
#40754=VERTEX_POINT('',#405501);
#40755=VERTEX_POINT('',#405532);
#40756=VERTEX_POINT('',#405671);
#40757=VERTEX_POINT('',#405672);
#40758=VERTEX_POINT('',#405674);
#40759=VERTEX_POINT('',#405679);
#40760=VERTEX_POINT('',#405681);
#40761=VERTEX_POINT('',#405691);
#40762=VERTEX_POINT('',#405692);
#40763=VERTEX_POINT('',#405694);
#40764=VERTEX_POINT('',#405699);
#40765=VERTEX_POINT('',#405701);
#40766=VERTEX_POINT('',#405773);
#40767=VERTEX_POINT('',#405805);
#40768=VERTEX_POINT('',#405836);
#40769=VERTEX_POINT('',#405975);
#40770=VERTEX_POINT('',#405976);
#40771=VERTEX_POINT('',#405978);
#40772=VERTEX_POINT('',#405983);
#40773=VERTEX_POINT('',#405985);
#40774=VERTEX_POINT('',#405995);
#40775=VERTEX_POINT('',#405996);
#40776=VERTEX_POINT('',#405998);
#40777=VERTEX_POINT('',#406003);
#40778=VERTEX_POINT('',#406005);
#40779=VERTEX_POINT('',#406077);
#40780=VERTEX_POINT('',#406109);
#40781=VERTEX_POINT('',#406140);
#40782=VERTEX_POINT('',#406279);
#40783=VERTEX_POINT('',#406280);
#40784=VERTEX_POINT('',#406282);
#40785=VERTEX_POINT('',#406287);
#40786=VERTEX_POINT('',#406289);
#40787=VERTEX_POINT('',#406299);
#40788=VERTEX_POINT('',#406300);
#40789=VERTEX_POINT('',#406302);
#40790=VERTEX_POINT('',#406307);
#40791=VERTEX_POINT('',#406309);
#40792=VERTEX_POINT('',#406381);
#40793=VERTEX_POINT('',#406413);
#40794=VERTEX_POINT('',#406444);
#40795=VERTEX_POINT('',#406583);
#40796=VERTEX_POINT('',#406584);
#40797=VERTEX_POINT('',#406586);
#40798=VERTEX_POINT('',#406591);
#40799=VERTEX_POINT('',#406593);
#40800=VERTEX_POINT('',#406603);
#40801=VERTEX_POINT('',#406604);
#40802=VERTEX_POINT('',#406606);
#40803=VERTEX_POINT('',#406611);
#40804=VERTEX_POINT('',#406613);
#40805=VERTEX_POINT('',#406685);
#40806=VERTEX_POINT('',#406717);
#40807=VERTEX_POINT('',#406748);
#40808=VERTEX_POINT('',#406887);
#40809=VERTEX_POINT('',#406888);
#40810=VERTEX_POINT('',#406890);
#40811=VERTEX_POINT('',#406895);
#40812=VERTEX_POINT('',#406897);
#40813=VERTEX_POINT('',#406907);
#40814=VERTEX_POINT('',#406908);
#40815=VERTEX_POINT('',#406910);
#40816=VERTEX_POINT('',#406915);
#40817=VERTEX_POINT('',#406917);
#40818=VERTEX_POINT('',#406989);
#40819=VERTEX_POINT('',#407021);
#40820=VERTEX_POINT('',#407052);
#40821=VERTEX_POINT('',#407191);
#40822=VERTEX_POINT('',#407192);
#40823=VERTEX_POINT('',#407194);
#40824=VERTEX_POINT('',#407199);
#40825=VERTEX_POINT('',#407201);
#40826=VERTEX_POINT('',#407211);
#40827=VERTEX_POINT('',#407212);
#40828=VERTEX_POINT('',#407214);
#40829=VERTEX_POINT('',#407219);
#40830=VERTEX_POINT('',#407221);
#40831=VERTEX_POINT('',#407293);
#40832=VERTEX_POINT('',#407325);
#40833=VERTEX_POINT('',#407356);
#40834=VERTEX_POINT('',#407495);
#40835=VERTEX_POINT('',#407496);
#40836=VERTEX_POINT('',#407498);
#40837=VERTEX_POINT('',#407503);
#40838=VERTEX_POINT('',#407505);
#40839=VERTEX_POINT('',#407515);
#40840=VERTEX_POINT('',#407516);
#40841=VERTEX_POINT('',#407518);
#40842=VERTEX_POINT('',#407523);
#40843=VERTEX_POINT('',#407525);
#40844=VERTEX_POINT('',#407597);
#40845=VERTEX_POINT('',#407629);
#40846=VERTEX_POINT('',#407660);
#40847=VERTEX_POINT('',#407799);
#40848=VERTEX_POINT('',#407800);
#40849=VERTEX_POINT('',#407802);
#40850=VERTEX_POINT('',#407807);
#40851=VERTEX_POINT('',#407809);
#40852=VERTEX_POINT('',#407819);
#40853=VERTEX_POINT('',#407820);
#40854=VERTEX_POINT('',#407822);
#40855=VERTEX_POINT('',#407827);
#40856=VERTEX_POINT('',#407829);
#40857=VERTEX_POINT('',#407901);
#40858=VERTEX_POINT('',#407933);
#40859=VERTEX_POINT('',#407964);
#40860=VERTEX_POINT('',#408103);
#40861=VERTEX_POINT('',#408104);
#40862=VERTEX_POINT('',#408106);
#40863=VERTEX_POINT('',#408111);
#40864=VERTEX_POINT('',#408113);
#40865=VERTEX_POINT('',#408123);
#40866=VERTEX_POINT('',#408124);
#40867=VERTEX_POINT('',#408126);
#40868=VERTEX_POINT('',#408131);
#40869=VERTEX_POINT('',#408133);
#40870=VERTEX_POINT('',#408205);
#40871=VERTEX_POINT('',#408237);
#40872=VERTEX_POINT('',#408268);
#40873=VERTEX_POINT('',#408407);
#40874=VERTEX_POINT('',#408408);
#40875=VERTEX_POINT('',#408410);
#40876=VERTEX_POINT('',#408415);
#40877=VERTEX_POINT('',#408417);
#40878=VERTEX_POINT('',#408427);
#40879=VERTEX_POINT('',#408428);
#40880=VERTEX_POINT('',#408430);
#40881=VERTEX_POINT('',#408435);
#40882=VERTEX_POINT('',#408437);
#40883=VERTEX_POINT('',#408509);
#40884=VERTEX_POINT('',#408541);
#40885=VERTEX_POINT('',#408572);
#40886=VERTEX_POINT('',#408711);
#40887=VERTEX_POINT('',#408712);
#40888=VERTEX_POINT('',#408714);
#40889=VERTEX_POINT('',#408719);
#40890=VERTEX_POINT('',#408721);
#40891=VERTEX_POINT('',#408731);
#40892=VERTEX_POINT('',#408732);
#40893=VERTEX_POINT('',#408734);
#40894=VERTEX_POINT('',#408739);
#40895=VERTEX_POINT('',#408741);
#40896=VERTEX_POINT('',#408813);
#40897=VERTEX_POINT('',#408845);
#40898=VERTEX_POINT('',#408876);
#40899=VERTEX_POINT('',#409015);
#40900=VERTEX_POINT('',#409016);
#40901=VERTEX_POINT('',#409018);
#40902=VERTEX_POINT('',#409023);
#40903=VERTEX_POINT('',#409025);
#40904=VERTEX_POINT('',#409035);
#40905=VERTEX_POINT('',#409036);
#40906=VERTEX_POINT('',#409038);
#40907=VERTEX_POINT('',#409043);
#40908=VERTEX_POINT('',#409045);
#40909=VERTEX_POINT('',#409117);
#40910=VERTEX_POINT('',#409149);
#40911=VERTEX_POINT('',#409180);
#40912=VERTEX_POINT('',#409319);
#40913=VERTEX_POINT('',#409320);
#40914=VERTEX_POINT('',#409322);
#40915=VERTEX_POINT('',#409327);
#40916=VERTEX_POINT('',#409329);
#40917=VERTEX_POINT('',#409339);
#40918=VERTEX_POINT('',#409340);
#40919=VERTEX_POINT('',#409342);
#40920=VERTEX_POINT('',#409347);
#40921=VERTEX_POINT('',#409349);
#40922=VERTEX_POINT('',#409421);
#40923=VERTEX_POINT('',#409453);
#40924=VERTEX_POINT('',#409484);
#40925=VERTEX_POINT('',#409624);
#40926=VERTEX_POINT('',#409625);
#40927=VERTEX_POINT('',#409627);
#40928=VERTEX_POINT('',#409633);
#40929=VERTEX_POINT('',#409634);
#40930=VERTEX_POINT('',#409663);
#40931=VERTEX_POINT('',#409664);
#40932=VERTEX_POINT('',#409693);
#40933=VERTEX_POINT('',#409694);
#40934=VERTEX_POINT('',#409723);
#40935=VERTEX_POINT('',#409724);
#40936=VERTEX_POINT('',#409753);
#40937=VERTEX_POINT('',#409754);
#40938=VERTEX_POINT('',#409783);
#40939=VERTEX_POINT('',#409784);
#40940=VERTEX_POINT('',#409813);
#40941=VERTEX_POINT('',#409814);
#40942=VERTEX_POINT('',#409843);
#40943=VERTEX_POINT('',#409844);
#40944=VERTEX_POINT('',#409873);
#40945=VERTEX_POINT('',#409874);
#40946=VERTEX_POINT('',#409903);
#40947=VERTEX_POINT('',#409904);
#40948=VERTEX_POINT('',#409933);
#40949=VERTEX_POINT('',#409934);
#40950=VERTEX_POINT('',#409963);
#40951=VERTEX_POINT('',#409964);
#40952=VERTEX_POINT('',#409993);
#40953=VERTEX_POINT('',#409994);
#40954=VERTEX_POINT('',#410023);
#40955=VERTEX_POINT('',#410024);
#40956=VERTEX_POINT('',#410053);
#40957=VERTEX_POINT('',#410054);
#40958=VERTEX_POINT('',#410083);
#40959=VERTEX_POINT('',#410084);
#40960=VERTEX_POINT('',#410113);
#40961=VERTEX_POINT('',#410114);
#40962=VERTEX_POINT('',#410143);
#40963=VERTEX_POINT('',#410144);
#40964=VERTEX_POINT('',#410173);
#40965=VERTEX_POINT('',#410174);
#40966=VERTEX_POINT('',#410203);
#40967=VERTEX_POINT('',#410204);
#40968=VERTEX_POINT('',#410233);
#40969=VERTEX_POINT('',#410234);
#40970=VERTEX_POINT('',#410263);
#40971=VERTEX_POINT('',#410264);
#40972=VERTEX_POINT('',#410293);
#40973=VERTEX_POINT('',#410294);
#40974=VERTEX_POINT('',#410323);
#40975=VERTEX_POINT('',#410324);
#40976=VERTEX_POINT('',#410353);
#40977=VERTEX_POINT('',#410354);
#40978=VERTEX_POINT('',#410383);
#40979=VERTEX_POINT('',#410384);
#40980=VERTEX_POINT('',#410413);
#40981=VERTEX_POINT('',#410414);
#40982=VERTEX_POINT('',#410443);
#40983=VERTEX_POINT('',#410444);
#40984=VERTEX_POINT('',#410473);
#40985=VERTEX_POINT('',#410474);
#40986=VERTEX_POINT('',#410503);
#40987=VERTEX_POINT('',#410504);
#40988=VERTEX_POINT('',#410533);
#40989=VERTEX_POINT('',#410534);
#40990=VERTEX_POINT('',#410563);
#40991=VERTEX_POINT('',#410564);
#40992=VERTEX_POINT('',#410593);
#40993=VERTEX_POINT('',#410594);
#40994=VERTEX_POINT('',#410623);
#40995=VERTEX_POINT('',#410624);
#40996=VERTEX_POINT('',#410653);
#40997=VERTEX_POINT('',#410654);
#40998=VERTEX_POINT('',#410683);
#40999=VERTEX_POINT('',#410684);
#41000=VERTEX_POINT('',#410686);
#41001=VERTEX_POINT('',#410701);
#41002=VERTEX_POINT('',#410714);
#41003=VERTEX_POINT('',#410715);
#41004=VERTEX_POINT('',#410739);
#41005=VERTEX_POINT('',#410740);
#41006=VERTEX_POINT('',#410742);
#41007=VERTEX_POINT('',#410761);
#41008=VERTEX_POINT('',#410780);
#41009=VERTEX_POINT('',#410781);
#41010=VERTEX_POINT('',#410856);
#41011=VERTEX_POINT('',#410857);
#41012=VERTEX_POINT('',#410934);
#41013=VERTEX_POINT('',#410935);
#41014=VERTEX_POINT('',#411012);
#41015=VERTEX_POINT('',#411013);
#41016=VERTEX_POINT('',#411088);
#41017=VERTEX_POINT('',#411089);
#41018=VERTEX_POINT('',#411164);
#41019=VERTEX_POINT('',#411165);
#41020=VERTEX_POINT('',#411240);
#41021=VERTEX_POINT('',#411241);
#41022=VERTEX_POINT('',#411318);
#41023=VERTEX_POINT('',#411319);
#41024=VERTEX_POINT('',#411394);
#41025=VERTEX_POINT('',#411395);
#41026=VERTEX_POINT('',#411470);
#41027=VERTEX_POINT('',#411471);
#41028=VERTEX_POINT('',#411548);
#41029=VERTEX_POINT('',#411549);
#41030=VERTEX_POINT('',#411624);
#41031=VERTEX_POINT('',#411625);
#41032=VERTEX_POINT('',#411700);
#41033=VERTEX_POINT('',#411701);
#41034=VERTEX_POINT('',#411776);
#41035=VERTEX_POINT('',#411777);
#41036=VERTEX_POINT('',#411854);
#41037=VERTEX_POINT('',#411855);
#41038=VERTEX_POINT('',#411930);
#41039=VERTEX_POINT('',#411931);
#41040=VERTEX_POINT('',#412006);
#41041=VERTEX_POINT('',#412007);
#41042=VERTEX_POINT('',#412084);
#41043=VERTEX_POINT('',#412085);
#41044=VERTEX_POINT('',#412160);
#41045=VERTEX_POINT('',#412161);
#41046=VERTEX_POINT('',#412236);
#41047=VERTEX_POINT('',#412237);
#41048=VERTEX_POINT('',#412314);
#41049=VERTEX_POINT('',#412315);
#41050=VERTEX_POINT('',#412390);
#41051=VERTEX_POINT('',#412391);
#41052=VERTEX_POINT('',#412466);
#41053=VERTEX_POINT('',#412467);
#41054=VERTEX_POINT('',#412544);
#41055=VERTEX_POINT('',#412545);
#41056=VERTEX_POINT('',#412620);
#41057=VERTEX_POINT('',#412621);
#41058=VERTEX_POINT('',#412696);
#41059=VERTEX_POINT('',#412697);
#41060=VERTEX_POINT('',#412772);
#41061=VERTEX_POINT('',#412773);
#41062=VERTEX_POINT('',#412850);
#41063=VERTEX_POINT('',#412851);
#41064=VERTEX_POINT('',#412926);
#41065=VERTEX_POINT('',#412927);
#41066=VERTEX_POINT('',#413002);
#41067=VERTEX_POINT('',#413003);
#41068=VERTEX_POINT('',#413080);
#41069=VERTEX_POINT('',#413081);
#41070=VERTEX_POINT('',#413119);
#41071=VERTEX_POINT('',#413161);
#41072=VERTEX_POINT('',#413162);
#41073=VERTEX_POINT('',#413237);
#41074=VERTEX_POINT('',#413238);
#41075=VERTEX_POINT('',#413315);
#41076=VERTEX_POINT('',#413318);
#41077=VERTEX_POINT('',#413320);
#41078=VERTEX_POINT('',#413353);
#41079=VERTEX_POINT('',#413392);
#41080=VERTEX_POINT('',#413393);
#41081=VERTEX_POINT('',#413395);
#41082=VERTEX_POINT('',#413397);
#41083=VERTEX_POINT('',#413401);
#41084=VERTEX_POINT('',#413402);
#41085=VERTEX_POINT('',#413404);
#41086=VERTEX_POINT('',#413406);
#41087=VERTEX_POINT('',#413410);
#41088=VERTEX_POINT('',#413411);
#41089=VERTEX_POINT('',#413413);
#41090=VERTEX_POINT('',#413415);
#41091=VERTEX_POINT('',#413419);
#41092=VERTEX_POINT('',#413420);
#41093=VERTEX_POINT('',#413422);
#41094=VERTEX_POINT('',#413424);
#41095=VERTEX_POINT('',#413428);
#41096=VERTEX_POINT('',#413429);
#41097=VERTEX_POINT('',#413431);
#41098=VERTEX_POINT('',#413433);
#41099=VERTEX_POINT('',#413437);
#41100=VERTEX_POINT('',#413438);
#41101=VERTEX_POINT('',#413440);
#41102=VERTEX_POINT('',#413442);
#41103=VERTEX_POINT('',#413446);
#41104=VERTEX_POINT('',#413447);
#41105=VERTEX_POINT('',#413449);
#41106=VERTEX_POINT('',#413451);
#41107=VERTEX_POINT('',#413455);
#41108=VERTEX_POINT('',#413456);
#41109=VERTEX_POINT('',#413458);
#41110=VERTEX_POINT('',#413460);
#41111=VERTEX_POINT('',#413464);
#41112=VERTEX_POINT('',#413465);
#41113=VERTEX_POINT('',#413467);
#41114=VERTEX_POINT('',#413469);
#41115=VERTEX_POINT('',#413473);
#41116=VERTEX_POINT('',#413474);
#41117=VERTEX_POINT('',#413476);
#41118=VERTEX_POINT('',#413478);
#41119=VERTEX_POINT('',#413482);
#41120=VERTEX_POINT('',#413483);
#41121=VERTEX_POINT('',#413485);
#41122=VERTEX_POINT('',#413487);
#41123=VERTEX_POINT('',#413491);
#41124=VERTEX_POINT('',#413492);
#41125=VERTEX_POINT('',#413494);
#41126=VERTEX_POINT('',#413496);
#41127=VERTEX_POINT('',#413500);
#41128=VERTEX_POINT('',#413501);
#41129=VERTEX_POINT('',#413503);
#41130=VERTEX_POINT('',#413505);
#41131=VERTEX_POINT('',#413509);
#41132=VERTEX_POINT('',#413510);
#41133=VERTEX_POINT('',#413512);
#41134=VERTEX_POINT('',#413514);
#41135=VERTEX_POINT('',#413518);
#41136=VERTEX_POINT('',#413519);
#41137=VERTEX_POINT('',#413521);
#41138=VERTEX_POINT('',#413523);
#41139=VERTEX_POINT('',#413527);
#41140=VERTEX_POINT('',#413528);
#41141=VERTEX_POINT('',#413530);
#41142=VERTEX_POINT('',#413532);
#41143=VERTEX_POINT('',#413536);
#41144=VERTEX_POINT('',#413537);
#41145=VERTEX_POINT('',#413539);
#41146=VERTEX_POINT('',#413541);
#41147=VERTEX_POINT('',#413545);
#41148=VERTEX_POINT('',#413546);
#41149=VERTEX_POINT('',#413548);
#41150=VERTEX_POINT('',#413550);
#41151=VERTEX_POINT('',#413554);
#41152=VERTEX_POINT('',#413555);
#41153=VERTEX_POINT('',#413557);
#41154=VERTEX_POINT('',#413559);
#41155=VERTEX_POINT('',#413563);
#41156=VERTEX_POINT('',#413564);
#41157=VERTEX_POINT('',#413566);
#41158=VERTEX_POINT('',#413568);
#41159=VERTEX_POINT('',#413572);
#41160=VERTEX_POINT('',#413573);
#41161=VERTEX_POINT('',#413575);
#41162=VERTEX_POINT('',#413577);
#41163=VERTEX_POINT('',#413581);
#41164=VERTEX_POINT('',#413582);
#41165=VERTEX_POINT('',#413584);
#41166=VERTEX_POINT('',#413586);
#41167=VERTEX_POINT('',#413590);
#41168=VERTEX_POINT('',#413591);
#41169=VERTEX_POINT('',#413593);
#41170=VERTEX_POINT('',#413595);
#41171=VERTEX_POINT('',#413599);
#41172=VERTEX_POINT('',#413600);
#41173=VERTEX_POINT('',#413602);
#41174=VERTEX_POINT('',#413604);
#41175=VERTEX_POINT('',#413608);
#41176=VERTEX_POINT('',#413609);
#41177=VERTEX_POINT('',#413611);
#41178=VERTEX_POINT('',#413613);
#41179=VERTEX_POINT('',#413617);
#41180=VERTEX_POINT('',#413618);
#41181=VERTEX_POINT('',#413620);
#41182=VERTEX_POINT('',#413622);
#41183=VERTEX_POINT('',#413626);
#41184=VERTEX_POINT('',#413627);
#41185=VERTEX_POINT('',#413629);
#41186=VERTEX_POINT('',#413631);
#41187=VERTEX_POINT('',#413635);
#41188=VERTEX_POINT('',#413636);
#41189=VERTEX_POINT('',#413638);
#41190=VERTEX_POINT('',#413640);
#41191=VERTEX_POINT('',#413644);
#41192=VERTEX_POINT('',#413645);
#41193=VERTEX_POINT('',#413647);
#41194=VERTEX_POINT('',#413649);
#41195=VERTEX_POINT('',#413653);
#41196=VERTEX_POINT('',#413654);
#41197=VERTEX_POINT('',#413656);
#41198=VERTEX_POINT('',#413658);
#41199=VERTEX_POINT('',#413662);
#41200=VERTEX_POINT('',#413663);
#41201=VERTEX_POINT('',#413665);
#41202=VERTEX_POINT('',#413667);
#41203=VERTEX_POINT('',#413671);
#41204=VERTEX_POINT('',#413672);
#41205=VERTEX_POINT('',#413674);
#41206=VERTEX_POINT('',#413676);
#41207=VERTEX_POINT('',#413680);
#41208=VERTEX_POINT('',#413681);
#41209=VERTEX_POINT('',#413683);
#41210=VERTEX_POINT('',#413685);
#41211=VERTEX_POINT('',#413689);
#41212=VERTEX_POINT('',#413690);
#41213=VERTEX_POINT('',#413692);
#41214=VERTEX_POINT('',#413694);
#41215=VERTEX_POINT('',#413698);
#41216=VERTEX_POINT('',#413699);
#41217=VERTEX_POINT('',#413701);
#41218=VERTEX_POINT('',#413703);
#41219=VERTEX_POINT('',#413707);
#41220=VERTEX_POINT('',#413708);
#41221=VERTEX_POINT('',#413710);
#41222=VERTEX_POINT('',#413712);
#41223=VERTEX_POINT('',#413716);
#41224=VERTEX_POINT('',#413717);
#41225=VERTEX_POINT('',#413719);
#41226=VERTEX_POINT('',#413721);
#41227=VERTEX_POINT('',#413725);
#41228=VERTEX_POINT('',#413726);
#41229=VERTEX_POINT('',#413728);
#41230=VERTEX_POINT('',#413730);
#41231=VERTEX_POINT('',#413734);
#41232=VERTEX_POINT('',#413735);
#41233=VERTEX_POINT('',#413737);
#41234=VERTEX_POINT('',#413739);
#41235=VERTEX_POINT('',#413743);
#41236=VERTEX_POINT('',#413744);
#41237=VERTEX_POINT('',#413746);
#41238=VERTEX_POINT('',#413748);
#41239=VERTEX_POINT('',#413752);
#41240=VERTEX_POINT('',#413753);
#41241=VERTEX_POINT('',#413755);
#41242=VERTEX_POINT('',#413757);
#41243=VERTEX_POINT('',#413761);
#41244=VERTEX_POINT('',#413762);
#41245=VERTEX_POINT('',#413764);
#41246=VERTEX_POINT('',#413766);
#41247=VERTEX_POINT('',#413770);
#41248=VERTEX_POINT('',#413771);
#41249=VERTEX_POINT('',#413773);
#41250=VERTEX_POINT('',#413775);
#41251=VERTEX_POINT('',#413779);
#41252=VERTEX_POINT('',#413780);
#41253=VERTEX_POINT('',#413782);
#41254=VERTEX_POINT('',#413784);
#41255=VERTEX_POINT('',#413788);
#41256=VERTEX_POINT('',#413789);
#41257=VERTEX_POINT('',#413791);
#41258=VERTEX_POINT('',#413793);
#41259=VERTEX_POINT('',#413797);
#41260=VERTEX_POINT('',#413798);
#41261=VERTEX_POINT('',#413800);
#41262=VERTEX_POINT('',#413802);
#41263=VERTEX_POINT('',#413806);
#41264=VERTEX_POINT('',#413807);
#41265=VERTEX_POINT('',#413809);
#41266=VERTEX_POINT('',#413811);
#41267=VERTEX_POINT('',#413815);
#41268=VERTEX_POINT('',#413816);
#41269=VERTEX_POINT('',#413818);
#41270=VERTEX_POINT('',#413820);
#41271=VERTEX_POINT('',#413824);
#41272=VERTEX_POINT('',#413825);
#41273=VERTEX_POINT('',#413827);
#41274=VERTEX_POINT('',#413829);
#41275=VERTEX_POINT('',#413833);
#41276=VERTEX_POINT('',#413834);
#41277=VERTEX_POINT('',#413836);
#41278=VERTEX_POINT('',#413838);
#41279=VERTEX_POINT('',#413842);
#41280=VERTEX_POINT('',#413843);
#41281=VERTEX_POINT('',#413845);
#41282=VERTEX_POINT('',#413847);
#41283=VERTEX_POINT('',#413851);
#41284=VERTEX_POINT('',#413852);
#41285=VERTEX_POINT('',#413854);
#41286=VERTEX_POINT('',#413856);
#41287=VERTEX_POINT('',#413860);
#41288=VERTEX_POINT('',#413861);
#41289=VERTEX_POINT('',#413863);
#41290=VERTEX_POINT('',#413865);
#41291=VERTEX_POINT('',#413869);
#41292=VERTEX_POINT('',#413870);
#41293=VERTEX_POINT('',#413872);
#41294=VERTEX_POINT('',#413874);
#41295=VERTEX_POINT('',#413878);
#41296=VERTEX_POINT('',#413879);
#41297=VERTEX_POINT('',#413881);
#41298=VERTEX_POINT('',#413883);
#41299=VERTEX_POINT('',#413887);
#41300=VERTEX_POINT('',#413888);
#41301=VERTEX_POINT('',#413890);
#41302=VERTEX_POINT('',#413892);
#41303=VERTEX_POINT('',#413896);
#41304=VERTEX_POINT('',#413897);
#41305=VERTEX_POINT('',#413899);
#41306=VERTEX_POINT('',#413901);
#41307=VERTEX_POINT('',#413905);
#41308=VERTEX_POINT('',#413906);
#41309=VERTEX_POINT('',#413908);
#41310=VERTEX_POINT('',#413910);
#41311=VERTEX_POINT('',#413914);
#41312=VERTEX_POINT('',#413915);
#41313=VERTEX_POINT('',#413917);
#41314=VERTEX_POINT('',#413919);
#41315=VERTEX_POINT('',#413923);
#41316=VERTEX_POINT('',#413924);
#41317=VERTEX_POINT('',#413926);
#41318=VERTEX_POINT('',#413928);
#41319=VERTEX_POINT('',#413932);
#41320=VERTEX_POINT('',#413933);
#41321=VERTEX_POINT('',#413935);
#41322=VERTEX_POINT('',#413937);
#41323=VERTEX_POINT('',#413941);
#41324=VERTEX_POINT('',#413942);
#41325=VERTEX_POINT('',#413944);
#41326=VERTEX_POINT('',#413946);
#41327=VERTEX_POINT('',#413950);
#41328=VERTEX_POINT('',#413951);
#41329=VERTEX_POINT('',#413953);
#41330=VERTEX_POINT('',#413955);
#41331=VERTEX_POINT('',#413959);
#41332=VERTEX_POINT('',#413960);
#41333=VERTEX_POINT('',#413962);
#41334=VERTEX_POINT('',#413964);
#41335=VERTEX_POINT('',#413968);
#41336=VERTEX_POINT('',#413969);
#41337=VERTEX_POINT('',#413971);
#41338=VERTEX_POINT('',#413973);
#41339=VERTEX_POINT('',#413977);
#41340=VERTEX_POINT('',#413978);
#41341=VERTEX_POINT('',#413980);
#41342=VERTEX_POINT('',#413982);
#41343=VERTEX_POINT('',#413986);
#41344=VERTEX_POINT('',#413987);
#41345=VERTEX_POINT('',#413989);
#41346=VERTEX_POINT('',#413991);
#41347=VERTEX_POINT('',#413995);
#41348=VERTEX_POINT('',#413996);
#41349=VERTEX_POINT('',#413998);
#41350=VERTEX_POINT('',#414000);
#41351=VERTEX_POINT('',#414004);
#41352=VERTEX_POINT('',#414005);
#41353=VERTEX_POINT('',#414007);
#41354=VERTEX_POINT('',#414009);
#41355=VERTEX_POINT('',#414013);
#41356=VERTEX_POINT('',#414014);
#41357=VERTEX_POINT('',#414016);
#41358=VERTEX_POINT('',#414018);
#41359=VERTEX_POINT('',#414022);
#41360=VERTEX_POINT('',#414023);
#41361=VERTEX_POINT('',#414025);
#41362=VERTEX_POINT('',#414027);
#41363=VERTEX_POINT('',#414031);
#41364=VERTEX_POINT('',#414032);
#41365=VERTEX_POINT('',#414034);
#41366=VERTEX_POINT('',#414036);
#41367=VERTEX_POINT('',#414040);
#41368=VERTEX_POINT('',#414041);
#41369=VERTEX_POINT('',#414043);
#41370=VERTEX_POINT('',#414045);
#41371=VERTEX_POINT('',#414049);
#41372=VERTEX_POINT('',#414050);
#41373=VERTEX_POINT('',#414052);
#41374=VERTEX_POINT('',#414054);
#41375=VERTEX_POINT('',#414058);
#41376=VERTEX_POINT('',#414059);
#41377=VERTEX_POINT('',#414061);
#41378=VERTEX_POINT('',#414063);
#41379=VERTEX_POINT('',#414067);
#41380=VERTEX_POINT('',#414068);
#41381=VERTEX_POINT('',#414070);
#41382=VERTEX_POINT('',#414072);
#41383=VERTEX_POINT('',#414076);
#41384=VERTEX_POINT('',#414077);
#41385=VERTEX_POINT('',#414079);
#41386=VERTEX_POINT('',#414081);
#41387=VERTEX_POINT('',#414083);
#41388=VERTEX_POINT('',#414196);
#41389=VERTEX_POINT('',#414233);
#41390=VERTEX_POINT('',#414234);
#41391=VERTEX_POINT('',#414236);
#41392=VERTEX_POINT('',#414238);
#41393=VERTEX_POINT('',#414240);
#41394=VERTEX_POINT('',#414242);
#41395=VERTEX_POINT('',#414244);
#41396=VERTEX_POINT('',#414248);
#41397=VERTEX_POINT('',#414249);
#41398=VERTEX_POINT('',#414255);
#41399=VERTEX_POINT('',#414257);
#41400=VERTEX_POINT('',#414261);
#41401=VERTEX_POINT('',#414265);
#41402=VERTEX_POINT('',#414269);
#41403=VERTEX_POINT('',#414270);
#41404=VERTEX_POINT('',#414287);
#41405=VERTEX_POINT('',#414289);
#41406=VERTEX_POINT('',#414291);
#41407=VERTEX_POINT('',#414293);
#41408=VERTEX_POINT('',#414319);
#41409=VERTEX_POINT('',#414321);
#41410=VERTEX_POINT('',#414323);
#41411=VERTEX_POINT('',#414325);
#41412=VERTEX_POINT('',#414351);
#41413=VERTEX_POINT('',#414353);
#41414=VERTEX_POINT('',#414355);
#41415=VERTEX_POINT('',#414357);
#41416=VERTEX_POINT('',#414383);
#41417=VERTEX_POINT('',#414385);
#41418=VERTEX_POINT('',#414387);
#41419=VERTEX_POINT('',#414389);
#41420=VERTEX_POINT('',#414415);
#41421=VERTEX_POINT('',#414417);
#41422=VERTEX_POINT('',#414419);
#41423=VERTEX_POINT('',#414421);
#41424=VERTEX_POINT('',#414447);
#41425=VERTEX_POINT('',#414449);
#41426=VERTEX_POINT('',#414451);
#41427=VERTEX_POINT('',#414453);
#41428=VERTEX_POINT('',#414479);
#41429=VERTEX_POINT('',#414481);
#41430=VERTEX_POINT('',#414483);
#41431=VERTEX_POINT('',#414485);
#41432=VERTEX_POINT('',#414511);
#41433=VERTEX_POINT('',#414513);
#41434=VERTEX_POINT('',#414515);
#41435=VERTEX_POINT('',#414517);
#41436=VERTEX_POINT('',#414543);
#41437=VERTEX_POINT('',#414545);
#41438=VERTEX_POINT('',#414547);
#41439=VERTEX_POINT('',#414549);
#41440=VERTEX_POINT('',#414575);
#41441=VERTEX_POINT('',#414577);
#41442=VERTEX_POINT('',#414579);
#41443=VERTEX_POINT('',#414581);
#41444=VERTEX_POINT('',#414607);
#41445=VERTEX_POINT('',#414609);
#41446=VERTEX_POINT('',#414611);
#41447=VERTEX_POINT('',#414613);
#41448=VERTEX_POINT('',#414639);
#41449=VERTEX_POINT('',#414641);
#41450=VERTEX_POINT('',#414643);
#41451=VERTEX_POINT('',#414645);
#41452=VERTEX_POINT('',#414671);
#41453=VERTEX_POINT('',#414673);
#41454=VERTEX_POINT('',#414675);
#41455=VERTEX_POINT('',#414677);
#41456=VERTEX_POINT('',#414703);
#41457=VERTEX_POINT('',#414705);
#41458=VERTEX_POINT('',#414707);
#41459=VERTEX_POINT('',#414709);
#41460=VERTEX_POINT('',#414735);
#41461=VERTEX_POINT('',#414737);
#41462=VERTEX_POINT('',#414739);
#41463=VERTEX_POINT('',#414741);
#41464=VERTEX_POINT('',#414767);
#41465=VERTEX_POINT('',#414769);
#41466=VERTEX_POINT('',#414771);
#41467=VERTEX_POINT('',#414773);
#41468=VERTEX_POINT('',#414799);
#41469=VERTEX_POINT('',#414801);
#41470=VERTEX_POINT('',#414803);
#41471=VERTEX_POINT('',#414805);
#41472=VERTEX_POINT('',#414831);
#41473=VERTEX_POINT('',#414833);
#41474=VERTEX_POINT('',#414835);
#41475=VERTEX_POINT('',#414837);
#41476=VERTEX_POINT('',#414863);
#41477=VERTEX_POINT('',#414865);
#41478=VERTEX_POINT('',#414867);
#41479=VERTEX_POINT('',#414869);
#41480=VERTEX_POINT('',#414895);
#41481=VERTEX_POINT('',#414897);
#41482=VERTEX_POINT('',#414899);
#41483=VERTEX_POINT('',#414901);
#41484=VERTEX_POINT('',#414927);
#41485=VERTEX_POINT('',#414929);
#41486=VERTEX_POINT('',#414931);
#41487=VERTEX_POINT('',#414933);
#41488=VERTEX_POINT('',#414959);
#41489=VERTEX_POINT('',#414961);
#41490=VERTEX_POINT('',#414963);
#41491=VERTEX_POINT('',#414965);
#41492=VERTEX_POINT('',#414991);
#41493=VERTEX_POINT('',#414993);
#41494=VERTEX_POINT('',#414995);
#41495=VERTEX_POINT('',#414997);
#41496=VERTEX_POINT('',#415023);
#41497=VERTEX_POINT('',#415025);
#41498=VERTEX_POINT('',#415027);
#41499=VERTEX_POINT('',#415029);
#41500=VERTEX_POINT('',#415055);
#41501=VERTEX_POINT('',#415057);
#41502=VERTEX_POINT('',#415059);
#41503=VERTEX_POINT('',#415061);
#41504=VERTEX_POINT('',#415087);
#41505=VERTEX_POINT('',#415089);
#41506=VERTEX_POINT('',#415091);
#41507=VERTEX_POINT('',#415093);
#41508=VERTEX_POINT('',#415119);
#41509=VERTEX_POINT('',#415121);
#41510=VERTEX_POINT('',#415123);
#41511=VERTEX_POINT('',#415125);
#41512=VERTEX_POINT('',#415151);
#41513=VERTEX_POINT('',#415153);
#41514=VERTEX_POINT('',#415155);
#41515=VERTEX_POINT('',#415157);
#41516=VERTEX_POINT('',#415183);
#41517=VERTEX_POINT('',#415185);
#41518=VERTEX_POINT('',#415187);
#41519=VERTEX_POINT('',#415189);
#41520=VERTEX_POINT('',#415215);
#41521=VERTEX_POINT('',#415217);
#41522=VERTEX_POINT('',#415219);
#41523=VERTEX_POINT('',#415221);
#41524=VERTEX_POINT('',#415247);
#41525=VERTEX_POINT('',#415249);
#41526=VERTEX_POINT('',#415251);
#41527=VERTEX_POINT('',#415253);
#41528=VERTEX_POINT('',#415279);
#41529=VERTEX_POINT('',#415281);
#41530=VERTEX_POINT('',#415283);
#41531=VERTEX_POINT('',#415285);
#41532=VERTEX_POINT('',#415311);
#41533=VERTEX_POINT('',#415313);
#41534=VERTEX_POINT('',#415315);
#41535=VERTEX_POINT('',#415317);
#41536=VERTEX_POINT('',#415343);
#41537=VERTEX_POINT('',#415345);
#41538=VERTEX_POINT('',#415347);
#41539=VERTEX_POINT('',#415349);
#41540=VERTEX_POINT('',#415375);
#41541=VERTEX_POINT('',#415377);
#41542=VERTEX_POINT('',#415379);
#41543=VERTEX_POINT('',#415381);
#41544=VERTEX_POINT('',#415407);
#41545=VERTEX_POINT('',#415409);
#41546=VERTEX_POINT('',#415411);
#41547=VERTEX_POINT('',#415413);
#41548=VERTEX_POINT('',#415439);
#41549=VERTEX_POINT('',#415441);
#41550=VERTEX_POINT('',#415443);
#41551=VERTEX_POINT('',#415445);
#41552=VERTEX_POINT('',#415471);
#41553=VERTEX_POINT('',#415473);
#41554=VERTEX_POINT('',#415475);
#41555=VERTEX_POINT('',#415477);
#41556=VERTEX_POINT('',#415503);
#41557=VERTEX_POINT('',#415505);
#41558=VERTEX_POINT('',#415507);
#41559=VERTEX_POINT('',#415509);
#41560=VERTEX_POINT('',#415512);
#41561=VERTEX_POINT('',#415514);
#41562=VERTEX_POINT('',#415516);
#41563=VERTEX_POINT('',#415542);
#41564=VERTEX_POINT('',#415544);
#41565=VERTEX_POINT('',#415546);
#41566=VERTEX_POINT('',#415548);
#41567=VERTEX_POINT('',#415574);
#41568=VERTEX_POINT('',#415576);
#41569=VERTEX_POINT('',#415578);
#41570=VERTEX_POINT('',#415580);
#41571=VERTEX_POINT('',#415606);
#41572=VERTEX_POINT('',#415608);
#41573=VERTEX_POINT('',#415610);
#41574=VERTEX_POINT('',#415612);
#41575=VERTEX_POINT('',#415638);
#41576=VERTEX_POINT('',#415640);
#41577=VERTEX_POINT('',#415642);
#41578=VERTEX_POINT('',#415644);
#41579=VERTEX_POINT('',#415670);
#41580=VERTEX_POINT('',#415672);
#41581=VERTEX_POINT('',#415674);
#41582=VERTEX_POINT('',#415676);
#41583=VERTEX_POINT('',#415702);
#41584=VERTEX_POINT('',#415704);
#41585=VERTEX_POINT('',#415706);
#41586=VERTEX_POINT('',#415708);
#41587=VERTEX_POINT('',#415734);
#41588=VERTEX_POINT('',#415736);
#41589=VERTEX_POINT('',#415738);
#41590=VERTEX_POINT('',#415740);
#41591=VERTEX_POINT('',#415766);
#41592=VERTEX_POINT('',#415768);
#41593=VERTEX_POINT('',#415770);
#41594=VERTEX_POINT('',#415772);
#41595=VERTEX_POINT('',#415798);
#41596=VERTEX_POINT('',#415800);
#41597=VERTEX_POINT('',#415802);
#41598=VERTEX_POINT('',#415804);
#41599=VERTEX_POINT('',#415830);
#41600=VERTEX_POINT('',#415832);
#41601=VERTEX_POINT('',#415834);
#41602=VERTEX_POINT('',#415836);
#41603=VERTEX_POINT('',#415862);
#41604=VERTEX_POINT('',#415864);
#41605=VERTEX_POINT('',#415866);
#41606=VERTEX_POINT('',#415868);
#41607=VERTEX_POINT('',#415894);
#41608=VERTEX_POINT('',#415896);
#41609=VERTEX_POINT('',#415898);
#41610=VERTEX_POINT('',#415900);
#41611=VERTEX_POINT('',#415926);
#41612=VERTEX_POINT('',#415928);
#41613=VERTEX_POINT('',#415930);
#41614=VERTEX_POINT('',#415932);
#41615=VERTEX_POINT('',#415958);
#41616=VERTEX_POINT('',#415960);
#41617=VERTEX_POINT('',#415962);
#41618=VERTEX_POINT('',#415964);
#41619=VERTEX_POINT('',#415990);
#41620=VERTEX_POINT('',#415992);
#41621=VERTEX_POINT('',#415994);
#41622=VERTEX_POINT('',#415996);
#41623=VERTEX_POINT('',#416022);
#41624=VERTEX_POINT('',#416024);
#41625=VERTEX_POINT('',#416026);
#41626=VERTEX_POINT('',#416028);
#41627=VERTEX_POINT('',#416054);
#41628=VERTEX_POINT('',#416056);
#41629=VERTEX_POINT('',#416058);
#41630=VERTEX_POINT('',#416060);
#41631=VERTEX_POINT('',#416086);
#41632=VERTEX_POINT('',#416088);
#41633=VERTEX_POINT('',#416090);
#41634=VERTEX_POINT('',#416092);
#41635=VERTEX_POINT('',#416118);
#41636=VERTEX_POINT('',#416120);
#41637=VERTEX_POINT('',#416122);
#41638=VERTEX_POINT('',#416124);
#41639=VERTEX_POINT('',#416150);
#41640=VERTEX_POINT('',#416152);
#41641=VERTEX_POINT('',#416154);
#41642=VERTEX_POINT('',#416156);
#41643=VERTEX_POINT('',#416182);
#41644=VERTEX_POINT('',#416184);
#41645=VERTEX_POINT('',#416186);
#41646=VERTEX_POINT('',#416188);
#41647=VERTEX_POINT('',#416214);
#41648=VERTEX_POINT('',#416216);
#41649=VERTEX_POINT('',#416218);
#41650=VERTEX_POINT('',#416220);
#41651=VERTEX_POINT('',#416246);
#41652=VERTEX_POINT('',#416248);
#41653=VERTEX_POINT('',#416250);
#41654=VERTEX_POINT('',#416252);
#41655=VERTEX_POINT('',#416278);
#41656=VERTEX_POINT('',#416280);
#41657=VERTEX_POINT('',#416282);
#41658=VERTEX_POINT('',#416284);
#41659=VERTEX_POINT('',#416310);
#41660=VERTEX_POINT('',#416312);
#41661=VERTEX_POINT('',#416314);
#41662=VERTEX_POINT('',#416316);
#41663=VERTEX_POINT('',#416342);
#41664=VERTEX_POINT('',#416344);
#41665=VERTEX_POINT('',#416346);
#41666=VERTEX_POINT('',#416348);
#41667=VERTEX_POINT('',#416374);
#41668=VERTEX_POINT('',#416376);
#41669=VERTEX_POINT('',#416378);
#41670=VERTEX_POINT('',#416380);
#41671=VERTEX_POINT('',#416406);
#41672=VERTEX_POINT('',#416408);
#41673=VERTEX_POINT('',#416410);
#41674=VERTEX_POINT('',#416412);
#41675=VERTEX_POINT('',#416438);
#41676=VERTEX_POINT('',#416440);
#41677=VERTEX_POINT('',#416442);
#41678=VERTEX_POINT('',#416444);
#41679=VERTEX_POINT('',#416470);
#41680=VERTEX_POINT('',#416472);
#41681=VERTEX_POINT('',#416474);
#41682=VERTEX_POINT('',#416476);
#41683=VERTEX_POINT('',#416502);
#41684=VERTEX_POINT('',#416504);
#41685=VERTEX_POINT('',#416506);
#41686=VERTEX_POINT('',#416508);
#41687=VERTEX_POINT('',#416534);
#41688=VERTEX_POINT('',#416536);
#41689=VERTEX_POINT('',#416538);
#41690=VERTEX_POINT('',#416540);
#41691=VERTEX_POINT('',#416566);
#41692=VERTEX_POINT('',#416568);
#41693=VERTEX_POINT('',#416570);
#41694=VERTEX_POINT('',#416572);
#41695=VERTEX_POINT('',#416598);
#41696=VERTEX_POINT('',#416600);
#41697=VERTEX_POINT('',#416602);
#41698=VERTEX_POINT('',#416604);
#41699=VERTEX_POINT('',#416630);
#41700=VERTEX_POINT('',#416632);
#41701=VERTEX_POINT('',#416634);
#41702=VERTEX_POINT('',#416636);
#41703=VERTEX_POINT('',#416662);
#41704=VERTEX_POINT('',#416664);
#41705=VERTEX_POINT('',#416666);
#41706=VERTEX_POINT('',#416668);
#41707=VERTEX_POINT('',#416694);
#41708=VERTEX_POINT('',#416696);
#41709=VERTEX_POINT('',#416698);
#41710=VERTEX_POINT('',#416700);
#41711=VERTEX_POINT('',#416726);
#41712=VERTEX_POINT('',#416728);
#41713=VERTEX_POINT('',#416730);
#41714=VERTEX_POINT('',#416746);
#41715=VERTEX_POINT('',#416750);
#41716=VERTEX_POINT('',#416751);
#41717=VERTEX_POINT('',#416753);
#41718=VERTEX_POINT('',#416771);
#41719=VERTEX_POINT('',#416788);
#41720=VERTEX_POINT('',#416790);
#41721=VERTEX_POINT('',#416792);
#41722=VERTEX_POINT('',#416810);
#41723=VERTEX_POINT('',#416827);
#41724=VERTEX_POINT('',#416829);
#41725=VERTEX_POINT('',#416831);
#41726=VERTEX_POINT('',#416849);
#41727=VERTEX_POINT('',#416866);
#41728=VERTEX_POINT('',#416868);
#41729=VERTEX_POINT('',#416870);
#41730=VERTEX_POINT('',#416888);
#41731=VERTEX_POINT('',#416905);
#41732=VERTEX_POINT('',#416907);
#41733=VERTEX_POINT('',#416909);
#41734=VERTEX_POINT('',#416927);
#41735=VERTEX_POINT('',#416944);
#41736=VERTEX_POINT('',#416946);
#41737=VERTEX_POINT('',#416948);
#41738=VERTEX_POINT('',#416966);
#41739=VERTEX_POINT('',#416983);
#41740=VERTEX_POINT('',#416985);
#41741=VERTEX_POINT('',#416987);
#41742=VERTEX_POINT('',#417005);
#41743=VERTEX_POINT('',#417022);
#41744=VERTEX_POINT('',#417024);
#41745=VERTEX_POINT('',#417026);
#41746=VERTEX_POINT('',#417044);
#41747=VERTEX_POINT('',#417061);
#41748=VERTEX_POINT('',#417063);
#41749=VERTEX_POINT('',#417065);
#41750=VERTEX_POINT('',#417083);
#41751=VERTEX_POINT('',#417100);
#41752=VERTEX_POINT('',#417102);
#41753=VERTEX_POINT('',#417104);
#41754=VERTEX_POINT('',#417122);
#41755=VERTEX_POINT('',#417139);
#41756=VERTEX_POINT('',#417141);
#41757=VERTEX_POINT('',#417143);
#41758=VERTEX_POINT('',#417161);
#41759=VERTEX_POINT('',#417178);
#41760=VERTEX_POINT('',#417180);
#41761=VERTEX_POINT('',#417182);
#41762=VERTEX_POINT('',#417200);
#41763=VERTEX_POINT('',#417217);
#41764=VERTEX_POINT('',#417219);
#41765=VERTEX_POINT('',#417221);
#41766=VERTEX_POINT('',#417239);
#41767=VERTEX_POINT('',#417256);
#41768=VERTEX_POINT('',#417258);
#41769=VERTEX_POINT('',#417260);
#41770=VERTEX_POINT('',#417278);
#41771=VERTEX_POINT('',#417295);
#41772=VERTEX_POINT('',#417297);
#41773=VERTEX_POINT('',#417299);
#41774=VERTEX_POINT('',#417317);
#41775=VERTEX_POINT('',#417334);
#41776=VERTEX_POINT('',#417336);
#41777=VERTEX_POINT('',#417338);
#41778=VERTEX_POINT('',#417356);
#41779=VERTEX_POINT('',#417373);
#41780=VERTEX_POINT('',#417375);
#41781=VERTEX_POINT('',#417377);
#41782=VERTEX_POINT('',#417395);
#41783=VERTEX_POINT('',#417412);
#41784=VERTEX_POINT('',#417414);
#41785=VERTEX_POINT('',#417416);
#41786=VERTEX_POINT('',#417434);
#41787=VERTEX_POINT('',#417451);
#41788=VERTEX_POINT('',#417453);
#41789=VERTEX_POINT('',#417455);
#41790=VERTEX_POINT('',#417473);
#41791=VERTEX_POINT('',#417490);
#41792=VERTEX_POINT('',#417492);
#41793=VERTEX_POINT('',#417494);
#41794=VERTEX_POINT('',#417512);
#41795=VERTEX_POINT('',#417529);
#41796=VERTEX_POINT('',#417531);
#41797=VERTEX_POINT('',#417533);
#41798=VERTEX_POINT('',#417551);
#41799=VERTEX_POINT('',#417568);
#41800=VERTEX_POINT('',#417570);
#41801=VERTEX_POINT('',#417572);
#41802=VERTEX_POINT('',#417590);
#41803=VERTEX_POINT('',#417607);
#41804=VERTEX_POINT('',#417609);
#41805=VERTEX_POINT('',#417611);
#41806=VERTEX_POINT('',#417629);
#41807=VERTEX_POINT('',#417646);
#41808=VERTEX_POINT('',#417648);
#41809=VERTEX_POINT('',#417650);
#41810=VERTEX_POINT('',#417668);
#41811=VERTEX_POINT('',#417685);
#41812=VERTEX_POINT('',#417687);
#41813=VERTEX_POINT('',#417689);
#41814=VERTEX_POINT('',#417707);
#41815=VERTEX_POINT('',#417724);
#41816=VERTEX_POINT('',#417726);
#41817=VERTEX_POINT('',#417728);
#41818=VERTEX_POINT('',#417746);
#41819=VERTEX_POINT('',#417763);
#41820=VERTEX_POINT('',#417765);
#41821=VERTEX_POINT('',#417767);
#41822=VERTEX_POINT('',#417785);
#41823=VERTEX_POINT('',#417802);
#41824=VERTEX_POINT('',#417804);
#41825=VERTEX_POINT('',#417806);
#41826=VERTEX_POINT('',#417824);
#41827=VERTEX_POINT('',#417841);
#41828=VERTEX_POINT('',#417843);
#41829=VERTEX_POINT('',#417845);
#41830=VERTEX_POINT('',#417863);
#41831=VERTEX_POINT('',#417880);
#41832=VERTEX_POINT('',#417882);
#41833=VERTEX_POINT('',#417884);
#41834=VERTEX_POINT('',#417902);
#41835=VERTEX_POINT('',#417919);
#41836=VERTEX_POINT('',#417921);
#41837=VERTEX_POINT('',#417923);
#41838=VERTEX_POINT('',#417941);
#41839=VERTEX_POINT('',#417958);
#41840=VERTEX_POINT('',#417960);
#41841=VERTEX_POINT('',#417962);
#41842=VERTEX_POINT('',#417980);
#41843=VERTEX_POINT('',#417997);
#41844=VERTEX_POINT('',#417999);
#41845=VERTEX_POINT('',#418001);
#41846=VERTEX_POINT('',#418019);
#41847=VERTEX_POINT('',#418036);
#41848=VERTEX_POINT('',#418038);
#41849=VERTEX_POINT('',#418040);
#41850=VERTEX_POINT('',#418058);
#41851=VERTEX_POINT('',#418075);
#41852=VERTEX_POINT('',#418077);
#41853=VERTEX_POINT('',#418079);
#41854=VERTEX_POINT('',#418097);
#41855=VERTEX_POINT('',#418114);
#41856=VERTEX_POINT('',#418116);
#41857=VERTEX_POINT('',#418118);
#41858=VERTEX_POINT('',#418136);
#41859=VERTEX_POINT('',#418153);
#41860=VERTEX_POINT('',#418155);
#41861=VERTEX_POINT('',#418157);
#41862=VERTEX_POINT('',#418175);
#41863=VERTEX_POINT('',#418192);
#41864=VERTEX_POINT('',#418194);
#41865=VERTEX_POINT('',#418196);
#41866=VERTEX_POINT('',#418214);
#41867=VERTEX_POINT('',#418231);
#41868=VERTEX_POINT('',#418233);
#41869=VERTEX_POINT('',#418235);
#41870=VERTEX_POINT('',#418254);
#41871=VERTEX_POINT('',#418271);
#41872=VERTEX_POINT('',#418273);
#41873=VERTEX_POINT('',#418275);
#41874=VERTEX_POINT('',#418293);
#41875=VERTEX_POINT('',#418310);
#41876=VERTEX_POINT('',#418312);
#41877=VERTEX_POINT('',#418314);
#41878=VERTEX_POINT('',#418332);
#41879=VERTEX_POINT('',#418349);
#41880=VERTEX_POINT('',#418351);
#41881=VERTEX_POINT('',#418353);
#41882=VERTEX_POINT('',#418371);
#41883=VERTEX_POINT('',#418388);
#41884=VERTEX_POINT('',#418390);
#41885=VERTEX_POINT('',#418392);
#41886=VERTEX_POINT('',#418410);
#41887=VERTEX_POINT('',#418427);
#41888=VERTEX_POINT('',#418429);
#41889=VERTEX_POINT('',#418431);
#41890=VERTEX_POINT('',#418449);
#41891=VERTEX_POINT('',#418466);
#41892=VERTEX_POINT('',#418468);
#41893=VERTEX_POINT('',#418470);
#41894=VERTEX_POINT('',#418488);
#41895=VERTEX_POINT('',#418505);
#41896=VERTEX_POINT('',#418507);
#41897=VERTEX_POINT('',#418509);
#41898=VERTEX_POINT('',#418527);
#41899=VERTEX_POINT('',#418544);
#41900=VERTEX_POINT('',#418546);
#41901=VERTEX_POINT('',#418548);
#41902=VERTEX_POINT('',#418566);
#41903=VERTEX_POINT('',#418583);
#41904=VERTEX_POINT('',#418585);
#41905=VERTEX_POINT('',#418587);
#41906=VERTEX_POINT('',#418605);
#41907=VERTEX_POINT('',#418622);
#41908=VERTEX_POINT('',#418624);
#41909=VERTEX_POINT('',#418626);
#41910=VERTEX_POINT('',#418644);
#41911=VERTEX_POINT('',#418661);
#41912=VERTEX_POINT('',#418663);
#41913=VERTEX_POINT('',#418665);
#41914=VERTEX_POINT('',#418683);
#41915=VERTEX_POINT('',#418700);
#41916=VERTEX_POINT('',#418702);
#41917=VERTEX_POINT('',#418704);
#41918=VERTEX_POINT('',#418722);
#41919=VERTEX_POINT('',#418739);
#41920=VERTEX_POINT('',#418741);
#41921=VERTEX_POINT('',#418743);
#41922=VERTEX_POINT('',#418761);
#41923=VERTEX_POINT('',#418778);
#41924=VERTEX_POINT('',#418780);
#41925=VERTEX_POINT('',#418782);
#41926=VERTEX_POINT('',#418800);
#41927=VERTEX_POINT('',#418817);
#41928=VERTEX_POINT('',#418819);
#41929=VERTEX_POINT('',#418821);
#41930=VERTEX_POINT('',#418839);
#41931=VERTEX_POINT('',#418856);
#41932=VERTEX_POINT('',#418858);
#41933=VERTEX_POINT('',#418860);
#41934=VERTEX_POINT('',#418878);
#41935=VERTEX_POINT('',#418895);
#41936=VERTEX_POINT('',#418897);
#41937=VERTEX_POINT('',#418899);
#41938=VERTEX_POINT('',#418917);
#41939=VERTEX_POINT('',#418934);
#41940=VERTEX_POINT('',#418936);
#41941=VERTEX_POINT('',#418938);
#41942=VERTEX_POINT('',#418956);
#41943=VERTEX_POINT('',#418973);
#41944=VERTEX_POINT('',#418975);
#41945=VERTEX_POINT('',#418977);
#41946=VERTEX_POINT('',#418995);
#41947=VERTEX_POINT('',#419012);
#41948=VERTEX_POINT('',#419014);
#41949=VERTEX_POINT('',#419016);
#41950=VERTEX_POINT('',#419034);
#41951=VERTEX_POINT('',#419051);
#41952=VERTEX_POINT('',#419053);
#41953=VERTEX_POINT('',#419055);
#41954=VERTEX_POINT('',#419073);
#41955=VERTEX_POINT('',#419090);
#41956=VERTEX_POINT('',#419092);
#41957=VERTEX_POINT('',#419094);
#41958=VERTEX_POINT('',#419112);
#41959=VERTEX_POINT('',#419129);
#41960=VERTEX_POINT('',#419131);
#41961=VERTEX_POINT('',#419133);
#41962=VERTEX_POINT('',#419151);
#41963=VERTEX_POINT('',#419168);
#41964=VERTEX_POINT('',#419170);
#41965=VERTEX_POINT('',#419172);
#41966=VERTEX_POINT('',#419190);
#41967=VERTEX_POINT('',#419207);
#41968=VERTEX_POINT('',#419209);
#41969=VERTEX_POINT('',#419211);
#41970=VERTEX_POINT('',#419229);
#41971=VERTEX_POINT('',#419246);
#41972=VERTEX_POINT('',#419248);
#41973=VERTEX_POINT('',#419250);
#41974=VERTEX_POINT('',#419268);
#41975=VERTEX_POINT('',#419285);
#41976=VERTEX_POINT('',#419287);
#41977=VERTEX_POINT('',#419289);
#41978=VERTEX_POINT('',#419307);
#41979=VERTEX_POINT('',#419324);
#41980=VERTEX_POINT('',#419326);
#41981=VERTEX_POINT('',#419328);
#41982=VERTEX_POINT('',#419346);
#41983=VERTEX_POINT('',#419363);
#41984=VERTEX_POINT('',#419365);
#41985=VERTEX_POINT('',#419367);
#41986=VERTEX_POINT('',#419385);
#41987=VERTEX_POINT('',#419402);
#41988=VERTEX_POINT('',#419404);
#41989=VERTEX_POINT('',#419406);
#41990=VERTEX_POINT('',#419424);
#41991=VERTEX_POINT('',#419441);
#41992=VERTEX_POINT('',#419443);
#41993=VERTEX_POINT('',#419445);
#41994=VERTEX_POINT('',#419463);
#41995=VERTEX_POINT('',#419480);
#41996=VERTEX_POINT('',#419482);
#41997=VERTEX_POINT('',#419484);
#41998=VERTEX_POINT('',#419502);
#41999=VERTEX_POINT('',#419519);
#42000=VERTEX_POINT('',#419521);
#42001=VERTEX_POINT('',#419523);
#42002=VERTEX_POINT('',#419541);
#42003=VERTEX_POINT('',#419558);
#42004=VERTEX_POINT('',#419560);
#42005=VERTEX_POINT('',#419562);
#42006=VERTEX_POINT('',#419580);
#42007=VERTEX_POINT('',#419597);
#42008=VERTEX_POINT('',#419599);
#42009=VERTEX_POINT('',#419601);
#42010=VERTEX_POINT('',#419619);
#42011=VERTEX_POINT('',#419636);
#42012=VERTEX_POINT('',#419638);
#42013=VERTEX_POINT('',#419640);
#42014=VERTEX_POINT('',#419658);
#42015=VERTEX_POINT('',#419675);
#42016=VERTEX_POINT('',#419677);
#42017=VERTEX_POINT('',#419679);
#42018=VERTEX_POINT('',#419697);
#42019=VERTEX_POINT('',#419714);
#42020=VERTEX_POINT('',#419716);
#42021=VERTEX_POINT('',#419718);
#42022=VERTEX_POINT('',#419736);
#42023=VERTEX_POINT('',#419983);
#42024=VERTEX_POINT('',#419984);
#42025=VERTEX_POINT('',#419986);
#42026=VERTEX_POINT('',#420024);
#42027=VERTEX_POINT('',#420053);
#42028=VERTEX_POINT('',#420055);
#42029=VERTEX_POINT('',#420059);
#42030=VERTEX_POINT('',#420060);
#42031=VERTEX_POINT('',#420063);
#42032=VERTEX_POINT('',#420070);
#42033=VERTEX_POINT('',#420072);
#42034=VERTEX_POINT('',#420074);
#42035=VERTEX_POINT('',#420082);
#42036=VERTEX_POINT('',#420086);
#42037=VERTEX_POINT('',#420090);
#42038=VERTEX_POINT('',#420094);
#42039=VERTEX_POINT('',#420098);
#42040=VERTEX_POINT('',#420102);
#42041=VERTEX_POINT('',#420103);
#42042=VERTEX_POINT('',#420106);
#42043=VERTEX_POINT('',#420108);
#42044=VERTEX_POINT('',#420119);
#42045=VERTEX_POINT('',#422617);
#42046=VERTEX_POINT('',#422618);
#42047=VERTEX_POINT('',#422868);
#42048=VERTEX_POINT('',#422869);
#42049=VERTEX_POINT('',#422871);
#42050=VERTEX_POINT('',#422873);
#42051=VERTEX_POINT('',#422875);
#42052=VERTEX_POINT('',#422882);
#42053=VERTEX_POINT('',#422883);
#42054=VERTEX_POINT('',#422885);
#42055=VERTEX_POINT('',#422887);
#42056=VERTEX_POINT('',#422889);
#42057=VERTEX_POINT('',#422896);
#42058=VERTEX_POINT('',#422962);
#42059=VERTEX_POINT('',#423005);
#42060=VERTEX_POINT('',#423032);
#42061=VERTEX_POINT('',#423217);
#42062=VERTEX_POINT('',#423218);
#42063=VERTEX_POINT('',#423220);
#42064=VERTEX_POINT('',#423222);
#42065=VERTEX_POINT('',#423224);
#42066=VERTEX_POINT('',#423231);
#42067=VERTEX_POINT('',#423232);
#42068=VERTEX_POINT('',#423234);
#42069=VERTEX_POINT('',#423236);
#42070=VERTEX_POINT('',#423238);
#42071=VERTEX_POINT('',#423245);
#42072=VERTEX_POINT('',#423311);
#42073=VERTEX_POINT('',#423354);
#42074=VERTEX_POINT('',#423381);
#42075=VERTEX_POINT('',#423566);
#42076=VERTEX_POINT('',#423567);
#42077=VERTEX_POINT('',#423569);
#42078=VERTEX_POINT('',#423571);
#42079=VERTEX_POINT('',#423573);
#42080=VERTEX_POINT('',#423580);
#42081=VERTEX_POINT('',#423581);
#42082=VERTEX_POINT('',#423583);
#42083=VERTEX_POINT('',#423585);
#42084=VERTEX_POINT('',#423587);
#42085=VERTEX_POINT('',#423594);
#42086=VERTEX_POINT('',#423660);
#42087=VERTEX_POINT('',#423703);
#42088=VERTEX_POINT('',#423730);
#42089=VERTEX_POINT('',#423915);
#42090=VERTEX_POINT('',#423916);
#42091=VERTEX_POINT('',#423918);
#42092=VERTEX_POINT('',#423920);
#42093=VERTEX_POINT('',#423922);
#42094=VERTEX_POINT('',#423929);
#42095=VERTEX_POINT('',#423930);
#42096=VERTEX_POINT('',#423932);
#42097=VERTEX_POINT('',#423934);
#42098=VERTEX_POINT('',#423936);
#42099=VERTEX_POINT('',#423943);
#42100=VERTEX_POINT('',#424009);
#42101=VERTEX_POINT('',#424052);
#42102=VERTEX_POINT('',#424079);
#42103=VERTEX_POINT('',#424264);
#42104=VERTEX_POINT('',#424265);
#42105=VERTEX_POINT('',#424267);
#42106=VERTEX_POINT('',#424269);
#42107=VERTEX_POINT('',#424271);
#42108=VERTEX_POINT('',#424278);
#42109=VERTEX_POINT('',#424279);
#42110=VERTEX_POINT('',#424281);
#42111=VERTEX_POINT('',#424283);
#42112=VERTEX_POINT('',#424285);
#42113=VERTEX_POINT('',#424292);
#42114=VERTEX_POINT('',#424358);
#42115=VERTEX_POINT('',#424401);
#42116=VERTEX_POINT('',#424428);
#42117=VERTEX_POINT('',#424613);
#42118=VERTEX_POINT('',#424614);
#42119=VERTEX_POINT('',#424616);
#42120=VERTEX_POINT('',#424618);
#42121=VERTEX_POINT('',#424620);
#42122=VERTEX_POINT('',#424627);
#42123=VERTEX_POINT('',#424628);
#42124=VERTEX_POINT('',#424630);
#42125=VERTEX_POINT('',#424632);
#42126=VERTEX_POINT('',#424634);
#42127=VERTEX_POINT('',#424641);
#42128=VERTEX_POINT('',#424707);
#42129=VERTEX_POINT('',#424750);
#42130=VERTEX_POINT('',#424777);
#42131=VERTEX_POINT('',#424962);
#42132=VERTEX_POINT('',#424963);
#42133=VERTEX_POINT('',#424965);
#42134=VERTEX_POINT('',#424967);
#42135=VERTEX_POINT('',#424969);
#42136=VERTEX_POINT('',#424976);
#42137=VERTEX_POINT('',#424977);
#42138=VERTEX_POINT('',#424979);
#42139=VERTEX_POINT('',#424981);
#42140=VERTEX_POINT('',#424983);
#42141=VERTEX_POINT('',#424990);
#42142=VERTEX_POINT('',#425056);
#42143=VERTEX_POINT('',#425099);
#42144=VERTEX_POINT('',#425126);
#42145=VERTEX_POINT('',#425311);
#42146=VERTEX_POINT('',#425312);
#42147=VERTEX_POINT('',#425314);
#42148=VERTEX_POINT('',#425316);
#42149=VERTEX_POINT('',#425318);
#42150=VERTEX_POINT('',#425325);
#42151=VERTEX_POINT('',#425326);
#42152=VERTEX_POINT('',#425328);
#42153=VERTEX_POINT('',#425330);
#42154=VERTEX_POINT('',#425332);
#42155=VERTEX_POINT('',#425339);
#42156=VERTEX_POINT('',#425405);
#42157=VERTEX_POINT('',#425448);
#42158=VERTEX_POINT('',#425475);
#42159=VERTEX_POINT('',#425660);
#42160=VERTEX_POINT('',#425661);
#42161=VERTEX_POINT('',#425663);
#42162=VERTEX_POINT('',#425665);
#42163=VERTEX_POINT('',#425667);
#42164=VERTEX_POINT('',#425674);
#42165=VERTEX_POINT('',#425675);
#42166=VERTEX_POINT('',#425677);
#42167=VERTEX_POINT('',#425679);
#42168=VERTEX_POINT('',#425681);
#42169=VERTEX_POINT('',#425688);
#42170=VERTEX_POINT('',#425754);
#42171=VERTEX_POINT('',#425797);
#42172=VERTEX_POINT('',#425824);
#42173=VERTEX_POINT('',#426009);
#42174=VERTEX_POINT('',#426010);
#42175=VERTEX_POINT('',#426012);
#42176=VERTEX_POINT('',#426014);
#42177=VERTEX_POINT('',#426016);
#42178=VERTEX_POINT('',#426023);
#42179=VERTEX_POINT('',#426024);
#42180=VERTEX_POINT('',#426026);
#42181=VERTEX_POINT('',#426028);
#42182=VERTEX_POINT('',#426030);
#42183=VERTEX_POINT('',#426037);
#42184=VERTEX_POINT('',#426103);
#42185=VERTEX_POINT('',#426146);
#42186=VERTEX_POINT('',#426173);
#42187=VERTEX_POINT('',#426358);
#42188=VERTEX_POINT('',#426359);
#42189=VERTEX_POINT('',#426361);
#42190=VERTEX_POINT('',#426363);
#42191=VERTEX_POINT('',#426365);
#42192=VERTEX_POINT('',#426372);
#42193=VERTEX_POINT('',#426373);
#42194=VERTEX_POINT('',#426375);
#42195=VERTEX_POINT('',#426377);
#42196=VERTEX_POINT('',#426379);
#42197=VERTEX_POINT('',#426386);
#42198=VERTEX_POINT('',#426452);
#42199=VERTEX_POINT('',#426495);
#42200=VERTEX_POINT('',#426522);
#42201=VERTEX_POINT('',#426707);
#42202=VERTEX_POINT('',#426708);
#42203=VERTEX_POINT('',#426710);
#42204=VERTEX_POINT('',#426712);
#42205=VERTEX_POINT('',#426714);
#42206=VERTEX_POINT('',#426721);
#42207=VERTEX_POINT('',#426722);
#42208=VERTEX_POINT('',#426724);
#42209=VERTEX_POINT('',#426726);
#42210=VERTEX_POINT('',#426728);
#42211=VERTEX_POINT('',#426735);
#42212=VERTEX_POINT('',#426801);
#42213=VERTEX_POINT('',#426844);
#42214=VERTEX_POINT('',#426871);
#42215=VERTEX_POINT('',#427056);
#42216=VERTEX_POINT('',#427057);
#42217=VERTEX_POINT('',#427059);
#42218=VERTEX_POINT('',#427061);
#42219=VERTEX_POINT('',#427063);
#42220=VERTEX_POINT('',#427070);
#42221=VERTEX_POINT('',#427071);
#42222=VERTEX_POINT('',#427073);
#42223=VERTEX_POINT('',#427075);
#42224=VERTEX_POINT('',#427077);
#42225=VERTEX_POINT('',#427084);
#42226=VERTEX_POINT('',#427150);
#42227=VERTEX_POINT('',#427193);
#42228=VERTEX_POINT('',#427220);
#42229=VERTEX_POINT('',#427405);
#42230=VERTEX_POINT('',#427406);
#42231=VERTEX_POINT('',#427408);
#42232=VERTEX_POINT('',#427410);
#42233=VERTEX_POINT('',#427412);
#42234=VERTEX_POINT('',#427419);
#42235=VERTEX_POINT('',#427420);
#42236=VERTEX_POINT('',#427422);
#42237=VERTEX_POINT('',#427424);
#42238=VERTEX_POINT('',#427426);
#42239=VERTEX_POINT('',#427433);
#42240=VERTEX_POINT('',#427499);
#42241=VERTEX_POINT('',#427542);
#42242=VERTEX_POINT('',#427569);
#42243=VERTEX_POINT('',#427754);
#42244=VERTEX_POINT('',#427755);
#42245=VERTEX_POINT('',#427757);
#42246=VERTEX_POINT('',#427759);
#42247=VERTEX_POINT('',#427761);
#42248=VERTEX_POINT('',#427768);
#42249=VERTEX_POINT('',#427769);
#42250=VERTEX_POINT('',#427771);
#42251=VERTEX_POINT('',#427773);
#42252=VERTEX_POINT('',#427775);
#42253=VERTEX_POINT('',#427782);
#42254=VERTEX_POINT('',#427848);
#42255=VERTEX_POINT('',#427891);
#42256=VERTEX_POINT('',#427918);
#42257=VERTEX_POINT('',#428103);
#42258=VERTEX_POINT('',#428104);
#42259=VERTEX_POINT('',#428106);
#42260=VERTEX_POINT('',#428108);
#42261=VERTEX_POINT('',#428110);
#42262=VERTEX_POINT('',#428117);
#42263=VERTEX_POINT('',#428118);
#42264=VERTEX_POINT('',#428120);
#42265=VERTEX_POINT('',#428122);
#42266=VERTEX_POINT('',#428124);
#42267=VERTEX_POINT('',#428131);
#42268=VERTEX_POINT('',#428197);
#42269=VERTEX_POINT('',#428240);
#42270=VERTEX_POINT('',#428267);
#42271=VERTEX_POINT('',#428452);
#42272=VERTEX_POINT('',#428453);
#42273=VERTEX_POINT('',#428455);
#42274=VERTEX_POINT('',#428457);
#42275=VERTEX_POINT('',#428459);
#42276=VERTEX_POINT('',#428466);
#42277=VERTEX_POINT('',#428467);
#42278=VERTEX_POINT('',#428469);
#42279=VERTEX_POINT('',#428471);
#42280=VERTEX_POINT('',#428473);
#42281=VERTEX_POINT('',#428480);
#42282=VERTEX_POINT('',#428546);
#42283=VERTEX_POINT('',#428589);
#42284=VERTEX_POINT('',#428616);
#42285=VERTEX_POINT('',#428801);
#42286=VERTEX_POINT('',#428802);
#42287=VERTEX_POINT('',#428804);
#42288=VERTEX_POINT('',#428806);
#42289=VERTEX_POINT('',#428808);
#42290=VERTEX_POINT('',#428815);
#42291=VERTEX_POINT('',#428816);
#42292=VERTEX_POINT('',#428818);
#42293=VERTEX_POINT('',#428820);
#42294=VERTEX_POINT('',#428822);
#42295=VERTEX_POINT('',#428829);
#42296=VERTEX_POINT('',#428895);
#42297=VERTEX_POINT('',#428938);
#42298=VERTEX_POINT('',#428965);
#42299=VERTEX_POINT('',#429150);
#42300=VERTEX_POINT('',#429151);
#42301=VERTEX_POINT('',#429153);
#42302=VERTEX_POINT('',#429155);
#42303=VERTEX_POINT('',#429157);
#42304=VERTEX_POINT('',#429164);
#42305=VERTEX_POINT('',#429165);
#42306=VERTEX_POINT('',#429167);
#42307=VERTEX_POINT('',#429169);
#42308=VERTEX_POINT('',#429171);
#42309=VERTEX_POINT('',#429178);
#42310=VERTEX_POINT('',#429244);
#42311=VERTEX_POINT('',#429287);
#42312=VERTEX_POINT('',#429314);
#42313=VERTEX_POINT('',#429499);
#42314=VERTEX_POINT('',#429500);
#42315=VERTEX_POINT('',#429502);
#42316=VERTEX_POINT('',#429504);
#42317=VERTEX_POINT('',#429506);
#42318=VERTEX_POINT('',#429513);
#42319=VERTEX_POINT('',#429514);
#42320=VERTEX_POINT('',#429516);
#42321=VERTEX_POINT('',#429518);
#42322=VERTEX_POINT('',#429520);
#42323=VERTEX_POINT('',#429527);
#42324=VERTEX_POINT('',#429593);
#42325=VERTEX_POINT('',#429636);
#42326=VERTEX_POINT('',#429663);
#42327=VERTEX_POINT('',#429848);
#42328=VERTEX_POINT('',#429849);
#42329=VERTEX_POINT('',#429851);
#42330=VERTEX_POINT('',#429853);
#42331=VERTEX_POINT('',#429855);
#42332=VERTEX_POINT('',#429862);
#42333=VERTEX_POINT('',#429863);
#42334=VERTEX_POINT('',#429865);
#42335=VERTEX_POINT('',#429867);
#42336=VERTEX_POINT('',#429869);
#42337=VERTEX_POINT('',#429876);
#42338=VERTEX_POINT('',#429942);
#42339=VERTEX_POINT('',#429985);
#42340=VERTEX_POINT('',#430012);
#42341=VERTEX_POINT('',#430197);
#42342=VERTEX_POINT('',#430198);
#42343=VERTEX_POINT('',#430200);
#42344=VERTEX_POINT('',#430202);
#42345=VERTEX_POINT('',#430204);
#42346=VERTEX_POINT('',#430211);
#42347=VERTEX_POINT('',#430212);
#42348=VERTEX_POINT('',#430214);
#42349=VERTEX_POINT('',#430216);
#42350=VERTEX_POINT('',#430218);
#42351=VERTEX_POINT('',#430225);
#42352=VERTEX_POINT('',#430291);
#42353=VERTEX_POINT('',#430334);
#42354=VERTEX_POINT('',#430361);
#42355=VERTEX_POINT('',#430546);
#42356=VERTEX_POINT('',#430547);
#42357=VERTEX_POINT('',#430549);
#42358=VERTEX_POINT('',#430551);
#42359=VERTEX_POINT('',#430553);
#42360=VERTEX_POINT('',#430560);
#42361=VERTEX_POINT('',#430561);
#42362=VERTEX_POINT('',#430563);
#42363=VERTEX_POINT('',#430565);
#42364=VERTEX_POINT('',#430567);
#42365=VERTEX_POINT('',#430574);
#42366=VERTEX_POINT('',#430640);
#42367=VERTEX_POINT('',#430683);
#42368=VERTEX_POINT('',#430710);
#42369=VERTEX_POINT('',#430895);
#42370=VERTEX_POINT('',#430896);
#42371=VERTEX_POINT('',#430898);
#42372=VERTEX_POINT('',#430900);
#42373=VERTEX_POINT('',#430902);
#42374=VERTEX_POINT('',#430909);
#42375=VERTEX_POINT('',#430910);
#42376=VERTEX_POINT('',#430912);
#42377=VERTEX_POINT('',#430914);
#42378=VERTEX_POINT('',#430916);
#42379=VERTEX_POINT('',#430923);
#42380=VERTEX_POINT('',#430989);
#42381=VERTEX_POINT('',#431032);
#42382=VERTEX_POINT('',#431059);
#42383=VERTEX_POINT('',#431244);
#42384=VERTEX_POINT('',#431245);
#42385=VERTEX_POINT('',#431247);
#42386=VERTEX_POINT('',#431249);
#42387=VERTEX_POINT('',#431251);
#42388=VERTEX_POINT('',#431258);
#42389=VERTEX_POINT('',#431259);
#42390=VERTEX_POINT('',#431261);
#42391=VERTEX_POINT('',#431263);
#42392=VERTEX_POINT('',#431265);
#42393=VERTEX_POINT('',#431272);
#42394=VERTEX_POINT('',#431338);
#42395=VERTEX_POINT('',#431381);
#42396=VERTEX_POINT('',#431408);
#42397=VERTEX_POINT('',#431593);
#42398=VERTEX_POINT('',#431594);
#42399=VERTEX_POINT('',#431596);
#42400=VERTEX_POINT('',#431598);
#42401=VERTEX_POINT('',#431600);
#42402=VERTEX_POINT('',#431607);
#42403=VERTEX_POINT('',#431608);
#42404=VERTEX_POINT('',#431610);
#42405=VERTEX_POINT('',#431612);
#42406=VERTEX_POINT('',#431614);
#42407=VERTEX_POINT('',#431621);
#42408=VERTEX_POINT('',#431687);
#42409=VERTEX_POINT('',#431730);
#42410=VERTEX_POINT('',#431757);
#42411=VERTEX_POINT('',#431942);
#42412=VERTEX_POINT('',#431943);
#42413=VERTEX_POINT('',#431945);
#42414=VERTEX_POINT('',#431947);
#42415=VERTEX_POINT('',#431949);
#42416=VERTEX_POINT('',#431956);
#42417=VERTEX_POINT('',#431957);
#42418=VERTEX_POINT('',#431959);
#42419=VERTEX_POINT('',#431961);
#42420=VERTEX_POINT('',#431963);
#42421=VERTEX_POINT('',#431970);
#42422=VERTEX_POINT('',#432036);
#42423=VERTEX_POINT('',#432079);
#42424=VERTEX_POINT('',#432106);
#42425=VERTEX_POINT('',#432291);
#42426=VERTEX_POINT('',#432292);
#42427=VERTEX_POINT('',#432294);
#42428=VERTEX_POINT('',#432296);
#42429=VERTEX_POINT('',#432298);
#42430=VERTEX_POINT('',#432305);
#42431=VERTEX_POINT('',#432306);
#42432=VERTEX_POINT('',#432308);
#42433=VERTEX_POINT('',#432310);
#42434=VERTEX_POINT('',#432312);
#42435=VERTEX_POINT('',#432319);
#42436=VERTEX_POINT('',#432385);
#42437=VERTEX_POINT('',#432428);
#42438=VERTEX_POINT('',#432455);
#42439=VERTEX_POINT('',#432640);
#42440=VERTEX_POINT('',#432641);
#42441=VERTEX_POINT('',#432643);
#42442=VERTEX_POINT('',#432645);
#42443=VERTEX_POINT('',#432647);
#42444=VERTEX_POINT('',#432654);
#42445=VERTEX_POINT('',#432655);
#42446=VERTEX_POINT('',#432657);
#42447=VERTEX_POINT('',#432659);
#42448=VERTEX_POINT('',#432661);
#42449=VERTEX_POINT('',#432668);
#42450=VERTEX_POINT('',#432734);
#42451=VERTEX_POINT('',#432777);
#42452=VERTEX_POINT('',#432804);
#42453=VERTEX_POINT('',#432989);
#42454=VERTEX_POINT('',#432990);
#42455=VERTEX_POINT('',#432992);
#42456=VERTEX_POINT('',#432994);
#42457=VERTEX_POINT('',#432996);
#42458=VERTEX_POINT('',#433003);
#42459=VERTEX_POINT('',#433004);
#42460=VERTEX_POINT('',#433006);
#42461=VERTEX_POINT('',#433008);
#42462=VERTEX_POINT('',#433010);
#42463=VERTEX_POINT('',#433017);
#42464=VERTEX_POINT('',#433083);
#42465=VERTEX_POINT('',#433126);
#42466=VERTEX_POINT('',#433153);
#42467=VERTEX_POINT('',#433338);
#42468=VERTEX_POINT('',#433339);
#42469=VERTEX_POINT('',#433341);
#42470=VERTEX_POINT('',#433343);
#42471=VERTEX_POINT('',#433345);
#42472=VERTEX_POINT('',#433352);
#42473=VERTEX_POINT('',#433353);
#42474=VERTEX_POINT('',#433355);
#42475=VERTEX_POINT('',#433357);
#42476=VERTEX_POINT('',#433359);
#42477=VERTEX_POINT('',#433366);
#42478=VERTEX_POINT('',#433432);
#42479=VERTEX_POINT('',#433475);
#42480=VERTEX_POINT('',#433502);
#42481=VERTEX_POINT('',#433687);
#42482=VERTEX_POINT('',#433688);
#42483=VERTEX_POINT('',#433690);
#42484=VERTEX_POINT('',#433692);
#42485=VERTEX_POINT('',#433694);
#42486=VERTEX_POINT('',#433701);
#42487=VERTEX_POINT('',#433702);
#42488=VERTEX_POINT('',#433704);
#42489=VERTEX_POINT('',#433706);
#42490=VERTEX_POINT('',#433708);
#42491=VERTEX_POINT('',#433715);
#42492=VERTEX_POINT('',#433781);
#42493=VERTEX_POINT('',#433824);
#42494=VERTEX_POINT('',#433851);
#42495=VERTEX_POINT('',#434036);
#42496=VERTEX_POINT('',#434037);
#42497=VERTEX_POINT('',#434039);
#42498=VERTEX_POINT('',#434041);
#42499=VERTEX_POINT('',#434043);
#42500=VERTEX_POINT('',#434050);
#42501=VERTEX_POINT('',#434051);
#42502=VERTEX_POINT('',#434053);
#42503=VERTEX_POINT('',#434055);
#42504=VERTEX_POINT('',#434057);
#42505=VERTEX_POINT('',#434064);
#42506=VERTEX_POINT('',#434130);
#42507=VERTEX_POINT('',#434173);
#42508=VERTEX_POINT('',#434200);
#42509=VERTEX_POINT('',#434385);
#42510=VERTEX_POINT('',#434386);
#42511=VERTEX_POINT('',#434388);
#42512=VERTEX_POINT('',#434390);
#42513=VERTEX_POINT('',#434392);
#42514=VERTEX_POINT('',#434399);
#42515=VERTEX_POINT('',#434400);
#42516=VERTEX_POINT('',#434402);
#42517=VERTEX_POINT('',#434404);
#42518=VERTEX_POINT('',#434406);
#42519=VERTEX_POINT('',#434413);
#42520=VERTEX_POINT('',#434479);
#42521=VERTEX_POINT('',#434522);
#42522=VERTEX_POINT('',#434549);
#42523=VERTEX_POINT('',#434734);
#42524=VERTEX_POINT('',#434735);
#42525=VERTEX_POINT('',#434737);
#42526=VERTEX_POINT('',#434739);
#42527=VERTEX_POINT('',#434741);
#42528=VERTEX_POINT('',#434748);
#42529=VERTEX_POINT('',#434749);
#42530=VERTEX_POINT('',#434751);
#42531=VERTEX_POINT('',#434753);
#42532=VERTEX_POINT('',#434755);
#42533=VERTEX_POINT('',#434762);
#42534=VERTEX_POINT('',#434828);
#42535=VERTEX_POINT('',#434871);
#42536=VERTEX_POINT('',#434898);
#42537=VERTEX_POINT('',#435083);
#42538=VERTEX_POINT('',#435084);
#42539=VERTEX_POINT('',#435086);
#42540=VERTEX_POINT('',#435088);
#42541=VERTEX_POINT('',#435090);
#42542=VERTEX_POINT('',#435097);
#42543=VERTEX_POINT('',#435098);
#42544=VERTEX_POINT('',#435100);
#42545=VERTEX_POINT('',#435102);
#42546=VERTEX_POINT('',#435104);
#42547=VERTEX_POINT('',#435111);
#42548=VERTEX_POINT('',#435177);
#42549=VERTEX_POINT('',#435220);
#42550=VERTEX_POINT('',#435247);
#42551=VERTEX_POINT('',#435432);
#42552=VERTEX_POINT('',#435433);
#42553=VERTEX_POINT('',#435435);
#42554=VERTEX_POINT('',#435437);
#42555=VERTEX_POINT('',#435439);
#42556=VERTEX_POINT('',#435446);
#42557=VERTEX_POINT('',#435447);
#42558=VERTEX_POINT('',#435449);
#42559=VERTEX_POINT('',#435451);
#42560=VERTEX_POINT('',#435453);
#42561=VERTEX_POINT('',#435460);
#42562=VERTEX_POINT('',#435526);
#42563=VERTEX_POINT('',#435569);
#42564=VERTEX_POINT('',#435596);
#42565=VERTEX_POINT('',#435781);
#42566=VERTEX_POINT('',#435782);
#42567=VERTEX_POINT('',#435784);
#42568=VERTEX_POINT('',#435786);
#42569=VERTEX_POINT('',#435788);
#42570=VERTEX_POINT('',#435795);
#42571=VERTEX_POINT('',#435796);
#42572=VERTEX_POINT('',#435798);
#42573=VERTEX_POINT('',#435800);
#42574=VERTEX_POINT('',#435802);
#42575=VERTEX_POINT('',#435809);
#42576=VERTEX_POINT('',#435875);
#42577=VERTEX_POINT('',#435918);
#42578=VERTEX_POINT('',#435945);
#42579=VERTEX_POINT('',#436130);
#42580=VERTEX_POINT('',#436131);
#42581=VERTEX_POINT('',#436133);
#42582=VERTEX_POINT('',#436135);
#42583=VERTEX_POINT('',#436137);
#42584=VERTEX_POINT('',#436144);
#42585=VERTEX_POINT('',#436145);
#42586=VERTEX_POINT('',#436147);
#42587=VERTEX_POINT('',#436149);
#42588=VERTEX_POINT('',#436151);
#42589=VERTEX_POINT('',#436158);
#42590=VERTEX_POINT('',#436224);
#42591=VERTEX_POINT('',#436267);
#42592=VERTEX_POINT('',#436294);
#42593=VERTEX_POINT('',#436479);
#42594=VERTEX_POINT('',#436480);
#42595=VERTEX_POINT('',#436482);
#42596=VERTEX_POINT('',#436484);
#42597=VERTEX_POINT('',#436486);
#42598=VERTEX_POINT('',#436493);
#42599=VERTEX_POINT('',#436494);
#42600=VERTEX_POINT('',#436496);
#42601=VERTEX_POINT('',#436498);
#42602=VERTEX_POINT('',#436500);
#42603=VERTEX_POINT('',#436507);
#42604=VERTEX_POINT('',#436573);
#42605=VERTEX_POINT('',#436616);
#42606=VERTEX_POINT('',#436643);
#42607=VERTEX_POINT('',#436828);
#42608=VERTEX_POINT('',#436829);
#42609=VERTEX_POINT('',#436831);
#42610=VERTEX_POINT('',#436833);
#42611=VERTEX_POINT('',#436835);
#42612=VERTEX_POINT('',#436842);
#42613=VERTEX_POINT('',#436843);
#42614=VERTEX_POINT('',#436845);
#42615=VERTEX_POINT('',#436847);
#42616=VERTEX_POINT('',#436849);
#42617=VERTEX_POINT('',#436856);
#42618=VERTEX_POINT('',#436922);
#42619=VERTEX_POINT('',#436965);
#42620=VERTEX_POINT('',#436992);
#42621=VERTEX_POINT('',#437177);
#42622=VERTEX_POINT('',#437178);
#42623=VERTEX_POINT('',#437180);
#42624=VERTEX_POINT('',#437182);
#42625=VERTEX_POINT('',#437184);
#42626=VERTEX_POINT('',#437191);
#42627=VERTEX_POINT('',#437192);
#42628=VERTEX_POINT('',#437194);
#42629=VERTEX_POINT('',#437196);
#42630=VERTEX_POINT('',#437198);
#42631=VERTEX_POINT('',#437205);
#42632=VERTEX_POINT('',#437271);
#42633=VERTEX_POINT('',#437314);
#42634=VERTEX_POINT('',#437341);
#42635=VERTEX_POINT('',#437526);
#42636=VERTEX_POINT('',#437527);
#42637=VERTEX_POINT('',#437529);
#42638=VERTEX_POINT('',#437531);
#42639=VERTEX_POINT('',#437533);
#42640=VERTEX_POINT('',#437540);
#42641=VERTEX_POINT('',#437541);
#42642=VERTEX_POINT('',#437543);
#42643=VERTEX_POINT('',#437545);
#42644=VERTEX_POINT('',#437547);
#42645=VERTEX_POINT('',#437554);
#42646=VERTEX_POINT('',#437620);
#42647=VERTEX_POINT('',#437663);
#42648=VERTEX_POINT('',#437690);
#42649=VERTEX_POINT('',#437875);
#42650=VERTEX_POINT('',#437876);
#42651=VERTEX_POINT('',#437878);
#42652=VERTEX_POINT('',#437880);
#42653=VERTEX_POINT('',#437882);
#42654=VERTEX_POINT('',#437889);
#42655=VERTEX_POINT('',#437890);
#42656=VERTEX_POINT('',#437892);
#42657=VERTEX_POINT('',#437894);
#42658=VERTEX_POINT('',#437896);
#42659=VERTEX_POINT('',#437903);
#42660=VERTEX_POINT('',#437969);
#42661=VERTEX_POINT('',#438012);
#42662=VERTEX_POINT('',#438039);
#42663=VERTEX_POINT('',#438224);
#42664=VERTEX_POINT('',#438225);
#42665=VERTEX_POINT('',#438227);
#42666=VERTEX_POINT('',#438229);
#42667=VERTEX_POINT('',#438231);
#42668=VERTEX_POINT('',#438238);
#42669=VERTEX_POINT('',#438239);
#42670=VERTEX_POINT('',#438241);
#42671=VERTEX_POINT('',#438243);
#42672=VERTEX_POINT('',#438245);
#42673=VERTEX_POINT('',#438252);
#42674=VERTEX_POINT('',#438318);
#42675=VERTEX_POINT('',#438361);
#42676=VERTEX_POINT('',#438388);
#42677=VERTEX_POINT('',#438573);
#42678=VERTEX_POINT('',#438574);
#42679=VERTEX_POINT('',#438576);
#42680=VERTEX_POINT('',#438578);
#42681=VERTEX_POINT('',#438580);
#42682=VERTEX_POINT('',#438587);
#42683=VERTEX_POINT('',#438588);
#42684=VERTEX_POINT('',#438590);
#42685=VERTEX_POINT('',#438592);
#42686=VERTEX_POINT('',#438594);
#42687=VERTEX_POINT('',#438601);
#42688=VERTEX_POINT('',#438667);
#42689=VERTEX_POINT('',#438710);
#42690=VERTEX_POINT('',#438737);
#42691=VERTEX_POINT('',#438922);
#42692=VERTEX_POINT('',#438923);
#42693=VERTEX_POINT('',#438925);
#42694=VERTEX_POINT('',#438927);
#42695=VERTEX_POINT('',#438929);
#42696=VERTEX_POINT('',#438936);
#42697=VERTEX_POINT('',#438937);
#42698=VERTEX_POINT('',#438939);
#42699=VERTEX_POINT('',#438941);
#42700=VERTEX_POINT('',#438943);
#42701=VERTEX_POINT('',#438950);
#42702=VERTEX_POINT('',#439016);
#42703=VERTEX_POINT('',#439059);
#42704=VERTEX_POINT('',#439086);
#42705=VERTEX_POINT('',#439271);
#42706=VERTEX_POINT('',#439272);
#42707=VERTEX_POINT('',#439274);
#42708=VERTEX_POINT('',#439276);
#42709=VERTEX_POINT('',#439278);
#42710=VERTEX_POINT('',#439285);
#42711=VERTEX_POINT('',#439286);
#42712=VERTEX_POINT('',#439288);
#42713=VERTEX_POINT('',#439290);
#42714=VERTEX_POINT('',#439292);
#42715=VERTEX_POINT('',#439299);
#42716=VERTEX_POINT('',#439365);
#42717=VERTEX_POINT('',#439408);
#42718=VERTEX_POINT('',#439435);
#42719=VERTEX_POINT('',#439620);
#42720=VERTEX_POINT('',#439621);
#42721=VERTEX_POINT('',#439623);
#42722=VERTEX_POINT('',#439625);
#42723=VERTEX_POINT('',#439627);
#42724=VERTEX_POINT('',#439634);
#42725=VERTEX_POINT('',#439635);
#42726=VERTEX_POINT('',#439637);
#42727=VERTEX_POINT('',#439639);
#42728=VERTEX_POINT('',#439641);
#42729=VERTEX_POINT('',#439648);
#42730=VERTEX_POINT('',#439714);
#42731=VERTEX_POINT('',#439757);
#42732=VERTEX_POINT('',#439784);
#42733=VERTEX_POINT('',#439969);
#42734=VERTEX_POINT('',#439970);
#42735=VERTEX_POINT('',#439972);
#42736=VERTEX_POINT('',#439974);
#42737=VERTEX_POINT('',#439976);
#42738=VERTEX_POINT('',#439983);
#42739=VERTEX_POINT('',#439984);
#42740=VERTEX_POINT('',#439986);
#42741=VERTEX_POINT('',#439988);
#42742=VERTEX_POINT('',#439990);
#42743=VERTEX_POINT('',#439997);
#42744=VERTEX_POINT('',#440063);
#42745=VERTEX_POINT('',#440106);
#42746=VERTEX_POINT('',#440133);
#42747=VERTEX_POINT('',#440318);
#42748=VERTEX_POINT('',#440319);
#42749=VERTEX_POINT('',#440321);
#42750=VERTEX_POINT('',#440323);
#42751=VERTEX_POINT('',#440325);
#42752=VERTEX_POINT('',#440332);
#42753=VERTEX_POINT('',#440333);
#42754=VERTEX_POINT('',#440335);
#42755=VERTEX_POINT('',#440337);
#42756=VERTEX_POINT('',#440339);
#42757=VERTEX_POINT('',#440346);
#42758=VERTEX_POINT('',#440412);
#42759=VERTEX_POINT('',#440455);
#42760=VERTEX_POINT('',#440482);
#42761=VERTEX_POINT('',#440667);
#42762=VERTEX_POINT('',#440668);
#42763=VERTEX_POINT('',#440670);
#42764=VERTEX_POINT('',#440672);
#42765=VERTEX_POINT('',#440674);
#42766=VERTEX_POINT('',#440681);
#42767=VERTEX_POINT('',#440682);
#42768=VERTEX_POINT('',#440684);
#42769=VERTEX_POINT('',#440686);
#42770=VERTEX_POINT('',#440688);
#42771=VERTEX_POINT('',#440695);
#42772=VERTEX_POINT('',#440761);
#42773=VERTEX_POINT('',#440804);
#42774=VERTEX_POINT('',#440831);
#42775=VERTEX_POINT('',#441016);
#42776=VERTEX_POINT('',#441017);
#42777=VERTEX_POINT('',#441019);
#42778=VERTEX_POINT('',#441021);
#42779=VERTEX_POINT('',#441023);
#42780=VERTEX_POINT('',#441030);
#42781=VERTEX_POINT('',#441031);
#42782=VERTEX_POINT('',#441033);
#42783=VERTEX_POINT('',#441035);
#42784=VERTEX_POINT('',#441037);
#42785=VERTEX_POINT('',#441044);
#42786=VERTEX_POINT('',#441110);
#42787=VERTEX_POINT('',#441153);
#42788=VERTEX_POINT('',#441180);
#42789=VERTEX_POINT('',#441365);
#42790=VERTEX_POINT('',#441366);
#42791=VERTEX_POINT('',#441368);
#42792=VERTEX_POINT('',#441370);
#42793=VERTEX_POINT('',#441372);
#42794=VERTEX_POINT('',#441379);
#42795=VERTEX_POINT('',#441380);
#42796=VERTEX_POINT('',#441382);
#42797=VERTEX_POINT('',#441384);
#42798=VERTEX_POINT('',#441386);
#42799=VERTEX_POINT('',#441393);
#42800=VERTEX_POINT('',#441459);
#42801=VERTEX_POINT('',#441502);
#42802=VERTEX_POINT('',#441529);
#42803=VERTEX_POINT('',#441714);
#42804=VERTEX_POINT('',#441715);
#42805=VERTEX_POINT('',#441717);
#42806=VERTEX_POINT('',#441719);
#42807=VERTEX_POINT('',#441721);
#42808=VERTEX_POINT('',#441728);
#42809=VERTEX_POINT('',#441729);
#42810=VERTEX_POINT('',#441731);
#42811=VERTEX_POINT('',#441733);
#42812=VERTEX_POINT('',#441735);
#42813=VERTEX_POINT('',#441742);
#42814=VERTEX_POINT('',#441808);
#42815=VERTEX_POINT('',#441851);
#42816=VERTEX_POINT('',#441878);
#42817=VERTEX_POINT('',#442063);
#42818=VERTEX_POINT('',#442064);
#42819=VERTEX_POINT('',#442066);
#42820=VERTEX_POINT('',#442068);
#42821=VERTEX_POINT('',#442070);
#42822=VERTEX_POINT('',#442077);
#42823=VERTEX_POINT('',#442078);
#42824=VERTEX_POINT('',#442080);
#42825=VERTEX_POINT('',#442082);
#42826=VERTEX_POINT('',#442084);
#42827=VERTEX_POINT('',#442091);
#42828=VERTEX_POINT('',#442157);
#42829=VERTEX_POINT('',#442200);
#42830=VERTEX_POINT('',#442227);
#42831=VERTEX_POINT('',#442412);
#42832=VERTEX_POINT('',#442413);
#42833=VERTEX_POINT('',#442415);
#42834=VERTEX_POINT('',#442417);
#42835=VERTEX_POINT('',#442419);
#42836=VERTEX_POINT('',#442426);
#42837=VERTEX_POINT('',#442427);
#42838=VERTEX_POINT('',#442429);
#42839=VERTEX_POINT('',#442431);
#42840=VERTEX_POINT('',#442433);
#42841=VERTEX_POINT('',#442440);
#42842=VERTEX_POINT('',#442506);
#42843=VERTEX_POINT('',#442549);
#42844=VERTEX_POINT('',#442576);
#42845=VERTEX_POINT('',#442761);
#42846=VERTEX_POINT('',#442762);
#42847=VERTEX_POINT('',#442764);
#42848=VERTEX_POINT('',#442766);
#42849=VERTEX_POINT('',#442768);
#42850=VERTEX_POINT('',#442775);
#42851=VERTEX_POINT('',#442776);
#42852=VERTEX_POINT('',#442778);
#42853=VERTEX_POINT('',#442780);
#42854=VERTEX_POINT('',#442782);
#42855=VERTEX_POINT('',#442789);
#42856=VERTEX_POINT('',#442855);
#42857=VERTEX_POINT('',#442898);
#42858=VERTEX_POINT('',#442925);
#42859=VERTEX_POINT('',#443110);
#42860=VERTEX_POINT('',#443111);
#42861=VERTEX_POINT('',#443113);
#42862=VERTEX_POINT('',#443115);
#42863=VERTEX_POINT('',#443117);
#42864=VERTEX_POINT('',#443124);
#42865=VERTEX_POINT('',#443125);
#42866=VERTEX_POINT('',#443127);
#42867=VERTEX_POINT('',#443129);
#42868=VERTEX_POINT('',#443131);
#42869=VERTEX_POINT('',#443138);
#42870=VERTEX_POINT('',#443204);
#42871=VERTEX_POINT('',#443247);
#42872=VERTEX_POINT('',#443274);
#42873=VERTEX_POINT('',#443459);
#42874=VERTEX_POINT('',#443460);
#42875=VERTEX_POINT('',#443462);
#42876=VERTEX_POINT('',#443464);
#42877=VERTEX_POINT('',#443466);
#42878=VERTEX_POINT('',#443473);
#42879=VERTEX_POINT('',#443474);
#42880=VERTEX_POINT('',#443476);
#42881=VERTEX_POINT('',#443478);
#42882=VERTEX_POINT('',#443480);
#42883=VERTEX_POINT('',#443487);
#42884=VERTEX_POINT('',#443553);
#42885=VERTEX_POINT('',#443596);
#42886=VERTEX_POINT('',#443623);
#42887=VERTEX_POINT('',#443808);
#42888=VERTEX_POINT('',#443809);
#42889=VERTEX_POINT('',#443811);
#42890=VERTEX_POINT('',#443813);
#42891=VERTEX_POINT('',#443815);
#42892=VERTEX_POINT('',#443822);
#42893=VERTEX_POINT('',#443823);
#42894=VERTEX_POINT('',#443825);
#42895=VERTEX_POINT('',#443827);
#42896=VERTEX_POINT('',#443829);
#42897=VERTEX_POINT('',#443836);
#42898=VERTEX_POINT('',#443902);
#42899=VERTEX_POINT('',#443945);
#42900=VERTEX_POINT('',#443972);
#42901=VERTEX_POINT('',#444157);
#42902=VERTEX_POINT('',#444158);
#42903=VERTEX_POINT('',#444160);
#42904=VERTEX_POINT('',#444162);
#42905=VERTEX_POINT('',#444164);
#42906=VERTEX_POINT('',#444171);
#42907=VERTEX_POINT('',#444172);
#42908=VERTEX_POINT('',#444174);
#42909=VERTEX_POINT('',#444176);
#42910=VERTEX_POINT('',#444178);
#42911=VERTEX_POINT('',#444185);
#42912=VERTEX_POINT('',#444251);
#42913=VERTEX_POINT('',#444294);
#42914=VERTEX_POINT('',#444321);
#42915=VERTEX_POINT('',#444506);
#42916=VERTEX_POINT('',#444507);
#42917=VERTEX_POINT('',#444509);
#42918=VERTEX_POINT('',#444511);
#42919=VERTEX_POINT('',#444513);
#42920=VERTEX_POINT('',#444520);
#42921=VERTEX_POINT('',#444521);
#42922=VERTEX_POINT('',#444523);
#42923=VERTEX_POINT('',#444525);
#42924=VERTEX_POINT('',#444527);
#42925=VERTEX_POINT('',#444534);
#42926=VERTEX_POINT('',#444600);
#42927=VERTEX_POINT('',#444643);
#42928=VERTEX_POINT('',#444670);
#42929=VERTEX_POINT('',#444855);
#42930=VERTEX_POINT('',#444856);
#42931=VERTEX_POINT('',#444858);
#42932=VERTEX_POINT('',#444860);
#42933=VERTEX_POINT('',#444862);
#42934=VERTEX_POINT('',#444869);
#42935=VERTEX_POINT('',#444870);
#42936=VERTEX_POINT('',#444872);
#42937=VERTEX_POINT('',#444874);
#42938=VERTEX_POINT('',#444876);
#42939=VERTEX_POINT('',#444883);
#42940=VERTEX_POINT('',#444949);
#42941=VERTEX_POINT('',#444992);
#42942=VERTEX_POINT('',#445019);
#42943=VERTEX_POINT('',#445204);
#42944=VERTEX_POINT('',#445205);
#42945=VERTEX_POINT('',#445207);
#42946=VERTEX_POINT('',#445209);
#42947=VERTEX_POINT('',#445211);
#42948=VERTEX_POINT('',#445218);
#42949=VERTEX_POINT('',#445219);
#42950=VERTEX_POINT('',#445221);
#42951=VERTEX_POINT('',#445223);
#42952=VERTEX_POINT('',#445225);
#42953=VERTEX_POINT('',#445232);
#42954=VERTEX_POINT('',#445298);
#42955=VERTEX_POINT('',#445341);
#42956=VERTEX_POINT('',#445368);
#42957=VERTEX_POINT('',#445553);
#42958=VERTEX_POINT('',#445554);
#42959=VERTEX_POINT('',#445556);
#42960=VERTEX_POINT('',#445558);
#42961=VERTEX_POINT('',#445560);
#42962=VERTEX_POINT('',#445567);
#42963=VERTEX_POINT('',#445568);
#42964=VERTEX_POINT('',#445570);
#42965=VERTEX_POINT('',#445572);
#42966=VERTEX_POINT('',#445574);
#42967=VERTEX_POINT('',#445581);
#42968=VERTEX_POINT('',#445647);
#42969=VERTEX_POINT('',#445690);
#42970=VERTEX_POINT('',#445717);
#42971=VERTEX_POINT('',#445902);
#42972=VERTEX_POINT('',#445903);
#42973=VERTEX_POINT('',#445905);
#42974=VERTEX_POINT('',#445907);
#42975=VERTEX_POINT('',#445909);
#42976=VERTEX_POINT('',#445916);
#42977=VERTEX_POINT('',#445917);
#42978=VERTEX_POINT('',#445919);
#42979=VERTEX_POINT('',#445921);
#42980=VERTEX_POINT('',#445923);
#42981=VERTEX_POINT('',#445930);
#42982=VERTEX_POINT('',#445996);
#42983=VERTEX_POINT('',#446039);
#42984=VERTEX_POINT('',#446066);
#42985=VERTEX_POINT('',#446251);
#42986=VERTEX_POINT('',#446252);
#42987=VERTEX_POINT('',#446254);
#42988=VERTEX_POINT('',#446256);
#42989=VERTEX_POINT('',#446258);
#42990=VERTEX_POINT('',#446265);
#42991=VERTEX_POINT('',#446266);
#42992=VERTEX_POINT('',#446268);
#42993=VERTEX_POINT('',#446270);
#42994=VERTEX_POINT('',#446272);
#42995=VERTEX_POINT('',#446279);
#42996=VERTEX_POINT('',#446345);
#42997=VERTEX_POINT('',#446388);
#42998=VERTEX_POINT('',#446415);
#42999=VERTEX_POINT('',#446600);
#43000=VERTEX_POINT('',#446601);
#43001=VERTEX_POINT('',#446603);
#43002=VERTEX_POINT('',#446605);
#43003=VERTEX_POINT('',#446607);
#43004=VERTEX_POINT('',#446614);
#43005=VERTEX_POINT('',#446615);
#43006=VERTEX_POINT('',#446617);
#43007=VERTEX_POINT('',#446619);
#43008=VERTEX_POINT('',#446621);
#43009=VERTEX_POINT('',#446628);
#43010=VERTEX_POINT('',#446694);
#43011=VERTEX_POINT('',#446737);
#43012=VERTEX_POINT('',#446764);
#43013=VERTEX_POINT('',#446949);
#43014=VERTEX_POINT('',#446950);
#43015=VERTEX_POINT('',#446952);
#43016=VERTEX_POINT('',#446954);
#43017=VERTEX_POINT('',#446956);
#43018=VERTEX_POINT('',#446963);
#43019=VERTEX_POINT('',#446964);
#43020=VERTEX_POINT('',#446966);
#43021=VERTEX_POINT('',#446968);
#43022=VERTEX_POINT('',#446970);
#43023=VERTEX_POINT('',#446977);
#43024=VERTEX_POINT('',#447043);
#43025=VERTEX_POINT('',#447086);
#43026=VERTEX_POINT('',#447113);
#43027=VERTEX_POINT('',#447298);
#43028=VERTEX_POINT('',#447299);
#43029=VERTEX_POINT('',#447301);
#43030=VERTEX_POINT('',#447303);
#43031=VERTEX_POINT('',#447305);
#43032=VERTEX_POINT('',#447312);
#43033=VERTEX_POINT('',#447313);
#43034=VERTEX_POINT('',#447315);
#43035=VERTEX_POINT('',#447317);
#43036=VERTEX_POINT('',#447319);
#43037=VERTEX_POINT('',#447326);
#43038=VERTEX_POINT('',#447392);
#43039=VERTEX_POINT('',#447435);
#43040=VERTEX_POINT('',#447462);
#43041=VERTEX_POINT('',#447647);
#43042=VERTEX_POINT('',#447648);
#43043=VERTEX_POINT('',#447650);
#43044=VERTEX_POINT('',#447652);
#43045=VERTEX_POINT('',#447654);
#43046=VERTEX_POINT('',#447661);
#43047=VERTEX_POINT('',#447662);
#43048=VERTEX_POINT('',#447664);
#43049=VERTEX_POINT('',#447666);
#43050=VERTEX_POINT('',#447668);
#43051=VERTEX_POINT('',#447675);
#43052=VERTEX_POINT('',#447741);
#43053=VERTEX_POINT('',#447784);
#43054=VERTEX_POINT('',#447811);
#43055=VERTEX_POINT('',#447996);
#43056=VERTEX_POINT('',#447997);
#43057=VERTEX_POINT('',#447999);
#43058=VERTEX_POINT('',#448001);
#43059=VERTEX_POINT('',#448003);
#43060=VERTEX_POINT('',#448010);
#43061=VERTEX_POINT('',#448011);
#43062=VERTEX_POINT('',#448013);
#43063=VERTEX_POINT('',#448015);
#43064=VERTEX_POINT('',#448017);
#43065=VERTEX_POINT('',#448024);
#43066=VERTEX_POINT('',#448090);
#43067=VERTEX_POINT('',#448133);
#43068=VERTEX_POINT('',#448160);
#43069=VERTEX_POINT('',#448345);
#43070=VERTEX_POINT('',#448346);
#43071=VERTEX_POINT('',#448348);
#43072=VERTEX_POINT('',#448350);
#43073=VERTEX_POINT('',#448352);
#43074=VERTEX_POINT('',#448359);
#43075=VERTEX_POINT('',#448360);
#43076=VERTEX_POINT('',#448362);
#43077=VERTEX_POINT('',#448364);
#43078=VERTEX_POINT('',#448366);
#43079=VERTEX_POINT('',#448373);
#43080=VERTEX_POINT('',#448439);
#43081=VERTEX_POINT('',#448482);
#43082=VERTEX_POINT('',#448509);
#43083=VERTEX_POINT('',#448694);
#43084=VERTEX_POINT('',#448695);
#43085=VERTEX_POINT('',#448697);
#43086=VERTEX_POINT('',#448699);
#43087=VERTEX_POINT('',#448701);
#43088=VERTEX_POINT('',#448708);
#43089=VERTEX_POINT('',#448709);
#43090=VERTEX_POINT('',#448711);
#43091=VERTEX_POINT('',#448713);
#43092=VERTEX_POINT('',#448715);
#43093=VERTEX_POINT('',#448722);
#43094=VERTEX_POINT('',#448788);
#43095=VERTEX_POINT('',#448831);
#43096=VERTEX_POINT('',#448858);
#43097=VERTEX_POINT('',#449043);
#43098=VERTEX_POINT('',#449044);
#43099=VERTEX_POINT('',#449046);
#43100=VERTEX_POINT('',#449048);
#43101=VERTEX_POINT('',#449050);
#43102=VERTEX_POINT('',#449057);
#43103=VERTEX_POINT('',#449058);
#43104=VERTEX_POINT('',#449060);
#43105=VERTEX_POINT('',#449062);
#43106=VERTEX_POINT('',#449064);
#43107=VERTEX_POINT('',#449071);
#43108=VERTEX_POINT('',#449137);
#43109=VERTEX_POINT('',#449180);
#43110=VERTEX_POINT('',#449207);
#43111=VERTEX_POINT('',#449394);
#43112=VERTEX_POINT('',#449395);
#43113=VERTEX_POINT('',#449397);
#43114=VERTEX_POINT('',#449407);
#43115=VERTEX_POINT('',#449408);
#43116=VERTEX_POINT('',#449410);
#43117=VERTEX_POINT('',#449454);
#43118=VERTEX_POINT('',#449455);
#43119=VERTEX_POINT('',#449502);
#43120=VERTEX_POINT('',#449503);
#43121=VERTEX_POINT('',#449553);
#43122=VERTEX_POINT('',#449554);
#43123=VERTEX_POINT('',#449604);
#43124=VERTEX_POINT('',#449605);
#43125=VERTEX_POINT('',#449652);
#43126=VERTEX_POINT('',#449653);
#43127=VERTEX_POINT('',#449703);
#43128=VERTEX_POINT('',#449704);
#43129=VERTEX_POINT('',#449706);
#43130=VERTEX_POINT('',#449720);
#43131=VERTEX_POINT('',#449742);
#43132=VERTEX_POINT('',#449743);
#43133=VERTEX_POINT('',#449745);
#43134=VERTEX_POINT('',#449753);
#43135=VERTEX_POINT('',#449763);
#43136=VERTEX_POINT('',#449764);
#43137=VERTEX_POINT('',#449787);
#43138=VERTEX_POINT('',#449788);
#43139=VERTEX_POINT('',#449812);
#43140=VERTEX_POINT('',#449813);
#43141=VERTEX_POINT('',#449836);
#43142=VERTEX_POINT('',#449837);
#43143=VERTEX_POINT('',#449861);
#43144=VERTEX_POINT('',#449862);
#43145=VERTEX_POINT('',#449886);
#43146=VERTEX_POINT('',#449887);
#43147=VERTEX_POINT('',#449910);
#43148=VERTEX_POINT('',#449911);
#43149=VERTEX_POINT('',#449913);
#43150=VERTEX_POINT('',#449919);
#43151=VERTEX_POINT('',#449927);
#43152=VERTEX_POINT('',#449928);
#43153=VERTEX_POINT('',#449930);
#43154=VERTEX_POINT('',#449940);
#43155=VERTEX_POINT('',#449941);
#43156=VERTEX_POINT('',#449943);
#43157=VERTEX_POINT('',#449987);
#43158=VERTEX_POINT('',#449988);
#43159=VERTEX_POINT('',#450035);
#43160=VERTEX_POINT('',#450036);
#43161=VERTEX_POINT('',#450086);
#43162=VERTEX_POINT('',#450087);
#43163=VERTEX_POINT('',#450137);
#43164=VERTEX_POINT('',#450138);
#43165=VERTEX_POINT('',#450185);
#43166=VERTEX_POINT('',#450186);
#43167=VERTEX_POINT('',#450236);
#43168=VERTEX_POINT('',#450237);
#43169=VERTEX_POINT('',#450239);
#43170=VERTEX_POINT('',#450253);
#43171=VERTEX_POINT('',#450275);
#43172=VERTEX_POINT('',#450276);
#43173=VERTEX_POINT('',#450278);
#43174=VERTEX_POINT('',#450286);
#43175=VERTEX_POINT('',#450296);
#43176=VERTEX_POINT('',#450297);
#43177=VERTEX_POINT('',#450320);
#43178=VERTEX_POINT('',#450321);
#43179=VERTEX_POINT('',#450345);
#43180=VERTEX_POINT('',#450346);
#43181=VERTEX_POINT('',#450369);
#43182=VERTEX_POINT('',#450370);
#43183=VERTEX_POINT('',#450394);
#43184=VERTEX_POINT('',#450395);
#43185=VERTEX_POINT('',#450419);
#43186=VERTEX_POINT('',#450420);
#43187=VERTEX_POINT('',#450443);
#43188=VERTEX_POINT('',#450444);
#43189=VERTEX_POINT('',#450446);
#43190=VERTEX_POINT('',#450452);
#43191=VERTEX_POINT('',#450460);
#43192=VERTEX_POINT('',#450461);
#43193=VERTEX_POINT('',#450463);
#43194=VERTEX_POINT('',#450473);
#43195=VERTEX_POINT('',#450474);
#43196=VERTEX_POINT('',#450476);
#43197=VERTEX_POINT('',#450520);
#43198=VERTEX_POINT('',#450521);
#43199=VERTEX_POINT('',#450568);
#43200=VERTEX_POINT('',#450569);
#43201=VERTEX_POINT('',#450619);
#43202=VERTEX_POINT('',#450620);
#43203=VERTEX_POINT('',#450670);
#43204=VERTEX_POINT('',#450671);
#43205=VERTEX_POINT('',#450718);
#43206=VERTEX_POINT('',#450719);
#43207=VERTEX_POINT('',#450769);
#43208=VERTEX_POINT('',#450770);
#43209=VERTEX_POINT('',#450772);
#43210=VERTEX_POINT('',#450786);
#43211=VERTEX_POINT('',#450808);
#43212=VERTEX_POINT('',#450809);
#43213=VERTEX_POINT('',#450811);
#43214=VERTEX_POINT('',#450819);
#43215=VERTEX_POINT('',#450829);
#43216=VERTEX_POINT('',#450830);
#43217=VERTEX_POINT('',#450853);
#43218=VERTEX_POINT('',#450854);
#43219=VERTEX_POINT('',#450878);
#43220=VERTEX_POINT('',#450879);
#43221=VERTEX_POINT('',#450902);
#43222=VERTEX_POINT('',#450903);
#43223=VERTEX_POINT('',#450927);
#43224=VERTEX_POINT('',#450928);
#43225=VERTEX_POINT('',#450952);
#43226=VERTEX_POINT('',#450953);
#43227=VERTEX_POINT('',#450976);
#43228=VERTEX_POINT('',#450977);
#43229=VERTEX_POINT('',#450979);
#43230=VERTEX_POINT('',#450985);
#43231=VERTEX_POINT('',#450993);
#43232=VERTEX_POINT('',#450994);
#43233=VERTEX_POINT('',#450996);
#43234=VERTEX_POINT('',#451006);
#43235=VERTEX_POINT('',#451007);
#43236=VERTEX_POINT('',#451009);
#43237=VERTEX_POINT('',#451053);
#43238=VERTEX_POINT('',#451054);
#43239=VERTEX_POINT('',#451101);
#43240=VERTEX_POINT('',#451102);
#43241=VERTEX_POINT('',#451152);
#43242=VERTEX_POINT('',#451153);
#43243=VERTEX_POINT('',#451203);
#43244=VERTEX_POINT('',#451204);
#43245=VERTEX_POINT('',#451251);
#43246=VERTEX_POINT('',#451252);
#43247=VERTEX_POINT('',#451302);
#43248=VERTEX_POINT('',#451303);
#43249=VERTEX_POINT('',#451305);
#43250=VERTEX_POINT('',#451319);
#43251=VERTEX_POINT('',#451341);
#43252=VERTEX_POINT('',#451342);
#43253=VERTEX_POINT('',#451344);
#43254=VERTEX_POINT('',#451352);
#43255=VERTEX_POINT('',#451362);
#43256=VERTEX_POINT('',#451363);
#43257=VERTEX_POINT('',#451386);
#43258=VERTEX_POINT('',#451387);
#43259=VERTEX_POINT('',#451411);
#43260=VERTEX_POINT('',#451412);
#43261=VERTEX_POINT('',#451435);
#43262=VERTEX_POINT('',#451436);
#43263=VERTEX_POINT('',#451460);
#43264=VERTEX_POINT('',#451461);
#43265=VERTEX_POINT('',#451485);
#43266=VERTEX_POINT('',#451486);
#43267=VERTEX_POINT('',#451509);
#43268=VERTEX_POINT('',#451510);
#43269=VERTEX_POINT('',#451512);
#43270=VERTEX_POINT('',#451518);
#43271=VERTEX_POINT('',#451526);
#43272=VERTEX_POINT('',#451528);
#43273=VERTEX_POINT('',#451532);
#43274=VERTEX_POINT('',#451533);
#43275=VERTEX_POINT('',#451538);
#43276=VERTEX_POINT('',#452832);
#43277=VERTEX_POINT('',#453308);
#43278=VERTEX_POINT('',#453312);
#43279=VERTEX_POINT('',#453314);
#43280=VERTEX_POINT('',#453318);
#43281=VERTEX_POINT('',#453322);
#43282=VERTEX_POINT('',#453326);
#43283=VERTEX_POINT('',#453330);
#43284=VERTEX_POINT('',#453334);
#43285=VERTEX_POINT('',#453338);
#43286=VERTEX_POINT('',#453340);
#43287=VERTEX_POINT('',#453344);
#43288=VERTEX_POINT('',#453346);
#43289=VERTEX_POINT('',#453350);
#43290=VERTEX_POINT('',#453352);
#43291=VERTEX_POINT('',#453356);
#43292=VERTEX_POINT('',#453358);
#43293=VERTEX_POINT('',#453362);
#43294=VERTEX_POINT('',#453364);
#43295=VERTEX_POINT('',#453368);
#43296=VERTEX_POINT('',#453370);
#43297=VERTEX_POINT('',#453374);
#43298=VERTEX_POINT('',#453376);
#43299=VERTEX_POINT('',#453380);
#43300=VERTEX_POINT('',#453382);
#43301=VERTEX_POINT('',#453386);
#43302=VERTEX_POINT('',#453388);
#43303=VERTEX_POINT('',#453392);
#43304=VERTEX_POINT('',#453394);
#43305=VERTEX_POINT('',#453398);
#43306=VERTEX_POINT('',#453400);
#43307=VERTEX_POINT('',#453404);
#43308=VERTEX_POINT('',#453406);
#43309=VERTEX_POINT('',#453410);
#43310=VERTEX_POINT('',#453412);
#43311=VERTEX_POINT('',#453416);
#43312=VERTEX_POINT('',#453418);
#43313=VERTEX_POINT('',#453422);
#43314=VERTEX_POINT('',#453424);
#43315=VERTEX_POINT('',#453428);
#43316=VERTEX_POINT('',#453430);
#43317=VERTEX_POINT('',#453434);
#43318=VERTEX_POINT('',#453436);
#43319=VERTEX_POINT('',#454967);
#43320=VERTEX_POINT('',#454968);
#43321=VERTEX_POINT('',#454970);
#43322=VERTEX_POINT('',#454981);
#43323=VERTEX_POINT('',#454991);
#43324=VERTEX_POINT('',#454992);
#43325=VERTEX_POINT('',#455039);
#43326=VERTEX_POINT('',#455040);
#43327=VERTEX_POINT('',#455087);
#43328=VERTEX_POINT('',#455088);
#43329=VERTEX_POINT('',#455141);
#43330=VERTEX_POINT('',#455142);
#43331=VERTEX_POINT('',#455189);
#43332=VERTEX_POINT('',#455190);
#43333=VERTEX_POINT('',#455237);
#43334=VERTEX_POINT('',#455238);
#43335=VERTEX_POINT('',#455291);
#43336=VERTEX_POINT('',#455292);
#43337=VERTEX_POINT('',#455339);
#43338=VERTEX_POINT('',#455340);
#43339=VERTEX_POINT('',#455387);
#43340=VERTEX_POINT('',#455388);
#43341=VERTEX_POINT('',#455435);
#43342=VERTEX_POINT('',#455436);
#43343=VERTEX_POINT('',#455438);
#43344=VERTEX_POINT('',#455446);
#43345=VERTEX_POINT('',#455447);
#43346=VERTEX_POINT('',#455459);
#43347=VERTEX_POINT('',#455472);
#43348=VERTEX_POINT('',#455473);
#43349=VERTEX_POINT('',#455496);
#43350=VERTEX_POINT('',#455497);
#43351=VERTEX_POINT('',#455520);
#43352=VERTEX_POINT('',#455521);
#43353=VERTEX_POINT('',#455545);
#43354=VERTEX_POINT('',#455546);
#43355=VERTEX_POINT('',#455570);
#43356=VERTEX_POINT('',#455571);
#43357=VERTEX_POINT('',#455594);
#43358=VERTEX_POINT('',#455595);
#43359=VERTEX_POINT('',#455619);
#43360=VERTEX_POINT('',#455620);
#43361=VERTEX_POINT('',#455644);
#43362=VERTEX_POINT('',#455645);
#43363=VERTEX_POINT('',#455668);
#43364=VERTEX_POINT('',#455669);
#43365=VERTEX_POINT('',#455671);
#43366=VERTEX_POINT('',#455682);
#43367=VERTEX_POINT('',#455692);
#43368=VERTEX_POINT('',#455693);
#43369=VERTEX_POINT('',#455740);
#43370=VERTEX_POINT('',#455741);
#43371=VERTEX_POINT('',#455788);
#43372=VERTEX_POINT('',#455789);
#43373=VERTEX_POINT('',#455842);
#43374=VERTEX_POINT('',#455843);
#43375=VERTEX_POINT('',#455890);
#43376=VERTEX_POINT('',#455891);
#43377=VERTEX_POINT('',#455893);
#43378=VERTEX_POINT('',#455900);
#43379=VERTEX_POINT('',#455907);
#43380=VERTEX_POINT('',#455908);
#43381=VERTEX_POINT('',#455932);
#43382=VERTEX_POINT('',#455933);
#43383=VERTEX_POINT('',#455957);
#43384=VERTEX_POINT('',#455958);
#43385=VERTEX_POINT('',#455982);
#43386=VERTEX_POINT('',#455983);
#43387=VERTEX_POINT('',#456153);
#43388=VERTEX_POINT('',#456264);
#43389=VERTEX_POINT('',#456366);
#43390=VERTEX_POINT('',#456524);
#43391=VERTEX_POINT('',#456725);
#43392=VERTEX_POINT('',#456729);
#43393=VERTEX_POINT('',#456730);
#43394=VERTEX_POINT('',#456754);
#43395=VERTEX_POINT('',#457043);
#43396=VERTEX_POINT('',#457130);
#43397=VERTEX_POINT('',#457229);
#43398=VERTEX_POINT('',#457601);
#43399=VERTEX_POINT('',#457683);
#43400=VERTEX_POINT('',#457684);
#43401=VERTEX_POINT('',#457687);
#43402=VERTEX_POINT('',#457691);
#43403=VERTEX_POINT('',#457700);
#43404=VERTEX_POINT('',#457702);
#43405=VERTEX_POINT('',#457706);
#43406=VERTEX_POINT('',#457710);
#43407=VERTEX_POINT('',#457719);
#43408=VERTEX_POINT('',#457721);
#43409=VERTEX_POINT('',#457724);
#43410=VERTEX_POINT('',#457728);
#43411=VERTEX_POINT('',#457734);
#43412=VERTEX_POINT('',#457735);
#43413=VERTEX_POINT('',#457737);
#43414=VERTEX_POINT('',#457748);
#43415=VERTEX_POINT('',#457758);
#43416=VERTEX_POINT('',#457759);
#43417=VERTEX_POINT('',#457806);
#43418=VERTEX_POINT('',#457807);
#43419=VERTEX_POINT('',#457854);
#43420=VERTEX_POINT('',#457855);
#43421=VERTEX_POINT('',#457908);
#43422=VERTEX_POINT('',#457909);
#43423=VERTEX_POINT('',#457956);
#43424=VERTEX_POINT('',#457957);
#43425=VERTEX_POINT('',#458004);
#43426=VERTEX_POINT('',#458005);
#43427=VERTEX_POINT('',#458007);
#43428=VERTEX_POINT('',#458014);
#43429=VERTEX_POINT('',#458021);
#43430=VERTEX_POINT('',#458022);
#43431=VERTEX_POINT('',#458046);
#43432=VERTEX_POINT('',#458047);
#43433=VERTEX_POINT('',#458070);
#43434=VERTEX_POINT('',#458071);
#43435=VERTEX_POINT('',#458095);
#43436=VERTEX_POINT('',#458096);
#43437=VERTEX_POINT('',#458120);
#43438=VERTEX_POINT('',#458121);
#43439=VERTEX_POINT('',#458315);
#43440=VERTEX_POINT('',#458426);
#43441=VERTEX_POINT('',#458500);
#43442=VERTEX_POINT('',#458530);
#43443=VERTEX_POINT('',#458532);
#43444=VERTEX_POINT('',#458737);
#43445=VERTEX_POINT('',#458910);
#43446=VERTEX_POINT('',#458915);
#43447=VERTEX_POINT('',#458919);
#43448=VERTEX_POINT('',#458921);
#43449=VERTEX_POINT('',#458923);
#43450=VERTEX_POINT('',#458927);
#43451=VERTEX_POINT('',#458931);
#43452=VERTEX_POINT('',#458935);
#43453=VERTEX_POINT('',#458937);
#43454=VERTEX_POINT('',#458941);
#43455=VERTEX_POINT('',#458945);
#43456=VERTEX_POINT('',#458946);
#43457=VERTEX_POINT('',#458953);
#43458=VERTEX_POINT('',#458957);
#43459=VERTEX_POINT('',#458958);
#43460=VERTEX_POINT('',#458960);
#43461=VERTEX_POINT('',#458962);
#43462=VERTEX_POINT('',#458964);
#43463=VERTEX_POINT('',#458966);
#43464=VERTEX_POINT('',#458970);
#43465=VERTEX_POINT('',#458971);
#43466=VERTEX_POINT('',#458973);
#43467=VERTEX_POINT('',#458975);
#43468=VERTEX_POINT('',#458977);
#43469=VERTEX_POINT('',#458979);
#43470=VERTEX_POINT('',#458997);
#43471=VERTEX_POINT('',#458999);
#43472=VERTEX_POINT('',#459003);
#43473=VERTEX_POINT('',#459005);
#43474=VERTEX_POINT('',#459009);
#43475=VERTEX_POINT('',#459011);
#43476=VERTEX_POINT('',#459015);
#43477=VERTEX_POINT('',#459017);
#43478=VERTEX_POINT('',#459021);
#43479=VERTEX_POINT('',#459023);
#43480=VERTEX_POINT('',#459027);
#43481=VERTEX_POINT('',#459028);
#43482=VERTEX_POINT('',#459030);
#43483=VERTEX_POINT('',#459032);
#43484=VERTEX_POINT('',#459036);
#43485=VERTEX_POINT('',#459037);
#43486=VERTEX_POINT('',#459039);
#43487=VERTEX_POINT('',#459041);
#43488=VERTEX_POINT('',#459045);
#43489=VERTEX_POINT('',#459046);
#43490=VERTEX_POINT('',#459048);
#43491=VERTEX_POINT('',#459050);
#43492=VERTEX_POINT('',#459054);
#43493=VERTEX_POINT('',#459056);
#43494=VERTEX_POINT('',#459058);
#43495=VERTEX_POINT('',#459060);
#43496=VERTEX_POINT('',#459062);
#43497=VERTEX_POINT('',#459064);
#43498=VERTEX_POINT('',#459068);
#43499=VERTEX_POINT('',#459069);
#43500=VERTEX_POINT('',#459071);
#43501=VERTEX_POINT('',#459073);
#43502=VERTEX_POINT('',#459077);
#43503=VERTEX_POINT('',#459078);
#43504=VERTEX_POINT('',#459080);
#43505=VERTEX_POINT('',#459083);
#43506=VERTEX_POINT('',#459085);
#43507=VERTEX_POINT('',#459087);
#43508=VERTEX_POINT('',#459091);
#43509=VERTEX_POINT('',#459092);
#43510=VERTEX_POINT('',#459094);
#43511=VERTEX_POINT('',#459096);
#43512=VERTEX_POINT('',#459100);
#43513=VERTEX_POINT('',#459101);
#43514=VERTEX_POINT('',#459103);
#43515=VERTEX_POINT('',#459105);
#43516=EDGE_CURVE('',#34651,#34652,#27047,.T.);
#43517=EDGE_CURVE('',#34652,#34653,#23498,.T.);
#43518=EDGE_CURVE('',#34653,#34654,#23499,.T.);
#43519=EDGE_CURVE('',#34655,#34654,#18132,.F.);
#43520=EDGE_CURVE('',#34655,#34651,#23500,.T.);
#43521=EDGE_CURVE('',#34656,#34657,#27048,.T.);
#43522=EDGE_CURVE('',#34657,#34658,#23501,.T.);
#43523=EDGE_CURVE('',#34658,#34652,#23502,.T.);
#43524=EDGE_CURVE('',#34651,#34656,#23503,.T.);
#43525=EDGE_CURVE('',#34659,#34660,#27049,.T.);
#43526=EDGE_CURVE('',#34660,#34661,#23504,.T.);
#43527=EDGE_CURVE('',#34661,#34657,#23505,.T.);
#43528=EDGE_CURVE('',#34656,#34659,#23506,.T.);
#43529=EDGE_CURVE('',#34662,#34663,#27050,.T.);
#43530=EDGE_CURVE('',#34662,#34664,#23507,.T.);
#43531=EDGE_CURVE('',#34664,#34665,#18133,.F.);
#43532=EDGE_CURVE('',#34665,#34663,#23508,.T.);
#43533=EDGE_CURVE('',#34666,#34667,#27051,.T.);
#43534=EDGE_CURVE('',#34667,#34668,#23509,.T.);
#43535=EDGE_CURVE('',#34668,#34669,#23510,.T.);
#43536=EDGE_CURVE('',#34670,#34669,#18134,.F.);
#43537=EDGE_CURVE('',#34670,#34666,#23511,.T.);
#43538=EDGE_CURVE('',#34671,#34672,#27052,.T.);
#43539=EDGE_CURVE('',#34672,#34673,#23512,.T.);
#43540=EDGE_CURVE('',#34673,#34667,#23513,.T.);
#43541=EDGE_CURVE('',#34666,#34671,#23514,.T.);
#43542=EDGE_CURVE('',#34674,#34675,#27053,.T.);
#43543=EDGE_CURVE('',#34675,#34676,#23515,.T.);
#43544=EDGE_CURVE('',#34676,#34672,#23516,.T.);
#43545=EDGE_CURVE('',#34671,#34674,#23517,.T.);
#43546=EDGE_CURVE('',#34677,#34678,#27054,.T.);
#43547=EDGE_CURVE('',#34677,#34679,#23518,.T.);
#43548=EDGE_CURVE('',#34679,#34680,#18135,.F.);
#43549=EDGE_CURVE('',#34680,#34678,#23519,.T.);
#43550=EDGE_CURVE('',#34681,#34682,#27055,.T.);
#43551=EDGE_CURVE('',#34682,#34683,#23520,.T.);
#43552=EDGE_CURVE('',#34684,#34683,#18136,.T.);
#43553=EDGE_CURVE('',#34681,#34684,#23521,.F.);
#43554=EDGE_CURVE('',#34685,#34686,#27056,.T.);
#43555=EDGE_CURVE('',#34686,#34687,#23522,.T.);
#43556=EDGE_CURVE('',#34687,#34682,#23523,.T.);
#43557=EDGE_CURVE('',#34688,#34681,#23524,.F.);
#43558=EDGE_CURVE('',#34685,#34688,#23525,.F.);
#43559=EDGE_CURVE('',#34689,#34690,#27057,.T.);
#43560=EDGE_CURVE('',#34690,#34691,#23526,.T.);
#43561=EDGE_CURVE('',#34691,#34686,#23527,.T.);
#43562=EDGE_CURVE('',#34692,#34685,#23528,.F.);
#43563=EDGE_CURVE('',#34689,#34692,#23529,.F.);
#43564=EDGE_CURVE('',#34693,#34694,#27058,.T.);
#43565=EDGE_CURVE('',#34695,#34693,#23530,.F.);
#43566=EDGE_CURVE('',#34696,#34695,#23531,.T.);
#43567=EDGE_CURVE('',#34697,#34696,#18137,.T.);
#43568=EDGE_CURVE('',#34697,#34694,#23532,.T.);
#43569=EDGE_CURVE('',#34698,#34699,#27059,.T.);
#43570=EDGE_CURVE('',#34699,#34700,#23533,.T.);
#43571=EDGE_CURVE('',#34701,#34700,#18138,.T.);
#43572=EDGE_CURVE('',#34698,#34701,#23534,.F.);
#43573=EDGE_CURVE('',#34702,#34703,#27060,.T.);
#43574=EDGE_CURVE('',#34703,#34704,#23535,.T.);
#43575=EDGE_CURVE('',#34704,#34699,#23536,.T.);
#43576=EDGE_CURVE('',#34705,#34698,#23537,.F.);
#43577=EDGE_CURVE('',#34702,#34705,#23538,.F.);
#43578=EDGE_CURVE('',#34706,#34707,#27061,.T.);
#43579=EDGE_CURVE('',#34707,#34708,#23539,.T.);
#43580=EDGE_CURVE('',#34708,#34703,#23540,.T.);
#43581=EDGE_CURVE('',#34709,#34702,#23541,.F.);
#43582=EDGE_CURVE('',#34706,#34709,#23542,.F.);
#43583=EDGE_CURVE('',#34710,#34711,#27062,.T.);
#43584=EDGE_CURVE('',#34712,#34710,#23543,.F.);
#43585=EDGE_CURVE('',#34713,#34712,#23544,.T.);
#43586=EDGE_CURVE('',#34714,#34713,#18139,.T.);
#43587=EDGE_CURVE('',#34714,#34711,#23545,.T.);
#43588=EDGE_CURVE('',#34711,#34707,#23546,.T.);
#43589=EDGE_CURVE('',#34710,#34706,#23547,.F.);
#43590=EDGE_CURVE('',#34694,#34690,#23548,.T.);
#43591=EDGE_CURVE('',#34693,#34689,#23549,.F.);
#43592=EDGE_CURVE('',#34678,#34715,#23550,.T.);
#43593=EDGE_CURVE('',#34715,#34675,#23551,.T.);
#43594=EDGE_CURVE('',#34674,#34677,#23552,.T.);
#43595=EDGE_CURVE('',#34663,#34716,#23553,.T.);
#43596=EDGE_CURVE('',#34716,#34660,#23554,.T.);
#43597=EDGE_CURVE('',#34659,#34662,#23555,.T.);
#43598=EDGE_CURVE('',#34700,#34655,#23556,.T.);
#43599=EDGE_CURVE('',#34664,#34714,#23557,.T.);
#43600=EDGE_CURVE('',#34654,#34701,#23558,.T.);
#43601=EDGE_CURVE('',#34665,#34717,#23559,.T.);
#43602=EDGE_CURVE('',#34713,#34717,#23560,.T.);
#43603=EDGE_CURVE('',#34718,#34719,#18140,.T.);
#43604=EDGE_CURVE('',#34720,#34718,#27063,.T.);
#43605=EDGE_CURVE('',#34721,#34720,#18141,.T.);
#43606=EDGE_CURVE('',#34722,#34721,#27064,.T.);
#43607=EDGE_CURVE('',#34723,#34722,#18142,.T.);
#43608=EDGE_CURVE('',#34719,#34723,#18143,.T.);
#43609=EDGE_CURVE('',#34683,#34670,#23561,.T.);
#43610=EDGE_CURVE('',#34679,#34697,#23562,.T.);
#43611=EDGE_CURVE('',#34669,#34684,#23563,.T.);
#43612=EDGE_CURVE('',#34680,#34724,#23564,.T.);
#43613=EDGE_CURVE('',#34696,#34724,#23565,.T.);
#43614=EDGE_CURVE('',#34725,#34726,#18144,.T.);
#43615=EDGE_CURVE('',#34727,#34725,#27065,.T.);
#43616=EDGE_CURVE('',#34728,#34727,#18145,.T.);
#43617=EDGE_CURVE('',#34729,#34728,#27066,.T.);
#43618=EDGE_CURVE('',#34730,#34729,#18146,.T.);
#43619=EDGE_CURVE('',#34731,#34730,#18147,.T.);
#43620=EDGE_CURVE('',#34726,#34731,#18148,.T.);
#43621=EDGE_CURVE('',#34732,#34732,#18149,.T.);
#43622=EDGE_CURVE('',#34732,#34733,#27067,.T.);
#43623=EDGE_CURVE('',#34733,#34733,#18150,.T.);
#43624=EDGE_CURVE('',#34732,#34734,#27068,.T.);
#43625=EDGE_CURVE('',#34734,#34734,#18151,.T.);
#43626=EDGE_CURVE('',#34735,#34735,#18152,.T.);
#43627=EDGE_CURVE('',#34736,#34737,#18153,.T.);
#43628=EDGE_CURVE('',#34737,#34738,#27069,.T.);
#43629=EDGE_CURVE('',#34738,#34738,#18154,.T.);
#43630=EDGE_CURVE('',#34737,#34736,#18155,.T.);
#43631=EDGE_CURVE('',#34736,#34731,#27070,.T.);
#43632=EDGE_CURVE('',#34739,#34730,#23566,.T.);
#43633=EDGE_CURVE('',#34740,#34739,#27071,.T.);
#43634=EDGE_CURVE('',#34741,#34740,#18156,.T.);
#43635=EDGE_CURVE('',#34742,#34741,#27072,.T.);
#43636=EDGE_CURVE('',#34719,#34742,#23567,.T.);
#43637=EDGE_CURVE('',#34743,#34723,#23568,.T.);
#43638=EDGE_CURVE('',#34744,#34743,#27073,.T.);
#43639=EDGE_CURVE('',#34745,#34744,#18157,.T.);
#43640=EDGE_CURVE('',#34746,#34745,#27074,.T.);
#43641=EDGE_CURVE('',#34726,#34746,#23569,.T.);
#43642=EDGE_CURVE('',#34747,#34747,#18158,.T.);
#43643=EDGE_CURVE('',#34748,#34749,#18159,.T.);
#43644=EDGE_CURVE('',#34749,#34750,#27075,.T.);
#43645=EDGE_CURVE('',#34750,#34750,#18160,.T.);
#43646=EDGE_CURVE('',#34749,#34748,#18161,.T.);
#43647=EDGE_CURVE('',#34751,#34751,#18162,.T.);
#43648=EDGE_CURVE('',#34751,#34748,#27076,.T.);
#43649=EDGE_CURVE('',#34752,#34752,#18163,.T.);
#43650=EDGE_CURVE('',#34753,#34753,#18164,.T.);
#43651=EDGE_CURVE('',#34753,#34754,#27077,.T.);
#43652=EDGE_CURVE('',#34754,#34754,#18165,.T.);
#43653=EDGE_CURVE('',#34755,#34755,#18166,.T.);
#43654=EDGE_CURVE('',#34753,#34756,#27078,.T.);
#43655=EDGE_CURVE('',#34756,#34756,#18167,.T.);
#43656=EDGE_CURVE('',#34751,#34755,#27079,.T.);
#43657=EDGE_CURVE('',#34722,#34757,#27080,.T.);
#43658=EDGE_CURVE('',#34757,#34743,#18168,.T.);
#43659=EDGE_CURVE('',#34721,#34758,#27081,.T.);
#43660=EDGE_CURVE('',#34758,#34757,#27082,.T.);
#43661=EDGE_CURVE('',#34720,#34759,#27083,.T.);
#43662=EDGE_CURVE('',#34759,#34758,#18169,.T.);
#43663=EDGE_CURVE('',#34718,#34760,#27084,.T.);
#43664=EDGE_CURVE('',#34760,#34759,#27085,.T.);
#43665=EDGE_CURVE('',#34742,#34760,#18170,.T.);
#43666=EDGE_CURVE('',#34729,#34761,#27086,.T.);
#43667=EDGE_CURVE('',#34761,#34739,#18171,.T.);
#43668=EDGE_CURVE('',#34728,#34762,#27087,.T.);
#43669=EDGE_CURVE('',#34762,#34761,#27088,.T.);
#43670=EDGE_CURVE('',#34727,#34763,#27089,.T.);
#43671=EDGE_CURVE('',#34763,#34762,#18172,.T.);
#43672=EDGE_CURVE('',#34725,#34764,#27090,.T.);
#43673=EDGE_CURVE('',#34764,#34763,#27091,.T.);
#43674=EDGE_CURVE('',#34746,#34764,#18173,.T.);
#43675=EDGE_CURVE('',#34765,#34766,#27092,.T.);
#43676=EDGE_CURVE('',#34766,#34767,#27093,.T.);
#43677=EDGE_CURVE('',#34767,#34768,#27094,.T.);
#43678=EDGE_CURVE('',#34768,#34765,#27095,.T.);
#43679=EDGE_CURVE('',#34769,#34770,#27096,.T.);
#43680=EDGE_CURVE('',#34770,#34766,#18174,.T.);
#43681=EDGE_CURVE('',#34765,#34769,#18175,.T.);
#43682=EDGE_CURVE('',#34771,#34772,#27097,.T.);
#43683=EDGE_CURVE('',#34772,#34770,#27098,.T.);
#43684=EDGE_CURVE('',#34769,#34771,#27099,.T.);
#43685=EDGE_CURVE('',#34773,#34740,#27100,.T.);
#43686=EDGE_CURVE('',#34740,#34772,#18176,.T.);
#43687=EDGE_CURVE('',#34771,#34773,#18177,.T.);
#43688=EDGE_CURVE('',#34774,#34741,#27101,.T.);
#43689=EDGE_CURVE('',#34773,#34774,#18178,.T.);
#43690=EDGE_CURVE('',#34775,#34776,#27102,.T.);
#43691=EDGE_CURVE('',#34776,#34741,#18179,.T.);
#43692=EDGE_CURVE('',#34774,#34775,#18180,.T.);
#43693=EDGE_CURVE('',#34775,#34777,#27103,.T.);
#43694=EDGE_CURVE('',#34777,#34778,#27104,.T.);
#43695=EDGE_CURVE('',#34778,#34776,#27105,.T.);
#43696=EDGE_CURVE('',#34779,#34780,#27106,.T.);
#43697=EDGE_CURVE('',#34780,#34778,#18181,.T.);
#43698=EDGE_CURVE('',#34777,#34779,#18182,.T.);
#43699=EDGE_CURVE('',#34779,#34781,#27107,.T.);
#43700=EDGE_CURVE('',#34781,#34782,#27108,.T.);
#43701=EDGE_CURVE('',#34782,#34780,#27109,.T.);
#43702=EDGE_CURVE('',#34783,#34744,#27110,.T.);
#43703=EDGE_CURVE('',#34744,#34782,#18183,.T.);
#43704=EDGE_CURVE('',#34781,#34783,#18184,.T.);
#43705=EDGE_CURVE('',#34784,#34745,#27111,.T.);
#43706=EDGE_CURVE('',#34783,#34784,#18185,.T.);
#43707=EDGE_CURVE('',#34767,#34745,#18186,.T.);
#43708=EDGE_CURVE('',#34784,#34768,#18187,.T.);
#43709=EDGE_CURVE('',#34778,#34759,#27112,.T.);
#43710=EDGE_CURVE('',#34780,#34758,#27113,.T.);
#43711=EDGE_CURVE('',#34757,#34782,#27114,.T.);
#43712=EDGE_CURVE('',#34767,#34764,#27115,.T.);
#43713=EDGE_CURVE('',#34766,#34763,#27116,.T.);
#43714=EDGE_CURVE('',#34776,#34760,#27117,.T.);
#43715=EDGE_CURVE('',#34761,#34772,#27118,.T.);
#43716=EDGE_CURVE('',#34770,#34762,#27119,.T.);
#43717=EDGE_CURVE('',#34785,#34785,#18188,.T.);
#43718=EDGE_CURVE('',#34785,#34786,#27120,.T.);
#43719=EDGE_CURVE('',#34786,#34786,#18189,.T.);
#43720=EDGE_CURVE('',#34785,#34787,#27121,.T.);
#43721=EDGE_CURVE('',#34787,#34787,#18190,.T.);
#43722=EDGE_CURVE('',#34788,#34789,#18191,.T.);
#43723=EDGE_CURVE('',#34789,#34790,#27122,.T.);
#43724=EDGE_CURVE('',#34790,#34791,#23570,.T.);
#43725=EDGE_CURVE('',#34792,#34791,#18192,.T.);
#43726=EDGE_CURVE('',#34792,#34793,#23571,.T.);
#43727=EDGE_CURVE('',#34793,#34794,#27123,.T.);
#43728=EDGE_CURVE('',#34794,#34795,#18193,.T.);
#43729=EDGE_CURVE('',#34795,#34796,#27124,.T.);
#43730=EDGE_CURVE('',#34796,#34797,#23572,.T.);
#43731=EDGE_CURVE('',#34798,#34797,#18194,.T.);
#43732=EDGE_CURVE('',#34798,#34799,#23573,.T.);
#43733=EDGE_CURVE('',#34799,#34800,#27125,.T.);
#43734=EDGE_CURVE('',#34800,#34801,#18195,.T.);
#43735=EDGE_CURVE('',#34801,#34802,#27126,.T.);
#43736=EDGE_CURVE('',#34802,#34803,#23574,.T.);
#43737=EDGE_CURVE('',#34804,#34803,#18196,.T.);
#43738=EDGE_CURVE('',#34804,#34805,#23575,.T.);
#43739=EDGE_CURVE('',#34805,#34806,#27127,.T.);
#43740=EDGE_CURVE('',#34806,#34807,#18197,.T.);
#43741=EDGE_CURVE('',#34807,#34808,#27128,.T.);
#43742=EDGE_CURVE('',#34808,#34809,#23576,.T.);
#43743=EDGE_CURVE('',#34810,#34809,#18198,.T.);
#43744=EDGE_CURVE('',#34810,#34811,#23577,.T.);
#43745=EDGE_CURVE('',#34811,#34812,#27129,.T.);
#43746=EDGE_CURVE('',#34812,#34813,#18199,.T.);
#43747=EDGE_CURVE('',#34813,#34814,#27130,.T.);
#43748=EDGE_CURVE('',#34814,#34815,#23578,.T.);
#43749=EDGE_CURVE('',#34816,#34815,#18200,.T.);
#43750=EDGE_CURVE('',#34816,#34817,#23579,.T.);
#43751=EDGE_CURVE('',#34817,#34818,#27131,.T.);
#43752=EDGE_CURVE('',#34818,#34819,#18201,.T.);
#43753=EDGE_CURVE('',#34819,#34820,#27132,.T.);
#43754=EDGE_CURVE('',#34820,#34821,#23580,.T.);
#43755=EDGE_CURVE('',#34822,#34821,#18202,.T.);
#43756=EDGE_CURVE('',#34822,#34823,#23581,.T.);
#43757=EDGE_CURVE('',#34823,#34824,#27133,.T.);
#43758=EDGE_CURVE('',#34824,#34825,#18203,.T.);
#43759=EDGE_CURVE('',#34825,#34826,#27134,.T.);
#43760=EDGE_CURVE('',#34826,#34827,#23582,.T.);
#43761=EDGE_CURVE('',#34828,#34827,#18204,.T.);
#43762=EDGE_CURVE('',#34828,#34829,#23583,.T.);
#43763=EDGE_CURVE('',#34829,#34830,#27135,.T.);
#43764=EDGE_CURVE('',#34830,#34831,#18205,.T.);
#43765=EDGE_CURVE('',#34831,#34832,#27136,.T.);
#43766=EDGE_CURVE('',#34832,#34833,#23584,.T.);
#43767=EDGE_CURVE('',#34834,#34833,#18206,.T.);
#43768=EDGE_CURVE('',#34834,#34835,#23585,.T.);
#43769=EDGE_CURVE('',#34835,#34836,#27137,.T.);
#43770=EDGE_CURVE('',#34836,#34837,#18207,.T.);
#43771=EDGE_CURVE('',#34837,#34838,#27138,.T.);
#43772=EDGE_CURVE('',#34838,#34839,#23586,.T.);
#43773=EDGE_CURVE('',#34840,#34839,#18208,.T.);
#43774=EDGE_CURVE('',#34840,#34841,#23587,.T.);
#43775=EDGE_CURVE('',#34841,#34842,#27139,.T.);
#43776=EDGE_CURVE('',#34842,#34843,#18209,.T.);
#43777=EDGE_CURVE('',#34843,#34844,#27140,.T.);
#43778=EDGE_CURVE('',#34844,#34845,#23588,.T.);
#43779=EDGE_CURVE('',#34846,#34845,#18210,.T.);
#43780=EDGE_CURVE('',#34846,#34847,#23589,.T.);
#43781=EDGE_CURVE('',#34847,#34788,#27141,.T.);
#43782=EDGE_CURVE('',#34848,#34849,#18211,.T.);
#43783=EDGE_CURVE('',#34850,#34848,#27142,.T.);
#43784=EDGE_CURVE('',#34851,#34850,#23590,.T.);
#43785=EDGE_CURVE('',#34852,#34851,#18212,.T.);
#43786=EDGE_CURVE('',#34853,#34852,#23591,.T.);
#43787=EDGE_CURVE('',#34854,#34853,#27143,.T.);
#43788=EDGE_CURVE('',#34855,#34854,#18213,.T.);
#43789=EDGE_CURVE('',#34856,#34855,#27144,.T.);
#43790=EDGE_CURVE('',#34857,#34856,#23592,.T.);
#43791=EDGE_CURVE('',#34858,#34857,#18214,.T.);
#43792=EDGE_CURVE('',#34859,#34858,#23593,.T.);
#43793=EDGE_CURVE('',#34860,#34859,#27145,.T.);
#43794=EDGE_CURVE('',#34861,#34860,#18215,.T.);
#43795=EDGE_CURVE('',#34862,#34861,#27146,.T.);
#43796=EDGE_CURVE('',#34863,#34862,#23594,.T.);
#43797=EDGE_CURVE('',#34864,#34863,#18216,.T.);
#43798=EDGE_CURVE('',#34865,#34864,#23595,.T.);
#43799=EDGE_CURVE('',#34866,#34865,#27147,.T.);
#43800=EDGE_CURVE('',#34867,#34866,#18217,.T.);
#43801=EDGE_CURVE('',#34868,#34867,#27148,.T.);
#43802=EDGE_CURVE('',#34869,#34868,#23596,.T.);
#43803=EDGE_CURVE('',#34870,#34869,#18218,.T.);
#43804=EDGE_CURVE('',#34871,#34870,#23597,.T.);
#43805=EDGE_CURVE('',#34872,#34871,#27149,.T.);
#43806=EDGE_CURVE('',#34873,#34872,#18219,.T.);
#43807=EDGE_CURVE('',#34874,#34873,#27150,.T.);
#43808=EDGE_CURVE('',#34875,#34874,#23598,.T.);
#43809=EDGE_CURVE('',#34876,#34875,#18220,.T.);
#43810=EDGE_CURVE('',#34877,#34876,#23599,.T.);
#43811=EDGE_CURVE('',#34878,#34877,#27151,.T.);
#43812=EDGE_CURVE('',#34879,#34878,#18221,.T.);
#43813=EDGE_CURVE('',#34880,#34879,#27152,.T.);
#43814=EDGE_CURVE('',#34881,#34880,#23600,.T.);
#43815=EDGE_CURVE('',#34882,#34881,#18222,.T.);
#43816=EDGE_CURVE('',#34883,#34882,#23601,.T.);
#43817=EDGE_CURVE('',#34884,#34883,#27153,.T.);
#43818=EDGE_CURVE('',#34885,#34884,#18223,.T.);
#43819=EDGE_CURVE('',#34886,#34885,#27154,.T.);
#43820=EDGE_CURVE('',#34887,#34886,#23602,.T.);
#43821=EDGE_CURVE('',#34888,#34887,#18224,.T.);
#43822=EDGE_CURVE('',#34889,#34888,#23603,.T.);
#43823=EDGE_CURVE('',#34890,#34889,#27155,.T.);
#43824=EDGE_CURVE('',#34891,#34890,#18225,.T.);
#43825=EDGE_CURVE('',#34892,#34891,#27156,.T.);
#43826=EDGE_CURVE('',#34893,#34892,#23604,.T.);
#43827=EDGE_CURVE('',#34894,#34893,#18226,.T.);
#43828=EDGE_CURVE('',#34895,#34894,#23605,.T.);
#43829=EDGE_CURVE('',#34896,#34895,#27157,.T.);
#43830=EDGE_CURVE('',#34897,#34896,#18227,.T.);
#43831=EDGE_CURVE('',#34898,#34897,#27158,.T.);
#43832=EDGE_CURVE('',#34899,#34898,#23606,.T.);
#43833=EDGE_CURVE('',#34900,#34899,#18228,.T.);
#43834=EDGE_CURVE('',#34901,#34900,#23607,.T.);
#43835=EDGE_CURVE('',#34902,#34901,#27159,.T.);
#43836=EDGE_CURVE('',#34903,#34902,#18229,.T.);
#43837=EDGE_CURVE('',#34904,#34903,#27160,.T.);
#43838=EDGE_CURVE('',#34905,#34904,#23608,.T.);
#43839=EDGE_CURVE('',#34906,#34905,#18230,.T.);
#43840=EDGE_CURVE('',#34907,#34906,#23609,.T.);
#43841=EDGE_CURVE('',#34849,#34907,#27161,.T.);
#43842=EDGE_CURVE('',#34908,#34908,#18231,.T.);
#43843=EDGE_CURVE('',#34849,#34843,#27162,.T.);
#43844=EDGE_CURVE('',#34907,#34844,#27163,.T.);
#43845=EDGE_CURVE('',#34845,#34906,#27164,.T.);
#43846=EDGE_CURVE('',#34905,#34846,#27165,.T.);
#43847=EDGE_CURVE('',#34904,#34847,#27166,.T.);
#43848=EDGE_CURVE('',#34788,#34903,#27167,.T.);
#43849=EDGE_CURVE('',#34842,#34848,#27168,.T.);
#43850=EDGE_CURVE('',#34902,#34789,#27169,.T.);
#43851=EDGE_CURVE('',#34854,#34837,#27170,.T.);
#43852=EDGE_CURVE('',#34853,#34838,#27171,.T.);
#43853=EDGE_CURVE('',#34839,#34852,#27172,.T.);
#43854=EDGE_CURVE('',#34851,#34840,#27173,.T.);
#43855=EDGE_CURVE('',#34850,#34841,#27174,.T.);
#43856=EDGE_CURVE('',#34836,#34855,#27175,.T.);
#43857=EDGE_CURVE('',#34860,#34831,#27176,.T.);
#43858=EDGE_CURVE('',#34859,#34832,#27177,.T.);
#43859=EDGE_CURVE('',#34833,#34858,#27178,.T.);
#43860=EDGE_CURVE('',#34857,#34834,#27179,.T.);
#43861=EDGE_CURVE('',#34856,#34835,#27180,.T.);
#43862=EDGE_CURVE('',#34830,#34861,#27181,.T.);
#43863=EDGE_CURVE('',#34866,#34825,#27182,.T.);
#43864=EDGE_CURVE('',#34865,#34826,#27183,.T.);
#43865=EDGE_CURVE('',#34827,#34864,#27184,.T.);
#43866=EDGE_CURVE('',#34863,#34828,#27185,.T.);
#43867=EDGE_CURVE('',#34862,#34829,#27186,.T.);
#43868=EDGE_CURVE('',#34824,#34867,#27187,.T.);
#43869=EDGE_CURVE('',#34872,#34819,#27188,.T.);
#43870=EDGE_CURVE('',#34871,#34820,#27189,.T.);
#43871=EDGE_CURVE('',#34821,#34870,#27190,.T.);
#43872=EDGE_CURVE('',#34869,#34822,#27191,.T.);
#43873=EDGE_CURVE('',#34868,#34823,#27192,.T.);
#43874=EDGE_CURVE('',#34818,#34873,#27193,.T.);
#43875=EDGE_CURVE('',#34878,#34813,#27194,.T.);
#43876=EDGE_CURVE('',#34877,#34814,#27195,.T.);
#43877=EDGE_CURVE('',#34815,#34876,#27196,.T.);
#43878=EDGE_CURVE('',#34875,#34816,#27197,.T.);
#43879=EDGE_CURVE('',#34874,#34817,#27198,.T.);
#43880=EDGE_CURVE('',#34812,#34879,#27199,.T.);
#43881=EDGE_CURVE('',#34884,#34807,#27200,.T.);
#43882=EDGE_CURVE('',#34883,#34808,#27201,.T.);
#43883=EDGE_CURVE('',#34809,#34882,#27202,.T.);
#43884=EDGE_CURVE('',#34881,#34810,#27203,.T.);
#43885=EDGE_CURVE('',#34880,#34811,#27204,.T.);
#43886=EDGE_CURVE('',#34806,#34885,#27205,.T.);
#43887=EDGE_CURVE('',#34890,#34801,#27206,.T.);
#43888=EDGE_CURVE('',#34889,#34802,#27207,.T.);
#43889=EDGE_CURVE('',#34803,#34888,#27208,.T.);
#43890=EDGE_CURVE('',#34887,#34804,#27209,.T.);
#43891=EDGE_CURVE('',#34886,#34805,#27210,.T.);
#43892=EDGE_CURVE('',#34800,#34891,#27211,.T.);
#43893=EDGE_CURVE('',#34896,#34795,#27212,.T.);
#43894=EDGE_CURVE('',#34895,#34796,#27213,.T.);
#43895=EDGE_CURVE('',#34797,#34894,#27214,.T.);
#43896=EDGE_CURVE('',#34893,#34798,#27215,.T.);
#43897=EDGE_CURVE('',#34892,#34799,#27216,.T.);
#43898=EDGE_CURVE('',#34794,#34897,#27217,.T.);
#43899=EDGE_CURVE('',#34901,#34790,#27218,.T.);
#43900=EDGE_CURVE('',#34791,#34900,#27219,.T.);
#43901=EDGE_CURVE('',#34899,#34792,#27220,.T.);
#43902=EDGE_CURVE('',#34898,#34793,#27221,.T.);
#43903=EDGE_CURVE('',#34909,#34910,#18232,.T.);
#43904=EDGE_CURVE('',#34910,#34911,#27222,.T.);
#43905=EDGE_CURVE('',#34911,#34911,#18233,.T.);
#43906=EDGE_CURVE('',#34910,#34909,#18234,.T.);
#43907=EDGE_CURVE('',#34912,#34913,#18235,.T.);
#43908=EDGE_CURVE('',#34913,#34911,#27223,.T.);
#43909=EDGE_CURVE('',#34913,#34912,#18236,.T.);
#43910=EDGE_CURVE('',#34909,#34914,#27224,.T.);
#43911=EDGE_CURVE('',#34915,#34914,#18237,.T.);
#43912=EDGE_CURVE('',#34914,#34915,#18238,.T.);
#43913=EDGE_CURVE('',#34752,#34912,#27225,.T.);
#43914=EDGE_CURVE('',#34916,#34917,#18239,.T.);
#43915=EDGE_CURVE('',#34917,#34918,#27226,.T.);
#43916=EDGE_CURVE('',#34918,#34918,#18240,.T.);
#43917=EDGE_CURVE('',#34917,#34916,#18241,.T.);
#43918=EDGE_CURVE('',#34915,#34918,#27227,.T.);
#43919=EDGE_CURVE('',#34916,#34919,#27228,.T.);
#43920=EDGE_CURVE('',#34920,#34919,#18242,.T.);
#43921=EDGE_CURVE('',#34919,#34920,#18243,.T.);
#43922=EDGE_CURVE('',#34921,#34922,#18244,.T.);
#43923=EDGE_CURVE('',#34922,#34923,#27229,.T.);
#43924=EDGE_CURVE('',#34923,#34923,#18245,.T.);
#43925=EDGE_CURVE('',#34922,#34921,#18246,.T.);
#43926=EDGE_CURVE('',#34920,#34923,#27230,.T.);
#43927=EDGE_CURVE('',#34921,#34924,#27231,.T.);
#43928=EDGE_CURVE('',#34925,#34924,#18247,.T.);
#43929=EDGE_CURVE('',#34924,#34925,#18248,.T.);
#43930=EDGE_CURVE('',#34926,#34927,#18249,.T.);
#43931=EDGE_CURVE('',#34927,#34928,#27232,.T.);
#43932=EDGE_CURVE('',#34928,#34928,#18250,.T.);
#43933=EDGE_CURVE('',#34927,#34926,#18251,.T.);
#43934=EDGE_CURVE('',#34925,#34928,#27233,.T.);
#43935=EDGE_CURVE('',#34926,#34929,#27234,.T.);
#43936=EDGE_CURVE('',#34930,#34929,#18252,.T.);
#43937=EDGE_CURVE('',#34929,#34930,#18253,.T.);
#43938=EDGE_CURVE('',#34931,#34932,#18254,.T.);
#43939=EDGE_CURVE('',#34932,#34933,#27235,.T.);
#43940=EDGE_CURVE('',#34933,#34933,#18255,.T.);
#43941=EDGE_CURVE('',#34932,#34931,#18256,.T.);
#43942=EDGE_CURVE('',#34930,#34933,#27236,.T.);
#43943=EDGE_CURVE('',#34931,#34934,#27237,.T.);
#43944=EDGE_CURVE('',#34935,#34934,#18257,.T.);
#43945=EDGE_CURVE('',#34934,#34935,#18258,.T.);
#43946=EDGE_CURVE('',#34936,#34937,#18259,.T.);
#43947=EDGE_CURVE('',#34937,#34938,#27238,.T.);
#43948=EDGE_CURVE('',#34938,#34938,#18260,.T.);
#43949=EDGE_CURVE('',#34937,#34936,#18261,.T.);
#43950=EDGE_CURVE('',#34935,#34938,#27239,.T.);
#43951=EDGE_CURVE('',#34936,#34939,#27240,.T.);
#43952=EDGE_CURVE('',#34940,#34939,#18262,.T.);
#43953=EDGE_CURVE('',#34939,#34940,#18263,.T.);
#43954=EDGE_CURVE('',#34941,#34942,#18264,.T.);
#43955=EDGE_CURVE('',#34942,#34943,#27241,.T.);
#43956=EDGE_CURVE('',#34943,#34943,#18265,.T.);
#43957=EDGE_CURVE('',#34942,#34941,#18266,.T.);
#43958=EDGE_CURVE('',#34940,#34943,#27242,.T.);
#43959=EDGE_CURVE('',#34941,#34944,#27243,.T.);
#43960=EDGE_CURVE('',#34945,#34944,#18267,.T.);
#43961=EDGE_CURVE('',#34944,#34945,#18268,.T.);
#43962=EDGE_CURVE('',#34946,#34947,#18269,.T.);
#43963=EDGE_CURVE('',#34947,#34948,#27244,.T.);
#43964=EDGE_CURVE('',#34948,#34948,#18270,.T.);
#43965=EDGE_CURVE('',#34947,#34946,#18271,.T.);
#43966=EDGE_CURVE('',#34945,#34948,#27245,.T.);
#43967=EDGE_CURVE('',#34946,#34949,#27246,.T.);
#43968=EDGE_CURVE('',#34950,#34949,#18272,.T.);
#43969=EDGE_CURVE('',#34949,#34950,#18273,.T.);
#43970=EDGE_CURVE('',#34951,#34952,#18274,.T.);
#43971=EDGE_CURVE('',#34952,#34953,#27247,.T.);
#43972=EDGE_CURVE('',#34953,#34953,#18275,.T.);
#43973=EDGE_CURVE('',#34952,#34951,#18276,.T.);
#43974=EDGE_CURVE('',#34950,#34953,#27248,.T.);
#43975=EDGE_CURVE('',#34951,#34954,#27249,.T.);
#43976=EDGE_CURVE('',#34955,#34954,#18277,.T.);
#43977=EDGE_CURVE('',#34954,#34955,#18278,.T.);
#43978=EDGE_CURVE('',#34956,#34957,#18279,.T.);
#43979=EDGE_CURVE('',#34957,#34958,#27250,.T.);
#43980=EDGE_CURVE('',#34958,#34958,#18280,.T.);
#43981=EDGE_CURVE('',#34957,#34956,#18281,.T.);
#43982=EDGE_CURVE('',#34955,#34958,#27251,.T.);
#43983=EDGE_CURVE('',#34956,#34959,#27252,.T.);
#43984=EDGE_CURVE('',#34960,#34959,#18282,.T.);
#43985=EDGE_CURVE('',#34959,#34960,#18283,.T.);
#43986=EDGE_CURVE('',#34961,#34962,#18284,.T.);
#43987=EDGE_CURVE('',#34962,#34963,#27253,.T.);
#43988=EDGE_CURVE('',#34963,#34963,#18285,.T.);
#43989=EDGE_CURVE('',#34962,#34961,#18286,.T.);
#43990=EDGE_CURVE('',#34960,#34963,#27254,.T.);
#43991=EDGE_CURVE('',#34961,#34964,#27255,.T.);
#43992=EDGE_CURVE('',#34965,#34964,#18287,.T.);
#43993=EDGE_CURVE('',#34964,#34965,#18288,.T.);
#43994=EDGE_CURVE('',#34966,#34967,#18289,.T.);
#43995=EDGE_CURVE('',#34967,#34968,#27256,.T.);
#43996=EDGE_CURVE('',#34968,#34968,#18290,.T.);
#43997=EDGE_CURVE('',#34967,#34966,#18291,.T.);
#43998=EDGE_CURVE('',#34965,#34968,#27257,.T.);
#43999=EDGE_CURVE('',#34966,#34969,#27258,.T.);
#44000=EDGE_CURVE('',#34970,#34969,#18292,.T.);
#44001=EDGE_CURVE('',#34969,#34970,#18293,.T.);
#44002=EDGE_CURVE('',#34971,#34972,#18294,.T.);
#44003=EDGE_CURVE('',#34972,#34973,#27259,.T.);
#44004=EDGE_CURVE('',#34973,#34973,#18295,.T.);
#44005=EDGE_CURVE('',#34972,#34971,#18296,.T.);
#44006=EDGE_CURVE('',#34970,#34973,#27260,.T.);
#44007=EDGE_CURVE('',#34971,#34974,#27261,.T.);
#44008=EDGE_CURVE('',#34975,#34974,#18297,.T.);
#44009=EDGE_CURVE('',#34974,#34975,#18298,.T.);
#44010=EDGE_CURVE('',#34976,#34977,#18299,.T.);
#44011=EDGE_CURVE('',#34977,#34978,#27262,.T.);
#44012=EDGE_CURVE('',#34978,#34978,#18300,.T.);
#44013=EDGE_CURVE('',#34977,#34976,#18301,.T.);
#44014=EDGE_CURVE('',#34975,#34978,#27263,.T.);
#44015=EDGE_CURVE('',#34976,#34979,#27264,.T.);
#44016=EDGE_CURVE('',#34979,#34980,#18302,.T.);
#44017=EDGE_CURVE('',#34980,#34979,#18303,.T.);
#44018=EDGE_CURVE('',#34981,#34982,#18304,.T.);
#44019=EDGE_CURVE('',#34982,#34981,#18305,.T.);
#44020=EDGE_CURVE('',#34982,#34983,#27265,.T.);
#44021=EDGE_CURVE('',#34983,#34983,#18306,.T.);
#44022=EDGE_CURVE('',#34980,#34983,#27266,.T.);
#44023=EDGE_CURVE('',#34981,#34747,#27267,.T.);
#44024=EDGE_CURVE('',#34735,#34908,#27268,.T.);
#44025=EDGE_CURVE('',#34984,#34985,#27269,.T.);
#44026=EDGE_CURVE('',#34984,#34986,#18307,.T.);
#44027=EDGE_CURVE('',#34987,#34986,#27270,.T.);
#44028=EDGE_CURVE('',#34985,#34987,#18308,.T.);
#44029=EDGE_CURVE('',#34988,#34989,#27271,.T.);
#44030=EDGE_CURVE('',#34990,#34988,#18309,.T.);
#44031=EDGE_CURVE('',#34991,#34990,#27272,.T.);
#44032=EDGE_CURVE('',#34991,#34989,#18310,.T.);
#44033=EDGE_CURVE('',#34992,#34993,#27273,.T.);
#44034=EDGE_CURVE('',#34994,#34992,#18311,.T.);
#44035=EDGE_CURVE('',#34995,#34994,#27274,.T.);
#44036=EDGE_CURVE('',#34995,#34993,#18312,.T.);
#44037=EDGE_CURVE('',#34996,#34984,#4073,.T.);
#44038=EDGE_CURVE('',#34996,#34997,#18313,.T.);
#44039=EDGE_CURVE('',#34986,#34997,#4074,.T.);
#44040=EDGE_CURVE('',#34989,#34998,#4075,.T.);
#44041=EDGE_CURVE('',#34999,#34991,#4076,.T.);
#44042=EDGE_CURVE('',#34999,#34998,#18314,.T.);
#44043=EDGE_CURVE('',#34993,#35000,#4077,.T.);
#44044=EDGE_CURVE('',#35001,#34995,#4078,.T.);
#44045=EDGE_CURVE('',#35001,#35000,#18315,.T.);
#44046=EDGE_CURVE('',#35002,#34996,#4079,.T.);
#44047=EDGE_CURVE('',#35002,#35003,#18316,.T.);
#44048=EDGE_CURVE('',#34997,#35003,#4080,.T.);
#44049=EDGE_CURVE('',#34998,#35004,#4081,.T.);
#44050=EDGE_CURVE('',#35005,#34999,#4082,.T.);
#44051=EDGE_CURVE('',#35005,#35004,#18317,.T.);
#44052=EDGE_CURVE('',#35000,#35006,#4083,.T.);
#44053=EDGE_CURVE('',#35007,#35001,#4084,.T.);
#44054=EDGE_CURVE('',#35007,#35006,#18318,.T.);
#44055=EDGE_CURVE('',#35008,#35002,#27275,.T.);
#44056=EDGE_CURVE('',#35008,#35009,#18319,.T.);
#44057=EDGE_CURVE('',#35003,#35009,#27276,.T.);
#44058=EDGE_CURVE('',#35004,#35010,#27277,.T.);
#44059=EDGE_CURVE('',#35011,#35005,#27278,.T.);
#44060=EDGE_CURVE('',#35011,#35010,#18320,.T.);
#44061=EDGE_CURVE('',#35006,#35012,#27279,.T.);
#44062=EDGE_CURVE('',#35013,#35007,#27280,.T.);
#44063=EDGE_CURVE('',#35013,#35012,#18321,.T.);
#44064=EDGE_CURVE('',#35014,#35014,#18322,.T.);
#44065=EDGE_CURVE('',#35014,#35015,#27281,.T.);
#44066=EDGE_CURVE('',#35015,#35016,#18323,.T.);
#44067=EDGE_CURVE('',#35016,#34994,#27282,.T.);
#44068=EDGE_CURVE('',#35017,#34992,#27283,.T.);
#44069=EDGE_CURVE('',#35017,#35018,#18324,.T.);
#44070=EDGE_CURVE('',#35018,#34990,#27284,.T.);
#44071=EDGE_CURVE('',#35019,#34988,#27285,.T.);
#44072=EDGE_CURVE('',#35019,#35020,#18325,.T.);
#44073=EDGE_CURVE('',#35020,#34985,#27286,.T.);
#44074=EDGE_CURVE('',#35021,#34987,#27287,.T.);
#44075=EDGE_CURVE('',#35021,#35022,#18326,.T.);
#44076=EDGE_CURVE('',#35022,#35023,#27288,.T.);
#44077=EDGE_CURVE('',#35023,#35024,#18327,.T.);
#44078=EDGE_CURVE('',#35025,#35024,#27289,.T.);
#44079=EDGE_CURVE('',#35025,#35015,#18328,.T.);
#44080=EDGE_CURVE('',#35026,#35023,#27290,.T.);
#44081=EDGE_CURVE('',#35026,#35027,#18329,.T.);
#44082=EDGE_CURVE('',#35024,#35027,#27291,.T.);
#44083=EDGE_CURVE('',#35028,#35026,#4085,.T.);
#44084=EDGE_CURVE('',#35028,#35029,#18330,.T.);
#44085=EDGE_CURVE('',#35027,#35029,#4086,.T.);
#44086=EDGE_CURVE('',#35030,#35028,#4087,.T.);
#44087=EDGE_CURVE('',#35030,#35031,#18331,.T.);
#44088=EDGE_CURVE('',#35029,#35031,#4088,.T.);
#44089=EDGE_CURVE('',#35032,#35030,#27292,.T.);
#44090=EDGE_CURVE('',#35032,#35033,#18332,.T.);
#44091=EDGE_CURVE('',#35031,#35033,#27293,.T.);
#44092=EDGE_CURVE('',#35034,#35035,#18333,.F.);
#44093=EDGE_CURVE('',#35035,#35036,#27294,.T.);
#44094=EDGE_CURVE('',#35036,#35036,#18334,.T.);
#44095=EDGE_CURVE('',#35035,#35037,#18335,.F.);
#44096=EDGE_CURVE('',#35033,#35037,#27295,.F.);
#44097=EDGE_CURVE('',#35038,#35032,#27296,.T.);
#44098=EDGE_CURVE('',#35038,#35039,#18336,.F.);
#44099=EDGE_CURVE('',#35009,#35039,#27297,.F.);
#44100=EDGE_CURVE('',#35040,#35008,#27298,.T.);
#44101=EDGE_CURVE('',#35040,#35041,#18337,.F.);
#44102=EDGE_CURVE('',#35010,#35041,#27299,.F.);
#44103=EDGE_CURVE('',#35042,#35011,#27300,.T.);
#44104=EDGE_CURVE('',#35042,#35043,#18338,.F.);
#44105=EDGE_CURVE('',#35012,#35043,#27301,.F.);
#44106=EDGE_CURVE('',#35034,#35013,#27302,.T.);
#44107=EDGE_CURVE('',#35044,#35044,#18339,.T.);
#44108=EDGE_CURVE('',#35044,#35045,#27303,.T.);
#44109=EDGE_CURVE('',#35045,#35045,#18340,.T.);
#44110=EDGE_CURVE('',#35037,#35025,#27304,.F.);
#44111=EDGE_CURVE('',#35016,#35034,#27305,.F.);
#44112=EDGE_CURVE('',#35039,#35021,#27306,.F.);
#44113=EDGE_CURVE('',#35022,#35038,#27307,.F.);
#44114=EDGE_CURVE('',#35018,#35042,#27308,.F.);
#44115=EDGE_CURVE('',#35043,#35017,#27309,.F.);
#44116=EDGE_CURVE('',#35020,#35040,#27310,.F.);
#44117=EDGE_CURVE('',#35041,#35019,#27311,.F.);
#44118=EDGE_CURVE('',#35046,#35047,#18341,.T.);
#44119=EDGE_CURVE('',#35047,#35048,#27312,.T.);
#44120=EDGE_CURVE('',#35048,#35049,#18342,.T.);
#44121=EDGE_CURVE('',#35049,#35046,#27313,.T.);
#44122=EDGE_CURVE('',#35049,#35050,#27314,.T.);
#44123=EDGE_CURVE('',#35051,#35050,#27315,.T.);
#44124=EDGE_CURVE('',#35046,#35051,#27316,.T.);
#44125=EDGE_CURVE('',#35048,#35052,#18343,.T.);
#44126=EDGE_CURVE('',#35053,#35052,#18344,.T.);
#44127=EDGE_CURVE('',#35053,#35054,#27317,.T.);
#44128=EDGE_CURVE('',#35055,#35054,#18345,.T.);
#44129=EDGE_CURVE('',#35056,#35055,#18346,.T.);
#44130=EDGE_CURVE('',#35057,#35056,#27318,.T.);
#44131=EDGE_CURVE('',#35057,#35058,#27319,.T.);
#44132=EDGE_CURVE('',#35058,#35059,#27320,.T.);
#44133=EDGE_CURVE('',#35060,#35059,#18347,.T.);
#44134=EDGE_CURVE('',#35050,#35060,#18348,.T.);
#44135=EDGE_CURVE('',#35061,#35051,#18349,.T.);
#44136=EDGE_CURVE('',#35060,#35061,#27321,.T.);
#44137=EDGE_CURVE('',#35059,#35062,#27322,.T.);
#44138=EDGE_CURVE('',#35061,#35062,#18350,.T.);
#44139=EDGE_CURVE('',#35063,#35064,#18351,.T.);
#44140=EDGE_CURVE('',#35064,#35053,#27323,.T.);
#44141=EDGE_CURVE('',#35052,#35063,#27324,.T.);
#44142=EDGE_CURVE('',#35063,#35047,#18352,.T.);
#44143=EDGE_CURVE('',#35065,#35066,#18353,.T.);
#44144=EDGE_CURVE('',#35066,#35055,#27325,.T.);
#44145=EDGE_CURVE('',#35054,#35065,#27326,.T.);
#44146=EDGE_CURVE('',#35067,#35066,#18354,.T.);
#44147=EDGE_CURVE('',#35056,#35067,#27327,.T.);
#44148=EDGE_CURVE('',#35057,#35068,#27328,.T.);
#44149=EDGE_CURVE('',#35069,#35068,#27329,.T.);
#44150=EDGE_CURVE('',#35058,#35069,#27330,.T.);
#44151=EDGE_CURVE('',#35068,#35070,#27331,.T.);
#44152=EDGE_CURVE('',#35070,#35071,#27332,.T.);
#44153=EDGE_CURVE('',#35071,#35069,#27333,.T.);
#44154=EDGE_CURVE('',#35072,#35070,#27334,.T.);
#44155=EDGE_CURVE('',#35073,#35072,#27335,.T.);
#44156=EDGE_CURVE('',#35071,#35073,#27336,.T.);
#44157=EDGE_CURVE('',#35062,#35073,#27337,.T.);
#44158=EDGE_CURVE('',#35065,#35064,#27338,.T.);
#44159=EDGE_CURVE('',#35072,#35067,#27339,.T.);
#44160=EDGE_CURVE('',#35074,#35075,#18355,.T.);
#44161=EDGE_CURVE('',#35075,#35076,#27340,.T.);
#44162=EDGE_CURVE('',#35076,#35077,#18356,.T.);
#44163=EDGE_CURVE('',#35077,#35074,#27341,.T.);
#44164=EDGE_CURVE('',#35078,#35079,#18357,.T.);
#44165=EDGE_CURVE('',#35079,#35077,#18358,.T.);
#44166=EDGE_CURVE('',#35076,#35078,#18359,.T.);
#44167=EDGE_CURVE('',#35080,#35081,#18360,.T.);
#44168=EDGE_CURVE('',#35081,#35079,#18361,.T.);
#44169=EDGE_CURVE('',#35078,#35080,#18362,.T.);
#44170=EDGE_CURVE('',#35082,#35083,#18363,.T.);
#44171=EDGE_CURVE('',#35083,#35081,#18364,.T.);
#44172=EDGE_CURVE('',#35080,#35082,#18365,.T.);
#44173=EDGE_CURVE('',#35084,#35085,#18366,.T.);
#44174=EDGE_CURVE('',#35085,#35083,#18367,.T.);
#44175=EDGE_CURVE('',#35082,#35084,#18368,.T.);
#44176=EDGE_CURVE('',#35086,#35087,#18369,.T.);
#44177=EDGE_CURVE('',#35087,#35085,#18370,.T.);
#44178=EDGE_CURVE('',#35084,#35086,#18371,.T.);
#44179=EDGE_CURVE('',#35088,#35089,#18372,.T.);
#44180=EDGE_CURVE('',#35089,#35087,#18373,.T.);
#44181=EDGE_CURVE('',#35086,#35088,#18374,.T.);
#44182=EDGE_CURVE('',#35090,#35091,#18375,.T.);
#44183=EDGE_CURVE('',#35091,#35089,#18376,.T.);
#44184=EDGE_CURVE('',#35088,#35090,#18377,.T.);
#44185=EDGE_CURVE('',#35092,#35093,#18378,.T.);
#44186=EDGE_CURVE('',#35093,#35091,#27342,.T.);
#44187=EDGE_CURVE('',#35090,#35092,#27343,.T.);
#44188=EDGE_CURVE('',#35074,#35093,#18379,.T.);
#44189=EDGE_CURVE('',#35092,#35075,#18380,.T.);
#44190=EDGE_CURVE('',#35094,#35089,#27344,.T.);
#44191=EDGE_CURVE('',#35094,#35095,#18381,.T.);
#44192=EDGE_CURVE('',#35096,#35095,#27345,.T.);
#44193=EDGE_CURVE('',#35096,#35097,#18382,.T.);
#44194=EDGE_CURVE('',#35098,#35097,#27346,.T.);
#44195=EDGE_CURVE('',#35099,#35098,#23610,.T.);
#44196=EDGE_CURVE('',#35100,#35099,#27347,.T.);
#44197=EDGE_CURVE('',#35101,#35100,#18383,.T.);
#44198=EDGE_CURVE('',#35087,#35101,#27348,.T.);
#44199=EDGE_CURVE('',#35091,#35102,#27349,.T.);
#44200=EDGE_CURVE('',#35102,#35094,#18384,.T.);
#44201=EDGE_CURVE('',#35103,#35093,#27350,.T.);
#44202=EDGE_CURVE('',#35102,#35103,#27351,.T.);
#44203=EDGE_CURVE('',#35074,#35104,#27352,.T.);
#44204=EDGE_CURVE('',#35104,#35103,#18385,.T.);
#44205=EDGE_CURVE('',#35105,#35077,#27353,.T.);
#44206=EDGE_CURVE('',#35104,#35105,#27354,.T.);
#44207=EDGE_CURVE('',#35106,#35107,#18386,.T.);
#44208=EDGE_CURVE('',#35107,#35108,#27355,.T.);
#44209=EDGE_CURVE('',#35108,#35109,#18387,.T.);
#44210=EDGE_CURVE('',#35109,#35106,#27356,.T.);
#44211=EDGE_CURVE('',#35110,#35111,#18388,.T.);
#44212=EDGE_CURVE('',#35111,#35109,#18389,.T.);
#44213=EDGE_CURVE('',#35108,#35110,#18390,.T.);
#44214=EDGE_CURVE('',#35112,#35113,#18391,.T.);
#44215=EDGE_CURVE('',#35113,#35111,#18392,.T.);
#44216=EDGE_CURVE('',#35110,#35112,#18393,.T.);
#44217=EDGE_CURVE('',#35114,#35115,#18394,.T.);
#44218=EDGE_CURVE('',#35115,#35113,#18395,.T.);
#44219=EDGE_CURVE('',#35112,#35114,#18396,.T.);
#44220=EDGE_CURVE('',#35116,#35117,#18397,.T.);
#44221=EDGE_CURVE('',#35117,#35115,#27357,.T.);
#44222=EDGE_CURVE('',#35114,#35116,#27358,.T.);
#44223=EDGE_CURVE('',#35118,#35119,#18398,.T.);
#44224=EDGE_CURVE('',#35119,#35117,#18399,.T.);
#44225=EDGE_CURVE('',#35116,#35118,#18400,.T.);
#44226=EDGE_CURVE('',#35120,#35121,#18401,.T.);
#44227=EDGE_CURVE('',#35121,#35119,#27359,.T.);
#44228=EDGE_CURVE('',#35118,#35120,#27360,.T.);
#44229=EDGE_CURVE('',#35122,#35123,#18402,.T.);
#44230=EDGE_CURVE('',#35123,#35121,#18403,.T.);
#44231=EDGE_CURVE('',#35120,#35122,#18404,.T.);
#44232=EDGE_CURVE('',#35124,#35125,#18405,.T.);
#44233=EDGE_CURVE('',#35125,#35123,#27361,.T.);
#44234=EDGE_CURVE('',#35122,#35124,#27362,.T.);
#44235=EDGE_CURVE('',#35126,#35127,#18406,.T.);
#44236=EDGE_CURVE('',#35127,#35125,#18407,.T.);
#44237=EDGE_CURVE('',#35124,#35126,#18408,.T.);
#44238=EDGE_CURVE('',#35128,#35129,#18409,.T.);
#44239=EDGE_CURVE('',#35129,#35127,#18410,.T.);
#44240=EDGE_CURVE('',#35126,#35128,#18411,.T.);
#44241=EDGE_CURVE('',#35130,#35131,#18412,.T.);
#44242=EDGE_CURVE('',#35131,#35129,#18413,.T.);
#44243=EDGE_CURVE('',#35128,#35130,#18414,.T.);
#44244=EDGE_CURVE('',#35132,#35133,#18415,.T.);
#44245=EDGE_CURVE('',#35133,#35134,#18416,.T.);
#44246=EDGE_CURVE('',#35134,#35131,#18417,.T.);
#44247=EDGE_CURVE('',#35130,#35132,#18418,.T.);
#44248=EDGE_CURVE('',#35106,#35133,#18419,.T.);
#44249=EDGE_CURVE('',#35132,#35107,#18420,.T.);
#44250=EDGE_CURVE('',#35135,#35125,#27363,.T.);
#44251=EDGE_CURVE('',#35135,#35136,#27364,.T.);
#44252=EDGE_CURVE('',#35123,#35136,#27365,.T.);
#44253=EDGE_CURVE('',#35127,#35137,#27366,.T.);
#44254=EDGE_CURVE('',#35135,#35137,#18421,.F.);
#44255=EDGE_CURVE('',#35138,#35129,#27367,.T.);
#44256=EDGE_CURVE('',#35138,#35137,#18422,.T.);
#44257=EDGE_CURVE('',#35131,#35139,#27368,.T.);
#44258=EDGE_CURVE('',#35139,#35138,#18423,.T.);
#44259=EDGE_CURVE('',#35140,#35140,#18424,.F.);
#44260=EDGE_CURVE('',#35140,#35134,#27369,.T.);
#44261=EDGE_CURVE('',#35141,#35133,#27370,.T.);
#44262=EDGE_CURVE('',#35141,#35142,#18425,.T.);
#44263=EDGE_CURVE('',#35143,#35142,#27371,.T.);
#44264=EDGE_CURVE('',#35144,#35143,#18426,.T.);
#44265=EDGE_CURVE('',#35145,#35144,#27372,.T.);
#44266=EDGE_CURVE('',#35145,#35146,#18427,.T.);
#44267=EDGE_CURVE('',#35147,#35146,#27373,.T.);
#44268=EDGE_CURVE('',#35148,#35147,#18428,.T.);
#44269=EDGE_CURVE('',#35149,#35148,#27374,.T.);
#44270=EDGE_CURVE('',#35149,#35139,#18429,.T.);
#44271=EDGE_CURVE('',#35106,#35150,#27375,.T.);
#44272=EDGE_CURVE('',#35150,#35141,#18430,.T.);
#44273=EDGE_CURVE('',#35151,#35109,#27376,.T.);
#44274=EDGE_CURVE('',#35151,#35150,#27377,.T.);
#44275=EDGE_CURVE('',#35152,#35153,#18431,.T.);
#44276=EDGE_CURVE('',#35153,#35154,#18432,.T.);
#44277=EDGE_CURVE('',#35154,#35155,#18433,.T.);
#44278=EDGE_CURVE('',#35155,#35152,#18434,.T.);
#44279=EDGE_CURVE('',#35156,#35157,#18435,.T.);
#44280=EDGE_CURVE('',#35157,#35155,#18436,.T.);
#44281=EDGE_CURVE('',#35154,#35156,#18437,.T.);
#44282=EDGE_CURVE('',#35158,#35159,#18438,.T.);
#44283=EDGE_CURVE('',#35159,#35157,#27378,.T.);
#44284=EDGE_CURVE('',#35156,#35158,#27379,.T.);
#44285=EDGE_CURVE('',#35160,#35161,#18439,.T.);
#44286=EDGE_CURVE('',#35161,#35159,#18440,.T.);
#44287=EDGE_CURVE('',#35158,#35160,#18441,.T.);
#44288=EDGE_CURVE('',#35162,#35163,#18442,.T.);
#44289=EDGE_CURVE('',#35163,#35161,#27380,.T.);
#44290=EDGE_CURVE('',#35160,#35162,#27381,.T.);
#44291=EDGE_CURVE('',#35164,#35165,#18443,.T.);
#44292=EDGE_CURVE('',#35165,#35163,#18444,.T.);
#44293=EDGE_CURVE('',#35162,#35164,#18445,.T.);
#44294=EDGE_CURVE('',#35166,#35167,#18446,.T.);
#44295=EDGE_CURVE('',#35167,#35165,#18447,.T.);
#44296=EDGE_CURVE('',#35164,#35166,#18448,.T.);
#44297=EDGE_CURVE('',#35168,#35169,#18449,.T.);
#44298=EDGE_CURVE('',#35169,#35167,#18450,.T.);
#44299=EDGE_CURVE('',#35166,#35168,#18451,.T.);
#44300=EDGE_CURVE('',#35170,#35171,#18452,.T.);
#44301=EDGE_CURVE('',#35171,#35169,#27382,.T.);
#44302=EDGE_CURVE('',#35168,#35170,#27383,.T.);
#44303=EDGE_CURVE('',#35172,#35143,#18453,.T.);
#44304=EDGE_CURVE('',#35143,#35171,#18454,.T.);
#44305=EDGE_CURVE('',#35170,#35172,#18455,.T.);
#44306=EDGE_CURVE('',#35173,#35144,#18456,.T.);
#44307=EDGE_CURVE('',#35172,#35173,#18457,.T.);
#44308=EDGE_CURVE('',#35152,#35144,#18458,.T.);
#44309=EDGE_CURVE('',#35173,#35153,#18459,.T.);
#44310=EDGE_CURVE('',#35169,#35174,#27384,.T.);
#44311=EDGE_CURVE('',#35174,#35175,#18460,.T.);
#44312=EDGE_CURVE('',#35175,#35176,#27385,.T.);
#44313=EDGE_CURVE('',#35176,#35177,#18461,.T.);
#44314=EDGE_CURVE('',#35177,#35167,#27386,.T.);
#44315=EDGE_CURVE('',#35178,#35171,#27387,.T.);
#44316=EDGE_CURVE('',#35178,#35174,#27388,.T.);
#44317=EDGE_CURVE('',#35142,#35178,#18462,.T.);
#44318=EDGE_CURVE('',#35152,#35179,#27389,.T.);
#44319=EDGE_CURVE('',#35179,#35145,#18463,.T.);
#44320=EDGE_CURVE('',#35180,#35155,#27390,.T.);
#44321=EDGE_CURVE('',#35180,#35179,#18464,.T.);
#44322=EDGE_CURVE('',#35181,#35182,#18465,.T.);
#44323=EDGE_CURVE('',#35182,#35183,#27391,.T.);
#44324=EDGE_CURVE('',#35183,#35184,#18466,.T.);
#44325=EDGE_CURVE('',#35184,#35181,#27392,.T.);
#44326=EDGE_CURVE('',#35185,#35186,#18467,.T.);
#44327=EDGE_CURVE('',#35186,#35184,#18468,.T.);
#44328=EDGE_CURVE('',#35183,#35185,#18469,.T.);
#44329=EDGE_CURVE('',#35187,#35188,#18470,.T.);
#44330=EDGE_CURVE('',#35188,#35186,#18471,.T.);
#44331=EDGE_CURVE('',#35185,#35187,#18472,.T.);
#44332=EDGE_CURVE('',#35189,#35190,#18473,.T.);
#44333=EDGE_CURVE('',#35190,#35188,#18474,.T.);
#44334=EDGE_CURVE('',#35187,#35189,#18475,.T.);
#44335=EDGE_CURVE('',#35191,#35192,#18476,.T.);
#44336=EDGE_CURVE('',#35192,#35190,#18477,.T.);
#44337=EDGE_CURVE('',#35189,#35191,#18478,.T.);
#44338=EDGE_CURVE('',#35193,#35194,#18479,.T.);
#44339=EDGE_CURVE('',#35194,#35192,#18480,.T.);
#44340=EDGE_CURVE('',#35191,#35193,#18481,.T.);
#44341=EDGE_CURVE('',#35195,#35196,#18482,.T.);
#44342=EDGE_CURVE('',#35196,#35194,#27393,.T.);
#44343=EDGE_CURVE('',#35193,#35195,#27394,.T.);
#44344=EDGE_CURVE('',#35197,#35198,#18483,.T.);
#44345=EDGE_CURVE('',#35198,#35196,#18484,.T.);
#44346=EDGE_CURVE('',#35195,#35197,#18485,.T.);
#44347=EDGE_CURVE('',#35199,#35200,#18486,.T.);
#44348=EDGE_CURVE('',#35200,#35198,#18487,.T.);
#44349=EDGE_CURVE('',#35197,#35199,#18488,.T.);
#44350=EDGE_CURVE('',#35201,#35202,#18489,.T.);
#44351=EDGE_CURVE('',#35202,#35200,#27395,.T.);
#44352=EDGE_CURVE('',#35199,#35201,#27396,.T.);
#44353=EDGE_CURVE('',#35181,#35202,#18490,.T.);
#44354=EDGE_CURVE('',#35201,#35182,#18491,.T.);
#44355=EDGE_CURVE('',#35203,#35196,#27397,.T.);
#44356=EDGE_CURVE('',#35204,#35203,#27398,.T.);
#44357=EDGE_CURVE('',#35204,#35205,#27399,.T.);
#44358=EDGE_CURVE('',#35205,#35206,#27400,.F.);
#44359=EDGE_CURVE('',#35206,#35194,#27401,.T.);
#44360=EDGE_CURVE('',#35207,#35198,#27402,.T.);
#44361=EDGE_CURVE('',#35203,#35207,#18492,.T.);
#44362=EDGE_CURVE('',#35200,#35208,#27403,.T.);
#44363=EDGE_CURVE('',#35208,#35207,#18493,.T.);
#44364=EDGE_CURVE('',#35209,#35202,#27404,.T.);
#44365=EDGE_CURVE('',#35208,#35209,#27405,.T.);
#44366=EDGE_CURVE('',#35181,#35210,#27406,.T.);
#44367=EDGE_CURVE('',#35210,#35209,#18494,.T.);
#44368=EDGE_CURVE('',#35211,#35184,#27407,.T.);
#44369=EDGE_CURVE('',#35211,#35212,#27408,.T.);
#44370=EDGE_CURVE('',#35213,#35212,#27409,.T.);
#44371=EDGE_CURVE('',#35210,#35213,#27410,.T.);
#44372=EDGE_CURVE('',#35214,#35215,#18495,.T.);
#44373=EDGE_CURVE('',#35215,#35216,#18496,.T.);
#44374=EDGE_CURVE('',#35216,#35217,#18497,.T.);
#44375=EDGE_CURVE('',#35217,#35214,#18498,.T.);
#44376=EDGE_CURVE('',#35218,#35219,#18499,.T.);
#44377=EDGE_CURVE('',#35219,#35217,#18500,.T.);
#44378=EDGE_CURVE('',#35216,#35218,#18501,.T.);
#44379=EDGE_CURVE('',#35220,#35221,#18502,.T.);
#44380=EDGE_CURVE('',#35221,#35219,#18503,.T.);
#44381=EDGE_CURVE('',#35218,#35220,#18504,.T.);
#44382=EDGE_CURVE('',#35222,#35223,#18505,.T.);
#44383=EDGE_CURVE('',#35223,#35221,#18506,.T.);
#44384=EDGE_CURVE('',#35220,#35222,#18507,.T.);
#44385=EDGE_CURVE('',#35224,#35225,#18508,.T.);
#44386=EDGE_CURVE('',#35225,#35223,#18509,.T.);
#44387=EDGE_CURVE('',#35222,#35224,#18510,.T.);
#44388=EDGE_CURVE('',#35226,#35227,#18511,.T.);
#44389=EDGE_CURVE('',#35227,#35225,#27411,.T.);
#44390=EDGE_CURVE('',#35224,#35226,#27412,.T.);
#44391=EDGE_CURVE('',#35228,#35229,#18512,.T.);
#44392=EDGE_CURVE('',#35229,#35227,#18513,.T.);
#44393=EDGE_CURVE('',#35226,#35228,#18514,.T.);
#44394=EDGE_CURVE('',#35230,#35231,#18515,.T.);
#44395=EDGE_CURVE('',#35231,#35229,#27413,.T.);
#44396=EDGE_CURVE('',#35228,#35230,#27414,.T.);
#44397=EDGE_CURVE('',#35232,#35233,#18516,.T.);
#44398=EDGE_CURVE('',#35233,#35231,#18517,.T.);
#44399=EDGE_CURVE('',#35230,#35232,#18518,.T.);
#44400=EDGE_CURVE('',#35234,#35235,#18519,.T.);
#44401=EDGE_CURVE('',#35235,#35233,#27415,.T.);
#44402=EDGE_CURVE('',#35232,#35234,#27416,.T.);
#44403=EDGE_CURVE('',#35236,#35237,#18520,.T.);
#44404=EDGE_CURVE('',#35237,#35235,#18521,.T.);
#44405=EDGE_CURVE('',#35234,#35236,#18522,.T.);
#44406=EDGE_CURVE('',#35238,#35239,#18523,.T.);
#44407=EDGE_CURVE('',#35239,#35237,#18524,.T.);
#44408=EDGE_CURVE('',#35236,#35238,#18525,.T.);
#44409=EDGE_CURVE('',#35240,#35241,#18526,.T.);
#44410=EDGE_CURVE('',#35241,#35239,#18527,.T.);
#44411=EDGE_CURVE('',#35238,#35240,#18528,.T.);
#44412=EDGE_CURVE('',#35214,#35241,#27417,.T.);
#44413=EDGE_CURVE('',#35240,#35215,#27418,.T.);
#44414=EDGE_CURVE('',#35233,#35242,#27419,.T.);
#44415=EDGE_CURVE('',#35242,#35243,#18529,.T.);
#44416=EDGE_CURVE('',#35243,#35231,#27420,.T.);
#44417=EDGE_CURVE('',#35244,#35235,#27421,.T.);
#44418=EDGE_CURVE('',#35242,#35244,#27422,.T.);
#44419=EDGE_CURVE('',#35237,#35245,#27423,.T.);
#44420=EDGE_CURVE('',#35245,#35244,#18530,.T.);
#44421=EDGE_CURVE('',#35246,#35239,#27424,.T.);
#44422=EDGE_CURVE('',#35245,#35246,#18531,.T.);
#44423=EDGE_CURVE('',#35241,#35247,#27425,.T.);
#44424=EDGE_CURVE('',#35247,#35246,#18532,.T.);
#44425=EDGE_CURVE('',#35248,#35214,#27426,.T.);
#44426=EDGE_CURVE('',#35248,#35247,#27427,.T.);
#44427=EDGE_CURVE('',#35249,#35217,#27428,.T.);
#44428=EDGE_CURVE('',#35249,#35248,#18533,.T.);
#44429=EDGE_CURVE('',#35250,#35251,#18534,.T.);
#44430=EDGE_CURVE('',#35251,#35252,#18535,.T.);
#44431=EDGE_CURVE('',#35252,#35253,#18536,.T.);
#44432=EDGE_CURVE('',#35253,#35250,#18537,.T.);
#44433=EDGE_CURVE('',#35254,#35255,#18538,.T.);
#44434=EDGE_CURVE('',#35255,#35253,#18539,.T.);
#44435=EDGE_CURVE('',#35252,#35254,#18540,.T.);
#44436=EDGE_CURVE('',#35256,#35257,#18541,.T.);
#44437=EDGE_CURVE('',#35257,#35255,#18542,.T.);
#44438=EDGE_CURVE('',#35254,#35256,#18543,.T.);
#44439=EDGE_CURVE('',#35258,#35259,#18544,.T.);
#44440=EDGE_CURVE('',#35259,#35257,#18545,.T.);
#44441=EDGE_CURVE('',#35256,#35258,#18546,.T.);
#44442=EDGE_CURVE('',#35260,#35261,#18547,.T.);
#44443=EDGE_CURVE('',#35261,#35259,#18548,.T.);
#44444=EDGE_CURVE('',#35258,#35260,#18549,.T.);
#44445=EDGE_CURVE('',#35262,#35263,#18550,.T.);
#44446=EDGE_CURVE('',#35263,#35261,#18551,.T.);
#44447=EDGE_CURVE('',#35260,#35262,#18552,.T.);
#44448=EDGE_CURVE('',#35264,#35265,#18553,.T.);
#44449=EDGE_CURVE('',#35265,#35263,#18554,.T.);
#44450=EDGE_CURVE('',#35262,#35264,#18555,.T.);
#44451=EDGE_CURVE('',#35266,#35267,#18556,.T.);
#44452=EDGE_CURVE('',#35267,#35265,#27429,.T.);
#44453=EDGE_CURVE('',#35264,#35266,#27430,.T.);
#44454=EDGE_CURVE('',#35250,#35267,#18557,.T.);
#44455=EDGE_CURVE('',#35266,#35251,#18558,.T.);
#44456=EDGE_CURVE('',#35268,#35263,#27431,.T.);
#44457=EDGE_CURVE('',#35268,#35269,#18559,.T.);
#44458=EDGE_CURVE('',#35261,#35269,#27432,.T.);
#44459=EDGE_CURVE('',#35265,#35270,#27433,.T.);
#44460=EDGE_CURVE('',#35270,#35268,#18560,.T.);
#44461=EDGE_CURVE('',#35271,#35267,#27434,.T.);
#44462=EDGE_CURVE('',#35270,#35271,#27435,.T.);
#44463=EDGE_CURVE('',#35250,#35272,#27436,.T.);
#44464=EDGE_CURVE('',#35271,#35272,#18561,.F.);
#44465=EDGE_CURVE('',#35273,#35253,#27437,.T.);
#44466=EDGE_CURVE('',#35272,#35273,#18562,.T.);
#44467=EDGE_CURVE('',#35274,#35275,#18563,.T.);
#44468=EDGE_CURVE('',#35275,#35276,#18564,.T.);
#44469=EDGE_CURVE('',#35276,#35277,#18565,.T.);
#44470=EDGE_CURVE('',#35277,#35274,#18566,.T.);
#44471=EDGE_CURVE('',#35278,#35279,#18567,.T.);
#44472=EDGE_CURVE('',#35279,#35277,#18568,.T.);
#44473=EDGE_CURVE('',#35276,#35278,#18569,.T.);
#44474=EDGE_CURVE('',#35280,#35281,#18570,.T.);
#44475=EDGE_CURVE('',#35281,#35279,#18571,.T.);
#44476=EDGE_CURVE('',#35278,#35280,#18572,.T.);
#44477=EDGE_CURVE('',#35282,#35283,#18573,.T.);
#44478=EDGE_CURVE('',#35283,#35281,#18574,.T.);
#44479=EDGE_CURVE('',#35280,#35282,#18575,.T.);
#44480=EDGE_CURVE('',#35284,#35285,#18576,.T.);
#44481=EDGE_CURVE('',#35285,#35283,#18577,.T.);
#44482=EDGE_CURVE('',#35282,#35284,#18578,.T.);
#44483=EDGE_CURVE('',#35286,#35287,#18579,.T.);
#44484=EDGE_CURVE('',#35287,#35285,#18580,.T.);
#44485=EDGE_CURVE('',#35284,#35286,#18581,.T.);
#44486=EDGE_CURVE('',#35288,#35289,#18582,.T.);
#44487=EDGE_CURVE('',#35289,#35287,#27438,.T.);
#44488=EDGE_CURVE('',#35286,#35288,#27439,.T.);
#44489=EDGE_CURVE('',#35290,#35291,#18583,.T.);
#44490=EDGE_CURVE('',#35291,#35289,#18584,.T.);
#44491=EDGE_CURVE('',#35288,#35290,#18585,.T.);
#44492=EDGE_CURVE('',#35292,#35293,#18586,.T.);
#44493=EDGE_CURVE('',#35293,#35291,#27440,.T.);
#44494=EDGE_CURVE('',#35290,#35292,#27441,.T.);
#44495=EDGE_CURVE('',#35294,#35295,#18587,.T.);
#44496=EDGE_CURVE('',#35295,#35293,#18588,.T.);
#44497=EDGE_CURVE('',#35292,#35294,#18589,.T.);
#44498=EDGE_CURVE('',#35296,#35297,#18590,.T.);
#44499=EDGE_CURVE('',#35297,#35295,#27442,.T.);
#44500=EDGE_CURVE('',#35294,#35296,#27443,.T.);
#44501=EDGE_CURVE('',#35298,#35299,#18591,.T.);
#44502=EDGE_CURVE('',#35299,#35297,#18592,.T.);
#44503=EDGE_CURVE('',#35296,#35298,#18593,.T.);
#44504=EDGE_CURVE('',#35300,#35301,#18594,.T.);
#44505=EDGE_CURVE('',#35301,#35299,#18595,.T.);
#44506=EDGE_CURVE('',#35298,#35300,#18596,.T.);
#44507=EDGE_CURVE('',#35302,#35303,#18597,.T.);
#44508=EDGE_CURVE('',#35303,#35301,#18598,.T.);
#44509=EDGE_CURVE('',#35300,#35302,#18599,.T.);
#44510=EDGE_CURVE('',#35304,#35305,#18600,.T.);
#44511=EDGE_CURVE('',#35305,#35303,#18601,.T.);
#44512=EDGE_CURVE('',#35302,#35304,#18602,.T.);
#44513=EDGE_CURVE('',#35274,#35305,#18603,.T.);
#44514=EDGE_CURVE('',#35304,#35275,#18604,.T.);
#44515=EDGE_CURVE('',#35295,#35306,#27444,.T.);
#44516=EDGE_CURVE('',#35306,#35307,#18605,.T.);
#44517=EDGE_CURVE('',#35307,#35293,#27445,.T.);
#44518=EDGE_CURVE('',#35308,#35297,#27446,.T.);
#44519=EDGE_CURVE('',#35306,#35308,#27447,.T.);
#44520=EDGE_CURVE('',#35299,#35309,#27448,.T.);
#44521=EDGE_CURVE('',#35309,#35308,#18606,.T.);
#44522=EDGE_CURVE('',#35310,#35301,#27449,.T.);
#44523=EDGE_CURVE('',#35309,#35310,#18607,.T.);
#44524=EDGE_CURVE('',#35303,#35311,#27450,.T.);
#44525=EDGE_CURVE('',#35311,#35310,#18608,.T.);
#44526=EDGE_CURVE('',#35312,#35305,#27451,.T.);
#44527=EDGE_CURVE('',#35312,#35311,#18609,.F.);
#44528=EDGE_CURVE('',#35274,#35313,#27452,.T.);
#44529=EDGE_CURVE('',#35313,#35312,#18610,.T.);
#44530=EDGE_CURVE('',#35314,#35277,#27453,.T.);
#44531=EDGE_CURVE('',#35315,#35314,#18611,.T.);
#44532=EDGE_CURVE('',#35316,#35315,#27454,.T.);
#44533=EDGE_CURVE('',#35316,#35313,#18612,.T.);
#44534=EDGE_CURVE('',#35317,#35318,#18613,.T.);
#44535=EDGE_CURVE('',#35318,#35319,#18614,.T.);
#44536=EDGE_CURVE('',#35319,#35320,#18615,.T.);
#44537=EDGE_CURVE('',#35320,#35317,#18616,.T.);
#44538=EDGE_CURVE('',#35321,#35322,#18617,.T.);
#44539=EDGE_CURVE('',#35322,#35320,#18618,.T.);
#44540=EDGE_CURVE('',#35319,#35321,#18619,.T.);
#44541=EDGE_CURVE('',#35323,#35324,#18620,.T.);
#44542=EDGE_CURVE('',#35324,#35322,#18621,.T.);
#44543=EDGE_CURVE('',#35321,#35323,#18622,.T.);
#44544=EDGE_CURVE('',#35325,#35326,#18623,.T.);
#44545=EDGE_CURVE('',#35326,#35324,#27455,.T.);
#44546=EDGE_CURVE('',#35323,#35325,#27456,.T.);
#44547=EDGE_CURVE('',#35327,#35328,#18624,.T.);
#44548=EDGE_CURVE('',#35328,#35326,#18625,.T.);
#44549=EDGE_CURVE('',#35325,#35327,#18626,.T.);
#44550=EDGE_CURVE('',#35329,#35330,#18627,.T.);
#44551=EDGE_CURVE('',#35330,#35328,#18628,.T.);
#44552=EDGE_CURVE('',#35327,#35329,#18629,.T.);
#44553=EDGE_CURVE('',#35331,#35332,#18630,.T.);
#44554=EDGE_CURVE('',#35332,#35330,#18631,.T.);
#44555=EDGE_CURVE('',#35329,#35331,#18632,.T.);
#44556=EDGE_CURVE('',#35333,#35334,#18633,.T.);
#44557=EDGE_CURVE('',#35334,#35332,#18634,.T.);
#44558=EDGE_CURVE('',#35331,#35333,#18635,.T.);
#44559=EDGE_CURVE('',#35317,#35334,#18636,.T.);
#44560=EDGE_CURVE('',#35333,#35318,#18637,.T.);
#44561=EDGE_CURVE('',#35335,#35330,#27457,.T.);
#44562=EDGE_CURVE('',#35336,#35335,#18638,.T.);
#44563=EDGE_CURVE('',#35337,#35336,#27458,.T.);
#44564=EDGE_CURVE('',#35338,#35337,#18639,.T.);
#44565=EDGE_CURVE('',#35339,#35338,#27459,.T.);
#44566=EDGE_CURVE('',#35340,#35339,#18640,.T.);
#44567=EDGE_CURVE('',#35328,#35340,#27460,.T.);
#44568=EDGE_CURVE('',#35332,#35341,#27461,.T.);
#44569=EDGE_CURVE('',#35341,#35335,#18641,.T.);
#44570=EDGE_CURVE('',#35342,#35334,#27462,.T.);
#44571=EDGE_CURVE('',#35341,#35342,#18642,.T.);
#44572=EDGE_CURVE('',#35317,#35343,#27463,.T.);
#44573=EDGE_CURVE('',#35343,#35342,#18643,.T.);
#44574=EDGE_CURVE('',#35344,#35320,#27464,.T.);
#44575=EDGE_CURVE('',#35343,#35344,#18644,.T.);
#44576=EDGE_CURVE('',#35345,#35346,#18645,.T.);
#44577=EDGE_CURVE('',#35346,#35347,#27465,.T.);
#44578=EDGE_CURVE('',#35347,#35348,#18646,.T.);
#44579=EDGE_CURVE('',#35348,#35345,#27466,.T.);
#44580=EDGE_CURVE('',#35349,#35350,#18647,.T.);
#44581=EDGE_CURVE('',#35350,#35348,#18648,.T.);
#44582=EDGE_CURVE('',#35347,#35349,#18649,.T.);
#44583=EDGE_CURVE('',#35351,#35352,#18650,.T.);
#44584=EDGE_CURVE('',#35352,#35350,#27467,.T.);
#44585=EDGE_CURVE('',#35349,#35351,#27468,.T.);
#44586=EDGE_CURVE('',#35353,#35354,#18651,.T.);
#44587=EDGE_CURVE('',#35354,#35352,#18652,.T.);
#44588=EDGE_CURVE('',#35351,#35353,#18653,.T.);
#44589=EDGE_CURVE('',#35355,#35356,#18654,.T.);
#44590=EDGE_CURVE('',#35356,#35354,#18655,.T.);
#44591=EDGE_CURVE('',#35353,#35355,#18656,.T.);
#44592=EDGE_CURVE('',#35357,#35358,#18657,.T.);
#44593=EDGE_CURVE('',#35358,#35356,#18658,.T.);
#44594=EDGE_CURVE('',#35355,#35357,#18659,.T.);
#44595=EDGE_CURVE('',#35359,#35360,#18660,.T.);
#44596=EDGE_CURVE('',#35360,#35358,#18661,.T.);
#44597=EDGE_CURVE('',#35357,#35359,#18662,.T.);
#44598=EDGE_CURVE('',#35345,#35360,#18663,.T.);
#44599=EDGE_CURVE('',#35359,#35346,#18664,.T.);
#44600=EDGE_CURVE('',#35358,#35361,#27469,.T.);
#44601=EDGE_CURVE('',#35361,#35362,#18665,.T.);
#44602=EDGE_CURVE('',#35362,#35356,#27470,.T.);
#44603=EDGE_CURVE('',#35363,#35360,#27471,.T.);
#44604=EDGE_CURVE('',#35361,#35363,#18666,.T.);
#44605=EDGE_CURVE('',#35345,#35364,#27472,.T.);
#44606=EDGE_CURVE('',#35364,#35363,#18667,.T.);
#44607=EDGE_CURVE('',#35365,#35348,#27473,.T.);
#44608=EDGE_CURVE('',#35364,#35365,#27474,.T.);
#44609=EDGE_CURVE('',#35366,#35367,#23611,.T.);
#44610=EDGE_CURVE('',#35367,#35368,#23612,.T.);
#44611=EDGE_CURVE('',#35368,#35369,#18668,.T.);
#44612=EDGE_CURVE('',#35369,#35366,#23613,.T.);
#44613=EDGE_CURVE('',#35099,#35370,#18669,.T.);
#44614=EDGE_CURVE('',#35370,#35369,#23614,.T.);
#44615=EDGE_CURVE('',#35368,#35099,#23615,.T.);
#44616=EDGE_CURVE('',#35098,#35371,#23616,.T.);
#44617=EDGE_CURVE('',#35371,#35370,#23617,.T.);
#44618=EDGE_CURVE('',#35368,#35372,#27475,.T.);
#44619=EDGE_CURVE('',#35372,#35100,#18670,.F.);
#44620=EDGE_CURVE('',#35373,#35367,#27476,.T.);
#44621=EDGE_CURVE('',#35373,#35374,#18671,.T.);
#44622=EDGE_CURVE('',#35375,#35374,#27477,.T.);
#44623=EDGE_CURVE('',#35375,#35376,#18672,.T.);
#44624=EDGE_CURVE('',#35376,#35377,#23618,.T.);
#44625=EDGE_CURVE('',#35378,#35377,#18673,.T.);
#44626=EDGE_CURVE('',#35379,#35378,#23619,.T.);
#44627=EDGE_CURVE('',#35380,#35379,#18674,.T.);
#44628=EDGE_CURVE('',#35381,#35380,#27478,.T.);
#44629=EDGE_CURVE('',#35382,#35381,#18675,.T.);
#44630=EDGE_CURVE('',#35383,#35382,#27479,.T.);
#44631=EDGE_CURVE('',#35384,#35383,#18676,.F.);
#44632=EDGE_CURVE('',#35384,#35385,#27480,.T.);
#44633=EDGE_CURVE('',#35385,#35385,#18677,.F.);
#44634=EDGE_CURVE('',#35372,#35384,#18678,.F.);
#44635=EDGE_CURVE('',#35371,#35148,#23620,.F.);
#44636=EDGE_CURVE('',#35366,#35147,#23621,.T.);
#44637=EDGE_CURVE('',#35386,#35096,#18679,.T.);
#44638=EDGE_CURVE('',#35095,#35387,#18680,.F.);
#44639=EDGE_CURVE('',#35387,#35386,#27481,.T.);
#44640=EDGE_CURVE('',#35386,#35388,#27482,.T.);
#44641=EDGE_CURVE('',#35389,#35388,#18681,.T.);
#44642=EDGE_CURVE('',#35390,#35389,#27483,.T.);
#44643=EDGE_CURVE('',#35391,#35390,#27484,.T.);
#44644=EDGE_CURVE('',#35392,#35391,#27485,.T.);
#44645=EDGE_CURVE('',#35136,#35392,#18682,.T.);
#44646=EDGE_CURVE('',#35097,#35149,#18683,.T.);
#44647=EDGE_CURVE('',#35393,#35387,#27486,.T.);
#44648=EDGE_CURVE('',#35394,#35393,#27487,.T.);
#44649=EDGE_CURVE('',#35395,#35394,#27488,.T.);
#44650=EDGE_CURVE('',#35388,#35395,#27489,.T.);
#44651=EDGE_CURVE('',#35396,#35397,#18684,.T.);
#44652=EDGE_CURVE('',#35397,#35398,#27490,.T.);
#44653=EDGE_CURVE('',#35398,#35399,#18685,.F.);
#44654=EDGE_CURVE('',#35399,#35396,#27491,.T.);
#44655=EDGE_CURVE('',#35396,#35400,#18686,.T.);
#44656=EDGE_CURVE('',#35400,#35401,#27492,.T.);
#44657=EDGE_CURVE('',#35401,#35402,#18687,.T.);
#44658=EDGE_CURVE('',#35402,#35204,#27493,.T.);
#44659=EDGE_CURVE('',#35213,#35403,#18688,.T.);
#44660=EDGE_CURVE('',#35403,#35404,#27494,.T.);
#44661=EDGE_CURVE('',#35405,#35404,#18689,.T.);
#44662=EDGE_CURVE('',#35405,#35406,#27495,.T.);
#44663=EDGE_CURVE('',#35407,#35406,#18690,.T.);
#44664=EDGE_CURVE('',#35407,#35177,#18691,.T.);
#44665=EDGE_CURVE('',#35176,#35408,#18692,.T.);
#44666=EDGE_CURVE('',#35408,#35409,#18693,.T.);
#44667=EDGE_CURVE('',#35410,#35409,#18694,.T.);
#44668=EDGE_CURVE('',#35410,#35411,#18695,.T.);
#44669=EDGE_CURVE('',#35412,#35411,#18696,.T.);
#44670=EDGE_CURVE('',#35412,#35413,#27496,.T.);
#44671=EDGE_CURVE('',#35414,#35413,#18697,.T.);
#44672=EDGE_CURVE('',#35414,#35415,#27497,.T.);
#44673=EDGE_CURVE('',#35415,#35416,#27498,.T.);
#44674=EDGE_CURVE('',#35416,#35417,#27499,.T.);
#44675=EDGE_CURVE('',#35418,#35417,#18698,.T.);
#44676=EDGE_CURVE('',#35418,#35419,#27500,.T.);
#44677=EDGE_CURVE('',#35419,#35420,#18699,.T.);
#44678=EDGE_CURVE('',#35420,#35397,#27501,.T.);
#44679=EDGE_CURVE('',#35421,#35421,#18700,.T.);
#44680=EDGE_CURVE('',#35399,#35422,#18701,.T.);
#44681=EDGE_CURVE('',#35400,#35422,#27502,.T.);
#44682=EDGE_CURVE('',#35423,#35398,#27503,.T.);
#44683=EDGE_CURVE('',#35424,#35423,#18702,.T.);
#44684=EDGE_CURVE('',#35425,#35424,#27504,.T.);
#44685=EDGE_CURVE('',#35426,#35425,#18703,.T.);
#44686=EDGE_CURVE('',#35426,#35427,#27505,.T.);
#44687=EDGE_CURVE('',#35428,#35427,#18704,.T.);
#44688=EDGE_CURVE('',#35428,#35429,#27506,.T.);
#44689=EDGE_CURVE('',#35430,#35429,#18705,.T.);
#44690=EDGE_CURVE('',#35376,#35430,#18706,.T.);
#44691=EDGE_CURVE('',#35212,#35375,#18707,.F.);
#44692=EDGE_CURVE('',#35431,#35211,#18708,.T.);
#44693=EDGE_CURVE('',#35432,#35431,#18709,.T.);
#44694=EDGE_CURVE('',#35433,#35432,#18710,.T.);
#44695=EDGE_CURVE('',#35434,#35433,#18711,.F.);
#44696=EDGE_CURVE('',#35206,#35434,#18712,.F.);
#44697=EDGE_CURVE('',#35435,#35205,#27507,.T.);
#44698=EDGE_CURVE('',#35436,#35435,#18713,.T.);
#44699=EDGE_CURVE('',#35422,#35436,#27508,.T.);
#44700=EDGE_CURVE('',#35437,#35438,#18714,.T.);
#44701=EDGE_CURVE('',#35437,#35243,#27509,.T.);
#44702=EDGE_CURVE('',#35439,#35249,#18715,.T.);
#44703=EDGE_CURVE('',#35439,#35440,#18716,.T.);
#44704=EDGE_CURVE('',#35440,#35441,#18717,.T.);
#44705=EDGE_CURVE('',#35442,#35441,#18718,.T.);
#44706=EDGE_CURVE('',#35442,#35438,#27510,.T.);
#44707=EDGE_CURVE('',#35443,#35443,#18719,.T.);
#44708=EDGE_CURVE('',#35444,#35420,#27511,.T.);
#44709=EDGE_CURVE('',#35444,#35445,#27512,.T.);
#44710=EDGE_CURVE('',#35423,#35445,#27513,.T.);
#44711=EDGE_CURVE('',#35425,#35446,#27514,.T.);
#44712=EDGE_CURVE('',#35446,#35447,#18720,.T.);
#44713=EDGE_CURVE('',#35447,#35426,#27515,.T.);
#44714=EDGE_CURVE('',#35448,#35447,#27516,.T.);
#44715=EDGE_CURVE('',#35427,#35448,#27517,.T.);
#44716=EDGE_CURVE('',#35449,#35446,#27518,.T.);
#44717=EDGE_CURVE('',#35445,#35449,#18721,.T.);
#44718=EDGE_CURVE('',#35450,#35444,#18722,.T.);
#44719=EDGE_CURVE('',#35450,#35451,#27519,.T.);
#44720=EDGE_CURVE('',#35452,#35451,#18723,.T.);
#44721=EDGE_CURVE('',#35452,#35453,#27520,.T.);
#44722=EDGE_CURVE('',#35395,#35453,#18724,.T.);
#44723=EDGE_CURVE('',#35454,#35394,#18725,.T.);
#44724=EDGE_CURVE('',#35454,#35455,#27521,.T.);
#44725=EDGE_CURVE('',#35456,#35455,#18726,.T.);
#44726=EDGE_CURVE('',#35457,#35456,#27522,.T.);
#44727=EDGE_CURVE('',#35458,#35457,#18727,.T.);
#44728=EDGE_CURVE('',#35458,#35459,#18728,.T.);
#44729=EDGE_CURVE('',#35459,#35460,#27523,.T.);
#44730=EDGE_CURVE('',#35460,#35461,#18729,.T.);
#44731=EDGE_CURVE('',#35462,#35461,#18730,.T.);
#44732=EDGE_CURVE('',#35463,#35462,#27524,.T.);
#44733=EDGE_CURVE('',#35464,#35463,#18731,.T.);
#44734=EDGE_CURVE('',#35464,#35465,#27525,.T.);
#44735=EDGE_CURVE('',#35466,#35465,#18732,.T.);
#44736=EDGE_CURVE('',#35466,#35467,#27526,.T.);
#44737=EDGE_CURVE('',#35448,#35467,#18733,.T.);
#44738=EDGE_CURVE('',#35468,#35469,#27527,.T.);
#44739=EDGE_CURVE('',#35469,#35470,#18734,.T.);
#44740=EDGE_CURVE('',#35470,#35471,#27528,.T.);
#44741=EDGE_CURVE('',#35471,#35468,#18735,.T.);
#44742=EDGE_CURVE('',#35472,#35472,#18736,.T.);
#44743=EDGE_CURVE('',#35473,#35473,#18737,.F.);
#44744=EDGE_CURVE('',#35474,#35474,#18738,.T.);
#44745=EDGE_CURVE('',#35467,#35428,#27529,.T.);
#44746=EDGE_CURVE('',#35475,#35466,#27530,.T.);
#44747=EDGE_CURVE('',#35476,#35475,#27531,.T.);
#44748=EDGE_CURVE('',#35429,#35476,#4089,.T.);
#44749=EDGE_CURVE('',#35477,#35475,#18739,.T.);
#44750=EDGE_CURVE('',#35465,#35477,#27532,.T.);
#44751=EDGE_CURVE('',#35463,#35478,#27533,.T.);
#44752=EDGE_CURVE('',#35478,#35479,#18740,.T.);
#44753=EDGE_CURVE('',#35479,#35464,#27534,.T.);
#44754=EDGE_CURVE('',#35480,#35479,#27535,.T.);
#44755=EDGE_CURVE('',#35481,#35480,#4090,.T.);
#44756=EDGE_CURVE('',#35477,#35481,#27536,.T.);
#44757=EDGE_CURVE('',#35482,#35478,#27537,.T.);
#44758=EDGE_CURVE('',#35483,#35482,#18741,.T.);
#44759=EDGE_CURVE('',#35483,#35484,#27538,.T.);
#44760=EDGE_CURVE('',#35485,#35484,#18742,.T.);
#44761=EDGE_CURVE('',#35485,#35486,#27539,.F.);
#44762=EDGE_CURVE('',#35486,#35487,#27540,.F.);
#44763=EDGE_CURVE('',#35488,#35487,#18743,.T.);
#44764=EDGE_CURVE('',#35488,#35489,#18744,.F.);
#44765=EDGE_CURVE('',#35489,#35490,#27541,.T.);
#44766=EDGE_CURVE('',#35491,#35490,#18745,.T.);
#44767=EDGE_CURVE('',#35491,#35307,#27542,.T.);
#44768=EDGE_CURVE('',#35316,#35492,#18746,.T.);
#44769=EDGE_CURVE('',#35380,#35492,#18747,.F.);
#44770=EDGE_CURVE('',#35480,#35379,#18748,.T.);
#44771=EDGE_CURVE('',#35455,#35493,#27543,.T.);
#44772=EDGE_CURVE('',#35493,#35494,#18749,.T.);
#44773=EDGE_CURVE('',#35494,#35456,#27544,.T.);
#44774=EDGE_CURVE('',#35495,#35454,#27545,.T.);
#44775=EDGE_CURVE('',#35493,#35495,#27546,.T.);
#44776=EDGE_CURVE('',#35393,#35495,#18750,.T.);
#44777=EDGE_CURVE('',#35496,#35105,#18751,.T.);
#44778=EDGE_CURVE('',#35496,#35497,#18752,.T.);
#44779=EDGE_CURVE('',#35498,#35497,#18753,.T.);
#44780=EDGE_CURVE('',#35498,#35499,#18754,.T.);
#44781=EDGE_CURVE('',#35101,#35499,#18755,.T.);
#44782=EDGE_CURVE('',#35336,#35383,#18756,.F.);
#44783=EDGE_CURVE('',#35344,#35500,#18757,.F.);
#44784=EDGE_CURVE('',#35500,#35501,#18758,.T.);
#44785=EDGE_CURVE('',#35501,#35502,#27547,.T.);
#44786=EDGE_CURVE('',#35340,#35502,#18759,.T.);
#44787=EDGE_CURVE('',#35503,#35339,#18760,.F.);
#44788=EDGE_CURVE('',#35503,#35494,#27548,.T.);
#44789=EDGE_CURVE('',#35504,#35504,#18761,.T.);
#44790=EDGE_CURVE('',#35453,#35389,#27549,.T.);
#44791=EDGE_CURVE('',#35451,#35418,#27550,.T.);
#44792=EDGE_CURVE('',#35417,#35452,#27551,.T.);
#44793=EDGE_CURVE('',#35416,#35390,#27552,.T.);
#44794=EDGE_CURVE('',#35391,#35415,#27553,.T.);
#44795=EDGE_CURVE('',#35440,#35221,#27554,.T.);
#44796=EDGE_CURVE('',#35219,#35439,#27555,.T.);
#44797=EDGE_CURVE('',#35441,#35223,#27556,.T.);
#44798=EDGE_CURVE('',#35225,#35442,#27557,.T.);
#44799=EDGE_CURVE('',#35438,#35227,#27558,.T.);
#44800=EDGE_CURVE('',#35229,#35437,#27559,.T.);
#44801=EDGE_CURVE('',#35257,#35505,#27560,.T.);
#44802=EDGE_CURVE('',#35505,#35506,#18762,.T.);
#44803=EDGE_CURVE('',#35506,#35255,#27561,.T.);
#44804=EDGE_CURVE('',#35507,#35259,#27562,.T.);
#44805=EDGE_CURVE('',#35505,#35507,#18763,.T.);
#44806=EDGE_CURVE('',#35269,#35507,#18764,.T.);
#44807=EDGE_CURVE('',#35508,#35281,#27563,.T.);
#44808=EDGE_CURVE('',#35509,#35508,#18765,.T.);
#44809=EDGE_CURVE('',#35279,#35509,#27564,.T.);
#44810=EDGE_CURVE('',#35510,#35283,#27565,.T.);
#44811=EDGE_CURVE('',#35508,#35510,#18766,.T.);
#44812=EDGE_CURVE('',#35488,#35285,#27566,.T.);
#44813=EDGE_CURVE('',#35487,#35511,#27567,.T.);
#44814=EDGE_CURVE('',#35511,#35510,#18767,.T.);
#44815=EDGE_CURVE('',#35287,#35489,#27568,.T.);
#44816=EDGE_CURVE('',#35490,#35289,#27569,.T.);
#44817=EDGE_CURVE('',#35291,#35491,#27570,.T.);
#44818=EDGE_CURVE('',#35481,#35268,#18768,.T.);
#44819=EDGE_CURVE('',#35476,#35272,#18769,.T.);
#44820=EDGE_CURVE('',#35411,#35113,#27571,.T.);
#44821=EDGE_CURVE('',#35111,#35410,#27572,.T.);
#44822=EDGE_CURVE('',#35115,#35412,#27573,.T.);
#44823=EDGE_CURVE('',#35413,#35117,#27574,.T.);
#44824=EDGE_CURVE('',#35119,#35414,#27575,.T.);
#44825=EDGE_CURVE('',#35392,#35121,#27576,.T.);
#44826=EDGE_CURVE('',#35083,#35498,#27577,.T.);
#44827=EDGE_CURVE('',#35497,#35081,#27578,.T.);
#44828=EDGE_CURVE('',#35499,#35085,#27579,.T.);
#44829=EDGE_CURVE('',#35079,#35496,#27580,.T.);
#44830=EDGE_CURVE('',#35450,#35419,#27581,.T.);
#44831=EDGE_CURVE('',#35378,#35269,#18770,.T.);
#44832=EDGE_CURVE('',#35449,#35424,#27582,.T.);
#44833=EDGE_CURVE('',#35512,#35462,#27583,.T.);
#44834=EDGE_CURVE('',#35512,#35513,#27584,.F.);
#44835=EDGE_CURVE('',#35482,#35513,#27585,.T.);
#44836=EDGE_CURVE('',#35374,#35514,#18771,.T.);
#44837=EDGE_CURVE('',#35146,#35373,#18772,.T.);
#44838=EDGE_CURVE('',#35515,#35180,#18773,.T.);
#44839=EDGE_CURVE('',#35514,#35515,#27586,.T.);
#44840=EDGE_CURVE('',#35157,#35515,#27587,.T.);
#44841=EDGE_CURVE('',#35516,#35516,#18774,.F.);
#44842=EDGE_CURVE('',#35408,#35517,#27588,.T.);
#44843=EDGE_CURVE('',#35517,#35518,#18775,.T.);
#44844=EDGE_CURVE('',#35409,#35518,#27589,.T.);
#44845=EDGE_CURVE('',#35175,#35517,#18776,.T.);
#44846=EDGE_CURVE('',#35518,#35151,#18777,.T.);
#44847=EDGE_CURVE('',#35315,#35519,#18778,.T.);
#44848=EDGE_CURVE('',#35519,#35492,#27590,.T.);
#44849=EDGE_CURVE('',#35519,#35381,#18779,.T.);
#44850=EDGE_CURVE('',#35520,#35352,#27591,.T.);
#44851=EDGE_CURVE('',#35521,#35520,#27592,.T.);
#44852=EDGE_CURVE('',#35350,#35521,#27593,.T.);
#44853=EDGE_CURVE('',#35354,#35522,#27594,.T.);
#44854=EDGE_CURVE('',#35522,#35520,#18780,.T.);
#44855=EDGE_CURVE('',#35522,#35362,#18781,.T.);
#44856=EDGE_CURVE('',#35190,#35433,#27595,.T.);
#44857=EDGE_CURVE('',#35432,#35188,#27596,.T.);
#44858=EDGE_CURVE('',#35434,#35192,#27597,.T.);
#44859=EDGE_CURVE('',#35404,#35159,#27598,.T.);
#44860=EDGE_CURVE('',#35403,#35514,#27599,.T.);
#44861=EDGE_CURVE('',#35161,#35405,#27600,.T.);
#44862=EDGE_CURVE('',#35406,#35163,#27601,.T.);
#44863=EDGE_CURVE('',#35165,#35407,#27602,.T.);
#44864=EDGE_CURVE('',#35322,#35500,#27603,.T.);
#44865=EDGE_CURVE('',#35501,#35324,#27604,.T.);
#44866=EDGE_CURVE('',#35502,#35326,#27605,.T.);
#44867=EDGE_CURVE('',#35521,#35365,#18782,.T.);
#44868=EDGE_CURVE('',#35186,#35431,#27606,.T.);
#44869=EDGE_CURVE('',#35509,#35314,#18783,.T.);
#44870=EDGE_CURVE('',#35511,#35523,#27607,.T.);
#44871=EDGE_CURVE('',#35523,#35524,#27608,.T.);
#44872=EDGE_CURVE('',#35525,#35524,#18784,.T.);
#44873=EDGE_CURVE('',#35525,#35526,#27609,.T.);
#44874=EDGE_CURVE('',#35527,#35526,#18785,.T.);
#44875=EDGE_CURVE('',#35527,#35528,#27610,.T.);
#44876=EDGE_CURVE('',#35338,#35528,#18786,.T.);
#44877=EDGE_CURVE('',#35382,#35337,#18787,.T.);
#44878=EDGE_CURVE('',#35529,#35529,#18788,.T.);
#44879=EDGE_CURVE('',#35273,#35506,#18789,.T.);
#44880=EDGE_CURVE('',#35506,#35377,#18790,.T.);
#44881=EDGE_CURVE('',#35273,#35430,#27611,.T.);
#44882=EDGE_CURVE('',#35402,#35435,#27612,.T.);
#44883=EDGE_CURVE('',#35436,#35401,#27613,.T.);
#44884=EDGE_CURVE('',#35530,#35530,#18791,.F.);
#44885=EDGE_CURVE('',#35531,#35531,#18792,.T.);
#44886=EDGE_CURVE('',#35531,#35530,#27614,.T.);
#44887=EDGE_CURVE('',#35532,#35532,#18793,.T.);
#44888=EDGE_CURVE('',#35443,#35473,#27615,.T.);
#44889=EDGE_CURVE('',#35533,#35458,#27616,.T.);
#44890=EDGE_CURVE('',#35534,#35533,#18794,.T.);
#44891=EDGE_CURVE('',#35534,#35459,#27617,.T.);
#44892=EDGE_CURVE('',#35535,#35460,#27618,.T.);
#44893=EDGE_CURVE('',#35535,#35534,#27619,.T.);
#44894=EDGE_CURVE('',#35461,#35536,#27620,.T.);
#44895=EDGE_CURVE('',#35536,#35535,#18795,.T.);
#44896=EDGE_CURVE('',#35537,#35538,#18796,.F.);
#44897=EDGE_CURVE('',#35537,#35470,#27621,.T.);
#44898=EDGE_CURVE('',#35538,#35469,#27622,.T.);
#44899=EDGE_CURVE('',#35539,#35537,#27623,.F.);
#44900=EDGE_CURVE('',#35539,#35471,#27624,.T.);
#44901=EDGE_CURVE('',#35540,#35539,#18797,.F.);
#44902=EDGE_CURVE('',#35540,#35468,#27625,.T.);
#44903=EDGE_CURVE('',#35538,#35540,#27626,.F.);
#44904=EDGE_CURVE('',#35541,#35541,#18798,.T.);
#44905=EDGE_CURVE('',#35504,#35474,#27627,.T.);
#44906=EDGE_CURVE('',#35542,#35542,#18799,.T.);
#44907=EDGE_CURVE('',#35542,#35532,#27628,.T.);
#44908=EDGE_CURVE('',#35533,#35543,#18800,.T.);
#44909=EDGE_CURVE('',#35457,#35543,#27629,.T.);
#44910=EDGE_CURVE('',#35544,#35545,#18801,.F.);
#44911=EDGE_CURVE('',#35544,#35485,#27630,.T.);
#44912=EDGE_CURVE('',#35484,#35545,#27631,.T.);
#44913=EDGE_CURVE('',#35546,#35483,#27632,.T.);
#44914=EDGE_CURVE('',#35546,#35545,#27633,.F.);
#44915=EDGE_CURVE('',#35536,#35512,#18802,.F.);
#44916=EDGE_CURVE('',#35513,#35546,#18803,.T.);
#44917=EDGE_CURVE('',#35547,#35548,#18804,.F.);
#44918=EDGE_CURVE('',#35548,#35544,#27634,.T.);
#44919=EDGE_CURVE('',#35543,#35549,#27635,.T.);
#44920=EDGE_CURVE('',#35549,#35550,#18805,.F.);
#44921=EDGE_CURVE('',#35550,#35547,#27636,.T.);
#44922=EDGE_CURVE('',#35421,#35472,#27637,.T.);
#44923=EDGE_CURVE('',#35516,#35541,#27638,.T.);
#44924=EDGE_CURVE('',#35529,#35542,#27639,.T.);
#44925=EDGE_CURVE('',#35528,#35503,#27640,.T.);
#44926=EDGE_CURVE('',#35549,#35527,#27641,.T.);
#44927=EDGE_CURVE('',#35526,#35550,#27642,.T.);
#44928=EDGE_CURVE('',#35547,#35525,#27643,.T.);
#44929=EDGE_CURVE('',#35524,#35548,#27644,.T.);
#44930=EDGE_CURVE('',#35486,#35523,#27645,.F.);
#44931=EDGE_CURVE('',#35551,#35552,#23622,.T.);
#44932=EDGE_CURVE('',#35553,#35551,#23623,.T.);
#44933=EDGE_CURVE('',#35553,#35552,#27646,.T.);
#44934=EDGE_CURVE('',#35552,#35554,#27647,.T.);
#44935=EDGE_CURVE('',#35555,#35553,#27648,.T.);
#44936=EDGE_CURVE('',#35554,#35555,#27649,.T.);
#44937=EDGE_CURVE('',#35556,#35555,#18806,.T.);
#44938=EDGE_CURVE('',#35554,#35556,#18807,.T.);
#44939=EDGE_CURVE('',#35556,#35551,#27650,.T.);
#44940=EDGE_CURVE('',#35557,#35558,#18808,.T.);
#44941=EDGE_CURVE('',#35558,#35559,#27651,.T.);
#44942=EDGE_CURVE('',#35559,#35560,#18809,.F.);
#44943=EDGE_CURVE('',#35560,#35557,#27652,.T.);
#44944=EDGE_CURVE('',#35557,#35561,#18810,.F.);
#44945=EDGE_CURVE('',#35562,#35561,#18811,.T.);
#44946=EDGE_CURVE('',#35562,#35563,#27653,.T.);
#44947=EDGE_CURVE('',#35564,#35563,#18812,.F.);
#44948=EDGE_CURVE('',#35564,#35565,#27654,.T.);
#44949=EDGE_CURVE('',#35566,#35565,#18813,.F.);
#44950=EDGE_CURVE('',#35566,#35567,#18814,.T.);
#44951=EDGE_CURVE('',#35568,#35567,#18815,.F.);
#44952=EDGE_CURVE('',#35568,#35569,#27655,.F.);
#44953=EDGE_CURVE('',#35570,#35569,#18816,.F.);
#44954=EDGE_CURVE('',#35570,#35571,#27656,.F.);
#44955=EDGE_CURVE('',#35572,#35571,#18817,.F.);
#44956=EDGE_CURVE('',#35572,#35573,#27657,.T.);
#44957=EDGE_CURVE('',#35573,#35574,#18818,.T.);
#44958=EDGE_CURVE('',#35574,#35575,#27658,.T.);
#44959=EDGE_CURVE('',#35576,#35575,#18819,.F.);
#44960=EDGE_CURVE('',#35576,#35577,#27659,.F.);
#44961=EDGE_CURVE('',#35578,#35577,#18820,.F.);
#44962=EDGE_CURVE('',#35578,#35558,#27660,.T.);
#44963=EDGE_CURVE('',#35579,#35560,#18821,.T.);
#44964=EDGE_CURVE('',#35561,#35579,#27661,.T.);
#44965=EDGE_CURVE('',#35579,#35580,#18822,.F.);
#44966=EDGE_CURVE('',#35580,#35562,#27662,.T.);
#44967=EDGE_CURVE('',#35581,#35580,#27663,.T.);
#44968=EDGE_CURVE('',#35582,#35581,#27664,.T.);
#44969=EDGE_CURVE('',#35583,#35582,#27665,.T.);
#44970=EDGE_CURVE('',#35563,#35583,#27666,.T.);
#44971=EDGE_CURVE('',#35584,#35585,#18823,.T.);
#44972=EDGE_CURVE('',#35585,#35586,#18824,.T.);
#44973=EDGE_CURVE('',#35586,#35587,#18825,.T.);
#44974=EDGE_CURVE('',#35587,#35584,#18826,.T.);
#44975=EDGE_CURVE('',#35588,#35582,#18827,.T.);
#44976=EDGE_CURVE('',#35582,#35587,#18828,.T.);
#44977=EDGE_CURVE('',#35586,#35588,#18829,.T.);
#44978=EDGE_CURVE('',#35589,#35583,#18830,.T.);
#44979=EDGE_CURVE('',#35588,#35589,#27667,.T.);
#44980=EDGE_CURVE('',#35590,#35591,#18831,.T.);
#44981=EDGE_CURVE('',#35591,#35583,#18832,.T.);
#44982=EDGE_CURVE('',#35589,#35590,#18833,.T.);
#44983=EDGE_CURVE('',#35592,#35593,#18834,.T.);
#44984=EDGE_CURVE('',#35593,#35591,#27668,.T.);
#44985=EDGE_CURVE('',#35590,#35592,#27669,.T.);
#44986=EDGE_CURVE('',#35594,#35595,#18835,.T.);
#44987=EDGE_CURVE('',#35595,#35593,#18836,.T.);
#44988=EDGE_CURVE('',#35592,#35594,#18837,.T.);
#44989=EDGE_CURVE('',#35596,#35597,#18838,.T.);
#44990=EDGE_CURVE('',#35597,#35595,#18839,.T.);
#44991=EDGE_CURVE('',#35594,#35596,#18840,.T.);
#44992=EDGE_CURVE('',#35584,#35597,#18841,.T.);
#44993=EDGE_CURVE('',#35596,#35585,#18842,.T.);
#44994=EDGE_CURVE('',#35595,#35598,#27670,.T.);
#44995=EDGE_CURVE('',#35599,#35598,#18843,.F.);
#44996=EDGE_CURVE('',#35599,#35593,#27671,.T.);
#44997=EDGE_CURVE('',#35600,#35597,#27672,.T.);
#44998=EDGE_CURVE('',#35598,#35600,#18844,.T.);
#44999=EDGE_CURVE('',#35584,#35601,#27673,.T.);
#45000=EDGE_CURVE('',#35601,#35600,#18845,.T.);
#45001=EDGE_CURVE('',#35602,#35587,#27674,.T.);
#45002=EDGE_CURVE('',#35603,#35602,#18846,.T.);
#45003=EDGE_CURVE('',#35604,#35603,#27675,.T.);
#45004=EDGE_CURVE('',#35604,#35601,#18847,.T.);
#45005=EDGE_CURVE('',#35605,#35606,#18848,.T.);
#45006=EDGE_CURVE('',#35606,#35607,#18849,.T.);
#45007=EDGE_CURVE('',#35607,#35608,#18850,.T.);
#45008=EDGE_CURVE('',#35608,#35605,#23624,.T.);
#45009=EDGE_CURVE('',#35609,#35610,#18851,.T.);
#45010=EDGE_CURVE('',#35610,#35611,#18852,.T.);
#45011=EDGE_CURVE('',#35611,#35612,#18853,.T.);
#45012=EDGE_CURVE('',#35612,#35609,#23625,.T.);
#45013=EDGE_CURVE('',#35613,#35614,#18854,.T.);
#45014=EDGE_CURVE('',#35614,#35611,#27676,.T.);
#45015=EDGE_CURVE('',#35610,#35613,#27677,.T.);
#45016=EDGE_CURVE('',#35608,#35614,#18855,.T.);
#45017=EDGE_CURVE('',#35613,#35605,#18856,.T.);
#45018=EDGE_CURVE('',#35615,#35616,#18857,.T.);
#45019=EDGE_CURVE('',#35616,#35617,#18858,.T.);
#45020=EDGE_CURVE('',#35617,#35618,#18859,.T.);
#45021=EDGE_CURVE('',#35618,#35615,#23626,.T.);
#45022=EDGE_CURVE('',#35612,#35617,#18860,.T.);
#45023=EDGE_CURVE('',#35616,#35609,#18861,.T.);
#45024=EDGE_CURVE('',#35619,#35607,#18862,.T.);
#45025=EDGE_CURVE('',#35606,#35620,#18863,.T.);
#45026=EDGE_CURVE('',#35620,#35619,#23627,.T.);
#45027=EDGE_CURVE('',#35618,#35619,#27678,.T.);
#45028=EDGE_CURVE('',#35620,#35615,#27679,.T.);
#45029=EDGE_CURVE('',#35621,#35607,#27680,.T.);
#45030=EDGE_CURVE('',#35622,#35621,#18864,.T.);
#45031=EDGE_CURVE('',#35608,#35622,#27681,.T.);
#45032=EDGE_CURVE('',#35619,#35623,#27682,.T.);
#45033=EDGE_CURVE('',#35621,#35623,#18865,.T.);
#45034=EDGE_CURVE('',#35624,#35618,#27683,.T.);
#45035=EDGE_CURVE('',#35623,#35624,#27684,.T.);
#45036=EDGE_CURVE('',#35625,#35617,#27685,.T.);
#45037=EDGE_CURVE('',#35624,#35625,#18866,.T.);
#45038=EDGE_CURVE('',#35626,#35627,#23628,.T.);
#45039=EDGE_CURVE('',#35626,#35628,#18867,.T.);
#45040=EDGE_CURVE('',#35628,#35629,#18868,.T.);
#45041=EDGE_CURVE('',#35629,#35630,#18869,.T.);
#45042=EDGE_CURVE('',#35627,#35630,#23629,.T.);
#45043=EDGE_CURVE('',#35631,#35632,#18870,.T.);
#45044=EDGE_CURVE('',#35632,#35629,#18871,.T.);
#45045=EDGE_CURVE('',#35628,#35631,#18872,.T.);
#45046=EDGE_CURVE('',#35633,#35634,#23630,.T.);
#45047=EDGE_CURVE('',#35633,#35635,#18873,.T.);
#45048=EDGE_CURVE('',#35636,#35635,#23631,.T.);
#45049=EDGE_CURVE('',#35636,#35632,#18874,.T.);
#45050=EDGE_CURVE('',#35631,#35637,#18875,.T.);
#45051=EDGE_CURVE('',#35634,#35637,#23632,.T.);
#45052=EDGE_CURVE('',#35638,#35629,#27686,.T.);
#45053=EDGE_CURVE('',#35639,#35638,#23633,.F.);
#45054=EDGE_CURVE('',#35640,#35639,#27687,.T.);
#45055=EDGE_CURVE('',#35641,#35640,#23634,.T.);
#45056=EDGE_CURVE('',#35642,#35641,#27688,.T.);
#45057=EDGE_CURVE('',#35643,#35642,#18876,.T.);
#45058=EDGE_CURVE('',#35644,#35643,#27689,.T.);
#45059=EDGE_CURVE('',#35644,#35645,#23635,.T.);
#45060=EDGE_CURVE('',#35645,#35646,#23636,.T.);
#45061=EDGE_CURVE('',#35646,#35647,#23637,.T.);
#45062=EDGE_CURVE('',#35647,#35648,#23638,.T.);
#45063=EDGE_CURVE('',#35648,#35630,#27690,.T.);
#45064=EDGE_CURVE('',#35632,#35649,#27691,.T.);
#45065=EDGE_CURVE('',#35638,#35649,#23639,.F.);
#45066=EDGE_CURVE('',#35636,#35650,#27692,.T.);
#45067=EDGE_CURVE('',#35651,#35650,#18877,.T.);
#45068=EDGE_CURVE('',#35651,#35652,#23640,.T.);
#45069=EDGE_CURVE('',#35652,#35653,#23641,.T.);
#45070=EDGE_CURVE('',#35649,#35653,#18878,.T.);
#45071=EDGE_CURVE('',#35635,#35654,#27693,.T.);
#45072=EDGE_CURVE('',#35654,#35655,#18879,.T.);
#45073=EDGE_CURVE('',#35655,#35636,#27694,.T.);
#45074=EDGE_CURVE('',#35656,#35633,#27695,.T.);
#45075=EDGE_CURVE('',#35657,#35656,#27696,.T.);
#45076=EDGE_CURVE('',#35654,#35657,#18880,.T.);
#45077=EDGE_CURVE('',#35658,#35634,#156,.T.);
#45078=EDGE_CURVE('',#35658,#35659,#27697,.T.);
#45079=EDGE_CURVE('',#35660,#35659,#4091,.T.);
#45080=EDGE_CURVE('',#35660,#35661,#27698,.T.);
#45081=EDGE_CURVE('',#35661,#35662,#4092,.F.);
#45082=EDGE_CURVE('',#35662,#35663,#23642,.T.);
#45083=EDGE_CURVE('',#35664,#35663,#27699,.T.);
#45084=EDGE_CURVE('',#35664,#35656,#18881,.T.);
#45085=EDGE_CURVE('',#35657,#35665,#18882,.T.);
#45086=EDGE_CURVE('',#35665,#35655,#18883,.T.);
#45087=EDGE_CURVE('',#35664,#35665,#27700,.T.);
#45088=EDGE_CURVE('',#35666,#35655,#27701,.T.);
#45089=EDGE_CURVE('',#35666,#35667,#18884,.F.);
#45090=EDGE_CURVE('',#35668,#35667,#18885,.F.);
#45091=EDGE_CURVE('',#35669,#35668,#27702,.T.);
#45092=EDGE_CURVE('',#35650,#35669,#4093,.T.);
#45093=EDGE_CURVE('',#35670,#35670,#18886,.T.);
#45094=EDGE_CURVE('',#35665,#35671,#27703,.T.);
#45095=EDGE_CURVE('',#35671,#35666,#23643,.F.);
#45096=EDGE_CURVE('',#35672,#35663,#18887,.T.);
#45097=EDGE_CURVE('',#35673,#35672,#27704,.T.);
#45098=EDGE_CURVE('',#35673,#35674,#27705,.T.);
#45099=EDGE_CURVE('',#35675,#35674,#27706,.T.);
#45100=EDGE_CURVE('',#35676,#35675,#27707,.T.);
#45101=EDGE_CURVE('',#35577,#35676,#27708,.T.);
#45102=EDGE_CURVE('',#35677,#35576,#27709,.T.);
#45103=EDGE_CURVE('',#35678,#35677,#27710,.T.);
#45104=EDGE_CURVE('',#35679,#35678,#27711,.T.);
#45105=EDGE_CURVE('',#35680,#35679,#27712,.T.);
#45106=EDGE_CURVE('',#35680,#35681,#4094,.T.);
#45107=EDGE_CURVE('',#35671,#35681,#27713,.T.);
#45108=EDGE_CURVE('',#35637,#35682,#27714,.T.);
#45109=EDGE_CURVE('',#35682,#35683,#157,.T.);
#45110=EDGE_CURVE('',#35683,#35658,#27715,.T.);
#45111=EDGE_CURVE('',#35627,#35684,#158,.T.);
#45112=EDGE_CURVE('',#35684,#35683,#27716,.T.);
#45113=EDGE_CURVE('',#35682,#35626,#27717,.T.);
#45114=EDGE_CURVE('',#35683,#35685,#27718,.T.);
#45115=EDGE_CURVE('',#35659,#35685,#4095,.T.);
#45116=EDGE_CURVE('',#35684,#35686,#27719,.T.);
#45117=EDGE_CURVE('',#35685,#35686,#27720,.T.);
#45118=EDGE_CURVE('',#35687,#35688,#18888,.T.);
#45119=EDGE_CURVE('',#35688,#35689,#18889,.T.);
#45120=EDGE_CURVE('',#35689,#35690,#18890,.T.);
#45121=EDGE_CURVE('',#35687,#35690,#23644,.T.);
#45122=EDGE_CURVE('',#35691,#35692,#18891,.T.);
#45123=EDGE_CURVE('',#35692,#35689,#18892,.T.);
#45124=EDGE_CURVE('',#35688,#35691,#18893,.T.);
#45125=EDGE_CURVE('',#35693,#35694,#18894,.T.);
#45126=EDGE_CURVE('',#35694,#35692,#18895,.T.);
#45127=EDGE_CURVE('',#35691,#35693,#18896,.T.);
#45128=EDGE_CURVE('',#35695,#35696,#18897,.T.);
#45129=EDGE_CURVE('',#35696,#35694,#18898,.T.);
#45130=EDGE_CURVE('',#35693,#35695,#18899,.T.);
#45131=EDGE_CURVE('',#35697,#35696,#27721,.T.);
#45132=EDGE_CURVE('',#35695,#35698,#27722,.T.);
#45133=EDGE_CURVE('',#35698,#35697,#159,.T.);
#45134=EDGE_CURVE('',#35690,#35697,#27723,.T.);
#45135=EDGE_CURVE('',#35698,#35687,#27724,.T.);
#45136=EDGE_CURVE('',#35697,#35699,#27725,.T.);
#45137=EDGE_CURVE('',#35700,#35699,#18900,.T.);
#45138=EDGE_CURVE('',#35701,#35700,#27726,.T.);
#45139=EDGE_CURVE('',#35702,#35701,#27727,.T.);
#45140=EDGE_CURVE('',#35696,#35702,#27728,.T.);
#45141=EDGE_CURVE('',#35690,#35703,#27729,.T.);
#45142=EDGE_CURVE('',#35704,#35703,#4096,.F.);
#45143=EDGE_CURVE('',#35705,#35704,#27730,.T.);
#45144=EDGE_CURVE('',#35706,#35705,#27731,.T.);
#45145=EDGE_CURVE('',#35706,#35699,#23645,.T.);
#45146=EDGE_CURVE('',#35707,#35689,#27732,.T.);
#45147=EDGE_CURVE('',#35703,#35707,#18901,.T.);
#45148=EDGE_CURVE('',#35708,#35709,#23646,.T.);
#45149=EDGE_CURVE('',#35708,#35710,#18902,.T.);
#45150=EDGE_CURVE('',#35711,#35710,#23647,.T.);
#45151=EDGE_CURVE('',#35712,#35711,#23648,.T.);
#45152=EDGE_CURVE('',#35712,#35713,#18903,.T.);
#45153=EDGE_CURVE('',#35714,#35713,#23649,.T.);
#45154=EDGE_CURVE('',#35715,#35714,#23650,.T.);
#45155=EDGE_CURVE('',#35709,#35715,#23651,.T.);
#45156=EDGE_CURVE('',#35715,#35716,#18904,.T.);
#45157=EDGE_CURVE('',#35716,#35709,#18905,.T.);
#45158=EDGE_CURVE('',#35714,#35717,#18906,.T.);
#45159=EDGE_CURVE('',#35717,#35716,#18907,.T.);
#45160=EDGE_CURVE('',#35713,#35718,#18908,.T.);
#45161=EDGE_CURVE('',#35718,#35719,#18909,.T.);
#45162=EDGE_CURVE('',#35719,#35717,#18910,.T.);
#45163=EDGE_CURVE('',#35720,#35712,#18911,.T.);
#45164=EDGE_CURVE('',#35721,#35720,#18912,.T.);
#45165=EDGE_CURVE('',#35722,#35721,#27733,.T.);
#45166=EDGE_CURVE('',#35723,#35722,#18913,.T.);
#45167=EDGE_CURVE('',#35724,#35723,#27734,.T.);
#45168=EDGE_CURVE('',#35725,#35724,#18914,.T.);
#45169=EDGE_CURVE('',#35718,#35725,#27735,.T.);
#45170=EDGE_CURVE('',#35725,#35726,#18915,.T.);
#45171=EDGE_CURVE('',#35726,#35719,#27736,.T.);
#45172=EDGE_CURVE('',#35724,#35727,#18916,.T.);
#45173=EDGE_CURVE('',#35727,#35726,#18917,.T.);
#45174=EDGE_CURVE('',#35723,#35728,#18918,.T.);
#45175=EDGE_CURVE('',#35728,#35727,#27737,.T.);
#45176=EDGE_CURVE('',#35722,#35729,#18919,.T.);
#45177=EDGE_CURVE('',#35729,#35728,#18920,.T.);
#45178=EDGE_CURVE('',#35721,#35730,#18921,.T.);
#45179=EDGE_CURVE('',#35730,#35729,#27738,.T.);
#45180=EDGE_CURVE('',#35720,#35731,#18922,.T.);
#45181=EDGE_CURVE('',#35731,#35730,#18923,.T.);
#45182=EDGE_CURVE('',#35711,#35731,#18924,.T.);
#45183=EDGE_CURVE('',#35716,#35732,#27739,.T.);
#45184=EDGE_CURVE('',#35733,#35732,#18925,.F.);
#45185=EDGE_CURVE('',#35733,#35734,#27740,.T.);
#45186=EDGE_CURVE('',#35708,#35734,#23652,.F.);
#45187=EDGE_CURVE('',#35735,#35717,#27741,.T.);
#45188=EDGE_CURVE('',#35732,#35735,#18926,.F.);
#45189=EDGE_CURVE('',#35736,#35719,#27742,.T.);
#45190=EDGE_CURVE('',#35735,#35736,#18927,.F.);
#45191=EDGE_CURVE('',#35737,#35726,#27743,.T.);
#45192=EDGE_CURVE('',#35736,#35737,#27744,.F.);
#45193=EDGE_CURVE('',#35727,#35738,#27745,.T.);
#45194=EDGE_CURVE('',#35738,#35737,#18928,.F.);
#45195=EDGE_CURVE('',#35739,#35728,#27746,.T.);
#45196=EDGE_CURVE('',#35738,#35739,#27747,.F.);
#45197=EDGE_CURVE('',#35729,#35740,#27748,.T.);
#45198=EDGE_CURVE('',#35740,#35739,#18929,.T.);
#45199=EDGE_CURVE('',#35741,#35730,#27749,.T.);
#45200=EDGE_CURVE('',#35740,#35741,#27750,.T.);
#45201=EDGE_CURVE('',#35731,#35742,#27751,.T.);
#45202=EDGE_CURVE('',#35742,#35741,#18930,.T.);
#45203=EDGE_CURVE('',#35710,#35734,#23653,.F.);
#45204=EDGE_CURVE('',#35733,#35743,#18931,.T.);
#45205=EDGE_CURVE('',#35743,#35744,#27752,.T.);
#45206=EDGE_CURVE('',#35745,#35744,#18932,.F.);
#45207=EDGE_CURVE('',#35746,#35745,#27753,.T.);
#45208=EDGE_CURVE('',#35746,#35747,#160,.T.);
#45209=EDGE_CURVE('',#35748,#35747,#23654,.T.);
#45210=EDGE_CURVE('',#35748,#35749,#23655,.F.);
#45211=EDGE_CURVE('',#35750,#35749,#23656,.T.);
#45212=EDGE_CURVE('',#35751,#35750,#27754,.T.);
#45213=EDGE_CURVE('',#35751,#35742,#18933,.T.);
#45214=EDGE_CURVE('',#35752,#35753,#18934,.T.);
#45215=EDGE_CURVE('',#35753,#35754,#18935,.T.);
#45216=EDGE_CURVE('',#35754,#35755,#18936,.T.);
#45217=EDGE_CURVE('',#35755,#35752,#18937,.T.);
#45218=EDGE_CURVE('',#35756,#35757,#18938,.T.);
#45219=EDGE_CURVE('',#35757,#35755,#18939,.T.);
#45220=EDGE_CURVE('',#35754,#35756,#18940,.T.);
#45221=EDGE_CURVE('',#35758,#35759,#18941,.T.);
#45222=EDGE_CURVE('',#35759,#35757,#27755,.T.);
#45223=EDGE_CURVE('',#35756,#35758,#27756,.T.);
#45224=EDGE_CURVE('',#35760,#35761,#18942,.T.);
#45225=EDGE_CURVE('',#35761,#35759,#18943,.T.);
#45226=EDGE_CURVE('',#35758,#35760,#18944,.T.);
#45227=EDGE_CURVE('',#35762,#35763,#18945,.T.);
#45228=EDGE_CURVE('',#35763,#35761,#27757,.T.);
#45229=EDGE_CURVE('',#35760,#35762,#27758,.T.);
#45230=EDGE_CURVE('',#35764,#35765,#18946,.T.);
#45231=EDGE_CURVE('',#35765,#35763,#18947,.T.);
#45232=EDGE_CURVE('',#35762,#35764,#18948,.T.);
#45233=EDGE_CURVE('',#35766,#35767,#18949,.T.);
#45234=EDGE_CURVE('',#35767,#35768,#18950,.T.);
#45235=EDGE_CURVE('',#35768,#35769,#18951,.T.);
#45236=EDGE_CURVE('',#35769,#35766,#18952,.T.);
#45237=EDGE_CURVE('',#35770,#35771,#18953,.T.);
#45238=EDGE_CURVE('',#35771,#35769,#18954,.T.);
#45239=EDGE_CURVE('',#35768,#35770,#18955,.T.);
#45240=EDGE_CURVE('',#35772,#35773,#18956,.T.);
#45241=EDGE_CURVE('',#35773,#35771,#18957,.T.);
#45242=EDGE_CURVE('',#35770,#35772,#18958,.T.);
#45243=EDGE_CURVE('',#35753,#35774,#18959,.T.);
#45244=EDGE_CURVE('',#35774,#35773,#27759,.T.);
#45245=EDGE_CURVE('',#35772,#35753,#27760,.T.);
#45246=EDGE_CURVE('',#35766,#35765,#18960,.T.);
#45247=EDGE_CURVE('',#35764,#35767,#18961,.T.);
#45248=EDGE_CURVE('',#35752,#35774,#18962,.T.);
#45249=EDGE_CURVE('',#35775,#35759,#27761,.T.);
#45250=EDGE_CURVE('',#35776,#35775,#27762,.T.);
#45251=EDGE_CURVE('',#35757,#35776,#27763,.T.);
#45252=EDGE_CURVE('',#35761,#35777,#27764,.T.);
#45253=EDGE_CURVE('',#35777,#35775,#18963,.T.);
#45254=EDGE_CURVE('',#35778,#35763,#27765,.T.);
#45255=EDGE_CURVE('',#35777,#35778,#27766,.T.);
#45256=EDGE_CURVE('',#35765,#35779,#27767,.T.);
#45257=EDGE_CURVE('',#35779,#35778,#18964,.T.);
#45258=EDGE_CURVE('',#35780,#35766,#27768,.T.);
#45259=EDGE_CURVE('',#35779,#35780,#18965,.T.);
#45260=EDGE_CURVE('',#35781,#35769,#27769,.T.);
#45261=EDGE_CURVE('',#35780,#35781,#18966,.T.);
#45262=EDGE_CURVE('',#35782,#35783,#18967,.T.);
#45263=EDGE_CURVE('',#35783,#35784,#27770,.T.);
#45264=EDGE_CURVE('',#35784,#35785,#18968,.T.);
#45265=EDGE_CURVE('',#35785,#35782,#27771,.T.);
#45266=EDGE_CURVE('',#35786,#35787,#18969,.T.);
#45267=EDGE_CURVE('',#35787,#35785,#18970,.T.);
#45268=EDGE_CURVE('',#35784,#35786,#18971,.T.);
#45269=EDGE_CURVE('',#35788,#35789,#18972,.T.);
#45270=EDGE_CURVE('',#35789,#35787,#27772,.T.);
#45271=EDGE_CURVE('',#35786,#35788,#27773,.T.);
#45272=EDGE_CURVE('',#35790,#35791,#18973,.T.);
#45273=EDGE_CURVE('',#35791,#35789,#18974,.T.);
#45274=EDGE_CURVE('',#35788,#35790,#18975,.T.);
#45275=EDGE_CURVE('',#35792,#35793,#18976,.T.);
#45276=EDGE_CURVE('',#35793,#35791,#18977,.T.);
#45277=EDGE_CURVE('',#35790,#35792,#18978,.T.);
#45278=EDGE_CURVE('',#35794,#35795,#18979,.T.);
#45279=EDGE_CURVE('',#35795,#35793,#27774,.T.);
#45280=EDGE_CURVE('',#35792,#35794,#27775,.T.);
#45281=EDGE_CURVE('',#35796,#35797,#18980,.T.);
#45282=EDGE_CURVE('',#35797,#35795,#18981,.T.);
#45283=EDGE_CURVE('',#35794,#35796,#18982,.T.);
#45284=EDGE_CURVE('',#35798,#35799,#18983,.T.);
#45285=EDGE_CURVE('',#35799,#35797,#18984,.T.);
#45286=EDGE_CURVE('',#35796,#35798,#18985,.T.);
#45287=EDGE_CURVE('',#35800,#35801,#18986,.T.);
#45288=EDGE_CURVE('',#35801,#35799,#18987,.T.);
#45289=EDGE_CURVE('',#35798,#35800,#18988,.T.);
#45290=EDGE_CURVE('',#35802,#35803,#18989,.T.);
#45291=EDGE_CURVE('',#35803,#35801,#18990,.T.);
#45292=EDGE_CURVE('',#35800,#35802,#18991,.T.);
#45293=EDGE_CURVE('',#35804,#35805,#18992,.T.);
#45294=EDGE_CURVE('',#35805,#35803,#27776,.T.);
#45295=EDGE_CURVE('',#35802,#35804,#27777,.T.);
#45296=EDGE_CURVE('',#35782,#35805,#18993,.T.);
#45297=EDGE_CURVE('',#35804,#35783,#18994,.T.);
#45298=EDGE_CURVE('',#35799,#35806,#27778,.T.);
#45299=EDGE_CURVE('',#35806,#35807,#18995,.T.);
#45300=EDGE_CURVE('',#35807,#35797,#27779,.T.);
#45301=EDGE_CURVE('',#35808,#35801,#27780,.T.);
#45302=EDGE_CURVE('',#35806,#35808,#18996,.T.);
#45303=EDGE_CURVE('',#35803,#35809,#27781,.T.);
#45304=EDGE_CURVE('',#35809,#35808,#18997,.T.);
#45305=EDGE_CURVE('',#35810,#35805,#27782,.T.);
#45306=EDGE_CURVE('',#35809,#35810,#27783,.T.);
#45307=EDGE_CURVE('',#35782,#35811,#27784,.T.);
#45308=EDGE_CURVE('',#35811,#35810,#18998,.T.);
#45309=EDGE_CURVE('',#35812,#35785,#27785,.T.);
#45310=EDGE_CURVE('',#35811,#35812,#27786,.T.);
#45311=EDGE_CURVE('',#35813,#35814,#18999,.T.);
#45312=EDGE_CURVE('',#35814,#35815,#27787,.T.);
#45313=EDGE_CURVE('',#35815,#35816,#19000,.T.);
#45314=EDGE_CURVE('',#35816,#35813,#27788,.T.);
#45315=EDGE_CURVE('',#35817,#35818,#19001,.T.);
#45316=EDGE_CURVE('',#35818,#35816,#19002,.T.);
#45317=EDGE_CURVE('',#35815,#35817,#19003,.T.);
#45318=EDGE_CURVE('',#35819,#35820,#19004,.T.);
#45319=EDGE_CURVE('',#35820,#35818,#27789,.T.);
#45320=EDGE_CURVE('',#35817,#35819,#27790,.T.);
#45321=EDGE_CURVE('',#35821,#35822,#19005,.T.);
#45322=EDGE_CURVE('',#35822,#35820,#19006,.T.);
#45323=EDGE_CURVE('',#35819,#35821,#19007,.T.);
#45324=EDGE_CURVE('',#35823,#35824,#19008,.T.);
#45325=EDGE_CURVE('',#35824,#35822,#27791,.T.);
#45326=EDGE_CURVE('',#35821,#35823,#27792,.T.);
#45327=EDGE_CURVE('',#35825,#35826,#19009,.T.);
#45328=EDGE_CURVE('',#35826,#35824,#19010,.T.);
#45329=EDGE_CURVE('',#35823,#35825,#19011,.T.);
#45330=EDGE_CURVE('',#35827,#35828,#19012,.T.);
#45331=EDGE_CURVE('',#35828,#35826,#19013,.T.);
#45332=EDGE_CURVE('',#35825,#35827,#19014,.T.);
#45333=EDGE_CURVE('',#35829,#35830,#19015,.T.);
#45334=EDGE_CURVE('',#35830,#35828,#19016,.T.);
#45335=EDGE_CURVE('',#35827,#35829,#19017,.T.);
#45336=EDGE_CURVE('',#35831,#35832,#19018,.T.);
#45337=EDGE_CURVE('',#35832,#35830,#19019,.T.);
#45338=EDGE_CURVE('',#35829,#35831,#19020,.T.);
#45339=EDGE_CURVE('',#35833,#35834,#19021,.T.);
#45340=EDGE_CURVE('',#35834,#35832,#19022,.T.);
#45341=EDGE_CURVE('',#35831,#35833,#19023,.T.);
#45342=EDGE_CURVE('',#35813,#35834,#19024,.T.);
#45343=EDGE_CURVE('',#35833,#35814,#19025,.T.);
#45344=EDGE_CURVE('',#35835,#35828,#27793,.T.);
#45345=EDGE_CURVE('',#35836,#35835,#19026,.F.);
#45346=EDGE_CURVE('',#35836,#35826,#27794,.T.);
#45347=EDGE_CURVE('',#35830,#35837,#27795,.T.);
#45348=EDGE_CURVE('',#35837,#35835,#19027,.T.);
#45349=EDGE_CURVE('',#35832,#35838,#27796,.T.);
#45350=EDGE_CURVE('',#35839,#35838,#19028,.T.);
#45351=EDGE_CURVE('',#35840,#35839,#27797,.T.);
#45352=EDGE_CURVE('',#35840,#35837,#19029,.T.);
#45353=EDGE_CURVE('',#35841,#35834,#27798,.T.);
#45354=EDGE_CURVE('',#35841,#35842,#19030,.F.);
#45355=EDGE_CURVE('',#35843,#35842,#27799,.T.);
#45356=EDGE_CURVE('',#35844,#35843,#23657,.T.);
#45357=EDGE_CURVE('',#35844,#35845,#23658,.F.);
#45358=EDGE_CURVE('',#35846,#35845,#23659,.T.);
#45359=EDGE_CURVE('',#35846,#35847,#161,.T.);
#45360=EDGE_CURVE('',#35848,#35847,#27800,.T.);
#45361=EDGE_CURVE('',#35838,#35848,#19031,.F.);
#45362=EDGE_CURVE('',#35813,#35849,#27801,.T.);
#45363=EDGE_CURVE('',#35849,#35841,#19032,.T.);
#45364=EDGE_CURVE('',#35850,#35816,#27802,.T.);
#45365=EDGE_CURVE('',#35849,#35850,#27803,.T.);
#45366=EDGE_CURVE('',#35851,#35852,#19033,.T.);
#45367=EDGE_CURVE('',#35852,#35853,#19034,.T.);
#45368=EDGE_CURVE('',#35853,#35854,#19035,.T.);
#45369=EDGE_CURVE('',#35854,#35851,#23660,.T.);
#45370=EDGE_CURVE('',#35855,#35856,#19036,.T.);
#45371=EDGE_CURVE('',#35856,#35853,#19037,.T.);
#45372=EDGE_CURVE('',#35852,#35855,#19038,.T.);
#45373=EDGE_CURVE('',#35857,#35858,#19039,.T.);
#45374=EDGE_CURVE('',#35858,#35856,#19040,.T.);
#45375=EDGE_CURVE('',#35855,#35857,#19041,.T.);
#45376=EDGE_CURVE('',#35859,#35860,#19042,.T.);
#45377=EDGE_CURVE('',#35860,#35858,#19043,.T.);
#45378=EDGE_CURVE('',#35857,#35859,#19044,.T.);
#45379=EDGE_CURVE('',#35861,#35860,#27804,.T.);
#45380=EDGE_CURVE('',#35859,#35862,#27805,.T.);
#45381=EDGE_CURVE('',#35861,#35862,#162,.T.);
#45382=EDGE_CURVE('',#35862,#35851,#27806,.T.);
#45383=EDGE_CURVE('',#35863,#35854,#23661,.T.);
#45384=EDGE_CURVE('',#35863,#35864,#27807,.T.);
#45385=EDGE_CURVE('',#35861,#35864,#19045,.T.);
#45386=EDGE_CURVE('',#35860,#35865,#27808,.T.);
#45387=EDGE_CURVE('',#35865,#35866,#19046,.T.);
#45388=EDGE_CURVE('',#35866,#35858,#27809,.T.);
#45389=EDGE_CURVE('',#35864,#35867,#19047,.T.);
#45390=EDGE_CURVE('',#35867,#35868,#27810,.T.);
#45391=EDGE_CURVE('',#35868,#35869,#19048,.F.);
#45392=EDGE_CURVE('',#35870,#35869,#27811,.T.);
#45393=EDGE_CURVE('',#35871,#35870,#27812,.T.);
#45394=EDGE_CURVE('',#35872,#35871,#19049,.T.);
#45395=EDGE_CURVE('',#35865,#35872,#27813,.T.);
#45396=EDGE_CURVE('',#35873,#35863,#23662,.F.);
#45397=EDGE_CURVE('',#35867,#35873,#27814,.T.);
#45398=EDGE_CURVE('',#35874,#35853,#27815,.T.);
#45399=EDGE_CURVE('',#35875,#35874,#19050,.T.);
#45400=EDGE_CURVE('',#35876,#35875,#23663,.T.);
#45401=EDGE_CURVE('',#35876,#35877,#27816,.T.);
#45402=EDGE_CURVE('',#35877,#35878,#23664,.T.);
#45403=EDGE_CURVE('',#35878,#35879,#27817,.T.);
#45404=EDGE_CURVE('',#35880,#35879,#23665,.T.);
#45405=EDGE_CURVE('',#35881,#35880,#19051,.T.);
#45406=EDGE_CURVE('',#35881,#35882,#27818,.T.);
#45407=EDGE_CURVE('',#35883,#35882,#23666,.T.);
#45408=EDGE_CURVE('',#35873,#35883,#27819,.F.);
#45409=EDGE_CURVE('',#35884,#35885,#19052,.T.);
#45410=EDGE_CURVE('',#35885,#35886,#27820,.T.);
#45411=EDGE_CURVE('',#35886,#35887,#19053,.T.);
#45412=EDGE_CURVE('',#35887,#35884,#27821,.T.);
#45413=EDGE_CURVE('',#35888,#35889,#19054,.T.);
#45414=EDGE_CURVE('',#35889,#35887,#19055,.T.);
#45415=EDGE_CURVE('',#35886,#35888,#19056,.T.);
#45416=EDGE_CURVE('',#35890,#35891,#19057,.T.);
#45417=EDGE_CURVE('',#35891,#35889,#27822,.T.);
#45418=EDGE_CURVE('',#35888,#35890,#27823,.T.);
#45419=EDGE_CURVE('',#35892,#35893,#19058,.T.);
#45420=EDGE_CURVE('',#35893,#35891,#19059,.T.);
#45421=EDGE_CURVE('',#35890,#35892,#19060,.T.);
#45422=EDGE_CURVE('',#35894,#35895,#19061,.T.);
#45423=EDGE_CURVE('',#35895,#35893,#19062,.T.);
#45424=EDGE_CURVE('',#35892,#35894,#19063,.T.);
#45425=EDGE_CURVE('',#35896,#35897,#19064,.T.);
#45426=EDGE_CURVE('',#35897,#35895,#19065,.T.);
#45427=EDGE_CURVE('',#35894,#35896,#19066,.T.);
#45428=EDGE_CURVE('',#35898,#35899,#19067,.T.);
#45429=EDGE_CURVE('',#35899,#35897,#27824,.T.);
#45430=EDGE_CURVE('',#35896,#35898,#27825,.T.);
#45431=EDGE_CURVE('',#35900,#35901,#19068,.T.);
#45432=EDGE_CURVE('',#35901,#35899,#19069,.T.);
#45433=EDGE_CURVE('',#35898,#35900,#19070,.T.);
#45434=EDGE_CURVE('',#35902,#35903,#19071,.T.);
#45435=EDGE_CURVE('',#35903,#35904,#19072,.T.);
#45436=EDGE_CURVE('',#35904,#35901,#19073,.T.);
#45437=EDGE_CURVE('',#35900,#35902,#19074,.T.);
#45438=EDGE_CURVE('',#35905,#35906,#19075,.T.);
#45439=EDGE_CURVE('',#35906,#35903,#19076,.T.);
#45440=EDGE_CURVE('',#35902,#35905,#19077,.T.);
#45441=EDGE_CURVE('',#35907,#35908,#19078,.T.);
#45442=EDGE_CURVE('',#35908,#35906,#27826,.T.);
#45443=EDGE_CURVE('',#35905,#35907,#27827,.T.);
#45444=EDGE_CURVE('',#35884,#35908,#19079,.T.);
#45445=EDGE_CURVE('',#35907,#35885,#19080,.T.);
#45446=EDGE_CURVE('',#35901,#35909,#27828,.T.);
#45447=EDGE_CURVE('',#35909,#35910,#19081,.F.);
#45448=EDGE_CURVE('',#35910,#35899,#27829,.T.);
#45449=EDGE_CURVE('',#35911,#35911,#19082,.T.);
#45450=EDGE_CURVE('',#35911,#35904,#27830,.T.);
#45451=EDGE_CURVE('',#35912,#35903,#27831,.T.);
#45452=EDGE_CURVE('',#35913,#35912,#19083,.F.);
#45453=EDGE_CURVE('',#35914,#35913,#27832,.T.);
#45454=EDGE_CURVE('',#35915,#35914,#19084,.T.);
#45455=EDGE_CURVE('',#35916,#35915,#27833,.T.);
#45456=EDGE_CURVE('',#35917,#35916,#19085,.F.);
#45457=EDGE_CURVE('',#35918,#35917,#27834,.T.);
#45458=EDGE_CURVE('',#35919,#35918,#19086,.T.);
#45459=EDGE_CURVE('',#35920,#35919,#27835,.T.);
#45460=EDGE_CURVE('',#35909,#35920,#19087,.F.);
#45461=EDGE_CURVE('',#35906,#35921,#27836,.T.);
#45462=EDGE_CURVE('',#35921,#35912,#19088,.F.);
#45463=EDGE_CURVE('',#35922,#35908,#27837,.T.);
#45464=EDGE_CURVE('',#35921,#35922,#27838,.F.);
#45465=EDGE_CURVE('',#35884,#35923,#27839,.T.);
#45466=EDGE_CURVE('',#35923,#35922,#19089,.F.);
#45467=EDGE_CURVE('',#35887,#35924,#27840,.T.);
#45468=EDGE_CURVE('',#35923,#35924,#27841,.T.);
#45469=EDGE_CURVE('',#35925,#35926,#19090,.T.);
#45470=EDGE_CURVE('',#35926,#35927,#19091,.T.);
#45471=EDGE_CURVE('',#35927,#35928,#19092,.T.);
#45472=EDGE_CURVE('',#35925,#35928,#23667,.T.);
#45473=EDGE_CURVE('',#35929,#35930,#19093,.T.);
#45474=EDGE_CURVE('',#35930,#35927,#19094,.T.);
#45475=EDGE_CURVE('',#35926,#35929,#19095,.T.);
#45476=EDGE_CURVE('',#35931,#35932,#19096,.T.);
#45477=EDGE_CURVE('',#35932,#35930,#27842,.T.);
#45478=EDGE_CURVE('',#35929,#35931,#27843,.T.);
#45479=EDGE_CURVE('',#35933,#35934,#19097,.T.);
#45480=EDGE_CURVE('',#35934,#35932,#19098,.T.);
#45481=EDGE_CURVE('',#35931,#35933,#19099,.T.);
#45482=EDGE_CURVE('',#35935,#35936,#19100,.T.);
#45483=EDGE_CURVE('',#35936,#35934,#27844,.T.);
#45484=EDGE_CURVE('',#35933,#35935,#27845,.T.);
#45485=EDGE_CURVE('',#35937,#35918,#19101,.T.);
#45486=EDGE_CURVE('',#35918,#35936,#19102,.T.);
#45487=EDGE_CURVE('',#35935,#35937,#19103,.T.);
#45488=EDGE_CURVE('',#35938,#35919,#19104,.T.);
#45489=EDGE_CURVE('',#35937,#35938,#19105,.T.);
#45490=EDGE_CURVE('',#35939,#35940,#19106,.T.);
#45491=EDGE_CURVE('',#35940,#35919,#19107,.T.);
#45492=EDGE_CURVE('',#35938,#35939,#19108,.T.);
#45493=EDGE_CURVE('',#35941,#35942,#19109,.T.);
#45494=EDGE_CURVE('',#35942,#35940,#27846,.T.);
#45495=EDGE_CURVE('',#35939,#35941,#27847,.T.);
#45496=EDGE_CURVE('',#35943,#35944,#19110,.T.);
#45497=EDGE_CURVE('',#35944,#35942,#19111,.T.);
#45498=EDGE_CURVE('',#35941,#35943,#19112,.T.);
#45499=EDGE_CURVE('',#35945,#35944,#19113,.T.);
#45500=EDGE_CURVE('',#35943,#35946,#19114,.T.);
#45501=EDGE_CURVE('',#35946,#35945,#23668,.T.);
#45502=EDGE_CURVE('',#35947,#35948,#19115,.T.);
#45503=EDGE_CURVE('',#35945,#35948,#23669,.T.);
#45504=EDGE_CURVE('',#35946,#35925,#19116,.T.);
#45505=EDGE_CURVE('',#35947,#35928,#23670,.T.);
#45506=EDGE_CURVE('',#35949,#35942,#27848,.T.);
#45507=EDGE_CURVE('',#35950,#35949,#27849,.F.);
#45508=EDGE_CURVE('',#35940,#35950,#27850,.T.);
#45509=EDGE_CURVE('',#35944,#35951,#27851,.T.);
#45510=EDGE_CURVE('',#35951,#35949,#19117,.T.);
#45511=EDGE_CURVE('',#35948,#35947,#23671,.F.);
#45512=EDGE_CURVE('',#35952,#35895,#27852,.T.);
#45513=EDGE_CURVE('',#35951,#35952,#19118,.T.);
#45514=EDGE_CURVE('',#35953,#35927,#27853,.T.);
#45515=EDGE_CURVE('',#35953,#35954,#19119,.T.);
#45516=EDGE_CURVE('',#35955,#35954,#27854,.T.);
#45517=EDGE_CURVE('',#35955,#35956,#163,.T.);
#45518=EDGE_CURVE('',#35957,#35956,#23672,.T.);
#45519=EDGE_CURVE('',#35958,#35957,#23673,.F.);
#45520=EDGE_CURVE('',#35959,#35958,#23674,.F.);
#45521=EDGE_CURVE('',#35960,#35959,#23675,.T.);
#45522=EDGE_CURVE('',#35960,#35961,#164,.T.);
#45523=EDGE_CURVE('',#35961,#35962,#165,.T.);
#45524=EDGE_CURVE('',#35963,#35962,#27855,.T.);
#45525=EDGE_CURVE('',#35963,#35964,#19120,.F.);
#45526=EDGE_CURVE('',#35965,#35964,#27856,.T.);
#45527=EDGE_CURVE('',#35965,#35966,#19121,.T.);
#45528=EDGE_CURVE('',#35893,#35966,#27857,.T.);
#45529=EDGE_CURVE('',#35967,#35968,#19122,.T.);
#45530=EDGE_CURVE('',#35968,#35969,#19123,.T.);
#45531=EDGE_CURVE('',#35969,#35970,#19124,.T.);
#45532=EDGE_CURVE('',#35970,#35967,#19125,.T.);
#45533=EDGE_CURVE('',#35971,#35972,#19126,.T.);
#45534=EDGE_CURVE('',#35972,#35970,#19127,.T.);
#45535=EDGE_CURVE('',#35969,#35971,#19128,.T.);
#45536=EDGE_CURVE('',#35973,#35974,#19129,.T.);
#45537=EDGE_CURVE('',#35974,#35972,#27858,.T.);
#45538=EDGE_CURVE('',#35971,#35973,#27859,.T.);
#45539=EDGE_CURVE('',#35975,#35914,#19130,.T.);
#45540=EDGE_CURVE('',#35914,#35974,#19131,.T.);
#45541=EDGE_CURVE('',#35973,#35975,#19132,.T.);
#45542=EDGE_CURVE('',#35976,#35915,#19133,.T.);
#45543=EDGE_CURVE('',#35975,#35976,#19134,.T.);
#45544=EDGE_CURVE('',#35977,#35978,#19135,.T.);
#45545=EDGE_CURVE('',#35978,#35915,#19136,.T.);
#45546=EDGE_CURVE('',#35976,#35977,#19137,.T.);
#45547=EDGE_CURVE('',#35979,#35980,#19138,.T.);
#45548=EDGE_CURVE('',#35980,#35978,#27860,.T.);
#45549=EDGE_CURVE('',#35977,#35979,#27861,.T.);
#45550=EDGE_CURVE('',#35981,#35982,#19139,.T.);
#45551=EDGE_CURVE('',#35982,#35980,#19140,.T.);
#45552=EDGE_CURVE('',#35979,#35981,#19141,.T.);
#45553=EDGE_CURVE('',#35983,#35984,#19142,.T.);
#45554=EDGE_CURVE('',#35984,#35982,#27862,.T.);
#45555=EDGE_CURVE('',#35981,#35983,#27863,.T.);
#45556=EDGE_CURVE('',#35967,#35984,#19143,.T.);
#45557=EDGE_CURVE('',#35983,#35968,#19144,.T.);
#45558=EDGE_CURVE('',#35985,#35980,#27864,.T.);
#45559=EDGE_CURVE('',#35986,#35985,#27865,.F.);
#45560=EDGE_CURVE('',#35978,#35986,#27866,.T.);
#45561=EDGE_CURVE('',#35982,#35987,#27867,.T.);
#45562=EDGE_CURVE('',#35987,#35985,#19145,.T.);
#45563=EDGE_CURVE('',#35988,#35984,#27868,.T.);
#45564=EDGE_CURVE('',#35988,#35987,#27869,.F.);
#45565=EDGE_CURVE('',#35967,#35989,#27870,.T.);
#45566=EDGE_CURVE('',#35989,#35988,#19146,.T.);
#45567=EDGE_CURVE('',#35990,#35970,#27871,.T.);
#45568=EDGE_CURVE('',#35991,#35990,#19147,.F.);
#45569=EDGE_CURVE('',#35992,#35991,#27872,.T.);
#45570=EDGE_CURVE('',#35992,#35993,#19148,.F.);
#45571=EDGE_CURVE('',#35994,#35993,#27873,.T.);
#45572=EDGE_CURVE('',#35994,#35995,#166,.T.);
#45573=EDGE_CURVE('',#35996,#35995,#23676,.T.);
#45574=EDGE_CURVE('',#35997,#35996,#23677,.F.);
#45575=EDGE_CURVE('',#35998,#35997,#23678,.F.);
#45576=EDGE_CURVE('',#35999,#35998,#23679,.T.);
#45577=EDGE_CURVE('',#35999,#36000,#167,.T.);
#45578=EDGE_CURVE('',#36001,#36000,#27874,.T.);
#45579=EDGE_CURVE('',#36001,#35989,#19149,.T.);
#45580=EDGE_CURVE('',#35889,#36002,#27875,.T.);
#45581=EDGE_CURVE('',#36002,#35924,#19150,.F.);
#45582=EDGE_CURVE('',#36003,#35891,#27876,.T.);
#45583=EDGE_CURVE('',#36002,#36003,#27877,.T.);
#45584=EDGE_CURVE('',#35966,#36003,#19151,.T.);
#45585=EDGE_CURVE('',#35856,#36004,#27878,.T.);
#45586=EDGE_CURVE('',#36004,#35874,#19152,.T.);
#45587=EDGE_CURVE('',#36004,#35866,#19153,.T.);
#45588=EDGE_CURVE('',#36005,#36006,#19154,.F.);
#45589=EDGE_CURVE('',#36006,#36007,#27879,.T.);
#45590=EDGE_CURVE('',#36007,#36008,#19155,.T.);
#45591=EDGE_CURVE('',#36008,#36005,#27880,.T.);
#45592=EDGE_CURVE('',#36005,#36009,#27881,.T.);
#45593=EDGE_CURVE('',#36010,#36008,#27882,.T.);
#45594=EDGE_CURVE('',#36011,#36010,#27883,.T.);
#45595=EDGE_CURVE('',#36012,#36011,#27884,.F.);
#45596=EDGE_CURVE('',#36013,#36012,#27885,.T.);
#45597=EDGE_CURVE('',#36014,#36013,#27886,.T.);
#45598=EDGE_CURVE('',#36009,#36014,#27887,.T.);
#45599=EDGE_CURVE('',#36015,#36006,#27888,.T.);
#45600=EDGE_CURVE('',#36016,#36015,#27889,.T.);
#45601=EDGE_CURVE('',#36007,#36016,#27890,.T.);
#45602=EDGE_CURVE('',#35964,#36009,#19156,.T.);
#45603=EDGE_CURVE('',#36014,#35965,#19157,.F.);
#45604=EDGE_CURVE('',#35897,#36017,#27891,.T.);
#45605=EDGE_CURVE('',#36017,#35952,#19158,.T.);
#45606=EDGE_CURVE('',#36010,#36018,#19159,.T.);
#45607=EDGE_CURVE('',#36018,#36019,#27892,.T.);
#45608=EDGE_CURVE('',#36019,#36011,#19160,.F.);
#45609=EDGE_CURVE('',#36020,#36015,#19161,.T.);
#45610=EDGE_CURVE('',#36020,#36021,#27893,.T.);
#45611=EDGE_CURVE('',#36021,#36016,#19162,.T.);
#45612=EDGE_CURVE('',#36020,#36022,#19163,.T.);
#45613=EDGE_CURVE('',#36023,#36022,#27894,.T.);
#45614=EDGE_CURVE('',#36021,#36023,#19164,.T.);
#45615=EDGE_CURVE('',#36024,#36018,#27895,.T.);
#45616=EDGE_CURVE('',#36025,#36024,#27896,.T.);
#45617=EDGE_CURVE('',#36019,#36025,#27897,.F.);
#45618=EDGE_CURVE('',#36025,#36026,#19165,.T.);
#45619=EDGE_CURVE('',#36027,#36024,#19166,.T.);
#45620=EDGE_CURVE('',#36026,#36027,#27898,.T.);
#45621=EDGE_CURVE('',#36028,#36028,#19167,.F.);
#45622=EDGE_CURVE('',#36029,#36029,#19168,.F.);
#45623=EDGE_CURVE('',#36030,#36030,#19169,.T.);
#45624=EDGE_CURVE('',#36030,#36029,#27899,.T.);
#45625=EDGE_CURVE('',#36031,#36031,#19170,.F.);
#45626=EDGE_CURVE('',#36031,#36028,#27900,.T.);
#45627=EDGE_CURVE('',#36032,#35774,#27901,.T.);
#45628=EDGE_CURVE('',#36032,#36033,#27902,.T.);
#45629=EDGE_CURVE('',#36033,#36034,#27903,.T.);
#45630=EDGE_CURVE('',#36035,#36034,#27904,.T.);
#45631=EDGE_CURVE('',#36036,#36035,#27905,.T.);
#45632=EDGE_CURVE('',#36037,#36036,#27906,.T.);
#45633=EDGE_CURVE('',#36038,#36037,#27907,.T.);
#45634=EDGE_CURVE('',#36038,#36039,#27908,.T.);
#45635=EDGE_CURVE('',#35773,#36039,#27909,.T.);
#45636=EDGE_CURVE('',#35752,#36040,#27910,.T.);
#45637=EDGE_CURVE('',#36032,#36040,#19171,.F.);
#45638=EDGE_CURVE('',#36041,#35755,#27911,.T.);
#45639=EDGE_CURVE('',#36040,#36041,#19172,.T.);
#45640=EDGE_CURVE('',#35776,#36041,#19173,.T.);
#45641=EDGE_CURVE('',#36037,#36042,#19174,.T.);
#45642=EDGE_CURVE('',#36042,#36043,#27912,.T.);
#45643=EDGE_CURVE('',#36043,#36038,#19175,.F.);
#45644=EDGE_CURVE('',#36044,#36045,#19176,.F.);
#45645=EDGE_CURVE('',#36045,#36046,#27913,.T.);
#45646=EDGE_CURVE('',#36046,#36047,#19177,.T.);
#45647=EDGE_CURVE('',#36047,#36044,#27914,.T.);
#45648=EDGE_CURVE('',#36048,#36047,#27915,.T.);
#45649=EDGE_CURVE('',#36049,#36048,#27916,.T.);
#45650=EDGE_CURVE('',#36044,#36049,#27917,.F.);
#45651=EDGE_CURVE('',#35771,#36050,#27918,.T.);
#45652=EDGE_CURVE('',#36050,#35781,#19178,.T.);
#45653=EDGE_CURVE('',#36051,#36045,#27919,.T.);
#45654=EDGE_CURVE('',#36052,#36051,#27920,.T.);
#45655=EDGE_CURVE('',#36046,#36052,#27921,.T.);
#45656=EDGE_CURVE('',#36053,#36051,#19179,.T.);
#45657=EDGE_CURVE('',#36053,#36054,#27922,.T.);
#45658=EDGE_CURVE('',#36054,#36052,#19180,.T.);
#45659=EDGE_CURVE('',#36055,#36056,#19181,.T.);
#45660=EDGE_CURVE('',#36056,#36057,#27923,.T.);
#45661=EDGE_CURVE('',#36057,#36058,#19182,.F.);
#45662=EDGE_CURVE('',#36058,#36055,#27924,.T.);
#45663=EDGE_CURVE('',#36034,#36056,#19183,.T.);
#45664=EDGE_CURVE('',#36057,#36033,#19184,.T.);
#45665=EDGE_CURVE('',#36059,#36059,#19185,.T.);
#45666=EDGE_CURVE('',#36059,#36060,#27925,.T.);
#45667=EDGE_CURVE('',#36060,#36060,#19186,.F.);
#45668=EDGE_CURVE('',#36035,#36061,#19187,.T.);
#45669=EDGE_CURVE('',#36061,#36062,#27926,.T.);
#45670=EDGE_CURVE('',#36062,#36036,#19188,.F.);
#45671=EDGE_CURVE('',#36063,#36064,#27927,.T.);
#45672=EDGE_CURVE('',#36064,#36065,#19189,.T.);
#45673=EDGE_CURVE('',#36065,#36066,#27928,.T.);
#45674=EDGE_CURVE('',#36066,#36063,#19190,.T.);
#45675=EDGE_CURVE('',#36067,#36068,#23680,.T.);
#45676=EDGE_CURVE('',#36067,#36069,#27929,.T.);
#45677=EDGE_CURVE('',#36070,#36069,#23681,.T.);
#45678=EDGE_CURVE('',#36068,#36070,#27930,.T.);
#45679=EDGE_CURVE('',#35877,#36071,#27931,.T.);
#45680=EDGE_CURVE('',#36072,#36071,#23682,.T.);
#45681=EDGE_CURVE('',#35878,#36072,#27932,.T.);
#45682=EDGE_CURVE('',#36073,#36073,#19191,.T.);
#45683=EDGE_CURVE('',#36073,#36074,#27933,.T.);
#45684=EDGE_CURVE('',#36074,#36074,#19192,.T.);
#45685=EDGE_CURVE('',#36075,#36076,#27934,.T.);
#45686=EDGE_CURVE('',#36076,#36075,#19193,.T.);
#45687=EDGE_CURVE('',#36077,#36077,#19194,.T.);
#45688=EDGE_CURVE('',#36077,#36074,#27935,.T.);
#45689=EDGE_CURVE('',#36078,#36078,#19195,.T.);
#45690=EDGE_CURVE('',#36078,#36079,#27936,.T.);
#45691=EDGE_CURVE('',#36079,#36079,#19196,.T.);
#45692=EDGE_CURVE('',#36080,#36081,#27937,.T.);
#45693=EDGE_CURVE('',#36081,#36080,#19197,.T.);
#45694=EDGE_CURVE('',#36082,#36082,#19198,.T.);
#45695=EDGE_CURVE('',#36082,#36079,#27938,.T.);
#45696=EDGE_CURVE('',#35871,#36075,#4097,.T.);
#45697=EDGE_CURVE('',#36076,#35872,#4098,.T.);
#45698=EDGE_CURVE('',#36083,#36084,#19199,.T.);
#45699=EDGE_CURVE('',#36085,#36084,#27939,.T.);
#45700=EDGE_CURVE('',#36086,#36085,#27940,.T.);
#45701=EDGE_CURVE('',#36086,#36087,#19200,.T.);
#45702=EDGE_CURVE('',#36088,#36087,#27941,.T.);
#45703=EDGE_CURVE('',#36083,#36088,#27942,.T.);
#45704=EDGE_CURVE('',#36089,#36090,#19201,.T.);
#45705=EDGE_CURVE('',#36091,#36090,#27943,.T.);
#45706=EDGE_CURVE('',#36092,#36091,#27944,.T.);
#45707=EDGE_CURVE('',#36092,#36093,#19202,.T.);
#45708=EDGE_CURVE('',#36094,#36093,#27945,.T.);
#45709=EDGE_CURVE('',#36089,#36094,#27946,.T.);
#45710=EDGE_CURVE('',#36095,#36085,#27947,.T.);
#45711=EDGE_CURVE('',#36095,#36096,#27948,.T.);
#45712=EDGE_CURVE('',#36086,#36096,#27949,.T.);
#45713=EDGE_CURVE('',#36096,#36097,#19203,.T.);
#45714=EDGE_CURVE('',#36097,#36098,#19204,.T.);
#45715=EDGE_CURVE('',#36087,#36098,#27950,.T.);
#45716=EDGE_CURVE('',#36098,#36099,#27951,.T.);
#45717=EDGE_CURVE('',#36088,#36099,#27952,.T.);
#45718=EDGE_CURVE('',#36100,#36091,#27953,.T.);
#45719=EDGE_CURVE('',#36100,#36101,#27954,.T.);
#45720=EDGE_CURVE('',#36092,#36101,#27955,.T.);
#45721=EDGE_CURVE('',#36101,#36102,#19205,.T.);
#45722=EDGE_CURVE('',#36102,#36103,#19206,.T.);
#45723=EDGE_CURVE('',#36093,#36103,#27956,.T.);
#45724=EDGE_CURVE('',#36103,#36104,#27957,.T.);
#45725=EDGE_CURVE('',#36094,#36104,#27958,.T.);
#45726=EDGE_CURVE('',#36101,#36103,#19207,.T.);
#45727=EDGE_CURVE('',#36102,#36105,#19208,.T.);
#45728=EDGE_CURVE('',#36104,#36100,#19209,.T.);
#45729=EDGE_CURVE('',#36096,#36098,#19210,.T.);
#45730=EDGE_CURVE('',#36097,#36106,#19211,.T.);
#45731=EDGE_CURVE('',#36099,#36095,#19212,.T.);
#45732=EDGE_CURVE('',#36107,#36108,#4099,.T.);
#45733=EDGE_CURVE('',#36109,#36108,#27959,.T.);
#45734=EDGE_CURVE('',#36110,#36109,#27960,.T.);
#45735=EDGE_CURVE('',#36110,#36107,#27961,.T.);
#45736=EDGE_CURVE('',#36111,#36107,#19213,.T.);
#45737=EDGE_CURVE('',#36112,#36110,#19214,.T.);
#45738=EDGE_CURVE('',#36112,#36111,#27962,.T.);
#45739=EDGE_CURVE('',#36113,#36111,#4100,.T.);
#45740=EDGE_CURVE('',#36114,#36112,#27963,.T.);
#45741=EDGE_CURVE('',#36113,#36114,#27964,.T.);
#45742=EDGE_CURVE('',#36090,#36113,#4101,.T.);
#45743=EDGE_CURVE('',#36108,#36089,#4102,.T.);
#45744=EDGE_CURVE('',#36115,#36116,#4103,.T.);
#45745=EDGE_CURVE('',#36117,#36116,#27965,.T.);
#45746=EDGE_CURVE('',#36118,#36117,#27966,.T.);
#45747=EDGE_CURVE('',#36118,#36115,#27967,.T.);
#45748=EDGE_CURVE('',#36119,#36115,#19215,.T.);
#45749=EDGE_CURVE('',#36120,#36118,#19216,.T.);
#45750=EDGE_CURVE('',#36120,#36119,#27968,.T.);
#45751=EDGE_CURVE('',#36121,#36119,#4104,.T.);
#45752=EDGE_CURVE('',#36122,#36120,#27969,.T.);
#45753=EDGE_CURVE('',#36121,#36122,#27970,.T.);
#45754=EDGE_CURVE('',#36084,#36121,#4105,.T.);
#45755=EDGE_CURVE('',#36116,#36083,#4106,.T.);
#45756=EDGE_CURVE('',#36123,#36061,#27971,.T.);
#45757=EDGE_CURVE('',#36123,#36124,#27972,.T.);
#45758=EDGE_CURVE('',#36124,#36062,#27973,.F.);
#45759=EDGE_CURVE('',#35744,#36042,#27974,.T.);
#45760=EDGE_CURVE('',#35743,#36043,#27975,.T.);
#45761=EDGE_CURVE('',#36125,#35869,#23683,.T.);
#45762=EDGE_CURVE('',#35883,#35868,#27976,.T.);
#45763=EDGE_CURVE('',#35882,#36126,#23684,.F.);
#45764=EDGE_CURVE('',#36125,#36126,#27977,.F.);
#45765=EDGE_CURVE('',#36125,#36127,#27978,.T.);
#45766=EDGE_CURVE('',#36128,#36126,#27979,.T.);
#45767=EDGE_CURVE('',#36127,#36128,#27980,.T.);
#45768=EDGE_CURVE('',#36129,#36130,#19217,.T.);
#45769=EDGE_CURVE('',#36130,#36131,#27981,.T.);
#45770=EDGE_CURVE('',#36132,#36131,#23685,.F.);
#45771=EDGE_CURVE('',#36132,#36129,#27982,.T.);
#45772=EDGE_CURVE('',#36133,#36134,#27983,.T.);
#45773=EDGE_CURVE('',#36133,#36135,#27984,.T.);
#45774=EDGE_CURVE('',#36135,#36136,#19218,.T.);
#45775=EDGE_CURVE('',#36134,#36136,#27985,.F.);
#45776=EDGE_CURVE('',#36134,#36137,#27986,.T.);
#45777=EDGE_CURVE('',#36136,#36138,#27987,.F.);
#45778=EDGE_CURVE('',#36138,#36137,#27988,.T.);
#45779=EDGE_CURVE('',#36139,#36140,#23686,.T.);
#45780=EDGE_CURVE('',#36132,#36140,#27989,.F.);
#45781=EDGE_CURVE('',#36131,#36135,#23687,.T.);
#45782=EDGE_CURVE('',#36139,#36133,#19219,.F.);
#45783=EDGE_CURVE('',#36141,#36141,#19220,.T.);
#45784=EDGE_CURVE('',#36142,#36142,#19221,.T.);
#45785=EDGE_CURVE('',#36143,#36143,#19222,.T.);
#45786=EDGE_CURVE('',#36143,#36141,#27990,.T.);
#45787=EDGE_CURVE('',#36144,#36145,#23688,.T.);
#45788=EDGE_CURVE('',#36080,#36145,#4107,.F.);
#45789=EDGE_CURVE('',#36081,#36146,#4108,.T.);
#45790=EDGE_CURVE('',#36146,#36144,#19223,.T.);
#45791=EDGE_CURVE('',#36147,#36140,#27991,.T.);
#45792=EDGE_CURVE('',#36129,#36147,#27992,.T.);
#45793=EDGE_CURVE('',#36139,#36148,#27993,.T.);
#45794=EDGE_CURVE('',#36148,#36147,#19224,.T.);
#45795=EDGE_CURVE('',#36144,#36149,#27994,.T.);
#45796=EDGE_CURVE('',#36148,#36146,#27995,.T.);
#45797=EDGE_CURVE('',#36137,#36149,#19225,.T.);
#45798=EDGE_CURVE('',#36150,#36151,#27996,.F.);
#45799=EDGE_CURVE('',#36150,#36149,#23689,.T.);
#45800=EDGE_CURVE('',#36152,#36138,#23690,.F.);
#45801=EDGE_CURVE('',#36151,#36152,#23691,.T.);
#45802=EDGE_CURVE('',#36153,#36150,#19226,.F.);
#45803=EDGE_CURVE('',#36153,#36154,#27997,.T.);
#45804=EDGE_CURVE('',#36154,#36145,#19227,.T.);
#45805=EDGE_CURVE('',#36151,#36155,#19228,.T.);
#45806=EDGE_CURVE('',#36153,#36155,#19229,.F.);
#45807=EDGE_CURVE('',#36127,#35870,#19230,.T.);
#45808=EDGE_CURVE('',#36154,#36156,#19231,.T.);
#45809=EDGE_CURVE('',#36156,#36155,#27998,.T.);
#45810=EDGE_CURVE('',#36157,#36158,#23692,.T.);
#45811=EDGE_CURVE('',#36156,#36157,#19232,.T.);
#45812=EDGE_CURVE('',#36152,#36158,#27999,.T.);
#45813=EDGE_CURVE('',#36159,#36160,#28000,.T.);
#45814=EDGE_CURVE('',#36068,#36159,#28001,.T.);
#45815=EDGE_CURVE('',#36160,#36070,#28002,.T.);
#45816=EDGE_CURVE('',#36160,#36161,#23693,.T.);
#45817=EDGE_CURVE('',#36161,#36157,#28003,.T.);
#45818=EDGE_CURVE('',#36158,#36159,#23694,.T.);
#45819=EDGE_CURVE('',#36162,#36163,#28004,.T.);
#45820=EDGE_CURVE('',#36069,#36162,#28005,.T.);
#45821=EDGE_CURVE('',#36163,#36067,#28006,.T.);
#45822=EDGE_CURVE('',#36163,#36164,#23695,.T.);
#45823=EDGE_CURVE('',#36130,#36164,#19233,.T.);
#45824=EDGE_CURVE('',#35881,#36128,#19234,.T.);
#45825=EDGE_CURVE('',#35879,#36165,#28007,.T.);
#45826=EDGE_CURVE('',#36165,#36072,#28008,.T.);
#45827=EDGE_CURVE('',#36022,#36066,#19235,.F.);
#45828=EDGE_CURVE('',#36166,#36065,#19236,.T.);
#45829=EDGE_CURVE('',#36165,#36166,#23696,.T.);
#45830=EDGE_CURVE('',#36071,#36167,#28009,.T.);
#45831=EDGE_CURVE('',#36168,#36167,#23697,.T.);
#45832=EDGE_CURVE('',#36023,#36168,#19237,.T.);
#45833=EDGE_CURVE('',#36167,#35876,#28010,.T.);
#45834=EDGE_CURVE('',#36169,#36162,#23698,.T.);
#45835=EDGE_CURVE('',#36064,#36169,#19238,.F.);
#45836=EDGE_CURVE('',#36124,#36063,#19239,.F.);
#45837=EDGE_CURVE('',#36161,#36123,#19240,.T.);
#45838=EDGE_CURVE('',#36164,#36169,#28011,.T.);
#45839=EDGE_CURVE('',#36166,#35880,#28012,.T.);
#45840=EDGE_CURVE('',#35875,#36168,#28013,.T.);
#45841=EDGE_CURVE('',#36055,#36027,#28014,.T.);
#45842=EDGE_CURVE('',#36053,#36114,#28015,.F.);
#45843=EDGE_CURVE('',#36109,#36122,#28016,.F.);
#45844=EDGE_CURVE('',#36026,#36117,#28017,.T.);
#45845=EDGE_CURVE('',#36054,#36058,#28018,.T.);
#45846=EDGE_CURVE('',#36170,#36171,#23699,.T.);
#45847=EDGE_CURVE('',#36171,#36172,#28019,.T.);
#45848=EDGE_CURVE('',#36172,#36173,#19241,.T.);
#45849=EDGE_CURVE('',#36173,#36170,#28020,.T.);
#45850=EDGE_CURVE('',#35641,#36174,#23700,.T.);
#45851=EDGE_CURVE('',#36174,#36175,#28021,.T.);
#45852=EDGE_CURVE('',#36175,#35642,#19242,.T.);
#45853=EDGE_CURVE('',#36176,#36177,#23701,.T.);
#45854=EDGE_CURVE('',#36177,#36178,#23702,.T.);
#45855=EDGE_CURVE('',#36179,#36178,#19243,.F.);
#45856=EDGE_CURVE('',#36179,#35681,#23703,.T.);
#45857=EDGE_CURVE('',#36180,#35680,#23704,.T.);
#45858=EDGE_CURVE('',#36180,#36176,#19244,.T.);
#45859=EDGE_CURVE('',#36181,#36182,#28022,.T.);
#45860=EDGE_CURVE('',#36183,#36181,#19245,.T.);
#45861=EDGE_CURVE('',#35705,#36183,#23705,.T.);
#45862=EDGE_CURVE('',#36182,#35704,#19246,.F.);
#45863=EDGE_CURVE('',#36175,#36173,#19247,.T.);
#45864=EDGE_CURVE('',#36170,#36174,#19248,.T.);
#45865=EDGE_CURVE('',#36179,#35667,#28023,.T.);
#45866=EDGE_CURVE('',#36184,#36185,#28024,.T.);
#45867=EDGE_CURVE('',#36186,#36184,#23706,.T.);
#45868=EDGE_CURVE('',#35640,#36186,#23707,.T.);
#45869=EDGE_CURVE('',#36185,#35639,#23708,.F.);
#45870=EDGE_CURVE('',#36187,#36188,#23709,.T.);
#45871=EDGE_CURVE('',#36187,#36189,#28025,.T.);
#45872=EDGE_CURVE('',#36189,#36190,#19249,.T.);
#45873=EDGE_CURVE('',#36190,#36188,#28026,.T.);
#45874=EDGE_CURVE('',#36191,#36190,#19250,.T.);
#45875=EDGE_CURVE('',#36192,#36191,#28027,.T.);
#45876=EDGE_CURVE('',#36192,#36193,#23710,.T.);
#45877=EDGE_CURVE('',#36193,#36194,#23711,.T.);
#45878=EDGE_CURVE('',#36194,#36195,#23712,.T.);
#45879=EDGE_CURVE('',#36195,#36188,#23713,.T.);
#45880=EDGE_CURVE('',#35644,#36196,#23714,.T.);
#45881=EDGE_CURVE('',#35643,#36197,#19251,.T.);
#45882=EDGE_CURVE('',#36197,#36196,#28028,.T.);
#45883=EDGE_CURVE('',#36187,#36198,#23715,.T.);
#45884=EDGE_CURVE('',#36198,#36199,#23716,.T.);
#45885=EDGE_CURVE('',#36199,#36196,#23717,.T.);
#45886=EDGE_CURVE('',#36189,#36197,#19252,.T.);
#45887=EDGE_CURVE('',#36200,#36200,#19253,.T.);
#45888=EDGE_CURVE('',#36200,#36201,#28029,.T.);
#45889=EDGE_CURVE('',#36201,#36201,#19254,.T.);
#45890=EDGE_CURVE('',#36202,#36202,#19255,.T.);
#45891=EDGE_CURVE('',#36200,#36203,#28030,.T.);
#45892=EDGE_CURVE('',#36203,#36203,#19256,.T.);
#45893=EDGE_CURVE('',#36202,#36204,#28031,.T.);
#45894=EDGE_CURVE('',#36204,#36204,#19257,.T.);
#45895=EDGE_CURVE('',#36205,#36205,#19258,.F.);
#45896=EDGE_CURVE('',#36205,#36206,#28032,.T.);
#45897=EDGE_CURVE('',#36206,#36206,#19259,.F.);
#45898=EDGE_CURVE('',#36178,#35668,#23718,.T.);
#45899=EDGE_CURVE('',#36207,#36207,#19260,.T.);
#45900=EDGE_CURVE('',#36207,#36208,#28033,.T.);
#45901=EDGE_CURVE('',#36208,#36208,#19261,.T.);
#45902=EDGE_CURVE('',#35692,#36209,#28034,.T.);
#45903=EDGE_CURVE('',#36209,#35707,#23719,.T.);
#45904=EDGE_CURVE('',#36210,#36210,#19262,.T.);
#45905=EDGE_CURVE('',#36210,#36211,#28035,.T.);
#45906=EDGE_CURVE('',#36211,#36211,#19263,.T.);
#45907=EDGE_CURVE('',#36211,#36212,#28036,.T.);
#45908=EDGE_CURVE('',#36212,#36212,#19264,.T.);
#45909=EDGE_CURVE('',#36213,#36214,#19265,.T.);
#45910=EDGE_CURVE('',#36214,#36215,#28037,.T.);
#45911=EDGE_CURVE('',#36215,#36216,#19266,.F.);
#45912=EDGE_CURVE('',#36216,#36213,#28038,.T.);
#45913=EDGE_CURVE('',#36217,#36218,#28039,.T.);
#45914=EDGE_CURVE('',#36219,#36217,#19267,.F.);
#45915=EDGE_CURVE('',#36220,#36219,#28040,.T.);
#45916=EDGE_CURVE('',#36218,#36220,#19268,.F.);
#45917=EDGE_CURVE('',#36221,#36222,#28041,.T.);
#45918=EDGE_CURVE('',#36222,#36217,#19269,.T.);
#45919=EDGE_CURVE('',#36218,#36221,#19270,.T.);
#45920=EDGE_CURVE('',#35575,#36223,#28042,.T.);
#45921=EDGE_CURVE('',#36223,#35677,#19271,.F.);
#45922=EDGE_CURVE('',#36224,#35574,#28043,.T.);
#45923=EDGE_CURVE('',#36223,#36224,#28044,.T.);
#45924=EDGE_CURVE('',#36224,#36225,#19272,.T.);
#45925=EDGE_CURVE('',#36225,#35573,#28045,.T.);
#45926=EDGE_CURVE('',#36226,#35611,#28046,.T.);
#45927=EDGE_CURVE('',#36226,#36227,#19273,.F.);
#45928=EDGE_CURVE('',#36227,#36228,#28047,.T.);
#45929=EDGE_CURVE('',#36229,#36228,#23720,.T.);
#45930=EDGE_CURVE('',#36230,#36229,#23721,.T.);
#45931=EDGE_CURVE('',#36230,#35612,#28048,.T.);
#45932=EDGE_CURVE('',#36231,#36231,#19274,.T.);
#45933=EDGE_CURVE('',#36231,#36232,#28049,.T.);
#45934=EDGE_CURVE('',#36232,#36232,#19275,.T.);
#45935=EDGE_CURVE('',#36233,#35614,#28050,.T.);
#45936=EDGE_CURVE('',#36226,#36233,#28051,.T.);
#45937=EDGE_CURVE('',#36234,#35622,#23722,.T.);
#45938=EDGE_CURVE('',#36234,#36235,#28052,.T.);
#45939=EDGE_CURVE('',#36235,#36233,#19276,.F.);
#45940=EDGE_CURVE('',#35917,#36236,#19277,.F.);
#45941=EDGE_CURVE('',#36236,#35936,#28053,.T.);
#45942=EDGE_CURVE('',#35625,#36229,#28054,.T.);
#45943=EDGE_CURVE('',#35625,#36230,#19278,.T.);
#45944=EDGE_CURVE('',#35621,#36237,#28055,.T.);
#45945=EDGE_CURVE('',#36237,#36238,#19279,.T.);
#45946=EDGE_CURVE('',#36234,#36238,#23723,.F.);
#45947=EDGE_CURVE('',#35950,#35920,#19280,.F.);
#45948=EDGE_CURVE('',#36239,#36239,#19281,.T.);
#45949=EDGE_CURVE('',#36240,#36240,#19282,.T.);
#45950=EDGE_CURVE('',#36241,#36241,#19283,.T.);
#45951=EDGE_CURVE('',#36239,#36242,#28056,.T.);
#45952=EDGE_CURVE('',#36242,#36242,#19284,.F.);
#45953=EDGE_CURVE('',#36241,#36243,#28057,.T.);
#45954=EDGE_CURVE('',#36243,#36243,#19285,.F.);
#45955=EDGE_CURVE('',#36244,#36245,#4109,.T.);
#45956=EDGE_CURVE('',#36245,#36237,#19286,.T.);
#45957=EDGE_CURVE('',#35623,#36244,#19287,.T.);
#45958=EDGE_CURVE('',#36213,#36219,#19288,.T.);
#45959=EDGE_CURVE('',#36216,#36220,#19289,.F.);
#45960=EDGE_CURVE('',#36246,#36246,#19290,.T.);
#45961=EDGE_CURVE('',#36246,#35670,#28058,.T.);
#45962=EDGE_CURVE('',#36232,#36203,#28059,.T.);
#45963=EDGE_CURVE('',#36247,#36247,#19291,.T.);
#45964=EDGE_CURVE('',#36248,#36248,#19292,.T.);
#45965=EDGE_CURVE('',#36249,#36250,#19293,.T.);
#45966=EDGE_CURVE('',#36250,#36248,#28060,.T.);
#45967=EDGE_CURVE('',#36250,#36249,#19294,.T.);
#45968=EDGE_CURVE('',#35669,#36251,#19295,.F.);
#45969=EDGE_CURVE('',#36251,#35651,#23724,.F.);
#45970=EDGE_CURVE('',#36252,#36185,#23725,.T.);
#45971=EDGE_CURVE('',#35653,#36253,#23726,.F.);
#45972=EDGE_CURVE('',#36253,#36252,#19296,.F.);
#45973=EDGE_CURVE('',#36254,#36182,#23727,.T.);
#45974=EDGE_CURVE('',#36209,#36254,#23728,.F.);
#45975=EDGE_CURVE('',#36204,#36247,#28061,.T.);
#45976=EDGE_CURVE('',#36255,#36251,#23729,.T.);
#45977=EDGE_CURVE('',#36194,#36255,#19297,.F.);
#45978=EDGE_CURVE('',#35661,#36193,#19298,.F.);
#45979=EDGE_CURVE('',#35652,#35660,#19299,.F.);
#45980=EDGE_CURVE('',#35685,#36195,#19300,.T.);
#45981=EDGE_CURVE('',#35647,#35686,#19301,.F.);
#45982=EDGE_CURVE('',#36198,#35646,#19302,.F.);
#45983=EDGE_CURVE('',#35686,#35648,#4110,.T.);
#45984=EDGE_CURVE('',#35645,#36199,#19303,.T.);
#45985=EDGE_CURVE('',#36256,#36257,#28062,.T.);
#45986=EDGE_CURVE('',#36256,#36192,#168,.T.);
#45987=EDGE_CURVE('',#36257,#36191,#28063,.T.);
#45988=EDGE_CURVE('',#36258,#35672,#23730,.T.);
#45989=EDGE_CURVE('',#36256,#36258,#23731,.T.);
#45990=EDGE_CURVE('',#35673,#36257,#19304,.F.);
#45991=EDGE_CURVE('',#36259,#36260,#28064,.T.);
#45992=EDGE_CURVE('',#36261,#36259,#28065,.T.);
#45993=EDGE_CURVE('',#36261,#36262,#28066,.T.);
#45994=EDGE_CURVE('',#36260,#36262,#28067,.T.);
#45995=EDGE_CURVE('',#36263,#36264,#28068,.T.);
#45996=EDGE_CURVE('',#36263,#36265,#28069,.T.);
#45997=EDGE_CURVE('',#36266,#36265,#28070,.T.);
#45998=EDGE_CURVE('',#36264,#36266,#19305,.T.);
#45999=EDGE_CURVE('',#36266,#36259,#23732,.T.);
#46000=EDGE_CURVE('',#36265,#36261,#19306,.T.);
#46001=EDGE_CURVE('',#35700,#36267,#19307,.T.);
#46002=EDGE_CURVE('',#35706,#36267,#19308,.T.);
#46003=EDGE_CURVE('',#36268,#36269,#19309,.T.);
#46004=EDGE_CURVE('',#36270,#36268,#23733,.T.);
#46005=EDGE_CURVE('',#36267,#36270,#28071,.T.);
#46006=EDGE_CURVE('',#36183,#36176,#23734,.T.);
#46007=EDGE_CURVE('',#36269,#36180,#28072,.T.);
#46008=EDGE_CURVE('',#36269,#35679,#19310,.T.);
#46009=EDGE_CURVE('',#35700,#36260,#19311,.T.);
#46010=EDGE_CURVE('',#36260,#36267,#19312,.T.);
#46011=EDGE_CURVE('',#36262,#35701,#19313,.T.);
#46012=EDGE_CURVE('',#36269,#36264,#19314,.T.);
#46013=EDGE_CURVE('',#36264,#35679,#19315,.T.);
#46014=EDGE_CURVE('',#36259,#36270,#19316,.T.);
#46015=EDGE_CURVE('',#36266,#36268,#19317,.T.);
#46016=EDGE_CURVE('',#35678,#36263,#19318,.T.);
#46017=EDGE_CURVE('',#36252,#36271,#28073,.T.);
#46018=EDGE_CURVE('',#36253,#36255,#23735,.T.);
#46019=EDGE_CURVE('',#36271,#36177,#19319,.T.);
#46020=EDGE_CURVE('',#36184,#36271,#23736,.T.);
#46021=EDGE_CURVE('',#36272,#35694,#28074,.T.);
#46022=EDGE_CURVE('',#36172,#36272,#19320,.T.);
#46023=EDGE_CURVE('',#36273,#36171,#23737,.T.);
#46024=EDGE_CURVE('',#36254,#36273,#28075,.T.);
#46025=EDGE_CURVE('',#36181,#36273,#23738,.T.);
#46026=EDGE_CURVE('',#36258,#36274,#23739,.T.);
#46027=EDGE_CURVE('',#36275,#35672,#19321,.T.);
#46028=EDGE_CURVE('',#36275,#36274,#19322,.T.);
#46029=EDGE_CURVE('',#35662,#36275,#19323,.T.);
#46030=EDGE_CURVE('',#36276,#35789,#28076,.T.);
#46031=EDGE_CURVE('',#36277,#36276,#28077,.T.);
#46032=EDGE_CURVE('',#35787,#36277,#28078,.T.);
#46033=EDGE_CURVE('',#36277,#35812,#19324,.T.);
#46034=EDGE_CURVE('',#36278,#35791,#28079,.T.);
#46035=EDGE_CURVE('',#36276,#36278,#19325,.T.);
#46036=EDGE_CURVE('',#35702,#36272,#19326,.T.);
#46037=EDGE_CURVE('',#36279,#35572,#28080,.T.);
#46038=EDGE_CURVE('',#36280,#36279,#28081,.T.);
#46039=EDGE_CURVE('',#36281,#36280,#28082,.T.);
#46040=EDGE_CURVE('',#36281,#36225,#28083,.T.);
#46041=EDGE_CURVE('',#36282,#36280,#19327,.T.);
#46042=EDGE_CURVE('',#36282,#36283,#28084,.T.);
#46043=EDGE_CURVE('',#36283,#36281,#19328,.T.);
#46044=EDGE_CURVE('',#36284,#36285,#19329,.T.);
#46045=EDGE_CURVE('',#36284,#36286,#28085,.T.);
#46046=EDGE_CURVE('',#36286,#36287,#19330,.T.);
#46047=EDGE_CURVE('',#36287,#36285,#28086,.T.);
#46048=EDGE_CURVE('',#36288,#36284,#28087,.F.);
#46049=EDGE_CURVE('',#36289,#36288,#28088,.T.);
#46050=EDGE_CURVE('',#36286,#36289,#28089,.T.);
#46051=EDGE_CURVE('',#36290,#36288,#19331,.T.);
#46052=EDGE_CURVE('',#36290,#36291,#28090,.T.);
#46053=EDGE_CURVE('',#36291,#36289,#19332,.T.);
#46054=EDGE_CURVE('',#36292,#36293,#4111,.T.);
#46055=EDGE_CURVE('',#36293,#35624,#19333,.T.);
#46056=EDGE_CURVE('',#36294,#36228,#23740,.F.);
#46057=EDGE_CURVE('',#36294,#36292,#19334,.T.);
#46058=EDGE_CURVE('',#36238,#36050,#19335,.T.);
#46059=EDGE_CURVE('',#36245,#36295,#28091,.T.);
#46060=EDGE_CURVE('',#36048,#36295,#19336,.T.);
#46061=EDGE_CURVE('',#35793,#36296,#28092,.T.);
#46062=EDGE_CURVE('',#36296,#36278,#19337,.T.);
#46063=EDGE_CURVE('',#35602,#35581,#19338,.T.);
#46064=EDGE_CURVE('',#36297,#35578,#28093,.T.);
#46065=EDGE_CURVE('',#35559,#36297,#28094,.T.);
#46066=EDGE_CURVE('',#36297,#35676,#19339,.T.);
#46067=EDGE_CURVE('',#36298,#36299,#28095,.T.);
#46068=EDGE_CURVE('',#36300,#36298,#28096,.T.);
#46069=EDGE_CURVE('',#36301,#36300,#28097,.T.);
#46070=EDGE_CURVE('',#36301,#36299,#28098,.T.);
#46071=EDGE_CURVE('',#35675,#36298,#19340,.T.);
#46072=EDGE_CURVE('',#35674,#36300,#19341,.T.);
#46073=EDGE_CURVE('',#36302,#36303,#28099,.T.);
#46074=EDGE_CURVE('',#36304,#36302,#28100,.T.);
#46075=EDGE_CURVE('',#36305,#36304,#28101,.F.);
#46076=EDGE_CURVE('',#35569,#36305,#28102,.T.);
#46077=EDGE_CURVE('',#36306,#35568,#28103,.T.);
#46078=EDGE_CURVE('',#36307,#36306,#28104,.T.);
#46079=EDGE_CURVE('',#36303,#36307,#28105,.T.);
#46080=EDGE_CURVE('',#36305,#36308,#19342,.F.);
#46081=EDGE_CURVE('',#36308,#35570,#28106,.T.);
#46082=EDGE_CURVE('',#35571,#36309,#28107,.T.);
#46083=EDGE_CURVE('',#36309,#36308,#28108,.F.);
#46084=EDGE_CURVE('',#36309,#36279,#19343,.F.);
#46085=EDGE_CURVE('',#36310,#36311,#19344,.T.);
#46086=EDGE_CURVE('',#36310,#36292,#28109,.T.);
#46087=EDGE_CURVE('',#35807,#36294,#19345,.F.);
#46088=EDGE_CURVE('',#36296,#36287,#28110,.T.);
#46089=EDGE_CURVE('',#36291,#36311,#28111,.T.);
#46090=EDGE_CURVE('',#36311,#36312,#28112,.T.);
#46091=EDGE_CURVE('',#36312,#36290,#28113,.T.);
#46092=EDGE_CURVE('',#36312,#36313,#19346,.F.);
#46093=EDGE_CURVE('',#36313,#36310,#28114,.T.);
#46094=EDGE_CURVE('',#36295,#36314,#28115,.T.);
#46095=EDGE_CURVE('',#36314,#36049,#19347,.F.);
#46096=EDGE_CURVE('',#36315,#36316,#28116,.T.);
#46097=EDGE_CURVE('',#36299,#36315,#19348,.T.);
#46098=EDGE_CURVE('',#36316,#36301,#19349,.T.);
#46099=EDGE_CURVE('',#36316,#36317,#19350,.T.);
#46100=EDGE_CURVE('',#36283,#36318,#28117,.T.);
#46101=EDGE_CURVE('',#36214,#36318,#19351,.T.);
#46102=EDGE_CURVE('',#36222,#36317,#19352,.T.);
#46103=EDGE_CURVE('',#36317,#36319,#28118,.T.);
#46104=EDGE_CURVE('',#36319,#36315,#19353,.F.);
#46105=EDGE_CURVE('',#36320,#36321,#23741,.T.);
#46106=EDGE_CURVE('',#36319,#36321,#19354,.T.);
#46107=EDGE_CURVE('',#36221,#36322,#19355,.F.);
#46108=EDGE_CURVE('',#36323,#36322,#28119,.T.);
#46109=EDGE_CURVE('',#36320,#36323,#19356,.T.);
#46110=EDGE_CURVE('',#35603,#36323,#19357,.T.);
#46111=EDGE_CURVE('',#36322,#35604,#19358,.F.);
#46112=EDGE_CURVE('',#36324,#36325,#19359,.T.);
#46113=EDGE_CURVE('',#36325,#36324,#19360,.T.);
#46114=EDGE_CURVE('',#36325,#36240,#28120,.T.);
#46115=EDGE_CURVE('',#36326,#36321,#19361,.T.);
#46116=EDGE_CURVE('',#36320,#36326,#19362,.T.);
#46117=EDGE_CURVE('',#36326,#36324,#28121,.T.);
#46118=EDGE_CURVE('',#36327,#35974,#28122,.T.);
#46119=EDGE_CURVE('',#36328,#36327,#28123,.F.);
#46120=EDGE_CURVE('',#35972,#36328,#28124,.T.);
#46121=EDGE_CURVE('',#36329,#35751,#19363,.F.);
#46122=EDGE_CURVE('',#36330,#36329,#28125,.T.);
#46123=EDGE_CURVE('',#35954,#36330,#19364,.F.);
#46124=EDGE_CURVE('',#36331,#35953,#19365,.T.);
#46125=EDGE_CURVE('',#36332,#36331,#28126,.F.);
#46126=EDGE_CURVE('',#36333,#36332,#19366,.T.);
#46127=EDGE_CURVE('',#36333,#36236,#28127,.F.);
#46128=EDGE_CURVE('',#35986,#35916,#19367,.F.);
#46129=EDGE_CURVE('',#36334,#36001,#19368,.F.);
#46130=EDGE_CURVE('',#36335,#36334,#28128,.T.);
#46131=EDGE_CURVE('',#35842,#36335,#19369,.F.);
#46132=EDGE_CURVE('',#36336,#35850,#19370,.T.);
#46133=EDGE_CURVE('',#36336,#36337,#28129,.F.);
#46134=EDGE_CURVE('',#36338,#36337,#19371,.F.);
#46135=EDGE_CURVE('',#36338,#36339,#28130,.F.);
#46136=EDGE_CURVE('',#36339,#35836,#19372,.F.);
#46137=EDGE_CURVE('',#36340,#35840,#19373,.F.);
#46138=EDGE_CURVE('',#36227,#36340,#19374,.T.);
#46139=EDGE_CURVE('',#36039,#36235,#19375,.F.);
#46140=EDGE_CURVE('',#36328,#35990,#19376,.T.);
#46141=EDGE_CURVE('',#35845,#35996,#169,.T.);
#46142=EDGE_CURVE('',#35998,#35844,#170,.T.);
#46143=EDGE_CURVE('',#35997,#36249,#28131,.T.);
#46144=EDGE_CURVE('',#35956,#36341,#171,.T.);
#46145=EDGE_CURVE('',#36342,#35955,#172,.T.);
#46146=EDGE_CURVE('',#36343,#36342,#28132,.T.);
#46147=EDGE_CURVE('',#36341,#36343,#173,.T.);
#46148=EDGE_CURVE('',#36344,#36345,#28133,.T.);
#46149=EDGE_CURVE('',#36346,#36344,#28134,.T.);
#46150=EDGE_CURVE('',#36347,#36346,#28135,.T.);
#46151=EDGE_CURVE('',#36347,#36345,#28136,.T.);
#46152=EDGE_CURVE('',#36348,#36349,#28137,.T.);
#46153=EDGE_CURVE('',#36350,#36348,#28138,.T.);
#46154=EDGE_CURVE('',#36351,#36350,#28139,.T.);
#46155=EDGE_CURVE('',#36349,#36351,#28140,.T.);
#46156=EDGE_CURVE('',#35747,#35961,#174,.T.);
#46157=EDGE_CURVE('',#36350,#35746,#175,.T.);
#46158=EDGE_CURVE('',#35962,#36348,#176,.T.);
#46159=EDGE_CURVE('',#36343,#36329,#28141,.T.);
#46160=EDGE_CURVE('',#36330,#36342,#28142,.T.);
#46161=EDGE_CURVE('',#36341,#35750,#23742,.T.);
#46162=EDGE_CURVE('',#35745,#36351,#19377,.T.);
#46163=EDGE_CURVE('',#36349,#35963,#19378,.T.);
#46164=EDGE_CURVE('',#36346,#35848,#19379,.T.);
#46165=EDGE_CURVE('',#35847,#36347,#177,.T.);
#46166=EDGE_CURVE('',#35993,#36344,#19380,.T.);
#46167=EDGE_CURVE('',#36345,#35994,#178,.T.);
#46168=EDGE_CURVE('',#36352,#36334,#28143,.T.);
#46169=EDGE_CURVE('',#36353,#36352,#28144,.T.);
#46170=EDGE_CURVE('',#36335,#36353,#28145,.T.);
#46171=EDGE_CURVE('',#36000,#36352,#179,.T.);
#46172=EDGE_CURVE('',#35843,#36354,#23743,.T.);
#46173=EDGE_CURVE('',#36353,#36354,#180,.T.);
#46174=EDGE_CURVE('',#36354,#35999,#181,.T.);
#46175=EDGE_CURVE('',#35749,#35957,#182,.T.);
#46176=EDGE_CURVE('',#35959,#36355,#23744,.T.);
#46177=EDGE_CURVE('',#35961,#36355,#19381,.T.);
#46178=EDGE_CURVE('',#36355,#35748,#183,.T.);
#46179=EDGE_CURVE('',#35995,#35846,#184,.T.);
#46180=EDGE_CURVE('',#35839,#36356,#19382,.T.);
#46181=EDGE_CURVE('',#36356,#36340,#28146,.T.);
#46182=EDGE_CURVE('',#35818,#36336,#28147,.T.);
#46183=EDGE_CURVE('',#35822,#36338,#28148,.T.);
#46184=EDGE_CURVE('',#36337,#35820,#28149,.T.);
#46185=EDGE_CURVE('',#35913,#36327,#19383,.F.);
#46186=EDGE_CURVE('',#35565,#36357,#28150,.T.);
#46187=EDGE_CURVE('',#36357,#36358,#19384,.F.);
#46188=EDGE_CURVE('',#36358,#35566,#28151,.T.);
#46189=EDGE_CURVE('',#35567,#36359,#28152,.T.);
#46190=EDGE_CURVE('',#36359,#36358,#19385,.T.);
#46191=EDGE_CURVE('',#36359,#36306,#19386,.F.);
#46192=EDGE_CURVE('',#36307,#35992,#19387,.T.);
#46193=EDGE_CURVE('',#35599,#36357,#28153,.T.);
#46194=EDGE_CURVE('',#36356,#36215,#19388,.F.);
#46195=EDGE_CURVE('',#35991,#36303,#19389,.F.);
#46196=EDGE_CURVE('',#35934,#36333,#28154,.T.);
#46197=EDGE_CURVE('',#36332,#35932,#28155,.T.);
#46198=EDGE_CURVE('',#35930,#36331,#28156,.T.);
#46199=EDGE_CURVE('',#36339,#35824,#28157,.T.);
#46200=EDGE_CURVE('',#36318,#35795,#28158,.T.);
#46201=EDGE_CURVE('',#36285,#36282,#28159,.T.);
#46202=EDGE_CURVE('',#35591,#35564,#28160,.T.);
#46203=EDGE_CURVE('',#36360,#36313,#28161,.F.);
#46204=EDGE_CURVE('',#36361,#36360,#28162,.T.);
#46205=EDGE_CURVE('',#36293,#36361,#28163,.T.);
#46206=EDGE_CURVE('',#36360,#36362,#19390,.F.);
#46207=EDGE_CURVE('',#36362,#36363,#28164,.T.);
#46208=EDGE_CURVE('',#36361,#36363,#19391,.T.);
#46209=EDGE_CURVE('',#36314,#36362,#28165,.F.);
#46210=EDGE_CURVE('',#36363,#36244,#28166,.T.);
#46211=EDGE_CURVE('',#36142,#35958,#28167,.T.);
#46212=EDGE_CURVE('',#36012,#36304,#19392,.F.);
#46213=EDGE_CURVE('',#36302,#36013,#19393,.F.);
#46214=EDGE_CURVE('',#36017,#35910,#28168,.F.);
#46215=EDGE_CURVE('',#36364,#36365,#28169,.T.);
#46216=EDGE_CURVE('',#36366,#36364,#28170,.T.);
#46217=EDGE_CURVE('',#36367,#36366,#28171,.T.);
#46218=EDGE_CURVE('',#36365,#36367,#28172,.T.);
#46219=EDGE_CURVE('',#36368,#36369,#28173,.T.);
#46220=EDGE_CURVE('',#36370,#36368,#28174,.T.);
#46221=EDGE_CURVE('',#36371,#36370,#28175,.T.);
#46222=EDGE_CURVE('',#36369,#36371,#28176,.T.);
#46223=EDGE_CURVE('',#36372,#36367,#28177,.T.);
#46224=EDGE_CURVE('',#36373,#36366,#28178,.T.);
#46225=EDGE_CURVE('',#36373,#36374,#19394,.T.);
#46226=EDGE_CURVE('',#36374,#36375,#28179,.T.);
#46227=EDGE_CURVE('',#36375,#36376,#19395,.F.);
#46228=EDGE_CURVE('',#36377,#36376,#19396,.T.);
#46229=EDGE_CURVE('',#36377,#36378,#19397,.F.);
#46230=EDGE_CURVE('',#36378,#36379,#28180,.T.);
#46231=EDGE_CURVE('',#36379,#36380,#28181,.T.);
#46232=EDGE_CURVE('',#36380,#36381,#28182,.T.);
#46233=EDGE_CURVE('',#36382,#36381,#19398,.T.);
#46234=EDGE_CURVE('',#36383,#36382,#28183,.T.);
#46235=EDGE_CURVE('',#36384,#36383,#19399,.T.);
#46236=EDGE_CURVE('',#36384,#36385,#28184,.T.);
#46237=EDGE_CURVE('',#36386,#36385,#28185,.T.);
#46238=EDGE_CURVE('',#36386,#36372,#28186,.T.);
#46239=EDGE_CURVE('',#36387,#36368,#28187,.T.);
#46240=EDGE_CURVE('',#36369,#36388,#28188,.T.);
#46241=EDGE_CURVE('',#36389,#36388,#19400,.T.);
#46242=EDGE_CURVE('',#36390,#36389,#19401,.T.);
#46243=EDGE_CURVE('',#36391,#36390,#19402,.T.);
#46244=EDGE_CURVE('',#36392,#36391,#28189,.T.);
#46245=EDGE_CURVE('',#36393,#36392,#19403,.T.);
#46246=EDGE_CURVE('',#36394,#36393,#19404,.T.);
#46247=EDGE_CURVE('',#36395,#36394,#19405,.T.);
#46248=EDGE_CURVE('',#36396,#36395,#19406,.T.);
#46249=EDGE_CURVE('',#36397,#36396,#19407,.T.);
#46250=EDGE_CURVE('',#36397,#36398,#28190,.T.);
#46251=EDGE_CURVE('',#36398,#36399,#28191,.T.);
#46252=EDGE_CURVE('',#36399,#36400,#28192,.T.);
#46253=EDGE_CURVE('',#36401,#36400,#28193,.T.);
#46254=EDGE_CURVE('',#36387,#36401,#28194,.T.);
#46255=EDGE_CURVE('',#36364,#36369,#28195,.T.);
#46256=EDGE_CURVE('',#36364,#36402,#28196,.T.);
#46257=EDGE_CURVE('',#36402,#36388,#28197,.T.);
#46258=EDGE_CURVE('',#36365,#36403,#28198,.T.);
#46259=EDGE_CURVE('',#36404,#36403,#28199,.T.);
#46260=EDGE_CURVE('',#36405,#36404,#28200,.T.);
#46261=EDGE_CURVE('',#36405,#36406,#28201,.T.);
#46262=EDGE_CURVE('',#36407,#36406,#28202,.F.);
#46263=EDGE_CURVE('',#36407,#36408,#28203,.T.);
#46264=EDGE_CURVE('',#36409,#36408,#19408,.T.);
#46265=EDGE_CURVE('',#36410,#36409,#19409,.T.);
#46266=EDGE_CURVE('',#36411,#36410,#19410,.T.);
#46267=EDGE_CURVE('',#36412,#36411,#19411,.T.);
#46268=EDGE_CURVE('',#36413,#36412,#19412,.T.);
#46269=EDGE_CURVE('',#36414,#36413,#28204,.T.);
#46270=EDGE_CURVE('',#36415,#36414,#19413,.T.);
#46271=EDGE_CURVE('',#36416,#36415,#19414,.T.);
#46272=EDGE_CURVE('',#36402,#36416,#19415,.T.);
#46273=EDGE_CURVE('',#36406,#36399,#28205,.T.);
#46274=EDGE_CURVE('',#36398,#36407,#28206,.T.);
#46275=EDGE_CURVE('',#36417,#36397,#28207,.T.);
#46276=EDGE_CURVE('',#36418,#36417,#28208,.F.);
#46277=EDGE_CURVE('',#36418,#36419,#28209,.T.);
#46278=EDGE_CURVE('',#36419,#36420,#19416,.T.);
#46279=EDGE_CURVE('',#36420,#36421,#28210,.T.);
#46280=EDGE_CURVE('',#36421,#36422,#19417,.T.);
#46281=EDGE_CURVE('',#36422,#36423,#28211,.T.);
#46282=EDGE_CURVE('',#36423,#36424,#19418,.T.);
#46283=EDGE_CURVE('',#36424,#36379,#28212,.T.);
#46284=EDGE_CURVE('',#36408,#36378,#28213,.T.);
#46285=EDGE_CURVE('',#36400,#36405,#28214,.T.);
#46286=EDGE_CURVE('',#36404,#36386,#28215,.T.);
#46287=EDGE_CURVE('',#36385,#36425,#28216,.F.);
#46288=EDGE_CURVE('',#36426,#36425,#28217,.F.);
#46289=EDGE_CURVE('',#36426,#36401,#28218,.T.);
#46290=EDGE_CURVE('',#36427,#36428,#19419,.T.);
#46291=EDGE_CURVE('',#36429,#36427,#28219,.T.);
#46292=EDGE_CURVE('',#36430,#36429,#19420,.T.);
#46293=EDGE_CURVE('',#36428,#36430,#28220,.T.);
#46294=EDGE_CURVE('',#36403,#36372,#28221,.T.);
#46295=EDGE_CURVE('',#36377,#36431,#23745,.T.);
#46296=EDGE_CURVE('',#36409,#36431,#28222,.T.);
#46297=EDGE_CURVE('',#36389,#36416,#28223,.T.);
#46298=EDGE_CURVE('',#36375,#36413,#28224,.T.);
#46299=EDGE_CURVE('',#36374,#36414,#28225,.T.);
#46300=EDGE_CURVE('',#36415,#36390,#28226,.T.);
#46301=EDGE_CURVE('',#36432,#36426,#28227,.T.);
#46302=EDGE_CURVE('',#36432,#36387,#28228,.T.);
#46303=EDGE_CURVE('',#36370,#36432,#28229,.T.);
#46304=EDGE_CURVE('',#36433,#36371,#28230,.F.);
#46305=EDGE_CURVE('',#36434,#36433,#28231,.F.);
#46306=EDGE_CURVE('',#36435,#36434,#28232,.F.);
#46307=EDGE_CURVE('',#36436,#36435,#28233,.T.);
#46308=EDGE_CURVE('',#36436,#36437,#28234,.T.);
#46309=EDGE_CURVE('',#36437,#36373,#19421,.T.);
#46310=EDGE_CURVE('',#36438,#36439,#19422,.T.);
#46311=EDGE_CURVE('',#36439,#36382,#28235,.T.);
#46312=EDGE_CURVE('',#36381,#36438,#28236,.T.);
#46313=EDGE_CURVE('',#36439,#36440,#28237,.T.);
#46314=EDGE_CURVE('',#36383,#36440,#28238,.T.);
#46315=EDGE_CURVE('',#36425,#36441,#28239,.T.);
#46316=EDGE_CURVE('',#36440,#36441,#19423,.T.);
#46317=EDGE_CURVE('',#36438,#36442,#28240,.T.);
#46318=EDGE_CURVE('',#36442,#36418,#28241,.T.);
#46319=EDGE_CURVE('',#36443,#36417,#19424,.T.);
#46320=EDGE_CURVE('',#36444,#36443,#19425,.T.);
#46321=EDGE_CURVE('',#36445,#36444,#19426,.T.);
#46322=EDGE_CURVE('',#36445,#36446,#28242,.F.);
#46323=EDGE_CURVE('',#36446,#36433,#19427,.T.);
#46324=EDGE_CURVE('',#36441,#36384,#28243,.T.);
#46325=EDGE_CURVE('',#36442,#36380,#28244,.T.);
#46326=EDGE_CURVE('',#36419,#36424,#185,.T.);
#46327=EDGE_CURVE('',#36447,#36423,#28245,.T.);
#46328=EDGE_CURVE('',#36447,#36448,#19428,.T.);
#46329=EDGE_CURVE('',#36448,#36420,#28246,.T.);
#46330=EDGE_CURVE('',#36449,#36427,#28247,.T.);
#46331=EDGE_CURVE('',#36428,#36450,#28248,.T.);
#46332=EDGE_CURVE('',#36450,#36449,#19429,.T.);
#46333=EDGE_CURVE('',#36451,#36429,#28249,.T.);
#46334=EDGE_CURVE('',#36449,#36451,#28250,.T.);
#46335=EDGE_CURVE('',#36452,#36430,#28251,.T.);
#46336=EDGE_CURVE('',#36451,#36452,#19430,.T.);
#46337=EDGE_CURVE('',#36452,#36450,#28252,.T.);
#46338=EDGE_CURVE('',#36449,#36453,#28253,.T.);
#46339=EDGE_CURVE('',#36453,#36454,#28254,.T.);
#46340=EDGE_CURVE('',#36451,#36454,#28255,.T.);
#46341=EDGE_CURVE('',#36450,#36455,#28256,.T.);
#46342=EDGE_CURVE('',#36455,#36453,#19431,.T.);
#46343=EDGE_CURVE('',#36452,#36456,#28257,.T.);
#46344=EDGE_CURVE('',#36456,#36455,#28258,.T.);
#46345=EDGE_CURVE('',#36454,#36456,#19432,.T.);
#46346=EDGE_CURVE('',#36457,#36447,#28259,.T.);
#46347=EDGE_CURVE('',#36458,#36457,#19433,.T.);
#46348=EDGE_CURVE('',#36448,#36458,#28260,.T.);
#46349=EDGE_CURVE('',#36457,#36422,#28261,.T.);
#46350=EDGE_CURVE('',#36458,#36421,#28262,.T.);
#46351=EDGE_CURVE('',#36376,#36459,#23746,.F.);
#46352=EDGE_CURVE('',#36460,#36459,#23747,.F.);
#46353=EDGE_CURVE('',#36461,#36460,#19434,.T.);
#46354=EDGE_CURVE('',#36431,#36461,#23748,.F.);
#46355=EDGE_CURVE('',#36444,#36462,#23749,.T.);
#46356=EDGE_CURVE('',#36443,#36463,#23750,.F.);
#46357=EDGE_CURVE('',#36464,#36463,#23751,.F.);
#46358=EDGE_CURVE('',#36465,#36464,#19435,.T.);
#46359=EDGE_CURVE('',#36462,#36465,#23752,.F.);
#46360=EDGE_CURVE('',#36466,#36467,#28263,.T.);
#46361=EDGE_CURVE('',#36467,#36461,#19436,.T.);
#46362=EDGE_CURVE('',#36460,#36466,#19437,.T.);
#46363=EDGE_CURVE('',#36468,#36468,#19438,.T.);
#46364=EDGE_CURVE('',#36464,#36469,#19439,.T.);
#46365=EDGE_CURVE('',#36469,#36470,#28264,.T.);
#46366=EDGE_CURVE('',#36470,#36465,#19440,.T.);
#46367=EDGE_CURVE('',#36471,#36471,#19441,.T.);
#46368=EDGE_CURVE('',#36394,#36472,#23753,.T.);
#46369=EDGE_CURVE('',#36473,#36472,#19442,.T.);
#46370=EDGE_CURVE('',#36473,#36395,#23754,.T.);
#46371=EDGE_CURVE('',#36410,#36474,#23755,.T.);
#46372=EDGE_CURVE('',#36475,#36474,#19443,.T.);
#46373=EDGE_CURVE('',#36475,#36411,#23756,.T.);
#46374=EDGE_CURVE('',#36476,#36477,#28265,.T.);
#46375=EDGE_CURVE('',#36477,#36475,#19444,.T.);
#46376=EDGE_CURVE('',#36474,#36476,#19445,.T.);
#46377=EDGE_CURVE('',#36478,#36478,#19446,.T.);
#46378=EDGE_CURVE('',#36479,#36473,#19447,.T.);
#46379=EDGE_CURVE('',#36472,#36480,#19448,.T.);
#46380=EDGE_CURVE('',#36480,#36479,#28266,.T.);
#46381=EDGE_CURVE('',#36481,#36481,#19449,.T.);
#46382=EDGE_CURVE('',#36463,#36396,#28267,.F.);
#46383=EDGE_CURVE('',#36477,#36466,#28268,.T.);
#46384=EDGE_CURVE('',#36459,#36412,#28269,.T.);
#46385=EDGE_CURVE('',#36467,#36476,#28270,.T.);
#46386=EDGE_CURVE('',#36482,#36482,#19450,.T.);
#46387=EDGE_CURVE('',#36483,#36483,#19451,.T.);
#46388=EDGE_CURVE('',#36434,#36484,#19452,.T.);
#46389=EDGE_CURVE('',#36484,#36435,#28271,.F.);
#46390=EDGE_CURVE('',#36485,#36485,#19453,.T.);
#46391=EDGE_CURVE('',#36486,#36486,#19454,.T.);
#46392=EDGE_CURVE('',#36487,#36437,#19455,.T.);
#46393=EDGE_CURVE('',#36436,#36487,#28272,.T.);
#46394=EDGE_CURVE('',#36391,#36446,#28273,.T.);
#46395=EDGE_CURVE('',#36392,#36445,#28274,.T.);
#46396=EDGE_CURVE('',#36470,#36480,#28275,.T.);
#46397=EDGE_CURVE('',#36479,#36469,#28276,.T.);
#46398=EDGE_CURVE('',#36462,#36393,#28277,.F.);
#46399=EDGE_CURVE('',#36478,#36468,#28278,.T.);
#46400=EDGE_CURVE('',#36487,#36484,#28279,.T.);
#46401=EDGE_CURVE('',#36483,#36486,#28280,.T.);
#46402=EDGE_CURVE('',#36471,#36481,#28281,.T.);
#46403=EDGE_CURVE('',#36482,#36434,#28282,.T.);
#46404=EDGE_CURVE('',#36437,#36485,#28283,.T.);
#46405=EDGE_CURVE('',#36488,#36488,#19456,.T.);
#46406=EDGE_CURVE('',#36488,#36489,#28284,.T.);
#46407=EDGE_CURVE('',#36489,#36489,#19457,.T.);
#46408=EDGE_CURVE('',#36489,#36490,#28285,.T.);
#46409=EDGE_CURVE('',#36490,#36490,#19458,.T.);
#46410=EDGE_CURVE('',#36491,#36491,#19459,.T.);
#46411=EDGE_CURVE('',#36491,#36490,#28286,.T.);
#46412=EDGE_CURVE('',#36492,#36492,#19460,.T.);
#46413=EDGE_CURVE('',#36492,#36493,#28287,.T.);
#46414=EDGE_CURVE('',#36493,#36493,#19461,.T.);
#46415=EDGE_CURVE('',#36494,#36494,#19462,.T.);
#46416=EDGE_CURVE('',#36494,#36493,#28288,.T.);
#46417=EDGE_CURVE('',#36495,#36495,#19463,.T.);
#46418=EDGE_CURVE('',#36495,#36494,#28289,.T.);
#46419=EDGE_CURVE('',#36496,#36497,#23757,.T.);
#46420=EDGE_CURVE('',#36496,#36498,#19464,.T.);
#46421=EDGE_CURVE('',#36499,#36498,#23758,.T.);
#46422=EDGE_CURVE('',#36497,#36499,#19465,.T.);
#46423=EDGE_CURVE('',#36500,#36501,#23759,.T.);
#46424=EDGE_CURVE('',#36500,#36502,#19466,.T.);
#46425=EDGE_CURVE('',#36503,#36502,#23760,.T.);
#46426=EDGE_CURVE('',#36501,#36503,#19467,.T.);
#46427=EDGE_CURVE('',#36504,#36505,#23761,.T.);
#46428=EDGE_CURVE('',#36504,#36506,#19468,.T.);
#46429=EDGE_CURVE('',#36507,#36506,#23762,.T.);
#46430=EDGE_CURVE('',#36505,#36507,#19469,.T.);
#46431=EDGE_CURVE('',#36508,#36509,#23763,.T.);
#46432=EDGE_CURVE('',#36508,#36510,#19470,.T.);
#46433=EDGE_CURVE('',#36511,#36510,#23764,.T.);
#46434=EDGE_CURVE('',#36509,#36511,#19471,.T.);
#46435=EDGE_CURVE('',#36512,#36513,#23765,.T.);
#46436=EDGE_CURVE('',#36512,#36514,#19472,.T.);
#46437=EDGE_CURVE('',#36515,#36514,#23766,.T.);
#46438=EDGE_CURVE('',#36513,#36515,#19473,.T.);
#46439=EDGE_CURVE('',#36516,#36517,#23767,.T.);
#46440=EDGE_CURVE('',#36516,#36518,#19474,.T.);
#46441=EDGE_CURVE('',#36519,#36518,#23768,.T.);
#46442=EDGE_CURVE('',#36517,#36519,#19475,.T.);
#46443=EDGE_CURVE('',#36520,#36521,#23769,.T.);
#46444=EDGE_CURVE('',#36520,#36522,#19476,.T.);
#46445=EDGE_CURVE('',#36523,#36522,#23770,.T.);
#46446=EDGE_CURVE('',#36521,#36523,#19477,.T.);
#46447=EDGE_CURVE('',#36524,#36525,#23771,.T.);
#46448=EDGE_CURVE('',#36524,#36526,#19478,.T.);
#46449=EDGE_CURVE('',#36527,#36526,#23772,.T.);
#46450=EDGE_CURVE('',#36525,#36527,#19479,.T.);
#46451=EDGE_CURVE('',#36528,#36529,#23773,.T.);
#46452=EDGE_CURVE('',#36528,#36530,#19480,.T.);
#46453=EDGE_CURVE('',#36531,#36530,#23774,.T.);
#46454=EDGE_CURVE('',#36529,#36531,#19481,.T.);
#46455=EDGE_CURVE('',#36532,#36533,#23775,.T.);
#46456=EDGE_CURVE('',#36532,#36534,#19482,.T.);
#46457=EDGE_CURVE('',#36535,#36534,#23776,.T.);
#46458=EDGE_CURVE('',#36533,#36535,#19483,.T.);
#46459=EDGE_CURVE('',#36536,#36537,#23777,.T.);
#46460=EDGE_CURVE('',#36536,#36538,#19484,.T.);
#46461=EDGE_CURVE('',#36539,#36538,#23778,.T.);
#46462=EDGE_CURVE('',#36537,#36539,#19485,.T.);
#46463=EDGE_CURVE('',#36540,#36541,#23779,.T.);
#46464=EDGE_CURVE('',#36540,#36542,#19486,.T.);
#46465=EDGE_CURVE('',#36543,#36542,#23780,.T.);
#46466=EDGE_CURVE('',#36541,#36543,#19487,.T.);
#46467=EDGE_CURVE('',#36544,#36545,#23781,.T.);
#46468=EDGE_CURVE('',#36544,#36546,#19488,.T.);
#46469=EDGE_CURVE('',#36547,#36546,#23782,.T.);
#46470=EDGE_CURVE('',#36545,#36547,#19489,.T.);
#46471=EDGE_CURVE('',#36548,#36549,#23783,.T.);
#46472=EDGE_CURVE('',#36548,#36550,#19490,.T.);
#46473=EDGE_CURVE('',#36551,#36550,#23784,.T.);
#46474=EDGE_CURVE('',#36549,#36551,#19491,.T.);
#46475=EDGE_CURVE('',#36552,#36553,#23785,.T.);
#46476=EDGE_CURVE('',#36552,#36554,#19492,.T.);
#46477=EDGE_CURVE('',#36555,#36554,#23786,.T.);
#46478=EDGE_CURVE('',#36553,#36555,#19493,.T.);
#46479=EDGE_CURVE('',#36556,#36557,#23787,.T.);
#46480=EDGE_CURVE('',#36556,#36558,#19494,.T.);
#46481=EDGE_CURVE('',#36559,#36558,#23788,.T.);
#46482=EDGE_CURVE('',#36557,#36559,#19495,.T.);
#46483=EDGE_CURVE('',#36560,#36561,#23789,.T.);
#46484=EDGE_CURVE('',#36560,#36562,#19496,.T.);
#46485=EDGE_CURVE('',#36563,#36562,#23790,.T.);
#46486=EDGE_CURVE('',#36561,#36563,#19497,.T.);
#46487=EDGE_CURVE('',#36564,#36565,#23791,.T.);
#46488=EDGE_CURVE('',#36564,#36566,#19498,.T.);
#46489=EDGE_CURVE('',#36567,#36566,#23792,.T.);
#46490=EDGE_CURVE('',#36565,#36567,#19499,.T.);
#46491=EDGE_CURVE('',#36568,#36569,#23793,.T.);
#46492=EDGE_CURVE('',#36568,#36570,#19500,.T.);
#46493=EDGE_CURVE('',#36571,#36570,#23794,.T.);
#46494=EDGE_CURVE('',#36569,#36571,#19501,.T.);
#46495=EDGE_CURVE('',#36572,#36573,#23795,.T.);
#46496=EDGE_CURVE('',#36572,#36574,#19502,.T.);
#46497=EDGE_CURVE('',#36575,#36574,#23796,.T.);
#46498=EDGE_CURVE('',#36573,#36575,#19503,.T.);
#46499=EDGE_CURVE('',#36576,#36577,#23797,.T.);
#46500=EDGE_CURVE('',#36576,#36578,#19504,.T.);
#46501=EDGE_CURVE('',#36579,#36578,#23798,.T.);
#46502=EDGE_CURVE('',#36577,#36579,#19505,.T.);
#46503=EDGE_CURVE('',#36580,#36581,#23799,.T.);
#46504=EDGE_CURVE('',#36580,#36582,#19506,.T.);
#46505=EDGE_CURVE('',#36583,#36582,#23800,.T.);
#46506=EDGE_CURVE('',#36581,#36583,#19507,.T.);
#46507=EDGE_CURVE('',#36584,#36585,#23801,.T.);
#46508=EDGE_CURVE('',#36584,#36586,#19508,.T.);
#46509=EDGE_CURVE('',#36587,#36586,#23802,.T.);
#46510=EDGE_CURVE('',#36585,#36587,#19509,.T.);
#46511=EDGE_CURVE('',#36588,#36589,#23803,.T.);
#46512=EDGE_CURVE('',#36588,#36590,#19510,.T.);
#46513=EDGE_CURVE('',#36591,#36590,#23804,.T.);
#46514=EDGE_CURVE('',#36589,#36591,#19511,.T.);
#46515=EDGE_CURVE('',#36592,#36593,#23805,.T.);
#46516=EDGE_CURVE('',#36592,#36594,#19512,.T.);
#46517=EDGE_CURVE('',#36595,#36594,#23806,.T.);
#46518=EDGE_CURVE('',#36593,#36595,#19513,.T.);
#46519=EDGE_CURVE('',#36596,#36597,#23807,.T.);
#46520=EDGE_CURVE('',#36596,#36598,#19514,.T.);
#46521=EDGE_CURVE('',#36599,#36598,#23808,.T.);
#46522=EDGE_CURVE('',#36597,#36599,#19515,.T.);
#46523=EDGE_CURVE('',#36600,#36601,#23809,.T.);
#46524=EDGE_CURVE('',#36600,#36602,#19516,.T.);
#46525=EDGE_CURVE('',#36603,#36602,#23810,.T.);
#46526=EDGE_CURVE('',#36601,#36603,#19517,.T.);
#46527=EDGE_CURVE('',#36604,#36605,#23811,.T.);
#46528=EDGE_CURVE('',#36604,#36606,#19518,.T.);
#46529=EDGE_CURVE('',#36607,#36606,#23812,.T.);
#46530=EDGE_CURVE('',#36605,#36607,#19519,.T.);
#46531=EDGE_CURVE('',#36608,#36609,#23813,.T.);
#46532=EDGE_CURVE('',#36608,#36610,#19520,.T.);
#46533=EDGE_CURVE('',#36611,#36610,#23814,.T.);
#46534=EDGE_CURVE('',#36609,#36611,#19521,.T.);
#46535=EDGE_CURVE('',#36612,#36613,#23815,.T.);
#46536=EDGE_CURVE('',#36612,#36614,#19522,.T.);
#46537=EDGE_CURVE('',#36615,#36614,#23816,.T.);
#46538=EDGE_CURVE('',#36613,#36615,#19523,.T.);
#46539=EDGE_CURVE('',#36616,#36617,#23817,.T.);
#46540=EDGE_CURVE('',#36616,#36618,#19524,.T.);
#46541=EDGE_CURVE('',#36619,#36618,#23818,.T.);
#46542=EDGE_CURVE('',#36617,#36619,#19525,.T.);
#46543=EDGE_CURVE('',#36620,#36621,#23819,.T.);
#46544=EDGE_CURVE('',#36620,#36622,#19526,.T.);
#46545=EDGE_CURVE('',#36623,#36622,#23820,.T.);
#46546=EDGE_CURVE('',#36621,#36623,#19527,.T.);
#46547=EDGE_CURVE('',#36624,#36625,#23821,.T.);
#46548=EDGE_CURVE('',#36624,#36626,#19528,.T.);
#46549=EDGE_CURVE('',#36627,#36626,#23822,.T.);
#46550=EDGE_CURVE('',#36625,#36627,#19529,.T.);
#46551=EDGE_CURVE('',#36628,#36629,#23823,.T.);
#46552=EDGE_CURVE('',#36628,#36630,#19530,.T.);
#46553=EDGE_CURVE('',#36631,#36630,#23824,.T.);
#46554=EDGE_CURVE('',#36629,#36631,#19531,.T.);
#46555=EDGE_CURVE('',#36632,#36633,#23825,.T.);
#46556=EDGE_CURVE('',#36632,#36634,#19532,.T.);
#46557=EDGE_CURVE('',#36635,#36634,#23826,.T.);
#46558=EDGE_CURVE('',#36633,#36635,#19533,.T.);
#46559=EDGE_CURVE('',#36636,#36637,#23827,.T.);
#46560=EDGE_CURVE('',#36636,#36638,#19534,.T.);
#46561=EDGE_CURVE('',#36639,#36638,#23828,.T.);
#46562=EDGE_CURVE('',#36637,#36639,#19535,.T.);
#46563=EDGE_CURVE('',#36640,#36641,#23829,.T.);
#46564=EDGE_CURVE('',#36640,#36642,#19536,.T.);
#46565=EDGE_CURVE('',#36643,#36642,#23830,.T.);
#46566=EDGE_CURVE('',#36641,#36643,#19537,.T.);
#46567=EDGE_CURVE('',#36644,#36645,#23831,.T.);
#46568=EDGE_CURVE('',#36644,#36646,#19538,.T.);
#46569=EDGE_CURVE('',#36647,#36646,#23832,.T.);
#46570=EDGE_CURVE('',#36645,#36647,#19539,.T.);
#46571=EDGE_CURVE('',#36648,#36649,#23833,.T.);
#46572=EDGE_CURVE('',#36648,#36650,#19540,.T.);
#46573=EDGE_CURVE('',#36651,#36650,#23834,.T.);
#46574=EDGE_CURVE('',#36649,#36651,#19541,.T.);
#46575=EDGE_CURVE('',#36652,#36653,#23835,.T.);
#46576=EDGE_CURVE('',#36652,#36654,#19542,.T.);
#46577=EDGE_CURVE('',#36655,#36654,#23836,.T.);
#46578=EDGE_CURVE('',#36653,#36655,#19543,.T.);
#46579=EDGE_CURVE('',#36656,#36657,#23837,.T.);
#46580=EDGE_CURVE('',#36656,#36658,#19544,.T.);
#46581=EDGE_CURVE('',#36659,#36658,#23838,.T.);
#46582=EDGE_CURVE('',#36657,#36659,#19545,.T.);
#46583=EDGE_CURVE('',#36660,#36661,#23839,.T.);
#46584=EDGE_CURVE('',#36660,#36662,#19546,.T.);
#46585=EDGE_CURVE('',#36663,#36662,#23840,.T.);
#46586=EDGE_CURVE('',#36661,#36663,#19547,.T.);
#46587=EDGE_CURVE('',#36664,#36665,#23841,.T.);
#46588=EDGE_CURVE('',#36664,#36666,#19548,.T.);
#46589=EDGE_CURVE('',#36667,#36666,#23842,.T.);
#46590=EDGE_CURVE('',#36665,#36667,#19549,.T.);
#46591=EDGE_CURVE('',#36668,#36669,#23843,.T.);
#46592=EDGE_CURVE('',#36668,#36670,#19550,.T.);
#46593=EDGE_CURVE('',#36671,#36670,#23844,.T.);
#46594=EDGE_CURVE('',#36669,#36671,#19551,.T.);
#46595=EDGE_CURVE('',#36672,#36673,#23845,.T.);
#46596=EDGE_CURVE('',#36672,#36674,#19552,.T.);
#46597=EDGE_CURVE('',#36675,#36674,#23846,.T.);
#46598=EDGE_CURVE('',#36673,#36675,#19553,.T.);
#46599=EDGE_CURVE('',#36676,#36677,#23847,.T.);
#46600=EDGE_CURVE('',#36676,#36678,#19554,.T.);
#46601=EDGE_CURVE('',#36679,#36678,#23848,.T.);
#46602=EDGE_CURVE('',#36677,#36679,#19555,.T.);
#46603=EDGE_CURVE('',#36680,#36681,#23849,.T.);
#46604=EDGE_CURVE('',#36680,#36682,#19556,.T.);
#46605=EDGE_CURVE('',#36683,#36682,#23850,.T.);
#46606=EDGE_CURVE('',#36681,#36683,#19557,.T.);
#46607=EDGE_CURVE('',#36684,#36685,#23851,.T.);
#46608=EDGE_CURVE('',#36684,#36686,#19558,.T.);
#46609=EDGE_CURVE('',#36687,#36686,#23852,.T.);
#46610=EDGE_CURVE('',#36685,#36687,#19559,.T.);
#46611=EDGE_CURVE('',#36688,#36689,#23853,.T.);
#46612=EDGE_CURVE('',#36688,#36690,#19560,.T.);
#46613=EDGE_CURVE('',#36691,#36690,#23854,.T.);
#46614=EDGE_CURVE('',#36689,#36691,#19561,.T.);
#46615=EDGE_CURVE('',#36692,#36693,#23855,.T.);
#46616=EDGE_CURVE('',#36692,#36694,#19562,.T.);
#46617=EDGE_CURVE('',#36695,#36694,#23856,.T.);
#46618=EDGE_CURVE('',#36693,#36695,#19563,.T.);
#46619=EDGE_CURVE('',#36696,#36697,#23857,.T.);
#46620=EDGE_CURVE('',#36696,#36698,#19564,.T.);
#46621=EDGE_CURVE('',#36699,#36698,#23858,.T.);
#46622=EDGE_CURVE('',#36697,#36699,#19565,.T.);
#46623=EDGE_CURVE('',#36700,#36701,#23859,.T.);
#46624=EDGE_CURVE('',#36700,#36702,#19566,.T.);
#46625=EDGE_CURVE('',#36703,#36702,#23860,.T.);
#46626=EDGE_CURVE('',#36701,#36703,#19567,.T.);
#46627=EDGE_CURVE('',#36704,#36705,#23861,.T.);
#46628=EDGE_CURVE('',#36704,#36706,#19568,.T.);
#46629=EDGE_CURVE('',#36707,#36706,#23862,.T.);
#46630=EDGE_CURVE('',#36705,#36707,#19569,.T.);
#46631=EDGE_CURVE('',#36708,#36709,#23863,.T.);
#46632=EDGE_CURVE('',#36708,#36710,#19570,.T.);
#46633=EDGE_CURVE('',#36711,#36710,#23864,.T.);
#46634=EDGE_CURVE('',#36709,#36711,#19571,.T.);
#46635=EDGE_CURVE('',#36712,#36713,#23865,.T.);
#46636=EDGE_CURVE('',#36712,#36714,#19572,.T.);
#46637=EDGE_CURVE('',#36715,#36714,#23866,.T.);
#46638=EDGE_CURVE('',#36713,#36715,#19573,.T.);
#46639=EDGE_CURVE('',#36716,#36717,#23867,.T.);
#46640=EDGE_CURVE('',#36716,#36718,#19574,.T.);
#46641=EDGE_CURVE('',#36719,#36718,#23868,.T.);
#46642=EDGE_CURVE('',#36717,#36719,#19575,.T.);
#46643=EDGE_CURVE('',#36720,#36721,#23869,.T.);
#46644=EDGE_CURVE('',#36720,#36722,#19576,.T.);
#46645=EDGE_CURVE('',#36723,#36722,#23870,.T.);
#46646=EDGE_CURVE('',#36721,#36723,#19577,.T.);
#46647=EDGE_CURVE('',#36724,#36725,#23871,.T.);
#46648=EDGE_CURVE('',#36724,#36726,#19578,.T.);
#46649=EDGE_CURVE('',#36727,#36726,#23872,.T.);
#46650=EDGE_CURVE('',#36725,#36727,#19579,.T.);
#46651=EDGE_CURVE('',#36728,#36729,#23873,.T.);
#46652=EDGE_CURVE('',#36728,#36730,#19580,.T.);
#46653=EDGE_CURVE('',#36731,#36730,#23874,.T.);
#46654=EDGE_CURVE('',#36729,#36731,#19581,.T.);
#46655=EDGE_CURVE('',#36732,#36733,#23875,.T.);
#46656=EDGE_CURVE('',#36732,#36734,#19582,.T.);
#46657=EDGE_CURVE('',#36735,#36734,#23876,.T.);
#46658=EDGE_CURVE('',#36733,#36735,#19583,.T.);
#46659=EDGE_CURVE('',#36736,#36737,#23877,.T.);
#46660=EDGE_CURVE('',#36736,#36738,#19584,.T.);
#46661=EDGE_CURVE('',#36739,#36738,#23878,.T.);
#46662=EDGE_CURVE('',#36737,#36739,#19585,.T.);
#46663=EDGE_CURVE('',#36740,#36741,#23879,.T.);
#46664=EDGE_CURVE('',#36740,#36742,#19586,.T.);
#46665=EDGE_CURVE('',#36743,#36742,#23880,.T.);
#46666=EDGE_CURVE('',#36741,#36743,#19587,.T.);
#46667=EDGE_CURVE('',#36744,#36745,#23881,.T.);
#46668=EDGE_CURVE('',#36744,#36746,#19588,.T.);
#46669=EDGE_CURVE('',#36747,#36746,#23882,.T.);
#46670=EDGE_CURVE('',#36745,#36747,#19589,.T.);
#46671=EDGE_CURVE('',#36748,#36749,#23883,.T.);
#46672=EDGE_CURVE('',#36748,#36750,#19590,.T.);
#46673=EDGE_CURVE('',#36751,#36750,#23884,.T.);
#46674=EDGE_CURVE('',#36749,#36751,#19591,.T.);
#46675=EDGE_CURVE('',#36752,#36753,#23885,.T.);
#46676=EDGE_CURVE('',#36752,#36754,#19592,.T.);
#46677=EDGE_CURVE('',#36755,#36754,#23886,.T.);
#46678=EDGE_CURVE('',#36753,#36755,#19593,.T.);
#46679=EDGE_CURVE('',#36756,#36757,#23887,.T.);
#46680=EDGE_CURVE('',#36756,#36758,#19594,.T.);
#46681=EDGE_CURVE('',#36759,#36758,#23888,.T.);
#46682=EDGE_CURVE('',#36757,#36759,#19595,.T.);
#46683=EDGE_CURVE('',#36760,#36761,#23889,.T.);
#46684=EDGE_CURVE('',#36760,#36762,#19596,.T.);
#46685=EDGE_CURVE('',#36763,#36762,#23890,.T.);
#46686=EDGE_CURVE('',#36761,#36763,#19597,.T.);
#46687=EDGE_CURVE('',#36764,#36765,#23891,.T.);
#46688=EDGE_CURVE('',#36764,#36766,#19598,.T.);
#46689=EDGE_CURVE('',#36767,#36766,#23892,.T.);
#46690=EDGE_CURVE('',#36765,#36767,#19599,.T.);
#46691=EDGE_CURVE('',#36768,#36769,#23893,.T.);
#46692=EDGE_CURVE('',#36768,#36770,#19600,.T.);
#46693=EDGE_CURVE('',#36771,#36770,#23894,.T.);
#46694=EDGE_CURVE('',#36769,#36771,#19601,.T.);
#46695=EDGE_CURVE('',#36772,#36773,#23895,.T.);
#46696=EDGE_CURVE('',#36772,#36774,#19602,.T.);
#46697=EDGE_CURVE('',#36775,#36774,#23896,.T.);
#46698=EDGE_CURVE('',#36773,#36775,#19603,.T.);
#46699=EDGE_CURVE('',#36776,#36777,#19604,.T.);
#46700=EDGE_CURVE('',#36776,#36778,#28290,.T.);
#46701=EDGE_CURVE('',#36778,#36778,#19605,.T.);
#46702=EDGE_CURVE('',#36777,#36776,#19606,.T.);
#46703=EDGE_CURVE('',#36779,#36780,#19607,.T.);
#46704=EDGE_CURVE('',#36779,#36781,#28291,.T.);
#46705=EDGE_CURVE('',#36781,#36781,#19608,.T.);
#46706=EDGE_CURVE('',#36780,#36779,#19609,.T.);
#46707=EDGE_CURVE('',#36782,#36783,#19610,.T.);
#46708=EDGE_CURVE('',#36782,#36784,#28292,.T.);
#46709=EDGE_CURVE('',#36784,#36784,#19611,.T.);
#46710=EDGE_CURVE('',#36783,#36782,#19612,.T.);
#46711=EDGE_CURVE('',#36785,#36786,#19613,.T.);
#46712=EDGE_CURVE('',#36785,#36787,#28293,.T.);
#46713=EDGE_CURVE('',#36787,#36787,#19614,.T.);
#46714=EDGE_CURVE('',#36786,#36785,#19615,.T.);
#46715=EDGE_CURVE('',#36788,#36788,#19616,.T.);
#46716=EDGE_CURVE('',#36788,#36789,#28294,.T.);
#46717=EDGE_CURVE('',#36789,#36789,#19617,.T.);
#46718=EDGE_CURVE('',#36790,#36790,#19618,.T.);
#46719=EDGE_CURVE('',#36790,#36791,#28295,.T.);
#46720=EDGE_CURVE('',#36791,#36791,#19619,.T.);
#46721=EDGE_CURVE('',#36792,#36793,#19620,.T.);
#46722=EDGE_CURVE('',#36792,#36794,#28296,.T.);
#46723=EDGE_CURVE('',#36794,#36794,#19621,.T.);
#46724=EDGE_CURVE('',#36793,#36792,#19622,.T.);
#46725=EDGE_CURVE('',#36795,#36795,#19623,.T.);
#46726=EDGE_CURVE('',#36795,#36796,#28297,.T.);
#46727=EDGE_CURVE('',#36796,#36796,#19624,.T.);
#46728=EDGE_CURVE('',#36780,#36790,#28298,.T.);
#46729=EDGE_CURVE('',#36783,#36788,#28299,.T.);
#46730=EDGE_CURVE('',#36797,#36798,#23897,.T.);
#46731=EDGE_CURVE('',#36774,#36797,#23898,.T.);
#46732=EDGE_CURVE('',#36799,#36772,#23899,.T.);
#46733=EDGE_CURVE('',#36800,#36799,#23900,.F.);
#46734=EDGE_CURVE('',#36770,#36800,#23901,.T.);
#46735=EDGE_CURVE('',#36801,#36768,#23902,.T.);
#46736=EDGE_CURVE('',#36802,#36801,#23903,.F.);
#46737=EDGE_CURVE('',#36766,#36802,#23904,.T.);
#46738=EDGE_CURVE('',#36803,#36764,#23905,.T.);
#46739=EDGE_CURVE('',#36804,#36803,#23906,.F.);
#46740=EDGE_CURVE('',#36762,#36804,#23907,.T.);
#46741=EDGE_CURVE('',#36805,#36760,#23908,.T.);
#46742=EDGE_CURVE('',#36806,#36805,#23909,.F.);
#46743=EDGE_CURVE('',#36758,#36806,#23910,.T.);
#46744=EDGE_CURVE('',#36807,#36756,#23911,.T.);
#46745=EDGE_CURVE('',#36808,#36807,#23912,.F.);
#46746=EDGE_CURVE('',#36754,#36808,#23913,.T.);
#46747=EDGE_CURVE('',#36809,#36752,#23914,.T.);
#46748=EDGE_CURVE('',#36810,#36809,#23915,.F.);
#46749=EDGE_CURVE('',#36750,#36810,#23916,.T.);
#46750=EDGE_CURVE('',#36811,#36748,#23917,.T.);
#46751=EDGE_CURVE('',#36812,#36811,#23918,.F.);
#46752=EDGE_CURVE('',#36746,#36812,#23919,.T.);
#46753=EDGE_CURVE('',#36813,#36744,#23920,.T.);
#46754=EDGE_CURVE('',#36814,#36813,#23921,.F.);
#46755=EDGE_CURVE('',#36742,#36814,#23922,.T.);
#46756=EDGE_CURVE('',#36815,#36740,#23923,.T.);
#46757=EDGE_CURVE('',#36816,#36815,#23924,.F.);
#46758=EDGE_CURVE('',#36738,#36816,#23925,.T.);
#46759=EDGE_CURVE('',#36817,#36736,#23926,.T.);
#46760=EDGE_CURVE('',#36818,#36817,#23927,.F.);
#46761=EDGE_CURVE('',#36734,#36818,#23928,.T.);
#46762=EDGE_CURVE('',#36819,#36732,#23929,.T.);
#46763=EDGE_CURVE('',#36820,#36819,#23930,.F.);
#46764=EDGE_CURVE('',#36730,#36820,#23931,.T.);
#46765=EDGE_CURVE('',#36821,#36728,#23932,.T.);
#46766=EDGE_CURVE('',#36822,#36821,#23933,.F.);
#46767=EDGE_CURVE('',#36726,#36822,#23934,.T.);
#46768=EDGE_CURVE('',#36823,#36724,#23935,.T.);
#46769=EDGE_CURVE('',#36824,#36823,#23936,.F.);
#46770=EDGE_CURVE('',#36722,#36824,#23937,.T.);
#46771=EDGE_CURVE('',#36825,#36720,#23938,.T.);
#46772=EDGE_CURVE('',#36826,#36825,#23939,.F.);
#46773=EDGE_CURVE('',#36718,#36826,#23940,.T.);
#46774=EDGE_CURVE('',#36827,#36716,#23941,.T.);
#46775=EDGE_CURVE('',#36828,#36827,#23942,.F.);
#46776=EDGE_CURVE('',#36714,#36828,#23943,.T.);
#46777=EDGE_CURVE('',#36829,#36712,#23944,.T.);
#46778=EDGE_CURVE('',#36830,#36829,#23945,.F.);
#46779=EDGE_CURVE('',#36710,#36830,#23946,.T.);
#46780=EDGE_CURVE('',#36831,#36708,#23947,.T.);
#46781=EDGE_CURVE('',#36832,#36831,#23948,.F.);
#46782=EDGE_CURVE('',#36706,#36832,#23949,.T.);
#46783=EDGE_CURVE('',#36833,#36704,#23950,.T.);
#46784=EDGE_CURVE('',#36834,#36833,#23951,.F.);
#46785=EDGE_CURVE('',#36702,#36834,#23952,.T.);
#46786=EDGE_CURVE('',#36835,#36700,#23953,.T.);
#46787=EDGE_CURVE('',#36836,#36835,#23954,.F.);
#46788=EDGE_CURVE('',#36698,#36836,#23955,.T.);
#46789=EDGE_CURVE('',#36837,#36696,#23956,.T.);
#46790=EDGE_CURVE('',#36838,#36837,#23957,.F.);
#46791=EDGE_CURVE('',#36694,#36838,#23958,.T.);
#46792=EDGE_CURVE('',#36839,#36692,#23959,.T.);
#46793=EDGE_CURVE('',#36840,#36839,#23960,.F.);
#46794=EDGE_CURVE('',#36690,#36840,#23961,.T.);
#46795=EDGE_CURVE('',#36841,#36688,#23962,.T.);
#46796=EDGE_CURVE('',#36842,#36841,#23963,.F.);
#46797=EDGE_CURVE('',#36686,#36842,#23964,.T.);
#46798=EDGE_CURVE('',#36843,#36684,#23965,.T.);
#46799=EDGE_CURVE('',#36844,#36843,#23966,.F.);
#46800=EDGE_CURVE('',#36682,#36844,#23967,.T.);
#46801=EDGE_CURVE('',#36845,#36680,#23968,.T.);
#46802=EDGE_CURVE('',#36846,#36845,#23969,.F.);
#46803=EDGE_CURVE('',#36678,#36846,#23970,.T.);
#46804=EDGE_CURVE('',#36847,#36676,#23971,.T.);
#46805=EDGE_CURVE('',#36848,#36847,#23972,.F.);
#46806=EDGE_CURVE('',#36674,#36848,#23973,.T.);
#46807=EDGE_CURVE('',#36849,#36672,#23974,.T.);
#46808=EDGE_CURVE('',#36850,#36849,#23975,.F.);
#46809=EDGE_CURVE('',#36670,#36850,#23976,.T.);
#46810=EDGE_CURVE('',#36851,#36668,#23977,.T.);
#46811=EDGE_CURVE('',#36852,#36851,#23978,.F.);
#46812=EDGE_CURVE('',#36666,#36852,#23979,.T.);
#46813=EDGE_CURVE('',#36853,#36664,#23980,.T.);
#46814=EDGE_CURVE('',#36854,#36853,#23981,.F.);
#46815=EDGE_CURVE('',#36662,#36854,#23982,.T.);
#46816=EDGE_CURVE('',#36855,#36660,#23983,.T.);
#46817=EDGE_CURVE('',#36856,#36855,#23984,.F.);
#46818=EDGE_CURVE('',#36658,#36856,#23985,.T.);
#46819=EDGE_CURVE('',#36857,#36656,#23986,.T.);
#46820=EDGE_CURVE('',#36858,#36857,#23987,.F.);
#46821=EDGE_CURVE('',#36654,#36858,#23988,.T.);
#46822=EDGE_CURVE('',#36859,#36652,#23989,.T.);
#46823=EDGE_CURVE('',#36860,#36859,#23990,.F.);
#46824=EDGE_CURVE('',#36650,#36860,#23991,.T.);
#46825=EDGE_CURVE('',#36861,#36648,#23992,.T.);
#46826=EDGE_CURVE('',#36862,#36861,#23993,.F.);
#46827=EDGE_CURVE('',#36646,#36862,#23994,.T.);
#46828=EDGE_CURVE('',#36863,#36644,#23995,.T.);
#46829=EDGE_CURVE('',#36864,#36863,#23996,.F.);
#46830=EDGE_CURVE('',#36642,#36864,#23997,.T.);
#46831=EDGE_CURVE('',#36865,#36640,#23998,.T.);
#46832=EDGE_CURVE('',#36866,#36865,#23999,.F.);
#46833=EDGE_CURVE('',#36638,#36866,#24000,.T.);
#46834=EDGE_CURVE('',#36867,#36636,#24001,.T.);
#46835=EDGE_CURVE('',#36868,#36867,#24002,.F.);
#46836=EDGE_CURVE('',#36868,#36869,#28300,.T.);
#46837=EDGE_CURVE('',#36869,#36869,#19625,.T.);
#46838=EDGE_CURVE('',#36870,#36868,#24003,.F.);
#46839=EDGE_CURVE('',#36634,#36870,#24004,.T.);
#46840=EDGE_CURVE('',#36871,#36632,#24005,.T.);
#46841=EDGE_CURVE('',#36872,#36871,#24006,.F.);
#46842=EDGE_CURVE('',#36630,#36872,#24007,.T.);
#46843=EDGE_CURVE('',#36873,#36628,#24008,.T.);
#46844=EDGE_CURVE('',#36874,#36873,#24009,.F.);
#46845=EDGE_CURVE('',#36626,#36874,#24010,.T.);
#46846=EDGE_CURVE('',#36875,#36624,#24011,.T.);
#46847=EDGE_CURVE('',#36876,#36875,#24012,.F.);
#46848=EDGE_CURVE('',#36622,#36876,#24013,.T.);
#46849=EDGE_CURVE('',#36877,#36620,#24014,.T.);
#46850=EDGE_CURVE('',#36878,#36877,#24015,.F.);
#46851=EDGE_CURVE('',#36618,#36878,#24016,.T.);
#46852=EDGE_CURVE('',#36879,#36616,#24017,.T.);
#46853=EDGE_CURVE('',#36880,#36879,#24018,.F.);
#46854=EDGE_CURVE('',#36614,#36880,#24019,.T.);
#46855=EDGE_CURVE('',#36881,#36612,#24020,.T.);
#46856=EDGE_CURVE('',#36882,#36881,#24021,.F.);
#46857=EDGE_CURVE('',#36610,#36882,#24022,.T.);
#46858=EDGE_CURVE('',#36883,#36608,#24023,.T.);
#46859=EDGE_CURVE('',#36884,#36883,#24024,.F.);
#46860=EDGE_CURVE('',#36606,#36884,#24025,.T.);
#46861=EDGE_CURVE('',#36885,#36604,#24026,.T.);
#46862=EDGE_CURVE('',#36886,#36885,#24027,.F.);
#46863=EDGE_CURVE('',#36602,#36886,#24028,.T.);
#46864=EDGE_CURVE('',#36887,#36600,#24029,.T.);
#46865=EDGE_CURVE('',#36888,#36887,#24030,.F.);
#46866=EDGE_CURVE('',#36598,#36888,#24031,.T.);
#46867=EDGE_CURVE('',#36889,#36596,#24032,.T.);
#46868=EDGE_CURVE('',#36890,#36889,#24033,.F.);
#46869=EDGE_CURVE('',#36594,#36890,#24034,.T.);
#46870=EDGE_CURVE('',#36891,#36592,#24035,.T.);
#46871=EDGE_CURVE('',#36892,#36891,#24036,.F.);
#46872=EDGE_CURVE('',#36590,#36892,#24037,.T.);
#46873=EDGE_CURVE('',#36893,#36588,#24038,.T.);
#46874=EDGE_CURVE('',#36894,#36893,#24039,.F.);
#46875=EDGE_CURVE('',#36586,#36894,#24040,.T.);
#46876=EDGE_CURVE('',#36895,#36584,#24041,.T.);
#46877=EDGE_CURVE('',#36896,#36895,#24042,.F.);
#46878=EDGE_CURVE('',#36582,#36896,#24043,.T.);
#46879=EDGE_CURVE('',#36897,#36580,#24044,.T.);
#46880=EDGE_CURVE('',#36898,#36897,#24045,.F.);
#46881=EDGE_CURVE('',#36578,#36898,#24046,.T.);
#46882=EDGE_CURVE('',#36899,#36576,#24047,.T.);
#46883=EDGE_CURVE('',#36900,#36899,#24048,.F.);
#46884=EDGE_CURVE('',#36574,#36900,#24049,.T.);
#46885=EDGE_CURVE('',#36901,#36572,#24050,.T.);
#46886=EDGE_CURVE('',#36902,#36901,#24051,.F.);
#46887=EDGE_CURVE('',#36570,#36902,#24052,.T.);
#46888=EDGE_CURVE('',#36903,#36568,#24053,.T.);
#46889=EDGE_CURVE('',#36904,#36903,#24054,.F.);
#46890=EDGE_CURVE('',#36566,#36904,#24055,.T.);
#46891=EDGE_CURVE('',#36905,#36564,#24056,.T.);
#46892=EDGE_CURVE('',#36906,#36905,#24057,.F.);
#46893=EDGE_CURVE('',#36562,#36906,#24058,.T.);
#46894=EDGE_CURVE('',#36907,#36560,#24059,.T.);
#46895=EDGE_CURVE('',#36908,#36907,#24060,.F.);
#46896=EDGE_CURVE('',#36558,#36908,#24061,.T.);
#46897=EDGE_CURVE('',#36909,#36556,#24062,.T.);
#46898=EDGE_CURVE('',#36910,#36909,#24063,.F.);
#46899=EDGE_CURVE('',#36554,#36910,#24064,.T.);
#46900=EDGE_CURVE('',#36911,#36552,#24065,.T.);
#46901=EDGE_CURVE('',#36912,#36911,#24066,.F.);
#46902=EDGE_CURVE('',#36550,#36912,#24067,.T.);
#46903=EDGE_CURVE('',#36913,#36548,#24068,.T.);
#46904=EDGE_CURVE('',#36914,#36913,#24069,.F.);
#46905=EDGE_CURVE('',#36546,#36914,#24070,.T.);
#46906=EDGE_CURVE('',#36915,#36544,#24071,.T.);
#46907=EDGE_CURVE('',#36916,#36915,#24072,.F.);
#46908=EDGE_CURVE('',#36542,#36916,#24073,.T.);
#46909=EDGE_CURVE('',#36917,#36540,#24074,.T.);
#46910=EDGE_CURVE('',#36918,#36917,#24075,.F.);
#46911=EDGE_CURVE('',#36538,#36918,#24076,.T.);
#46912=EDGE_CURVE('',#36919,#36536,#24077,.T.);
#46913=EDGE_CURVE('',#36920,#36919,#24078,.F.);
#46914=EDGE_CURVE('',#36534,#36920,#24079,.T.);
#46915=EDGE_CURVE('',#36921,#36532,#24080,.T.);
#46916=EDGE_CURVE('',#36922,#36921,#24081,.F.);
#46917=EDGE_CURVE('',#36530,#36922,#24082,.T.);
#46918=EDGE_CURVE('',#36923,#36528,#24083,.T.);
#46919=EDGE_CURVE('',#36924,#36923,#24084,.F.);
#46920=EDGE_CURVE('',#36526,#36924,#24085,.T.);
#46921=EDGE_CURVE('',#36925,#36524,#24086,.T.);
#46922=EDGE_CURVE('',#36926,#36925,#24087,.F.);
#46923=EDGE_CURVE('',#36522,#36926,#24088,.T.);
#46924=EDGE_CURVE('',#36927,#36520,#24089,.T.);
#46925=EDGE_CURVE('',#36928,#36927,#24090,.F.);
#46926=EDGE_CURVE('',#36518,#36928,#24091,.T.);
#46927=EDGE_CURVE('',#36929,#36516,#24092,.T.);
#46928=EDGE_CURVE('',#36930,#36929,#24093,.F.);
#46929=EDGE_CURVE('',#36514,#36930,#24094,.T.);
#46930=EDGE_CURVE('',#36931,#36512,#24095,.T.);
#46931=EDGE_CURVE('',#36932,#36931,#24096,.F.);
#46932=EDGE_CURVE('',#36510,#36932,#24097,.T.);
#46933=EDGE_CURVE('',#36933,#36508,#24098,.T.);
#46934=EDGE_CURVE('',#36934,#36933,#24099,.F.);
#46935=EDGE_CURVE('',#36506,#36934,#24100,.T.);
#46936=EDGE_CURVE('',#36935,#36504,#24101,.T.);
#46937=EDGE_CURVE('',#36936,#36935,#24102,.F.);
#46938=EDGE_CURVE('',#36502,#36936,#24103,.T.);
#46939=EDGE_CURVE('',#36937,#36500,#24104,.T.);
#46940=EDGE_CURVE('',#36938,#36937,#24105,.F.);
#46941=EDGE_CURVE('',#36498,#36938,#24106,.T.);
#46942=EDGE_CURVE('',#36798,#36496,#24107,.T.);
#46943=EDGE_CURVE('',#36786,#36939,#28301,.T.);
#46944=EDGE_CURVE('',#36940,#36939,#24108,.F.);
#46945=EDGE_CURVE('',#36637,#36940,#24109,.T.);
#46946=EDGE_CURVE('',#36941,#36639,#24110,.T.);
#46947=EDGE_CURVE('',#36942,#36941,#24111,.F.);
#46948=EDGE_CURVE('',#36641,#36942,#24112,.T.);
#46949=EDGE_CURVE('',#36943,#36643,#24113,.T.);
#46950=EDGE_CURVE('',#36944,#36943,#24114,.F.);
#46951=EDGE_CURVE('',#36645,#36944,#24115,.T.);
#46952=EDGE_CURVE('',#36945,#36647,#24116,.T.);
#46953=EDGE_CURVE('',#36946,#36945,#24117,.F.);
#46954=EDGE_CURVE('',#36649,#36946,#24118,.T.);
#46955=EDGE_CURVE('',#36947,#36651,#24119,.T.);
#46956=EDGE_CURVE('',#36948,#36947,#24120,.F.);
#46957=EDGE_CURVE('',#36653,#36948,#24121,.T.);
#46958=EDGE_CURVE('',#36949,#36655,#24122,.T.);
#46959=EDGE_CURVE('',#36950,#36949,#24123,.F.);
#46960=EDGE_CURVE('',#36657,#36950,#24124,.T.);
#46961=EDGE_CURVE('',#36951,#36659,#24125,.T.);
#46962=EDGE_CURVE('',#36952,#36951,#24126,.F.);
#46963=EDGE_CURVE('',#36661,#36952,#24127,.T.);
#46964=EDGE_CURVE('',#36953,#36663,#24128,.T.);
#46965=EDGE_CURVE('',#36954,#36953,#24129,.F.);
#46966=EDGE_CURVE('',#36665,#36954,#24130,.T.);
#46967=EDGE_CURVE('',#36955,#36667,#24131,.T.);
#46968=EDGE_CURVE('',#36956,#36955,#24132,.F.);
#46969=EDGE_CURVE('',#36669,#36956,#24133,.T.);
#46970=EDGE_CURVE('',#36957,#36671,#24134,.T.);
#46971=EDGE_CURVE('',#36958,#36957,#24135,.F.);
#46972=EDGE_CURVE('',#36673,#36958,#24136,.T.);
#46973=EDGE_CURVE('',#36959,#36675,#24137,.T.);
#46974=EDGE_CURVE('',#36960,#36959,#24138,.F.);
#46975=EDGE_CURVE('',#36677,#36960,#24139,.T.);
#46976=EDGE_CURVE('',#36961,#36679,#24140,.T.);
#46977=EDGE_CURVE('',#36962,#36961,#24141,.F.);
#46978=EDGE_CURVE('',#36681,#36962,#24142,.T.);
#46979=EDGE_CURVE('',#36963,#36683,#24143,.T.);
#46980=EDGE_CURVE('',#36964,#36963,#24144,.F.);
#46981=EDGE_CURVE('',#36685,#36964,#24145,.T.);
#46982=EDGE_CURVE('',#36965,#36687,#24146,.T.);
#46983=EDGE_CURVE('',#36966,#36965,#24147,.F.);
#46984=EDGE_CURVE('',#36689,#36966,#24148,.T.);
#46985=EDGE_CURVE('',#36967,#36691,#24149,.T.);
#46986=EDGE_CURVE('',#36968,#36967,#24150,.F.);
#46987=EDGE_CURVE('',#36693,#36968,#24151,.T.);
#46988=EDGE_CURVE('',#36969,#36695,#24152,.T.);
#46989=EDGE_CURVE('',#36970,#36969,#24153,.F.);
#46990=EDGE_CURVE('',#36697,#36970,#24154,.T.);
#46991=EDGE_CURVE('',#36971,#36699,#24155,.T.);
#46992=EDGE_CURVE('',#36972,#36971,#24156,.F.);
#46993=EDGE_CURVE('',#36701,#36972,#24157,.T.);
#46994=EDGE_CURVE('',#36973,#36703,#24158,.T.);
#46995=EDGE_CURVE('',#36974,#36973,#24159,.F.);
#46996=EDGE_CURVE('',#36705,#36974,#24160,.T.);
#46997=EDGE_CURVE('',#36975,#36707,#24161,.T.);
#46998=EDGE_CURVE('',#36976,#36975,#24162,.F.);
#46999=EDGE_CURVE('',#36709,#36976,#24163,.T.);
#47000=EDGE_CURVE('',#36977,#36711,#24164,.T.);
#47001=EDGE_CURVE('',#36978,#36977,#24165,.F.);
#47002=EDGE_CURVE('',#36713,#36978,#24166,.T.);
#47003=EDGE_CURVE('',#36979,#36715,#24167,.T.);
#47004=EDGE_CURVE('',#36980,#36979,#24168,.F.);
#47005=EDGE_CURVE('',#36717,#36980,#24169,.T.);
#47006=EDGE_CURVE('',#36981,#36719,#24170,.T.);
#47007=EDGE_CURVE('',#36982,#36981,#24171,.F.);
#47008=EDGE_CURVE('',#36721,#36982,#24172,.T.);
#47009=EDGE_CURVE('',#36983,#36723,#24173,.T.);
#47010=EDGE_CURVE('',#36984,#36983,#24174,.F.);
#47011=EDGE_CURVE('',#36725,#36984,#24175,.T.);
#47012=EDGE_CURVE('',#36985,#36727,#24176,.T.);
#47013=EDGE_CURVE('',#36986,#36985,#24177,.F.);
#47014=EDGE_CURVE('',#36729,#36986,#24178,.T.);
#47015=EDGE_CURVE('',#36987,#36731,#24179,.T.);
#47016=EDGE_CURVE('',#36988,#36987,#24180,.F.);
#47017=EDGE_CURVE('',#36733,#36988,#24181,.T.);
#47018=EDGE_CURVE('',#36989,#36735,#24182,.T.);
#47019=EDGE_CURVE('',#36990,#36989,#24183,.F.);
#47020=EDGE_CURVE('',#36737,#36990,#24184,.T.);
#47021=EDGE_CURVE('',#36991,#36739,#24185,.T.);
#47022=EDGE_CURVE('',#36992,#36991,#24186,.F.);
#47023=EDGE_CURVE('',#36741,#36992,#24187,.T.);
#47024=EDGE_CURVE('',#36993,#36743,#24188,.T.);
#47025=EDGE_CURVE('',#36994,#36993,#24189,.F.);
#47026=EDGE_CURVE('',#36745,#36994,#24190,.T.);
#47027=EDGE_CURVE('',#36995,#36747,#24191,.T.);
#47028=EDGE_CURVE('',#36996,#36995,#24192,.F.);
#47029=EDGE_CURVE('',#36749,#36996,#24193,.T.);
#47030=EDGE_CURVE('',#36997,#36751,#24194,.T.);
#47031=EDGE_CURVE('',#36998,#36997,#24195,.F.);
#47032=EDGE_CURVE('',#36753,#36998,#24196,.T.);
#47033=EDGE_CURVE('',#36999,#36755,#24197,.T.);
#47034=EDGE_CURVE('',#37000,#36999,#24198,.F.);
#47035=EDGE_CURVE('',#36757,#37000,#24199,.T.);
#47036=EDGE_CURVE('',#37001,#36759,#24200,.T.);
#47037=EDGE_CURVE('',#37002,#37001,#24201,.F.);
#47038=EDGE_CURVE('',#36761,#37002,#24202,.T.);
#47039=EDGE_CURVE('',#37003,#36763,#24203,.T.);
#47040=EDGE_CURVE('',#37004,#37003,#24204,.F.);
#47041=EDGE_CURVE('',#36765,#37004,#24205,.T.);
#47042=EDGE_CURVE('',#37005,#36767,#24206,.T.);
#47043=EDGE_CURVE('',#37006,#37005,#24207,.F.);
#47044=EDGE_CURVE('',#36769,#37006,#24208,.T.);
#47045=EDGE_CURVE('',#37007,#36771,#24209,.T.);
#47046=EDGE_CURVE('',#37008,#37007,#24210,.F.);
#47047=EDGE_CURVE('',#36773,#37008,#24211,.T.);
#47048=EDGE_CURVE('',#37009,#36775,#24212,.T.);
#47049=EDGE_CURVE('',#37010,#37009,#24213,.T.);
#47050=EDGE_CURVE('',#36497,#37010,#24214,.T.);
#47051=EDGE_CURVE('',#37011,#36499,#24215,.T.);
#47052=EDGE_CURVE('',#37012,#37011,#24216,.F.);
#47053=EDGE_CURVE('',#36501,#37012,#24217,.T.);
#47054=EDGE_CURVE('',#37013,#36503,#24218,.T.);
#47055=EDGE_CURVE('',#37014,#37013,#24219,.F.);
#47056=EDGE_CURVE('',#36505,#37014,#24220,.T.);
#47057=EDGE_CURVE('',#37015,#36507,#24221,.T.);
#47058=EDGE_CURVE('',#37016,#37015,#24222,.F.);
#47059=EDGE_CURVE('',#36509,#37016,#24223,.T.);
#47060=EDGE_CURVE('',#37017,#36511,#24224,.T.);
#47061=EDGE_CURVE('',#37018,#37017,#24225,.F.);
#47062=EDGE_CURVE('',#36513,#37018,#24226,.T.);
#47063=EDGE_CURVE('',#37019,#36515,#24227,.T.);
#47064=EDGE_CURVE('',#37020,#37019,#24228,.F.);
#47065=EDGE_CURVE('',#36517,#37020,#24229,.T.);
#47066=EDGE_CURVE('',#37021,#36519,#24230,.T.);
#47067=EDGE_CURVE('',#37022,#37021,#24231,.F.);
#47068=EDGE_CURVE('',#36521,#37022,#24232,.T.);
#47069=EDGE_CURVE('',#37023,#36523,#24233,.T.);
#47070=EDGE_CURVE('',#37024,#37023,#24234,.F.);
#47071=EDGE_CURVE('',#36525,#37024,#24235,.T.);
#47072=EDGE_CURVE('',#37025,#36527,#24236,.T.);
#47073=EDGE_CURVE('',#37026,#37025,#24237,.F.);
#47074=EDGE_CURVE('',#36529,#37026,#24238,.T.);
#47075=EDGE_CURVE('',#37027,#36531,#24239,.T.);
#47076=EDGE_CURVE('',#37028,#37027,#24240,.F.);
#47077=EDGE_CURVE('',#36533,#37028,#24241,.T.);
#47078=EDGE_CURVE('',#37029,#36535,#24242,.T.);
#47079=EDGE_CURVE('',#37030,#37029,#24243,.F.);
#47080=EDGE_CURVE('',#36537,#37030,#24244,.T.);
#47081=EDGE_CURVE('',#37031,#36539,#24245,.T.);
#47082=EDGE_CURVE('',#37032,#37031,#24246,.F.);
#47083=EDGE_CURVE('',#36541,#37032,#24247,.T.);
#47084=EDGE_CURVE('',#37033,#36543,#24248,.T.);
#47085=EDGE_CURVE('',#37034,#37033,#24249,.F.);
#47086=EDGE_CURVE('',#36545,#37034,#24250,.T.);
#47087=EDGE_CURVE('',#37035,#36547,#24251,.T.);
#47088=EDGE_CURVE('',#37036,#37035,#24252,.F.);
#47089=EDGE_CURVE('',#36549,#37036,#24253,.T.);
#47090=EDGE_CURVE('',#37037,#36551,#24254,.T.);
#47091=EDGE_CURVE('',#37038,#37037,#24255,.F.);
#47092=EDGE_CURVE('',#36553,#37038,#24256,.T.);
#47093=EDGE_CURVE('',#37039,#36555,#24257,.T.);
#47094=EDGE_CURVE('',#37040,#37039,#24258,.F.);
#47095=EDGE_CURVE('',#36557,#37040,#24259,.T.);
#47096=EDGE_CURVE('',#37041,#36559,#24260,.T.);
#47097=EDGE_CURVE('',#37042,#37041,#24261,.F.);
#47098=EDGE_CURVE('',#36561,#37042,#24262,.T.);
#47099=EDGE_CURVE('',#37043,#36563,#24263,.T.);
#47100=EDGE_CURVE('',#37044,#37043,#24264,.F.);
#47101=EDGE_CURVE('',#36565,#37044,#24265,.T.);
#47102=EDGE_CURVE('',#37045,#36567,#24266,.T.);
#47103=EDGE_CURVE('',#37046,#37045,#24267,.F.);
#47104=EDGE_CURVE('',#36569,#37046,#24268,.T.);
#47105=EDGE_CURVE('',#37047,#36571,#24269,.T.);
#47106=EDGE_CURVE('',#37048,#37047,#24270,.F.);
#47107=EDGE_CURVE('',#36573,#37048,#24271,.T.);
#47108=EDGE_CURVE('',#37049,#36575,#24272,.T.);
#47109=EDGE_CURVE('',#37050,#37049,#24273,.F.);
#47110=EDGE_CURVE('',#36577,#37050,#24274,.T.);
#47111=EDGE_CURVE('',#37051,#36579,#24275,.T.);
#47112=EDGE_CURVE('',#37052,#37051,#24276,.F.);
#47113=EDGE_CURVE('',#36581,#37052,#24277,.T.);
#47114=EDGE_CURVE('',#37053,#36583,#24278,.T.);
#47115=EDGE_CURVE('',#37054,#37053,#24279,.F.);
#47116=EDGE_CURVE('',#36585,#37054,#24280,.T.);
#47117=EDGE_CURVE('',#37055,#36587,#24281,.T.);
#47118=EDGE_CURVE('',#37056,#37055,#24282,.F.);
#47119=EDGE_CURVE('',#36589,#37056,#24283,.T.);
#47120=EDGE_CURVE('',#37057,#36591,#24284,.T.);
#47121=EDGE_CURVE('',#37058,#37057,#24285,.F.);
#47122=EDGE_CURVE('',#36593,#37058,#24286,.T.);
#47123=EDGE_CURVE('',#37059,#36595,#24287,.T.);
#47124=EDGE_CURVE('',#37060,#37059,#24288,.F.);
#47125=EDGE_CURVE('',#36597,#37060,#24289,.T.);
#47126=EDGE_CURVE('',#37061,#36599,#24290,.T.);
#47127=EDGE_CURVE('',#37062,#37061,#24291,.F.);
#47128=EDGE_CURVE('',#36601,#37062,#24292,.T.);
#47129=EDGE_CURVE('',#37063,#36603,#24293,.T.);
#47130=EDGE_CURVE('',#37064,#37063,#24294,.F.);
#47131=EDGE_CURVE('',#36605,#37064,#24295,.T.);
#47132=EDGE_CURVE('',#37065,#36607,#24296,.T.);
#47133=EDGE_CURVE('',#37066,#37065,#24297,.F.);
#47134=EDGE_CURVE('',#36609,#37066,#24298,.T.);
#47135=EDGE_CURVE('',#37067,#36611,#24299,.T.);
#47136=EDGE_CURVE('',#37068,#37067,#24300,.F.);
#47137=EDGE_CURVE('',#36613,#37068,#24301,.T.);
#47138=EDGE_CURVE('',#37069,#36615,#24302,.T.);
#47139=EDGE_CURVE('',#37070,#37069,#24303,.F.);
#47140=EDGE_CURVE('',#36617,#37070,#24304,.T.);
#47141=EDGE_CURVE('',#37071,#36619,#24305,.T.);
#47142=EDGE_CURVE('',#37072,#37071,#24306,.F.);
#47143=EDGE_CURVE('',#36621,#37072,#24307,.T.);
#47144=EDGE_CURVE('',#37073,#36623,#24308,.T.);
#47145=EDGE_CURVE('',#37074,#37073,#24309,.F.);
#47146=EDGE_CURVE('',#36625,#37074,#24310,.T.);
#47147=EDGE_CURVE('',#37075,#36627,#24311,.T.);
#47148=EDGE_CURVE('',#37076,#37075,#24312,.F.);
#47149=EDGE_CURVE('',#36629,#37076,#24313,.T.);
#47150=EDGE_CURVE('',#37077,#36631,#24314,.T.);
#47151=EDGE_CURVE('',#37078,#37077,#24315,.F.);
#47152=EDGE_CURVE('',#36633,#37078,#24316,.T.);
#47153=EDGE_CURVE('',#37079,#36635,#24317,.T.);
#47154=EDGE_CURVE('',#36939,#37079,#24318,.F.);
#47155=EDGE_CURVE('',#36793,#37080,#28302,.T.);
#47156=EDGE_CURVE('',#37080,#37080,#19626,.T.);
#47157=EDGE_CURVE('',#36777,#36795,#28303,.T.);
#47158=EDGE_CURVE('',#36797,#37009,#19627,.T.);
#47159=EDGE_CURVE('',#36798,#37010,#19628,.T.);
#47160=EDGE_CURVE('',#36938,#37011,#19629,.T.);
#47161=EDGE_CURVE('',#36937,#37012,#19630,.T.);
#47162=EDGE_CURVE('',#36936,#37013,#19631,.T.);
#47163=EDGE_CURVE('',#36935,#37014,#19632,.T.);
#47164=EDGE_CURVE('',#36934,#37015,#19633,.T.);
#47165=EDGE_CURVE('',#36933,#37016,#19634,.T.);
#47166=EDGE_CURVE('',#36932,#37017,#19635,.T.);
#47167=EDGE_CURVE('',#36931,#37018,#19636,.T.);
#47168=EDGE_CURVE('',#36930,#37019,#19637,.T.);
#47169=EDGE_CURVE('',#36929,#37020,#19638,.T.);
#47170=EDGE_CURVE('',#36928,#37021,#19639,.T.);
#47171=EDGE_CURVE('',#36927,#37022,#19640,.T.);
#47172=EDGE_CURVE('',#36926,#37023,#19641,.T.);
#47173=EDGE_CURVE('',#36925,#37024,#19642,.T.);
#47174=EDGE_CURVE('',#36924,#37025,#19643,.T.);
#47175=EDGE_CURVE('',#36923,#37026,#19644,.T.);
#47176=EDGE_CURVE('',#36922,#37027,#19645,.T.);
#47177=EDGE_CURVE('',#36921,#37028,#19646,.T.);
#47178=EDGE_CURVE('',#36920,#37029,#19647,.T.);
#47179=EDGE_CURVE('',#36919,#37030,#19648,.T.);
#47180=EDGE_CURVE('',#36918,#37031,#19649,.T.);
#47181=EDGE_CURVE('',#36917,#37032,#19650,.T.);
#47182=EDGE_CURVE('',#36916,#37033,#19651,.T.);
#47183=EDGE_CURVE('',#36915,#37034,#19652,.T.);
#47184=EDGE_CURVE('',#36914,#37035,#19653,.T.);
#47185=EDGE_CURVE('',#36913,#37036,#19654,.T.);
#47186=EDGE_CURVE('',#36912,#37037,#19655,.T.);
#47187=EDGE_CURVE('',#36911,#37038,#19656,.T.);
#47188=EDGE_CURVE('',#36910,#37039,#19657,.T.);
#47189=EDGE_CURVE('',#36909,#37040,#19658,.T.);
#47190=EDGE_CURVE('',#36908,#37041,#19659,.T.);
#47191=EDGE_CURVE('',#36907,#37042,#19660,.T.);
#47192=EDGE_CURVE('',#36906,#37043,#19661,.T.);
#47193=EDGE_CURVE('',#36905,#37044,#19662,.T.);
#47194=EDGE_CURVE('',#36904,#37045,#19663,.T.);
#47195=EDGE_CURVE('',#36903,#37046,#19664,.T.);
#47196=EDGE_CURVE('',#36902,#37047,#19665,.T.);
#47197=EDGE_CURVE('',#36901,#37048,#19666,.T.);
#47198=EDGE_CURVE('',#36900,#37049,#19667,.T.);
#47199=EDGE_CURVE('',#36899,#37050,#19668,.T.);
#47200=EDGE_CURVE('',#36898,#37051,#19669,.T.);
#47201=EDGE_CURVE('',#36897,#37052,#19670,.T.);
#47202=EDGE_CURVE('',#36896,#37053,#19671,.T.);
#47203=EDGE_CURVE('',#36895,#37054,#19672,.T.);
#47204=EDGE_CURVE('',#36894,#37055,#19673,.T.);
#47205=EDGE_CURVE('',#36893,#37056,#19674,.T.);
#47206=EDGE_CURVE('',#36892,#37057,#19675,.T.);
#47207=EDGE_CURVE('',#36891,#37058,#19676,.T.);
#47208=EDGE_CURVE('',#36890,#37059,#19677,.T.);
#47209=EDGE_CURVE('',#36889,#37060,#19678,.T.);
#47210=EDGE_CURVE('',#36888,#37061,#19679,.T.);
#47211=EDGE_CURVE('',#36887,#37062,#19680,.T.);
#47212=EDGE_CURVE('',#36886,#37063,#19681,.T.);
#47213=EDGE_CURVE('',#36885,#37064,#19682,.T.);
#47214=EDGE_CURVE('',#36884,#37065,#19683,.T.);
#47215=EDGE_CURVE('',#36883,#37066,#19684,.T.);
#47216=EDGE_CURVE('',#36882,#37067,#19685,.T.);
#47217=EDGE_CURVE('',#36881,#37068,#19686,.T.);
#47218=EDGE_CURVE('',#36880,#37069,#19687,.T.);
#47219=EDGE_CURVE('',#36879,#37070,#19688,.T.);
#47220=EDGE_CURVE('',#36878,#37071,#19689,.T.);
#47221=EDGE_CURVE('',#36877,#37072,#19690,.T.);
#47222=EDGE_CURVE('',#36876,#37073,#19691,.T.);
#47223=EDGE_CURVE('',#36875,#37074,#19692,.T.);
#47224=EDGE_CURVE('',#36874,#37075,#19693,.T.);
#47225=EDGE_CURVE('',#36873,#37076,#19694,.T.);
#47226=EDGE_CURVE('',#36872,#37077,#19695,.T.);
#47227=EDGE_CURVE('',#36871,#37078,#19696,.T.);
#47228=EDGE_CURVE('',#36870,#37079,#19697,.T.);
#47229=EDGE_CURVE('',#36867,#36940,#19698,.T.);
#47230=EDGE_CURVE('',#36866,#36941,#19699,.T.);
#47231=EDGE_CURVE('',#36865,#36942,#19700,.T.);
#47232=EDGE_CURVE('',#36864,#36943,#19701,.T.);
#47233=EDGE_CURVE('',#36863,#36944,#19702,.T.);
#47234=EDGE_CURVE('',#36862,#36945,#19703,.T.);
#47235=EDGE_CURVE('',#36861,#36946,#19704,.T.);
#47236=EDGE_CURVE('',#36860,#36947,#19705,.T.);
#47237=EDGE_CURVE('',#36859,#36948,#19706,.T.);
#47238=EDGE_CURVE('',#36858,#36949,#19707,.T.);
#47239=EDGE_CURVE('',#36857,#36950,#19708,.T.);
#47240=EDGE_CURVE('',#36856,#36951,#19709,.T.);
#47241=EDGE_CURVE('',#36855,#36952,#19710,.T.);
#47242=EDGE_CURVE('',#36854,#36953,#19711,.T.);
#47243=EDGE_CURVE('',#36853,#36954,#19712,.T.);
#47244=EDGE_CURVE('',#36852,#36955,#19713,.T.);
#47245=EDGE_CURVE('',#36851,#36956,#19714,.T.);
#47246=EDGE_CURVE('',#36850,#36957,#19715,.T.);
#47247=EDGE_CURVE('',#36849,#36958,#19716,.T.);
#47248=EDGE_CURVE('',#36848,#36959,#19717,.T.);
#47249=EDGE_CURVE('',#36847,#36960,#19718,.T.);
#47250=EDGE_CURVE('',#36846,#36961,#19719,.T.);
#47251=EDGE_CURVE('',#36845,#36962,#19720,.T.);
#47252=EDGE_CURVE('',#36844,#36963,#19721,.T.);
#47253=EDGE_CURVE('',#36843,#36964,#19722,.T.);
#47254=EDGE_CURVE('',#36842,#36965,#19723,.T.);
#47255=EDGE_CURVE('',#36841,#36966,#19724,.T.);
#47256=EDGE_CURVE('',#36840,#36967,#19725,.T.);
#47257=EDGE_CURVE('',#36839,#36968,#19726,.T.);
#47258=EDGE_CURVE('',#36838,#36969,#19727,.T.);
#47259=EDGE_CURVE('',#36837,#36970,#19728,.T.);
#47260=EDGE_CURVE('',#36836,#36971,#19729,.T.);
#47261=EDGE_CURVE('',#36835,#36972,#19730,.T.);
#47262=EDGE_CURVE('',#36834,#36973,#19731,.T.);
#47263=EDGE_CURVE('',#36833,#36974,#19732,.T.);
#47264=EDGE_CURVE('',#36832,#36975,#19733,.T.);
#47265=EDGE_CURVE('',#36831,#36976,#19734,.T.);
#47266=EDGE_CURVE('',#36830,#36977,#19735,.T.);
#47267=EDGE_CURVE('',#36829,#36978,#19736,.T.);
#47268=EDGE_CURVE('',#36828,#36979,#19737,.T.);
#47269=EDGE_CURVE('',#36827,#36980,#19738,.T.);
#47270=EDGE_CURVE('',#36826,#36981,#19739,.T.);
#47271=EDGE_CURVE('',#36825,#36982,#19740,.T.);
#47272=EDGE_CURVE('',#36824,#36983,#19741,.T.);
#47273=EDGE_CURVE('',#36823,#36984,#19742,.T.);
#47274=EDGE_CURVE('',#36822,#36985,#19743,.T.);
#47275=EDGE_CURVE('',#36821,#36986,#19744,.T.);
#47276=EDGE_CURVE('',#36820,#36987,#19745,.T.);
#47277=EDGE_CURVE('',#36819,#36988,#19746,.T.);
#47278=EDGE_CURVE('',#36818,#36989,#19747,.T.);
#47279=EDGE_CURVE('',#36817,#36990,#19748,.T.);
#47280=EDGE_CURVE('',#36816,#36991,#19749,.T.);
#47281=EDGE_CURVE('',#36815,#36992,#19750,.T.);
#47282=EDGE_CURVE('',#36814,#36993,#19751,.T.);
#47283=EDGE_CURVE('',#36813,#36994,#19752,.T.);
#47284=EDGE_CURVE('',#36812,#36995,#19753,.T.);
#47285=EDGE_CURVE('',#36811,#36996,#19754,.T.);
#47286=EDGE_CURVE('',#36810,#36997,#19755,.T.);
#47287=EDGE_CURVE('',#36809,#36998,#19756,.T.);
#47288=EDGE_CURVE('',#36808,#36999,#19757,.T.);
#47289=EDGE_CURVE('',#36807,#37000,#19758,.T.);
#47290=EDGE_CURVE('',#36806,#37001,#19759,.T.);
#47291=EDGE_CURVE('',#36805,#37002,#19760,.T.);
#47292=EDGE_CURVE('',#36804,#37003,#19761,.T.);
#47293=EDGE_CURVE('',#36803,#37004,#19762,.T.);
#47294=EDGE_CURVE('',#36802,#37005,#19763,.T.);
#47295=EDGE_CURVE('',#36801,#37006,#19764,.T.);
#47296=EDGE_CURVE('',#36800,#37007,#19765,.T.);
#47297=EDGE_CURVE('',#36799,#37008,#19766,.T.);
#47298=EDGE_CURVE('',#37081,#37081,#19767,.T.);
#47299=EDGE_CURVE('',#37081,#37082,#28304,.T.);
#47300=EDGE_CURVE('',#37082,#37082,#19768,.T.);
#47301=EDGE_CURVE('',#37083,#37083,#19769,.T.);
#47302=EDGE_CURVE('',#37083,#37084,#28305,.T.);
#47303=EDGE_CURVE('',#37084,#37084,#19770,.T.);
#47304=EDGE_CURVE('',#37085,#37085,#19771,.T.);
#47305=EDGE_CURVE('',#37085,#37086,#19772,.T.);
#47306=EDGE_CURVE('',#37086,#37086,#19773,.T.);
#47307=EDGE_CURVE('',#37087,#37087,#19774,.T.);
#47308=EDGE_CURVE('',#37087,#37088,#19775,.T.);
#47309=EDGE_CURVE('',#37088,#37088,#19776,.T.);
#47310=EDGE_CURVE('',#37089,#37090,#19777,.T.);
#47311=EDGE_CURVE('',#37089,#37091,#19778,.T.);
#47312=EDGE_CURVE('',#37091,#37091,#19779,.T.);
#47313=EDGE_CURVE('',#37090,#37089,#19780,.T.);
#47314=EDGE_CURVE('',#37092,#37092,#19781,.T.);
#47315=EDGE_CURVE('',#37092,#37093,#19782,.T.);
#47316=EDGE_CURVE('',#37093,#37093,#19783,.T.);
#47317=EDGE_CURVE('',#37094,#37094,#19784,.T.);
#47318=EDGE_CURVE('',#37094,#37095,#19785,.T.);
#47319=EDGE_CURVE('',#37096,#37095,#19786,.T.);
#47320=EDGE_CURVE('',#37095,#37096,#19787,.T.);
#47321=EDGE_CURVE('',#37097,#37098,#19788,.T.);
#47322=EDGE_CURVE('',#37097,#37099,#19789,.T.);
#47323=EDGE_CURVE('',#37100,#37099,#19790,.T.);
#47324=EDGE_CURVE('',#37098,#37100,#19791,.T.);
#47325=EDGE_CURVE('',#37101,#37102,#19792,.T.);
#47326=EDGE_CURVE('',#37101,#37103,#19793,.T.);
#47327=EDGE_CURVE('',#37104,#37103,#19794,.T.);
#47328=EDGE_CURVE('',#37102,#37104,#19795,.T.);
#47329=EDGE_CURVE('',#37105,#37105,#19796,.T.);
#47330=EDGE_CURVE('',#37105,#37106,#19797,.T.);
#47331=EDGE_CURVE('',#37107,#37106,#19798,.T.);
#47332=EDGE_CURVE('',#37106,#37107,#19799,.T.);
#47333=EDGE_CURVE('',#37108,#37108,#19800,.T.);
#47334=EDGE_CURVE('',#37108,#37109,#19801,.T.);
#47335=EDGE_CURVE('',#37110,#37109,#19802,.T.);
#47336=EDGE_CURVE('',#37109,#37110,#19803,.T.);
#47337=EDGE_CURVE('',#37111,#37111,#19804,.T.);
#47338=EDGE_CURVE('',#37111,#37112,#19805,.T.);
#47339=EDGE_CURVE('',#37113,#37112,#19806,.T.);
#47340=EDGE_CURVE('',#37112,#37113,#19807,.T.);
#47341=EDGE_CURVE('',#37114,#37115,#19808,.T.);
#47342=EDGE_CURVE('',#37116,#37115,#28306,.T.);
#47343=EDGE_CURVE('',#37116,#37117,#19809,.T.);
#47344=EDGE_CURVE('',#37117,#37114,#28307,.T.);
#47345=EDGE_CURVE('',#37118,#37119,#19810,.T.);
#47346=EDGE_CURVE('',#37120,#37119,#28308,.T.);
#47347=EDGE_CURVE('',#37120,#37121,#19811,.T.);
#47348=EDGE_CURVE('',#37121,#37118,#28309,.T.);
#47349=EDGE_CURVE('',#37122,#37122,#19812,.T.);
#47350=EDGE_CURVE('',#37122,#37107,#28310,.T.);
#47351=EDGE_CURVE('',#37086,#37110,#28311,.T.);
#47352=EDGE_CURVE('',#37088,#37113,#28312,.T.);
#47353=EDGE_CURVE('',#37123,#37123,#19813,.T.);
#47354=EDGE_CURVE('',#37123,#37096,#28313,.T.);
#47355=EDGE_CURVE('',#37124,#37125,#19814,.T.);
#47356=EDGE_CURVE('',#37125,#37126,#28314,.T.);
#47357=EDGE_CURVE('',#37127,#37126,#19815,.T.);
#47358=EDGE_CURVE('',#37124,#37127,#28315,.T.);
#47359=EDGE_CURVE('',#37128,#37129,#19816,.T.);
#47360=EDGE_CURVE('',#37129,#37130,#28316,.T.);
#47361=EDGE_CURVE('',#37131,#37130,#19817,.T.);
#47362=EDGE_CURVE('',#37128,#37131,#28317,.T.);
#47363=EDGE_CURVE('',#37132,#37133,#19818,.T.);
#47364=EDGE_CURVE('',#37133,#37134,#28318,.T.);
#47365=EDGE_CURVE('',#37134,#37135,#19819,.T.);
#47366=EDGE_CURVE('',#37135,#37132,#28319,.T.);
#47367=EDGE_CURVE('',#37136,#37137,#19820,.T.);
#47368=EDGE_CURVE('',#37137,#37138,#28320,.T.);
#47369=EDGE_CURVE('',#37138,#37139,#19821,.T.);
#47370=EDGE_CURVE('',#37139,#37136,#28321,.T.);
#47371=EDGE_CURVE('',#37090,#37092,#28322,.T.);
#47372=EDGE_CURVE('',#37140,#37141,#19822,.T.);
#47373=EDGE_CURVE('',#37142,#37140,#19823,.T.);
#47374=EDGE_CURVE('',#37143,#37142,#19824,.T.);
#47375=EDGE_CURVE('',#37144,#37143,#19825,.T.);
#47376=EDGE_CURVE('',#37145,#37144,#19826,.T.);
#47377=EDGE_CURVE('',#37146,#37145,#19827,.T.);
#47378=EDGE_CURVE('',#37147,#37146,#19828,.T.);
#47379=EDGE_CURVE('',#37148,#37147,#19829,.T.);
#47380=EDGE_CURVE('',#37149,#37148,#19830,.T.);
#47381=EDGE_CURVE('',#37150,#37149,#19831,.T.);
#47382=EDGE_CURVE('',#37151,#37150,#19832,.T.);
#47383=EDGE_CURVE('',#37152,#37151,#19833,.T.);
#47384=EDGE_CURVE('',#37153,#37152,#19834,.T.);
#47385=EDGE_CURVE('',#37154,#37153,#19835,.T.);
#47386=EDGE_CURVE('',#37155,#37154,#19836,.T.);
#47387=EDGE_CURVE('',#37156,#37155,#19837,.T.);
#47388=EDGE_CURVE('',#37157,#37156,#19838,.T.);
#47389=EDGE_CURVE('',#37158,#37157,#19839,.T.);
#47390=EDGE_CURVE('',#37159,#37158,#19840,.T.);
#47391=EDGE_CURVE('',#37160,#37159,#19841,.T.);
#47392=EDGE_CURVE('',#37161,#37160,#19842,.T.);
#47393=EDGE_CURVE('',#37162,#37161,#19843,.T.);
#47394=EDGE_CURVE('',#37163,#37162,#19844,.T.);
#47395=EDGE_CURVE('',#37164,#37163,#19845,.T.);
#47396=EDGE_CURVE('',#37165,#37164,#19846,.T.);
#47397=EDGE_CURVE('',#37166,#37165,#19847,.T.);
#47398=EDGE_CURVE('',#37167,#37166,#19848,.T.);
#47399=EDGE_CURVE('',#37168,#37167,#19849,.T.);
#47400=EDGE_CURVE('',#37169,#37168,#19850,.T.);
#47401=EDGE_CURVE('',#37133,#37169,#19851,.T.);
#47402=EDGE_CURVE('',#37170,#37132,#19852,.T.);
#47403=EDGE_CURVE('',#37171,#37170,#19853,.T.);
#47404=EDGE_CURVE('',#37137,#37171,#19854,.T.);
#47405=EDGE_CURVE('',#37172,#37136,#19855,.T.);
#47406=EDGE_CURVE('',#37173,#37172,#19856,.T.);
#47407=EDGE_CURVE('',#37174,#37173,#19857,.T.);
#47408=EDGE_CURVE('',#37175,#37174,#19858,.T.);
#47409=EDGE_CURVE('',#37176,#37175,#19859,.T.);
#47410=EDGE_CURVE('',#37177,#37176,#19860,.T.);
#47411=EDGE_CURVE('',#37178,#37177,#19861,.T.);
#47412=EDGE_CURVE('',#37179,#37178,#19862,.T.);
#47413=EDGE_CURVE('',#37180,#37179,#19863,.T.);
#47414=EDGE_CURVE('',#37181,#37180,#19864,.T.);
#47415=EDGE_CURVE('',#37182,#37181,#19865,.T.);
#47416=EDGE_CURVE('',#37183,#37182,#19866,.T.);
#47417=EDGE_CURVE('',#37184,#37183,#19867,.T.);
#47418=EDGE_CURVE('',#37185,#37184,#19868,.T.);
#47419=EDGE_CURVE('',#37186,#37185,#19869,.T.);
#47420=EDGE_CURVE('',#37187,#37186,#19870,.T.);
#47421=EDGE_CURVE('',#37188,#37187,#19871,.T.);
#47422=EDGE_CURVE('',#37189,#37188,#19872,.T.);
#47423=EDGE_CURVE('',#37190,#37189,#19873,.T.);
#47424=EDGE_CURVE('',#37191,#37190,#19874,.T.);
#47425=EDGE_CURVE('',#37192,#37191,#19875,.T.);
#47426=EDGE_CURVE('',#37193,#37192,#19876,.T.);
#47427=EDGE_CURVE('',#37194,#37193,#19877,.T.);
#47428=EDGE_CURVE('',#37195,#37194,#19878,.T.);
#47429=EDGE_CURVE('',#37196,#37195,#19879,.T.);
#47430=EDGE_CURVE('',#37197,#37196,#19880,.T.);
#47431=EDGE_CURVE('',#37198,#37197,#19881,.T.);
#47432=EDGE_CURVE('',#37199,#37198,#19882,.T.);
#47433=EDGE_CURVE('',#37200,#37199,#19883,.T.);
#47434=EDGE_CURVE('',#37201,#37200,#19884,.T.);
#47435=EDGE_CURVE('',#37202,#37201,#19885,.T.);
#47436=EDGE_CURVE('',#37203,#37202,#19886,.T.);
#47437=EDGE_CURVE('',#37204,#37203,#19887,.T.);
#47438=EDGE_CURVE('',#37205,#37204,#19888,.T.);
#47439=EDGE_CURVE('',#37206,#37205,#19889,.T.);
#47440=EDGE_CURVE('',#37207,#37206,#19890,.T.);
#47441=EDGE_CURVE('',#37208,#37207,#19891,.T.);
#47442=EDGE_CURVE('',#37209,#37208,#19892,.T.);
#47443=EDGE_CURVE('',#37210,#37209,#19893,.T.);
#47444=EDGE_CURVE('',#37211,#37210,#19894,.T.);
#47445=EDGE_CURVE('',#37212,#37211,#19895,.T.);
#47446=EDGE_CURVE('',#37213,#37212,#19896,.T.);
#47447=EDGE_CURVE('',#37214,#37213,#19897,.T.);
#47448=EDGE_CURVE('',#37215,#37214,#19898,.T.);
#47449=EDGE_CURVE('',#37216,#37215,#19899,.T.);
#47450=EDGE_CURVE('',#37217,#37216,#19900,.T.);
#47451=EDGE_CURVE('',#37218,#37217,#19901,.T.);
#47452=EDGE_CURVE('',#37219,#37218,#19902,.T.);
#47453=EDGE_CURVE('',#37220,#37219,#19903,.T.);
#47454=EDGE_CURVE('',#37221,#37220,#19904,.T.);
#47455=EDGE_CURVE('',#37222,#37221,#19905,.T.);
#47456=EDGE_CURVE('',#37223,#37222,#19906,.T.);
#47457=EDGE_CURVE('',#37224,#37223,#19907,.T.);
#47458=EDGE_CURVE('',#37225,#37224,#19908,.T.);
#47459=EDGE_CURVE('',#37226,#37225,#19909,.T.);
#47460=EDGE_CURVE('',#37227,#37226,#19910,.T.);
#47461=EDGE_CURVE('',#37228,#37227,#19911,.T.);
#47462=EDGE_CURVE('',#37229,#37228,#19912,.T.);
#47463=EDGE_CURVE('',#37230,#37229,#19913,.T.);
#47464=EDGE_CURVE('',#37231,#37230,#19914,.T.);
#47465=EDGE_CURVE('',#37232,#37231,#19915,.T.);
#47466=EDGE_CURVE('',#37233,#37232,#19916,.T.);
#47467=EDGE_CURVE('',#37234,#37233,#19917,.T.);
#47468=EDGE_CURVE('',#37235,#37234,#19918,.T.);
#47469=EDGE_CURVE('',#37236,#37235,#19919,.T.);
#47470=EDGE_CURVE('',#37237,#37236,#19920,.T.);
#47471=EDGE_CURVE('',#37238,#37237,#19921,.T.);
#47472=EDGE_CURVE('',#37239,#37238,#19922,.T.);
#47473=EDGE_CURVE('',#37240,#37239,#19923,.T.);
#47474=EDGE_CURVE('',#37241,#37240,#19924,.T.);
#47475=EDGE_CURVE('',#37242,#37241,#19925,.T.);
#47476=EDGE_CURVE('',#37243,#37242,#19926,.T.);
#47477=EDGE_CURVE('',#37244,#37243,#19927,.T.);
#47478=EDGE_CURVE('',#37245,#37244,#19928,.T.);
#47479=EDGE_CURVE('',#37246,#37245,#19929,.T.);
#47480=EDGE_CURVE('',#37247,#37246,#19930,.T.);
#47481=EDGE_CURVE('',#37248,#37247,#19931,.T.);
#47482=EDGE_CURVE('',#37249,#37248,#19932,.T.);
#47483=EDGE_CURVE('',#37250,#37249,#19933,.T.);
#47484=EDGE_CURVE('',#37251,#37250,#19934,.T.);
#47485=EDGE_CURVE('',#37252,#37251,#19935,.T.);
#47486=EDGE_CURVE('',#37253,#37252,#19936,.T.);
#47487=EDGE_CURVE('',#37254,#37253,#19937,.T.);
#47488=EDGE_CURVE('',#37255,#37254,#19938,.T.);
#47489=EDGE_CURVE('',#37125,#37255,#19939,.T.);
#47490=EDGE_CURVE('',#37256,#37124,#19940,.T.);
#47491=EDGE_CURVE('',#37257,#37256,#19941,.T.);
#47492=EDGE_CURVE('',#37129,#37257,#19942,.T.);
#47493=EDGE_CURVE('',#37258,#37128,#19943,.T.);
#47494=EDGE_CURVE('',#37259,#37258,#19944,.T.);
#47495=EDGE_CURVE('',#37260,#37259,#19945,.T.);
#47496=EDGE_CURVE('',#37261,#37260,#19946,.T.);
#47497=EDGE_CURVE('',#37262,#37261,#19947,.T.);
#47498=EDGE_CURVE('',#37263,#37262,#19948,.T.);
#47499=EDGE_CURVE('',#37264,#37263,#19949,.T.);
#47500=EDGE_CURVE('',#37265,#37264,#19950,.T.);
#47501=EDGE_CURVE('',#37266,#37265,#19951,.T.);
#47502=EDGE_CURVE('',#37267,#37266,#19952,.T.);
#47503=EDGE_CURVE('',#37268,#37267,#19953,.T.);
#47504=EDGE_CURVE('',#37269,#37268,#19954,.T.);
#47505=EDGE_CURVE('',#37270,#37269,#19955,.T.);
#47506=EDGE_CURVE('',#37271,#37270,#19956,.T.);
#47507=EDGE_CURVE('',#37272,#37271,#19957,.T.);
#47508=EDGE_CURVE('',#37273,#37272,#19958,.T.);
#47509=EDGE_CURVE('',#37274,#37273,#19959,.T.);
#47510=EDGE_CURVE('',#37275,#37274,#19960,.T.);
#47511=EDGE_CURVE('',#37276,#37275,#19961,.T.);
#47512=EDGE_CURVE('',#37277,#37276,#19962,.T.);
#47513=EDGE_CURVE('',#37278,#37277,#19963,.T.);
#47514=EDGE_CURVE('',#37279,#37278,#19964,.T.);
#47515=EDGE_CURVE('',#37141,#37279,#19965,.T.);
#47516=EDGE_CURVE('',#37280,#37281,#19966,.T.);
#47517=EDGE_CURVE('',#37281,#37282,#19967,.T.);
#47518=EDGE_CURVE('',#37282,#37104,#28323,.T.);
#47519=EDGE_CURVE('',#37103,#37283,#19968,.T.);
#47520=EDGE_CURVE('',#37283,#37284,#19969,.T.);
#47521=EDGE_CURVE('',#37284,#37285,#28324,.T.);
#47522=EDGE_CURVE('',#37285,#37280,#19970,.T.);
#47523=EDGE_CURVE('',#37286,#37287,#28325,.T.);
#47524=EDGE_CURVE('',#37287,#37288,#19971,.T.);
#47525=EDGE_CURVE('',#37288,#37100,#19972,.T.);
#47526=EDGE_CURVE('',#37099,#37289,#28326,.T.);
#47527=EDGE_CURVE('',#37289,#37290,#19973,.T.);
#47528=EDGE_CURVE('',#37290,#37291,#19974,.T.);
#47529=EDGE_CURVE('',#37291,#37286,#19975,.T.);
#47530=EDGE_CURVE('',#37141,#37292,#28327,.T.);
#47531=EDGE_CURVE('',#37293,#37279,#28328,.T.);
#47532=EDGE_CURVE('',#37292,#37293,#19976,.T.);
#47533=EDGE_CURVE('',#37294,#37143,#28329,.T.);
#47534=EDGE_CURVE('',#37295,#37294,#19977,.T.);
#47535=EDGE_CURVE('',#37144,#37295,#28330,.T.);
#47536=EDGE_CURVE('',#37276,#37296,#28331,.T.);
#47537=EDGE_CURVE('',#37297,#37275,#28332,.T.);
#47538=EDGE_CURVE('',#37296,#37297,#19978,.T.);
#47539=EDGE_CURVE('',#37272,#37298,#28333,.T.);
#47540=EDGE_CURVE('',#37299,#37271,#28334,.T.);
#47541=EDGE_CURVE('',#37298,#37299,#19979,.T.);
#47542=EDGE_CURVE('',#37268,#37300,#28335,.T.);
#47543=EDGE_CURVE('',#37301,#37267,#28336,.T.);
#47544=EDGE_CURVE('',#37300,#37301,#19980,.T.);
#47545=EDGE_CURVE('',#37302,#37255,#28337,.T.);
#47546=EDGE_CURVE('',#37126,#37302,#19981,.T.);
#47547=EDGE_CURVE('',#37303,#37257,#28338,.T.);
#47548=EDGE_CURVE('',#37130,#37303,#19982,.T.);
#47549=EDGE_CURVE('',#37304,#37259,#28339,.T.);
#47550=EDGE_CURVE('',#37305,#37304,#19983,.T.);
#47551=EDGE_CURVE('',#37260,#37305,#28340,.T.);
#47552=EDGE_CURVE('',#37264,#37306,#28341,.T.);
#47553=EDGE_CURVE('',#37307,#37263,#28342,.T.);
#47554=EDGE_CURVE('',#37306,#37307,#19984,.T.);
#47555=EDGE_CURVE('',#37164,#37308,#28343,.T.);
#47556=EDGE_CURVE('',#37309,#37163,#28344,.T.);
#47557=EDGE_CURVE('',#37308,#37309,#19985,.T.);
#47558=EDGE_CURVE('',#37310,#37167,#28345,.T.);
#47559=EDGE_CURVE('',#37311,#37310,#19986,.T.);
#47560=EDGE_CURVE('',#37168,#37311,#28346,.T.);
#47561=EDGE_CURVE('',#37160,#37312,#28347,.T.);
#47562=EDGE_CURVE('',#37313,#37159,#28348,.T.);
#47563=EDGE_CURVE('',#37312,#37313,#19987,.T.);
#47564=EDGE_CURVE('',#37314,#37135,#19988,.T.);
#47565=EDGE_CURVE('',#37170,#37314,#28349,.T.);
#47566=EDGE_CURVE('',#37315,#37139,#19989,.T.);
#47567=EDGE_CURVE('',#37172,#37315,#28350,.T.);
#47568=EDGE_CURVE('',#37316,#37175,#28351,.T.);
#47569=EDGE_CURVE('',#37317,#37316,#19990,.T.);
#47570=EDGE_CURVE('',#37176,#37317,#28352,.T.);
#47571=EDGE_CURVE('',#37152,#37318,#28353,.T.);
#47572=EDGE_CURVE('',#37319,#37151,#28354,.T.);
#47573=EDGE_CURVE('',#37318,#37319,#19991,.T.);
#47574=EDGE_CURVE('',#37320,#37155,#28355,.T.);
#47575=EDGE_CURVE('',#37321,#37320,#19992,.T.);
#47576=EDGE_CURVE('',#37156,#37321,#28356,.T.);
#47577=EDGE_CURVE('',#37148,#37322,#28357,.T.);
#47578=EDGE_CURVE('',#37323,#37147,#28358,.T.);
#47579=EDGE_CURVE('',#37322,#37323,#19993,.T.);
#47580=EDGE_CURVE('',#37196,#37324,#28359,.T.);
#47581=EDGE_CURVE('',#37325,#37195,#28360,.T.);
#47582=EDGE_CURVE('',#37324,#37325,#19994,.T.);
#47583=EDGE_CURVE('',#37326,#37199,#28361,.T.);
#47584=EDGE_CURVE('',#37327,#37326,#19995,.T.);
#47585=EDGE_CURVE('',#37200,#37327,#28362,.T.);
#47586=EDGE_CURVE('',#37192,#37328,#28363,.T.);
#47587=EDGE_CURVE('',#37329,#37191,#28364,.T.);
#47588=EDGE_CURVE('',#37328,#37329,#19996,.T.);
#47589=EDGE_CURVE('',#37330,#37203,#28365,.T.);
#47590=EDGE_CURVE('',#37331,#37330,#19997,.T.);
#47591=EDGE_CURVE('',#37204,#37331,#28366,.T.);
#47592=EDGE_CURVE('',#37332,#37207,#28367,.T.);
#47593=EDGE_CURVE('',#37333,#37332,#19998,.T.);
#47594=EDGE_CURVE('',#37208,#37333,#28368,.T.);
#47595=EDGE_CURVE('',#37334,#37211,#28369,.T.);
#47596=EDGE_CURVE('',#37335,#37334,#19999,.T.);
#47597=EDGE_CURVE('',#37212,#37335,#28370,.T.);
#47598=EDGE_CURVE('',#37184,#37336,#28371,.T.);
#47599=EDGE_CURVE('',#37337,#37183,#28372,.T.);
#47600=EDGE_CURVE('',#37336,#37337,#20000,.T.);
#47601=EDGE_CURVE('',#37338,#37187,#28373,.T.);
#47602=EDGE_CURVE('',#37339,#37338,#20001,.T.);
#47603=EDGE_CURVE('',#37188,#37339,#28374,.T.);
#47604=EDGE_CURVE('',#37180,#37340,#28375,.T.);
#47605=EDGE_CURVE('',#37341,#37179,#28376,.T.);
#47606=EDGE_CURVE('',#37340,#37341,#20002,.T.);
#47607=EDGE_CURVE('',#37232,#37342,#28377,.T.);
#47608=EDGE_CURVE('',#37343,#37231,#28378,.T.);
#47609=EDGE_CURVE('',#37342,#37343,#20003,.T.);
#47610=EDGE_CURVE('',#37344,#37235,#28379,.T.);
#47611=EDGE_CURVE('',#37345,#37344,#20004,.T.);
#47612=EDGE_CURVE('',#37236,#37345,#28380,.T.);
#47613=EDGE_CURVE('',#37228,#37346,#28381,.T.);
#47614=EDGE_CURVE('',#37347,#37227,#28382,.T.);
#47615=EDGE_CURVE('',#37346,#37347,#20005,.T.);
#47616=EDGE_CURVE('',#37348,#37239,#28383,.T.);
#47617=EDGE_CURVE('',#37349,#37348,#20006,.T.);
#47618=EDGE_CURVE('',#37240,#37349,#28384,.T.);
#47619=EDGE_CURVE('',#37350,#37243,#28385,.T.);
#47620=EDGE_CURVE('',#37351,#37350,#20007,.T.);
#47621=EDGE_CURVE('',#37244,#37351,#28386,.T.);
#47622=EDGE_CURVE('',#37352,#37247,#28387,.T.);
#47623=EDGE_CURVE('',#37353,#37352,#20008,.T.);
#47624=EDGE_CURVE('',#37248,#37353,#28388,.T.);
#47625=EDGE_CURVE('',#37224,#37354,#28389,.T.);
#47626=EDGE_CURVE('',#37355,#37223,#28390,.T.);
#47627=EDGE_CURVE('',#37354,#37355,#20009,.T.);
#47628=EDGE_CURVE('',#37220,#37356,#28391,.T.);
#47629=EDGE_CURVE('',#37357,#37219,#28392,.T.);
#47630=EDGE_CURVE('',#37356,#37357,#20010,.T.);
#47631=EDGE_CURVE('',#37216,#37358,#28393,.T.);
#47632=EDGE_CURVE('',#37359,#37215,#28394,.T.);
#47633=EDGE_CURVE('',#37358,#37359,#20011,.T.);
#47634=EDGE_CURVE('',#37360,#37292,#20012,.T.);
#47635=EDGE_CURVE('',#37361,#37293,#20013,.T.);
#47636=EDGE_CURVE('',#37361,#37362,#20014,.T.);
#47637=EDGE_CURVE('',#37362,#37296,#20015,.T.);
#47638=EDGE_CURVE('',#37363,#37297,#20016,.T.);
#47639=EDGE_CURVE('',#37363,#37364,#20017,.T.);
#47640=EDGE_CURVE('',#37364,#37298,#20018,.T.);
#47641=EDGE_CURVE('',#37365,#37299,#20019,.T.);
#47642=EDGE_CURVE('',#37365,#37366,#20020,.T.);
#47643=EDGE_CURVE('',#37366,#37300,#20021,.T.);
#47644=EDGE_CURVE('',#37367,#37301,#20022,.T.);
#47645=EDGE_CURVE('',#37367,#37368,#20023,.T.);
#47646=EDGE_CURVE('',#37368,#37306,#20024,.T.);
#47647=EDGE_CURVE('',#37369,#37307,#20025,.T.);
#47648=EDGE_CURVE('',#37369,#37370,#20026,.T.);
#47649=EDGE_CURVE('',#37370,#37305,#20027,.T.);
#47650=EDGE_CURVE('',#37371,#37304,#20028,.T.);
#47651=EDGE_CURVE('',#37371,#37131,#20029,.T.);
#47652=EDGE_CURVE('',#37372,#37303,#20030,.T.);
#47653=EDGE_CURVE('',#37372,#37127,#20031,.T.);
#47654=EDGE_CURVE('',#37373,#37302,#20032,.T.);
#47655=EDGE_CURVE('',#37373,#37374,#20033,.T.);
#47656=EDGE_CURVE('',#37374,#37375,#20034,.T.);
#47657=EDGE_CURVE('',#37375,#37376,#20035,.T.);
#47658=EDGE_CURVE('',#37377,#37376,#20036,.T.);
#47659=EDGE_CURVE('',#37377,#37378,#20037,.T.);
#47660=EDGE_CURVE('',#37378,#37353,#20038,.T.);
#47661=EDGE_CURVE('',#37379,#37352,#20039,.T.);
#47662=EDGE_CURVE('',#37379,#37380,#20040,.T.);
#47663=EDGE_CURVE('',#37380,#37351,#20041,.T.);
#47664=EDGE_CURVE('',#37381,#37350,#20042,.T.);
#47665=EDGE_CURVE('',#37381,#37382,#20043,.T.);
#47666=EDGE_CURVE('',#37382,#37349,#20044,.T.);
#47667=EDGE_CURVE('',#37383,#37348,#20045,.T.);
#47668=EDGE_CURVE('',#37383,#37384,#20046,.T.);
#47669=EDGE_CURVE('',#37384,#37345,#20047,.T.);
#47670=EDGE_CURVE('',#37385,#37344,#20048,.T.);
#47671=EDGE_CURVE('',#37385,#37386,#20049,.T.);
#47672=EDGE_CURVE('',#37386,#37342,#20050,.T.);
#47673=EDGE_CURVE('',#37387,#37343,#20051,.T.);
#47674=EDGE_CURVE('',#37387,#37388,#20052,.T.);
#47675=EDGE_CURVE('',#37388,#37346,#20053,.T.);
#47676=EDGE_CURVE('',#37389,#37347,#20054,.T.);
#47677=EDGE_CURVE('',#37389,#37390,#20055,.T.);
#47678=EDGE_CURVE('',#37390,#37354,#20056,.T.);
#47679=EDGE_CURVE('',#37391,#37355,#20057,.T.);
#47680=EDGE_CURVE('',#37391,#37392,#20058,.T.);
#47681=EDGE_CURVE('',#37392,#37356,#20059,.T.);
#47682=EDGE_CURVE('',#37393,#37357,#20060,.T.);
#47683=EDGE_CURVE('',#37393,#37394,#20061,.T.);
#47684=EDGE_CURVE('',#37394,#37358,#20062,.T.);
#47685=EDGE_CURVE('',#37395,#37359,#20063,.T.);
#47686=EDGE_CURVE('',#37395,#37396,#20064,.T.);
#47687=EDGE_CURVE('',#37396,#37335,#20065,.T.);
#47688=EDGE_CURVE('',#37397,#37334,#20066,.T.);
#47689=EDGE_CURVE('',#37397,#37398,#20067,.T.);
#47690=EDGE_CURVE('',#37398,#37333,#20068,.T.);
#47691=EDGE_CURVE('',#37399,#37332,#20069,.T.);
#47692=EDGE_CURVE('',#37399,#37400,#20070,.T.);
#47693=EDGE_CURVE('',#37400,#37331,#20071,.T.);
#47694=EDGE_CURVE('',#37401,#37330,#20072,.T.);
#47695=EDGE_CURVE('',#37401,#37402,#20073,.T.);
#47696=EDGE_CURVE('',#37402,#37327,#20074,.T.);
#47697=EDGE_CURVE('',#37403,#37326,#20075,.T.);
#47698=EDGE_CURVE('',#37403,#37404,#20076,.T.);
#47699=EDGE_CURVE('',#37404,#37324,#20077,.T.);
#47700=EDGE_CURVE('',#37405,#37325,#20078,.T.);
#47701=EDGE_CURVE('',#37405,#37406,#20079,.T.);
#47702=EDGE_CURVE('',#37406,#37328,#20080,.T.);
#47703=EDGE_CURVE('',#37407,#37329,#20081,.T.);
#47704=EDGE_CURVE('',#37407,#37408,#20082,.T.);
#47705=EDGE_CURVE('',#37408,#37339,#20083,.T.);
#47706=EDGE_CURVE('',#37409,#37338,#20084,.T.);
#47707=EDGE_CURVE('',#37409,#37410,#20085,.T.);
#47708=EDGE_CURVE('',#37410,#37336,#20086,.T.);
#47709=EDGE_CURVE('',#37411,#37337,#20087,.T.);
#47710=EDGE_CURVE('',#37411,#37412,#20088,.T.);
#47711=EDGE_CURVE('',#37412,#37340,#20089,.T.);
#47712=EDGE_CURVE('',#37413,#37341,#20090,.T.);
#47713=EDGE_CURVE('',#37413,#37414,#20091,.T.);
#47714=EDGE_CURVE('',#37414,#37317,#20092,.T.);
#47715=EDGE_CURVE('',#37415,#37316,#20093,.T.);
#47716=EDGE_CURVE('',#37415,#37416,#20094,.T.);
#47717=EDGE_CURVE('',#37416,#37315,#20095,.T.);
#47718=EDGE_CURVE('',#37138,#37417,#20096,.T.);
#47719=EDGE_CURVE('',#37417,#37314,#20097,.T.);
#47720=EDGE_CURVE('',#37134,#37418,#20098,.T.);
#47721=EDGE_CURVE('',#37418,#37311,#20099,.T.);
#47722=EDGE_CURVE('',#37419,#37310,#20100,.T.);
#47723=EDGE_CURVE('',#37419,#37420,#20101,.T.);
#47724=EDGE_CURVE('',#37420,#37308,#20102,.T.);
#47725=EDGE_CURVE('',#37421,#37309,#20103,.T.);
#47726=EDGE_CURVE('',#37421,#37422,#20104,.T.);
#47727=EDGE_CURVE('',#37422,#37312,#20105,.T.);
#47728=EDGE_CURVE('',#37423,#37313,#20106,.T.);
#47729=EDGE_CURVE('',#37423,#37424,#20107,.T.);
#47730=EDGE_CURVE('',#37424,#37321,#20108,.T.);
#47731=EDGE_CURVE('',#37425,#37320,#20109,.T.);
#47732=EDGE_CURVE('',#37425,#37426,#20110,.T.);
#47733=EDGE_CURVE('',#37426,#37318,#20111,.T.);
#47734=EDGE_CURVE('',#37427,#37319,#20112,.T.);
#47735=EDGE_CURVE('',#37427,#37428,#20113,.T.);
#47736=EDGE_CURVE('',#37428,#37322,#20114,.T.);
#47737=EDGE_CURVE('',#37429,#37323,#20115,.T.);
#47738=EDGE_CURVE('',#37429,#37430,#20116,.T.);
#47739=EDGE_CURVE('',#37430,#37295,#20117,.T.);
#47740=EDGE_CURVE('',#37431,#37294,#20118,.T.);
#47741=EDGE_CURVE('',#37431,#37360,#20119,.T.);
#47742=EDGE_CURVE('',#37252,#37375,#28395,.T.);
#47743=EDGE_CURVE('',#37376,#37251,#28396,.T.);
#47744=EDGE_CURVE('',#37249,#37378,#28397,.T.);
#47745=EDGE_CURVE('',#37250,#37377,#28398,.T.);
#47746=EDGE_CURVE('',#37253,#37374,#28399,.T.);
#47747=EDGE_CURVE('',#37254,#37373,#28400,.T.);
#47748=EDGE_CURVE('',#37213,#37396,#28401,.T.);
#47749=EDGE_CURVE('',#37214,#37395,#28402,.T.);
#47750=EDGE_CURVE('',#37217,#37394,#28403,.T.);
#47751=EDGE_CURVE('',#37218,#37393,#28404,.T.);
#47752=EDGE_CURVE('',#37221,#37392,#28405,.T.);
#47753=EDGE_CURVE('',#37222,#37391,#28406,.T.);
#47754=EDGE_CURVE('',#37225,#37390,#28407,.T.);
#47755=EDGE_CURVE('',#37226,#37389,#28408,.T.);
#47756=EDGE_CURVE('',#37245,#37380,#28409,.T.);
#47757=EDGE_CURVE('',#37246,#37379,#28410,.T.);
#47758=EDGE_CURVE('',#37241,#37382,#28411,.T.);
#47759=EDGE_CURVE('',#37242,#37381,#28412,.T.);
#47760=EDGE_CURVE('',#37237,#37384,#28413,.T.);
#47761=EDGE_CURVE('',#37238,#37383,#28414,.T.);
#47762=EDGE_CURVE('',#37229,#37388,#28415,.T.);
#47763=EDGE_CURVE('',#37230,#37387,#28416,.T.);
#47764=EDGE_CURVE('',#37233,#37386,#28417,.T.);
#47765=EDGE_CURVE('',#37234,#37385,#28418,.T.);
#47766=EDGE_CURVE('',#37177,#37414,#28419,.T.);
#47767=EDGE_CURVE('',#37178,#37413,#28420,.T.);
#47768=EDGE_CURVE('',#37181,#37412,#28421,.T.);
#47769=EDGE_CURVE('',#37182,#37411,#28422,.T.);
#47770=EDGE_CURVE('',#37189,#37408,#28423,.T.);
#47771=EDGE_CURVE('',#37190,#37407,#28424,.T.);
#47772=EDGE_CURVE('',#37185,#37410,#28425,.T.);
#47773=EDGE_CURVE('',#37186,#37409,#28426,.T.);
#47774=EDGE_CURVE('',#37209,#37398,#28427,.T.);
#47775=EDGE_CURVE('',#37210,#37397,#28428,.T.);
#47776=EDGE_CURVE('',#37205,#37400,#28429,.T.);
#47777=EDGE_CURVE('',#37206,#37399,#28430,.T.);
#47778=EDGE_CURVE('',#37201,#37402,#28431,.T.);
#47779=EDGE_CURVE('',#37202,#37401,#28432,.T.);
#47780=EDGE_CURVE('',#37193,#37406,#28433,.T.);
#47781=EDGE_CURVE('',#37194,#37405,#28434,.T.);
#47782=EDGE_CURVE('',#37197,#37404,#28435,.T.);
#47783=EDGE_CURVE('',#37198,#37403,#28436,.T.);
#47784=EDGE_CURVE('',#37145,#37430,#28437,.T.);
#47785=EDGE_CURVE('',#37146,#37429,#28438,.T.);
#47786=EDGE_CURVE('',#37149,#37428,#28439,.T.);
#47787=EDGE_CURVE('',#37150,#37427,#28440,.T.);
#47788=EDGE_CURVE('',#37157,#37424,#28441,.T.);
#47789=EDGE_CURVE('',#37158,#37423,#28442,.T.);
#47790=EDGE_CURVE('',#37153,#37426,#28443,.T.);
#47791=EDGE_CURVE('',#37154,#37425,#28444,.T.);
#47792=EDGE_CURVE('',#37173,#37416,#28445,.T.);
#47793=EDGE_CURVE('',#37174,#37415,#28446,.T.);
#47794=EDGE_CURVE('',#37171,#37417,#28447,.T.);
#47795=EDGE_CURVE('',#37169,#37418,#28448,.T.);
#47796=EDGE_CURVE('',#37161,#37422,#28449,.T.);
#47797=EDGE_CURVE('',#37162,#37421,#28450,.T.);
#47798=EDGE_CURVE('',#37165,#37420,#28451,.T.);
#47799=EDGE_CURVE('',#37166,#37419,#28452,.T.);
#47800=EDGE_CURVE('',#37261,#37370,#28453,.T.);
#47801=EDGE_CURVE('',#37262,#37369,#28454,.T.);
#47802=EDGE_CURVE('',#37265,#37368,#28455,.T.);
#47803=EDGE_CURVE('',#37266,#37367,#28456,.T.);
#47804=EDGE_CURVE('',#37258,#37371,#28457,.T.);
#47805=EDGE_CURVE('',#37256,#37372,#28458,.T.);
#47806=EDGE_CURVE('',#37269,#37366,#28459,.T.);
#47807=EDGE_CURVE('',#37270,#37365,#28460,.T.);
#47808=EDGE_CURVE('',#37273,#37364,#28461,.T.);
#47809=EDGE_CURVE('',#37274,#37363,#28462,.T.);
#47810=EDGE_CURVE('',#37277,#37362,#28463,.T.);
#47811=EDGE_CURVE('',#37278,#37361,#28464,.T.);
#47812=EDGE_CURVE('',#37140,#37360,#28465,.T.);
#47813=EDGE_CURVE('',#37142,#37431,#28466,.T.);
#47814=EDGE_CURVE('',#37432,#37433,#28467,.T.);
#47815=EDGE_CURVE('',#37433,#37118,#28468,.T.);
#47816=EDGE_CURVE('',#37121,#37432,#28469,.T.);
#47817=EDGE_CURVE('',#37434,#37435,#28470,.T.);
#47818=EDGE_CURVE('',#37435,#37433,#20120,.T.);
#47819=EDGE_CURVE('',#37432,#37434,#20121,.T.);
#47820=EDGE_CURVE('',#37436,#37437,#28471,.T.);
#47821=EDGE_CURVE('',#37437,#37435,#20122,.T.);
#47822=EDGE_CURVE('',#37434,#37436,#20123,.T.);
#47823=EDGE_CURVE('',#37438,#37439,#28472,.T.);
#47824=EDGE_CURVE('',#37439,#37437,#20124,.T.);
#47825=EDGE_CURVE('',#37436,#37438,#20125,.T.);
#47826=EDGE_CURVE('',#37440,#37102,#28473,.T.);
#47827=EDGE_CURVE('',#37102,#37439,#28474,.T.);
#47828=EDGE_CURVE('',#37438,#37440,#28475,.T.);
#47829=EDGE_CURVE('',#37441,#37101,#28476,.T.);
#47830=EDGE_CURVE('',#37440,#37441,#20126,.T.);
#47831=EDGE_CURVE('',#37119,#37101,#20127,.T.);
#47832=EDGE_CURVE('',#37441,#37120,#20128,.T.);
#47833=EDGE_CURVE('',#37442,#37443,#28477,.T.);
#47834=EDGE_CURVE('',#37443,#37444,#20129,.T.);
#47835=EDGE_CURVE('',#37445,#37444,#28478,.T.);
#47836=EDGE_CURVE('',#37445,#37442,#20130,.T.);
#47837=EDGE_CURVE('',#37115,#37443,#28479,.T.);
#47838=EDGE_CURVE('',#37442,#37116,#28480,.T.);
#47839=EDGE_CURVE('',#37446,#37098,#28481,.T.);
#47840=EDGE_CURVE('',#37098,#37114,#20131,.T.);
#47841=EDGE_CURVE('',#37117,#37446,#20132,.T.);
#47842=EDGE_CURVE('',#37447,#37097,#28482,.T.);
#47843=EDGE_CURVE('',#37446,#37447,#20133,.T.);
#47844=EDGE_CURVE('',#37448,#37449,#28483,.T.);
#47845=EDGE_CURVE('',#37449,#37097,#28484,.T.);
#47846=EDGE_CURVE('',#37447,#37448,#28485,.T.);
#47847=EDGE_CURVE('',#37450,#37451,#28486,.T.);
#47848=EDGE_CURVE('',#37451,#37449,#20134,.T.);
#47849=EDGE_CURVE('',#37448,#37450,#20135,.T.);
#47850=EDGE_CURVE('',#37444,#37451,#20136,.T.);
#47851=EDGE_CURVE('',#37450,#37445,#20137,.T.);
#47852=EDGE_CURVE('',#37119,#37283,#20138,.T.);
#47853=EDGE_CURVE('',#37284,#37118,#20139,.T.);
#47854=EDGE_CURVE('',#37285,#37433,#20140,.T.);
#47855=EDGE_CURVE('',#37280,#37435,#20141,.T.);
#47856=EDGE_CURVE('',#37281,#37437,#20142,.T.);
#47857=EDGE_CURVE('',#37439,#37282,#20143,.T.);
#47858=EDGE_CURVE('',#37449,#37289,#20144,.T.);
#47859=EDGE_CURVE('',#37290,#37451,#20145,.T.);
#47860=EDGE_CURVE('',#37291,#37444,#20146,.T.);
#47861=EDGE_CURVE('',#37286,#37443,#20147,.T.);
#47862=EDGE_CURVE('',#37287,#37115,#20148,.T.);
#47863=EDGE_CURVE('',#37114,#37288,#20149,.T.);
#47864=EDGE_CURVE('',#37452,#37453,#20150,.T.);
#47865=EDGE_CURVE('',#37453,#37454,#28487,.T.);
#47866=EDGE_CURVE('',#37455,#37454,#20151,.T.);
#47867=EDGE_CURVE('',#37452,#37455,#28488,.T.);
#47868=EDGE_CURVE('',#37456,#37457,#28489,.T.);
#47869=EDGE_CURVE('',#37456,#37452,#24319,.T.);
#47870=EDGE_CURVE('',#37457,#37455,#24320,.T.);
#47871=EDGE_CURVE('',#37458,#37459,#28490,.T.);
#47872=EDGE_CURVE('',#37454,#37458,#24321,.T.);
#47873=EDGE_CURVE('',#37459,#37453,#24322,.T.);
#47874=EDGE_CURVE('',#37460,#37461,#28491,.T.);
#47875=EDGE_CURVE('',#37458,#37461,#20152,.T.);
#47876=EDGE_CURVE('',#37459,#37460,#20153,.T.);
#47877=EDGE_CURVE('',#37462,#37463,#20154,.T.);
#47878=EDGE_CURVE('',#37463,#37464,#28492,.T.);
#47879=EDGE_CURVE('',#37465,#37464,#20155,.T.);
#47880=EDGE_CURVE('',#37462,#37465,#28493,.T.);
#47881=EDGE_CURVE('',#37466,#37467,#28494,.T.);
#47882=EDGE_CURVE('',#37464,#37466,#24323,.T.);
#47883=EDGE_CURVE('',#37467,#37463,#24324,.T.);
#47884=EDGE_CURVE('',#37460,#37462,#24325,.T.);
#47885=EDGE_CURVE('',#37461,#37465,#24326,.T.);
#47886=EDGE_CURVE('',#37468,#37469,#28495,.T.);
#47887=EDGE_CURVE('',#37466,#37469,#20156,.T.);
#47888=EDGE_CURVE('',#37467,#37468,#20157,.T.);
#47889=EDGE_CURVE('',#37470,#37471,#20158,.T.);
#47890=EDGE_CURVE('',#37471,#37472,#28496,.T.);
#47891=EDGE_CURVE('',#37473,#37472,#20159,.T.);
#47892=EDGE_CURVE('',#37470,#37473,#28497,.T.);
#47893=EDGE_CURVE('',#37468,#37470,#24327,.T.);
#47894=EDGE_CURVE('',#37469,#37473,#24328,.T.);
#47895=EDGE_CURVE('',#37474,#37475,#28498,.T.);
#47896=EDGE_CURVE('',#37472,#37474,#24329,.T.);
#47897=EDGE_CURVE('',#37475,#37471,#24330,.T.);
#47898=EDGE_CURVE('',#37476,#37477,#28499,.T.);
#47899=EDGE_CURVE('',#37474,#37477,#20160,.T.);
#47900=EDGE_CURVE('',#37475,#37476,#20161,.T.);
#47901=EDGE_CURVE('',#37478,#37479,#20162,.T.);
#47902=EDGE_CURVE('',#37479,#37480,#28500,.T.);
#47903=EDGE_CURVE('',#37481,#37480,#20163,.T.);
#47904=EDGE_CURVE('',#37478,#37481,#28501,.T.);
#47905=EDGE_CURVE('',#37482,#37483,#28502,.T.);
#47906=EDGE_CURVE('',#37480,#37482,#24331,.T.);
#47907=EDGE_CURVE('',#37483,#37479,#24332,.T.);
#47908=EDGE_CURVE('',#37476,#37478,#24333,.T.);
#47909=EDGE_CURVE('',#37477,#37481,#24334,.T.);
#47910=EDGE_CURVE('',#37484,#37485,#28503,.T.);
#47911=EDGE_CURVE('',#37482,#37485,#20164,.T.);
#47912=EDGE_CURVE('',#37483,#37484,#20165,.T.);
#47913=EDGE_CURVE('',#37486,#37487,#20166,.T.);
#47914=EDGE_CURVE('',#37487,#37488,#28504,.T.);
#47915=EDGE_CURVE('',#37489,#37488,#20167,.T.);
#47916=EDGE_CURVE('',#37486,#37489,#28505,.T.);
#47917=EDGE_CURVE('',#37484,#37486,#24335,.T.);
#47918=EDGE_CURVE('',#37485,#37489,#24336,.T.);
#47919=EDGE_CURVE('',#37490,#37491,#28506,.T.);
#47920=EDGE_CURVE('',#37488,#37490,#24337,.T.);
#47921=EDGE_CURVE('',#37491,#37487,#24338,.T.);
#47922=EDGE_CURVE('',#37492,#37493,#28507,.T.);
#47923=EDGE_CURVE('',#37490,#37493,#20168,.T.);
#47924=EDGE_CURVE('',#37491,#37492,#20169,.T.);
#47925=EDGE_CURVE('',#37494,#37495,#20170,.T.);
#47926=EDGE_CURVE('',#37495,#37496,#28508,.T.);
#47927=EDGE_CURVE('',#37497,#37496,#20171,.T.);
#47928=EDGE_CURVE('',#37494,#37497,#28509,.T.);
#47929=EDGE_CURVE('',#37498,#37499,#28510,.T.);
#47930=EDGE_CURVE('',#37496,#37498,#24339,.T.);
#47931=EDGE_CURVE('',#37499,#37495,#24340,.T.);
#47932=EDGE_CURVE('',#37492,#37494,#24341,.T.);
#47933=EDGE_CURVE('',#37493,#37497,#24342,.T.);
#47934=EDGE_CURVE('',#37500,#37501,#28511,.T.);
#47935=EDGE_CURVE('',#37498,#37501,#20172,.T.);
#47936=EDGE_CURVE('',#37499,#37500,#20173,.T.);
#47937=EDGE_CURVE('',#37502,#37503,#20174,.T.);
#47938=EDGE_CURVE('',#37503,#37504,#28512,.T.);
#47939=EDGE_CURVE('',#37505,#37504,#20175,.T.);
#47940=EDGE_CURVE('',#37502,#37505,#28513,.T.);
#47941=EDGE_CURVE('',#37500,#37502,#24343,.T.);
#47942=EDGE_CURVE('',#37501,#37505,#24344,.T.);
#47943=EDGE_CURVE('',#37506,#37507,#28514,.T.);
#47944=EDGE_CURVE('',#37504,#37506,#24345,.T.);
#47945=EDGE_CURVE('',#37507,#37503,#24346,.T.);
#47946=EDGE_CURVE('',#37508,#37509,#28515,.T.);
#47947=EDGE_CURVE('',#37506,#37509,#20176,.T.);
#47948=EDGE_CURVE('',#37507,#37508,#20177,.T.);
#47949=EDGE_CURVE('',#37510,#37511,#20178,.T.);
#47950=EDGE_CURVE('',#37511,#37512,#28516,.T.);
#47951=EDGE_CURVE('',#37513,#37512,#20179,.T.);
#47952=EDGE_CURVE('',#37510,#37513,#28517,.T.);
#47953=EDGE_CURVE('',#37514,#37515,#28518,.T.);
#47954=EDGE_CURVE('',#37512,#37514,#24347,.T.);
#47955=EDGE_CURVE('',#37515,#37511,#24348,.T.);
#47956=EDGE_CURVE('',#37508,#37510,#24349,.T.);
#47957=EDGE_CURVE('',#37509,#37513,#24350,.T.);
#47958=EDGE_CURVE('',#37516,#37517,#28519,.T.);
#47959=EDGE_CURVE('',#37514,#37517,#20180,.T.);
#47960=EDGE_CURVE('',#37515,#37516,#20181,.T.);
#47961=EDGE_CURVE('',#37518,#37519,#20182,.T.);
#47962=EDGE_CURVE('',#37519,#37520,#28520,.T.);
#47963=EDGE_CURVE('',#37521,#37520,#20183,.T.);
#47964=EDGE_CURVE('',#37518,#37521,#28521,.T.);
#47965=EDGE_CURVE('',#37516,#37518,#24351,.T.);
#47966=EDGE_CURVE('',#37517,#37521,#24352,.T.);
#47967=EDGE_CURVE('',#37522,#37523,#28522,.T.);
#47968=EDGE_CURVE('',#37520,#37522,#24353,.T.);
#47969=EDGE_CURVE('',#37523,#37519,#24354,.T.);
#47970=EDGE_CURVE('',#37524,#37525,#28523,.T.);
#47971=EDGE_CURVE('',#37522,#37525,#20184,.T.);
#47972=EDGE_CURVE('',#37523,#37524,#20185,.T.);
#47973=EDGE_CURVE('',#37526,#37527,#20186,.T.);
#47974=EDGE_CURVE('',#37527,#37528,#28524,.T.);
#47975=EDGE_CURVE('',#37529,#37528,#20187,.T.);
#47976=EDGE_CURVE('',#37526,#37529,#28525,.T.);
#47977=EDGE_CURVE('',#37530,#37531,#28526,.T.);
#47978=EDGE_CURVE('',#37528,#37530,#24355,.T.);
#47979=EDGE_CURVE('',#37531,#37527,#24356,.T.);
#47980=EDGE_CURVE('',#37524,#37526,#24357,.T.);
#47981=EDGE_CURVE('',#37525,#37529,#24358,.T.);
#47982=EDGE_CURVE('',#37532,#37533,#28527,.T.);
#47983=EDGE_CURVE('',#37530,#37533,#20188,.T.);
#47984=EDGE_CURVE('',#37531,#37532,#20189,.T.);
#47985=EDGE_CURVE('',#37534,#37535,#20190,.T.);
#47986=EDGE_CURVE('',#37535,#37536,#28528,.T.);
#47987=EDGE_CURVE('',#37537,#37536,#20191,.T.);
#47988=EDGE_CURVE('',#37534,#37537,#28529,.T.);
#47989=EDGE_CURVE('',#37532,#37534,#24359,.T.);
#47990=EDGE_CURVE('',#37533,#37537,#24360,.T.);
#47991=EDGE_CURVE('',#37538,#37539,#28530,.T.);
#47992=EDGE_CURVE('',#37536,#37538,#24361,.T.);
#47993=EDGE_CURVE('',#37539,#37535,#24362,.T.);
#47994=EDGE_CURVE('',#37540,#37541,#28531,.T.);
#47995=EDGE_CURVE('',#37538,#37541,#20192,.T.);
#47996=EDGE_CURVE('',#37539,#37540,#20193,.T.);
#47997=EDGE_CURVE('',#37542,#37543,#20194,.T.);
#47998=EDGE_CURVE('',#37543,#37544,#28532,.T.);
#47999=EDGE_CURVE('',#37545,#37544,#20195,.T.);
#48000=EDGE_CURVE('',#37542,#37545,#28533,.T.);
#48001=EDGE_CURVE('',#37546,#37547,#28534,.T.);
#48002=EDGE_CURVE('',#37544,#37546,#24363,.T.);
#48003=EDGE_CURVE('',#37547,#37543,#24364,.T.);
#48004=EDGE_CURVE('',#37540,#37542,#24365,.T.);
#48005=EDGE_CURVE('',#37541,#37545,#24366,.T.);
#48006=EDGE_CURVE('',#37548,#37549,#28535,.T.);
#48007=EDGE_CURVE('',#37546,#37549,#20196,.T.);
#48008=EDGE_CURVE('',#37547,#37548,#20197,.T.);
#48009=EDGE_CURVE('',#37550,#37551,#20198,.T.);
#48010=EDGE_CURVE('',#37551,#37552,#28536,.T.);
#48011=EDGE_CURVE('',#37553,#37552,#20199,.T.);
#48012=EDGE_CURVE('',#37550,#37553,#28537,.T.);
#48013=EDGE_CURVE('',#37548,#37550,#24367,.T.);
#48014=EDGE_CURVE('',#37549,#37553,#24368,.T.);
#48015=EDGE_CURVE('',#37554,#37555,#28538,.T.);
#48016=EDGE_CURVE('',#37552,#37554,#24369,.T.);
#48017=EDGE_CURVE('',#37555,#37551,#24370,.T.);
#48018=EDGE_CURVE('',#37556,#37557,#28539,.T.);
#48019=EDGE_CURVE('',#37554,#37557,#20200,.T.);
#48020=EDGE_CURVE('',#37555,#37556,#20201,.T.);
#48021=EDGE_CURVE('',#37558,#37559,#20202,.T.);
#48022=EDGE_CURVE('',#37559,#37560,#28540,.T.);
#48023=EDGE_CURVE('',#37561,#37560,#20203,.T.);
#48024=EDGE_CURVE('',#37558,#37561,#28541,.T.);
#48025=EDGE_CURVE('',#37562,#37563,#28542,.T.);
#48026=EDGE_CURVE('',#37560,#37562,#24371,.T.);
#48027=EDGE_CURVE('',#37563,#37559,#24372,.T.);
#48028=EDGE_CURVE('',#37556,#37558,#24373,.T.);
#48029=EDGE_CURVE('',#37557,#37561,#24374,.T.);
#48030=EDGE_CURVE('',#37564,#37565,#28543,.T.);
#48031=EDGE_CURVE('',#37562,#37565,#20204,.T.);
#48032=EDGE_CURVE('',#37563,#37564,#20205,.T.);
#48033=EDGE_CURVE('',#37566,#37567,#20206,.T.);
#48034=EDGE_CURVE('',#37567,#37568,#28544,.T.);
#48035=EDGE_CURVE('',#37569,#37568,#20207,.T.);
#48036=EDGE_CURVE('',#37566,#37569,#28545,.T.);
#48037=EDGE_CURVE('',#37564,#37566,#24375,.T.);
#48038=EDGE_CURVE('',#37565,#37569,#24376,.T.);
#48039=EDGE_CURVE('',#37570,#37571,#28546,.T.);
#48040=EDGE_CURVE('',#37568,#37570,#24377,.T.);
#48041=EDGE_CURVE('',#37571,#37567,#24378,.T.);
#48042=EDGE_CURVE('',#37572,#37573,#28547,.T.);
#48043=EDGE_CURVE('',#37570,#37573,#20208,.T.);
#48044=EDGE_CURVE('',#37571,#37572,#20209,.T.);
#48045=EDGE_CURVE('',#37574,#37575,#20210,.T.);
#48046=EDGE_CURVE('',#37575,#37576,#28548,.T.);
#48047=EDGE_CURVE('',#37577,#37576,#20211,.T.);
#48048=EDGE_CURVE('',#37574,#37577,#28549,.T.);
#48049=EDGE_CURVE('',#37578,#37579,#28550,.T.);
#48050=EDGE_CURVE('',#37576,#37578,#24379,.T.);
#48051=EDGE_CURVE('',#37579,#37575,#24380,.T.);
#48052=EDGE_CURVE('',#37572,#37574,#24381,.T.);
#48053=EDGE_CURVE('',#37573,#37577,#24382,.T.);
#48054=EDGE_CURVE('',#37580,#37581,#28551,.T.);
#48055=EDGE_CURVE('',#37578,#37581,#20212,.T.);
#48056=EDGE_CURVE('',#37579,#37580,#20213,.T.);
#48057=EDGE_CURVE('',#37582,#37583,#20214,.T.);
#48058=EDGE_CURVE('',#37583,#37584,#28552,.T.);
#48059=EDGE_CURVE('',#37585,#37584,#20215,.T.);
#48060=EDGE_CURVE('',#37582,#37585,#28553,.T.);
#48061=EDGE_CURVE('',#37580,#37582,#24383,.T.);
#48062=EDGE_CURVE('',#37581,#37585,#24384,.T.);
#48063=EDGE_CURVE('',#37586,#37587,#28554,.T.);
#48064=EDGE_CURVE('',#37584,#37586,#24385,.T.);
#48065=EDGE_CURVE('',#37587,#37583,#24386,.T.);
#48066=EDGE_CURVE('',#37588,#37589,#28555,.T.);
#48067=EDGE_CURVE('',#37586,#37589,#20216,.T.);
#48068=EDGE_CURVE('',#37587,#37588,#20217,.T.);
#48069=EDGE_CURVE('',#37590,#37591,#20218,.T.);
#48070=EDGE_CURVE('',#37591,#37592,#28556,.T.);
#48071=EDGE_CURVE('',#37593,#37592,#20219,.T.);
#48072=EDGE_CURVE('',#37590,#37593,#28557,.T.);
#48073=EDGE_CURVE('',#37594,#37595,#28558,.T.);
#48074=EDGE_CURVE('',#37592,#37594,#24387,.T.);
#48075=EDGE_CURVE('',#37595,#37591,#24388,.T.);
#48076=EDGE_CURVE('',#37588,#37590,#24389,.T.);
#48077=EDGE_CURVE('',#37589,#37593,#24390,.T.);
#48078=EDGE_CURVE('',#37596,#37597,#28559,.T.);
#48079=EDGE_CURVE('',#37594,#37597,#20220,.T.);
#48080=EDGE_CURVE('',#37595,#37596,#20221,.T.);
#48081=EDGE_CURVE('',#37598,#37599,#20222,.T.);
#48082=EDGE_CURVE('',#37599,#37600,#28560,.T.);
#48083=EDGE_CURVE('',#37601,#37600,#20223,.T.);
#48084=EDGE_CURVE('',#37598,#37601,#28561,.T.);
#48085=EDGE_CURVE('',#37596,#37598,#24391,.T.);
#48086=EDGE_CURVE('',#37597,#37601,#24392,.T.);
#48087=EDGE_CURVE('',#37602,#37603,#28562,.T.);
#48088=EDGE_CURVE('',#37600,#37602,#24393,.T.);
#48089=EDGE_CURVE('',#37603,#37599,#24394,.T.);
#48090=EDGE_CURVE('',#37604,#37605,#28563,.T.);
#48091=EDGE_CURVE('',#37602,#37605,#20224,.T.);
#48092=EDGE_CURVE('',#37603,#37604,#20225,.T.);
#48093=EDGE_CURVE('',#37606,#37607,#20226,.T.);
#48094=EDGE_CURVE('',#37607,#37608,#28564,.T.);
#48095=EDGE_CURVE('',#37609,#37608,#20227,.T.);
#48096=EDGE_CURVE('',#37606,#37609,#28565,.T.);
#48097=EDGE_CURVE('',#37610,#37611,#28566,.T.);
#48098=EDGE_CURVE('',#37608,#37610,#24395,.T.);
#48099=EDGE_CURVE('',#37611,#37607,#24396,.T.);
#48100=EDGE_CURVE('',#37604,#37606,#24397,.T.);
#48101=EDGE_CURVE('',#37605,#37609,#24398,.T.);
#48102=EDGE_CURVE('',#37612,#37613,#28567,.T.);
#48103=EDGE_CURVE('',#37610,#37613,#20228,.T.);
#48104=EDGE_CURVE('',#37611,#37612,#20229,.T.);
#48105=EDGE_CURVE('',#37614,#37615,#20230,.T.);
#48106=EDGE_CURVE('',#37615,#37616,#28568,.T.);
#48107=EDGE_CURVE('',#37617,#37616,#20231,.T.);
#48108=EDGE_CURVE('',#37614,#37617,#28569,.T.);
#48109=EDGE_CURVE('',#37612,#37614,#24399,.T.);
#48110=EDGE_CURVE('',#37613,#37617,#24400,.T.);
#48111=EDGE_CURVE('',#37618,#37619,#28570,.T.);
#48112=EDGE_CURVE('',#37616,#37618,#24401,.T.);
#48113=EDGE_CURVE('',#37619,#37615,#24402,.T.);
#48114=EDGE_CURVE('',#37620,#37621,#28571,.T.);
#48115=EDGE_CURVE('',#37618,#37621,#20232,.T.);
#48116=EDGE_CURVE('',#37619,#37620,#20233,.T.);
#48117=EDGE_CURVE('',#37622,#37623,#20234,.T.);
#48118=EDGE_CURVE('',#37623,#37624,#28572,.T.);
#48119=EDGE_CURVE('',#37625,#37624,#20235,.T.);
#48120=EDGE_CURVE('',#37622,#37625,#28573,.T.);
#48121=EDGE_CURVE('',#37626,#37627,#28574,.T.);
#48122=EDGE_CURVE('',#37624,#37626,#24403,.T.);
#48123=EDGE_CURVE('',#37627,#37623,#24404,.T.);
#48124=EDGE_CURVE('',#37620,#37622,#24405,.T.);
#48125=EDGE_CURVE('',#37621,#37625,#24406,.T.);
#48126=EDGE_CURVE('',#37628,#37629,#28575,.T.);
#48127=EDGE_CURVE('',#37626,#37629,#20236,.T.);
#48128=EDGE_CURVE('',#37627,#37628,#20237,.T.);
#48129=EDGE_CURVE('',#37630,#37631,#20238,.T.);
#48130=EDGE_CURVE('',#37631,#37632,#28576,.T.);
#48131=EDGE_CURVE('',#37633,#37632,#20239,.T.);
#48132=EDGE_CURVE('',#37630,#37633,#28577,.T.);
#48133=EDGE_CURVE('',#37628,#37630,#24407,.T.);
#48134=EDGE_CURVE('',#37629,#37633,#24408,.T.);
#48135=EDGE_CURVE('',#37634,#37635,#28578,.T.);
#48136=EDGE_CURVE('',#37632,#37634,#24409,.T.);
#48137=EDGE_CURVE('',#37635,#37631,#24410,.T.);
#48138=EDGE_CURVE('',#37636,#37637,#28579,.T.);
#48139=EDGE_CURVE('',#37634,#37637,#20240,.T.);
#48140=EDGE_CURVE('',#37635,#37636,#20241,.T.);
#48141=EDGE_CURVE('',#37638,#37639,#20242,.T.);
#48142=EDGE_CURVE('',#37639,#37640,#28580,.T.);
#48143=EDGE_CURVE('',#37641,#37640,#20243,.T.);
#48144=EDGE_CURVE('',#37638,#37641,#28581,.T.);
#48145=EDGE_CURVE('',#37642,#37643,#28582,.T.);
#48146=EDGE_CURVE('',#37640,#37642,#24411,.T.);
#48147=EDGE_CURVE('',#37643,#37639,#24412,.T.);
#48148=EDGE_CURVE('',#37636,#37638,#24413,.T.);
#48149=EDGE_CURVE('',#37637,#37641,#24414,.T.);
#48150=EDGE_CURVE('',#37644,#37645,#28583,.T.);
#48151=EDGE_CURVE('',#37642,#37645,#20244,.T.);
#48152=EDGE_CURVE('',#37643,#37644,#20245,.T.);
#48153=EDGE_CURVE('',#37646,#37647,#20246,.T.);
#48154=EDGE_CURVE('',#37647,#37648,#28584,.T.);
#48155=EDGE_CURVE('',#37649,#37648,#20247,.T.);
#48156=EDGE_CURVE('',#37646,#37649,#28585,.T.);
#48157=EDGE_CURVE('',#37644,#37646,#24415,.T.);
#48158=EDGE_CURVE('',#37645,#37649,#24416,.T.);
#48159=EDGE_CURVE('',#37650,#37651,#28586,.T.);
#48160=EDGE_CURVE('',#37648,#37650,#24417,.T.);
#48161=EDGE_CURVE('',#37651,#37647,#24418,.T.);
#48162=EDGE_CURVE('',#37652,#37653,#28587,.T.);
#48163=EDGE_CURVE('',#37650,#37653,#20248,.T.);
#48164=EDGE_CURVE('',#37651,#37652,#20249,.T.);
#48165=EDGE_CURVE('',#37654,#37655,#20250,.T.);
#48166=EDGE_CURVE('',#37655,#37656,#28588,.T.);
#48167=EDGE_CURVE('',#37657,#37656,#20251,.T.);
#48168=EDGE_CURVE('',#37654,#37657,#28589,.T.);
#48169=EDGE_CURVE('',#37658,#37659,#28590,.T.);
#48170=EDGE_CURVE('',#37656,#37658,#24419,.T.);
#48171=EDGE_CURVE('',#37659,#37655,#24420,.T.);
#48172=EDGE_CURVE('',#37652,#37654,#24421,.T.);
#48173=EDGE_CURVE('',#37653,#37657,#24422,.T.);
#48174=EDGE_CURVE('',#37660,#37661,#28591,.T.);
#48175=EDGE_CURVE('',#37658,#37661,#20252,.T.);
#48176=EDGE_CURVE('',#37659,#37660,#20253,.T.);
#48177=EDGE_CURVE('',#37662,#37663,#20254,.T.);
#48178=EDGE_CURVE('',#37663,#37664,#28592,.T.);
#48179=EDGE_CURVE('',#37665,#37664,#20255,.T.);
#48180=EDGE_CURVE('',#37662,#37665,#28593,.T.);
#48181=EDGE_CURVE('',#37660,#37662,#24423,.T.);
#48182=EDGE_CURVE('',#37661,#37665,#24424,.T.);
#48183=EDGE_CURVE('',#37666,#37667,#28594,.T.);
#48184=EDGE_CURVE('',#37664,#37666,#24425,.T.);
#48185=EDGE_CURVE('',#37667,#37663,#24426,.T.);
#48186=EDGE_CURVE('',#37668,#37669,#28595,.T.);
#48187=EDGE_CURVE('',#37666,#37669,#20256,.T.);
#48188=EDGE_CURVE('',#37667,#37668,#20257,.T.);
#48189=EDGE_CURVE('',#37670,#37671,#20258,.T.);
#48190=EDGE_CURVE('',#37671,#37672,#28596,.T.);
#48191=EDGE_CURVE('',#37673,#37672,#20259,.T.);
#48192=EDGE_CURVE('',#37670,#37673,#28597,.T.);
#48193=EDGE_CURVE('',#37674,#37675,#28598,.T.);
#48194=EDGE_CURVE('',#37672,#37674,#24427,.T.);
#48195=EDGE_CURVE('',#37675,#37671,#24428,.T.);
#48196=EDGE_CURVE('',#37668,#37670,#24429,.T.);
#48197=EDGE_CURVE('',#37669,#37673,#24430,.T.);
#48198=EDGE_CURVE('',#37676,#37677,#28599,.T.);
#48199=EDGE_CURVE('',#37674,#37677,#20260,.T.);
#48200=EDGE_CURVE('',#37675,#37676,#20261,.T.);
#48201=EDGE_CURVE('',#37678,#37679,#20262,.T.);
#48202=EDGE_CURVE('',#37679,#37680,#28600,.T.);
#48203=EDGE_CURVE('',#37681,#37680,#20263,.T.);
#48204=EDGE_CURVE('',#37678,#37681,#28601,.T.);
#48205=EDGE_CURVE('',#37676,#37678,#24431,.T.);
#48206=EDGE_CURVE('',#37677,#37681,#24432,.T.);
#48207=EDGE_CURVE('',#37682,#37683,#28602,.T.);
#48208=EDGE_CURVE('',#37680,#37682,#24433,.T.);
#48209=EDGE_CURVE('',#37683,#37679,#24434,.T.);
#48210=EDGE_CURVE('',#37684,#37685,#28603,.T.);
#48211=EDGE_CURVE('',#37682,#37685,#20264,.T.);
#48212=EDGE_CURVE('',#37683,#37684,#20265,.T.);
#48213=EDGE_CURVE('',#37686,#37687,#20266,.T.);
#48214=EDGE_CURVE('',#37687,#37688,#28604,.T.);
#48215=EDGE_CURVE('',#37689,#37688,#20267,.T.);
#48216=EDGE_CURVE('',#37686,#37689,#28605,.T.);
#48217=EDGE_CURVE('',#37690,#37691,#28606,.T.);
#48218=EDGE_CURVE('',#37688,#37690,#24435,.T.);
#48219=EDGE_CURVE('',#37691,#37687,#24436,.T.);
#48220=EDGE_CURVE('',#37684,#37686,#24437,.T.);
#48221=EDGE_CURVE('',#37685,#37689,#24438,.T.);
#48222=EDGE_CURVE('',#37692,#37693,#28607,.T.);
#48223=EDGE_CURVE('',#37690,#37693,#20268,.T.);
#48224=EDGE_CURVE('',#37691,#37692,#20269,.T.);
#48225=EDGE_CURVE('',#37694,#37695,#20270,.T.);
#48226=EDGE_CURVE('',#37695,#37696,#28608,.T.);
#48227=EDGE_CURVE('',#37697,#37696,#20271,.T.);
#48228=EDGE_CURVE('',#37694,#37697,#28609,.T.);
#48229=EDGE_CURVE('',#37692,#37694,#24439,.T.);
#48230=EDGE_CURVE('',#37693,#37697,#24440,.T.);
#48231=EDGE_CURVE('',#37698,#37699,#28610,.T.);
#48232=EDGE_CURVE('',#37696,#37698,#24441,.T.);
#48233=EDGE_CURVE('',#37699,#37695,#24442,.T.);
#48234=EDGE_CURVE('',#37700,#37701,#28611,.T.);
#48235=EDGE_CURVE('',#37698,#37701,#20272,.T.);
#48236=EDGE_CURVE('',#37699,#37700,#20273,.T.);
#48237=EDGE_CURVE('',#37702,#37703,#20274,.T.);
#48238=EDGE_CURVE('',#37703,#37704,#28612,.T.);
#48239=EDGE_CURVE('',#37705,#37704,#20275,.T.);
#48240=EDGE_CURVE('',#37702,#37705,#28613,.T.);
#48241=EDGE_CURVE('',#37706,#37707,#28614,.T.);
#48242=EDGE_CURVE('',#37704,#37706,#24443,.T.);
#48243=EDGE_CURVE('',#37707,#37703,#24444,.T.);
#48244=EDGE_CURVE('',#37700,#37702,#24445,.T.);
#48245=EDGE_CURVE('',#37701,#37705,#24446,.T.);
#48246=EDGE_CURVE('',#37708,#37709,#28615,.T.);
#48247=EDGE_CURVE('',#37706,#37709,#20276,.T.);
#48248=EDGE_CURVE('',#37707,#37708,#20277,.T.);
#48249=EDGE_CURVE('',#37710,#37711,#20278,.T.);
#48250=EDGE_CURVE('',#37711,#37712,#28616,.T.);
#48251=EDGE_CURVE('',#37713,#37712,#20279,.T.);
#48252=EDGE_CURVE('',#37710,#37713,#28617,.T.);
#48253=EDGE_CURVE('',#37708,#37710,#24447,.T.);
#48254=EDGE_CURVE('',#37709,#37713,#24448,.T.);
#48255=EDGE_CURVE('',#37714,#37715,#28618,.T.);
#48256=EDGE_CURVE('',#37712,#37714,#24449,.T.);
#48257=EDGE_CURVE('',#37715,#37711,#24450,.T.);
#48258=EDGE_CURVE('',#37716,#37717,#28619,.T.);
#48259=EDGE_CURVE('',#37714,#37717,#20280,.T.);
#48260=EDGE_CURVE('',#37715,#37716,#20281,.T.);
#48261=EDGE_CURVE('',#37718,#37719,#20282,.T.);
#48262=EDGE_CURVE('',#37719,#37720,#28620,.T.);
#48263=EDGE_CURVE('',#37721,#37720,#20283,.T.);
#48264=EDGE_CURVE('',#37718,#37721,#28621,.T.);
#48265=EDGE_CURVE('',#37722,#37723,#28622,.T.);
#48266=EDGE_CURVE('',#37720,#37722,#24451,.T.);
#48267=EDGE_CURVE('',#37723,#37719,#24452,.T.);
#48268=EDGE_CURVE('',#37716,#37718,#24453,.T.);
#48269=EDGE_CURVE('',#37717,#37721,#24454,.T.);
#48270=EDGE_CURVE('',#37724,#37725,#28623,.T.);
#48271=EDGE_CURVE('',#37722,#37725,#20284,.T.);
#48272=EDGE_CURVE('',#37723,#37724,#20285,.T.);
#48273=EDGE_CURVE('',#37726,#37727,#20286,.T.);
#48274=EDGE_CURVE('',#37727,#37728,#28624,.T.);
#48275=EDGE_CURVE('',#37729,#37728,#20287,.T.);
#48276=EDGE_CURVE('',#37726,#37729,#28625,.T.);
#48277=EDGE_CURVE('',#37724,#37726,#24455,.T.);
#48278=EDGE_CURVE('',#37725,#37729,#24456,.T.);
#48279=EDGE_CURVE('',#37730,#37731,#28626,.T.);
#48280=EDGE_CURVE('',#37728,#37730,#24457,.T.);
#48281=EDGE_CURVE('',#37731,#37727,#24458,.T.);
#48282=EDGE_CURVE('',#37732,#37733,#28627,.T.);
#48283=EDGE_CURVE('',#37730,#37733,#20288,.T.);
#48284=EDGE_CURVE('',#37731,#37732,#20289,.T.);
#48285=EDGE_CURVE('',#37734,#37735,#20290,.T.);
#48286=EDGE_CURVE('',#37735,#37736,#28628,.T.);
#48287=EDGE_CURVE('',#37737,#37736,#20291,.T.);
#48288=EDGE_CURVE('',#37734,#37737,#28629,.T.);
#48289=EDGE_CURVE('',#37738,#37739,#28630,.T.);
#48290=EDGE_CURVE('',#37736,#37738,#24459,.T.);
#48291=EDGE_CURVE('',#37739,#37735,#24460,.T.);
#48292=EDGE_CURVE('',#37732,#37734,#24461,.T.);
#48293=EDGE_CURVE('',#37733,#37737,#24462,.T.);
#48294=EDGE_CURVE('',#37740,#37741,#28631,.T.);
#48295=EDGE_CURVE('',#37738,#37741,#20292,.T.);
#48296=EDGE_CURVE('',#37739,#37740,#20293,.T.);
#48297=EDGE_CURVE('',#37742,#37743,#20294,.T.);
#48298=EDGE_CURVE('',#37743,#37744,#28632,.T.);
#48299=EDGE_CURVE('',#37745,#37744,#20295,.T.);
#48300=EDGE_CURVE('',#37742,#37745,#28633,.T.);
#48301=EDGE_CURVE('',#37740,#37742,#24463,.T.);
#48302=EDGE_CURVE('',#37741,#37745,#24464,.T.);
#48303=EDGE_CURVE('',#37746,#37747,#28634,.T.);
#48304=EDGE_CURVE('',#37744,#37746,#24465,.T.);
#48305=EDGE_CURVE('',#37747,#37743,#24466,.T.);
#48306=EDGE_CURVE('',#37748,#37749,#28635,.T.);
#48307=EDGE_CURVE('',#37746,#37749,#20296,.T.);
#48308=EDGE_CURVE('',#37747,#37748,#20297,.T.);
#48309=EDGE_CURVE('',#37750,#37751,#20298,.T.);
#48310=EDGE_CURVE('',#37751,#37752,#28636,.T.);
#48311=EDGE_CURVE('',#37753,#37752,#20299,.T.);
#48312=EDGE_CURVE('',#37750,#37753,#28637,.T.);
#48313=EDGE_CURVE('',#37754,#37755,#28638,.T.);
#48314=EDGE_CURVE('',#37752,#37754,#24467,.T.);
#48315=EDGE_CURVE('',#37755,#37751,#24468,.T.);
#48316=EDGE_CURVE('',#37748,#37750,#24469,.T.);
#48317=EDGE_CURVE('',#37749,#37753,#24470,.T.);
#48318=EDGE_CURVE('',#37756,#37757,#28639,.T.);
#48319=EDGE_CURVE('',#37754,#37757,#20300,.T.);
#48320=EDGE_CURVE('',#37755,#37756,#20301,.T.);
#48321=EDGE_CURVE('',#37758,#37759,#20302,.T.);
#48322=EDGE_CURVE('',#37759,#37760,#28640,.T.);
#48323=EDGE_CURVE('',#37761,#37760,#20303,.T.);
#48324=EDGE_CURVE('',#37758,#37761,#28641,.T.);
#48325=EDGE_CURVE('',#37756,#37758,#24471,.T.);
#48326=EDGE_CURVE('',#37757,#37761,#24472,.T.);
#48327=EDGE_CURVE('',#37762,#37763,#28642,.T.);
#48328=EDGE_CURVE('',#37760,#37762,#24473,.T.);
#48329=EDGE_CURVE('',#37763,#37759,#24474,.T.);
#48330=EDGE_CURVE('',#37764,#37765,#28643,.T.);
#48331=EDGE_CURVE('',#37762,#37765,#20304,.T.);
#48332=EDGE_CURVE('',#37763,#37764,#20305,.T.);
#48333=EDGE_CURVE('',#37766,#37767,#20306,.T.);
#48334=EDGE_CURVE('',#37767,#37768,#28644,.T.);
#48335=EDGE_CURVE('',#37769,#37768,#20307,.T.);
#48336=EDGE_CURVE('',#37766,#37769,#28645,.T.);
#48337=EDGE_CURVE('',#37770,#37771,#28646,.T.);
#48338=EDGE_CURVE('',#37768,#37770,#24475,.T.);
#48339=EDGE_CURVE('',#37771,#37767,#24476,.T.);
#48340=EDGE_CURVE('',#37764,#37766,#24477,.T.);
#48341=EDGE_CURVE('',#37765,#37769,#24478,.T.);
#48342=EDGE_CURVE('',#37772,#37773,#28647,.T.);
#48343=EDGE_CURVE('',#37770,#37773,#20308,.T.);
#48344=EDGE_CURVE('',#37771,#37772,#20309,.T.);
#48345=EDGE_CURVE('',#37774,#37775,#20310,.T.);
#48346=EDGE_CURVE('',#37775,#37776,#28648,.T.);
#48347=EDGE_CURVE('',#37777,#37776,#20311,.T.);
#48348=EDGE_CURVE('',#37774,#37777,#28649,.T.);
#48349=EDGE_CURVE('',#37772,#37774,#24479,.T.);
#48350=EDGE_CURVE('',#37773,#37777,#24480,.T.);
#48351=EDGE_CURVE('',#37778,#37779,#28650,.T.);
#48352=EDGE_CURVE('',#37776,#37778,#24481,.T.);
#48353=EDGE_CURVE('',#37779,#37775,#24482,.T.);
#48354=EDGE_CURVE('',#37780,#37781,#28651,.T.);
#48355=EDGE_CURVE('',#37778,#37781,#20312,.T.);
#48356=EDGE_CURVE('',#37779,#37780,#20313,.T.);
#48357=EDGE_CURVE('',#37782,#37783,#20314,.T.);
#48358=EDGE_CURVE('',#37783,#37784,#28652,.T.);
#48359=EDGE_CURVE('',#37785,#37784,#20315,.T.);
#48360=EDGE_CURVE('',#37782,#37785,#28653,.T.);
#48361=EDGE_CURVE('',#37786,#37787,#28654,.T.);
#48362=EDGE_CURVE('',#37784,#37786,#24483,.T.);
#48363=EDGE_CURVE('',#37787,#37783,#24484,.T.);
#48364=EDGE_CURVE('',#37780,#37782,#24485,.T.);
#48365=EDGE_CURVE('',#37781,#37785,#24486,.T.);
#48366=EDGE_CURVE('',#37788,#37789,#28655,.T.);
#48367=EDGE_CURVE('',#37786,#37789,#20316,.T.);
#48368=EDGE_CURVE('',#37787,#37788,#20317,.T.);
#48369=EDGE_CURVE('',#37790,#37791,#20318,.T.);
#48370=EDGE_CURVE('',#37791,#37792,#28656,.T.);
#48371=EDGE_CURVE('',#37793,#37792,#20319,.T.);
#48372=EDGE_CURVE('',#37790,#37793,#28657,.T.);
#48373=EDGE_CURVE('',#37788,#37790,#24487,.T.);
#48374=EDGE_CURVE('',#37789,#37793,#24488,.T.);
#48375=EDGE_CURVE('',#37794,#37795,#28658,.T.);
#48376=EDGE_CURVE('',#37792,#37794,#24489,.T.);
#48377=EDGE_CURVE('',#37795,#37791,#24490,.T.);
#48378=EDGE_CURVE('',#37795,#37796,#20320,.T.);
#48379=EDGE_CURVE('',#37797,#37456,#20321,.T.);
#48380=EDGE_CURVE('',#37797,#37798,#24491,.T.);
#48381=EDGE_CURVE('',#37799,#37798,#20322,.T.);
#48382=EDGE_CURVE('',#37796,#37799,#24492,.T.);
#48383=EDGE_CURVE('',#37800,#37800,#20323,.T.);
#48384=EDGE_CURVE('',#37801,#37797,#28659,.T.);
#48385=EDGE_CURVE('',#37801,#37457,#20324,.T.);
#48386=EDGE_CURVE('',#37796,#37802,#28660,.T.);
#48387=EDGE_CURVE('',#37794,#37802,#20325,.T.);
#48388=EDGE_CURVE('',#37798,#37803,#28661,.T.);
#48389=EDGE_CURVE('',#37804,#37803,#20326,.T.);
#48390=EDGE_CURVE('',#37799,#37804,#28662,.T.);
#48391=EDGE_CURVE('',#37803,#37801,#24493,.T.);
#48392=EDGE_CURVE('',#37802,#37804,#24494,.T.);
#48393=EDGE_CURVE('',#37800,#37805,#28663,.T.);
#48394=EDGE_CURVE('',#37805,#37805,#20327,.T.);
#48395=EDGE_CURVE('',#37806,#37806,#20328,.T.);
#48396=EDGE_CURVE('',#37806,#37807,#28664,.T.);
#48397=EDGE_CURVE('',#37807,#37807,#20329,.T.);
#48398=EDGE_CURVE('',#37808,#37808,#20330,.F.);
#48399=EDGE_CURVE('',#37808,#37809,#28665,.T.);
#48400=EDGE_CURVE('',#37809,#37809,#20331,.T.);
#48401=EDGE_CURVE('',#37810,#37811,#28666,.T.);
#48402=EDGE_CURVE('',#37811,#37812,#20332,.T.);
#48403=EDGE_CURVE('',#37812,#37813,#28667,.T.);
#48404=EDGE_CURVE('',#37813,#37814,#24495,.T.);
#48405=EDGE_CURVE('',#37814,#37815,#20333,.T.);
#48406=EDGE_CURVE('',#37815,#37816,#24496,.T.);
#48407=EDGE_CURVE('',#37816,#37817,#28668,.T.);
#48408=EDGE_CURVE('',#37817,#37818,#20334,.T.);
#48409=EDGE_CURVE('',#37818,#37819,#28669,.T.);
#48410=EDGE_CURVE('',#37819,#37820,#24497,.T.);
#48411=EDGE_CURVE('',#37820,#37821,#20335,.T.);
#48412=EDGE_CURVE('',#37821,#37822,#24498,.T.);
#48413=EDGE_CURVE('',#37822,#37823,#28670,.T.);
#48414=EDGE_CURVE('',#37823,#37824,#20336,.T.);
#48415=EDGE_CURVE('',#37824,#37825,#28671,.T.);
#48416=EDGE_CURVE('',#37825,#37826,#24499,.T.);
#48417=EDGE_CURVE('',#37826,#37827,#20337,.T.);
#48418=EDGE_CURVE('',#37827,#37828,#24500,.T.);
#48419=EDGE_CURVE('',#37828,#37829,#28672,.T.);
#48420=EDGE_CURVE('',#37829,#37830,#20338,.T.);
#48421=EDGE_CURVE('',#37830,#37831,#28673,.T.);
#48422=EDGE_CURVE('',#37831,#37832,#24501,.T.);
#48423=EDGE_CURVE('',#37832,#37833,#20339,.T.);
#48424=EDGE_CURVE('',#37833,#37834,#24502,.T.);
#48425=EDGE_CURVE('',#37834,#37835,#28674,.T.);
#48426=EDGE_CURVE('',#37835,#37836,#20340,.T.);
#48427=EDGE_CURVE('',#37836,#37837,#28675,.T.);
#48428=EDGE_CURVE('',#37837,#37838,#24503,.T.);
#48429=EDGE_CURVE('',#37838,#37839,#20341,.T.);
#48430=EDGE_CURVE('',#37839,#37840,#24504,.T.);
#48431=EDGE_CURVE('',#37840,#37841,#28676,.T.);
#48432=EDGE_CURVE('',#37841,#37842,#20342,.T.);
#48433=EDGE_CURVE('',#37842,#37843,#28677,.T.);
#48434=EDGE_CURVE('',#37843,#37844,#24505,.T.);
#48435=EDGE_CURVE('',#37844,#37845,#20343,.T.);
#48436=EDGE_CURVE('',#37845,#37846,#24506,.T.);
#48437=EDGE_CURVE('',#37846,#37847,#28678,.T.);
#48438=EDGE_CURVE('',#37847,#37848,#20344,.T.);
#48439=EDGE_CURVE('',#37848,#37849,#28679,.T.);
#48440=EDGE_CURVE('',#37849,#37850,#24507,.T.);
#48441=EDGE_CURVE('',#37850,#37851,#20345,.T.);
#48442=EDGE_CURVE('',#37851,#37852,#24508,.T.);
#48443=EDGE_CURVE('',#37852,#37853,#28680,.T.);
#48444=EDGE_CURVE('',#37853,#37854,#20346,.T.);
#48445=EDGE_CURVE('',#37854,#37855,#28681,.T.);
#48446=EDGE_CURVE('',#37855,#37856,#24509,.T.);
#48447=EDGE_CURVE('',#37856,#37857,#20347,.T.);
#48448=EDGE_CURVE('',#37857,#37858,#24510,.T.);
#48449=EDGE_CURVE('',#37858,#37859,#28682,.T.);
#48450=EDGE_CURVE('',#37859,#37860,#20348,.T.);
#48451=EDGE_CURVE('',#37860,#37861,#28683,.T.);
#48452=EDGE_CURVE('',#37861,#37862,#24511,.T.);
#48453=EDGE_CURVE('',#37862,#37863,#20349,.T.);
#48454=EDGE_CURVE('',#37863,#37864,#24512,.T.);
#48455=EDGE_CURVE('',#37864,#37865,#28684,.T.);
#48456=EDGE_CURVE('',#37865,#37866,#20350,.T.);
#48457=EDGE_CURVE('',#37866,#37867,#28685,.T.);
#48458=EDGE_CURVE('',#37867,#37868,#24513,.T.);
#48459=EDGE_CURVE('',#37868,#37869,#20351,.T.);
#48460=EDGE_CURVE('',#37869,#37870,#24514,.T.);
#48461=EDGE_CURVE('',#37870,#37871,#28686,.T.);
#48462=EDGE_CURVE('',#37871,#37872,#20352,.T.);
#48463=EDGE_CURVE('',#37872,#37873,#28687,.T.);
#48464=EDGE_CURVE('',#37873,#37874,#24515,.T.);
#48465=EDGE_CURVE('',#37874,#37875,#20353,.T.);
#48466=EDGE_CURVE('',#37875,#37876,#24516,.T.);
#48467=EDGE_CURVE('',#37876,#37877,#28688,.T.);
#48468=EDGE_CURVE('',#37877,#37878,#20354,.T.);
#48469=EDGE_CURVE('',#37878,#37879,#28689,.T.);
#48470=EDGE_CURVE('',#37879,#37880,#24517,.T.);
#48471=EDGE_CURVE('',#37880,#37881,#20355,.T.);
#48472=EDGE_CURVE('',#37881,#37882,#24518,.T.);
#48473=EDGE_CURVE('',#37882,#37883,#28690,.T.);
#48474=EDGE_CURVE('',#37883,#37884,#20356,.T.);
#48475=EDGE_CURVE('',#37884,#37885,#28691,.T.);
#48476=EDGE_CURVE('',#37885,#37886,#24519,.T.);
#48477=EDGE_CURVE('',#37886,#37887,#20357,.T.);
#48478=EDGE_CURVE('',#37887,#37888,#24520,.T.);
#48479=EDGE_CURVE('',#37888,#37889,#28692,.T.);
#48480=EDGE_CURVE('',#37889,#37890,#20358,.T.);
#48481=EDGE_CURVE('',#37890,#37891,#28693,.T.);
#48482=EDGE_CURVE('',#37891,#37892,#24521,.T.);
#48483=EDGE_CURVE('',#37892,#37893,#20359,.T.);
#48484=EDGE_CURVE('',#37893,#37894,#24522,.T.);
#48485=EDGE_CURVE('',#37894,#37895,#28694,.T.);
#48486=EDGE_CURVE('',#37895,#37896,#20360,.T.);
#48487=EDGE_CURVE('',#37896,#37897,#28695,.T.);
#48488=EDGE_CURVE('',#37897,#37898,#24523,.T.);
#48489=EDGE_CURVE('',#37898,#37899,#20361,.T.);
#48490=EDGE_CURVE('',#37899,#37900,#24524,.T.);
#48491=EDGE_CURVE('',#37900,#37901,#28696,.T.);
#48492=EDGE_CURVE('',#37901,#37902,#20362,.T.);
#48493=EDGE_CURVE('',#37902,#37903,#28697,.T.);
#48494=EDGE_CURVE('',#37903,#37904,#24525,.T.);
#48495=EDGE_CURVE('',#37904,#37905,#20363,.T.);
#48496=EDGE_CURVE('',#37905,#37906,#24526,.T.);
#48497=EDGE_CURVE('',#37906,#37907,#28698,.T.);
#48498=EDGE_CURVE('',#37907,#37908,#20364,.T.);
#48499=EDGE_CURVE('',#37908,#37909,#28699,.T.);
#48500=EDGE_CURVE('',#37909,#37910,#24527,.T.);
#48501=EDGE_CURVE('',#37910,#37911,#20365,.T.);
#48502=EDGE_CURVE('',#37911,#37810,#24528,.T.);
#48503=EDGE_CURVE('',#37912,#37912,#20366,.T.);
#48504=EDGE_CURVE('',#37913,#37913,#20367,.F.);
#48505=EDGE_CURVE('',#37913,#37914,#28700,.T.);
#48506=EDGE_CURVE('',#37914,#37914,#20368,.T.);
#48507=EDGE_CURVE('',#37862,#37915,#28701,.T.);
#48508=EDGE_CURVE('',#37916,#37915,#20369,.T.);
#48509=EDGE_CURVE('',#37863,#37916,#28702,.T.);
#48510=EDGE_CURVE('',#37861,#37917,#28703,.T.);
#48511=EDGE_CURVE('',#37915,#37917,#24529,.T.);
#48512=EDGE_CURVE('',#37918,#37860,#28704,.T.);
#48513=EDGE_CURVE('',#37917,#37918,#28705,.T.);
#48514=EDGE_CURVE('',#37859,#37919,#28706,.T.);
#48515=EDGE_CURVE('',#37918,#37919,#20370,.T.);
#48516=EDGE_CURVE('',#37858,#37920,#28707,.T.);
#48517=EDGE_CURVE('',#37919,#37920,#28708,.T.);
#48518=EDGE_CURVE('',#37857,#37921,#28709,.T.);
#48519=EDGE_CURVE('',#37920,#37921,#24530,.T.);
#48520=EDGE_CURVE('',#37856,#37922,#28710,.T.);
#48521=EDGE_CURVE('',#37921,#37922,#20371,.T.);
#48522=EDGE_CURVE('',#37855,#37923,#28711,.T.);
#48523=EDGE_CURVE('',#37922,#37923,#24531,.T.);
#48524=EDGE_CURVE('',#37924,#37854,#28712,.T.);
#48525=EDGE_CURVE('',#37923,#37924,#28713,.T.);
#48526=EDGE_CURVE('',#37853,#37925,#28714,.T.);
#48527=EDGE_CURVE('',#37924,#37925,#20372,.T.);
#48528=EDGE_CURVE('',#37852,#37926,#28715,.T.);
#48529=EDGE_CURVE('',#37925,#37926,#28716,.T.);
#48530=EDGE_CURVE('',#37851,#37927,#28717,.T.);
#48531=EDGE_CURVE('',#37926,#37927,#24532,.T.);
#48532=EDGE_CURVE('',#37850,#37928,#28718,.T.);
#48533=EDGE_CURVE('',#37927,#37928,#20373,.T.);
#48534=EDGE_CURVE('',#37849,#37929,#28719,.T.);
#48535=EDGE_CURVE('',#37928,#37929,#24533,.T.);
#48536=EDGE_CURVE('',#37930,#37848,#28720,.T.);
#48537=EDGE_CURVE('',#37929,#37930,#28721,.T.);
#48538=EDGE_CURVE('',#37847,#37931,#28722,.T.);
#48539=EDGE_CURVE('',#37930,#37931,#20374,.T.);
#48540=EDGE_CURVE('',#37846,#37932,#28723,.T.);
#48541=EDGE_CURVE('',#37931,#37932,#28724,.T.);
#48542=EDGE_CURVE('',#37845,#37933,#28725,.T.);
#48543=EDGE_CURVE('',#37932,#37933,#24534,.T.);
#48544=EDGE_CURVE('',#37844,#37934,#28726,.T.);
#48545=EDGE_CURVE('',#37933,#37934,#20375,.T.);
#48546=EDGE_CURVE('',#37843,#37935,#28727,.T.);
#48547=EDGE_CURVE('',#37934,#37935,#24535,.T.);
#48548=EDGE_CURVE('',#37936,#37842,#28728,.T.);
#48549=EDGE_CURVE('',#37935,#37936,#28729,.T.);
#48550=EDGE_CURVE('',#37841,#37937,#28730,.T.);
#48551=EDGE_CURVE('',#37936,#37937,#20376,.T.);
#48552=EDGE_CURVE('',#37840,#37938,#28731,.T.);
#48553=EDGE_CURVE('',#37937,#37938,#28732,.T.);
#48554=EDGE_CURVE('',#37839,#37939,#28733,.T.);
#48555=EDGE_CURVE('',#37938,#37939,#24536,.T.);
#48556=EDGE_CURVE('',#37838,#37940,#28734,.T.);
#48557=EDGE_CURVE('',#37939,#37940,#20377,.T.);
#48558=EDGE_CURVE('',#37837,#37941,#28735,.T.);
#48559=EDGE_CURVE('',#37940,#37941,#24537,.T.);
#48560=EDGE_CURVE('',#37942,#37836,#28736,.T.);
#48561=EDGE_CURVE('',#37941,#37942,#28737,.T.);
#48562=EDGE_CURVE('',#37835,#37943,#28738,.T.);
#48563=EDGE_CURVE('',#37942,#37943,#20378,.T.);
#48564=EDGE_CURVE('',#37834,#37944,#28739,.T.);
#48565=EDGE_CURVE('',#37943,#37944,#28740,.T.);
#48566=EDGE_CURVE('',#37833,#37945,#28741,.T.);
#48567=EDGE_CURVE('',#37944,#37945,#24538,.T.);
#48568=EDGE_CURVE('',#37832,#37946,#28742,.T.);
#48569=EDGE_CURVE('',#37945,#37946,#20379,.T.);
#48570=EDGE_CURVE('',#37831,#37947,#28743,.T.);
#48571=EDGE_CURVE('',#37946,#37947,#24539,.T.);
#48572=EDGE_CURVE('',#37948,#37830,#28744,.T.);
#48573=EDGE_CURVE('',#37947,#37948,#28745,.T.);
#48574=EDGE_CURVE('',#37829,#37949,#28746,.T.);
#48575=EDGE_CURVE('',#37948,#37949,#20380,.T.);
#48576=EDGE_CURVE('',#37828,#37950,#28747,.T.);
#48577=EDGE_CURVE('',#37949,#37950,#28748,.T.);
#48578=EDGE_CURVE('',#37827,#37951,#28749,.T.);
#48579=EDGE_CURVE('',#37950,#37951,#24540,.T.);
#48580=EDGE_CURVE('',#37826,#37952,#28750,.T.);
#48581=EDGE_CURVE('',#37951,#37952,#20381,.T.);
#48582=EDGE_CURVE('',#37825,#37953,#28751,.T.);
#48583=EDGE_CURVE('',#37952,#37953,#24541,.T.);
#48584=EDGE_CURVE('',#37954,#37824,#28752,.T.);
#48585=EDGE_CURVE('',#37953,#37954,#28753,.T.);
#48586=EDGE_CURVE('',#37823,#37955,#28754,.T.);
#48587=EDGE_CURVE('',#37954,#37955,#20382,.T.);
#48588=EDGE_CURVE('',#37822,#37956,#28755,.T.);
#48589=EDGE_CURVE('',#37955,#37956,#28756,.T.);
#48590=EDGE_CURVE('',#37821,#37957,#28757,.T.);
#48591=EDGE_CURVE('',#37956,#37957,#24542,.T.);
#48592=EDGE_CURVE('',#37820,#37958,#28758,.T.);
#48593=EDGE_CURVE('',#37957,#37958,#20383,.T.);
#48594=EDGE_CURVE('',#37819,#37959,#28759,.T.);
#48595=EDGE_CURVE('',#37958,#37959,#24543,.T.);
#48596=EDGE_CURVE('',#37960,#37818,#28760,.T.);
#48597=EDGE_CURVE('',#37959,#37960,#28761,.T.);
#48598=EDGE_CURVE('',#37817,#37961,#28762,.T.);
#48599=EDGE_CURVE('',#37960,#37961,#20384,.T.);
#48600=EDGE_CURVE('',#37816,#37962,#28763,.T.);
#48601=EDGE_CURVE('',#37961,#37962,#28764,.T.);
#48602=EDGE_CURVE('',#37815,#37963,#28765,.T.);
#48603=EDGE_CURVE('',#37962,#37963,#24544,.T.);
#48604=EDGE_CURVE('',#37814,#37964,#28766,.T.);
#48605=EDGE_CURVE('',#37963,#37964,#20385,.T.);
#48606=EDGE_CURVE('',#37813,#37965,#28767,.T.);
#48607=EDGE_CURVE('',#37964,#37965,#24545,.T.);
#48608=EDGE_CURVE('',#37966,#37812,#28768,.T.);
#48609=EDGE_CURVE('',#37965,#37966,#28769,.T.);
#48610=EDGE_CURVE('',#37966,#37967,#20386,.T.);
#48611=EDGE_CURVE('',#37967,#37968,#28770,.T.);
#48612=EDGE_CURVE('',#37968,#37969,#24546,.T.);
#48613=EDGE_CURVE('',#37969,#37970,#20387,.T.);
#48614=EDGE_CURVE('',#37970,#37971,#24547,.T.);
#48615=EDGE_CURVE('',#37971,#37972,#28771,.T.);
#48616=EDGE_CURVE('',#37972,#37973,#20388,.T.);
#48617=EDGE_CURVE('',#37973,#37974,#28772,.T.);
#48618=EDGE_CURVE('',#37974,#37975,#24548,.T.);
#48619=EDGE_CURVE('',#37975,#37976,#20389,.T.);
#48620=EDGE_CURVE('',#37976,#37977,#24549,.T.);
#48621=EDGE_CURVE('',#37977,#37978,#28773,.T.);
#48622=EDGE_CURVE('',#37978,#37979,#20390,.T.);
#48623=EDGE_CURVE('',#37979,#37980,#28774,.T.);
#48624=EDGE_CURVE('',#37980,#37981,#24550,.T.);
#48625=EDGE_CURVE('',#37981,#37982,#20391,.T.);
#48626=EDGE_CURVE('',#37982,#37983,#24551,.T.);
#48627=EDGE_CURVE('',#37983,#37984,#28775,.T.);
#48628=EDGE_CURVE('',#37984,#37985,#20392,.T.);
#48629=EDGE_CURVE('',#37985,#37986,#28776,.T.);
#48630=EDGE_CURVE('',#37986,#37987,#24552,.T.);
#48631=EDGE_CURVE('',#37987,#37988,#20393,.T.);
#48632=EDGE_CURVE('',#37988,#37989,#24553,.T.);
#48633=EDGE_CURVE('',#37989,#37990,#28777,.T.);
#48634=EDGE_CURVE('',#37990,#37991,#20394,.T.);
#48635=EDGE_CURVE('',#37991,#37992,#28778,.T.);
#48636=EDGE_CURVE('',#37992,#37993,#24554,.T.);
#48637=EDGE_CURVE('',#37993,#37994,#20395,.T.);
#48638=EDGE_CURVE('',#37994,#37995,#24555,.T.);
#48639=EDGE_CURVE('',#37995,#37996,#28779,.T.);
#48640=EDGE_CURVE('',#37996,#37997,#20396,.T.);
#48641=EDGE_CURVE('',#37997,#37998,#28780,.T.);
#48642=EDGE_CURVE('',#37998,#37999,#24556,.T.);
#48643=EDGE_CURVE('',#37999,#38000,#20397,.T.);
#48644=EDGE_CURVE('',#38000,#38001,#24557,.T.);
#48645=EDGE_CURVE('',#38001,#38002,#28781,.T.);
#48646=EDGE_CURVE('',#38002,#38003,#20398,.T.);
#48647=EDGE_CURVE('',#38003,#38004,#28782,.T.);
#48648=EDGE_CURVE('',#38004,#38005,#24558,.T.);
#48649=EDGE_CURVE('',#38005,#38006,#20399,.T.);
#48650=EDGE_CURVE('',#38006,#38007,#24559,.T.);
#48651=EDGE_CURVE('',#38007,#38008,#28783,.T.);
#48652=EDGE_CURVE('',#38008,#38009,#20400,.T.);
#48653=EDGE_CURVE('',#38009,#38010,#28784,.T.);
#48654=EDGE_CURVE('',#38010,#38011,#24560,.T.);
#48655=EDGE_CURVE('',#38011,#38012,#20401,.T.);
#48656=EDGE_CURVE('',#38012,#38013,#24561,.T.);
#48657=EDGE_CURVE('',#38013,#38014,#28785,.T.);
#48658=EDGE_CURVE('',#38014,#38015,#20402,.T.);
#48659=EDGE_CURVE('',#38015,#38016,#28786,.T.);
#48660=EDGE_CURVE('',#38016,#37916,#24562,.T.);
#48661=EDGE_CURVE('',#37864,#38016,#28787,.T.);
#48662=EDGE_CURVE('',#37865,#38015,#28788,.T.);
#48663=EDGE_CURVE('',#38014,#37866,#28789,.T.);
#48664=EDGE_CURVE('',#37867,#38013,#28790,.T.);
#48665=EDGE_CURVE('',#37868,#38012,#28791,.T.);
#48666=EDGE_CURVE('',#37869,#38011,#28792,.T.);
#48667=EDGE_CURVE('',#37870,#38010,#28793,.T.);
#48668=EDGE_CURVE('',#37871,#38009,#28794,.T.);
#48669=EDGE_CURVE('',#38008,#37872,#28795,.T.);
#48670=EDGE_CURVE('',#37876,#38004,#28796,.T.);
#48671=EDGE_CURVE('',#37877,#38003,#28797,.T.);
#48672=EDGE_CURVE('',#37873,#38007,#28798,.T.);
#48673=EDGE_CURVE('',#37874,#38006,#28799,.T.);
#48674=EDGE_CURVE('',#37875,#38005,#28800,.T.);
#48675=EDGE_CURVE('',#38002,#37878,#28801,.T.);
#48676=EDGE_CURVE('',#37879,#38001,#28802,.T.);
#48677=EDGE_CURVE('',#37882,#37998,#28803,.T.);
#48678=EDGE_CURVE('',#37883,#37997,#28804,.T.);
#48679=EDGE_CURVE('',#37880,#38000,#28805,.T.);
#48680=EDGE_CURVE('',#37881,#37999,#28806,.T.);
#48681=EDGE_CURVE('',#37996,#37884,#28807,.T.);
#48682=EDGE_CURVE('',#37885,#37995,#28808,.T.);
#48683=EDGE_CURVE('',#37886,#37994,#28809,.T.);
#48684=EDGE_CURVE('',#37887,#37993,#28810,.T.);
#48685=EDGE_CURVE('',#37888,#37992,#28811,.T.);
#48686=EDGE_CURVE('',#37889,#37991,#28812,.T.);
#48687=EDGE_CURVE('',#37990,#37890,#28813,.T.);
#48688=EDGE_CURVE('',#37894,#37986,#28814,.T.);
#48689=EDGE_CURVE('',#37895,#37985,#28815,.T.);
#48690=EDGE_CURVE('',#37891,#37989,#28816,.T.);
#48691=EDGE_CURVE('',#37892,#37988,#28817,.T.);
#48692=EDGE_CURVE('',#37893,#37987,#28818,.T.);
#48693=EDGE_CURVE('',#37984,#37896,#28819,.T.);
#48694=EDGE_CURVE('',#37897,#37983,#28820,.T.);
#48695=EDGE_CURVE('',#37900,#37980,#28821,.T.);
#48696=EDGE_CURVE('',#37901,#37979,#28822,.T.);
#48697=EDGE_CURVE('',#37898,#37982,#28823,.T.);
#48698=EDGE_CURVE('',#37899,#37981,#28824,.T.);
#48699=EDGE_CURVE('',#37978,#37902,#28825,.T.);
#48700=EDGE_CURVE('',#37903,#37977,#28826,.T.);
#48701=EDGE_CURVE('',#37904,#37976,#28827,.T.);
#48702=EDGE_CURVE('',#37905,#37975,#28828,.T.);
#48703=EDGE_CURVE('',#37906,#37974,#28829,.T.);
#48704=EDGE_CURVE('',#37907,#37973,#28830,.T.);
#48705=EDGE_CURVE('',#37972,#37908,#28831,.T.);
#48706=EDGE_CURVE('',#37810,#37968,#28832,.T.);
#48707=EDGE_CURVE('',#37811,#37967,#28833,.T.);
#48708=EDGE_CURVE('',#37909,#37971,#28834,.T.);
#48709=EDGE_CURVE('',#37910,#37970,#28835,.T.);
#48710=EDGE_CURVE('',#37911,#37969,#28836,.T.);
#48711=EDGE_CURVE('',#37912,#38017,#28837,.T.);
#48712=EDGE_CURVE('',#38017,#38017,#20403,.T.);
#48713=EDGE_CURVE('',#38018,#38018,#20404,.T.);
#48714=EDGE_CURVE('',#38018,#38019,#20405,.T.);
#48715=EDGE_CURVE('',#38019,#38019,#20406,.T.);
#48716=EDGE_CURVE('',#38020,#38020,#20407,.T.);
#48717=EDGE_CURVE('',#38019,#38021,#28838,.T.);
#48718=EDGE_CURVE('',#38021,#38022,#20408,.T.);
#48719=EDGE_CURVE('',#38022,#38023,#28839,.T.);
#48720=EDGE_CURVE('',#38023,#38024,#20409,.T.);
#48721=EDGE_CURVE('',#38024,#38025,#28840,.T.);
#48722=EDGE_CURVE('',#38026,#38025,#20410,.T.);
#48723=EDGE_CURVE('',#38025,#38026,#20411,.T.);
#48724=EDGE_CURVE('',#38024,#38027,#20412,.T.);
#48725=EDGE_CURVE('',#38027,#38028,#28841,.T.);
#48726=EDGE_CURVE('',#38028,#38021,#20413,.T.);
#48727=EDGE_CURVE('',#38029,#38030,#20414,.T.);
#48728=EDGE_CURVE('',#38030,#38031,#28842,.T.);
#48729=EDGE_CURVE('',#38031,#38032,#20415,.T.);
#48730=EDGE_CURVE('',#38032,#38029,#28843,.T.);
#48731=EDGE_CURVE('',#38033,#38034,#20416,.T.);
#48732=EDGE_CURVE('',#38034,#38035,#28844,.T.);
#48733=EDGE_CURVE('',#38035,#38036,#20417,.T.);
#48734=EDGE_CURVE('',#38036,#38033,#28845,.T.);
#48735=EDGE_CURVE('',#38037,#38038,#20418,.T.);
#48736=EDGE_CURVE('',#38038,#38039,#28846,.T.);
#48737=EDGE_CURVE('',#38039,#38040,#20419,.T.);
#48738=EDGE_CURVE('',#38040,#38037,#28847,.T.);
#48739=EDGE_CURVE('',#38041,#38042,#20420,.T.);
#48740=EDGE_CURVE('',#38042,#38043,#28848,.T.);
#48741=EDGE_CURVE('',#38043,#38044,#20421,.T.);
#48742=EDGE_CURVE('',#38044,#38041,#28849,.T.);
#48743=EDGE_CURVE('',#38045,#38046,#20422,.T.);
#48744=EDGE_CURVE('',#38046,#38047,#28850,.T.);
#48745=EDGE_CURVE('',#38047,#38048,#20423,.T.);
#48746=EDGE_CURVE('',#38048,#38045,#28851,.T.);
#48747=EDGE_CURVE('',#38049,#38050,#20424,.T.);
#48748=EDGE_CURVE('',#38050,#38051,#28852,.T.);
#48749=EDGE_CURVE('',#38051,#38052,#20425,.T.);
#48750=EDGE_CURVE('',#38052,#38049,#28853,.T.);
#48751=EDGE_CURVE('',#38053,#38054,#20426,.T.);
#48752=EDGE_CURVE('',#38054,#38055,#28854,.T.);
#48753=EDGE_CURVE('',#38055,#38056,#20427,.T.);
#48754=EDGE_CURVE('',#38056,#38053,#28855,.T.);
#48755=EDGE_CURVE('',#38020,#38057,#20428,.T.);
#48756=EDGE_CURVE('',#38057,#38058,#20429,.T.);
#48757=EDGE_CURVE('',#38058,#38057,#20430,.T.);
#48758=EDGE_CURVE('',#38059,#38059,#20431,.T.);
#48759=EDGE_CURVE('',#38059,#38060,#28856,.T.);
#48760=EDGE_CURVE('',#38060,#38061,#20432,.T.);
#48761=EDGE_CURVE('',#38061,#38062,#28857,.T.);
#48762=EDGE_CURVE('',#38062,#38063,#20433,.T.);
#48763=EDGE_CURVE('',#38063,#38058,#28858,.T.);
#48764=EDGE_CURVE('',#38063,#38064,#20434,.T.);
#48765=EDGE_CURVE('',#38064,#38065,#28859,.T.);
#48766=EDGE_CURVE('',#38065,#38060,#20435,.T.);
#48767=EDGE_CURVE('',#38066,#38067,#20436,.T.);
#48768=EDGE_CURVE('',#38067,#38068,#28860,.T.);
#48769=EDGE_CURVE('',#38068,#38069,#20437,.T.);
#48770=EDGE_CURVE('',#38069,#38066,#28861,.T.);
#48771=EDGE_CURVE('',#38070,#38071,#20438,.T.);
#48772=EDGE_CURVE('',#38071,#38072,#28862,.T.);
#48773=EDGE_CURVE('',#38072,#38073,#20439,.T.);
#48774=EDGE_CURVE('',#38073,#38070,#28863,.T.);
#48775=EDGE_CURVE('',#38074,#38075,#20440,.T.);
#48776=EDGE_CURVE('',#38075,#38076,#28864,.T.);
#48777=EDGE_CURVE('',#38076,#38077,#20441,.T.);
#48778=EDGE_CURVE('',#38077,#38074,#28865,.T.);
#48779=EDGE_CURVE('',#38078,#38079,#20442,.T.);
#48780=EDGE_CURVE('',#38079,#38080,#28866,.T.);
#48781=EDGE_CURVE('',#38080,#38081,#20443,.T.);
#48782=EDGE_CURVE('',#38081,#38078,#28867,.T.);
#48783=EDGE_CURVE('',#38082,#38083,#20444,.T.);
#48784=EDGE_CURVE('',#38083,#38084,#28868,.T.);
#48785=EDGE_CURVE('',#38084,#38085,#20445,.T.);
#48786=EDGE_CURVE('',#38085,#38082,#28869,.T.);
#48787=EDGE_CURVE('',#38086,#38087,#20446,.T.);
#48788=EDGE_CURVE('',#38087,#38088,#28870,.T.);
#48789=EDGE_CURVE('',#38088,#38089,#20447,.T.);
#48790=EDGE_CURVE('',#38089,#38086,#28871,.T.);
#48791=EDGE_CURVE('',#38090,#38091,#20448,.T.);
#48792=EDGE_CURVE('',#38091,#38092,#28872,.T.);
#48793=EDGE_CURVE('',#38092,#38093,#20449,.T.);
#48794=EDGE_CURVE('',#38093,#38090,#28873,.T.);
#48795=EDGE_CURVE('',#38094,#38094,#20450,.T.);
#48796=EDGE_CURVE('',#38094,#38059,#20451,.T.);
#48797=EDGE_CURVE('',#38095,#38095,#20452,.T.);
#48798=EDGE_CURVE('',#38095,#38026,#20453,.T.);
#48799=EDGE_CURVE('',#38069,#38031,#20454,.T.);
#48800=EDGE_CURVE('',#38032,#38068,#20455,.T.);
#48801=EDGE_CURVE('',#38067,#38029,#20456,.T.);
#48802=EDGE_CURVE('',#38030,#38066,#20457,.T.);
#48803=EDGE_CURVE('',#38073,#38035,#20458,.T.);
#48804=EDGE_CURVE('',#38036,#38072,#20459,.T.);
#48805=EDGE_CURVE('',#38071,#38033,#20460,.T.);
#48806=EDGE_CURVE('',#38034,#38070,#20461,.T.);
#48807=EDGE_CURVE('',#38077,#38039,#20462,.T.);
#48808=EDGE_CURVE('',#38040,#38076,#20463,.T.);
#48809=EDGE_CURVE('',#38075,#38037,#20464,.T.);
#48810=EDGE_CURVE('',#38038,#38074,#20465,.T.);
#48811=EDGE_CURVE('',#38061,#38023,#20466,.T.);
#48812=EDGE_CURVE('',#38027,#38065,#20467,.T.);
#48813=EDGE_CURVE('',#38064,#38028,#20468,.T.);
#48814=EDGE_CURVE('',#38022,#38062,#20469,.T.);
#48815=EDGE_CURVE('',#38081,#38043,#20470,.T.);
#48816=EDGE_CURVE('',#38044,#38080,#20471,.T.);
#48817=EDGE_CURVE('',#38079,#38041,#20472,.T.);
#48818=EDGE_CURVE('',#38042,#38078,#20473,.T.);
#48819=EDGE_CURVE('',#38085,#38047,#20474,.T.);
#48820=EDGE_CURVE('',#38048,#38084,#20475,.T.);
#48821=EDGE_CURVE('',#38083,#38045,#20476,.T.);
#48822=EDGE_CURVE('',#38046,#38082,#20477,.T.);
#48823=EDGE_CURVE('',#38089,#38051,#20478,.T.);
#48824=EDGE_CURVE('',#38052,#38088,#20479,.T.);
#48825=EDGE_CURVE('',#38087,#38049,#20480,.T.);
#48826=EDGE_CURVE('',#38050,#38086,#20481,.T.);
#48827=EDGE_CURVE('',#38093,#38055,#20482,.T.);
#48828=EDGE_CURVE('',#38056,#38092,#20483,.T.);
#48829=EDGE_CURVE('',#38091,#38053,#20484,.T.);
#48830=EDGE_CURVE('',#38054,#38090,#20485,.T.);
#48831=EDGE_CURVE('',#38096,#38096,#20486,.T.);
#48832=EDGE_CURVE('',#38096,#38097,#28874,.T.);
#48833=EDGE_CURVE('',#38097,#38097,#20487,.T.);
#48834=EDGE_CURVE('',#38098,#38098,#20488,.T.);
#48835=EDGE_CURVE('',#38098,#38096,#28875,.T.);
#48836=EDGE_CURVE('',#38098,#38099,#28876,.T.);
#48837=EDGE_CURVE('',#38099,#38099,#20489,.T.);
#48838=EDGE_CURVE('',#38100,#38100,#20490,.T.);
#48839=EDGE_CURVE('',#38100,#38101,#28877,.T.);
#48840=EDGE_CURVE('',#38101,#38101,#20491,.T.);
#48841=EDGE_CURVE('',#38102,#38102,#20492,.T.);
#48842=EDGE_CURVE('',#38102,#38100,#28878,.T.);
#48843=EDGE_CURVE('',#38102,#38103,#28879,.T.);
#48844=EDGE_CURVE('',#38103,#38103,#20493,.T.);
#48845=EDGE_CURVE('',#38104,#38104,#20494,.T.);
#48846=EDGE_CURVE('',#38104,#38105,#28880,.T.);
#48847=EDGE_CURVE('',#38105,#38105,#20495,.T.);
#48848=EDGE_CURVE('',#38106,#38106,#20496,.T.);
#48849=EDGE_CURVE('',#38106,#38104,#28881,.T.);
#48850=EDGE_CURVE('',#38106,#38107,#28882,.T.);
#48851=EDGE_CURVE('',#38107,#38107,#20497,.T.);
#48852=EDGE_CURVE('',#38108,#38108,#20498,.T.);
#48853=EDGE_CURVE('',#38108,#38109,#28883,.T.);
#48854=EDGE_CURVE('',#38109,#38109,#20499,.T.);
#48855=EDGE_CURVE('',#38110,#38110,#20500,.T.);
#48856=EDGE_CURVE('',#38110,#38108,#28884,.T.);
#48857=EDGE_CURVE('',#38110,#38111,#28885,.T.);
#48858=EDGE_CURVE('',#38111,#38111,#20501,.T.);
#48859=EDGE_CURVE('',#38112,#38112,#20502,.T.);
#48860=EDGE_CURVE('',#38112,#38113,#28886,.T.);
#48861=EDGE_CURVE('',#38113,#38113,#20503,.T.);
#48862=EDGE_CURVE('',#38114,#38114,#20504,.T.);
#48863=EDGE_CURVE('',#38114,#38112,#28887,.T.);
#48864=EDGE_CURVE('',#38114,#38115,#28888,.T.);
#48865=EDGE_CURVE('',#38115,#38115,#20505,.T.);
#48866=EDGE_CURVE('',#38116,#38116,#20506,.T.);
#48867=EDGE_CURVE('',#38116,#38117,#28889,.T.);
#48868=EDGE_CURVE('',#38117,#38117,#20507,.T.);
#48869=EDGE_CURVE('',#38118,#38118,#20508,.T.);
#48870=EDGE_CURVE('',#38118,#38116,#28890,.T.);
#48871=EDGE_CURVE('',#38118,#38119,#28891,.T.);
#48872=EDGE_CURVE('',#38119,#38119,#20509,.T.);
#48873=EDGE_CURVE('',#38120,#38120,#20510,.T.);
#48874=EDGE_CURVE('',#38120,#38121,#28892,.T.);
#48875=EDGE_CURVE('',#38121,#38121,#20511,.T.);
#48876=EDGE_CURVE('',#38122,#38122,#20512,.T.);
#48877=EDGE_CURVE('',#38122,#38120,#28893,.T.);
#48878=EDGE_CURVE('',#38122,#38123,#28894,.T.);
#48879=EDGE_CURVE('',#38123,#38123,#20513,.T.);
#48880=EDGE_CURVE('',#38124,#38124,#20514,.T.);
#48881=EDGE_CURVE('',#38124,#38125,#28895,.T.);
#48882=EDGE_CURVE('',#38125,#38125,#20515,.T.);
#48883=EDGE_CURVE('',#38126,#38126,#20516,.T.);
#48884=EDGE_CURVE('',#38126,#38124,#28896,.T.);
#48885=EDGE_CURVE('',#38126,#38127,#28897,.T.);
#48886=EDGE_CURVE('',#38127,#38127,#20517,.T.);
#48887=EDGE_CURVE('',#38128,#38129,#28898,.T.);
#48888=EDGE_CURVE('',#38128,#38130,#4112,.T.);
#48889=EDGE_CURVE('',#38130,#38131,#20518,.T.);
#48890=EDGE_CURVE('',#38129,#38131,#4113,.T.);
#48891=EDGE_CURVE('',#38132,#38133,#28899,.T.);
#48892=EDGE_CURVE('',#38132,#38128,#4114,.T.);
#48893=EDGE_CURVE('',#38133,#38129,#4115,.T.);
#48894=EDGE_CURVE('',#38134,#38135,#28900,.T.);
#48895=EDGE_CURVE('',#38134,#38132,#4116,.T.);
#48896=EDGE_CURVE('',#38135,#38133,#4117,.T.);
#48897=EDGE_CURVE('',#38136,#38137,#28901,.T.);
#48898=EDGE_CURVE('',#38136,#38134,#4118,.T.);
#48899=EDGE_CURVE('',#38137,#38135,#4119,.T.);
#48900=EDGE_CURVE('',#38138,#38139,#28902,.T.);
#48901=EDGE_CURVE('',#38138,#38136,#4120,.T.);
#48902=EDGE_CURVE('',#38139,#38137,#4121,.T.);
#48903=EDGE_CURVE('',#38140,#38141,#28903,.T.);
#48904=EDGE_CURVE('',#38140,#38138,#4122,.T.);
#48905=EDGE_CURVE('',#38141,#38139,#4123,.T.);
#48906=EDGE_CURVE('',#38142,#38143,#28904,.T.);
#48907=EDGE_CURVE('',#38142,#38140,#4124,.T.);
#48908=EDGE_CURVE('',#38143,#38141,#4125,.T.);
#48909=EDGE_CURVE('',#38144,#38145,#28905,.T.);
#48910=EDGE_CURVE('',#38144,#38142,#4126,.T.);
#48911=EDGE_CURVE('',#38145,#38143,#4127,.T.);
#48912=EDGE_CURVE('',#38146,#38147,#28906,.T.);
#48913=EDGE_CURVE('',#38146,#38144,#4128,.T.);
#48914=EDGE_CURVE('',#38147,#38145,#4129,.T.);
#48915=EDGE_CURVE('',#38148,#38149,#28907,.T.);
#48916=EDGE_CURVE('',#38148,#38146,#4130,.T.);
#48917=EDGE_CURVE('',#38149,#38147,#4131,.T.);
#48918=EDGE_CURVE('',#38150,#38151,#28908,.T.);
#48919=EDGE_CURVE('',#38150,#38148,#4132,.T.);
#48920=EDGE_CURVE('',#38151,#38149,#4133,.T.);
#48921=EDGE_CURVE('',#38152,#38153,#28909,.T.);
#48922=EDGE_CURVE('',#38152,#38150,#4134,.T.);
#48923=EDGE_CURVE('',#38153,#38151,#4135,.T.);
#48924=EDGE_CURVE('',#38154,#38155,#28910,.T.);
#48925=EDGE_CURVE('',#38154,#38152,#4136,.T.);
#48926=EDGE_CURVE('',#38155,#38153,#4137,.T.);
#48927=EDGE_CURVE('',#38156,#38157,#28911,.T.);
#48928=EDGE_CURVE('',#38156,#38154,#4138,.T.);
#48929=EDGE_CURVE('',#38157,#38155,#4139,.T.);
#48930=EDGE_CURVE('',#38158,#38159,#28912,.T.);
#48931=EDGE_CURVE('',#38158,#38156,#4140,.T.);
#48932=EDGE_CURVE('',#38159,#38157,#4141,.T.);
#48933=EDGE_CURVE('',#38160,#38161,#28913,.T.);
#48934=EDGE_CURVE('',#38160,#38158,#4142,.T.);
#48935=EDGE_CURVE('',#38161,#38159,#4143,.T.);
#48936=EDGE_CURVE('',#38162,#38163,#28914,.T.);
#48937=EDGE_CURVE('',#38162,#38160,#4144,.T.);
#48938=EDGE_CURVE('',#38163,#38161,#4145,.T.);
#48939=EDGE_CURVE('',#38164,#38165,#28915,.T.);
#48940=EDGE_CURVE('',#38164,#38162,#4146,.T.);
#48941=EDGE_CURVE('',#38165,#38163,#4147,.T.);
#48942=EDGE_CURVE('',#38166,#38167,#28916,.T.);
#48943=EDGE_CURVE('',#38166,#38164,#4148,.T.);
#48944=EDGE_CURVE('',#38167,#38165,#4149,.T.);
#48945=EDGE_CURVE('',#38168,#38169,#28917,.T.);
#48946=EDGE_CURVE('',#38168,#38166,#4150,.T.);
#48947=EDGE_CURVE('',#38169,#38167,#4151,.T.);
#48948=EDGE_CURVE('',#38170,#38171,#28918,.T.);
#48949=EDGE_CURVE('',#38170,#38168,#4152,.T.);
#48950=EDGE_CURVE('',#38171,#38169,#4153,.T.);
#48951=EDGE_CURVE('',#38172,#38173,#28919,.T.);
#48952=EDGE_CURVE('',#38172,#38170,#4154,.T.);
#48953=EDGE_CURVE('',#38173,#38171,#4155,.T.);
#48954=EDGE_CURVE('',#38174,#38175,#28920,.T.);
#48955=EDGE_CURVE('',#38174,#38172,#4156,.T.);
#48956=EDGE_CURVE('',#38175,#38173,#4157,.T.);
#48957=EDGE_CURVE('',#38176,#38177,#28921,.T.);
#48958=EDGE_CURVE('',#38176,#38174,#4158,.T.);
#48959=EDGE_CURVE('',#38177,#38175,#4159,.T.);
#48960=EDGE_CURVE('',#38178,#38179,#28922,.T.);
#48961=EDGE_CURVE('',#38178,#38176,#4160,.T.);
#48962=EDGE_CURVE('',#38179,#38177,#4161,.T.);
#48963=EDGE_CURVE('',#38180,#38181,#28923,.T.);
#48964=EDGE_CURVE('',#38180,#38178,#4162,.T.);
#48965=EDGE_CURVE('',#38181,#38179,#4163,.T.);
#48966=EDGE_CURVE('',#38182,#38183,#28924,.T.);
#48967=EDGE_CURVE('',#38182,#38180,#4164,.T.);
#48968=EDGE_CURVE('',#38183,#38181,#4165,.T.);
#48969=EDGE_CURVE('',#38184,#38185,#28925,.T.);
#48970=EDGE_CURVE('',#38184,#38182,#4166,.T.);
#48971=EDGE_CURVE('',#38185,#38183,#4167,.T.);
#48972=EDGE_CURVE('',#38186,#38187,#28926,.T.);
#48973=EDGE_CURVE('',#38186,#38184,#4168,.T.);
#48974=EDGE_CURVE('',#38187,#38185,#4169,.T.);
#48975=EDGE_CURVE('',#38188,#38189,#28927,.T.);
#48976=EDGE_CURVE('',#38188,#38186,#4170,.T.);
#48977=EDGE_CURVE('',#38189,#38187,#4171,.T.);
#48978=EDGE_CURVE('',#38190,#38191,#28928,.T.);
#48979=EDGE_CURVE('',#38190,#38188,#4172,.T.);
#48980=EDGE_CURVE('',#38191,#38189,#4173,.T.);
#48981=EDGE_CURVE('',#38192,#38193,#28929,.T.);
#48982=EDGE_CURVE('',#38194,#38192,#20519,.T.);
#48983=EDGE_CURVE('',#38194,#38190,#4174,.T.);
#48984=EDGE_CURVE('',#38193,#38191,#4175,.T.);
#48985=EDGE_CURVE('',#38195,#38196,#28930,.T.);
#48986=EDGE_CURVE('',#38195,#38197,#4176,.T.);
#48987=EDGE_CURVE('',#38197,#38198,#20520,.T.);
#48988=EDGE_CURVE('',#38196,#38198,#24563,.F.);
#48989=EDGE_CURVE('',#38199,#38200,#28931,.T.);
#48990=EDGE_CURVE('',#38199,#38195,#24564,.T.);
#48991=EDGE_CURVE('',#38200,#38196,#24565,.F.);
#48992=EDGE_CURVE('',#38201,#38202,#28932,.T.);
#48993=EDGE_CURVE('',#38201,#38199,#24566,.T.);
#48994=EDGE_CURVE('',#38202,#38200,#24567,.F.);
#48995=EDGE_CURVE('',#38203,#38204,#28933,.T.);
#48996=EDGE_CURVE('',#38203,#38201,#24568,.T.);
#48997=EDGE_CURVE('',#38204,#38202,#24569,.F.);
#48998=EDGE_CURVE('',#38205,#38206,#28934,.T.);
#48999=EDGE_CURVE('',#38205,#38203,#24570,.T.);
#49000=EDGE_CURVE('',#38206,#38204,#24571,.F.);
#49001=EDGE_CURVE('',#38207,#38208,#28935,.T.);
#49002=EDGE_CURVE('',#38207,#38205,#24572,.T.);
#49003=EDGE_CURVE('',#38208,#38206,#24573,.F.);
#49004=EDGE_CURVE('',#38209,#38210,#28936,.T.);
#49005=EDGE_CURVE('',#38209,#38207,#24574,.T.);
#49006=EDGE_CURVE('',#38210,#38208,#24575,.F.);
#49007=EDGE_CURVE('',#38211,#38212,#28937,.T.);
#49008=EDGE_CURVE('',#38211,#38209,#24576,.T.);
#49009=EDGE_CURVE('',#38212,#38210,#24577,.F.);
#49010=EDGE_CURVE('',#38213,#38214,#28938,.T.);
#49011=EDGE_CURVE('',#38213,#38211,#24578,.T.);
#49012=EDGE_CURVE('',#38214,#38212,#24579,.F.);
#49013=EDGE_CURVE('',#38215,#38216,#28939,.T.);
#49014=EDGE_CURVE('',#38215,#38213,#24580,.T.);
#49015=EDGE_CURVE('',#38216,#38214,#24581,.F.);
#49016=EDGE_CURVE('',#38217,#38218,#28940,.T.);
#49017=EDGE_CURVE('',#38217,#38215,#24582,.T.);
#49018=EDGE_CURVE('',#38218,#38216,#24583,.F.);
#49019=EDGE_CURVE('',#38219,#38220,#28941,.T.);
#49020=EDGE_CURVE('',#38219,#38217,#24584,.T.);
#49021=EDGE_CURVE('',#38220,#38218,#24585,.F.);
#49022=EDGE_CURVE('',#38221,#38222,#28942,.T.);
#49023=EDGE_CURVE('',#38221,#38219,#24586,.T.);
#49024=EDGE_CURVE('',#38222,#38220,#24587,.F.);
#49025=EDGE_CURVE('',#38223,#38224,#28943,.T.);
#49026=EDGE_CURVE('',#38223,#38221,#24588,.T.);
#49027=EDGE_CURVE('',#38224,#38222,#24589,.F.);
#49028=EDGE_CURVE('',#38225,#38226,#28944,.T.);
#49029=EDGE_CURVE('',#38225,#38223,#24590,.T.);
#49030=EDGE_CURVE('',#38226,#38224,#24591,.F.);
#49031=EDGE_CURVE('',#38227,#38228,#28945,.T.);
#49032=EDGE_CURVE('',#38227,#38225,#24592,.T.);
#49033=EDGE_CURVE('',#38228,#38226,#24593,.F.);
#49034=EDGE_CURVE('',#38229,#38230,#28946,.T.);
#49035=EDGE_CURVE('',#38229,#38227,#24594,.T.);
#49036=EDGE_CURVE('',#38230,#38228,#24595,.F.);
#49037=EDGE_CURVE('',#38231,#38232,#28947,.T.);
#49038=EDGE_CURVE('',#38231,#38229,#24596,.T.);
#49039=EDGE_CURVE('',#38232,#38230,#24597,.F.);
#49040=EDGE_CURVE('',#38233,#38234,#28948,.T.);
#49041=EDGE_CURVE('',#38233,#38231,#24598,.T.);
#49042=EDGE_CURVE('',#38234,#38232,#24599,.F.);
#49043=EDGE_CURVE('',#38235,#38236,#28949,.T.);
#49044=EDGE_CURVE('',#38235,#38233,#24600,.T.);
#49045=EDGE_CURVE('',#38236,#38234,#24601,.F.);
#49046=EDGE_CURVE('',#38237,#38238,#28950,.T.);
#49047=EDGE_CURVE('',#38237,#38235,#24602,.T.);
#49048=EDGE_CURVE('',#38238,#38236,#24603,.F.);
#49049=EDGE_CURVE('',#38239,#38240,#28951,.T.);
#49050=EDGE_CURVE('',#38239,#38237,#24604,.T.);
#49051=EDGE_CURVE('',#38240,#38238,#24605,.F.);
#49052=EDGE_CURVE('',#38241,#38242,#28952,.T.);
#49053=EDGE_CURVE('',#38241,#38239,#24606,.T.);
#49054=EDGE_CURVE('',#38242,#38240,#24607,.F.);
#49055=EDGE_CURVE('',#38243,#38244,#28953,.T.);
#49056=EDGE_CURVE('',#38243,#38241,#24608,.T.);
#49057=EDGE_CURVE('',#38244,#38242,#24609,.F.);
#49058=EDGE_CURVE('',#38245,#38246,#28954,.T.);
#49059=EDGE_CURVE('',#38245,#38243,#24610,.T.);
#49060=EDGE_CURVE('',#38246,#38244,#24611,.F.);
#49061=EDGE_CURVE('',#38247,#38248,#28955,.T.);
#49062=EDGE_CURVE('',#38247,#38245,#24612,.T.);
#49063=EDGE_CURVE('',#38248,#38246,#24613,.F.);
#49064=EDGE_CURVE('',#38249,#38250,#28956,.T.);
#49065=EDGE_CURVE('',#38249,#38247,#24614,.T.);
#49066=EDGE_CURVE('',#38250,#38248,#24615,.F.);
#49067=EDGE_CURVE('',#38251,#38252,#28957,.T.);
#49068=EDGE_CURVE('',#38251,#38249,#24616,.T.);
#49069=EDGE_CURVE('',#38252,#38250,#24617,.F.);
#49070=EDGE_CURVE('',#38253,#38254,#28958,.T.);
#49071=EDGE_CURVE('',#38253,#38251,#24618,.T.);
#49072=EDGE_CURVE('',#38254,#38252,#24619,.F.);
#49073=EDGE_CURVE('',#38255,#38256,#28959,.T.);
#49074=EDGE_CURVE('',#38255,#38253,#24620,.T.);
#49075=EDGE_CURVE('',#38256,#38254,#24621,.F.);
#49076=EDGE_CURVE('',#38257,#38258,#28960,.T.);
#49077=EDGE_CURVE('',#38257,#38255,#24622,.T.);
#49078=EDGE_CURVE('',#38258,#38256,#24623,.F.);
#49079=EDGE_CURVE('',#38259,#38260,#4177,.F.);
#49080=EDGE_CURVE('',#38259,#38260,#20521,.T.);
#49081=EDGE_CURVE('',#38261,#38261,#20522,.T.);
#49082=EDGE_CURVE('',#38262,#38262,#20523,.T.);
#49083=EDGE_CURVE('',#38263,#38263,#20524,.T.);
#49084=EDGE_CURVE('',#38263,#38264,#28961,.T.);
#49085=EDGE_CURVE('',#38264,#38264,#20525,.T.);
#49086=EDGE_CURVE('',#38192,#38265,#20526,.T.);
#49087=EDGE_CURVE('',#38265,#38266,#24624,.T.);
#49088=EDGE_CURVE('',#38267,#38266,#20527,.T.);
#49089=EDGE_CURVE('',#38267,#38268,#24625,.T.);
#49090=EDGE_CURVE('',#38268,#38269,#28962,.T.);
#49091=EDGE_CURVE('',#38269,#38269,#20528,.T.);
#49092=EDGE_CURVE('',#38268,#38194,#24626,.T.);
#49093=EDGE_CURVE('',#38270,#38258,#24627,.F.);
#49094=EDGE_CURVE('',#38267,#38270,#4178,.T.);
#49095=EDGE_CURVE('',#38266,#38257,#24628,.T.);
#49096=EDGE_CURVE('',#38131,#38197,#24629,.T.);
#49097=EDGE_CURVE('',#38198,#38130,#24630,.T.);
#49098=EDGE_CURVE('',#38271,#38272,#20529,.T.);
#49099=EDGE_CURVE('',#38273,#38271,#20530,.T.);
#49100=EDGE_CURVE('',#38260,#38273,#20531,.T.);
#49101=EDGE_CURVE('',#38274,#38259,#20532,.T.);
#49102=EDGE_CURVE('',#38272,#38274,#20533,.T.);
#49103=EDGE_CURVE('',#38260,#38273,#4179,.T.);
#49104=EDGE_CURVE('',#38273,#38271,#4180,.T.);
#49105=EDGE_CURVE('',#38271,#38272,#4181,.T.);
#49106=EDGE_CURVE('',#38272,#38274,#4182,.T.);
#49107=EDGE_CURVE('',#38274,#38259,#4183,.T.);
#49108=EDGE_CURVE('',#38275,#38276,#28963,.T.);
#49109=EDGE_CURVE('',#38276,#38277,#28964,.T.);
#49110=EDGE_CURVE('',#38277,#38278,#28965,.T.);
#49111=EDGE_CURVE('',#38278,#38279,#28966,.T.);
#49112=EDGE_CURVE('',#38279,#38280,#28967,.T.);
#49113=EDGE_CURVE('',#38280,#38275,#28968,.T.);
#49114=EDGE_CURVE('',#38276,#38259,#28969,.T.);
#49115=EDGE_CURVE('',#38277,#38260,#28970,.T.);
#49116=EDGE_CURVE('',#38278,#38273,#28971,.T.);
#49117=EDGE_CURVE('',#38279,#38271,#28972,.T.);
#49118=EDGE_CURVE('',#38280,#38272,#28973,.T.);
#49119=EDGE_CURVE('',#38275,#38274,#28974,.T.);
#49120=EDGE_CURVE('',#38265,#38193,#4184,.T.);
#49121=EDGE_CURVE('',#38281,#38282,#186,.T.);
#49122=EDGE_CURVE('',#38281,#38283,#24631,.T.);
#49123=EDGE_CURVE('',#38284,#38283,#187,.T.);
#49124=EDGE_CURVE('',#38285,#38284,#24632,.T.);
#49125=EDGE_CURVE('',#38282,#38285,#188,.T.);
#49126=EDGE_CURVE('',#38286,#38287,#189,.T.);
#49127=EDGE_CURVE('',#38287,#38288,#190,.T.);
#49128=EDGE_CURVE('',#38288,#38281,#24633,.T.);
#49129=EDGE_CURVE('',#38286,#38285,#24634,.T.);
#49130=EDGE_CURVE('',#38289,#38290,#191,.T.);
#49131=EDGE_CURVE('',#38289,#38288,#24635,.T.);
#49132=EDGE_CURVE('',#38290,#38286,#24636,.T.);
#49133=EDGE_CURVE('',#38290,#38289,#192,.T.);
#49134=EDGE_CURVE('',#38291,#38286,#193,.T.);
#49135=EDGE_CURVE('',#38288,#38291,#194,.T.);
#49136=EDGE_CURVE('',#38285,#38292,#195,.T.);
#49137=EDGE_CURVE('',#38292,#38281,#196,.T.);
#49138=EDGE_CURVE('',#38283,#38284,#197,.T.);
#49139=EDGE_CURVE('',#38293,#38293,#20534,.T.);
#49140=EDGE_CURVE('',#38293,#38294,#28975,.T.);
#49141=EDGE_CURVE('',#38294,#38294,#20535,.T.);
#49142=EDGE_CURVE('',#38295,#38295,#20536,.T.);
#49143=EDGE_CURVE('',#38295,#38293,#20537,.T.);
#49144=EDGE_CURVE('',#38296,#38296,#20538,.T.);
#49145=EDGE_CURVE('',#38296,#38295,#28976,.T.);
#49146=EDGE_CURVE('',#38297,#38297,#20539,.T.);
#49147=EDGE_CURVE('',#38297,#38298,#28977,.T.);
#49148=EDGE_CURVE('',#38298,#38298,#20540,.T.);
#49149=EDGE_CURVE('',#38299,#38300,#20541,.T.);
#49150=EDGE_CURVE('',#38300,#38299,#20542,.T.);
#49151=EDGE_CURVE('',#38300,#38297,#28978,.T.);
#49152=EDGE_CURVE('',#38299,#38301,#28979,.T.);
#49153=EDGE_CURVE('',#38301,#38301,#20543,.T.);
#49154=EDGE_CURVE('',#38302,#38302,#20544,.T.);
#49155=EDGE_CURVE('',#38302,#38303,#20545,.T.);
#49156=EDGE_CURVE('',#38303,#38303,#20546,.T.);
#49157=EDGE_CURVE('',#38304,#38304,#20547,.T.);
#49158=EDGE_CURVE('',#38304,#38305,#28980,.T.);
#49159=EDGE_CURVE('',#38305,#38305,#20548,.T.);
#49160=EDGE_CURVE('',#38306,#38307,#20549,.T.);
#49161=EDGE_CURVE('',#38307,#38306,#20550,.T.);
#49162=EDGE_CURVE('',#38307,#38304,#28981,.T.);
#49163=EDGE_CURVE('',#38306,#38308,#28982,.T.);
#49164=EDGE_CURVE('',#38308,#38308,#20551,.T.);
#49165=EDGE_CURVE('',#38303,#38309,#28983,.T.);
#49166=EDGE_CURVE('',#38309,#38309,#20552,.T.);
#49167=EDGE_CURVE('',#38310,#38310,#20553,.T.);
#49168=EDGE_CURVE('',#38310,#38302,#28984,.T.);
#49169=EDGE_CURVE('',#38311,#38312,#20554,.T.);
#49170=EDGE_CURVE('',#38313,#38314,#20555,.T.);
#49171=EDGE_CURVE('',#38315,#38316,#20556,.T.);
#49172=EDGE_CURVE('',#38317,#38318,#20557,.T.);
#49173=EDGE_CURVE('',#38319,#38320,#20558,.T.);
#49174=EDGE_CURVE('',#38321,#38322,#20559,.T.);
#49175=EDGE_CURVE('',#38323,#38324,#20560,.T.);
#49176=EDGE_CURVE('',#38325,#38326,#20561,.T.);
#49177=EDGE_CURVE('',#38327,#38328,#20562,.T.);
#49178=EDGE_CURVE('',#38329,#38330,#20563,.T.);
#49179=EDGE_CURVE('',#38331,#38332,#20564,.T.);
#49180=EDGE_CURVE('',#38333,#38334,#20565,.T.);
#49181=EDGE_CURVE('',#38335,#38335,#20566,.T.);
#49182=EDGE_CURVE('',#38335,#38336,#28985,.T.);
#49183=EDGE_CURVE('',#38336,#38336,#20567,.T.);
#49184=EDGE_CURVE('',#38337,#38337,#20568,.T.);
#49185=EDGE_CURVE('',#38337,#38338,#28986,.T.);
#49186=EDGE_CURVE('',#38338,#38338,#20569,.T.);
#49187=EDGE_CURVE('',#38339,#38339,#20570,.T.);
#49188=EDGE_CURVE('',#38339,#38340,#28987,.T.);
#49189=EDGE_CURVE('',#38340,#38340,#20571,.T.);
#49190=EDGE_CURVE('',#38341,#38341,#20572,.T.);
#49191=EDGE_CURVE('',#38341,#38342,#28988,.T.);
#49192=EDGE_CURVE('',#38342,#38342,#20573,.T.);
#49193=EDGE_CURVE('',#38343,#38344,#28989,.T.);
#49194=EDGE_CURVE('',#38345,#38343,#4185,.T.);
#49195=EDGE_CURVE('',#38344,#38345,#20574,.T.);
#49196=EDGE_CURVE('',#38346,#38347,#28990,.T.);
#49197=EDGE_CURVE('',#38343,#38346,#4186,.T.);
#49198=EDGE_CURVE('',#38348,#38344,#20575,.T.);
#49199=EDGE_CURVE('',#38348,#38347,#4187,.T.);
#49200=EDGE_CURVE('',#38349,#38350,#28991,.T.);
#49201=EDGE_CURVE('',#38346,#38349,#4188,.T.);
#49202=EDGE_CURVE('',#38347,#38350,#4189,.T.);
#49203=EDGE_CURVE('',#38351,#38352,#28992,.T.);
#49204=EDGE_CURVE('',#38349,#38351,#4190,.T.);
#49205=EDGE_CURVE('',#38350,#38352,#4191,.T.);
#49206=EDGE_CURVE('',#38353,#38354,#28993,.T.);
#49207=EDGE_CURVE('',#38351,#38353,#4192,.T.);
#49208=EDGE_CURVE('',#38352,#38354,#4193,.T.);
#49209=EDGE_CURVE('',#38355,#38356,#28994,.T.);
#49210=EDGE_CURVE('',#38353,#38355,#4194,.T.);
#49211=EDGE_CURVE('',#38354,#38356,#4195,.T.);
#49212=EDGE_CURVE('',#38357,#38358,#28995,.T.);
#49213=EDGE_CURVE('',#38355,#38357,#4196,.T.);
#49214=EDGE_CURVE('',#38356,#38358,#4197,.T.);
#49215=EDGE_CURVE('',#38359,#38360,#28996,.T.);
#49216=EDGE_CURVE('',#38357,#38359,#4198,.T.);
#49217=EDGE_CURVE('',#38358,#38360,#4199,.T.);
#49218=EDGE_CURVE('',#38361,#38362,#28997,.T.);
#49219=EDGE_CURVE('',#38359,#38361,#4200,.T.);
#49220=EDGE_CURVE('',#38360,#38362,#4201,.T.);
#49221=EDGE_CURVE('',#38363,#38364,#28998,.T.);
#49222=EDGE_CURVE('',#38361,#38363,#4202,.T.);
#49223=EDGE_CURVE('',#38362,#38364,#4203,.T.);
#49224=EDGE_CURVE('',#38365,#38366,#28999,.T.);
#49225=EDGE_CURVE('',#38363,#38365,#4204,.T.);
#49226=EDGE_CURVE('',#38364,#38366,#4205,.T.);
#49227=EDGE_CURVE('',#38367,#38368,#29000,.T.);
#49228=EDGE_CURVE('',#38365,#38367,#4206,.T.);
#49229=EDGE_CURVE('',#38366,#38368,#4207,.T.);
#49230=EDGE_CURVE('',#38369,#38370,#29001,.T.);
#49231=EDGE_CURVE('',#38367,#38369,#4208,.T.);
#49232=EDGE_CURVE('',#38368,#38370,#4209,.T.);
#49233=EDGE_CURVE('',#38371,#38372,#29002,.T.);
#49234=EDGE_CURVE('',#38369,#38371,#4210,.T.);
#49235=EDGE_CURVE('',#38370,#38372,#4211,.T.);
#49236=EDGE_CURVE('',#38373,#38374,#29003,.T.);
#49237=EDGE_CURVE('',#38371,#38373,#4212,.T.);
#49238=EDGE_CURVE('',#38372,#38374,#4213,.T.);
#49239=EDGE_CURVE('',#38375,#38376,#29004,.T.);
#49240=EDGE_CURVE('',#38373,#38375,#4214,.T.);
#49241=EDGE_CURVE('',#38374,#38376,#4215,.T.);
#49242=EDGE_CURVE('',#38377,#38378,#29005,.T.);
#49243=EDGE_CURVE('',#38377,#38379,#24637,.T.);
#49244=EDGE_CURVE('',#38379,#38380,#20576,.T.);
#49245=EDGE_CURVE('',#38378,#38380,#24638,.F.);
#49246=EDGE_CURVE('',#38381,#38382,#29006,.T.);
#49247=EDGE_CURVE('',#38381,#38377,#24639,.T.);
#49248=EDGE_CURVE('',#38382,#38378,#24640,.F.);
#49249=EDGE_CURVE('',#38383,#38384,#29007,.T.);
#49250=EDGE_CURVE('',#38383,#38381,#24641,.T.);
#49251=EDGE_CURVE('',#38384,#38382,#24642,.F.);
#49252=EDGE_CURVE('',#38385,#38386,#29008,.T.);
#49253=EDGE_CURVE('',#38385,#38383,#24643,.T.);
#49254=EDGE_CURVE('',#38386,#38384,#24644,.F.);
#49255=EDGE_CURVE('',#38387,#38388,#29009,.T.);
#49256=EDGE_CURVE('',#38387,#38385,#24645,.T.);
#49257=EDGE_CURVE('',#38388,#38386,#24646,.F.);
#49258=EDGE_CURVE('',#38389,#38390,#29010,.T.);
#49259=EDGE_CURVE('',#38389,#38387,#24647,.T.);
#49260=EDGE_CURVE('',#38390,#38388,#24648,.F.);
#49261=EDGE_CURVE('',#38391,#38392,#29011,.T.);
#49262=EDGE_CURVE('',#38391,#38389,#24649,.T.);
#49263=EDGE_CURVE('',#38392,#38390,#24650,.F.);
#49264=EDGE_CURVE('',#38393,#38394,#29012,.T.);
#49265=EDGE_CURVE('',#38393,#38391,#24651,.T.);
#49266=EDGE_CURVE('',#38394,#38392,#24652,.F.);
#49267=EDGE_CURVE('',#38395,#38396,#29013,.T.);
#49268=EDGE_CURVE('',#38395,#38393,#24653,.T.);
#49269=EDGE_CURVE('',#38396,#38394,#24654,.F.);
#49270=EDGE_CURVE('',#38397,#38398,#29014,.T.);
#49271=EDGE_CURVE('',#38397,#38395,#24655,.T.);
#49272=EDGE_CURVE('',#38398,#38396,#24656,.F.);
#49273=EDGE_CURVE('',#38399,#38400,#29015,.T.);
#49274=EDGE_CURVE('',#38399,#38397,#24657,.T.);
#49275=EDGE_CURVE('',#38400,#38398,#24658,.F.);
#49276=EDGE_CURVE('',#38401,#38402,#29016,.T.);
#49277=EDGE_CURVE('',#38401,#38399,#24659,.T.);
#49278=EDGE_CURVE('',#38402,#38400,#24660,.F.);
#49279=EDGE_CURVE('',#38403,#38404,#29017,.T.);
#49280=EDGE_CURVE('',#38403,#38401,#24661,.T.);
#49281=EDGE_CURVE('',#38404,#38402,#24662,.F.);
#49282=EDGE_CURVE('',#38405,#38406,#29018,.T.);
#49283=EDGE_CURVE('',#38405,#38403,#24663,.T.);
#49284=EDGE_CURVE('',#38406,#38404,#24664,.F.);
#49285=EDGE_CURVE('',#38407,#38408,#29019,.T.);
#49286=EDGE_CURVE('',#38407,#38405,#24665,.T.);
#49287=EDGE_CURVE('',#38408,#38406,#24666,.F.);
#49288=EDGE_CURVE('',#38409,#38410,#4216,.F.);
#49289=EDGE_CURVE('',#38409,#38410,#20577,.T.);
#49290=EDGE_CURVE('',#38411,#38411,#20578,.T.);
#49291=EDGE_CURVE('',#38412,#38412,#20579,.T.);
#49292=EDGE_CURVE('',#38413,#38413,#20580,.T.);
#49293=EDGE_CURVE('',#38413,#38414,#29020,.T.);
#49294=EDGE_CURVE('',#38414,#38414,#20581,.T.);
#49295=EDGE_CURVE('',#38345,#38415,#24667,.T.);
#49296=EDGE_CURVE('',#38416,#38415,#20582,.T.);
#49297=EDGE_CURVE('',#38416,#38417,#24668,.T.);
#49298=EDGE_CURVE('',#38417,#38418,#29021,.T.);
#49299=EDGE_CURVE('',#38418,#38418,#20583,.T.);
#49300=EDGE_CURVE('',#38417,#38348,#24669,.T.);
#49301=EDGE_CURVE('',#38416,#38408,#24670,.F.);
#49302=EDGE_CURVE('',#38415,#38407,#24671,.T.);
#49303=EDGE_CURVE('',#38419,#38379,#24672,.T.);
#49304=EDGE_CURVE('',#38420,#38419,#20584,.T.);
#49305=EDGE_CURVE('',#38380,#38420,#24673,.T.);
#49306=EDGE_CURVE('',#38421,#38422,#20585,.T.);
#49307=EDGE_CURVE('',#38423,#38421,#20586,.T.);
#49308=EDGE_CURVE('',#38410,#38423,#20587,.T.);
#49309=EDGE_CURVE('',#38424,#38409,#20588,.T.);
#49310=EDGE_CURVE('',#38422,#38424,#20589,.T.);
#49311=EDGE_CURVE('',#38410,#38423,#4217,.T.);
#49312=EDGE_CURVE('',#38423,#38421,#4218,.T.);
#49313=EDGE_CURVE('',#38421,#38422,#4219,.T.);
#49314=EDGE_CURVE('',#38422,#38424,#4220,.T.);
#49315=EDGE_CURVE('',#38424,#38409,#4221,.T.);
#49316=EDGE_CURVE('',#38425,#38426,#29022,.T.);
#49317=EDGE_CURVE('',#38426,#38427,#29023,.T.);
#49318=EDGE_CURVE('',#38427,#38428,#29024,.T.);
#49319=EDGE_CURVE('',#38428,#38429,#29025,.T.);
#49320=EDGE_CURVE('',#38429,#38430,#29026,.T.);
#49321=EDGE_CURVE('',#38430,#38425,#29027,.T.);
#49322=EDGE_CURVE('',#38426,#38409,#29028,.T.);
#49323=EDGE_CURVE('',#38427,#38410,#29029,.T.);
#49324=EDGE_CURVE('',#38428,#38423,#29030,.T.);
#49325=EDGE_CURVE('',#38429,#38421,#29031,.T.);
#49326=EDGE_CURVE('',#38430,#38422,#29032,.T.);
#49327=EDGE_CURVE('',#38425,#38424,#29033,.T.);
#49328=EDGE_CURVE('',#38376,#38420,#4222,.T.);
#49329=EDGE_CURVE('',#38375,#38419,#4223,.T.);
#49330=EDGE_CURVE('',#38431,#38432,#29034,.T.);
#49331=EDGE_CURVE('',#38431,#38433,#4224,.T.);
#49332=EDGE_CURVE('',#38433,#38434,#20590,.T.);
#49333=EDGE_CURVE('',#38432,#38434,#4225,.T.);
#49334=EDGE_CURVE('',#38435,#38436,#29035,.T.);
#49335=EDGE_CURVE('',#38435,#38431,#4226,.T.);
#49336=EDGE_CURVE('',#38436,#38432,#4227,.T.);
#49337=EDGE_CURVE('',#38437,#38438,#29036,.T.);
#49338=EDGE_CURVE('',#38437,#38435,#4228,.T.);
#49339=EDGE_CURVE('',#38438,#38436,#4229,.T.);
#49340=EDGE_CURVE('',#38439,#38440,#29037,.T.);
#49341=EDGE_CURVE('',#38439,#38437,#4230,.T.);
#49342=EDGE_CURVE('',#38440,#38438,#4231,.T.);
#49343=EDGE_CURVE('',#38441,#38442,#29038,.T.);
#49344=EDGE_CURVE('',#38441,#38439,#4232,.T.);
#49345=EDGE_CURVE('',#38442,#38440,#4233,.T.);
#49346=EDGE_CURVE('',#38443,#38444,#29039,.T.);
#49347=EDGE_CURVE('',#38443,#38441,#4234,.T.);
#49348=EDGE_CURVE('',#38444,#38442,#4235,.T.);
#49349=EDGE_CURVE('',#38445,#38446,#29040,.T.);
#49350=EDGE_CURVE('',#38445,#38443,#4236,.T.);
#49351=EDGE_CURVE('',#38446,#38444,#4237,.T.);
#49352=EDGE_CURVE('',#38447,#38448,#29041,.T.);
#49353=EDGE_CURVE('',#38447,#38445,#4238,.T.);
#49354=EDGE_CURVE('',#38448,#38446,#4239,.T.);
#49355=EDGE_CURVE('',#38449,#38450,#29042,.T.);
#49356=EDGE_CURVE('',#38449,#38447,#4240,.T.);
#49357=EDGE_CURVE('',#38450,#38448,#4241,.T.);
#49358=EDGE_CURVE('',#38451,#38452,#29043,.T.);
#49359=EDGE_CURVE('',#38451,#38449,#4242,.T.);
#49360=EDGE_CURVE('',#38452,#38450,#4243,.T.);
#49361=EDGE_CURVE('',#38453,#38454,#29044,.T.);
#49362=EDGE_CURVE('',#38453,#38451,#4244,.T.);
#49363=EDGE_CURVE('',#38454,#38452,#4245,.T.);
#49364=EDGE_CURVE('',#38455,#38456,#29045,.T.);
#49365=EDGE_CURVE('',#38455,#38453,#4246,.T.);
#49366=EDGE_CURVE('',#38456,#38454,#4247,.T.);
#49367=EDGE_CURVE('',#38457,#38458,#29046,.T.);
#49368=EDGE_CURVE('',#38457,#38455,#4248,.T.);
#49369=EDGE_CURVE('',#38458,#38456,#4249,.T.);
#49370=EDGE_CURVE('',#38459,#38460,#29047,.T.);
#49371=EDGE_CURVE('',#38459,#38457,#4250,.T.);
#49372=EDGE_CURVE('',#38460,#38458,#4251,.T.);
#49373=EDGE_CURVE('',#38461,#38462,#29048,.T.);
#49374=EDGE_CURVE('',#38463,#38461,#20591,.T.);
#49375=EDGE_CURVE('',#38463,#38459,#4252,.T.);
#49376=EDGE_CURVE('',#38462,#38460,#4253,.T.);
#49377=EDGE_CURVE('',#38464,#38465,#29049,.T.);
#49378=EDGE_CURVE('',#38466,#38464,#24674,.F.);
#49379=EDGE_CURVE('',#38466,#38467,#20592,.T.);
#49380=EDGE_CURVE('',#38467,#38465,#24675,.T.);
#49381=EDGE_CURVE('',#38468,#38469,#29050,.T.);
#49382=EDGE_CURVE('',#38464,#38468,#24676,.F.);
#49383=EDGE_CURVE('',#38465,#38469,#24677,.T.);
#49384=EDGE_CURVE('',#38470,#38471,#29051,.T.);
#49385=EDGE_CURVE('',#38468,#38470,#24678,.F.);
#49386=EDGE_CURVE('',#38469,#38471,#24679,.T.);
#49387=EDGE_CURVE('',#38472,#38473,#29052,.T.);
#49388=EDGE_CURVE('',#38470,#38472,#24680,.F.);
#49389=EDGE_CURVE('',#38471,#38473,#24681,.T.);
#49390=EDGE_CURVE('',#38474,#38475,#29053,.T.);
#49391=EDGE_CURVE('',#38472,#38474,#24682,.F.);
#49392=EDGE_CURVE('',#38473,#38475,#24683,.T.);
#49393=EDGE_CURVE('',#38476,#38477,#29054,.T.);
#49394=EDGE_CURVE('',#38474,#38476,#24684,.F.);
#49395=EDGE_CURVE('',#38475,#38477,#24685,.T.);
#49396=EDGE_CURVE('',#38478,#38479,#29055,.T.);
#49397=EDGE_CURVE('',#38476,#38478,#24686,.F.);
#49398=EDGE_CURVE('',#38477,#38479,#24687,.T.);
#49399=EDGE_CURVE('',#38480,#38481,#29056,.T.);
#49400=EDGE_CURVE('',#38478,#38480,#24688,.F.);
#49401=EDGE_CURVE('',#38479,#38481,#24689,.T.);
#49402=EDGE_CURVE('',#38482,#38483,#29057,.T.);
#49403=EDGE_CURVE('',#38480,#38482,#24690,.F.);
#49404=EDGE_CURVE('',#38481,#38483,#24691,.T.);
#49405=EDGE_CURVE('',#38484,#38485,#29058,.T.);
#49406=EDGE_CURVE('',#38482,#38484,#24692,.F.);
#49407=EDGE_CURVE('',#38483,#38485,#24693,.T.);
#49408=EDGE_CURVE('',#38486,#38487,#29059,.T.);
#49409=EDGE_CURVE('',#38484,#38486,#24694,.F.);
#49410=EDGE_CURVE('',#38485,#38487,#24695,.T.);
#49411=EDGE_CURVE('',#38488,#38489,#29060,.T.);
#49412=EDGE_CURVE('',#38486,#38488,#24696,.F.);
#49413=EDGE_CURVE('',#38487,#38489,#24697,.T.);
#49414=EDGE_CURVE('',#38490,#38491,#29061,.T.);
#49415=EDGE_CURVE('',#38488,#38490,#24698,.F.);
#49416=EDGE_CURVE('',#38489,#38491,#24699,.T.);
#49417=EDGE_CURVE('',#38492,#38493,#29062,.T.);
#49418=EDGE_CURVE('',#38490,#38492,#24700,.F.);
#49419=EDGE_CURVE('',#38491,#38493,#24701,.T.);
#49420=EDGE_CURVE('',#38461,#38494,#20593,.T.);
#49421=EDGE_CURVE('',#38494,#38467,#24702,.T.);
#49422=EDGE_CURVE('',#38466,#38495,#24703,.T.);
#49423=EDGE_CURVE('',#38495,#38496,#29063,.T.);
#49424=EDGE_CURVE('',#38496,#38496,#20594,.T.);
#49425=EDGE_CURVE('',#38495,#38463,#24704,.T.);
#49426=EDGE_CURVE('',#38493,#38497,#24705,.T.);
#49427=EDGE_CURVE('',#38498,#38497,#20595,.T.);
#49428=EDGE_CURVE('',#38492,#38498,#24706,.F.);
#49429=EDGE_CURVE('',#38499,#38500,#4254,.T.);
#49430=EDGE_CURVE('',#38499,#38500,#20596,.T.);
#49431=EDGE_CURVE('',#38501,#38501,#20597,.T.);
#49432=EDGE_CURVE('',#38501,#38502,#29064,.T.);
#49433=EDGE_CURVE('',#38502,#38502,#20598,.T.);
#49434=EDGE_CURVE('',#38502,#38503,#29065,.T.);
#49435=EDGE_CURVE('',#38503,#38504,#20599,.T.);
#49436=EDGE_CURVE('',#38498,#38504,#24707,.T.);
#49437=EDGE_CURVE('',#38505,#38497,#24708,.T.);
#49438=EDGE_CURVE('',#38505,#38503,#20600,.T.);
#49439=EDGE_CURVE('',#38500,#38506,#20601,.T.);
#49440=EDGE_CURVE('',#38506,#38507,#20602,.T.);
#49441=EDGE_CURVE('',#38507,#38508,#20603,.T.);
#49442=EDGE_CURVE('',#38508,#38509,#20604,.T.);
#49443=EDGE_CURVE('',#38509,#38499,#20605,.T.);
#49444=EDGE_CURVE('',#38504,#38433,#24709,.T.);
#49445=EDGE_CURVE('',#38434,#38505,#24710,.T.);
#49446=EDGE_CURVE('',#38507,#38508,#4255,.T.);
#49447=EDGE_CURVE('',#38506,#38507,#4256,.T.);
#49448=EDGE_CURVE('',#38500,#38506,#4257,.T.);
#49449=EDGE_CURVE('',#38509,#38499,#4258,.T.);
#49450=EDGE_CURVE('',#38508,#38509,#4259,.T.);
#49451=EDGE_CURVE('',#38510,#38511,#29066,.T.);
#49452=EDGE_CURVE('',#38511,#38512,#29067,.T.);
#49453=EDGE_CURVE('',#38512,#38513,#29068,.T.);
#49454=EDGE_CURVE('',#38513,#38514,#29069,.T.);
#49455=EDGE_CURVE('',#38514,#38515,#29070,.T.);
#49456=EDGE_CURVE('',#38515,#38510,#29071,.T.);
#49457=EDGE_CURVE('',#38512,#38507,#29072,.T.);
#49458=EDGE_CURVE('',#38511,#38508,#29073,.T.);
#49459=EDGE_CURVE('',#38513,#38506,#29074,.T.);
#49460=EDGE_CURVE('',#38514,#38500,#29075,.T.);
#49461=EDGE_CURVE('',#38515,#38499,#29076,.T.);
#49462=EDGE_CURVE('',#38510,#38509,#29077,.T.);
#49463=EDGE_CURVE('',#38494,#38462,#4260,.T.);
#49464=EDGE_CURVE('',#38516,#38517,#29078,.T.);
#49465=EDGE_CURVE('',#38518,#38516,#4261,.T.);
#49466=EDGE_CURVE('',#38518,#38517,#20606,.T.);
#49467=EDGE_CURVE('',#38519,#38520,#29079,.T.);
#49468=EDGE_CURVE('',#38516,#38519,#4262,.T.);
#49469=EDGE_CURVE('',#38517,#38520,#4263,.T.);
#49470=EDGE_CURVE('',#38521,#38522,#29080,.T.);
#49471=EDGE_CURVE('',#38519,#38521,#4264,.T.);
#49472=EDGE_CURVE('',#38520,#38522,#4265,.T.);
#49473=EDGE_CURVE('',#38523,#38524,#29081,.T.);
#49474=EDGE_CURVE('',#38521,#38523,#4266,.T.);
#49475=EDGE_CURVE('',#38522,#38524,#4267,.T.);
#49476=EDGE_CURVE('',#38525,#38526,#29082,.T.);
#49477=EDGE_CURVE('',#38523,#38525,#4268,.T.);
#49478=EDGE_CURVE('',#38524,#38526,#4269,.T.);
#49479=EDGE_CURVE('',#38527,#38528,#29083,.T.);
#49480=EDGE_CURVE('',#38525,#38527,#4270,.T.);
#49481=EDGE_CURVE('',#38526,#38528,#4271,.T.);
#49482=EDGE_CURVE('',#38529,#38530,#29084,.T.);
#49483=EDGE_CURVE('',#38527,#38529,#4272,.T.);
#49484=EDGE_CURVE('',#38528,#38530,#4273,.T.);
#49485=EDGE_CURVE('',#38531,#38532,#29085,.T.);
#49486=EDGE_CURVE('',#38529,#38531,#4274,.T.);
#49487=EDGE_CURVE('',#38530,#38532,#4275,.T.);
#49488=EDGE_CURVE('',#38533,#38534,#29086,.T.);
#49489=EDGE_CURVE('',#38531,#38533,#4276,.T.);
#49490=EDGE_CURVE('',#38532,#38534,#4277,.T.);
#49491=EDGE_CURVE('',#38535,#38536,#29087,.T.);
#49492=EDGE_CURVE('',#38533,#38535,#4278,.T.);
#49493=EDGE_CURVE('',#38534,#38536,#4279,.T.);
#49494=EDGE_CURVE('',#38537,#38538,#29088,.T.);
#49495=EDGE_CURVE('',#38535,#38537,#4280,.T.);
#49496=EDGE_CURVE('',#38536,#38538,#4281,.T.);
#49497=EDGE_CURVE('',#38539,#38540,#29089,.T.);
#49498=EDGE_CURVE('',#38537,#38539,#4282,.T.);
#49499=EDGE_CURVE('',#38538,#38540,#4283,.T.);
#49500=EDGE_CURVE('',#38541,#38542,#29090,.T.);
#49501=EDGE_CURVE('',#38539,#38541,#4284,.T.);
#49502=EDGE_CURVE('',#38540,#38542,#4285,.T.);
#49503=EDGE_CURVE('',#38543,#38544,#29091,.T.);
#49504=EDGE_CURVE('',#38541,#38543,#4286,.T.);
#49505=EDGE_CURVE('',#38542,#38544,#4287,.T.);
#49506=EDGE_CURVE('',#38545,#38546,#29092,.T.);
#49507=EDGE_CURVE('',#38543,#38545,#4288,.T.);
#49508=EDGE_CURVE('',#38544,#38546,#4289,.T.);
#49509=EDGE_CURVE('',#38547,#38548,#29093,.T.);
#49510=EDGE_CURVE('',#38545,#38547,#4290,.T.);
#49511=EDGE_CURVE('',#38546,#38548,#4291,.T.);
#49512=EDGE_CURVE('',#38549,#38550,#29094,.T.);
#49513=EDGE_CURVE('',#38547,#38549,#4292,.T.);
#49514=EDGE_CURVE('',#38548,#38550,#4293,.T.);
#49515=EDGE_CURVE('',#38551,#38552,#29095,.T.);
#49516=EDGE_CURVE('',#38549,#38551,#4294,.T.);
#49517=EDGE_CURVE('',#38550,#38552,#4295,.T.);
#49518=EDGE_CURVE('',#38553,#38554,#29096,.T.);
#49519=EDGE_CURVE('',#38551,#38553,#4296,.T.);
#49520=EDGE_CURVE('',#38552,#38554,#4297,.T.);
#49521=EDGE_CURVE('',#38555,#38556,#29097,.T.);
#49522=EDGE_CURVE('',#38553,#38555,#4298,.T.);
#49523=EDGE_CURVE('',#38554,#38556,#4299,.T.);
#49524=EDGE_CURVE('',#38557,#38558,#29098,.T.);
#49525=EDGE_CURVE('',#38555,#38557,#4300,.T.);
#49526=EDGE_CURVE('',#38556,#38558,#4301,.T.);
#49527=EDGE_CURVE('',#38559,#38560,#29099,.T.);
#49528=EDGE_CURVE('',#38557,#38559,#4302,.T.);
#49529=EDGE_CURVE('',#38558,#38560,#4303,.T.);
#49530=EDGE_CURVE('',#38561,#38562,#29100,.T.);
#49531=EDGE_CURVE('',#38559,#38561,#4304,.T.);
#49532=EDGE_CURVE('',#38560,#38562,#4305,.T.);
#49533=EDGE_CURVE('',#38563,#38564,#29101,.T.);
#49534=EDGE_CURVE('',#38561,#38563,#4306,.T.);
#49535=EDGE_CURVE('',#38562,#38564,#4307,.T.);
#49536=EDGE_CURVE('',#38565,#38566,#29102,.T.);
#49537=EDGE_CURVE('',#38563,#38565,#4308,.T.);
#49538=EDGE_CURVE('',#38564,#38566,#4309,.T.);
#49539=EDGE_CURVE('',#38567,#38568,#29103,.T.);
#49540=EDGE_CURVE('',#38565,#38567,#4310,.T.);
#49541=EDGE_CURVE('',#38566,#38568,#4311,.T.);
#49542=EDGE_CURVE('',#38569,#38570,#29104,.T.);
#49543=EDGE_CURVE('',#38567,#38569,#4312,.T.);
#49544=EDGE_CURVE('',#38568,#38570,#4313,.T.);
#49545=EDGE_CURVE('',#38571,#38572,#29105,.T.);
#49546=EDGE_CURVE('',#38569,#38571,#4314,.T.);
#49547=EDGE_CURVE('',#38570,#38572,#4315,.T.);
#49548=EDGE_CURVE('',#38573,#38574,#29106,.T.);
#49549=EDGE_CURVE('',#38571,#38573,#4316,.T.);
#49550=EDGE_CURVE('',#38572,#38574,#4317,.T.);
#49551=EDGE_CURVE('',#38575,#38576,#29107,.T.);
#49552=EDGE_CURVE('',#38575,#38577,#24711,.T.);
#49553=EDGE_CURVE('',#38578,#38577,#20607,.T.);
#49554=EDGE_CURVE('',#38578,#38579,#29108,.T.);
#49555=EDGE_CURVE('',#38579,#38579,#20608,.T.);
#49556=EDGE_CURVE('',#38580,#38578,#20609,.T.);
#49557=EDGE_CURVE('',#38580,#38576,#24712,.T.);
#49558=EDGE_CURVE('',#38581,#38582,#29109,.T.);
#49559=EDGE_CURVE('',#38581,#38575,#24713,.T.);
#49560=EDGE_CURVE('',#38576,#38582,#24714,.T.);
#49561=EDGE_CURVE('',#38583,#38584,#29110,.T.);
#49562=EDGE_CURVE('',#38583,#38581,#24715,.T.);
#49563=EDGE_CURVE('',#38582,#38584,#24716,.T.);
#49564=EDGE_CURVE('',#38585,#38586,#29111,.T.);
#49565=EDGE_CURVE('',#38585,#38583,#24717,.T.);
#49566=EDGE_CURVE('',#38584,#38586,#24718,.T.);
#49567=EDGE_CURVE('',#38587,#38588,#29112,.T.);
#49568=EDGE_CURVE('',#38587,#38585,#24719,.T.);
#49569=EDGE_CURVE('',#38586,#38588,#24720,.T.);
#49570=EDGE_CURVE('',#38589,#38590,#29113,.T.);
#49571=EDGE_CURVE('',#38589,#38587,#24721,.T.);
#49572=EDGE_CURVE('',#38588,#38590,#24722,.T.);
#49573=EDGE_CURVE('',#38591,#38592,#29114,.T.);
#49574=EDGE_CURVE('',#38591,#38589,#24723,.T.);
#49575=EDGE_CURVE('',#38590,#38592,#24724,.T.);
#49576=EDGE_CURVE('',#38593,#38594,#29115,.T.);
#49577=EDGE_CURVE('',#38593,#38591,#24725,.T.);
#49578=EDGE_CURVE('',#38592,#38594,#24726,.T.);
#49579=EDGE_CURVE('',#38595,#38596,#29116,.T.);
#49580=EDGE_CURVE('',#38595,#38593,#24727,.T.);
#49581=EDGE_CURVE('',#38594,#38596,#24728,.T.);
#49582=EDGE_CURVE('',#38597,#38598,#29117,.T.);
#49583=EDGE_CURVE('',#38597,#38595,#24729,.T.);
#49584=EDGE_CURVE('',#38596,#38598,#24730,.T.);
#49585=EDGE_CURVE('',#38599,#38600,#29118,.T.);
#49586=EDGE_CURVE('',#38599,#38597,#24731,.T.);
#49587=EDGE_CURVE('',#38598,#38600,#24732,.T.);
#49588=EDGE_CURVE('',#38601,#38602,#29119,.T.);
#49589=EDGE_CURVE('',#38601,#38599,#24733,.T.);
#49590=EDGE_CURVE('',#38600,#38602,#24734,.T.);
#49591=EDGE_CURVE('',#38603,#38604,#29120,.T.);
#49592=EDGE_CURVE('',#38603,#38601,#24735,.T.);
#49593=EDGE_CURVE('',#38602,#38604,#24736,.T.);
#49594=EDGE_CURVE('',#38605,#38606,#29121,.T.);
#49595=EDGE_CURVE('',#38605,#38603,#24737,.T.);
#49596=EDGE_CURVE('',#38604,#38606,#24738,.T.);
#49597=EDGE_CURVE('',#38607,#38608,#29122,.T.);
#49598=EDGE_CURVE('',#38607,#38605,#24739,.T.);
#49599=EDGE_CURVE('',#38606,#38608,#24740,.T.);
#49600=EDGE_CURVE('',#38609,#38610,#29123,.T.);
#49601=EDGE_CURVE('',#38609,#38607,#24741,.T.);
#49602=EDGE_CURVE('',#38608,#38610,#24742,.T.);
#49603=EDGE_CURVE('',#38611,#38612,#29124,.T.);
#49604=EDGE_CURVE('',#38611,#38609,#24743,.T.);
#49605=EDGE_CURVE('',#38610,#38612,#24744,.T.);
#49606=EDGE_CURVE('',#38613,#38614,#29125,.T.);
#49607=EDGE_CURVE('',#38613,#38611,#24745,.T.);
#49608=EDGE_CURVE('',#38612,#38614,#24746,.T.);
#49609=EDGE_CURVE('',#38615,#38616,#29126,.T.);
#49610=EDGE_CURVE('',#38615,#38613,#24747,.T.);
#49611=EDGE_CURVE('',#38614,#38616,#24748,.T.);
#49612=EDGE_CURVE('',#38617,#38618,#29127,.T.);
#49613=EDGE_CURVE('',#38617,#38615,#24749,.T.);
#49614=EDGE_CURVE('',#38616,#38618,#24750,.T.);
#49615=EDGE_CURVE('',#38619,#38620,#29128,.T.);
#49616=EDGE_CURVE('',#38619,#38617,#24751,.T.);
#49617=EDGE_CURVE('',#38618,#38620,#24752,.T.);
#49618=EDGE_CURVE('',#38621,#38622,#29129,.T.);
#49619=EDGE_CURVE('',#38621,#38619,#24753,.T.);
#49620=EDGE_CURVE('',#38620,#38622,#24754,.T.);
#49621=EDGE_CURVE('',#38623,#38624,#29130,.T.);
#49622=EDGE_CURVE('',#38623,#38621,#24755,.T.);
#49623=EDGE_CURVE('',#38622,#38624,#24756,.T.);
#49624=EDGE_CURVE('',#38625,#38626,#29131,.T.);
#49625=EDGE_CURVE('',#38625,#38623,#24757,.T.);
#49626=EDGE_CURVE('',#38624,#38626,#24758,.T.);
#49627=EDGE_CURVE('',#38627,#38628,#29132,.T.);
#49628=EDGE_CURVE('',#38627,#38625,#24759,.T.);
#49629=EDGE_CURVE('',#38626,#38628,#24760,.T.);
#49630=EDGE_CURVE('',#38629,#38630,#29133,.T.);
#49631=EDGE_CURVE('',#38629,#38627,#24761,.T.);
#49632=EDGE_CURVE('',#38628,#38630,#24762,.T.);
#49633=EDGE_CURVE('',#38631,#38632,#29134,.T.);
#49634=EDGE_CURVE('',#38631,#38629,#24763,.T.);
#49635=EDGE_CURVE('',#38630,#38632,#24764,.T.);
#49636=EDGE_CURVE('',#38633,#38634,#29135,.T.);
#49637=EDGE_CURVE('',#38633,#38631,#24765,.T.);
#49638=EDGE_CURVE('',#38632,#38634,#24766,.T.);
#49639=EDGE_CURVE('',#38577,#38635,#29136,.T.);
#49640=EDGE_CURVE('',#38636,#38577,#24767,.T.);
#49641=EDGE_CURVE('',#38637,#38636,#20610,.T.);
#49642=EDGE_CURVE('',#38635,#38637,#24768,.F.);
#49643=EDGE_CURVE('',#38638,#38639,#29137,.T.);
#49644=EDGE_CURVE('',#38517,#38638,#24769,.F.);
#49645=EDGE_CURVE('',#38517,#38639,#20611,.T.);
#49646=EDGE_CURVE('',#38639,#38518,#20612,.T.);
#49647=EDGE_CURVE('',#38640,#38518,#24770,.T.);
#49648=EDGE_CURVE('',#38641,#38640,#20613,.T.);
#49649=EDGE_CURVE('',#38638,#38641,#24771,.F.);
#49650=EDGE_CURVE('',#38580,#38635,#24772,.F.);
#49651=EDGE_CURVE('',#38634,#38641,#24773,.T.);
#49652=EDGE_CURVE('',#38640,#38633,#24774,.T.);
#49653=EDGE_CURVE('',#38579,#38642,#20614,.T.);
#49654=EDGE_CURVE('',#38642,#38642,#20615,.T.);
#49655=EDGE_CURVE('',#38643,#38644,#29138,.T.);
#49656=EDGE_CURVE('',#38645,#38644,#20616,.T.);
#49657=EDGE_CURVE('',#38646,#38645,#20617,.T.);
#49658=EDGE_CURVE('',#38647,#38646,#20618,.T.);
#49659=EDGE_CURVE('',#38647,#38648,#20619,.T.);
#49660=EDGE_CURVE('',#38649,#38648,#20620,.T.);
#49661=EDGE_CURVE('',#38644,#38649,#20621,.T.);
#49662=EDGE_CURVE('',#38650,#38651,#4318,.T.);
#49663=EDGE_CURVE('',#38651,#38650,#20622,.T.);
#49664=EDGE_CURVE('',#38652,#38652,#20623,.T.);
#49665=EDGE_CURVE('',#38652,#38653,#20624,.T.);
#49666=EDGE_CURVE('',#38653,#38653,#20625,.T.);
#49667=EDGE_CURVE('',#38654,#38654,#20626,.T.);
#49668=EDGE_CURVE('',#38654,#38652,#29139,.T.);
#49669=EDGE_CURVE('',#38655,#38655,#20627,.T.);
#49670=EDGE_CURVE('',#38655,#38654,#20628,.T.);
#49671=EDGE_CURVE('',#38656,#38657,#20629,.T.);
#49672=EDGE_CURVE('',#38657,#38658,#24775,.T.);
#49673=EDGE_CURVE('',#38658,#38659,#198,.T.);
#49674=EDGE_CURVE('',#38659,#38660,#24776,.T.);
#49675=EDGE_CURVE('',#38660,#38661,#20630,.T.);
#49676=EDGE_CURVE('',#38661,#38662,#24777,.T.);
#49677=EDGE_CURVE('',#38662,#38663,#199,.T.);
#49678=EDGE_CURVE('',#38663,#38664,#24778,.T.);
#49679=EDGE_CURVE('',#38664,#38665,#20631,.T.);
#49680=EDGE_CURVE('',#38665,#38666,#24779,.T.);
#49681=EDGE_CURVE('',#38666,#38667,#200,.T.);
#49682=EDGE_CURVE('',#38667,#38668,#24780,.T.);
#49683=EDGE_CURVE('',#38668,#38669,#20632,.T.);
#49684=EDGE_CURVE('',#38669,#38670,#24781,.T.);
#49685=EDGE_CURVE('',#38670,#38671,#201,.T.);
#49686=EDGE_CURVE('',#38671,#38672,#24782,.T.);
#49687=EDGE_CURVE('',#38672,#38673,#20633,.T.);
#49688=EDGE_CURVE('',#38673,#38674,#24783,.T.);
#49689=EDGE_CURVE('',#38674,#38675,#202,.T.);
#49690=EDGE_CURVE('',#38675,#38676,#24784,.T.);
#49691=EDGE_CURVE('',#38676,#38677,#20634,.T.);
#49692=EDGE_CURVE('',#38677,#38678,#24785,.T.);
#49693=EDGE_CURVE('',#38678,#38679,#203,.T.);
#49694=EDGE_CURVE('',#38679,#38680,#24786,.T.);
#49695=EDGE_CURVE('',#38680,#38681,#20635,.T.);
#49696=EDGE_CURVE('',#38681,#38682,#24787,.T.);
#49697=EDGE_CURVE('',#38682,#38683,#204,.T.);
#49698=EDGE_CURVE('',#38683,#38684,#24788,.T.);
#49699=EDGE_CURVE('',#38684,#38685,#20636,.T.);
#49700=EDGE_CURVE('',#38685,#38686,#24789,.T.);
#49701=EDGE_CURVE('',#38686,#38687,#205,.T.);
#49702=EDGE_CURVE('',#38687,#38688,#24790,.T.);
#49703=EDGE_CURVE('',#38688,#38689,#20637,.T.);
#49704=EDGE_CURVE('',#38689,#38690,#24791,.T.);
#49705=EDGE_CURVE('',#38690,#38691,#206,.T.);
#49706=EDGE_CURVE('',#38691,#38692,#24792,.T.);
#49707=EDGE_CURVE('',#38692,#38693,#20638,.T.);
#49708=EDGE_CURVE('',#38693,#38694,#24793,.T.);
#49709=EDGE_CURVE('',#38694,#38695,#207,.T.);
#49710=EDGE_CURVE('',#38695,#38696,#24794,.T.);
#49711=EDGE_CURVE('',#38696,#38697,#20639,.T.);
#49712=EDGE_CURVE('',#38697,#38698,#24795,.T.);
#49713=EDGE_CURVE('',#38698,#38699,#208,.T.);
#49714=EDGE_CURVE('',#38699,#38700,#24796,.T.);
#49715=EDGE_CURVE('',#38700,#38701,#20640,.T.);
#49716=EDGE_CURVE('',#38701,#38702,#24797,.T.);
#49717=EDGE_CURVE('',#38702,#38703,#209,.T.);
#49718=EDGE_CURVE('',#38703,#38704,#24798,.T.);
#49719=EDGE_CURVE('',#38704,#38705,#20641,.T.);
#49720=EDGE_CURVE('',#38705,#38706,#24799,.T.);
#49721=EDGE_CURVE('',#38706,#38707,#210,.T.);
#49722=EDGE_CURVE('',#38707,#38708,#24800,.T.);
#49723=EDGE_CURVE('',#38708,#38709,#20642,.T.);
#49724=EDGE_CURVE('',#38709,#38710,#24801,.T.);
#49725=EDGE_CURVE('',#38710,#38711,#211,.T.);
#49726=EDGE_CURVE('',#38711,#38712,#24802,.T.);
#49727=EDGE_CURVE('',#38712,#38713,#20643,.T.);
#49728=EDGE_CURVE('',#38713,#38714,#24803,.T.);
#49729=EDGE_CURVE('',#38714,#38715,#212,.T.);
#49730=EDGE_CURVE('',#38715,#38716,#24804,.T.);
#49731=EDGE_CURVE('',#38716,#38717,#20644,.T.);
#49732=EDGE_CURVE('',#38717,#38718,#24805,.T.);
#49733=EDGE_CURVE('',#38718,#38719,#213,.T.);
#49734=EDGE_CURVE('',#38719,#38720,#24806,.T.);
#49735=EDGE_CURVE('',#38720,#38721,#20645,.T.);
#49736=EDGE_CURVE('',#38721,#38722,#24807,.T.);
#49737=EDGE_CURVE('',#38722,#38723,#214,.T.);
#49738=EDGE_CURVE('',#38723,#38724,#24808,.T.);
#49739=EDGE_CURVE('',#38724,#38725,#20646,.T.);
#49740=EDGE_CURVE('',#38725,#38726,#24809,.T.);
#49741=EDGE_CURVE('',#38726,#38727,#215,.T.);
#49742=EDGE_CURVE('',#38727,#38728,#24810,.T.);
#49743=EDGE_CURVE('',#38728,#38729,#20647,.T.);
#49744=EDGE_CURVE('',#38729,#38730,#24811,.T.);
#49745=EDGE_CURVE('',#38730,#38731,#216,.T.);
#49746=EDGE_CURVE('',#38731,#38732,#24812,.T.);
#49747=EDGE_CURVE('',#38732,#38733,#20648,.T.);
#49748=EDGE_CURVE('',#38733,#38734,#24813,.T.);
#49749=EDGE_CURVE('',#38734,#38735,#217,.T.);
#49750=EDGE_CURVE('',#38735,#38736,#24814,.T.);
#49751=EDGE_CURVE('',#38736,#38737,#20649,.T.);
#49752=EDGE_CURVE('',#38737,#38738,#24815,.T.);
#49753=EDGE_CURVE('',#38738,#38739,#218,.T.);
#49754=EDGE_CURVE('',#38739,#38740,#24816,.T.);
#49755=EDGE_CURVE('',#38740,#38741,#20650,.T.);
#49756=EDGE_CURVE('',#38741,#38742,#24817,.T.);
#49757=EDGE_CURVE('',#38742,#38743,#219,.T.);
#49758=EDGE_CURVE('',#38743,#38744,#24818,.T.);
#49759=EDGE_CURVE('',#38744,#38745,#20651,.T.);
#49760=EDGE_CURVE('',#38745,#38746,#24819,.T.);
#49761=EDGE_CURVE('',#38746,#38747,#220,.T.);
#49762=EDGE_CURVE('',#38747,#38748,#24820,.T.);
#49763=EDGE_CURVE('',#38748,#38749,#20652,.T.);
#49764=EDGE_CURVE('',#38749,#38750,#24821,.T.);
#49765=EDGE_CURVE('',#38750,#38751,#221,.T.);
#49766=EDGE_CURVE('',#38751,#38752,#24822,.T.);
#49767=EDGE_CURVE('',#38752,#38753,#20653,.T.);
#49768=EDGE_CURVE('',#38753,#38754,#24823,.T.);
#49769=EDGE_CURVE('',#38754,#38755,#222,.T.);
#49770=EDGE_CURVE('',#38755,#38756,#24824,.T.);
#49771=EDGE_CURVE('',#38756,#38757,#20654,.T.);
#49772=EDGE_CURVE('',#38757,#38758,#24825,.T.);
#49773=EDGE_CURVE('',#38758,#38759,#223,.T.);
#49774=EDGE_CURVE('',#38759,#38760,#24826,.T.);
#49775=EDGE_CURVE('',#38760,#38761,#20655,.T.);
#49776=EDGE_CURVE('',#38761,#38762,#24827,.T.);
#49777=EDGE_CURVE('',#38762,#38763,#224,.T.);
#49778=EDGE_CURVE('',#38763,#38764,#24828,.T.);
#49779=EDGE_CURVE('',#38764,#38765,#20656,.T.);
#49780=EDGE_CURVE('',#38765,#38766,#24829,.T.);
#49781=EDGE_CURVE('',#38766,#38767,#225,.T.);
#49782=EDGE_CURVE('',#38767,#38768,#24830,.T.);
#49783=EDGE_CURVE('',#38768,#38769,#20657,.T.);
#49784=EDGE_CURVE('',#38769,#38770,#24831,.T.);
#49785=EDGE_CURVE('',#38770,#38771,#226,.T.);
#49786=EDGE_CURVE('',#38771,#38772,#24832,.T.);
#49787=EDGE_CURVE('',#38772,#38773,#20658,.T.);
#49788=EDGE_CURVE('',#38773,#38774,#24833,.T.);
#49789=EDGE_CURVE('',#38774,#38775,#227,.T.);
#49790=EDGE_CURVE('',#38775,#38776,#24834,.T.);
#49791=EDGE_CURVE('',#38776,#38777,#20659,.T.);
#49792=EDGE_CURVE('',#38777,#38778,#24835,.T.);
#49793=EDGE_CURVE('',#38778,#38779,#228,.T.);
#49794=EDGE_CURVE('',#38779,#38780,#24836,.T.);
#49795=EDGE_CURVE('',#38780,#38781,#20660,.T.);
#49796=EDGE_CURVE('',#38781,#38782,#24837,.T.);
#49797=EDGE_CURVE('',#38782,#38783,#229,.T.);
#49798=EDGE_CURVE('',#38783,#38784,#24838,.T.);
#49799=EDGE_CURVE('',#38784,#38785,#20661,.T.);
#49800=EDGE_CURVE('',#38785,#38786,#24839,.T.);
#49801=EDGE_CURVE('',#38786,#38787,#230,.T.);
#49802=EDGE_CURVE('',#38787,#38788,#24840,.T.);
#49803=EDGE_CURVE('',#38788,#38789,#20662,.T.);
#49804=EDGE_CURVE('',#38789,#38790,#24841,.T.);
#49805=EDGE_CURVE('',#38790,#38791,#231,.T.);
#49806=EDGE_CURVE('',#38791,#38792,#24842,.T.);
#49807=EDGE_CURVE('',#38792,#38793,#20663,.T.);
#49808=EDGE_CURVE('',#38793,#38794,#24843,.T.);
#49809=EDGE_CURVE('',#38794,#38795,#232,.T.);
#49810=EDGE_CURVE('',#38795,#38796,#24844,.T.);
#49811=EDGE_CURVE('',#38796,#38797,#20664,.T.);
#49812=EDGE_CURVE('',#38797,#38798,#24845,.T.);
#49813=EDGE_CURVE('',#38798,#38799,#233,.T.);
#49814=EDGE_CURVE('',#38799,#38800,#24846,.T.);
#49815=EDGE_CURVE('',#38800,#38801,#20665,.T.);
#49816=EDGE_CURVE('',#38801,#38802,#24847,.T.);
#49817=EDGE_CURVE('',#38802,#38803,#234,.T.);
#49818=EDGE_CURVE('',#38803,#38804,#24848,.T.);
#49819=EDGE_CURVE('',#38804,#38805,#20666,.T.);
#49820=EDGE_CURVE('',#38805,#38806,#24849,.T.);
#49821=EDGE_CURVE('',#38806,#38807,#235,.T.);
#49822=EDGE_CURVE('',#38807,#38808,#24850,.T.);
#49823=EDGE_CURVE('',#38808,#38809,#20667,.T.);
#49824=EDGE_CURVE('',#38809,#38810,#24851,.T.);
#49825=EDGE_CURVE('',#38810,#38811,#236,.T.);
#49826=EDGE_CURVE('',#38811,#38812,#24852,.T.);
#49827=EDGE_CURVE('',#38812,#38813,#20668,.T.);
#49828=EDGE_CURVE('',#38813,#38814,#24853,.T.);
#49829=EDGE_CURVE('',#38814,#38815,#237,.T.);
#49830=EDGE_CURVE('',#38815,#38816,#24854,.T.);
#49831=EDGE_CURVE('',#38816,#38817,#20669,.T.);
#49832=EDGE_CURVE('',#38817,#38818,#24855,.T.);
#49833=EDGE_CURVE('',#38818,#38819,#238,.T.);
#49834=EDGE_CURVE('',#38819,#38820,#24856,.T.);
#49835=EDGE_CURVE('',#38820,#38821,#20670,.T.);
#49836=EDGE_CURVE('',#38821,#38822,#24857,.T.);
#49837=EDGE_CURVE('',#38822,#38823,#239,.T.);
#49838=EDGE_CURVE('',#38823,#38824,#24858,.T.);
#49839=EDGE_CURVE('',#38824,#38825,#20671,.T.);
#49840=EDGE_CURVE('',#38825,#38826,#24859,.T.);
#49841=EDGE_CURVE('',#38826,#38827,#240,.T.);
#49842=EDGE_CURVE('',#38827,#38828,#24860,.T.);
#49843=EDGE_CURVE('',#38828,#38829,#20672,.T.);
#49844=EDGE_CURVE('',#38829,#38830,#24861,.T.);
#49845=EDGE_CURVE('',#38830,#38831,#241,.T.);
#49846=EDGE_CURVE('',#38831,#38832,#24862,.T.);
#49847=EDGE_CURVE('',#38832,#38833,#20673,.T.);
#49848=EDGE_CURVE('',#38833,#38834,#24863,.T.);
#49849=EDGE_CURVE('',#38834,#38835,#242,.T.);
#49850=EDGE_CURVE('',#38835,#38836,#24864,.T.);
#49851=EDGE_CURVE('',#38836,#38837,#20674,.T.);
#49852=EDGE_CURVE('',#38837,#38838,#24865,.T.);
#49853=EDGE_CURVE('',#38838,#38839,#243,.T.);
#49854=EDGE_CURVE('',#38839,#38840,#24866,.T.);
#49855=EDGE_CURVE('',#38840,#38841,#20675,.T.);
#49856=EDGE_CURVE('',#38841,#38842,#24867,.T.);
#49857=EDGE_CURVE('',#38842,#38843,#244,.T.);
#49858=EDGE_CURVE('',#38843,#38844,#24868,.T.);
#49859=EDGE_CURVE('',#38844,#38845,#20676,.T.);
#49860=EDGE_CURVE('',#38845,#38846,#24869,.T.);
#49861=EDGE_CURVE('',#38846,#38847,#245,.T.);
#49862=EDGE_CURVE('',#38847,#38848,#24870,.T.);
#49863=EDGE_CURVE('',#38848,#38849,#20677,.T.);
#49864=EDGE_CURVE('',#38849,#38850,#24871,.T.);
#49865=EDGE_CURVE('',#38850,#38851,#246,.T.);
#49866=EDGE_CURVE('',#38851,#38852,#24872,.T.);
#49867=EDGE_CURVE('',#38852,#38853,#20678,.T.);
#49868=EDGE_CURVE('',#38853,#38854,#29140,.T.);
#49869=EDGE_CURVE('',#38855,#38854,#20679,.T.);
#49870=EDGE_CURVE('',#38854,#38855,#20680,.T.);
#49871=EDGE_CURVE('',#38853,#38856,#20681,.T.);
#49872=EDGE_CURVE('',#38856,#38857,#24873,.T.);
#49873=EDGE_CURVE('',#38857,#38858,#247,.T.);
#49874=EDGE_CURVE('',#38858,#38859,#24874,.T.);
#49875=EDGE_CURVE('',#38859,#38860,#20682,.T.);
#49876=EDGE_CURVE('',#38860,#38861,#24875,.T.);
#49877=EDGE_CURVE('',#38861,#38862,#248,.T.);
#49878=EDGE_CURVE('',#38862,#38863,#24876,.T.);
#49879=EDGE_CURVE('',#38863,#38864,#20683,.T.);
#49880=EDGE_CURVE('',#38864,#38865,#24877,.T.);
#49881=EDGE_CURVE('',#38865,#38866,#249,.T.);
#49882=EDGE_CURVE('',#38866,#38867,#24878,.T.);
#49883=EDGE_CURVE('',#38867,#38868,#20684,.T.);
#49884=EDGE_CURVE('',#38868,#38869,#24879,.T.);
#49885=EDGE_CURVE('',#38869,#38870,#250,.T.);
#49886=EDGE_CURVE('',#38870,#38871,#24880,.T.);
#49887=EDGE_CURVE('',#38871,#38872,#20685,.T.);
#49888=EDGE_CURVE('',#38872,#38873,#24881,.T.);
#49889=EDGE_CURVE('',#38873,#38874,#251,.T.);
#49890=EDGE_CURVE('',#38874,#38875,#24882,.T.);
#49891=EDGE_CURVE('',#38875,#38876,#20686,.T.);
#49892=EDGE_CURVE('',#38876,#38877,#24883,.T.);
#49893=EDGE_CURVE('',#38877,#38878,#252,.T.);
#49894=EDGE_CURVE('',#38878,#38879,#24884,.T.);
#49895=EDGE_CURVE('',#38879,#38880,#20687,.T.);
#49896=EDGE_CURVE('',#38880,#38881,#24885,.T.);
#49897=EDGE_CURVE('',#38881,#38882,#253,.T.);
#49898=EDGE_CURVE('',#38882,#38883,#24886,.T.);
#49899=EDGE_CURVE('',#38883,#38884,#20688,.T.);
#49900=EDGE_CURVE('',#38884,#38885,#24887,.T.);
#49901=EDGE_CURVE('',#38885,#38886,#254,.T.);
#49902=EDGE_CURVE('',#38886,#38887,#24888,.T.);
#49903=EDGE_CURVE('',#38887,#38888,#20689,.T.);
#49904=EDGE_CURVE('',#38888,#38889,#24889,.T.);
#49905=EDGE_CURVE('',#38889,#38890,#255,.T.);
#49906=EDGE_CURVE('',#38890,#38891,#24890,.T.);
#49907=EDGE_CURVE('',#38891,#38892,#20690,.T.);
#49908=EDGE_CURVE('',#38892,#38893,#24891,.T.);
#49909=EDGE_CURVE('',#38893,#38894,#256,.T.);
#49910=EDGE_CURVE('',#38894,#38895,#24892,.T.);
#49911=EDGE_CURVE('',#38895,#38896,#20691,.T.);
#49912=EDGE_CURVE('',#38896,#38897,#24893,.T.);
#49913=EDGE_CURVE('',#38897,#38898,#257,.T.);
#49914=EDGE_CURVE('',#38898,#38899,#24894,.T.);
#49915=EDGE_CURVE('',#38899,#38900,#20692,.T.);
#49916=EDGE_CURVE('',#38900,#38901,#24895,.T.);
#49917=EDGE_CURVE('',#38901,#38902,#258,.T.);
#49918=EDGE_CURVE('',#38902,#38903,#24896,.T.);
#49919=EDGE_CURVE('',#38903,#38904,#20693,.T.);
#49920=EDGE_CURVE('',#38904,#38905,#24897,.T.);
#49921=EDGE_CURVE('',#38905,#38906,#259,.T.);
#49922=EDGE_CURVE('',#38906,#38907,#24898,.T.);
#49923=EDGE_CURVE('',#38907,#38908,#20694,.T.);
#49924=EDGE_CURVE('',#38908,#38909,#24899,.T.);
#49925=EDGE_CURVE('',#38909,#38910,#260,.T.);
#49926=EDGE_CURVE('',#38910,#38911,#24900,.T.);
#49927=EDGE_CURVE('',#38911,#38912,#20695,.T.);
#49928=EDGE_CURVE('',#38912,#38913,#24901,.T.);
#49929=EDGE_CURVE('',#38913,#38914,#261,.T.);
#49930=EDGE_CURVE('',#38914,#38915,#24902,.T.);
#49931=EDGE_CURVE('',#38915,#38916,#20696,.T.);
#49932=EDGE_CURVE('',#38916,#38917,#24903,.T.);
#49933=EDGE_CURVE('',#38917,#38918,#262,.T.);
#49934=EDGE_CURVE('',#38918,#38919,#24904,.T.);
#49935=EDGE_CURVE('',#38919,#38920,#20697,.T.);
#49936=EDGE_CURVE('',#38920,#38921,#24905,.T.);
#49937=EDGE_CURVE('',#38921,#38922,#263,.T.);
#49938=EDGE_CURVE('',#38922,#38923,#24906,.T.);
#49939=EDGE_CURVE('',#38923,#38924,#20698,.T.);
#49940=EDGE_CURVE('',#38924,#38925,#24907,.T.);
#49941=EDGE_CURVE('',#38925,#38926,#264,.T.);
#49942=EDGE_CURVE('',#38926,#38927,#24908,.T.);
#49943=EDGE_CURVE('',#38927,#38928,#20699,.T.);
#49944=EDGE_CURVE('',#38928,#38929,#24909,.T.);
#49945=EDGE_CURVE('',#38929,#38930,#265,.T.);
#49946=EDGE_CURVE('',#38930,#38931,#24910,.T.);
#49947=EDGE_CURVE('',#38931,#38932,#20700,.T.);
#49948=EDGE_CURVE('',#38932,#38933,#24911,.T.);
#49949=EDGE_CURVE('',#38933,#38934,#266,.T.);
#49950=EDGE_CURVE('',#38934,#38935,#24912,.T.);
#49951=EDGE_CURVE('',#38935,#38936,#20701,.T.);
#49952=EDGE_CURVE('',#38936,#38937,#24913,.T.);
#49953=EDGE_CURVE('',#38937,#38938,#267,.T.);
#49954=EDGE_CURVE('',#38938,#38939,#24914,.T.);
#49955=EDGE_CURVE('',#38939,#38940,#20702,.T.);
#49956=EDGE_CURVE('',#38940,#38941,#24915,.T.);
#49957=EDGE_CURVE('',#38941,#38942,#268,.T.);
#49958=EDGE_CURVE('',#38942,#38943,#24916,.T.);
#49959=EDGE_CURVE('',#38943,#38944,#20703,.T.);
#49960=EDGE_CURVE('',#38944,#38945,#24917,.T.);
#49961=EDGE_CURVE('',#38945,#38946,#269,.T.);
#49962=EDGE_CURVE('',#38946,#38947,#24918,.T.);
#49963=EDGE_CURVE('',#38947,#38948,#20704,.T.);
#49964=EDGE_CURVE('',#38948,#38949,#24919,.T.);
#49965=EDGE_CURVE('',#38949,#38950,#270,.T.);
#49966=EDGE_CURVE('',#38950,#38951,#24920,.T.);
#49967=EDGE_CURVE('',#38951,#38952,#20705,.T.);
#49968=EDGE_CURVE('',#38952,#38953,#24921,.T.);
#49969=EDGE_CURVE('',#38953,#38954,#271,.T.);
#49970=EDGE_CURVE('',#38954,#38955,#24922,.T.);
#49971=EDGE_CURVE('',#38955,#38956,#20706,.T.);
#49972=EDGE_CURVE('',#38956,#38957,#24923,.T.);
#49973=EDGE_CURVE('',#38957,#38958,#272,.T.);
#49974=EDGE_CURVE('',#38958,#38959,#24924,.T.);
#49975=EDGE_CURVE('',#38959,#38960,#20707,.T.);
#49976=EDGE_CURVE('',#38960,#38961,#24925,.T.);
#49977=EDGE_CURVE('',#38961,#38962,#273,.T.);
#49978=EDGE_CURVE('',#38962,#38963,#24926,.T.);
#49979=EDGE_CURVE('',#38963,#38964,#20708,.T.);
#49980=EDGE_CURVE('',#38964,#38965,#24927,.T.);
#49981=EDGE_CURVE('',#38965,#38966,#274,.T.);
#49982=EDGE_CURVE('',#38966,#38967,#24928,.T.);
#49983=EDGE_CURVE('',#38967,#38968,#20709,.T.);
#49984=EDGE_CURVE('',#38968,#38969,#24929,.T.);
#49985=EDGE_CURVE('',#38969,#38970,#275,.T.);
#49986=EDGE_CURVE('',#38970,#38971,#24930,.T.);
#49987=EDGE_CURVE('',#38971,#38972,#20710,.T.);
#49988=EDGE_CURVE('',#38972,#38973,#24931,.T.);
#49989=EDGE_CURVE('',#38973,#38974,#276,.T.);
#49990=EDGE_CURVE('',#38974,#38975,#24932,.T.);
#49991=EDGE_CURVE('',#38975,#38976,#20711,.T.);
#49992=EDGE_CURVE('',#38976,#38977,#24933,.T.);
#49993=EDGE_CURVE('',#38977,#38978,#277,.T.);
#49994=EDGE_CURVE('',#38978,#38979,#24934,.T.);
#49995=EDGE_CURVE('',#38979,#38980,#20712,.T.);
#49996=EDGE_CURVE('',#38980,#38981,#24935,.T.);
#49997=EDGE_CURVE('',#38981,#38982,#278,.T.);
#49998=EDGE_CURVE('',#38982,#38983,#24936,.T.);
#49999=EDGE_CURVE('',#38983,#38984,#20713,.T.);
#50000=EDGE_CURVE('',#38984,#38985,#24937,.T.);
#50001=EDGE_CURVE('',#38985,#38986,#279,.T.);
#50002=EDGE_CURVE('',#38986,#38987,#24938,.T.);
#50003=EDGE_CURVE('',#38987,#38988,#20714,.T.);
#50004=EDGE_CURVE('',#38988,#38989,#24939,.T.);
#50005=EDGE_CURVE('',#38989,#38990,#280,.T.);
#50006=EDGE_CURVE('',#38990,#38991,#24940,.T.);
#50007=EDGE_CURVE('',#38991,#38992,#20715,.T.);
#50008=EDGE_CURVE('',#38992,#38993,#24941,.T.);
#50009=EDGE_CURVE('',#38993,#38994,#281,.T.);
#50010=EDGE_CURVE('',#38994,#38995,#24942,.T.);
#50011=EDGE_CURVE('',#38995,#38996,#20716,.T.);
#50012=EDGE_CURVE('',#38996,#38997,#24943,.T.);
#50013=EDGE_CURVE('',#38997,#38998,#282,.T.);
#50014=EDGE_CURVE('',#38998,#38999,#24944,.T.);
#50015=EDGE_CURVE('',#38999,#39000,#20717,.T.);
#50016=EDGE_CURVE('',#39000,#39001,#24945,.T.);
#50017=EDGE_CURVE('',#39001,#39002,#283,.T.);
#50018=EDGE_CURVE('',#39002,#39003,#24946,.T.);
#50019=EDGE_CURVE('',#39003,#39004,#20718,.T.);
#50020=EDGE_CURVE('',#39004,#39005,#24947,.T.);
#50021=EDGE_CURVE('',#39005,#39006,#284,.T.);
#50022=EDGE_CURVE('',#39006,#39007,#24948,.T.);
#50023=EDGE_CURVE('',#39007,#39008,#20719,.T.);
#50024=EDGE_CURVE('',#39008,#39009,#24949,.T.);
#50025=EDGE_CURVE('',#39009,#39010,#285,.T.);
#50026=EDGE_CURVE('',#39010,#39011,#24950,.T.);
#50027=EDGE_CURVE('',#39011,#39012,#20720,.T.);
#50028=EDGE_CURVE('',#39012,#39013,#24951,.T.);
#50029=EDGE_CURVE('',#39013,#39014,#286,.T.);
#50030=EDGE_CURVE('',#39014,#39015,#24952,.T.);
#50031=EDGE_CURVE('',#39015,#39016,#20721,.T.);
#50032=EDGE_CURVE('',#39016,#39017,#24953,.T.);
#50033=EDGE_CURVE('',#39017,#39018,#287,.T.);
#50034=EDGE_CURVE('',#39018,#39019,#24954,.T.);
#50035=EDGE_CURVE('',#39019,#39020,#20722,.T.);
#50036=EDGE_CURVE('',#39020,#39021,#24955,.T.);
#50037=EDGE_CURVE('',#39021,#39022,#288,.T.);
#50038=EDGE_CURVE('',#39022,#39023,#24956,.T.);
#50039=EDGE_CURVE('',#39023,#39024,#20723,.T.);
#50040=EDGE_CURVE('',#39024,#39025,#24957,.T.);
#50041=EDGE_CURVE('',#39025,#39026,#289,.T.);
#50042=EDGE_CURVE('',#39026,#39027,#24958,.T.);
#50043=EDGE_CURVE('',#39027,#39028,#20724,.T.);
#50044=EDGE_CURVE('',#39028,#39029,#24959,.T.);
#50045=EDGE_CURVE('',#39029,#39030,#290,.T.);
#50046=EDGE_CURVE('',#39030,#39031,#24960,.T.);
#50047=EDGE_CURVE('',#39031,#39032,#20725,.T.);
#50048=EDGE_CURVE('',#39032,#39033,#24961,.T.);
#50049=EDGE_CURVE('',#39033,#39034,#291,.T.);
#50050=EDGE_CURVE('',#39034,#39035,#24962,.T.);
#50051=EDGE_CURVE('',#39035,#39036,#20726,.T.);
#50052=EDGE_CURVE('',#39036,#39037,#24963,.T.);
#50053=EDGE_CURVE('',#39037,#39038,#292,.T.);
#50054=EDGE_CURVE('',#39038,#39039,#24964,.T.);
#50055=EDGE_CURVE('',#39039,#39040,#20727,.T.);
#50056=EDGE_CURVE('',#39040,#39041,#24965,.T.);
#50057=EDGE_CURVE('',#39041,#39042,#293,.T.);
#50058=EDGE_CURVE('',#39042,#39043,#24966,.T.);
#50059=EDGE_CURVE('',#39043,#39044,#20728,.T.);
#50060=EDGE_CURVE('',#39044,#39045,#24967,.T.);
#50061=EDGE_CURVE('',#39045,#39046,#294,.T.);
#50062=EDGE_CURVE('',#39046,#39047,#24968,.T.);
#50063=EDGE_CURVE('',#39047,#39048,#20729,.T.);
#50064=EDGE_CURVE('',#39048,#39049,#24969,.T.);
#50065=EDGE_CURVE('',#39049,#39050,#295,.T.);
#50066=EDGE_CURVE('',#39050,#38656,#24970,.T.);
#50067=EDGE_CURVE('',#39051,#39051,#20730,.T.);
#50068=EDGE_CURVE('',#39051,#38855,#20731,.T.);
#50069=EDGE_CURVE('',#39052,#39053,#20732,.T.);
#50070=EDGE_CURVE('',#39052,#39054,#29141,.T.);
#50071=EDGE_CURVE('',#39055,#39054,#296,.T.);
#50072=EDGE_CURVE('',#39055,#39056,#20733,.T.);
#50073=EDGE_CURVE('',#39057,#39056,#297,.T.);
#50074=EDGE_CURVE('',#39057,#39058,#29142,.T.);
#50075=EDGE_CURVE('',#39059,#39058,#20734,.T.);
#50076=EDGE_CURVE('',#39059,#39060,#29143,.T.);
#50077=EDGE_CURVE('',#39061,#39060,#298,.T.);
#50078=EDGE_CURVE('',#39061,#39062,#20735,.T.);
#50079=EDGE_CURVE('',#39063,#39062,#299,.T.);
#50080=EDGE_CURVE('',#39063,#39064,#29144,.T.);
#50081=EDGE_CURVE('',#39065,#39064,#20736,.T.);
#50082=EDGE_CURVE('',#39065,#39066,#29145,.T.);
#50083=EDGE_CURVE('',#39067,#39066,#300,.T.);
#50084=EDGE_CURVE('',#39067,#39068,#20737,.T.);
#50085=EDGE_CURVE('',#39069,#39068,#301,.T.);
#50086=EDGE_CURVE('',#39069,#39070,#29146,.T.);
#50087=EDGE_CURVE('',#39071,#39070,#20738,.T.);
#50088=EDGE_CURVE('',#39071,#39072,#29147,.T.);
#50089=EDGE_CURVE('',#39073,#39072,#302,.T.);
#50090=EDGE_CURVE('',#39073,#39074,#20739,.T.);
#50091=EDGE_CURVE('',#39075,#39074,#303,.T.);
#50092=EDGE_CURVE('',#39075,#39076,#29148,.T.);
#50093=EDGE_CURVE('',#39077,#39076,#20740,.T.);
#50094=EDGE_CURVE('',#39077,#39078,#29149,.T.);
#50095=EDGE_CURVE('',#39079,#39078,#304,.T.);
#50096=EDGE_CURVE('',#39079,#39080,#20741,.T.);
#50097=EDGE_CURVE('',#39081,#39080,#305,.T.);
#50098=EDGE_CURVE('',#39081,#39082,#29150,.T.);
#50099=EDGE_CURVE('',#39083,#39082,#20742,.T.);
#50100=EDGE_CURVE('',#39083,#39084,#29151,.T.);
#50101=EDGE_CURVE('',#39085,#39084,#306,.T.);
#50102=EDGE_CURVE('',#39085,#39086,#20743,.T.);
#50103=EDGE_CURVE('',#39087,#39086,#307,.T.);
#50104=EDGE_CURVE('',#39087,#39088,#29152,.T.);
#50105=EDGE_CURVE('',#39089,#39088,#20744,.T.);
#50106=EDGE_CURVE('',#39089,#39090,#29153,.T.);
#50107=EDGE_CURVE('',#39091,#39090,#308,.T.);
#50108=EDGE_CURVE('',#39091,#39092,#20745,.T.);
#50109=EDGE_CURVE('',#39093,#39092,#309,.T.);
#50110=EDGE_CURVE('',#39093,#39094,#29154,.T.);
#50111=EDGE_CURVE('',#39095,#39094,#20746,.T.);
#50112=EDGE_CURVE('',#39095,#39096,#29155,.T.);
#50113=EDGE_CURVE('',#39097,#39096,#310,.T.);
#50114=EDGE_CURVE('',#39097,#39098,#20747,.T.);
#50115=EDGE_CURVE('',#39099,#39098,#311,.T.);
#50116=EDGE_CURVE('',#39099,#39100,#29156,.T.);
#50117=EDGE_CURVE('',#39101,#39100,#20748,.T.);
#50118=EDGE_CURVE('',#39101,#39102,#29157,.T.);
#50119=EDGE_CURVE('',#39103,#39102,#312,.T.);
#50120=EDGE_CURVE('',#39103,#39104,#20749,.T.);
#50121=EDGE_CURVE('',#39105,#39104,#313,.T.);
#50122=EDGE_CURVE('',#39105,#39106,#29158,.T.);
#50123=EDGE_CURVE('',#39107,#39106,#20750,.T.);
#50124=EDGE_CURVE('',#39107,#39108,#29159,.T.);
#50125=EDGE_CURVE('',#39109,#39108,#314,.T.);
#50126=EDGE_CURVE('',#39109,#39110,#20751,.T.);
#50127=EDGE_CURVE('',#39111,#39110,#315,.T.);
#50128=EDGE_CURVE('',#39111,#39112,#29160,.T.);
#50129=EDGE_CURVE('',#39113,#39112,#20752,.T.);
#50130=EDGE_CURVE('',#39113,#39114,#29161,.T.);
#50131=EDGE_CURVE('',#39115,#39114,#316,.T.);
#50132=EDGE_CURVE('',#39115,#39116,#20753,.T.);
#50133=EDGE_CURVE('',#39117,#39116,#317,.T.);
#50134=EDGE_CURVE('',#39117,#39118,#29162,.T.);
#50135=EDGE_CURVE('',#39119,#39118,#20754,.T.);
#50136=EDGE_CURVE('',#39119,#39120,#29163,.T.);
#50137=EDGE_CURVE('',#39121,#39120,#318,.T.);
#50138=EDGE_CURVE('',#39121,#39122,#20755,.T.);
#50139=EDGE_CURVE('',#39123,#39122,#319,.T.);
#50140=EDGE_CURVE('',#39123,#39124,#29164,.T.);
#50141=EDGE_CURVE('',#39125,#39124,#20756,.T.);
#50142=EDGE_CURVE('',#39125,#39126,#29165,.T.);
#50143=EDGE_CURVE('',#39127,#39126,#320,.T.);
#50144=EDGE_CURVE('',#39127,#39128,#20757,.T.);
#50145=EDGE_CURVE('',#39129,#39128,#321,.T.);
#50146=EDGE_CURVE('',#39129,#39130,#29166,.T.);
#50147=EDGE_CURVE('',#39131,#39130,#20758,.T.);
#50148=EDGE_CURVE('',#39131,#39132,#29167,.T.);
#50149=EDGE_CURVE('',#39133,#39132,#322,.T.);
#50150=EDGE_CURVE('',#39133,#39134,#20759,.T.);
#50151=EDGE_CURVE('',#39135,#39134,#323,.T.);
#50152=EDGE_CURVE('',#39135,#39136,#29168,.T.);
#50153=EDGE_CURVE('',#39137,#39136,#20760,.T.);
#50154=EDGE_CURVE('',#39137,#39138,#29169,.T.);
#50155=EDGE_CURVE('',#39139,#39138,#324,.T.);
#50156=EDGE_CURVE('',#39139,#39140,#20761,.T.);
#50157=EDGE_CURVE('',#39141,#39140,#325,.T.);
#50158=EDGE_CURVE('',#39141,#39142,#29170,.T.);
#50159=EDGE_CURVE('',#39143,#39142,#20762,.T.);
#50160=EDGE_CURVE('',#39143,#39144,#29171,.T.);
#50161=EDGE_CURVE('',#39145,#39144,#326,.T.);
#50162=EDGE_CURVE('',#39145,#39146,#20763,.T.);
#50163=EDGE_CURVE('',#39147,#39146,#327,.T.);
#50164=EDGE_CURVE('',#39147,#39148,#29172,.T.);
#50165=EDGE_CURVE('',#39149,#39148,#20764,.T.);
#50166=EDGE_CURVE('',#39149,#39150,#29173,.T.);
#50167=EDGE_CURVE('',#39151,#39150,#328,.T.);
#50168=EDGE_CURVE('',#39151,#39152,#20765,.T.);
#50169=EDGE_CURVE('',#39153,#39152,#329,.T.);
#50170=EDGE_CURVE('',#39153,#39154,#29174,.T.);
#50171=EDGE_CURVE('',#39155,#39154,#20766,.T.);
#50172=EDGE_CURVE('',#39155,#39156,#29175,.T.);
#50173=EDGE_CURVE('',#39157,#39156,#330,.T.);
#50174=EDGE_CURVE('',#39157,#39158,#20767,.T.);
#50175=EDGE_CURVE('',#39159,#39158,#331,.T.);
#50176=EDGE_CURVE('',#39159,#39160,#29176,.T.);
#50177=EDGE_CURVE('',#39161,#39160,#20768,.T.);
#50178=EDGE_CURVE('',#39161,#39162,#29177,.T.);
#50179=EDGE_CURVE('',#39163,#39162,#332,.T.);
#50180=EDGE_CURVE('',#39163,#39164,#20769,.T.);
#50181=EDGE_CURVE('',#39165,#39164,#333,.T.);
#50182=EDGE_CURVE('',#39165,#39166,#29178,.T.);
#50183=EDGE_CURVE('',#39167,#39166,#20770,.T.);
#50184=EDGE_CURVE('',#39167,#39168,#29179,.T.);
#50185=EDGE_CURVE('',#39169,#39168,#334,.T.);
#50186=EDGE_CURVE('',#39169,#39170,#20771,.T.);
#50187=EDGE_CURVE('',#39171,#39170,#335,.T.);
#50188=EDGE_CURVE('',#39171,#39172,#29180,.T.);
#50189=EDGE_CURVE('',#39173,#39172,#20772,.T.);
#50190=EDGE_CURVE('',#39173,#39174,#29181,.T.);
#50191=EDGE_CURVE('',#39175,#39174,#336,.T.);
#50192=EDGE_CURVE('',#39175,#39176,#20773,.T.);
#50193=EDGE_CURVE('',#39177,#39176,#337,.T.);
#50194=EDGE_CURVE('',#39177,#39178,#29182,.T.);
#50195=EDGE_CURVE('',#39179,#39178,#20774,.T.);
#50196=EDGE_CURVE('',#39179,#39180,#29183,.T.);
#50197=EDGE_CURVE('',#39181,#39180,#338,.T.);
#50198=EDGE_CURVE('',#39181,#39182,#20775,.T.);
#50199=EDGE_CURVE('',#39183,#39182,#339,.T.);
#50200=EDGE_CURVE('',#39183,#39184,#29184,.T.);
#50201=EDGE_CURVE('',#39185,#39184,#20776,.T.);
#50202=EDGE_CURVE('',#39185,#39186,#29185,.T.);
#50203=EDGE_CURVE('',#39187,#39186,#340,.T.);
#50204=EDGE_CURVE('',#39187,#39188,#20777,.T.);
#50205=EDGE_CURVE('',#39189,#39188,#341,.T.);
#50206=EDGE_CURVE('',#39189,#39190,#29186,.T.);
#50207=EDGE_CURVE('',#39191,#39190,#20778,.T.);
#50208=EDGE_CURVE('',#39191,#39192,#29187,.T.);
#50209=EDGE_CURVE('',#39193,#39192,#342,.T.);
#50210=EDGE_CURVE('',#39193,#39194,#20779,.T.);
#50211=EDGE_CURVE('',#39195,#39194,#343,.T.);
#50212=EDGE_CURVE('',#39195,#39196,#29188,.T.);
#50213=EDGE_CURVE('',#39197,#39196,#20780,.T.);
#50214=EDGE_CURVE('',#39197,#39198,#29189,.T.);
#50215=EDGE_CURVE('',#39199,#39198,#344,.T.);
#50216=EDGE_CURVE('',#39199,#39200,#20781,.T.);
#50217=EDGE_CURVE('',#39201,#39200,#345,.T.);
#50218=EDGE_CURVE('',#39201,#39202,#29190,.T.);
#50219=EDGE_CURVE('',#39203,#39202,#20782,.T.);
#50220=EDGE_CURVE('',#39203,#39204,#29191,.T.);
#50221=EDGE_CURVE('',#39205,#39204,#346,.T.);
#50222=EDGE_CURVE('',#39205,#39206,#20783,.T.);
#50223=EDGE_CURVE('',#39207,#39206,#347,.T.);
#50224=EDGE_CURVE('',#39207,#39208,#29192,.T.);
#50225=EDGE_CURVE('',#39209,#39208,#20784,.T.);
#50226=EDGE_CURVE('',#39209,#39210,#29193,.T.);
#50227=EDGE_CURVE('',#39211,#39210,#348,.T.);
#50228=EDGE_CURVE('',#39211,#39212,#20785,.T.);
#50229=EDGE_CURVE('',#39213,#39212,#349,.T.);
#50230=EDGE_CURVE('',#39213,#39214,#29194,.T.);
#50231=EDGE_CURVE('',#39215,#39214,#20786,.T.);
#50232=EDGE_CURVE('',#39215,#39216,#29195,.T.);
#50233=EDGE_CURVE('',#39217,#39216,#350,.T.);
#50234=EDGE_CURVE('',#39217,#39218,#20787,.T.);
#50235=EDGE_CURVE('',#39219,#39218,#351,.T.);
#50236=EDGE_CURVE('',#39219,#39220,#29196,.T.);
#50237=EDGE_CURVE('',#39221,#39220,#20788,.T.);
#50238=EDGE_CURVE('',#39221,#39222,#29197,.T.);
#50239=EDGE_CURVE('',#39223,#39222,#352,.T.);
#50240=EDGE_CURVE('',#39223,#39224,#20789,.T.);
#50241=EDGE_CURVE('',#39225,#39224,#353,.T.);
#50242=EDGE_CURVE('',#39225,#39226,#29198,.T.);
#50243=EDGE_CURVE('',#39227,#39226,#20790,.T.);
#50244=EDGE_CURVE('',#39227,#39228,#29199,.T.);
#50245=EDGE_CURVE('',#39229,#39228,#354,.T.);
#50246=EDGE_CURVE('',#39229,#39230,#20791,.T.);
#50247=EDGE_CURVE('',#39231,#39230,#355,.T.);
#50248=EDGE_CURVE('',#39231,#39232,#29200,.T.);
#50249=EDGE_CURVE('',#39233,#39232,#20792,.T.);
#50250=EDGE_CURVE('',#39233,#39234,#29201,.T.);
#50251=EDGE_CURVE('',#39235,#39234,#356,.T.);
#50252=EDGE_CURVE('',#39235,#39236,#20793,.T.);
#50253=EDGE_CURVE('',#39237,#39236,#357,.T.);
#50254=EDGE_CURVE('',#39237,#39238,#29202,.T.);
#50255=EDGE_CURVE('',#39239,#39238,#20794,.T.);
#50256=EDGE_CURVE('',#39239,#39240,#29203,.T.);
#50257=EDGE_CURVE('',#39241,#39240,#358,.T.);
#50258=EDGE_CURVE('',#39241,#39242,#20795,.T.);
#50259=EDGE_CURVE('',#39243,#39242,#359,.T.);
#50260=EDGE_CURVE('',#39243,#39244,#29204,.T.);
#50261=EDGE_CURVE('',#39245,#39244,#20796,.T.);
#50262=EDGE_CURVE('',#39245,#39246,#29205,.T.);
#50263=EDGE_CURVE('',#39247,#39246,#360,.T.);
#50264=EDGE_CURVE('',#39247,#39248,#20797,.T.);
#50265=EDGE_CURVE('',#39249,#39248,#361,.T.);
#50266=EDGE_CURVE('',#39249,#39250,#29206,.T.);
#50267=EDGE_CURVE('',#39251,#39250,#20798,.T.);
#50268=EDGE_CURVE('',#39251,#39252,#29207,.T.);
#50269=EDGE_CURVE('',#39253,#39252,#362,.T.);
#50270=EDGE_CURVE('',#39253,#39254,#20799,.T.);
#50271=EDGE_CURVE('',#39255,#39254,#363,.T.);
#50272=EDGE_CURVE('',#39255,#39256,#29208,.T.);
#50273=EDGE_CURVE('',#39257,#39256,#20800,.T.);
#50274=EDGE_CURVE('',#39257,#39258,#29209,.T.);
#50275=EDGE_CURVE('',#39259,#39258,#364,.T.);
#50276=EDGE_CURVE('',#39259,#39260,#20801,.T.);
#50277=EDGE_CURVE('',#39261,#39260,#365,.T.);
#50278=EDGE_CURVE('',#39261,#39262,#29210,.T.);
#50279=EDGE_CURVE('',#39263,#39262,#20802,.T.);
#50280=EDGE_CURVE('',#39263,#39264,#29211,.T.);
#50281=EDGE_CURVE('',#39265,#39264,#366,.T.);
#50282=EDGE_CURVE('',#39265,#39266,#20803,.T.);
#50283=EDGE_CURVE('',#39267,#39266,#367,.T.);
#50284=EDGE_CURVE('',#39267,#39268,#29212,.T.);
#50285=EDGE_CURVE('',#39269,#39268,#20804,.T.);
#50286=EDGE_CURVE('',#39269,#39270,#29213,.T.);
#50287=EDGE_CURVE('',#39271,#39270,#368,.T.);
#50288=EDGE_CURVE('',#39271,#39272,#20805,.T.);
#50289=EDGE_CURVE('',#39273,#39272,#369,.T.);
#50290=EDGE_CURVE('',#39273,#39274,#29214,.T.);
#50291=EDGE_CURVE('',#39275,#39274,#20806,.T.);
#50292=EDGE_CURVE('',#39275,#39276,#29215,.T.);
#50293=EDGE_CURVE('',#39277,#39276,#370,.T.);
#50294=EDGE_CURVE('',#39277,#39278,#20807,.T.);
#50295=EDGE_CURVE('',#39279,#39278,#371,.T.);
#50296=EDGE_CURVE('',#39279,#39280,#29216,.T.);
#50297=EDGE_CURVE('',#39281,#39280,#20808,.T.);
#50298=EDGE_CURVE('',#39281,#39282,#29217,.T.);
#50299=EDGE_CURVE('',#39283,#39282,#372,.T.);
#50300=EDGE_CURVE('',#39283,#39284,#20809,.T.);
#50301=EDGE_CURVE('',#39285,#39284,#373,.T.);
#50302=EDGE_CURVE('',#39285,#39286,#29218,.T.);
#50303=EDGE_CURVE('',#39287,#39286,#20810,.T.);
#50304=EDGE_CURVE('',#39287,#39288,#29219,.T.);
#50305=EDGE_CURVE('',#39289,#39288,#374,.T.);
#50306=EDGE_CURVE('',#39289,#39290,#20811,.T.);
#50307=EDGE_CURVE('',#39291,#39290,#375,.T.);
#50308=EDGE_CURVE('',#39291,#39292,#29220,.T.);
#50309=EDGE_CURVE('',#39293,#39292,#20812,.T.);
#50310=EDGE_CURVE('',#39293,#39294,#29221,.T.);
#50311=EDGE_CURVE('',#39295,#39294,#376,.T.);
#50312=EDGE_CURVE('',#39295,#39296,#20813,.T.);
#50313=EDGE_CURVE('',#39297,#39296,#377,.T.);
#50314=EDGE_CURVE('',#39297,#39298,#29222,.T.);
#50315=EDGE_CURVE('',#39299,#39298,#20814,.T.);
#50316=EDGE_CURVE('',#39299,#39300,#29223,.T.);
#50317=EDGE_CURVE('',#39301,#39300,#378,.T.);
#50318=EDGE_CURVE('',#39301,#39302,#20815,.T.);
#50319=EDGE_CURVE('',#39303,#39302,#379,.T.);
#50320=EDGE_CURVE('',#39303,#39304,#29224,.T.);
#50321=EDGE_CURVE('',#39305,#39304,#20816,.T.);
#50322=EDGE_CURVE('',#39305,#39306,#29225,.T.);
#50323=EDGE_CURVE('',#39307,#39306,#380,.T.);
#50324=EDGE_CURVE('',#39307,#39308,#20817,.T.);
#50325=EDGE_CURVE('',#39309,#39308,#381,.T.);
#50326=EDGE_CURVE('',#39309,#39310,#29226,.T.);
#50327=EDGE_CURVE('',#39311,#39310,#20818,.T.);
#50328=EDGE_CURVE('',#39311,#39312,#29227,.T.);
#50329=EDGE_CURVE('',#39313,#39312,#382,.T.);
#50330=EDGE_CURVE('',#39313,#39314,#20819,.T.);
#50331=EDGE_CURVE('',#39315,#39314,#383,.T.);
#50332=EDGE_CURVE('',#39315,#39316,#29228,.T.);
#50333=EDGE_CURVE('',#39317,#39316,#20820,.T.);
#50334=EDGE_CURVE('',#39317,#39318,#29229,.T.);
#50335=EDGE_CURVE('',#39319,#39318,#384,.T.);
#50336=EDGE_CURVE('',#39319,#39320,#20821,.T.);
#50337=EDGE_CURVE('',#39321,#39320,#385,.T.);
#50338=EDGE_CURVE('',#39321,#39322,#29230,.T.);
#50339=EDGE_CURVE('',#39323,#39322,#20822,.T.);
#50340=EDGE_CURVE('',#39323,#39324,#29231,.T.);
#50341=EDGE_CURVE('',#39325,#39324,#386,.T.);
#50342=EDGE_CURVE('',#39325,#39326,#20823,.T.);
#50343=EDGE_CURVE('',#39327,#39326,#387,.T.);
#50344=EDGE_CURVE('',#39327,#39328,#29232,.T.);
#50345=EDGE_CURVE('',#39329,#39328,#20824,.T.);
#50346=EDGE_CURVE('',#39329,#39330,#29233,.T.);
#50347=EDGE_CURVE('',#39331,#39330,#388,.T.);
#50348=EDGE_CURVE('',#39331,#39332,#20825,.T.);
#50349=EDGE_CURVE('',#39333,#39332,#389,.T.);
#50350=EDGE_CURVE('',#39333,#39334,#29234,.T.);
#50351=EDGE_CURVE('',#39335,#39334,#20826,.T.);
#50352=EDGE_CURVE('',#39335,#39336,#29235,.T.);
#50353=EDGE_CURVE('',#39337,#39336,#390,.T.);
#50354=EDGE_CURVE('',#39337,#39338,#20827,.T.);
#50355=EDGE_CURVE('',#39339,#39338,#391,.T.);
#50356=EDGE_CURVE('',#39339,#39340,#29236,.T.);
#50357=EDGE_CURVE('',#39341,#39340,#20828,.T.);
#50358=EDGE_CURVE('',#39341,#39342,#29237,.T.);
#50359=EDGE_CURVE('',#39343,#39342,#392,.T.);
#50360=EDGE_CURVE('',#39343,#39344,#20829,.T.);
#50361=EDGE_CURVE('',#39345,#39344,#393,.T.);
#50362=EDGE_CURVE('',#39345,#39346,#29238,.T.);
#50363=EDGE_CURVE('',#39347,#39346,#20830,.T.);
#50364=EDGE_CURVE('',#39347,#38655,#29239,.T.);
#50365=EDGE_CURVE('',#39348,#39347,#20831,.T.);
#50366=EDGE_CURVE('',#39348,#39349,#29240,.T.);
#50367=EDGE_CURVE('',#39350,#39349,#394,.T.);
#50368=EDGE_CURVE('',#39350,#39351,#20832,.T.);
#50369=EDGE_CURVE('',#39352,#39351,#395,.T.);
#50370=EDGE_CURVE('',#39352,#39353,#29241,.T.);
#50371=EDGE_CURVE('',#39354,#39353,#20833,.T.);
#50372=EDGE_CURVE('',#39354,#39355,#29242,.T.);
#50373=EDGE_CURVE('',#39356,#39355,#396,.T.);
#50374=EDGE_CURVE('',#39356,#39357,#20834,.T.);
#50375=EDGE_CURVE('',#39358,#39357,#397,.T.);
#50376=EDGE_CURVE('',#39358,#39359,#29243,.T.);
#50377=EDGE_CURVE('',#39360,#39359,#20835,.T.);
#50378=EDGE_CURVE('',#39360,#39361,#29244,.T.);
#50379=EDGE_CURVE('',#39362,#39361,#398,.T.);
#50380=EDGE_CURVE('',#39362,#39363,#20836,.T.);
#50381=EDGE_CURVE('',#39364,#39363,#399,.T.);
#50382=EDGE_CURVE('',#39364,#39365,#29245,.T.);
#50383=EDGE_CURVE('',#39366,#39365,#20837,.T.);
#50384=EDGE_CURVE('',#39366,#39367,#29246,.T.);
#50385=EDGE_CURVE('',#39368,#39367,#400,.T.);
#50386=EDGE_CURVE('',#39368,#39369,#20838,.T.);
#50387=EDGE_CURVE('',#39370,#39369,#401,.T.);
#50388=EDGE_CURVE('',#39370,#39371,#29247,.T.);
#50389=EDGE_CURVE('',#39372,#39371,#20839,.T.);
#50390=EDGE_CURVE('',#39372,#39373,#29248,.T.);
#50391=EDGE_CURVE('',#39374,#39373,#402,.T.);
#50392=EDGE_CURVE('',#39374,#39375,#20840,.T.);
#50393=EDGE_CURVE('',#39376,#39375,#403,.T.);
#50394=EDGE_CURVE('',#39376,#39377,#29249,.T.);
#50395=EDGE_CURVE('',#39378,#39377,#20841,.T.);
#50396=EDGE_CURVE('',#39378,#39379,#29250,.T.);
#50397=EDGE_CURVE('',#39380,#39379,#404,.T.);
#50398=EDGE_CURVE('',#39380,#39381,#20842,.T.);
#50399=EDGE_CURVE('',#39382,#39381,#405,.T.);
#50400=EDGE_CURVE('',#39382,#39383,#29251,.T.);
#50401=EDGE_CURVE('',#39384,#39383,#20843,.T.);
#50402=EDGE_CURVE('',#39384,#39385,#29252,.T.);
#50403=EDGE_CURVE('',#39386,#39385,#406,.T.);
#50404=EDGE_CURVE('',#39386,#39387,#20844,.T.);
#50405=EDGE_CURVE('',#39388,#39387,#407,.T.);
#50406=EDGE_CURVE('',#39388,#39389,#29253,.T.);
#50407=EDGE_CURVE('',#39390,#39389,#20845,.T.);
#50408=EDGE_CURVE('',#39390,#39391,#29254,.T.);
#50409=EDGE_CURVE('',#39392,#39391,#408,.T.);
#50410=EDGE_CURVE('',#39392,#39393,#20846,.T.);
#50411=EDGE_CURVE('',#39394,#39393,#409,.T.);
#50412=EDGE_CURVE('',#39394,#39395,#29255,.T.);
#50413=EDGE_CURVE('',#39396,#39395,#20847,.T.);
#50414=EDGE_CURVE('',#39396,#39397,#29256,.T.);
#50415=EDGE_CURVE('',#39398,#39397,#410,.T.);
#50416=EDGE_CURVE('',#39398,#39399,#20848,.T.);
#50417=EDGE_CURVE('',#39400,#39399,#411,.T.);
#50418=EDGE_CURVE('',#39400,#39401,#29257,.T.);
#50419=EDGE_CURVE('',#39402,#39401,#20849,.T.);
#50420=EDGE_CURVE('',#39402,#39403,#29258,.T.);
#50421=EDGE_CURVE('',#39404,#39403,#412,.T.);
#50422=EDGE_CURVE('',#39404,#39405,#20850,.T.);
#50423=EDGE_CURVE('',#39406,#39405,#413,.T.);
#50424=EDGE_CURVE('',#39406,#39407,#29259,.T.);
#50425=EDGE_CURVE('',#39408,#39407,#20851,.T.);
#50426=EDGE_CURVE('',#39408,#39409,#29260,.T.);
#50427=EDGE_CURVE('',#39410,#39409,#414,.T.);
#50428=EDGE_CURVE('',#39410,#39411,#20852,.T.);
#50429=EDGE_CURVE('',#39412,#39411,#415,.T.);
#50430=EDGE_CURVE('',#39412,#39413,#29261,.T.);
#50431=EDGE_CURVE('',#39414,#39413,#20853,.T.);
#50432=EDGE_CURVE('',#39414,#39415,#29262,.T.);
#50433=EDGE_CURVE('',#39416,#39415,#416,.T.);
#50434=EDGE_CURVE('',#39416,#39417,#20854,.T.);
#50435=EDGE_CURVE('',#39418,#39417,#417,.T.);
#50436=EDGE_CURVE('',#39418,#39419,#29263,.T.);
#50437=EDGE_CURVE('',#39420,#39419,#20855,.T.);
#50438=EDGE_CURVE('',#39420,#39421,#29264,.T.);
#50439=EDGE_CURVE('',#39422,#39421,#418,.T.);
#50440=EDGE_CURVE('',#39422,#39423,#20856,.T.);
#50441=EDGE_CURVE('',#39424,#39423,#419,.T.);
#50442=EDGE_CURVE('',#39424,#39425,#29265,.T.);
#50443=EDGE_CURVE('',#39426,#39425,#20857,.T.);
#50444=EDGE_CURVE('',#39426,#39427,#29266,.T.);
#50445=EDGE_CURVE('',#39428,#39427,#420,.T.);
#50446=EDGE_CURVE('',#39428,#39429,#20858,.T.);
#50447=EDGE_CURVE('',#39430,#39429,#421,.T.);
#50448=EDGE_CURVE('',#39430,#39431,#29267,.T.);
#50449=EDGE_CURVE('',#39432,#39431,#20859,.T.);
#50450=EDGE_CURVE('',#39432,#39433,#29268,.T.);
#50451=EDGE_CURVE('',#39434,#39433,#422,.T.);
#50452=EDGE_CURVE('',#39434,#39435,#20860,.T.);
#50453=EDGE_CURVE('',#39436,#39435,#423,.T.);
#50454=EDGE_CURVE('',#39436,#39437,#29269,.T.);
#50455=EDGE_CURVE('',#39438,#39437,#20861,.T.);
#50456=EDGE_CURVE('',#39438,#39439,#29270,.T.);
#50457=EDGE_CURVE('',#39440,#39439,#424,.T.);
#50458=EDGE_CURVE('',#39440,#39441,#20862,.T.);
#50459=EDGE_CURVE('',#39442,#39441,#425,.T.);
#50460=EDGE_CURVE('',#39442,#39443,#29271,.T.);
#50461=EDGE_CURVE('',#39444,#39443,#20863,.T.);
#50462=EDGE_CURVE('',#39444,#39445,#29272,.T.);
#50463=EDGE_CURVE('',#39446,#39445,#426,.T.);
#50464=EDGE_CURVE('',#39446,#39447,#20864,.T.);
#50465=EDGE_CURVE('',#39448,#39447,#427,.T.);
#50466=EDGE_CURVE('',#39448,#39449,#29273,.T.);
#50467=EDGE_CURVE('',#39450,#39449,#20865,.T.);
#50468=EDGE_CURVE('',#39450,#39451,#29274,.T.);
#50469=EDGE_CURVE('',#39452,#39451,#428,.T.);
#50470=EDGE_CURVE('',#39452,#39453,#20866,.T.);
#50471=EDGE_CURVE('',#39454,#39453,#429,.T.);
#50472=EDGE_CURVE('',#39454,#39455,#29275,.T.);
#50473=EDGE_CURVE('',#39456,#39455,#20867,.T.);
#50474=EDGE_CURVE('',#39456,#39457,#29276,.T.);
#50475=EDGE_CURVE('',#39458,#39457,#430,.T.);
#50476=EDGE_CURVE('',#39458,#39459,#20868,.T.);
#50477=EDGE_CURVE('',#39460,#39459,#431,.T.);
#50478=EDGE_CURVE('',#39460,#39461,#29277,.T.);
#50479=EDGE_CURVE('',#39462,#39461,#20869,.T.);
#50480=EDGE_CURVE('',#39462,#39463,#29278,.T.);
#50481=EDGE_CURVE('',#39464,#39463,#432,.T.);
#50482=EDGE_CURVE('',#39464,#39465,#20870,.T.);
#50483=EDGE_CURVE('',#39466,#39465,#433,.T.);
#50484=EDGE_CURVE('',#39466,#39467,#29279,.T.);
#50485=EDGE_CURVE('',#39468,#39467,#20871,.T.);
#50486=EDGE_CURVE('',#39468,#39469,#29280,.T.);
#50487=EDGE_CURVE('',#39470,#39469,#434,.T.);
#50488=EDGE_CURVE('',#39470,#39471,#20872,.T.);
#50489=EDGE_CURVE('',#39472,#39471,#435,.T.);
#50490=EDGE_CURVE('',#39472,#39473,#29281,.T.);
#50491=EDGE_CURVE('',#39474,#39473,#20873,.T.);
#50492=EDGE_CURVE('',#39474,#39475,#29282,.T.);
#50493=EDGE_CURVE('',#39476,#39475,#436,.T.);
#50494=EDGE_CURVE('',#39476,#39477,#20874,.T.);
#50495=EDGE_CURVE('',#39478,#39477,#437,.T.);
#50496=EDGE_CURVE('',#39478,#39479,#29283,.T.);
#50497=EDGE_CURVE('',#39480,#39479,#20875,.T.);
#50498=EDGE_CURVE('',#39480,#39481,#29284,.T.);
#50499=EDGE_CURVE('',#39482,#39481,#438,.T.);
#50500=EDGE_CURVE('',#39482,#39483,#20876,.T.);
#50501=EDGE_CURVE('',#39484,#39483,#439,.T.);
#50502=EDGE_CURVE('',#39484,#39485,#29285,.T.);
#50503=EDGE_CURVE('',#39486,#39485,#20877,.T.);
#50504=EDGE_CURVE('',#39486,#39487,#29286,.T.);
#50505=EDGE_CURVE('',#39488,#39487,#440,.T.);
#50506=EDGE_CURVE('',#39488,#39489,#20878,.T.);
#50507=EDGE_CURVE('',#39490,#39489,#441,.T.);
#50508=EDGE_CURVE('',#39490,#39491,#29287,.T.);
#50509=EDGE_CURVE('',#39492,#39491,#20879,.T.);
#50510=EDGE_CURVE('',#39492,#39493,#29288,.T.);
#50511=EDGE_CURVE('',#39494,#39493,#442,.T.);
#50512=EDGE_CURVE('',#39494,#39495,#20880,.T.);
#50513=EDGE_CURVE('',#39496,#39495,#443,.T.);
#50514=EDGE_CURVE('',#39496,#39497,#29289,.T.);
#50515=EDGE_CURVE('',#39498,#39497,#20881,.T.);
#50516=EDGE_CURVE('',#39498,#39499,#29290,.T.);
#50517=EDGE_CURVE('',#39500,#39499,#444,.T.);
#50518=EDGE_CURVE('',#39500,#39501,#20882,.T.);
#50519=EDGE_CURVE('',#39502,#39501,#445,.T.);
#50520=EDGE_CURVE('',#39502,#39503,#29291,.T.);
#50521=EDGE_CURVE('',#39504,#39503,#20883,.T.);
#50522=EDGE_CURVE('',#39504,#39505,#29292,.T.);
#50523=EDGE_CURVE('',#39506,#39505,#446,.T.);
#50524=EDGE_CURVE('',#39506,#39507,#20884,.T.);
#50525=EDGE_CURVE('',#39508,#39507,#447,.T.);
#50526=EDGE_CURVE('',#39508,#39509,#29293,.T.);
#50527=EDGE_CURVE('',#39510,#39509,#20885,.T.);
#50528=EDGE_CURVE('',#39510,#39511,#29294,.T.);
#50529=EDGE_CURVE('',#39512,#39511,#448,.T.);
#50530=EDGE_CURVE('',#39512,#39513,#20886,.T.);
#50531=EDGE_CURVE('',#39514,#39513,#449,.T.);
#50532=EDGE_CURVE('',#39514,#39515,#29295,.T.);
#50533=EDGE_CURVE('',#39516,#39515,#20887,.T.);
#50534=EDGE_CURVE('',#39516,#39517,#29296,.T.);
#50535=EDGE_CURVE('',#39518,#39517,#450,.T.);
#50536=EDGE_CURVE('',#39518,#39519,#20888,.T.);
#50537=EDGE_CURVE('',#39520,#39519,#451,.T.);
#50538=EDGE_CURVE('',#39520,#39521,#29297,.T.);
#50539=EDGE_CURVE('',#39522,#39521,#20889,.T.);
#50540=EDGE_CURVE('',#39522,#39523,#29298,.T.);
#50541=EDGE_CURVE('',#39524,#39523,#452,.T.);
#50542=EDGE_CURVE('',#39524,#39525,#20890,.T.);
#50543=EDGE_CURVE('',#39526,#39525,#453,.T.);
#50544=EDGE_CURVE('',#39526,#39527,#29299,.T.);
#50545=EDGE_CURVE('',#39528,#39527,#20891,.T.);
#50546=EDGE_CURVE('',#39528,#39529,#29300,.T.);
#50547=EDGE_CURVE('',#39530,#39529,#454,.T.);
#50548=EDGE_CURVE('',#39530,#39531,#20892,.T.);
#50549=EDGE_CURVE('',#39532,#39531,#455,.T.);
#50550=EDGE_CURVE('',#39532,#39533,#29301,.T.);
#50551=EDGE_CURVE('',#39534,#39533,#20893,.T.);
#50552=EDGE_CURVE('',#39534,#39535,#29302,.T.);
#50553=EDGE_CURVE('',#39536,#39535,#456,.T.);
#50554=EDGE_CURVE('',#39536,#39537,#20894,.T.);
#50555=EDGE_CURVE('',#39538,#39537,#457,.T.);
#50556=EDGE_CURVE('',#39538,#39539,#29303,.T.);
#50557=EDGE_CURVE('',#39540,#39539,#20895,.T.);
#50558=EDGE_CURVE('',#39540,#39541,#29304,.T.);
#50559=EDGE_CURVE('',#39542,#39541,#458,.T.);
#50560=EDGE_CURVE('',#39542,#39543,#20896,.T.);
#50561=EDGE_CURVE('',#39544,#39543,#459,.T.);
#50562=EDGE_CURVE('',#39544,#39545,#29305,.T.);
#50563=EDGE_CURVE('',#39546,#39545,#20897,.T.);
#50564=EDGE_CURVE('',#39546,#39547,#29306,.T.);
#50565=EDGE_CURVE('',#39548,#39547,#460,.T.);
#50566=EDGE_CURVE('',#39548,#39549,#20898,.T.);
#50567=EDGE_CURVE('',#39550,#39549,#461,.T.);
#50568=EDGE_CURVE('',#39550,#39551,#29307,.T.);
#50569=EDGE_CURVE('',#39552,#39551,#20899,.T.);
#50570=EDGE_CURVE('',#39552,#39553,#29308,.T.);
#50571=EDGE_CURVE('',#39554,#39553,#462,.T.);
#50572=EDGE_CURVE('',#39554,#39555,#20900,.T.);
#50573=EDGE_CURVE('',#39556,#39555,#463,.T.);
#50574=EDGE_CURVE('',#39556,#39557,#29309,.T.);
#50575=EDGE_CURVE('',#39558,#39557,#20901,.T.);
#50576=EDGE_CURVE('',#39558,#39559,#29310,.T.);
#50577=EDGE_CURVE('',#39560,#39559,#464,.T.);
#50578=EDGE_CURVE('',#39560,#39561,#20902,.T.);
#50579=EDGE_CURVE('',#39562,#39561,#465,.T.);
#50580=EDGE_CURVE('',#39562,#39563,#29311,.T.);
#50581=EDGE_CURVE('',#39564,#39563,#20903,.T.);
#50582=EDGE_CURVE('',#39564,#39565,#29312,.T.);
#50583=EDGE_CURVE('',#39566,#39565,#466,.T.);
#50584=EDGE_CURVE('',#39566,#39567,#20904,.T.);
#50585=EDGE_CURVE('',#39568,#39567,#467,.T.);
#50586=EDGE_CURVE('',#39568,#39569,#29313,.T.);
#50587=EDGE_CURVE('',#39570,#39569,#20905,.T.);
#50588=EDGE_CURVE('',#39570,#39571,#29314,.T.);
#50589=EDGE_CURVE('',#39572,#39571,#468,.T.);
#50590=EDGE_CURVE('',#39572,#39573,#20906,.T.);
#50591=EDGE_CURVE('',#39574,#39573,#469,.T.);
#50592=EDGE_CURVE('',#39574,#39575,#29315,.T.);
#50593=EDGE_CURVE('',#39576,#39575,#20907,.T.);
#50594=EDGE_CURVE('',#39576,#39577,#29316,.T.);
#50595=EDGE_CURVE('',#39578,#39577,#470,.T.);
#50596=EDGE_CURVE('',#39578,#39579,#20908,.T.);
#50597=EDGE_CURVE('',#39580,#39579,#471,.T.);
#50598=EDGE_CURVE('',#39580,#39581,#29317,.T.);
#50599=EDGE_CURVE('',#39582,#39581,#20909,.T.);
#50600=EDGE_CURVE('',#39582,#39583,#29318,.T.);
#50601=EDGE_CURVE('',#39584,#39583,#472,.T.);
#50602=EDGE_CURVE('',#39584,#39585,#20910,.T.);
#50603=EDGE_CURVE('',#39586,#39585,#473,.T.);
#50604=EDGE_CURVE('',#39586,#39587,#29319,.T.);
#50605=EDGE_CURVE('',#39588,#39587,#20911,.T.);
#50606=EDGE_CURVE('',#39588,#39589,#29320,.T.);
#50607=EDGE_CURVE('',#39590,#39589,#474,.T.);
#50608=EDGE_CURVE('',#39590,#39591,#20912,.T.);
#50609=EDGE_CURVE('',#39592,#39591,#475,.T.);
#50610=EDGE_CURVE('',#39592,#39593,#29321,.T.);
#50611=EDGE_CURVE('',#39594,#39593,#20913,.T.);
#50612=EDGE_CURVE('',#39594,#39595,#29322,.T.);
#50613=EDGE_CURVE('',#39596,#39595,#476,.T.);
#50614=EDGE_CURVE('',#39596,#39597,#20914,.T.);
#50615=EDGE_CURVE('',#39598,#39597,#477,.T.);
#50616=EDGE_CURVE('',#39598,#39599,#29323,.T.);
#50617=EDGE_CURVE('',#39600,#39599,#20915,.T.);
#50618=EDGE_CURVE('',#39600,#39601,#29324,.T.);
#50619=EDGE_CURVE('',#39602,#39601,#478,.T.);
#50620=EDGE_CURVE('',#39602,#39603,#20916,.T.);
#50621=EDGE_CURVE('',#39604,#39603,#479,.T.);
#50622=EDGE_CURVE('',#39604,#39605,#29325,.T.);
#50623=EDGE_CURVE('',#39606,#39605,#20917,.T.);
#50624=EDGE_CURVE('',#39606,#39607,#29326,.T.);
#50625=EDGE_CURVE('',#39608,#39607,#480,.T.);
#50626=EDGE_CURVE('',#39608,#39609,#20918,.T.);
#50627=EDGE_CURVE('',#39610,#39609,#481,.T.);
#50628=EDGE_CURVE('',#39610,#39611,#29327,.T.);
#50629=EDGE_CURVE('',#39612,#39611,#20919,.T.);
#50630=EDGE_CURVE('',#39612,#39613,#29328,.T.);
#50631=EDGE_CURVE('',#39614,#39613,#482,.T.);
#50632=EDGE_CURVE('',#39614,#39615,#20920,.T.);
#50633=EDGE_CURVE('',#39616,#39615,#483,.T.);
#50634=EDGE_CURVE('',#39616,#39617,#29329,.T.);
#50635=EDGE_CURVE('',#39618,#39617,#20921,.T.);
#50636=EDGE_CURVE('',#39618,#39619,#29330,.T.);
#50637=EDGE_CURVE('',#39620,#39619,#484,.T.);
#50638=EDGE_CURVE('',#39620,#39621,#20922,.T.);
#50639=EDGE_CURVE('',#39622,#39621,#485,.T.);
#50640=EDGE_CURVE('',#39622,#39623,#29331,.T.);
#50641=EDGE_CURVE('',#39624,#39623,#20923,.T.);
#50642=EDGE_CURVE('',#39624,#39625,#29332,.T.);
#50643=EDGE_CURVE('',#39626,#39625,#486,.T.);
#50644=EDGE_CURVE('',#39626,#39627,#20924,.T.);
#50645=EDGE_CURVE('',#39628,#39627,#487,.T.);
#50646=EDGE_CURVE('',#39628,#39629,#29333,.T.);
#50647=EDGE_CURVE('',#39630,#39629,#20925,.T.);
#50648=EDGE_CURVE('',#39630,#39631,#29334,.T.);
#50649=EDGE_CURVE('',#39632,#39631,#488,.T.);
#50650=EDGE_CURVE('',#39632,#39633,#20926,.T.);
#50651=EDGE_CURVE('',#39634,#39633,#489,.T.);
#50652=EDGE_CURVE('',#39634,#39635,#29335,.T.);
#50653=EDGE_CURVE('',#39636,#39635,#20927,.T.);
#50654=EDGE_CURVE('',#39636,#39637,#29336,.T.);
#50655=EDGE_CURVE('',#39638,#39637,#490,.T.);
#50656=EDGE_CURVE('',#39638,#39639,#20928,.T.);
#50657=EDGE_CURVE('',#39640,#39639,#491,.T.);
#50658=EDGE_CURVE('',#39640,#39053,#29337,.T.);
#50659=EDGE_CURVE('',#39053,#38856,#492,.T.);
#50660=EDGE_CURVE('',#38852,#39052,#493,.T.);
#50661=EDGE_CURVE('',#38820,#39101,#494,.T.);
#50662=EDGE_CURVE('',#39100,#38821,#495,.T.);
#50663=EDGE_CURVE('',#39106,#38817,#496,.T.);
#50664=EDGE_CURVE('',#38816,#39107,#497,.T.);
#50665=EDGE_CURVE('',#39112,#38813,#498,.T.);
#50666=EDGE_CURVE('',#38812,#39113,#499,.T.);
#50667=EDGE_CURVE('',#39118,#38809,#500,.T.);
#50668=EDGE_CURVE('',#38808,#39119,#501,.T.);
#50669=EDGE_CURVE('',#39124,#38805,#502,.T.);
#50670=EDGE_CURVE('',#38804,#39125,#503,.T.);
#50671=EDGE_CURVE('',#39130,#38801,#504,.T.);
#50672=EDGE_CURVE('',#38800,#39131,#505,.T.);
#50673=EDGE_CURVE('',#39136,#38797,#506,.T.);
#50674=EDGE_CURVE('',#38796,#39137,#507,.T.);
#50675=EDGE_CURVE('',#39142,#38793,#508,.T.);
#50676=EDGE_CURVE('',#38792,#39143,#509,.T.);
#50677=EDGE_CURVE('',#39148,#38789,#510,.T.);
#50678=EDGE_CURVE('',#38788,#39149,#511,.T.);
#50679=EDGE_CURVE('',#39154,#38785,#512,.T.);
#50680=EDGE_CURVE('',#38784,#39155,#513,.T.);
#50681=EDGE_CURVE('',#39160,#38781,#514,.T.);
#50682=EDGE_CURVE('',#38780,#39161,#515,.T.);
#50683=EDGE_CURVE('',#39166,#38777,#516,.T.);
#50684=EDGE_CURVE('',#38776,#39167,#517,.T.);
#50685=EDGE_CURVE('',#39172,#38773,#518,.T.);
#50686=EDGE_CURVE('',#38772,#39173,#519,.T.);
#50687=EDGE_CURVE('',#39178,#38769,#520,.T.);
#50688=EDGE_CURVE('',#38768,#39179,#521,.T.);
#50689=EDGE_CURVE('',#39184,#38765,#522,.T.);
#50690=EDGE_CURVE('',#38764,#39185,#523,.T.);
#50691=EDGE_CURVE('',#39190,#38761,#524,.T.);
#50692=EDGE_CURVE('',#38760,#39191,#525,.T.);
#50693=EDGE_CURVE('',#39196,#38757,#526,.T.);
#50694=EDGE_CURVE('',#38756,#39197,#527,.T.);
#50695=EDGE_CURVE('',#39202,#38753,#528,.T.);
#50696=EDGE_CURVE('',#38752,#39203,#529,.T.);
#50697=EDGE_CURVE('',#39208,#38749,#530,.T.);
#50698=EDGE_CURVE('',#38748,#39209,#531,.T.);
#50699=EDGE_CURVE('',#39214,#38745,#532,.T.);
#50700=EDGE_CURVE('',#38744,#39215,#533,.T.);
#50701=EDGE_CURVE('',#39220,#38741,#534,.T.);
#50702=EDGE_CURVE('',#38740,#39221,#535,.T.);
#50703=EDGE_CURVE('',#39226,#38737,#536,.T.);
#50704=EDGE_CURVE('',#38736,#39227,#537,.T.);
#50705=EDGE_CURVE('',#39232,#38733,#538,.T.);
#50706=EDGE_CURVE('',#38732,#39233,#539,.T.);
#50707=EDGE_CURVE('',#39238,#38729,#540,.T.);
#50708=EDGE_CURVE('',#38728,#39239,#541,.T.);
#50709=EDGE_CURVE('',#39244,#38725,#542,.T.);
#50710=EDGE_CURVE('',#38724,#39245,#543,.T.);
#50711=EDGE_CURVE('',#39250,#38721,#544,.T.);
#50712=EDGE_CURVE('',#38720,#39251,#545,.T.);
#50713=EDGE_CURVE('',#39256,#38717,#546,.T.);
#50714=EDGE_CURVE('',#38716,#39257,#547,.T.);
#50715=EDGE_CURVE('',#39262,#38713,#548,.T.);
#50716=EDGE_CURVE('',#38712,#39263,#549,.T.);
#50717=EDGE_CURVE('',#39268,#38709,#550,.T.);
#50718=EDGE_CURVE('',#38708,#39269,#551,.T.);
#50719=EDGE_CURVE('',#39274,#38705,#552,.T.);
#50720=EDGE_CURVE('',#38704,#39275,#553,.T.);
#50721=EDGE_CURVE('',#39280,#38701,#554,.T.);
#50722=EDGE_CURVE('',#38700,#39281,#555,.T.);
#50723=EDGE_CURVE('',#39286,#38697,#556,.T.);
#50724=EDGE_CURVE('',#38696,#39287,#557,.T.);
#50725=EDGE_CURVE('',#39292,#38693,#558,.T.);
#50726=EDGE_CURVE('',#38692,#39293,#559,.T.);
#50727=EDGE_CURVE('',#39298,#38689,#560,.T.);
#50728=EDGE_CURVE('',#38688,#39299,#561,.T.);
#50729=EDGE_CURVE('',#39304,#38685,#562,.T.);
#50730=EDGE_CURVE('',#38684,#39305,#563,.T.);
#50731=EDGE_CURVE('',#39310,#38681,#564,.T.);
#50732=EDGE_CURVE('',#38680,#39311,#565,.T.);
#50733=EDGE_CURVE('',#39316,#38677,#566,.T.);
#50734=EDGE_CURVE('',#38676,#39317,#567,.T.);
#50735=EDGE_CURVE('',#39322,#38673,#568,.T.);
#50736=EDGE_CURVE('',#38672,#39323,#569,.T.);
#50737=EDGE_CURVE('',#39328,#38669,#570,.T.);
#50738=EDGE_CURVE('',#38668,#39329,#571,.T.);
#50739=EDGE_CURVE('',#39334,#38665,#572,.T.);
#50740=EDGE_CURVE('',#38664,#39335,#573,.T.);
#50741=EDGE_CURVE('',#39340,#38661,#574,.T.);
#50742=EDGE_CURVE('',#38660,#39341,#575,.T.);
#50743=EDGE_CURVE('',#39346,#38657,#576,.T.);
#50744=EDGE_CURVE('',#38656,#39348,#577,.T.);
#50745=EDGE_CURVE('',#39353,#39048,#578,.T.);
#50746=EDGE_CURVE('',#39047,#39354,#579,.T.);
#50747=EDGE_CURVE('',#39359,#39044,#580,.T.);
#50748=EDGE_CURVE('',#39043,#39360,#581,.T.);
#50749=EDGE_CURVE('',#39365,#39040,#582,.T.);
#50750=EDGE_CURVE('',#39039,#39366,#583,.T.);
#50751=EDGE_CURVE('',#39371,#39036,#584,.T.);
#50752=EDGE_CURVE('',#39035,#39372,#585,.T.);
#50753=EDGE_CURVE('',#39377,#39032,#586,.T.);
#50754=EDGE_CURVE('',#39031,#39378,#587,.T.);
#50755=EDGE_CURVE('',#39383,#39028,#588,.T.);
#50756=EDGE_CURVE('',#39027,#39384,#589,.T.);
#50757=EDGE_CURVE('',#39389,#39024,#590,.T.);
#50758=EDGE_CURVE('',#39023,#39390,#591,.T.);
#50759=EDGE_CURVE('',#39395,#39020,#592,.T.);
#50760=EDGE_CURVE('',#39019,#39396,#593,.T.);
#50761=EDGE_CURVE('',#39401,#39016,#594,.T.);
#50762=EDGE_CURVE('',#39015,#39402,#595,.T.);
#50763=EDGE_CURVE('',#39407,#39012,#596,.T.);
#50764=EDGE_CURVE('',#39011,#39408,#597,.T.);
#50765=EDGE_CURVE('',#39413,#39008,#598,.T.);
#50766=EDGE_CURVE('',#39007,#39414,#599,.T.);
#50767=EDGE_CURVE('',#39419,#39004,#600,.T.);
#50768=EDGE_CURVE('',#39003,#39420,#601,.T.);
#50769=EDGE_CURVE('',#39425,#39000,#602,.T.);
#50770=EDGE_CURVE('',#38999,#39426,#603,.T.);
#50771=EDGE_CURVE('',#39431,#38996,#604,.T.);
#50772=EDGE_CURVE('',#38995,#39432,#605,.T.);
#50773=EDGE_CURVE('',#39437,#38992,#606,.T.);
#50774=EDGE_CURVE('',#38991,#39438,#607,.T.);
#50775=EDGE_CURVE('',#39443,#38988,#608,.T.);
#50776=EDGE_CURVE('',#38987,#39444,#609,.T.);
#50777=EDGE_CURVE('',#39449,#38984,#610,.T.);
#50778=EDGE_CURVE('',#38983,#39450,#611,.T.);
#50779=EDGE_CURVE('',#39455,#38980,#612,.T.);
#50780=EDGE_CURVE('',#38979,#39456,#613,.T.);
#50781=EDGE_CURVE('',#39461,#38976,#614,.T.);
#50782=EDGE_CURVE('',#38975,#39462,#615,.T.);
#50783=EDGE_CURVE('',#39467,#38972,#616,.T.);
#50784=EDGE_CURVE('',#38971,#39468,#617,.T.);
#50785=EDGE_CURVE('',#39473,#38968,#618,.T.);
#50786=EDGE_CURVE('',#38967,#39474,#619,.T.);
#50787=EDGE_CURVE('',#39479,#38964,#620,.T.);
#50788=EDGE_CURVE('',#38963,#39480,#621,.T.);
#50789=EDGE_CURVE('',#38824,#39095,#622,.T.);
#50790=EDGE_CURVE('',#39094,#38825,#623,.T.);
#50791=EDGE_CURVE('',#38828,#39089,#624,.T.);
#50792=EDGE_CURVE('',#39088,#38829,#625,.T.);
#50793=EDGE_CURVE('',#38832,#39083,#626,.T.);
#50794=EDGE_CURVE('',#39082,#38833,#627,.T.);
#50795=EDGE_CURVE('',#38836,#39077,#628,.T.);
#50796=EDGE_CURVE('',#39076,#38837,#629,.T.);
#50797=EDGE_CURVE('',#38840,#39071,#630,.T.);
#50798=EDGE_CURVE('',#39070,#38841,#631,.T.);
#50799=EDGE_CURVE('',#38844,#39065,#632,.T.);
#50800=EDGE_CURVE('',#39064,#38845,#633,.T.);
#50801=EDGE_CURVE('',#38848,#39059,#634,.T.);
#50802=EDGE_CURVE('',#39058,#38849,#635,.T.);
#50803=EDGE_CURVE('',#38859,#39636,#636,.T.);
#50804=EDGE_CURVE('',#39635,#38860,#637,.T.);
#50805=EDGE_CURVE('',#38863,#39630,#638,.T.);
#50806=EDGE_CURVE('',#39629,#38864,#639,.T.);
#50807=EDGE_CURVE('',#38867,#39624,#640,.T.);
#50808=EDGE_CURVE('',#39623,#38868,#641,.T.);
#50809=EDGE_CURVE('',#38871,#39618,#642,.T.);
#50810=EDGE_CURVE('',#39617,#38872,#643,.T.);
#50811=EDGE_CURVE('',#38875,#39612,#644,.T.);
#50812=EDGE_CURVE('',#39611,#38876,#645,.T.);
#50813=EDGE_CURVE('',#38879,#39606,#646,.T.);
#50814=EDGE_CURVE('',#39605,#38880,#647,.T.);
#50815=EDGE_CURVE('',#38883,#39600,#648,.T.);
#50816=EDGE_CURVE('',#39599,#38884,#649,.T.);
#50817=EDGE_CURVE('',#38887,#39594,#650,.T.);
#50818=EDGE_CURVE('',#39593,#38888,#651,.T.);
#50819=EDGE_CURVE('',#38891,#39588,#652,.T.);
#50820=EDGE_CURVE('',#39587,#38892,#653,.T.);
#50821=EDGE_CURVE('',#38895,#39582,#654,.T.);
#50822=EDGE_CURVE('',#39581,#38896,#655,.T.);
#50823=EDGE_CURVE('',#38899,#39576,#656,.T.);
#50824=EDGE_CURVE('',#39575,#38900,#657,.T.);
#50825=EDGE_CURVE('',#38903,#39570,#658,.T.);
#50826=EDGE_CURVE('',#39569,#38904,#659,.T.);
#50827=EDGE_CURVE('',#38907,#39564,#660,.T.);
#50828=EDGE_CURVE('',#39563,#38908,#661,.T.);
#50829=EDGE_CURVE('',#38911,#39558,#662,.T.);
#50830=EDGE_CURVE('',#39557,#38912,#663,.T.);
#50831=EDGE_CURVE('',#38915,#39552,#664,.T.);
#50832=EDGE_CURVE('',#39551,#38916,#665,.T.);
#50833=EDGE_CURVE('',#38919,#39546,#666,.T.);
#50834=EDGE_CURVE('',#39545,#38920,#667,.T.);
#50835=EDGE_CURVE('',#38923,#39540,#668,.T.);
#50836=EDGE_CURVE('',#39539,#38924,#669,.T.);
#50837=EDGE_CURVE('',#38927,#39534,#670,.T.);
#50838=EDGE_CURVE('',#39533,#38928,#671,.T.);
#50839=EDGE_CURVE('',#38931,#39528,#672,.T.);
#50840=EDGE_CURVE('',#39527,#38932,#673,.T.);
#50841=EDGE_CURVE('',#38935,#39522,#674,.T.);
#50842=EDGE_CURVE('',#39521,#38936,#675,.T.);
#50843=EDGE_CURVE('',#38939,#39516,#676,.T.);
#50844=EDGE_CURVE('',#39515,#38940,#677,.T.);
#50845=EDGE_CURVE('',#38943,#39510,#678,.T.);
#50846=EDGE_CURVE('',#39509,#38944,#679,.T.);
#50847=EDGE_CURVE('',#38947,#39504,#680,.T.);
#50848=EDGE_CURVE('',#39503,#38948,#681,.T.);
#50849=EDGE_CURVE('',#38951,#39498,#682,.T.);
#50850=EDGE_CURVE('',#39497,#38952,#683,.T.);
#50851=EDGE_CURVE('',#39485,#38960,#684,.T.);
#50852=EDGE_CURVE('',#38959,#39486,#685,.T.);
#50853=EDGE_CURVE('',#39641,#39642,#29338,.T.);
#50854=EDGE_CURVE('',#39642,#39643,#24971,.T.);
#50855=EDGE_CURVE('',#39644,#39643,#29339,.T.);
#50856=EDGE_CURVE('',#39644,#39641,#20929,.T.);
#50857=EDGE_CURVE('',#39645,#39646,#686,.T.);
#50858=EDGE_CURVE('',#39646,#39642,#24972,.T.);
#50859=EDGE_CURVE('',#39641,#39647,#24973,.T.);
#50860=EDGE_CURVE('',#39647,#39645,#29340,.T.);
#50861=EDGE_CURVE('',#39643,#39648,#24974,.T.);
#50862=EDGE_CURVE('',#39648,#39649,#687,.T.);
#50863=EDGE_CURVE('',#39649,#39650,#29341,.T.);
#50864=EDGE_CURVE('',#39650,#39644,#24975,.T.);
#50865=EDGE_CURVE('',#39651,#38644,#29342,.T.);
#50866=EDGE_CURVE('',#38649,#39651,#29343,.T.);
#50867=EDGE_CURVE('',#39652,#38649,#29344,.T.);
#50868=EDGE_CURVE('',#38648,#39652,#29345,.T.);
#50869=EDGE_CURVE('',#39653,#38648,#29346,.T.);
#50870=EDGE_CURVE('',#38647,#39653,#29347,.T.);
#50871=EDGE_CURVE('',#39654,#38647,#29348,.T.);
#50872=EDGE_CURVE('',#38646,#39654,#29349,.T.);
#50873=EDGE_CURVE('',#39655,#38646,#29350,.T.);
#50874=EDGE_CURVE('',#38645,#39655,#29351,.T.);
#50875=EDGE_CURVE('',#39656,#39657,#20930,.T.);
#50876=EDGE_CURVE('',#38650,#39656,#20931,.T.);
#50877=EDGE_CURVE('',#39658,#38651,#20932,.T.);
#50878=EDGE_CURVE('',#39659,#39658,#20933,.T.);
#50879=EDGE_CURVE('',#39657,#39659,#20934,.T.);
#50880=EDGE_CURVE('',#39491,#38956,#688,.T.);
#50881=EDGE_CURVE('',#38955,#39492,#689,.T.);
#50882=EDGE_CURVE('',#39653,#38650,#29352,.T.);
#50883=EDGE_CURVE('',#39656,#38650,#4319,.T.);
#50884=EDGE_CURVE('',#39652,#39656,#29353,.T.);
#50885=EDGE_CURVE('',#39654,#38651,#29354,.T.);
#50886=EDGE_CURVE('',#39655,#39658,#29355,.T.);
#50887=EDGE_CURVE('',#38651,#39658,#4320,.T.);
#50888=EDGE_CURVE('',#39660,#39659,#29356,.T.);
#50889=EDGE_CURVE('',#39658,#39659,#4321,.T.);
#50890=EDGE_CURVE('',#39660,#38645,#29357,.T.);
#50891=EDGE_CURVE('',#39651,#39657,#29358,.T.);
#50892=EDGE_CURVE('',#39659,#39657,#4322,.T.);
#50893=EDGE_CURVE('',#38644,#39660,#29359,.T.);
#50894=EDGE_CURVE('',#39657,#39656,#4323,.T.);
#50895=EDGE_CURVE('',#38574,#38637,#4324,.T.);
#50896=EDGE_CURVE('',#38573,#38636,#4325,.T.);
#50897=EDGE_CURVE('',#39661,#39662,#24976,.T.);
#50898=EDGE_CURVE('',#39662,#39663,#24977,.T.);
#50899=EDGE_CURVE('',#39663,#39661,#20935,.T.);
#50900=EDGE_CURVE('',#39647,#39661,#24978,.T.);
#50901=EDGE_CURVE('',#39662,#39641,#690,.T.);
#50902=EDGE_CURVE('',#39645,#39492,#20936,.T.);
#50903=EDGE_CURVE('',#39493,#39647,#20937,.T.);
#50904=EDGE_CURVE('',#39662,#39644,#691,.T.);
#50905=EDGE_CURVE('',#39494,#39661,#20938,.T.);
#50906=EDGE_CURVE('',#39646,#38955,#20939,.T.);
#50907=EDGE_CURVE('',#39663,#39650,#24979,.T.);
#50908=EDGE_CURVE('',#39495,#39663,#20940,.T.);
#50909=EDGE_CURVE('',#39642,#38954,#20941,.T.);
#50910=EDGE_CURVE('',#39496,#39650,#20942,.T.);
#50911=EDGE_CURVE('',#39643,#38953,#20943,.T.);
#50912=EDGE_CURVE('',#39497,#39649,#20944,.T.);
#50913=EDGE_CURVE('',#39648,#38952,#20945,.T.);
#50914=EDGE_CURVE('',#39664,#39665,#29360,.T.);
#50915=EDGE_CURVE('',#39665,#39666,#24980,.T.);
#50916=EDGE_CURVE('',#39666,#39667,#692,.T.);
#50917=EDGE_CURVE('',#39667,#39668,#29361,.T.);
#50918=EDGE_CURVE('',#39668,#39664,#24981,.T.);
#50919=EDGE_CURVE('',#39669,#39670,#693,.T.);
#50920=EDGE_CURVE('',#39670,#39671,#24982,.T.);
#50921=EDGE_CURVE('',#39672,#39671,#29362,.T.);
#50922=EDGE_CURVE('',#39672,#39673,#24983,.T.);
#50923=EDGE_CURVE('',#39673,#39669,#29363,.T.);
#50924=EDGE_CURVE('',#39671,#39665,#24984,.T.);
#50925=EDGE_CURVE('',#39664,#39672,#20946,.T.);
#50926=EDGE_CURVE('',#39673,#39674,#24985,.T.);
#50927=EDGE_CURVE('',#39675,#39672,#694,.T.);
#50928=EDGE_CURVE('',#39674,#39675,#24986,.T.);
#50929=EDGE_CURVE('',#39675,#39664,#695,.T.);
#50930=EDGE_CURVE('',#39676,#39668,#24987,.T.);
#50931=EDGE_CURVE('',#39675,#39676,#24988,.T.);
#50932=EDGE_CURVE('',#39488,#39674,#20947,.T.);
#50933=EDGE_CURVE('',#39676,#39674,#20948,.T.);
#50934=EDGE_CURVE('',#39489,#39676,#20949,.T.);
#50935=EDGE_CURVE('',#39487,#39673,#20950,.T.);
#50936=EDGE_CURVE('',#39669,#39486,#20951,.T.);
#50937=EDGE_CURVE('',#39670,#38959,#20952,.T.);
#50938=EDGE_CURVE('',#39671,#38958,#20953,.T.);
#50939=EDGE_CURVE('',#39665,#38957,#20954,.T.);
#50940=EDGE_CURVE('',#39666,#38956,#20955,.T.);
#50941=EDGE_CURVE('',#39491,#39667,#20956,.T.);
#50942=EDGE_CURVE('',#39490,#39668,#20957,.T.);
#50943=EDGE_CURVE('',#39677,#39678,#29364,.T.);
#50944=EDGE_CURVE('',#39678,#39679,#24989,.T.);
#50945=EDGE_CURVE('',#39679,#39680,#696,.T.);
#50946=EDGE_CURVE('',#39680,#39681,#29365,.T.);
#50947=EDGE_CURVE('',#39681,#39677,#24990,.T.);
#50948=EDGE_CURVE('',#39682,#39683,#697,.T.);
#50949=EDGE_CURVE('',#39683,#39684,#24991,.T.);
#50950=EDGE_CURVE('',#39685,#39684,#29366,.T.);
#50951=EDGE_CURVE('',#39685,#39686,#24992,.T.);
#50952=EDGE_CURVE('',#39686,#39682,#29367,.T.);
#50953=EDGE_CURVE('',#39684,#39678,#24993,.T.);
#50954=EDGE_CURVE('',#39677,#39685,#20958,.T.);
#50955=EDGE_CURVE('',#39686,#39687,#24994,.T.);
#50956=EDGE_CURVE('',#39688,#39685,#698,.T.);
#50957=EDGE_CURVE('',#39687,#39688,#24995,.T.);
#50958=EDGE_CURVE('',#39688,#39677,#699,.T.);
#50959=EDGE_CURVE('',#39689,#39681,#24996,.T.);
#50960=EDGE_CURVE('',#39688,#39689,#24997,.T.);
#50961=EDGE_CURVE('',#39500,#39687,#20959,.T.);
#50962=EDGE_CURVE('',#39689,#39687,#20960,.T.);
#50963=EDGE_CURVE('',#39501,#39689,#20961,.T.);
#50964=EDGE_CURVE('',#39499,#39686,#20962,.T.);
#50965=EDGE_CURVE('',#39682,#39498,#20963,.T.);
#50966=EDGE_CURVE('',#39683,#38951,#20964,.T.);
#50967=EDGE_CURVE('',#39684,#38950,#20965,.T.);
#50968=EDGE_CURVE('',#39678,#38949,#20966,.T.);
#50969=EDGE_CURVE('',#39679,#38948,#20967,.T.);
#50970=EDGE_CURVE('',#39503,#39680,#20968,.T.);
#50971=EDGE_CURVE('',#39502,#39681,#20969,.T.);
#50972=EDGE_CURVE('',#39690,#39691,#29368,.T.);
#50973=EDGE_CURVE('',#39691,#39692,#24998,.T.);
#50974=EDGE_CURVE('',#39692,#39693,#700,.T.);
#50975=EDGE_CURVE('',#39693,#39694,#29369,.T.);
#50976=EDGE_CURVE('',#39694,#39690,#24999,.T.);
#50977=EDGE_CURVE('',#39695,#39696,#701,.T.);
#50978=EDGE_CURVE('',#39696,#39697,#25000,.T.);
#50979=EDGE_CURVE('',#39698,#39697,#29370,.T.);
#50980=EDGE_CURVE('',#39698,#39699,#25001,.T.);
#50981=EDGE_CURVE('',#39699,#39695,#29371,.T.);
#50982=EDGE_CURVE('',#39697,#39691,#25002,.T.);
#50983=EDGE_CURVE('',#39690,#39698,#20970,.T.);
#50984=EDGE_CURVE('',#39699,#39700,#25003,.T.);
#50985=EDGE_CURVE('',#39701,#39698,#702,.T.);
#50986=EDGE_CURVE('',#39700,#39701,#25004,.T.);
#50987=EDGE_CURVE('',#39701,#39690,#703,.T.);
#50988=EDGE_CURVE('',#39702,#39694,#25005,.T.);
#50989=EDGE_CURVE('',#39701,#39702,#25006,.T.);
#50990=EDGE_CURVE('',#39506,#39700,#20971,.T.);
#50991=EDGE_CURVE('',#39702,#39700,#20972,.T.);
#50992=EDGE_CURVE('',#39507,#39702,#20973,.T.);
#50993=EDGE_CURVE('',#39505,#39699,#20974,.T.);
#50994=EDGE_CURVE('',#39695,#39504,#20975,.T.);
#50995=EDGE_CURVE('',#39696,#38947,#20976,.T.);
#50996=EDGE_CURVE('',#39697,#38946,#20977,.T.);
#50997=EDGE_CURVE('',#39691,#38945,#20978,.T.);
#50998=EDGE_CURVE('',#39692,#38944,#20979,.T.);
#50999=EDGE_CURVE('',#39509,#39693,#20980,.T.);
#51000=EDGE_CURVE('',#39508,#39694,#20981,.T.);
#51001=EDGE_CURVE('',#39703,#39704,#29372,.T.);
#51002=EDGE_CURVE('',#39704,#39705,#25007,.T.);
#51003=EDGE_CURVE('',#39705,#39706,#704,.T.);
#51004=EDGE_CURVE('',#39706,#39707,#29373,.T.);
#51005=EDGE_CURVE('',#39707,#39703,#25008,.T.);
#51006=EDGE_CURVE('',#39708,#39709,#705,.T.);
#51007=EDGE_CURVE('',#39709,#39710,#25009,.T.);
#51008=EDGE_CURVE('',#39711,#39710,#29374,.T.);
#51009=EDGE_CURVE('',#39711,#39712,#25010,.T.);
#51010=EDGE_CURVE('',#39712,#39708,#29375,.T.);
#51011=EDGE_CURVE('',#39710,#39704,#25011,.T.);
#51012=EDGE_CURVE('',#39703,#39711,#20982,.T.);
#51013=EDGE_CURVE('',#39712,#39713,#25012,.T.);
#51014=EDGE_CURVE('',#39714,#39711,#706,.T.);
#51015=EDGE_CURVE('',#39713,#39714,#25013,.T.);
#51016=EDGE_CURVE('',#39714,#39703,#707,.T.);
#51017=EDGE_CURVE('',#39715,#39707,#25014,.T.);
#51018=EDGE_CURVE('',#39714,#39715,#25015,.T.);
#51019=EDGE_CURVE('',#39512,#39713,#20983,.T.);
#51020=EDGE_CURVE('',#39715,#39713,#20984,.T.);
#51021=EDGE_CURVE('',#39513,#39715,#20985,.T.);
#51022=EDGE_CURVE('',#39511,#39712,#20986,.T.);
#51023=EDGE_CURVE('',#39708,#39510,#20987,.T.);
#51024=EDGE_CURVE('',#39709,#38943,#20988,.T.);
#51025=EDGE_CURVE('',#39710,#38942,#20989,.T.);
#51026=EDGE_CURVE('',#39704,#38941,#20990,.T.);
#51027=EDGE_CURVE('',#39705,#38940,#20991,.T.);
#51028=EDGE_CURVE('',#39515,#39706,#20992,.T.);
#51029=EDGE_CURVE('',#39514,#39707,#20993,.T.);
#51030=EDGE_CURVE('',#39716,#39717,#29376,.T.);
#51031=EDGE_CURVE('',#39717,#39718,#25016,.T.);
#51032=EDGE_CURVE('',#39718,#39719,#708,.T.);
#51033=EDGE_CURVE('',#39719,#39720,#29377,.T.);
#51034=EDGE_CURVE('',#39720,#39716,#25017,.T.);
#51035=EDGE_CURVE('',#39721,#39722,#709,.T.);
#51036=EDGE_CURVE('',#39722,#39723,#25018,.T.);
#51037=EDGE_CURVE('',#39724,#39723,#29378,.T.);
#51038=EDGE_CURVE('',#39724,#39725,#25019,.T.);
#51039=EDGE_CURVE('',#39725,#39721,#29379,.T.);
#51040=EDGE_CURVE('',#39723,#39717,#25020,.T.);
#51041=EDGE_CURVE('',#39716,#39724,#20994,.T.);
#51042=EDGE_CURVE('',#39725,#39726,#25021,.T.);
#51043=EDGE_CURVE('',#39727,#39724,#710,.T.);
#51044=EDGE_CURVE('',#39726,#39727,#25022,.T.);
#51045=EDGE_CURVE('',#39727,#39716,#711,.T.);
#51046=EDGE_CURVE('',#39728,#39720,#25023,.T.);
#51047=EDGE_CURVE('',#39727,#39728,#25024,.T.);
#51048=EDGE_CURVE('',#39518,#39726,#20995,.T.);
#51049=EDGE_CURVE('',#39728,#39726,#20996,.T.);
#51050=EDGE_CURVE('',#39519,#39728,#20997,.T.);
#51051=EDGE_CURVE('',#39517,#39725,#20998,.T.);
#51052=EDGE_CURVE('',#39721,#39516,#20999,.T.);
#51053=EDGE_CURVE('',#39722,#38939,#21000,.T.);
#51054=EDGE_CURVE('',#39723,#38938,#21001,.T.);
#51055=EDGE_CURVE('',#39717,#38937,#21002,.T.);
#51056=EDGE_CURVE('',#39718,#38936,#21003,.T.);
#51057=EDGE_CURVE('',#39521,#39719,#21004,.T.);
#51058=EDGE_CURVE('',#39520,#39720,#21005,.T.);
#51059=EDGE_CURVE('',#39729,#39730,#29380,.T.);
#51060=EDGE_CURVE('',#39730,#39731,#25025,.T.);
#51061=EDGE_CURVE('',#39731,#39732,#712,.T.);
#51062=EDGE_CURVE('',#39732,#39733,#29381,.T.);
#51063=EDGE_CURVE('',#39733,#39729,#25026,.T.);
#51064=EDGE_CURVE('',#39734,#39735,#713,.T.);
#51065=EDGE_CURVE('',#39735,#39736,#25027,.T.);
#51066=EDGE_CURVE('',#39737,#39736,#29382,.T.);
#51067=EDGE_CURVE('',#39737,#39738,#25028,.T.);
#51068=EDGE_CURVE('',#39738,#39734,#29383,.T.);
#51069=EDGE_CURVE('',#39736,#39730,#25029,.T.);
#51070=EDGE_CURVE('',#39729,#39737,#21006,.T.);
#51071=EDGE_CURVE('',#39738,#39739,#25030,.T.);
#51072=EDGE_CURVE('',#39740,#39737,#714,.T.);
#51073=EDGE_CURVE('',#39739,#39740,#25031,.T.);
#51074=EDGE_CURVE('',#39740,#39729,#715,.T.);
#51075=EDGE_CURVE('',#39741,#39733,#25032,.T.);
#51076=EDGE_CURVE('',#39740,#39741,#25033,.T.);
#51077=EDGE_CURVE('',#39524,#39739,#21007,.T.);
#51078=EDGE_CURVE('',#39741,#39739,#21008,.T.);
#51079=EDGE_CURVE('',#39525,#39741,#21009,.T.);
#51080=EDGE_CURVE('',#39523,#39738,#21010,.T.);
#51081=EDGE_CURVE('',#39734,#39522,#21011,.T.);
#51082=EDGE_CURVE('',#39735,#38935,#21012,.T.);
#51083=EDGE_CURVE('',#39736,#38934,#21013,.T.);
#51084=EDGE_CURVE('',#39730,#38933,#21014,.T.);
#51085=EDGE_CURVE('',#39731,#38932,#21015,.T.);
#51086=EDGE_CURVE('',#39527,#39732,#21016,.T.);
#51087=EDGE_CURVE('',#39526,#39733,#21017,.T.);
#51088=EDGE_CURVE('',#39742,#39743,#29384,.T.);
#51089=EDGE_CURVE('',#39743,#39744,#25034,.T.);
#51090=EDGE_CURVE('',#39744,#39745,#716,.T.);
#51091=EDGE_CURVE('',#39745,#39746,#29385,.T.);
#51092=EDGE_CURVE('',#39746,#39742,#25035,.T.);
#51093=EDGE_CURVE('',#39747,#39748,#717,.T.);
#51094=EDGE_CURVE('',#39748,#39749,#25036,.T.);
#51095=EDGE_CURVE('',#39750,#39749,#29386,.T.);
#51096=EDGE_CURVE('',#39750,#39751,#25037,.T.);
#51097=EDGE_CURVE('',#39751,#39747,#29387,.T.);
#51098=EDGE_CURVE('',#39749,#39743,#25038,.T.);
#51099=EDGE_CURVE('',#39742,#39750,#21018,.T.);
#51100=EDGE_CURVE('',#39751,#39752,#25039,.T.);
#51101=EDGE_CURVE('',#39753,#39750,#718,.T.);
#51102=EDGE_CURVE('',#39752,#39753,#25040,.T.);
#51103=EDGE_CURVE('',#39753,#39742,#719,.T.);
#51104=EDGE_CURVE('',#39754,#39746,#25041,.T.);
#51105=EDGE_CURVE('',#39753,#39754,#25042,.T.);
#51106=EDGE_CURVE('',#39530,#39752,#21019,.T.);
#51107=EDGE_CURVE('',#39754,#39752,#21020,.T.);
#51108=EDGE_CURVE('',#39531,#39754,#21021,.T.);
#51109=EDGE_CURVE('',#39529,#39751,#21022,.T.);
#51110=EDGE_CURVE('',#39747,#39528,#21023,.T.);
#51111=EDGE_CURVE('',#39748,#38931,#21024,.T.);
#51112=EDGE_CURVE('',#39749,#38930,#21025,.T.);
#51113=EDGE_CURVE('',#39743,#38929,#21026,.T.);
#51114=EDGE_CURVE('',#39744,#38928,#21027,.T.);
#51115=EDGE_CURVE('',#39533,#39745,#21028,.T.);
#51116=EDGE_CURVE('',#39532,#39746,#21029,.T.);
#51117=EDGE_CURVE('',#39755,#39756,#29388,.T.);
#51118=EDGE_CURVE('',#39756,#39757,#25043,.T.);
#51119=EDGE_CURVE('',#39757,#39758,#720,.T.);
#51120=EDGE_CURVE('',#39758,#39759,#29389,.T.);
#51121=EDGE_CURVE('',#39759,#39755,#25044,.T.);
#51122=EDGE_CURVE('',#39760,#39761,#721,.T.);
#51123=EDGE_CURVE('',#39761,#39762,#25045,.T.);
#51124=EDGE_CURVE('',#39763,#39762,#29390,.T.);
#51125=EDGE_CURVE('',#39763,#39764,#25046,.T.);
#51126=EDGE_CURVE('',#39764,#39760,#29391,.T.);
#51127=EDGE_CURVE('',#39762,#39756,#25047,.T.);
#51128=EDGE_CURVE('',#39755,#39763,#21030,.T.);
#51129=EDGE_CURVE('',#39764,#39765,#25048,.T.);
#51130=EDGE_CURVE('',#39766,#39763,#722,.T.);
#51131=EDGE_CURVE('',#39765,#39766,#25049,.T.);
#51132=EDGE_CURVE('',#39766,#39755,#723,.T.);
#51133=EDGE_CURVE('',#39767,#39759,#25050,.T.);
#51134=EDGE_CURVE('',#39766,#39767,#25051,.T.);
#51135=EDGE_CURVE('',#39536,#39765,#21031,.T.);
#51136=EDGE_CURVE('',#39767,#39765,#21032,.T.);
#51137=EDGE_CURVE('',#39537,#39767,#21033,.T.);
#51138=EDGE_CURVE('',#39535,#39764,#21034,.T.);
#51139=EDGE_CURVE('',#39760,#39534,#21035,.T.);
#51140=EDGE_CURVE('',#39761,#38927,#21036,.T.);
#51141=EDGE_CURVE('',#39762,#38926,#21037,.T.);
#51142=EDGE_CURVE('',#39756,#38925,#21038,.T.);
#51143=EDGE_CURVE('',#39757,#38924,#21039,.T.);
#51144=EDGE_CURVE('',#39539,#39758,#21040,.T.);
#51145=EDGE_CURVE('',#39538,#39759,#21041,.T.);
#51146=EDGE_CURVE('',#39768,#39769,#29392,.T.);
#51147=EDGE_CURVE('',#39769,#39770,#25052,.T.);
#51148=EDGE_CURVE('',#39770,#39771,#724,.T.);
#51149=EDGE_CURVE('',#39771,#39772,#29393,.T.);
#51150=EDGE_CURVE('',#39772,#39768,#25053,.T.);
#51151=EDGE_CURVE('',#39773,#39774,#725,.T.);
#51152=EDGE_CURVE('',#39774,#39775,#25054,.T.);
#51153=EDGE_CURVE('',#39776,#39775,#29394,.T.);
#51154=EDGE_CURVE('',#39776,#39777,#25055,.T.);
#51155=EDGE_CURVE('',#39777,#39773,#29395,.T.);
#51156=EDGE_CURVE('',#39775,#39769,#25056,.T.);
#51157=EDGE_CURVE('',#39768,#39776,#21042,.T.);
#51158=EDGE_CURVE('',#39777,#39778,#25057,.T.);
#51159=EDGE_CURVE('',#39779,#39776,#726,.T.);
#51160=EDGE_CURVE('',#39778,#39779,#25058,.T.);
#51161=EDGE_CURVE('',#39779,#39768,#727,.T.);
#51162=EDGE_CURVE('',#39780,#39772,#25059,.T.);
#51163=EDGE_CURVE('',#39779,#39780,#25060,.T.);
#51164=EDGE_CURVE('',#39542,#39778,#21043,.T.);
#51165=EDGE_CURVE('',#39780,#39778,#21044,.T.);
#51166=EDGE_CURVE('',#39543,#39780,#21045,.T.);
#51167=EDGE_CURVE('',#39541,#39777,#21046,.T.);
#51168=EDGE_CURVE('',#39773,#39540,#21047,.T.);
#51169=EDGE_CURVE('',#39774,#38923,#21048,.T.);
#51170=EDGE_CURVE('',#39775,#38922,#21049,.T.);
#51171=EDGE_CURVE('',#39769,#38921,#21050,.T.);
#51172=EDGE_CURVE('',#39770,#38920,#21051,.T.);
#51173=EDGE_CURVE('',#39545,#39771,#21052,.T.);
#51174=EDGE_CURVE('',#39544,#39772,#21053,.T.);
#51175=EDGE_CURVE('',#39781,#39782,#29396,.T.);
#51176=EDGE_CURVE('',#39782,#39783,#25061,.T.);
#51177=EDGE_CURVE('',#39783,#39784,#728,.T.);
#51178=EDGE_CURVE('',#39784,#39785,#29397,.T.);
#51179=EDGE_CURVE('',#39785,#39781,#25062,.T.);
#51180=EDGE_CURVE('',#39786,#39787,#729,.T.);
#51181=EDGE_CURVE('',#39787,#39788,#25063,.T.);
#51182=EDGE_CURVE('',#39789,#39788,#29398,.T.);
#51183=EDGE_CURVE('',#39789,#39790,#25064,.T.);
#51184=EDGE_CURVE('',#39790,#39786,#29399,.T.);
#51185=EDGE_CURVE('',#39788,#39782,#25065,.T.);
#51186=EDGE_CURVE('',#39781,#39789,#21054,.T.);
#51187=EDGE_CURVE('',#39790,#39791,#25066,.T.);
#51188=EDGE_CURVE('',#39792,#39789,#730,.T.);
#51189=EDGE_CURVE('',#39791,#39792,#25067,.T.);
#51190=EDGE_CURVE('',#39792,#39781,#731,.T.);
#51191=EDGE_CURVE('',#39793,#39785,#25068,.T.);
#51192=EDGE_CURVE('',#39792,#39793,#25069,.T.);
#51193=EDGE_CURVE('',#39548,#39791,#21055,.T.);
#51194=EDGE_CURVE('',#39793,#39791,#21056,.T.);
#51195=EDGE_CURVE('',#39549,#39793,#21057,.T.);
#51196=EDGE_CURVE('',#39547,#39790,#21058,.T.);
#51197=EDGE_CURVE('',#39786,#39546,#21059,.T.);
#51198=EDGE_CURVE('',#39787,#38919,#21060,.T.);
#51199=EDGE_CURVE('',#39788,#38918,#21061,.T.);
#51200=EDGE_CURVE('',#39782,#38917,#21062,.T.);
#51201=EDGE_CURVE('',#39783,#38916,#21063,.T.);
#51202=EDGE_CURVE('',#39551,#39784,#21064,.T.);
#51203=EDGE_CURVE('',#39550,#39785,#21065,.T.);
#51204=EDGE_CURVE('',#39794,#39795,#29400,.T.);
#51205=EDGE_CURVE('',#39795,#39796,#25070,.T.);
#51206=EDGE_CURVE('',#39796,#39797,#732,.T.);
#51207=EDGE_CURVE('',#39797,#39798,#29401,.T.);
#51208=EDGE_CURVE('',#39798,#39794,#25071,.T.);
#51209=EDGE_CURVE('',#39799,#39800,#733,.T.);
#51210=EDGE_CURVE('',#39800,#39801,#25072,.T.);
#51211=EDGE_CURVE('',#39802,#39801,#29402,.T.);
#51212=EDGE_CURVE('',#39802,#39803,#25073,.T.);
#51213=EDGE_CURVE('',#39803,#39799,#29403,.T.);
#51214=EDGE_CURVE('',#39801,#39795,#25074,.T.);
#51215=EDGE_CURVE('',#39794,#39802,#21066,.T.);
#51216=EDGE_CURVE('',#39803,#39804,#25075,.T.);
#51217=EDGE_CURVE('',#39805,#39802,#734,.T.);
#51218=EDGE_CURVE('',#39804,#39805,#25076,.T.);
#51219=EDGE_CURVE('',#39805,#39794,#735,.T.);
#51220=EDGE_CURVE('',#39806,#39798,#25077,.T.);
#51221=EDGE_CURVE('',#39805,#39806,#25078,.T.);
#51222=EDGE_CURVE('',#39554,#39804,#21067,.T.);
#51223=EDGE_CURVE('',#39806,#39804,#21068,.T.);
#51224=EDGE_CURVE('',#39555,#39806,#21069,.T.);
#51225=EDGE_CURVE('',#39553,#39803,#21070,.T.);
#51226=EDGE_CURVE('',#39799,#39552,#21071,.T.);
#51227=EDGE_CURVE('',#39800,#38915,#21072,.T.);
#51228=EDGE_CURVE('',#39801,#38914,#21073,.T.);
#51229=EDGE_CURVE('',#39795,#38913,#21074,.T.);
#51230=EDGE_CURVE('',#39796,#38912,#21075,.T.);
#51231=EDGE_CURVE('',#39557,#39797,#21076,.T.);
#51232=EDGE_CURVE('',#39556,#39798,#21077,.T.);
#51233=EDGE_CURVE('',#39807,#39808,#29404,.T.);
#51234=EDGE_CURVE('',#39808,#39809,#25079,.T.);
#51235=EDGE_CURVE('',#39809,#39810,#736,.T.);
#51236=EDGE_CURVE('',#39810,#39811,#29405,.T.);
#51237=EDGE_CURVE('',#39811,#39807,#25080,.T.);
#51238=EDGE_CURVE('',#39812,#39813,#737,.T.);
#51239=EDGE_CURVE('',#39813,#39814,#25081,.T.);
#51240=EDGE_CURVE('',#39815,#39814,#29406,.T.);
#51241=EDGE_CURVE('',#39815,#39816,#25082,.T.);
#51242=EDGE_CURVE('',#39816,#39812,#29407,.T.);
#51243=EDGE_CURVE('',#39814,#39808,#25083,.T.);
#51244=EDGE_CURVE('',#39807,#39815,#21078,.T.);
#51245=EDGE_CURVE('',#39816,#39817,#25084,.T.);
#51246=EDGE_CURVE('',#39818,#39815,#738,.T.);
#51247=EDGE_CURVE('',#39817,#39818,#25085,.T.);
#51248=EDGE_CURVE('',#39818,#39807,#739,.T.);
#51249=EDGE_CURVE('',#39819,#39811,#25086,.T.);
#51250=EDGE_CURVE('',#39818,#39819,#25087,.T.);
#51251=EDGE_CURVE('',#39560,#39817,#21079,.T.);
#51252=EDGE_CURVE('',#39819,#39817,#21080,.T.);
#51253=EDGE_CURVE('',#39561,#39819,#21081,.T.);
#51254=EDGE_CURVE('',#39559,#39816,#21082,.T.);
#51255=EDGE_CURVE('',#39812,#39558,#21083,.T.);
#51256=EDGE_CURVE('',#39813,#38911,#21084,.T.);
#51257=EDGE_CURVE('',#39814,#38910,#21085,.T.);
#51258=EDGE_CURVE('',#39808,#38909,#21086,.T.);
#51259=EDGE_CURVE('',#39809,#38908,#21087,.T.);
#51260=EDGE_CURVE('',#39563,#39810,#21088,.T.);
#51261=EDGE_CURVE('',#39562,#39811,#21089,.T.);
#51262=EDGE_CURVE('',#39820,#39821,#29408,.T.);
#51263=EDGE_CURVE('',#39821,#39822,#25088,.T.);
#51264=EDGE_CURVE('',#39822,#39823,#740,.T.);
#51265=EDGE_CURVE('',#39823,#39824,#29409,.T.);
#51266=EDGE_CURVE('',#39824,#39820,#25089,.T.);
#51267=EDGE_CURVE('',#39825,#39826,#741,.T.);
#51268=EDGE_CURVE('',#39826,#39827,#25090,.T.);
#51269=EDGE_CURVE('',#39828,#39827,#29410,.T.);
#51270=EDGE_CURVE('',#39828,#39829,#25091,.T.);
#51271=EDGE_CURVE('',#39829,#39825,#29411,.T.);
#51272=EDGE_CURVE('',#39827,#39821,#25092,.T.);
#51273=EDGE_CURVE('',#39820,#39828,#21090,.T.);
#51274=EDGE_CURVE('',#39829,#39830,#25093,.T.);
#51275=EDGE_CURVE('',#39831,#39828,#742,.T.);
#51276=EDGE_CURVE('',#39830,#39831,#25094,.T.);
#51277=EDGE_CURVE('',#39831,#39820,#743,.T.);
#51278=EDGE_CURVE('',#39832,#39824,#25095,.T.);
